#209082=CARTESIAN_POINT('Ctrl Pts',(2.52028415758831,-6.28271462300916,
104.318570490676));
#209083=CARTESIAN_POINT('Ctrl Pts',(2.68460881655648,-6.21169578312293,
104.327018513438));
#209084=CARTESIAN_POINT('Ctrl Pts',(2.84878299852662,-6.14074197730947,
104.335458800094));
#209085=CARTESIAN_POINT('Ctrl Pts',(3.01026364408896,-6.06322319471181,
104.34389908675));
#209086=CARTESIAN_POINT('Ctrl Pts',(3.16850999156815,-5.97936731045458,
104.352339373406));
#209087=CARTESIAN_POINT('Ctrl Pts',(3.3266357892767,-5.89557530639284,104.360773230374));
#209088=CARTESIAN_POINT('Ctrl Pts',(3.48153190691948,-5.80545597994448,
104.369207087342));
#209089=CARTESIAN_POINT('Ctrl Pts',(3.63267947922354,-5.70928443863399,
104.37764094431));
#209090=CARTESIAN_POINT('Ctrl Pts',(3.78373514595703,-5.61317137461322,
104.386069673055));
#209091=CARTESIAN_POINT('Ctrl Pts',(3.93104653099945,-5.51101361138082,
104.3944984018));
#209092=CARTESIAN_POINT('Ctrl Pts',(4.07412086986689,-5.40313132708386,
104.402927130545));
#209093=CARTESIAN_POINT('Ctrl Pts',(4.21713018301642,-5.29529807410197,
104.411352028525));
#209094=CARTESIAN_POINT('Ctrl Pts',(4.35590602398585,-5.18174568838335,
104.419776926505));
#209095=CARTESIAN_POINT('Ctrl Pts',(4.48998571657338,-5.06283687915847,
104.428201824485));
#209096=CARTESIAN_POINT('Ctrl Pts',(4.62403572369899,-4.94395439653726,
104.43662485718));
#209097=CARTESIAN_POINT('Ctrl Pts',(4.75339140443516,-4.81971807401098,
104.445047889874));
#209098=CARTESIAN_POINT('Ctrl Pts',(4.87762380648971,-4.69053035406071,
104.453470922568));
#209099=CARTESIAN_POINT('Ctrl Pts',(5.00184215178932,-4.56135725155395,
104.461893002206));
#209100=CARTESIAN_POINT('Ctrl Pts',(5.12093814295353,-4.42723410881617,
104.470315081843));
#209101=CARTESIAN_POINT('Ctrl Pts',(5.23452007913682,-4.28859983457463,
104.478737161481));
#209102=CARTESIAN_POINT('Ctrl Pts',(5.34810501884234,-4.1499618943353,104.487159463829));
#209103=CARTESIAN_POINT('Ctrl Pts',(5.45617540181385,-4.00681284295275,
104.495581766177));
#209104=CARTESIAN_POINT('Ctrl Pts',(5.55837994643813,-3.8596245116636,104.504004068525));
#209105=CARTESIAN_POINT('Ctrl Pts',(5.6606014615458,-3.71241174058912,104.512427769349));
#209106=CARTESIAN_POINT('Ctrl Pts',(5.75695500678292,-3.5611586266538,104.520851470173));
#209107=CARTESIAN_POINT('Ctrl Pts',(5.84713254406289,-3.40636610072385,
104.529275170996));
#209108=CARTESIAN_POINT('Ctrl Pts',(5.93737110530676,-3.25146882527647,
104.537704572215));
#209109=CARTESIAN_POINT('Ctrl Pts',(6.02142513918779,-3.09302764017662,
104.546133973434));
#209110=CARTESIAN_POINT('Ctrl Pts',(6.09903202398758,-2.93156909698099,
104.554563374653));
#209111=CARTESIAN_POINT('Ctrl Pts',(6.17666659881646,-2.77005294560062,
104.562995783471));
#209112=CARTESIAN_POINT('Ctrl Pts',(6.2478492989051,-2.60551759265549,104.571428192289));
#209113=CARTESIAN_POINT('Ctrl Pts',(6.31236539513704,-2.43851022517365,
104.579860601106));
#209114=CARTESIAN_POINT('Ctrl Pts',(6.37694118353806,-2.27134833761696,
104.588300811834));
#209115=CARTESIAN_POINT('Ctrl Pts',(6.43483792971866,-2.10171017917188,
104.596741022562));
#209116=CARTESIAN_POINT('Ctrl Pts',(6.48589022627108,-1.93015983088483,
104.605181233289));
#209117=CARTESIAN_POINT('Ctrl Pts',(6.51492790138721,-1.83258492013611,
104.609981881126));
#209118=CARTESIAN_POINT('Ctrl Pts',(6.54175222038416,-1.73439164339507,
104.614782528963));
#209119=CARTESIAN_POINT('Ctrl Pts',(6.56634009650628,-1.63568540282473,
104.6195831768));
#209120=CARTESIAN_POINT('Ctrl Pts',(6.6080299499784,-1.46832451790231,104.627722891833));
#209121=CARTESIAN_POINT('Ctrl Pts',(6.6433704814629,-1.29915463673605,104.635862606866));
#209122=CARTESIAN_POINT('Ctrl Pts',(6.67220489363832,-1.12870317502381,
104.644002321899));
#209123=CARTESIAN_POINT('Ctrl Pts',(6.70101408740983,-0.958400789137468,
104.652134917986));
#209124=CARTESIAN_POINT('Ctrl Pts',(6.72332842754207,-0.786819412381466,
104.660267514073));
#209125=CARTESIAN_POINT('Ctrl Pts',(6.73904139668091,-0.614499840375114,
104.66840011016));
#209126=CARTESIAN_POINT('Ctrl Pts',(6.75474362359105,-0.442298075273033,
104.676527146368));
#209127=CARTESIAN_POINT('Ctrl Pts',(6.76385343164389,-0.269359482892504,
104.684654182576));
#209128=CARTESIAN_POINT('Ctrl Pts',(6.76631570154596,-0.0962331908053344,
104.692781218783));
#209129=CARTESIAN_POINT('Ctrl Pts',(6.76877679443847,0.0768103437815226,
104.700904370121));
#209130=CARTESIAN_POINT('Ctrl Pts',(6.76459667171424,0.250041034011858,
104.709027521459));
#209131=CARTESIAN_POINT('Ctrl Pts',(6.75377220999347,0.422906532841329,
104.717150672796));
#209132=CARTESIAN_POINT('Ctrl Pts',(6.74295079002694,0.59572345518014,104.725271541468));
#209133=CARTESIAN_POINT('Ctrl Pts',(6.72548877363209,0.768175025394373,
104.733392410139));
#209134=CARTESIAN_POINT('Ctrl Pts',(6.7014351104815,0.939710838506064,104.741513278811));
#209135=CARTESIAN_POINT('Ctrl Pts',(6.6773801473788,1.11125592207034,104.749634586366));
#209136=CARTESIAN_POINT('Ctrl Pts',(6.6467328727442,1.28188478642956,104.75775589392));
#209137=CARTESIAN_POINT('Ctrl Pts',(6.60959390715445,1.4510538868377,104.765877201475));
#209138=CARTESIAN_POINT('Ctrl Pts',(6.59029520961563,1.53896003203717,104.770097315191));
#209139=CARTESIAN_POINT('Ctrl Pts',(6.56924446865013,1.62647215923695,104.774317428908));
#209140=CARTESIAN_POINT('Ctrl Pts',(6.5464612221734,1.71351523675161,104.778537542625));
#209141=CARTESIAN_POINT('Ctrl Pts',(6.49795668150834,1.89882616235804,104.787521981151));
#209142=CARTESIAN_POINT('Ctrl Pts',(6.44162091720304,2.08191852549232,104.796506419677));
#209143=CARTESIAN_POINT('Ctrl Pts',(6.37768797078266,2.26216381973856,104.805490858203));
#209144=CARTESIAN_POINT('Ctrl Pts',(6.3136446799129,2.44272020660387,104.814490803333));
#209145=CARTESIAN_POINT('Ctrl Pts',(6.24197807890539,2.62041947783379,104.823490748463));
#209146=CARTESIAN_POINT('Ctrl Pts',(6.16297031630131,2.79465308766382,104.832490693594));
#209147=CARTESIAN_POINT('Ctrl Pts',(6.08377636987625,2.9692972834686,104.841511847326));
#209148=CARTESIAN_POINT('Ctrl Pts',(5.99720674718061,3.14045925867974,104.850533001058));
#209149=CARTESIAN_POINT('Ctrl Pts',(5.90359083813182,3.30755260214044,104.859554154791));
#209150=CARTESIAN_POINT('Ctrl Pts',(5.80987967415799,3.47481596439463,104.868584487618));
#209151=CARTESIAN_POINT('Ctrl Pts',(5.70910802255661,3.6380022191138,104.877614820445));
#209152=CARTESIAN_POINT('Ctrl Pts',(5.60164951120217,3.79655261436589,104.886645153272));
#209153=CARTESIAN_POINT('Ctrl Pts',(5.49403865755124,3.95532778410088,104.895688288265));
#209154=CARTESIAN_POINT('Ctrl Pts',(5.37972212307625,4.10945375520907,104.904731423258));
#209155=CARTESIAN_POINT('Ctrl Pts',(5.25911622901807,4.25840175296774,104.91377455825));
#209156=CARTESIAN_POINT('Ctrl Pts',(5.15367889163944,4.38861661861916,104.92168034165));
#209157=CARTESIAN_POINT('Ctrl Pts',(5.04343541851787,4.51487448688405,104.92958612505));
#209158=CARTESIAN_POINT('Ctrl Pts',(4.92868823279422,4.63684389471069,104.93749190845));
#209159=CARTESIAN_POINT('Ctrl Pts',(4.79755503406507,4.77623065608998,104.946526645635));
#209160=CARTESIAN_POINT('Ctrl Pts',(4.66041770868393,4.91014402847871,104.955561382819));
#209161=CARTESIAN_POINT('Ctrl Pts',(4.51775470906506,5.03807318215213,104.964596120004));
#209162=CARTESIAN_POINT('Ctrl Pts',(4.38125891205211,5.16047206510353,104.973240293028));
#209163=CARTESIAN_POINT('Ctrl Pts',(4.23970535783228,5.27739295980276,104.981884466052));
#209164=CARTESIAN_POINT('Ctrl Pts',(4.09355174753297,5.38842491738261,104.990528639076));
#209165=CARTESIAN_POINT('Ctrl Pts',(3.94751050382896,5.49937151078282,104.999166166241));
#209166=CARTESIAN_POINT('Ctrl Pts',(3.79687649770736,5.60443801198851,105.007803693406));
#209167=CARTESIAN_POINT('Ctrl Pts',(3.64214091206989,5.70325333267134,105.016441220571));
#209168=CARTESIAN_POINT('Ctrl Pts',(3.48754311963719,5.80198065756663,105.025071055953));
#209169=CARTESIAN_POINT('Ctrl Pts',(3.32885129101073,5.89446774573588,105.033700891335));
#209170=CARTESIAN_POINT('Ctrl Pts',(3.16658630182934,5.98038629129146,105.042330726717));
#209171=CARTESIAN_POINT('Ctrl Pts',(3.14416066484509,5.99226056018066,105.0435234027));
#209172=CARTESIAN_POINT('Ctrl Pts',(3.12166682451649,6.00400943580988,105.044716078683));
#209173=CARTESIAN_POINT('Ctrl Pts',(3.09910619832126,6.01563211736944,105.045908754666));
#209174=CARTESIAN_POINT('Ctrl Pts',(3.09910619832139,6.01563211736937,103.045799558392));
#209175=CARTESIAN_POINT('Ctrl Pts',(2.94236430513783,6.09638169833182,103.054111211667));
#209176=CARTESIAN_POINT('Ctrl Pts',(2.78233017481925,6.17107055504067,103.062422864941));
#209177=CARTESIAN_POINT('Ctrl Pts',(2.61950763306529,6.2394285603982,103.070734518215));
#209178=CARTESIAN_POINT('Ctrl Pts',(2.45680390152898,6.30773668550323,103.079040106547));
#209179=CARTESIAN_POINT('Ctrl Pts',(2.29131613225174,6.36972302967539,103.087345694879));
#209180=CARTESIAN_POINT('Ctrl Pts',(2.12357116630314,6.42516416145502,103.095651283211));
#209181=CARTESIAN_POINT('Ctrl Pts',(1.9559178560199,6.48057500026106,103.103952333379));
#209182=CARTESIAN_POINT('Ctrl Pts',(1.78601013636463,6.52944764453699,103.112253383547));
#209183=CARTESIAN_POINT('Ctrl Pts',(1.61439338256553,6.57160733811209,103.120554433714));
#209184=CARTESIAN_POINT('Ctrl Pts',(1.44283895574051,6.61375172032585,103.128852469145));
#209185=CARTESIAN_POINT('Ctrl Pts',(1.26957706925807,6.64918792812348,103.137150504576));
#209186=CARTESIAN_POINT('Ctrl Pts',(1.09516698237773,6.67779142237235,103.145448540007));
#209187=CARTESIAN_POINT('Ctrl Pts',(0.917825849735268,6.70687561215953,
103.153886027932));
#209188=CARTESIAN_POINT('Ctrl Pts',(0.739297935222967,6.72889528581189,
103.162323515856));
#209189=CARTESIAN_POINT('Ctrl Pts',(0.560181124280923,6.74377387728854,
103.170761003781));
#209190=CARTESIAN_POINT('Ctrl Pts',(0.384014197523693,6.75840743245924,
103.179059534273));
#209191=CARTESIAN_POINT('Ctrl Pts',(0.207277979361667,6.76613330032755,
103.187358064766));
#209192=CARTESIAN_POINT('Ctrl Pts',(0.0305455202347726,6.76693106002962,
103.195656595258));
#209193=CARTESIAN_POINT('Ctrl Pts',(-0.14622375551021,6.7677289859197,103.203956854486));
#209194=CARTESIAN_POINT('Ctrl Pts',(-0.322988922558483,6.76159592535089,
103.212257113715));
#209195=CARTESIAN_POINT('Ctrl Pts',(-0.499177629272033,6.74856360231082,
103.220557372943));
#209196=CARTESIAN_POINT('Ctrl Pts',(-0.675432321873086,6.73552639842783,
103.22886074077));
#209197=CARTESIAN_POINT('Ctrl Pts',(-0.851109776893836,6.71558480798511,
103.237164108598));
#209198=CARTESIAN_POINT('Ctrl Pts',(-1.02564326441134,6.68882238470777,
103.245467476425));
#209199=CARTESIAN_POINT('Ctrl Pts',(-1.20515202141174,6.66129706904963,
103.254007540906));
#209200=CARTESIAN_POINT('Ctrl Pts',(-1.38345023086992,6.62655634228058,
103.262547605388));
#209201=CARTESIAN_POINT('Ctrl Pts',(-1.55993391594156,6.58474716127318,
103.271087669869));
#209202=CARTESIAN_POINT('Ctrl Pts',(-1.73182960695066,6.54402488115492,
103.279405720825));
#209203=CARTESIAN_POINT('Ctrl Pts',(-1.90200362431914,6.49659723332589,
103.287723771781));
#209204=CARTESIAN_POINT('Ctrl Pts',(-2.0699146776535,6.44265024871245,103.296041822737));
#209205=CARTESIAN_POINT('Ctrl Pts',(-2.24454819370229,6.3865434504035,103.304692893981));
#209206=CARTESIAN_POINT('Ctrl Pts',(-2.41673340417195,6.32338468216138,
103.313343965225));
#209207=CARTESIAN_POINT('Ctrl Pts',(-2.58588599787128,6.25343766307887,
103.321995036469));
#209208=CARTESIAN_POINT('Ctrl Pts',(-2.7550385915706,6.18349064399635,103.330646107713));
#209209=CARTESIAN_POINT('Ctrl Pts',(-2.92115821549834,6.1067556047809,103.339297178958));
#209210=CARTESIAN_POINT('Ctrl Pts',(-3.08369109684616,6.02354864006524,
103.347948250202));
#209211=CARTESIAN_POINT('Ctrl Pts',(-3.23530414982311,5.94593196432015,
103.356018096205));
#209212=CARTESIAN_POINT('Ctrl Pts',(-3.38426480533369,5.86244398788228,
103.364087942207));
#209213=CARTESIAN_POINT('Ctrl Pts',(-3.5300736531061,5.7732892707404,103.37215778821));
#209214=CARTESIAN_POINT('Ctrl Pts',(-3.67569905480191,5.68424672157268,
103.38021748132));
#209215=CARTESIAN_POINT('Ctrl Pts',(-3.81818022451315,5.58955180955035,
103.38827717443));
#209216=CARTESIAN_POINT('Ctrl Pts',(-3.95703853568271,5.48945671511508,
103.39633686754));
#209217=CARTESIAN_POINT('Ctrl Pts',(-4.09575262044103,5.38946558533365,
103.404388189379));
#209218=CARTESIAN_POINT('Ctrl Pts',(-4.23085103481182,5.28408565131226,
103.412439511218));
#209219=CARTESIAN_POINT('Ctrl Pts',(-4.36188064280269,5.17361442880538,
103.420490833056));
#209220=CARTESIAN_POINT('Ctrl Pts',(-4.49280286878587,5.06323374020031,
103.428535556637));
#209221=CARTESIAN_POINT('Ctrl Pts',(-4.61966264130249,4.94777030686426,
103.436580280218));
#209222=CARTESIAN_POINT('Ctrl Pts',(-4.74203676498044,4.82756422221122,
103.444625003799));
#209223=CARTESIAN_POINT('Ctrl Pts',(-4.86433738778352,4.70743033625609,
103.452664895524));
#209224=CARTESIAN_POINT('Ctrl Pts',(-4.98215745955112,4.58255973036248,
103.460704787248));
#209225=CARTESIAN_POINT('Ctrl Pts',(-5.09510787076625,4.45333187459186,
103.468744678972));
#209226=CARTESIAN_POINT('Ctrl Pts',(-5.21049041378296,4.32132138904337,
103.476957691592));
#209227=CARTESIAN_POINT('Ctrl Pts',(-5.3207908982104,4.1847641347449,103.485170704212));
#209228=CARTESIAN_POINT('Ctrl Pts',(-5.42563495129075,4.04410365536447,
103.493383716832));
#209229=CARTESIAN_POINT('Ctrl Pts',(-5.5282332020267,3.90645618077615,103.501420803375));
#209230=CARTESIAN_POINT('Ctrl Pts',(-5.62560618959596,3.76487980538032,
103.509457889917));
#209231=CARTESIAN_POINT('Ctrl Pts',(-5.71744473488568,3.61982246850975,
103.51749497646));
#209232=CARTESIAN_POINT('Ctrl Pts',(-5.80929206955164,3.47475124897689,
103.525532832189));
#209233=CARTESIAN_POINT('Ctrl Pts',(-5.89560370729836,3.32619872024178,
103.533570687918));
#209234=CARTESIAN_POINT('Ctrl Pts',(-5.97611480369843,3.17464027143493,
103.541608543648));
#209235=CARTESIAN_POINT('Ctrl Pts',(-6.05664955732139,3.0230372889903,103.549648761205));
#209236=CARTESIAN_POINT('Ctrl Pts',(-6.13138020182837,2.86842695816172,
103.557688978762));
#209237=CARTESIAN_POINT('Ctrl Pts',(-6.20008876476533,2.71130749068245,
103.565729196319));
#209238=CARTESIAN_POINT('Ctrl Pts',(-6.27139318123286,2.54825194905253,
103.574073178446));
#209239=CARTESIAN_POINT('Ctrl Pts',(-6.33621141358448,2.38249438169519,
103.582417160574));
#209240=CARTESIAN_POINT('Ctrl Pts',(-6.39435583166184,2.21461113925045,
103.590761142702));
#209241=CARTESIAN_POINT('Ctrl Pts',(-6.45048102793904,2.05255809537398,
103.598815357537));
#209242=CARTESIAN_POINT('Ctrl Pts',(-6.50038812801885,1.88852491222502,
103.606869572372));
#209243=CARTESIAN_POINT('Ctrl Pts',(-6.54396024116556,1.72304189213275,
103.614923787207));
#209244=CARTESIAN_POINT('Ctrl Pts',(-6.58756496083387,1.55743503536424,
103.62298402929));
#209245=CARTESIAN_POINT('Ctrl Pts',(-6.62482517347593,1.39037654348746,
103.631044271373));
#209246=CARTESIAN_POINT('Ctrl Pts',(-6.65567557661696,1.2224040325623,103.639104513456));
#209247=CARTESIAN_POINT('Ctrl Pts',(-6.68656911073776,1.05419668454476,
103.647176024311));
#209248=CARTESIAN_POINT('Ctrl Pts',(-6.71103490292835,0.885073134178257,
103.655247535165));
#209249=CARTESIAN_POINT('Ctrl Pts',(-6.72905960490018,0.715573779355196,
103.663319046019));
#209250=CARTESIAN_POINT('Ctrl Pts',(-6.7309487818599,0.697808477253693,
103.66416502463));
#209251=CARTESIAN_POINT('Ctrl Pts',(-6.73276724909369,0.680039044307874,
103.665011003241));
#209252=CARTESIAN_POINT('Ctrl Pts',(-6.73451502427644,0.662266100442202,
103.665856981852));
#209253=CARTESIAN_POINT('Ctrl Pts',(-6.75608578867897,0.442915243049773,
103.676297915838));
#209254=CARTESIAN_POINT('Ctrl Pts',(-6.76693576375581,0.222572616147481,
103.686738849824));
#209255=CARTESIAN_POINT('Ctrl Pts',(-6.76699971567234,0.00196165502752502,
103.69717978381));
#209256=CARTESIAN_POINT('',(-6.767,-8.20588493674615E-10,103.302820216229));
#209257=CARTESIAN_POINT('Ctrl Pts',(3.09910619832148,6.01563211736933,102.651395695404));
#209258=CARTESIAN_POINT('Ctrl Pts',(2.93375330764841,6.10081787314646,102.660145143307));
#209259=CARTESIAN_POINT('Ctrl Pts',(2.76488627843085,6.17918207037032,102.668894591209));
#209260=CARTESIAN_POINT('Ctrl Pts',(2.59307866646717,6.25045854553991,102.677644039111));
#209261=CARTESIAN_POINT('Ctrl Pts',(2.42127244185387,6.32173444515033,102.686393416361));
#209262=CARTESIAN_POINT('Ctrl Pts',(2.2465259467247,6.38592262741836,102.695142793612));
#209263=CARTESIAN_POINT('Ctrl Pts',(2.06943269687121,6.44280508110562,102.703892170862));
#209264=CARTESIAN_POINT('Ctrl Pts',(1.89234081822078,6.49968709436166,102.712641480367));
#209265=CARTESIAN_POINT('Ctrl Pts',(1.7129024940559,6.54926340459544,102.721390789873));
#209266=CARTESIAN_POINT('Ctrl Pts',(1.53172716625061,6.59136563150383,102.730140099378));
#209267=CARTESIAN_POINT('Ctrl Pts',(1.35055318107354,6.63346754640705,102.738889344045));
#209268=CARTESIAN_POINT('Ctrl Pts',(1.16764249714457,6.66809542395769,102.747638588713));
#209269=CARTESIAN_POINT('Ctrl Pts',(0.983616340614903,6.6951316562466,102.75638783338));
#209270=CARTESIAN_POINT('Ctrl Pts',(0.799591486714394,6.72216769715954,
102.765137016116));
#209271=CARTESIAN_POINT('Ctrl Pts',(0.614451459527268,6.74161215869366,
102.773886198851));
#209272=CARTESIAN_POINT('Ctrl Pts',(0.428825047910842,6.75339900185709,
102.782635381587));
#209273=CARTESIAN_POINT('Ctrl Pts',(0.243199888597644,6.76518576550218,
102.791384505298));
#209274=CARTESIAN_POINT('Ctrl Pts',(0.057088637392555,6.76931499599834,
102.800133629008));
#209275=CARTESIAN_POINT('Ctrl Pts',(-0.128876626810473,6.76577266947848,
102.808882752719));
#209276=CARTESIAN_POINT('Ctrl Pts',(-0.314840698187551,6.76223036567996,
102.81763182031));
#209277=CARTESIAN_POINT('Ctrl Pts',(-0.500658497950714,6.75101660879227,
102.826380887902));
#209278=CARTESIAN_POINT('Ctrl Pts',(-0.685698951925747,6.73216948296223,
102.835129955493));
#209279=CARTESIAN_POINT('Ctrl Pts',(-0.870738280459417,6.71332247176299,
102.843878969872));
#209280=CARTESIAN_POINT('Ctrl Pts',(-1.05499998761211,6.68684221356193,
102.85262798425));
#209281=CARTESIAN_POINT('Ctrl Pts',(-1.23785829161383,6.65281863948529,
102.861376998629));
#209282=CARTESIAN_POINT('Ctrl Pts',(-1.43007412917363,6.6170539536887,102.870573732328));
#209283=CARTESIAN_POINT('Ctrl Pts',(-1.62073882535748,6.57295372727801,
102.879770466027));
#209284=CARTESIAN_POINT('Ctrl Pts',(-1.80913696091466,6.52068343478293,
102.888967199726));
#209285=CARTESIAN_POINT('Ctrl Pts',(-1.98838356186064,6.47095219815213,
102.89771719744));
#209286=CARTESIAN_POINT('Ctrl Pts',(-2.16557827572486,6.41382586850907,
102.906467195154));
#209287=CARTESIAN_POINT('Ctrl Pts',(-2.34011918621653,6.34949849943295,
102.915217192867));
#209288=CARTESIAN_POINT('Ctrl Pts',(-2.51465655691045,6.28517243495572,
102.923967013126));
#209289=CARTESIAN_POINT('Ctrl Pts',(-2.68653996295269,6.213645722424,102.932716833384));
#209290=CARTESIAN_POINT('Ctrl Pts',(-2.85518555379923,6.13516132252251,
102.941466653642));
#209291=CARTESIAN_POINT('Ctrl Pts',(-3.02382794858626,6.05667841000538,
102.95021630808));
#209292=CARTESIAN_POINT('Ctrl Pts',(-3.1892323910922,5.97123819492113,102.958965962517));
#209293=CARTESIAN_POINT('Ctrl Pts',(-3.3508370596764,5.87913088810746,102.967715616955));
#209294=CARTESIAN_POINT('Ctrl Pts',(-3.51243888042337,5.78702520443141,
102.976465117204));
#209295=CARTESIAN_POINT('Ctrl Pts',(-3.67024081223624,5.68825280605826,
102.985214617453));
#209296=CARTESIAN_POINT('Ctrl Pts',(-3.82370687544332,5.58314917682552,
102.993964117702));
#209297=CARTESIAN_POINT('Ctrl Pts',(-3.97717043817743,5.47804726008073,
103.002713475392));
#209298=CARTESIAN_POINT('Ctrl Pts',(-4.12629803722387,5.36661448084292,
103.011462833083));
#209299=CARTESIAN_POINT('Ctrl Pts',(-4.27058317206833,5.24922931204638,
103.020212190773));
#209300=CARTESIAN_POINT('Ctrl Pts',(-4.41486614774765,5.13184589986851,
103.028961417533));
#209301=CARTESIAN_POINT('Ctrl Pts',(-4.55430658194349,5.00851045723093,
103.037710644293));
#209302=CARTESIAN_POINT('Ctrl Pts',(-4.68843089001786,4.87964187103176,
103.046459871053));
#209303=CARTESIAN_POINT('Ctrl Pts',(-4.82255336917795,4.75077504208004,
103.055208978509));
#209304=CARTESIAN_POINT('Ctrl Pts',(-4.95135966065109,4.61637541908121,
103.063958085965));
#209305=CARTESIAN_POINT('Ctrl Pts',(-5.07441230869235,4.47689945401855,
103.072707193421));
#209306=CARTESIAN_POINT('Ctrl Pts',(-5.19746344226414,4.3374252055552,103.081456193197));
#209307=CARTESIAN_POINT('Ctrl Pts',(-5.31476088454769,4.19287495491334,
103.090205192974));
#209308=CARTESIAN_POINT('Ctrl Pts',(-5.42590627628861,4.04373961586696,
103.09895419275));
#209309=CARTESIAN_POINT('Ctrl Pts',(-5.53706380672676,3.89458798906723,
103.107704148045));
#209310=CARTESIAN_POINT('Ctrl Pts',(-5.64206777071873,3.7408505015527,103.11645410334));
#209311=CARTESIAN_POINT('Ctrl Pts',(-5.74056148164017,3.58304938223145,
103.125204058634));
#209312=CARTESIAN_POINT('Ctrl Pts',(-5.83905138951896,3.42525435593261,
103.133953676075));
#209313=CARTESIAN_POINT('Ctrl Pts',(-5.93103139557668,3.26339625497156,
103.142703293516));
#209314=CARTESIAN_POINT('Ctrl Pts',(-6.01618907820863,3.09802485064971,
103.151452910958));
#209315=CARTESIAN_POINT('Ctrl Pts',(-6.10134392544994,2.93265895249617,
103.160202237073));
#209316=CARTESIAN_POINT('Ctrl Pts',(-6.17967677261837,2.76378023986023,
103.168951563189));
#209317=CARTESIAN_POINT('Ctrl Pts',(-6.25092157009224,2.59196229227116,
103.177700889305));
#209318=CARTESIAN_POINT('Ctrl Pts',(-6.32216437407745,2.4201491522911,103.186449970608));
#209319=CARTESIAN_POINT('Ctrl Pts',(-6.38631941548907,2.2453972066289,103.19519905191));
#209320=CARTESIAN_POINT('Ctrl Pts',(-6.44316881037518,2.06829994947746,
103.203948133213));
#209321=CARTESIAN_POINT('Ctrl Pts',(-6.50002334524552,1.89118668024516,
103.212698005555));
#209322=CARTESIAN_POINT('Ctrl Pts',(-6.54957082411077,1.71172794807774,
103.221447877897));
#209323=CARTESIAN_POINT('Ctrl Pts',(-6.59164294296065,1.53053334250419,
103.23019775024));
#209324=CARTESIAN_POINT('Ctrl Pts',(-6.63371214082118,1.34935131693678,
103.238947015094));
#209325=CARTESIAN_POINT('Ctrl Pts',(-6.66830695239676,1.16643393829841,
103.247696279949));
#209326=CARTESIAN_POINT('Ctrl Pts',(-6.69530988153977,0.982402458341761,
103.256445544804));
#209327=CARTESIAN_POINT('Ctrl Pts',(-6.72231419690474,0.798361530947849,
103.265195258811));
#209328=CARTESIAN_POINT('Ctrl Pts',(-6.7417258082927,0.613206671363285,
103.273944972818));
#209329=CARTESIAN_POINT('Ctrl Pts',(-6.75347878028174,0.427566795114224,
103.282694686825));
#209330=CARTESIAN_POINT('Ctrl Pts',(-6.76248992368206,0.285234494207036,
103.289403196614));
#209331=CARTESIAN_POINT('Ctrl Pts',(-6.76699999999989,0.142617266094836,
103.296111706402));
#209332=CARTESIAN_POINT('Ctrl Pts',(-6.767,5.08377026670387E-12,103.30282021619));
#209333=CARTESIAN_POINT('Ctrl Pts',(-6.767,-8.20396992685389E-10,103.302820216229));
#209334=CARTESIAN_POINT('Ctrl Pts',(-6.76699999997745,-0.18600725034739,
103.31156972804));
#209335=CARTESIAN_POINT('Ctrl Pts',(-6.75932637290009,-0.372014356569628,
103.320319239851));
#209336=CARTESIAN_POINT('Ctrl Pts',(-6.7440051825742,-0.557389538305465,
103.329068751662));
#209337=CARTESIAN_POINT('Ctrl Pts',(-6.72868405696075,-0.742763937068103,
103.337818226518));
#209338=CARTESIAN_POINT('Ctrl Pts',(-6.7057154563447,-0.927506131055983,
103.346567701374));
#209339=CARTESIAN_POINT('Ctrl Pts',(-6.67517739391316,-1.11098864071181,
103.355317176229));
#209340=CARTESIAN_POINT('Ctrl Pts',(-6.6446394579296,-1.29447039062751,
103.364066614856));
#209341=CARTESIAN_POINT('Ctrl Pts',(-6.60653216990395,-1.47669218394034,
103.372816053483));
#209342=CARTESIAN_POINT('Ctrl Pts',(-6.56098496072521,-1.65703510679093,
103.38156549211));
#209343=CARTESIAN_POINT('Ctrl Pts',(-6.51543793635944,-1.83737729787963,
103.390314895236));
#209344=CARTESIAN_POINT('Ctrl Pts',(-6.46245112142894,-2.01584035589556,
103.399064298361));
#209345=CARTESIAN_POINT('Ctrl Pts',(-6.40220448347582,-2.19181813838697,
103.407813701486));
#209346=CARTESIAN_POINT('Ctrl Pts',(-6.34195808497692,-2.36779522144313,
103.416563069836));
#209347=CARTESIAN_POINT('Ctrl Pts',(-6.27445201402183,-2.5412867776051,
103.425312438186));
#209348=CARTESIAN_POINT('Ctrl Pts',(-6.19991555038909,-2.71170355460246,
103.434061806536));
#209349=CARTESIAN_POINT('Ctrl Pts',(-6.12537937681621,-2.88211966842015,
103.442811140838));
#209350=CARTESIAN_POINT('Ctrl Pts',(-6.04381298015407,-3.04946076445341,
103.45156047514));
#209351=CARTESIAN_POINT('Ctrl Pts',(-5.9554933929672,-3.21315848447038,
103.460309809442));
#209352=CARTESIAN_POINT('Ctrl Pts',(-5.86717414214314,-3.37685558104894,
103.469059110422));
#209353=CARTESIAN_POINT('Ctrl Pts',(-5.77210188833564,-3.53690907716986,
103.477808411402));
#209354=CARTESIAN_POINT('Ctrl Pts',(-5.67059953302075,-3.69277537038267,
103.486557712382));
#209355=CARTESIAN_POINT('Ctrl Pts',(-5.56909755584588,-3.84864108292636,
103.495306980767));
#209356=CARTESIAN_POINT('Ctrl Pts',(-5.46116568148233,-4.00031938363886,
103.504056249153));
#209357=CARTESIAN_POINT('Ctrl Pts',(-5.34717048483224,-4.14729511924808,
103.512805517538));
#209358=CARTESIAN_POINT('Ctrl Pts',(-5.23317570339677,-4.2942703195148,
103.521554754055));
#209359=CARTESIAN_POINT('Ctrl Pts',(-5.11311781949632,-4.43654276251646,
103.530303990572));
#209360=CARTESIAN_POINT('Ctrl Pts',(-4.98740458929211,-4.57362924412419,
103.539053227089));
#209361=CARTESIAN_POINT('Ctrl Pts',(-4.86169180654557,-4.71071523779284,
103.547802432465));
#209362=CARTESIAN_POINT('Ctrl Pts',(-4.73032391145408,-4.84261509580638,
103.55655163784));
#209363=CARTESIAN_POINT('Ctrl Pts',(-4.59374706953327,-4.96888084594052,
103.565300843215));
#209364=CARTESIAN_POINT('Ctrl Pts',(-4.45717070239636,-5.09514615713534,
103.574050018176));
#209365=CARTESIAN_POINT('Ctrl Pts',(-4.31538563507762,-5.21577720511883,
103.582799193136));
#209366=CARTESIAN_POINT('Ctrl Pts',(-4.16887340964834,-5.33036429283469,
103.591548368097));
#209367=CARTESIAN_POINT('Ctrl Pts',(-4.02236168137632,-5.44495099172427,
103.600297513369));
#209368=CARTESIAN_POINT('Ctrl Pts',(-3.87112305280765,-5.55349359485584,
103.609046658641));
#209369=CARTESIAN_POINT('Ctrl Pts',(-3.71567116949112,-5.65562346343995,
103.617795803913));
#209370=CARTESIAN_POINT('Ctrl Pts',(-3.56021980075929,-5.75775299394859,
103.626544920223));
#209371=CARTESIAN_POINT('Ctrl Pts',(-3.40055544467297,-5.8534696750515,
103.635294036533));
#209372=CARTESIAN_POINT('Ctrl Pts',(-3.2372203591472,-5.94244843026197,
103.644043152843));
#209373=CARTESIAN_POINT('Ctrl Pts',(-3.07388580073972,-6.03142689831839,
103.652792240918));
#209374=CARTESIAN_POINT('Ctrl Pts',(-2.90688078822377,-6.11366734692062,
103.661541328993));
#209375=CARTESIAN_POINT('Ctrl Pts',(-2.73677250646261,-6.18889046985567,
103.670290417068));
#209376=CARTESIAN_POINT('Ctrl Pts',(-2.5666647595545,-6.26411335627481,
103.679039477634));
#209377=CARTESIAN_POINT('Ctrl Pts',(-2.39345402498295,-6.33231884529611,
103.6877885382));
#209378=CARTESIAN_POINT('Ctrl Pts',(-2.2177285598797,-6.39327529789653,
103.696537598766));
#209379=CARTESIAN_POINT('Ctrl Pts',(-2.04200363270099,-6.45423156389922,
103.70528663255));
#209380=CARTESIAN_POINT('Ctrl Pts',(-1.86376426110157,-6.50793874398319,
103.714035666333));
#209381=CARTESIAN_POINT('Ctrl Pts',(-1.68361577673416,-6.55421443930025,
103.722784700117));
#209382=CARTESIAN_POINT('Ctrl Pts',(-1.50346782887536,-6.6004899968015,
103.731533707845));
#209383=CARTESIAN_POINT('Ctrl Pts',(-1.32141105714289,-6.63933404253772,
103.740282715573));
#209384=CARTESIAN_POINT('Ctrl Pts',(-1.13806375405982,-6.67061465621387,
103.749031723301));
#209385=CARTESIAN_POINT('Ctrl Pts',(-0.954716981788821,-6.70189517932895,
103.757780705699));
#209386=CARTESIAN_POINT('Ctrl Pts',(-0.770079968085066,-6.72561226601584,
103.766529688097));
#209387=CARTESIAN_POINT('Ctrl Pts',(-0.584779764739224,-6.74168536990207,
103.775278670496));
#209388=CARTESIAN_POINT('Ctrl Pts',(-0.391489829838794,-6.75845151018535,
103.784404889505));
#209389=CARTESIAN_POINT('Ctrl Pts',(-0.197478577433421,-6.7668998303395,
103.793531108515));
#209390=CARTESIAN_POINT('Ctrl Pts',(-0.0034628756550048,-6.76699911397159,
103.802657327524));
#209391=CARTESIAN_POINT('Ctrl Pts',(0.184489835442792,-6.76709529499017,
103.81149835219));
#209392=CARTESIAN_POINT('Ctrl Pts',(0.372446405029021,-6.75935639733849,
103.820339376855));
#209393=CARTESIAN_POINT('Ctrl Pts',(0.559755020257901,-6.74380925866799,
103.82918040152));
#209394=CARTESIAN_POINT('Ctrl Pts',(0.745134706289568,-6.72842222651303,
103.83793038013));
#209395=CARTESIAN_POINT('Ctrl Pts',(0.929879431993717,-6.70538706046913,
103.84668035874));
#209396=CARTESIAN_POINT('Ctrl Pts',(1.1133616370299,-6.67478200881423,103.85543033735));
#209397=CARTESIAN_POINT('Ctrl Pts',(1.29684196376553,-6.64417727046211,
103.864180226386));
#209398=CARTESIAN_POINT('Ctrl Pts',(1.47905951292928,-6.60600284873705,
103.872930115423));
#209399=CARTESIAN_POINT('Ctrl Pts',(1.65939532142,-6.56038841588281,103.881680004459));
#209400=CARTESIAN_POINT('Ctrl Pts',(1.83972934375199,-6.51477443482247,
103.890429806831));
#209401=CARTESIAN_POINT('Ctrl Pts',(2.01818138480058,-6.46172066039093,
103.899179609204));
#209402=CARTESIAN_POINT('Ctrl Pts',(2.19414528427307,-6.4014073039842,103.907929411576));
#209403=CARTESIAN_POINT('Ctrl Pts',(2.3701074993642,-6.34109452491574,103.916679130192));
#209404=CARTESIAN_POINT('Ctrl Pts',(2.5435813493811,-6.27352239587453,103.925428848808));
#209405=CARTESIAN_POINT('Ctrl Pts',(2.71397759506356,-6.19892043935821,
103.934178567425));
#209406=CARTESIAN_POINT('Ctrl Pts',(2.8843722662808,-6.12431917216568,103.942928205193));
#209407=CARTESIAN_POINT('Ctrl Pts',(3.05168912749988,-6.04268832243936,
103.951677842962));
#209408=CARTESIAN_POINT('Ctrl Pts',(3.21535986341885,-5.95430516086597,
103.960427480731));
#209409=CARTESIAN_POINT('Ctrl Pts',(3.3790291413987,-5.8659227865883,103.96917704056));
#209410=CARTESIAN_POINT('Ctrl Pts',(3.5390521068752,-5.77078835701498,103.977926600389));
#209411=CARTESIAN_POINT('Ctrl Pts',(3.69488522896492,-5.66922500389399,
103.986676160218));
#209412=CARTESIAN_POINT('Ctrl Pts',(3.85071701470592,-5.56766252173071,
103.995425645015));
#209413=CARTESIAN_POINT('Ctrl Pts',(4.00235878884838,-5.45967138283602,
104.004175129812));
#209414=CARTESIAN_POINT('Ctrl Pts',(4.14929549672471,-5.34561838152145,
104.012924614609));
#209415=CARTESIAN_POINT('Ctrl Pts',(4.29623099335929,-5.23156632037875,
104.021674027282));
#209416=CARTESIAN_POINT('Ctrl Pts',(4.4384612749449,-5.11145267254199,104.030423439955));
#209417=CARTESIAN_POINT('Ctrl Pts',(4.57550326111464,-4.98568539997555,
104.039172852627));
#209418=CARTESIAN_POINT('Ctrl Pts',(4.71254416313363,-4.85991912236464,
104.047922196082));
#209419=CARTESIAN_POINT('Ctrl Pts',(4.84439664072839,-4.72849950330015,
104.056671539538));
#209420=CARTESIAN_POINT('Ctrl Pts',(4.9706128684726,-4.59187289804222,104.065420882993));
#209421=CARTESIAN_POINT('Ctrl Pts',(5.09682813963641,-4.45524732826391,
104.074170160138));
#209422=CARTESIAN_POINT('Ctrl Pts',(5.21740705197177,-4.31341506176109,
104.082919437283));
#209423=CARTESIAN_POINT('Ctrl Pts',(5.33194007593362,-4.16685781214731,
104.091668714427));
#209424=CARTESIAN_POINT('Ctrl Pts',(5.44647226990471,-4.02030162459543,
104.100417928168));
#209425=CARTESIAN_POINT('Ctrl Pts',(5.55495848672365,-3.86902074824399,
104.10916714191));
#209426=CARTESIAN_POINT('Ctrl Pts',(5.65703027334258,-3.71352898015965,
104.117916355651));
#209427=CARTESIAN_POINT('Ctrl Pts',(5.75910135417682,-3.55803828723734,
104.126665508895));
#209428=CARTESIAN_POINT('Ctrl Pts',(5.85475793631605,-3.39833700039775,
104.135414662138));
#209429=CARTESIAN_POINT('Ctrl Pts',(5.94367514464377,-3.23496750755612,
104.144163815382));
#209430=CARTESIAN_POINT('Ctrl Pts',(6.03259176767751,-3.07159909008767,
104.152912911035));
#209431=CARTESIAN_POINT('Ctrl Pts',(6.11476896869126,-2.90456276661537,
104.161662006688));
#209432=CARTESIAN_POINT('Ctrl Pts',(6.18992765579143,-2.73442582932294,
104.170411102341));
#209433=CARTESIAN_POINT('Ctrl Pts',(6.26508587312365,-2.56428995544558,
104.179160143309));
#209434=CARTESIAN_POINT('Ctrl Pts',(6.3332255485449,-2.39105376862813,104.187909184277));
#209435=CARTESIAN_POINT('Ctrl Pts',(6.3941152675835,-2.21530560980998,104.196658225245));
#209436=CARTESIAN_POINT('Ctrl Pts',(6.45500462626153,-2.03955849111338,
104.205407214434));
#209437=CARTESIAN_POINT('Ctrl Pts',(6.50864402062003,-1.8612997009019,104.214156203623));
#209438=CARTESIAN_POINT('Ctrl Pts',(6.55485128387801,-1.68113463061194,
104.222905192812));
#209439=CARTESIAN_POINT('Ctrl Pts',(6.60199809571025,-1.49730620043037,
104.231832078283));
#209440=CARTESIAN_POINT('Ctrl Pts',(6.64140720722179,-1.31149343173021,
104.240758963754));
#209441=CARTESIAN_POINT('Ctrl Pts',(6.67293928734917,-1.1243532662611,104.249685849224));
#209442=CARTESIAN_POINT('Ctrl Pts',(6.70384625886327,-0.940923066289126,
104.258435763402));
#209443=CARTESIAN_POINT('Ctrl Pts',(6.72718554587889,-0.756217898801698,
104.267185677579));
#209444=CARTESIAN_POINT('Ctrl Pts',(6.74287786821437,-0.570865180532846,
104.275935591757));
#209445=CARTESIAN_POINT('Ctrl Pts',(6.75856988194971,-0.385516107350657,
104.284685333861));
#209446=CARTESIAN_POINT('Ctrl Pts',(6.76661520775538,-0.199519794502239,
104.293435075966));
#209447=CARTESIAN_POINT('Ctrl Pts',(6.76698651789723,-0.013508019731541,
104.30218481807));
#209448=CARTESIAN_POINT('Ctrl Pts',(6.76735782123057,0.172500344237066,
104.310934399735));
#209449=CARTESIAN_POINT('Ctrl Pts',(6.76005538991348,0.358523882934203,
104.3196839814));
#209450=CARTESIAN_POINT('Ctrl Pts',(6.74510402736542,0.543930749286017,
104.328433563065));
#209451=CARTESIAN_POINT('Ctrl Pts',(6.73015291910227,0.729334462335302,
104.337182995922));
#209452=CARTESIAN_POINT('Ctrl Pts',(6.70755316296814,0.914121238352356,
104.345932428778));
#209453=CARTESIAN_POINT('Ctrl Pts',(6.67738151862829,1.09766345237569,104.354681861635));
#209454=CARTESIAN_POINT('Ctrl Pts',(6.64721034733862,1.28120278870779,104.363431157313));
#209455=CARTESIAN_POINT('Ctrl Pts',(6.60946757189487,1.4634973193103,104.37218045299));
#209456=CARTESIAN_POINT('Ctrl Pts',(6.5642813809394,1.6439279034837,104.380929748668));
#209457=CARTESIAN_POINT('Ctrl Pts',(6.51909583840338,1.8243558984878,104.389678918793));
#209458=CARTESIAN_POINT('Ctrl Pts',(6.46646716371454,2.00291972261425,104.398428088919));
#209459=CARTESIAN_POINT('Ctrl Pts',(6.40657409849579,2.17901292343182,104.407177259044));
#209460=CARTESIAN_POINT('Ctrl Pts',(6.34668181316888,2.35510383126856,104.415926315244));
#209461=CARTESIAN_POINT('Ctrl Pts',(6.27952541887005,2.52872390889741,104.424675371443));
#209462=CARTESIAN_POINT('Ctrl Pts',(6.20533299146647,2.69928350956653,104.433424427642));
#209463=CARTESIAN_POINT('Ctrl Pts',(6.12831602961987,2.87633638028405,104.442506563799));
#209464=CARTESIAN_POINT('Ctrl Pts',(6.04371690575289,3.05009086660679,104.451588699955));
#209465=CARTESIAN_POINT('Ctrl Pts',(5.95184520286494,3.21991112938442,104.460670836112));
#209466=CARTESIAN_POINT('Ctrl Pts',(5.86333549477603,3.38351691237901,104.469420616456));
#209467=CARTESIAN_POINT('Ctrl Pts',(5.76807618066197,3.54347103766002,104.478170396799));
#209468=CARTESIAN_POINT('Ctrl Pts',(5.66639083274382,3.69923018080746,104.486920177143));
#209469=CARTESIAN_POINT('Ctrl Pts',(5.56470914046111,3.85498372434145,104.495669642928));
#209470=CARTESIAN_POINT('Ctrl Pts',(5.45660203334561,4.00654234753078,104.504419108713));
#209471=CARTESIAN_POINT('Ctrl Pts',(5.34243669800338,4.15339128036677,104.513168574498));
#209472=CARTESIAN_POINT('Ctrl Pts',(5.22827486010339,4.30023571450219,104.521917772244));
#209473=CARTESIAN_POINT('Ctrl Pts',(5.10805534125529,4.44237052076283,104.53066696999));
#209474=CARTESIAN_POINT('Ctrl Pts',(4.98218644297088,4.57931296675355,104.539416167736));
#209475=CARTESIAN_POINT('Ctrl Pts',(4.85632073175437,4.71625194528822,104.548165143947));
#209476=CARTESIAN_POINT('Ctrl Pts',(4.72480612124931,4.84799861568743,104.556914120159));
#209477=CARTESIAN_POINT('Ctrl Pts',(4.58808925188738,4.97410554941444,104.565663096371));
#209478=CARTESIAN_POINT('Ctrl Pts',(4.45136349426295,5.10022068162884,104.574412641372));
#209479=CARTESIAN_POINT('Ctrl Pts',(4.309435011612,5.22069514912182,104.583162186374));
#209480=CARTESIAN_POINT('Ctrl Pts',(4.16278587381831,5.33511975205231,104.591911731376));
#209481=CARTESIAN_POINT('Ctrl Pts',(4.01614535689419,5.44953762845449,104.600660762029));
#209482=CARTESIAN_POINT('Ctrl Pts',(3.86478496605872,5.55790617568979,104.609409792683));
#209483=CARTESIAN_POINT('Ctrl Pts',(3.70921874694181,5.65985735574099,104.618158823337));
#209484=CARTESIAN_POINT('Ctrl Pts',(3.55365041551934,5.76180992010331,104.626907972786));
#209485=CARTESIAN_POINT('Ctrl Pts',(3.39387638119663,5.857344785846,104.635657122236));
#209486=CARTESIAN_POINT('Ctrl Pts',(3.2304392784885,5.94613749151487,104.644406271686));
#209487=CARTESIAN_POINT('Ctrl Pts',(3.18691767033081,5.96978206963911,104.646736079592));
#209488=CARTESIAN_POINT('Ctrl Pts',(3.14313645900847,5.99294880643102,104.649065887498));
#209489=CARTESIAN_POINT('Ctrl Pts',(3.09910619832133,6.0156321173694,104.651395695404));
#209490=CARTESIAN_POINT('Origin',(0.,0.,4.30282021618968));
#209491=CARTESIAN_POINT('',(3.09910619832138,6.01563211736938,107.045755263024));
#209492=CARTESIAN_POINT('',(3.09910619832136,6.01563211736939,106.651504649108));
#209493=CARTESIAN_POINT('',(3.09910619832133,6.0156321173694,4.30282021618968));
#209494=CARTESIAN_POINT('',(-6.76699890702215,0.00271959186415095,105.69717978381));
#209495=CARTESIAN_POINT('Ctrl Pts',(-6.767,5.0761025263598E-12,105.69717978381));
#209496=CARTESIAN_POINT('Ctrl Pts',(-6.76700000000014,-0.186007249521759,
105.705929295621));
#209497=CARTESIAN_POINT('Ctrl Pts',(-6.75932637294548,-0.372014355744774,
105.714678807432));
#209498=CARTESIAN_POINT('Ctrl Pts',(-6.74400518264223,-0.557389537482324,
105.723428319244));
#209499=CARTESIAN_POINT('Ctrl Pts',(-6.72868405705141,-0.742763936246801,
105.732177794099));
#209500=CARTESIAN_POINT('Ctrl Pts',(-6.70571545645792,-0.927506130237453,
105.740927268955));
#209501=CARTESIAN_POINT('Ctrl Pts',(-6.67517739404878,-1.11098863989697,
105.749676743811));
#209502=CARTESIAN_POINT('Ctrl Pts',(-6.64463945808762,-1.29447038981637,
105.758426182438));
#209503=CARTESIAN_POINT('Ctrl Pts',(-6.60653217008422,-1.47669218313383,
105.767175621065));
#209504=CARTESIAN_POINT('Ctrl Pts',(-6.56098496092751,-1.65703510598994,
105.775925059692));
#209505=CARTESIAN_POINT('Ctrl Pts',(-6.51543793658379,-1.83737729708406,
105.784674462817));
#209506=CARTESIAN_POINT('Ctrl Pts',(-6.46245112167513,-2.0158403551063,
105.793423865942));
#209507=CARTESIAN_POINT('Ctrl Pts',(-6.40220448374356,-2.19181813760493,
105.802173269067));
#209508=CARTESIAN_POINT('Ctrl Pts',(-6.34195808526612,-2.36779522066854,
105.810922637417));
#209509=CARTESIAN_POINT('Ctrl Pts',(-6.27445201433218,-2.54128677683884,
105.819672005767));
#209510=CARTESIAN_POINT('Ctrl Pts',(-6.19991555072021,-2.71170355384539,
105.828421374117));
#209511=CARTESIAN_POINT('Ctrl Pts',(-6.12537937716821,-2.88211966767204,
105.837170708419));
#209512=CARTESIAN_POINT('Ctrl Pts',(-6.04381298052658,-3.04946076371513,
105.845920042721));
#209513=CARTESIAN_POINT('Ctrl Pts',(-5.95549339335978,-3.21315848374275,
105.854669377023));
#209514=CARTESIAN_POINT('Ctrl Pts',(-5.86717414255561,-3.37685558033229,
105.863418678003));
#209515=CARTESIAN_POINT('Ctrl Pts',(-5.77210188876755,-3.53690907646502,
105.872167978983));
#209516=CARTESIAN_POINT('Ctrl Pts',(-5.67059953347156,-3.69277536969041,
105.880917279963));
#209517=CARTESIAN_POINT('Ctrl Pts',(-5.56909755631545,-3.8486410822469,
105.889666548349));
#209518=CARTESIAN_POINT('Ctrl Pts',(-5.46116568197013,-4.00031938297295,
105.898415816734));
#209519=CARTESIAN_POINT('Ctrl Pts',(-5.34717048533766,-4.14729511859644,
105.907165085119));
#209520=CARTESIAN_POINT('Ctrl Pts',(-5.23317570392011,-4.29427031887703,
105.915914321636));
#209521=CARTESIAN_POINT('Ctrl Pts',(-5.11311782003702,-4.43654276189331,
105.924663558153));
#209522=CARTESIAN_POINT('Ctrl Pts',(-4.98740458984954,-4.57362924351634,
105.93341279467));
#209523=CARTESIAN_POINT('Ctrl Pts',(-4.86169180711956,-4.71071523720047,
105.942162000046));
#209524=CARTESIAN_POINT('Ctrl Pts',(-4.73032391204397,-4.84261509523018,
105.950911205421));
#209525=CARTESIAN_POINT('Ctrl Pts',(-4.59374707013837,-4.9688808453811,
105.959660410797));
#209526=CARTESIAN_POINT('Ctrl Pts',(-4.45717070301705,-5.09514615659236,
105.968409585757));
#209527=CARTESIAN_POINT('Ctrl Pts',(-4.31538563571323,-5.21577720459293,
105.977158760717));
#209528=CARTESIAN_POINT('Ctrl Pts',(-4.16887341029814,-5.33036429232648,
105.985907935678));
#209529=CARTESIAN_POINT('Ctrl Pts',(-4.02236168204012,-5.4449509912339,
105.99465708095));
#209530=CARTESIAN_POINT('Ctrl Pts',(-3.87112305348471,-5.55349359438389,
106.003406226222));
#209531=CARTESIAN_POINT('Ctrl Pts',(-3.71567117018065,-5.65562346298694,
106.012155371494));
#209532=CARTESIAN_POINT('Ctrl Pts',(-3.56021980146119,-5.75775299351459,
106.020904487804));
#209533=CARTESIAN_POINT('Ctrl Pts',(-3.40055544538645,-5.85346967463701,
106.029653604114));
#209534=CARTESIAN_POINT('Ctrl Pts',(-3.23722035987143,-5.94244842986743,
106.038402720425));
#209535=CARTESIAN_POINT('Ctrl Pts',(-3.07388580147449,-6.03142689794393,
106.047151808499));
#209536=CARTESIAN_POINT('Ctrl Pts',(-2.90688078896824,-6.11366734656666,
106.055900896574));
#209537=CARTESIAN_POINT('Ctrl Pts',(-2.73677250721591,-6.18889046952256,
106.064649984649));
#209538=CARTESIAN_POINT('Ctrl Pts',(-2.56666476031699,-6.26411335596239,
106.073399045215));
#209539=CARTESIAN_POINT('Ctrl Pts',(-2.39345402575377,-6.33231884500476,
106.082148105781));
#209540=CARTESIAN_POINT('Ctrl Pts',(-2.21772856065797,-6.39327529762656,
106.090897166347));
#209541=CARTESIAN_POINT('Ctrl Pts',(-2.04200363348683,-6.45423156365059,
106.099646200131));
#209542=CARTESIAN_POINT('Ctrl Pts',(-1.8637642618941,-6.50793874375622,
106.108395233915));
#209543=CARTESIAN_POINT('Ctrl Pts',(-1.68361577753247,-6.55421443909518,
106.117144267698));
#209544=CARTESIAN_POINT('Ctrl Pts',(-1.50346782967897,-6.60048999661846,
106.125893275426));
#209545=CARTESIAN_POINT('Ctrl Pts',(-1.32141105795088,-6.63933404237692,
106.134642283154));
#209546=CARTESIAN_POINT('Ctrl Pts',(-1.13806375487127,-6.67061465607543,
106.143391290882));
#209547=CARTESIAN_POINT('Ctrl Pts',(-0.954716982603977,-6.70189517921283,
106.15214027328));
#209548=CARTESIAN_POINT('Ctrl Pts',(-0.770079968903007,-6.72561226592218,
106.160889255679));
#209549=CARTESIAN_POINT('Ctrl Pts',(-0.584779765559023,-6.74168536983096,
106.169638238077));
#209550=CARTESIAN_POINT('Ctrl Pts',(-0.391489830652104,-6.75845151013848,
106.178764457087));
#209551=CARTESIAN_POINT('Ctrl Pts',(-0.197478578239171,-6.76689983031623,
106.187890676097));
#209552=CARTESIAN_POINT('Ctrl Pts',(-0.00346287645220683,-6.76699911397118,
106.197016895107));
#209553=CARTESIAN_POINT('Ctrl Pts',(0.184489834653883,-6.76709529501191,
106.205857919772));
#209554=CARTESIAN_POINT('Ctrl Pts',(0.372446404249327,-6.75935639738168,
106.214698944438));
#209555=CARTESIAN_POINT('Ctrl Pts',(0.559755019488257,-6.74380925873187,
106.223539969104));
#209556=CARTESIAN_POINT('Ctrl Pts',(0.74513470552165,-6.72842222659807,
106.232289947714));
#209557=CARTESIAN_POINT('Ctrl Pts',(0.9298794312284,-6.70538706057526,106.241039926324));
#209558=CARTESIAN_POINT('Ctrl Pts',(1.11336163626804,-6.67478200894131,
106.249789904933));
#209559=CARTESIAN_POINT('Ctrl Pts',(1.29684196300714,-6.64417727061014,
106.25853979397));
#209560=CARTESIAN_POINT('Ctrl Pts',(1.47905951217522,-6.60600284890588,
106.267289683006));
#209561=CARTESIAN_POINT('Ctrl Pts',(1.65939532067112,-6.56038841607224,
106.276039572043));
#209562=CARTESIAN_POINT('Ctrl Pts',(1.83972934300828,-6.51477443503249,
106.284789374415));
#209563=CARTESIAN_POINT('Ctrl Pts',(2.0181813840629,-6.46172066062133,106.293539176787));
#209564=CARTESIAN_POINT('Ctrl Pts',(2.19414528354225,-6.4014073042347,106.302288979159));
#209565=CARTESIAN_POINT('Ctrl Pts',(2.37010749864023,-6.34109452518633,
106.311038697776));
#209566=CARTESIAN_POINT('Ctrl Pts',(2.54358134866482,-6.27352239616495,
106.319788416392));
#209567=CARTESIAN_POINT('Ctrl Pts',(2.71397759435577,-6.1989204396681,106.328538135008));
#209568=CARTESIAN_POINT('Ctrl Pts',(2.88437226558162,-6.12431917249498,
106.337287772777));
#209569=CARTESIAN_POINT('Ctrl Pts',(3.0516891268101,-6.04268832278772,106.346037410546));
#209570=CARTESIAN_POINT('Ctrl Pts',(3.21535986273924,-5.95430516123296,
106.354787048314));
#209571=CARTESIAN_POINT('Ctrl Pts',(3.37902914072916,-5.86592278697398,
106.363536608144));
#209572=CARTESIAN_POINT('Ctrl Pts',(3.5390521062165,-5.77078835741894,106.372286167973));
#209573=CARTESIAN_POINT('Ctrl Pts',(3.69488522831778,-5.66922500431577,
106.381035727802));
#209574=CARTESIAN_POINT('Ctrl Pts',(3.85071701407023,-5.56766252217036,
106.389785212599));
#209575=CARTESIAN_POINT('Ctrl Pts',(4.0023587882249,-5.45967138329307,106.398534697396));
#209576=CARTESIAN_POINT('Ctrl Pts',(4.14929549611414,-5.34561838199538,
106.407284182193));
#209577=CARTESIAN_POINT('Ctrl Pts',(4.29623099276182,-5.2315663208694,106.416033594866));
#209578=CARTESIAN_POINT('Ctrl Pts',(4.43846127436122,-5.11145267304882,
106.424783007538));
#209579=CARTESIAN_POINT('Ctrl Pts',(4.57550326054539,-4.98568540049796,
106.433532420211));
#209580=CARTESIAN_POINT('Ctrl Pts',(4.71254416257872,-4.85991912290272,
106.442281763666));
#209581=CARTESIAN_POINT('Ctrl Pts',(4.84439664018847,-4.72849950385331,
106.451031107121));
#209582=CARTESIAN_POINT('Ctrl Pts',(4.97061286794825,-4.59187289860981,
106.459780450577));
#209583=CARTESIAN_POINT('Ctrl Pts',(5.09682813912764,-4.45524732884594,
106.468529727721));
#209584=CARTESIAN_POINT('Ctrl Pts',(5.21740705147918,-4.31341506235692,
106.477279004866));
#209585=CARTESIAN_POINT('Ctrl Pts',(5.33194007545775,-4.16685781275623,
106.486028282011));
#209586=CARTESIAN_POINT('Ctrl Pts',(5.44647226944556,-4.02030162521746,
106.494777495752));
#209587=CARTESIAN_POINT('Ctrl Pts',(5.55495848628176,-3.86902074887843,
106.503526709493));
#209588=CARTESIAN_POINT('Ctrl Pts',(5.65703027291843,-3.71352898080578,
106.512275923234));
#209589=CARTESIAN_POINT('Ctrl Pts',(5.75910135377042,-3.55803828789515,
106.521025076478));
#209590=CARTESIAN_POINT('Ctrl Pts',(5.85475793592787,-3.39833700106652,
106.529774229722));
#209591=CARTESIAN_POINT('Ctrl Pts',(5.94367514427424,-3.23496750823506,
106.538523382966));
#209592=CARTESIAN_POINT('Ctrl Pts',(6.03259176732663,-3.0715990907768,106.547272478619));
#209593=CARTESIAN_POINT('Ctrl Pts',(6.11476896835944,-2.90456276731392,
106.556021574272));
#209594=CARTESIAN_POINT('Ctrl Pts',(6.18992765547904,-2.7344258300301,106.564770669925));
#209595=CARTESIAN_POINT('Ctrl Pts',(6.26508587283073,-2.56428995616123,
106.573519710893));
#209596=CARTESIAN_POINT('Ctrl Pts',(6.33322554827181,-2.39105376935148,
106.582268751861));
#209597=CARTESIAN_POINT('Ctrl Pts',(6.39411526733052,-2.21530561054019,
106.591017792829));
#209598=CARTESIAN_POINT('Ctrl Pts',(6.4550046260286,-2.03955849185057,106.599766782018));
#209599=CARTESIAN_POINT('Ctrl Pts',(6.50864402040746,-1.86129970164524,
106.608515771207));
#209600=CARTESIAN_POINT('Ctrl Pts',(6.55485128368601,-1.6811346313606,106.617264760396));
#209601=CARTESIAN_POINT('Ctrl Pts',(6.60199809554324,-1.49730620116879,
106.626191645867));
#209602=CARTESIAN_POINT('Ctrl Pts',(6.64140720707869,-1.31149343245718,
106.635118531339));
#209603=CARTESIAN_POINT('Ctrl Pts',(6.67293928722879,-1.12435326697554,
106.64404541681));
#209604=CARTESIAN_POINT('Ctrl Pts',(6.70384625876252,-0.940923067006904,
106.652795330988));
#209605=CARTESIAN_POINT('Ctrl Pts',(6.72718554579792,-0.756217899522007,
106.661545245165));
#209606=CARTESIAN_POINT('Ctrl Pts',(6.74287786815325,-0.570865181254865,
106.670295159343));
#209607=CARTESIAN_POINT('Ctrl Pts',(6.75856988190843,-0.385516108074387,
106.679044901447));
#209608=CARTESIAN_POINT('Ctrl Pts',(6.76661520773401,-0.199519795226859,
106.687794643552));
#209609=CARTESIAN_POINT('Ctrl Pts',(6.76698651789579,-0.0135080204562311,
106.696544385656));
#209610=CARTESIAN_POINT('Ctrl Pts',(6.76735782124904,0.172500343512306,
106.705293967321));
#209611=CARTESIAN_POINT('Ctrl Pts',(6.76005538995187,0.358523882210194,
106.714043548986));
#209612=CARTESIAN_POINT('Ctrl Pts',(6.74510402742368,0.54393074856358,106.722793130651));
#209613=CARTESIAN_POINT('Ctrl Pts',(6.73015291918039,0.729334461614436,
106.731542563508));
#209614=CARTESIAN_POINT('Ctrl Pts',(6.70755316306606,0.91412123763388,106.740291996364));
#209615=CARTESIAN_POINT('Ctrl Pts',(6.67738151874587,1.09766345166042,106.749041429221));
#209616=CARTESIAN_POINT('Ctrl Pts',(6.64721034747585,1.28120278799584,106.757790724899));
#209617=CARTESIAN_POINT('Ctrl Pts',(6.60946757205159,1.46349731860249,106.766540020576));
#209618=CARTESIAN_POINT('Ctrl Pts',(6.56428138111543,1.64392790278083,106.775289316254));
#209619=CARTESIAN_POINT('Ctrl Pts',(6.51909583859873,1.82435589778973,106.784038486379));
#209620=CARTESIAN_POINT('Ctrl Pts',(6.46646716392902,2.00291972192179,106.792787656505));
#209621=CARTESIAN_POINT('Ctrl Pts',(6.40657409872914,2.17901292274575,106.80153682663));
#209622=CARTESIAN_POINT('Ctrl Pts',(6.3466818134211,2.35510383058887,106.810285882829));
#209623=CARTESIAN_POINT('Ctrl Pts',(6.27952541914087,2.52872390822489,106.819034939029));
#209624=CARTESIAN_POINT('Ctrl Pts',(6.20533299175557,2.69928350890193,106.827783995228));
#209625=CARTESIAN_POINT('Ctrl Pts',(6.12831602991588,2.87633637965541,106.836866131386));
#209626=CARTESIAN_POINT('Ctrl Pts',(6.04371690605307,3.0500908660139,106.845948267544));
#209627=CARTESIAN_POINT('Ctrl Pts',(5.95184520316665,3.21991112882672,106.855030403702));
#209628=CARTESIAN_POINT('Ctrl Pts',(5.86333549509308,3.38351691182958,106.863780184046));
#209629=CARTESIAN_POINT('Ctrl Pts',(5.76807618099402,3.54347103711949,106.872529964389));
#209630=CARTESIAN_POINT('Ctrl Pts',(5.66639083309049,3.69923018027644,106.881279744733));
#209631=CARTESIAN_POINT('Ctrl Pts',(5.56470914082232,3.85498372382004,106.890029210518));
#209632=CARTESIAN_POINT('Ctrl Pts',(5.45660203372097,4.00654234701958,106.898778676303));
#209633=CARTESIAN_POINT('Ctrl Pts',(5.34243669839244,4.15339127986634,106.907528142088));
#209634=CARTESIAN_POINT('Ctrl Pts',(5.22827486050622,4.30023571401242,106.916277339834));
#209635=CARTESIAN_POINT('Ctrl Pts',(5.10805534167145,4.4423705202843,106.92502653758));
#209636=CARTESIAN_POINT('Ctrl Pts',(4.98218644339989,4.5793129662868,106.933775735326));
#209637=CARTESIAN_POINT('Ctrl Pts',(4.8563207321964,4.71625194483304,106.942524711537));
#209638=CARTESIAN_POINT('Ctrl Pts',(4.7248061217039,4.84799861524438,106.951273687749));
#209639=CARTESIAN_POINT('Ctrl Pts',(4.58808925235401,4.97410554898402,106.960022663961));
#209640=CARTESIAN_POINT('Ctrl Pts',(4.45136349474143,5.10022068121123,106.968772208962));
#209641=CARTESIAN_POINT('Ctrl Pts',(4.30943501210181,5.22069514871751,106.977521753964));
#209642=CARTESIAN_POINT('Ctrl Pts',(4.16278587431888,5.33511975166174,106.986271298966));
#209643=CARTESIAN_POINT('Ctrl Pts',(4.01614535740551,5.44953762807766,106.995020329619));
#209644=CARTESIAN_POINT('Ctrl Pts',(3.86478496658024,5.55790617532714,107.003769360273));
#209645=CARTESIAN_POINT('Ctrl Pts',(3.70921874747293,5.65985735539292,107.012518390927));
#209646=CARTESIAN_POINT('Ctrl Pts',(3.55365041605993,5.76180991976989,107.021267540377));
#209647=CARTESIAN_POINT('Ctrl Pts',(3.39387638174611,5.85734478552762,107.030016689826));
#209648=CARTESIAN_POINT('Ctrl Pts',(3.23043927904622,5.94613749121187,107.038765839276));
#209649=CARTESIAN_POINT('Ctrl Pts',(3.18691767070485,5.96978206944118,107.041095647192));
#209650=CARTESIAN_POINT('Ctrl Pts',(3.14313645919658,5.99294880633411,107.043425455108));
#209651=CARTESIAN_POINT('Ctrl Pts',(3.09910619832137,6.01563211736938,107.045755263024));
#209652=CARTESIAN_POINT('Ctrl Pts',(3.09910619832126,6.01563211736944,105.045908754666));
#209653=CARTESIAN_POINT('Ctrl Pts',(2.93603787272548,6.09964092122308,105.054529422988));
#209654=CARTESIAN_POINT('Ctrl Pts',(2.76947833120977,6.17705310480651,105.063150091309));
#209655=CARTESIAN_POINT('Ctrl Pts',(2.59997745762146,6.24759203372469,105.071770759631));
#209656=CARTESIAN_POINT('Ctrl Pts',(2.4382529009184,6.31489479605329,105.079995931179));
#209657=CARTESIAN_POINT('Ctrl Pts',(2.2738510884678,6.37594069435382,105.088221102727));
#209658=CARTESIAN_POINT('Ctrl Pts',(2.10726897706669,6.43052925180287,105.096446274275));
#209659=CARTESIAN_POINT('Ctrl Pts',(1.9366406840343,6.48644373324562,105.104871230408));
#209660=CARTESIAN_POINT('Ctrl Pts',(1.76379950164895,6.53555832413088,105.113296186541));
#209661=CARTESIAN_POINT('Ctrl Pts',(1.58931484550919,6.57771748571221,105.121721142675));
#209662=CARTESIAN_POINT('Ctrl Pts',(1.41478968980506,6.61988643283982,105.130148054321));
#209663=CARTESIAN_POINT('Ctrl Pts',(1.23862062209066,6.655096653863,105.138574965967));
#209664=CARTESIAN_POINT('Ctrl Pts',(1.0613883661554,6.68324350418193,105.147001877614));
#209665=CARTESIAN_POINT('Ctrl Pts',(0.884090935017014,6.71140070519395,
105.155431888164));
#209666=CARTESIAN_POINT('Ctrl Pts',(0.705729863433054,6.73248930439252,
105.163861898714));
#209667=CARTESIAN_POINT('Ctrl Pts',(0.526892519575836,6.74645634928553,
105.172291909264));
#209668=CARTESIAN_POINT('Ctrl Pts',(0.347890434496955,6.76043626032824,
105.180729685363));
#209669=CARTESIAN_POINT('Ctrl Pts',(0.168411531428975,6.76728148447363,
105.189167461463));
#209670=CARTESIAN_POINT('Ctrl Pts',(-0.0109541556863898,6.76699113391419,
105.197605237562));
#209671=CARTESIAN_POINT('Ctrl Pts',(-0.190413996565524,6.76670063094211,
105.206047442872));
#209672=CARTESIAN_POINT('Ctrl Pts',(-0.369760171767688,6.75926709135523,
105.214489648182));
#209673=CARTESIAN_POINT('Ctrl Pts',(-0.548405656251683,6.74474167305103,
105.222931853492));
#209674=CARTESIAN_POINT('Ctrl Pts',(-0.727239601892981,6.73020093122968,
105.231382964864));
#209675=CARTESIAN_POINT('Ctrl Pts',(-0.905371050717434,6.70855340028196,
105.239834076236));
#209676=CARTESIAN_POINT('Ctrl Pts',(-1.08222000645191,6.67990185988052,
105.248285187608));
#209677=CARTESIAN_POINT('Ctrl Pts',(-1.13185293981417,6.67186076068622,
105.250657005105));
#209678=CARTESIAN_POINT('Ctrl Pts',(-1.18138492736455,6.66326829616464,
105.253028822602));
#209679=CARTESIAN_POINT('Ctrl Pts',(-1.23080332752517,6.65412745361501,
105.2554006401));
#209680=CARTESIAN_POINT('Ctrl Pts',(-1.40407841213977,6.62207703795834,
105.263716912504));
#209681=CARTESIAN_POINT('Ctrl Pts',(-1.5762688014823,6.58322310852279,105.272033184908));
#209682=CARTESIAN_POINT('Ctrl Pts',(-1.74681042239048,6.53765572267522,
105.280349457312));
#209683=CARTESIAN_POINT('Ctrl Pts',(-1.91720785015746,6.492126864106,105.288658698298));
#209684=CARTESIAN_POINT('Ctrl Pts',(-2.08595895246826,6.43989594763906,
105.296967939284));
#209685=CARTESIAN_POINT('Ctrl Pts',(-2.25250951445243,6.38110412760216,
105.30527718027));
#209686=CARTESIAN_POINT('Ctrl Pts',(-2.41894979418782,6.32235123684922,
105.313580919252));
#209687=CARTESIAN_POINT('Ctrl Pts',(-2.58319211002671,6.25704621452549,
105.321884658235));
#209688=CARTESIAN_POINT('Ctrl Pts',(-2.74469687365095,6.18538018813482,
105.330188397217));
#209689=CARTESIAN_POINT('Ctrl Pts',(-2.9061242942684,6.11374848188333,105.338488159623));
#209690=CARTESIAN_POINT('Ctrl Pts',(-3.06481645794534,6.0357619831874,105.346787922028));
#209691=CARTESIAN_POINT('Ctrl Pts',(-3.22025304185457,5.95166021765578,
105.355087684434));
#209692=CARTESIAN_POINT('Ctrl Pts',(-3.37564366520775,5.86758331991146,
105.363384992708));
#209693=CARTESIAN_POINT('Ctrl Pts',(-3.52778032193459,5.77739492497551,
105.371682300983));
#209694=CARTESIAN_POINT('Ctrl Pts',(-3.6761664216275,5.68138094484945,105.379979609258));
#209695=CARTESIAN_POINT('Ctrl Pts',(-3.82456751358164,5.58535726390455,
105.388277755855));
#209696=CARTESIAN_POINT('Ctrl Pts',(-3.96921699511729,5.48350700435032,
105.396575902452));
#209697=CARTESIAN_POINT('Ctrl Pts',(-4.10964596501876,5.37616025079285,
105.404874049049));
#209698=CARTESIAN_POINT('Ctrl Pts',(-4.2500890559367,5.26880270284391,105.413173030077));
#209699=CARTESIAN_POINT('Ctrl Pts',(-4.386310512387,5.15594777022021,105.421472011105));
#209700=CARTESIAN_POINT('Ctrl Pts',(-4.51787341058359,5.03796673728021,
105.429770992133));
#209701=CARTESIAN_POINT('Ctrl Pts',(-4.64947140252216,4.91995423349254,
105.438072186873));
#209702=CARTESIAN_POINT('Ctrl Pts',(-4.77640810036555,4.79681313647768,
105.446373381613));
#209703=CARTESIAN_POINT('Ctrl Pts',(-4.89828230214976,4.66895271859187,
105.454674576352));
#209704=CARTESIAN_POINT('Ctrl Pts',(-5.02020926976148,4.54103694312705,
105.462979365121));
#209705=CARTESIAN_POINT('Ctrl Pts',(-5.13706913301943,4.40839802634082,
105.471284153889));
#209706=CARTESIAN_POINT('Ctrl Pts',(-5.24849982706175,4.27147966931049,
105.479588942658));
#209707=CARTESIAN_POINT('Ctrl Pts',(-5.36006262119077,4.13439899679795,
105.487903576679));
#209708=CARTESIAN_POINT('Ctrl Pts',(-5.46618316670318,3.99302901800606,
105.4962182107));
#209709=CARTESIAN_POINT('Ctrl Pts',(-5.56654103991165,3.84784483197794,
105.504532844721));
#209710=CARTESIAN_POINT('Ctrl Pts',(-5.66696237029346,3.70256884470132,
105.512852736158));
#209711=CARTESIAN_POINT('Ctrl Pts',(-5.76161357549936,3.55347413394155,
105.521172627596));
#209712=CARTESIAN_POINT('Ctrl Pts',(-5.85021929934244,3.40106206200376,
105.529492519034));
#209713=CARTESIAN_POINT('Ctrl Pts',(-5.93895751747274,3.24842208459938,
105.537824851407));
#209714=CARTESIAN_POINT('Ctrl Pts',(-6.0216320250837,3.09245513978424,105.54615718378));
#209715=CARTESIAN_POINT('Ctrl Pts',(-6.0980142825194,2.9336855336231,105.554489516154));
#209716=CARTESIAN_POINT('Ctrl Pts',(-6.1555213121882,2.81415033319126,105.560762801352));
#209717=CARTESIAN_POINT('Ctrl Pts',(-6.20946265235995,2.69302694323137,
105.567036086551));
#209718=CARTESIAN_POINT('Ctrl Pts',(-6.25975931743687,2.5705451343562,105.573309371749));
#209719=CARTESIAN_POINT('Ctrl Pts',(-6.33159816989002,2.39560406057879,
105.582269520679));
#209720=CARTESIAN_POINT('Ctrl Pts',(-6.3961918499594,2.21742488974813,105.591229669609));
#209721=CARTESIAN_POINT('Ctrl Pts',(-6.45325885736035,2.03659989195232,
105.600189818539));
#209722=CARTESIAN_POINT('Ctrl Pts',(-6.51007255865339,1.85657753088988,
105.609110195619));
#209723=CARTESIAN_POINT('Ctrl Pts',(-6.55942612505177,1.67393299626588,
105.618030572699));
#209724=CARTESIAN_POINT('Ctrl Pts',(-6.60108670157509,1.48927611888747,
105.626950949779));
#209725=CARTESIAN_POINT('Ctrl Pts',(-6.64263461531691,1.30511860947664,
105.635847203465));
#209726=CARTESIAN_POINT('Ctrl Pts',(-6.67653095978652,1.11895984650007,
105.644743457152));
#209727=CARTESIAN_POINT('Ctrl Pts',(-6.70259152190307,0.931426803626106,
105.653639710838));
#209728=CARTESIAN_POINT('Ctrl Pts',(-6.72854166544343,0.74468833807128,
105.662498271106));
#209729=CARTESIAN_POINT('Ctrl Pts',(-6.74672218185817,0.556587447153096,
105.671356831374));
#209730=CARTESIAN_POINT('Ctrl Pts',(-6.75699935893056,0.367761693780166,
105.680215391642));
#209731=CARTESIAN_POINT('Ctrl Pts',(-6.76355972001835,0.247226150208622,
105.685870189032));
#209732=CARTESIAN_POINT('Ctrl Pts',(-6.7669005915834,0.126395601807584,
105.691524986421));
#209733=CARTESIAN_POINT('Ctrl Pts',(-6.76699781404431,0.0054391837232258,
105.69717978381));
#209734=CARTESIAN_POINT('',(-6.76699999713954,0.000196757566297466,105.302810960999));
#209735=CARTESIAN_POINT('Ctrl Pts',(3.09910619832133,6.0156321173694,104.651395695404));
#209736=CARTESIAN_POINT('Ctrl Pts',(2.93375330812867,6.10081787289904,104.660145143281));
#209737=CARTESIAN_POINT('Ctrl Pts',(2.76488627941195,6.17918206991506,104.668894591158));
#209738=CARTESIAN_POINT('Ctrl Pts',(2.5930786679645,6.25045854491872,104.677644039035));
#209739=CARTESIAN_POINT('Ctrl Pts',(2.42127244384742,6.32173444437152,104.686393416261));
#209740=CARTESIAN_POINT('Ctrl Pts',(2.24652594922919,6.38592262652219,104.695142793487));
#209741=CARTESIAN_POINT('Ctrl Pts',(2.0694326998963,6.44280508013396,104.703892170713));
#209742=CARTESIAN_POINT('Ctrl Pts',(1.89234082174572,6.49968709332118,104.712641480195));
#209743=CARTESIAN_POINT('Ctrl Pts',(1.7129024980898,6.5492634035263,104.721390789677));
#209744=CARTESIAN_POINT('Ctrl Pts',(1.5317271707976,6.59136563044718,104.730140099159));
#209745=CARTESIAN_POINT('Ctrl Pts',(1.35055318611214,6.63346754536789,104.738889343804));
#209746=CARTESIAN_POINT('Ctrl Pts',(1.1676425026785,6.6680954229754,104.747638588448));
#209747=CARTESIAN_POINT('Ctrl Pts',(0.983616346643032,6.69513165536098,
104.756387833093));
#209748=CARTESIAN_POINT('Ctrl Pts',(0.79959149321553,6.72216769637369,104.765137015808));
#209749=CARTESIAN_POINT('Ctrl Pts',(0.614451466500017,6.74161215804563,
104.773886198522));
#209750=CARTESIAN_POINT('Ctrl Pts',(0.428825055349143,6.75339900138477,
104.782635381236));
#209751=CARTESIAN_POINT('Ctrl Pts',(0.243199896479616,6.76518576520697,
104.791384504927));
#209752=CARTESIAN_POINT('Ctrl Pts',(0.0570886457120184,6.76931499591632,
104.800133628617));
#209753=CARTESIAN_POINT('Ctrl Pts',(-0.128876618064112,6.76577266964508,
104.808882752307));
#209754=CARTESIAN_POINT('Ctrl Pts',(-0.314840689036212,6.76223036609477,
104.817631819879));
#209755=CARTESIAN_POINT('Ctrl Pts',(-0.500658488404962,6.7510166094889,
104.826380887452));
#209756=CARTESIAN_POINT('Ctrl Pts',(-0.68569894200026,6.73216948397318,
104.835129955024));
#209757=CARTESIAN_POINT('Ctrl Pts',(-0.87073827017588,6.71332247308605,
104.843878969384));
#209758=CARTESIAN_POINT('Ctrl Pts',(-1.05499997698502,6.6868422152278,104.852627983744));
#209759=CARTESIAN_POINT('Ctrl Pts',(-1.23785828066146,6.65281864152314,
104.861376998105));
#209760=CARTESIAN_POINT('Ctrl Pts',(-1.43007008855791,6.61705470583422,
104.870573538998));
#209761=CARTESIAN_POINT('Ctrl Pts',(-1.62073082018146,6.57295557924323,
104.879770079892));
#209762=CARTESIAN_POINT('Ctrl Pts',(-1.80912510111958,6.52068672522297,
104.888966620786));
#209763=CARTESIAN_POINT('Ctrl Pts',(-1.9883717912753,6.47095581494953,104.897716618439));
#209764=CARTESIAN_POINT('Ctrl Pts',(-2.16556660782784,6.41382980803431,
104.906466616092));
#209765=CARTESIAN_POINT('Ctrl Pts',(-2.34010763414595,6.34950275695758,
104.915216613745));
#209766=CARTESIAN_POINT('Ctrl Pts',(-2.51464512074081,6.28517701044495,
104.923966433947));
#209767=CARTESIAN_POINT('Ctrl Pts',(-2.68652865581904,6.21365061114273,
104.932716254148));
#209768=CARTESIAN_POINT('Ctrl Pts',(-2.85517438840589,6.13516651866851,
104.94146607435));
#209769=CARTESIAN_POINT('Ctrl Pts',(-3.02381692500434,6.05668391353847,
104.950215728734));
#209770=CARTESIAN_POINT('Ctrl Pts',(-3.18922152202248,5.97124400003274,
104.958965383119));
#209771=CARTESIAN_POINT('Ctrl Pts',(-3.35082635730161,5.87913698796114,
104.967715037504));
#209772=CARTESIAN_POINT('Ctrl Pts',(-3.51242834481176,5.7870315989814,104.976464537703));
#209773=CARTESIAN_POINT('Ctrl Pts',(-3.67023045556651,5.68825948846204,
104.985214037903));
#209774=CARTESIAN_POINT('Ctrl Pts',(-3.82369670929241,5.58315613925908,
104.993963538103));
#209775=CARTESIAN_POINT('Ctrl Pts',(-3.97716046260951,5.47805450249345,
105.002712895749));
#209776=CARTESIAN_POINT('Ctrl Pts',(-4.12628826381138,5.36662199540506,
105.011462253394));
#209777=CARTESIAN_POINT('Ctrl Pts',(-4.27057361170237,5.24923708999997,
105.020211611039));
#209778=CARTESIAN_POINT('Ctrl Pts',(-4.41485680048839,5.13185394115808,
105.028960837758));
#209779=CARTESIAN_POINT('Ctrl Pts',(-4.5542974586771,5.00851875309314,105.037710064476));
#209780=CARTESIAN_POINT('Ctrl Pts',(-4.68842200087424,4.87965041183468,
105.046459291195));
#209781=CARTESIAN_POINT('Ctrl Pts',(-4.8225447142129,4.75078382776366,105.055208398614));
#209782=CARTESIAN_POINT('Ctrl Pts',(-4.9513512499892,4.61638444000864,105.063957506032));
#209783=CARTESIAN_POINT('Ctrl Pts',(-5.07440415163224,4.47690869975003,
105.07270661345));
#209784=CARTESIAN_POINT('Ctrl Pts',(-5.1974555388563,4.3374346760272,105.081455613193));
#209785=CARTESIAN_POINT('Ctrl Pts',(-5.31475324408513,4.1928846396816,105.090204612936));
#209786=CARTESIAN_POINT('Ctrl Pts',(-5.42589890717437,4.04374950375564,
105.098953612678));
#209787=CARTESIAN_POINT('Ctrl Pts',(-5.53705670790261,3.89459808155823,
105.107703567854));
#209788=CARTESIAN_POINT('Ctrl Pts',(-5.64206095070966,3.74086078755725,
105.116453523029));
#209789=CARTESIAN_POINT('Ctrl Pts',(-5.74055494803381,3.58305984998919,
105.125203478205));
#209790=CARTESIAN_POINT('Ctrl Pts',(-5.83904514247732,3.42526500515924,
105.133953095542));
#209791=CARTESIAN_POINT('Ctrl Pts',(-5.93102544266345,3.26340707389305,
105.142702712879));
#209792=CARTESIAN_POINT('Ctrl Pts',(-6.01618342599591,3.0980358269026,105.151452330216));
#209793=CARTESIAN_POINT('Ctrl Pts',(-6.10133857407737,2.9326700857846,105.160201656243));
#209794=CARTESIAN_POINT('Ctrl Pts',(-6.17967172863313,2.76379151780895,
105.168950982271));
#209795=CARTESIAN_POINT('Ctrl Pts',(-6.25091683900291,2.59197370200198,
105.177700308298));
#209796=CARTESIAN_POINT('Ctrl Pts',(-6.32215995600044,2.42016069349849,
105.186449389527));
#209797=CARTESIAN_POINT('Ctrl Pts',(-6.38631531590723,2.24540886642485,
105.195198470756));
#209798=CARTESIAN_POINT('Ctrl Pts',(-6.44316503369334,2.0683117145613,105.203947551986));
#209799=CARTESIAN_POINT('Ctrl Pts',(-6.50001989046453,1.89119855382987,
105.212697424096));
#209800=CARTESIAN_POINT('Ctrl Pts',(-6.54956769590024,1.71173991694497,
105.221447296207));
#209801=CARTESIAN_POINT('Ctrl Pts',(-6.59164014488978,1.53054539307967,
105.230197168318));
#209802=CARTESIAN_POINT('Ctrl Pts',(-6.63370967316269,1.34936344794161,
105.238946433003));
#209803=CARTESIAN_POINT('Ctrl Pts',(-6.66830481861374,1.16644613613568,
105.247695697688));
#209804=CARTESIAN_POINT('Ctrl Pts',(-6.69530808396591,0.982414709163446,
105.256444962373));
#209805=CARTESIAN_POINT('Ctrl Pts',(-6.72231273474192,0.798373840313651,
105.265194675946));
#209806=CARTESIAN_POINT('Ctrl Pts',(-6.74172468433312,0.61321902549096,
105.273944389519));
#209807=CARTESIAN_POINT('Ctrl Pts',(-6.75347799617534,0.427579180007128,
105.282694103092));
#209808=CARTESIAN_POINT('Ctrl Pts',(-6.76248551786179,0.285308222126213,
105.289399722394));
#209809=CARTESIAN_POINT('Ctrl Pts',(-6.76699585218083,0.142752574305234,
105.296105341697));
#209810=CARTESIAN_POINT('Ctrl Pts',(-6.76699999713954,0.000196757566300471,
105.302810960999));
#209811=CARTESIAN_POINT('Ctrl Pts',(-6.76699999690187,0.00020476833760498,
105.302983892799));
#209812=CARTESIAN_POINT('Ctrl Pts',(-6.76700511243132,-0.168848651656523,
105.310950501476));
#209813=CARTESIAN_POINT('Ctrl Pts',(-6.76067096858633,-0.338125069321827,
105.318917110153));
#209814=CARTESIAN_POINT('Ctrl Pts',(-6.74797342414344,-0.507093351419459,
105.32688371883));
#209815=CARTESIAN_POINT('Ctrl Pts',(-6.73528508990087,-0.675939071888637,
105.334844548905));
#209816=CARTESIAN_POINT('Ctrl Pts',(-6.7162425649944,-0.844476722711796,
105.34280537898));
#209817=CARTESIAN_POINT('Ctrl Pts',(-6.69087376521969,-1.01217451948514,
105.350766209054));
#209818=CARTESIAN_POINT('Ctrl Pts',(-6.6655172193102,-1.17979131336441,
105.358723193817));
#209819=CARTESIAN_POINT('Ctrl Pts',(-6.63384053379525,-1.34656868357456,
105.36668017858));
#209820=CARTESIAN_POINT('Ctrl Pts',(-6.5959235073992,-1.51197952517176,
105.374637163343));
#209821=CARTESIAN_POINT('Ctrl Pts',(-6.55801769950983,-1.67734142668037,
105.382591793874));
#209822=CARTESIAN_POINT('Ctrl Pts',(-6.51387531155373,-1.84133723257834,
105.390546424405));
#209823=CARTESIAN_POINT('Ctrl Pts',(-6.46362727444644,-2.0034498888248,
105.398501054936));
#209824=CARTESIAN_POINT('Ctrl Pts',(-6.41337338753906,-2.16558141798025,
105.406456611532));
#209825=CARTESIAN_POINT('Ctrl Pts',(-6.35701253929677,-2.32582899297134,
105.414412168129));
#209826=CARTESIAN_POINT('Ctrl Pts',(-6.29472559629214,-2.48369053373898,
105.422367724726));
#209827=CARTESIAN_POINT('Ctrl Pts',(-6.25125037920287,-2.59387517957091,
105.427920566677));
#209828=CARTESIAN_POINT('Ctrl Pts',(-6.20488913351062,-2.70289770984355,
105.433473408628));
#209829=CARTESIAN_POINT('Ctrl Pts',(-6.15571725662235,-2.81059318588119,
105.439026250579));
#209830=CARTESIAN_POINT('Ctrl Pts',(-6.07615768892623,-2.98484330726363,
105.448010689104));
#209831=CARTESIAN_POINT('Ctrl Pts',(-5.98926326254738,-3.15556498263556,
105.45699512763));
#209832=CARTESIAN_POINT('Ctrl Pts',(-5.89537231653845,-3.32217914167675,
105.465979566156));
#209833=CARTESIAN_POINT('Ctrl Pts',(-5.80131932036034,-3.48908086681252,
105.474979511286));
#209834=CARTESIAN_POINT('Ctrl Pts',(-5.70024578606546,-3.65186069775247,
105.483979456417));
#209835=CARTESIAN_POINT('Ctrl Pts',(-5.59253402486987,-3.80996747763979,
105.492979401547));
#209836=CARTESIAN_POINT('Ctrl Pts',(-5.48456843814425,-3.96844684021222,
105.502000555279));
#209837=CARTESIAN_POINT('Ctrl Pts',(-5.36993346019752,-4.12223091989116,
105.511021709011));
#209838=CARTESIAN_POINT('Ctrl Pts',(-5.24905414884304,-4.2707984666235,
105.520042862744));
#209839=CARTESIAN_POINT('Ctrl Pts',(-5.12805184183638,-4.41951718200579,
105.529073195571));
#209840=CARTESIAN_POINT('Ctrl Pts',(-5.00079266370581,-4.56300857922963,
105.538103528398));
#209841=CARTESIAN_POINT('Ctrl Pts',(-4.86774051267167,-4.7007862428848,
105.547133861225));
#209842=CARTESIAN_POINT('Ctrl Pts',(-4.73449973562801,-4.8387592318368,
105.556176996218));
#209843=CARTESIAN_POINT('Ctrl Pts',(-4.5954497304539,-4.971002118546,105.56522013121));
#209844=CARTESIAN_POINT('Ctrl Pts',(-4.45109131661908,-5.09706534106815,
105.574263266203));
#209845=CARTESIAN_POINT('Ctrl Pts',(-4.32488880469304,-5.20727364082124,
105.582169049603));
#209846=CARTESIAN_POINT('Ctrl Pts',(-4.19462979517459,-5.31275948396984,
105.590074833003));
#209847=CARTESIAN_POINT('Ctrl Pts',(-4.06066906516676,-5.41324816937093,
105.597980616403));
#209848=CARTESIAN_POINT('Ctrl Pts',(-3.91404043325983,-5.52323949639361,
105.606634004631));
#209849=CARTESIAN_POINT('Ctrl Pts',(-3.76284656150001,-5.6273400054027,
105.61528739286));
#209850=CARTESIAN_POINT('Ctrl Pts',(-3.60757784903758,-5.72517869268143,
105.623940781088));
#209851=CARTESIAN_POINT('Ctrl Pts',(-3.45245253824524,-5.82292701899217,
105.632586177298));
#209852=CARTESIAN_POINT('Ctrl Pts',(-3.2932601492652,-5.91442489684805,
105.641231573509));
#209853=CARTESIAN_POINT('Ctrl Pts',(-3.13052099310498,-5.99934390677256,
105.649876969719));
#209854=CARTESIAN_POINT('Ctrl Pts',(-2.96258449650236,-6.08697494381471,
105.658798470762));
#209855=CARTESIAN_POINT('Ctrl Pts',(-2.79087119428749,-6.16759974134333,
105.667719971804));
#209856=CARTESIAN_POINT('Ctrl Pts',(-2.6159836391453,-6.2409068731815,105.676641472846));
#209857=CARTESIAN_POINT('Ctrl Pts',(-2.44683132678979,-6.31180997919437,
105.685270403188));
#209858=CARTESIAN_POINT('Ctrl Pts',(-2.27470995381919,-6.37586761055618,
105.69389933353));
#209859=CARTESIAN_POINT('Ctrl Pts',(-2.1001885551175,-6.43284517402319,
105.702528263872));
#209860=CARTESIAN_POINT('Ctrl Pts',(-1.91679122756421,-6.49272054144567,
105.711596050265));
#209861=CARTESIAN_POINT('Ctrl Pts',(-1.73074368961585,-6.54477675029657,
105.720663836658));
#209862=CARTESIAN_POINT('Ctrl Pts',(-1.54272919699996,-6.58879925515445,
105.72973162305));
#209863=CARTESIAN_POINT('Ctrl Pts',(-1.35471470438408,-6.63282176001234,
105.738799409443));
#209864=CARTESIAN_POINT('Ctrl Pts',(-1.16473362930391,-6.66881043757078,
105.747867195835));
#209865=CARTESIAN_POINT('Ctrl Pts',(-0.97348730648406,-6.69661193919092,
105.756934982228));
#209866=CARTESIAN_POINT('Ctrl Pts',(-0.795798749362242,-6.72244254673341,
105.765359938361));
#209867=CARTESIAN_POINT('Ctrl Pts',(-0.617095979185703,-6.74119454122236,
105.773784894494));
#209868=CARTESIAN_POINT('Ctrl Pts',(-0.437966647770672,-6.75281231898537,
105.782209850627));
#209869=CARTESIAN_POINT('Ctrl Pts',(-0.258795738717023,-6.7644327933462,
105.790636762274));
#209870=CARTESIAN_POINT('Ctrl Pts',(-0.0791984019269233,-6.76891572785916,
105.79906367392));
#209871=CARTESIAN_POINT('Ctrl Pts',(0.100235296339718,-6.76625759821245,
105.807490585567));
#209872=CARTESIAN_POINT('Ctrl Pts',(0.279734979366334,-6.76359849106793,
105.815920596117));
#209873=CARTESIAN_POINT('Ctrl Pts',(0.459070572473804,-6.75379308858288,
105.824350606667));
#209874=CARTESIAN_POINT('Ctrl Pts',(0.637654326518938,-6.73688993229604,
105.832780617217));
#209875=CARTESIAN_POINT('Ctrl Pts',(0.816402588182952,-6.71997120517517,
105.841218393316));
#209876=CARTESIAN_POINT('Ctrl Pts',(0.994397296711167,-6.69594169257105,
105.849656169416));
#209877=CARTESIAN_POINT('Ctrl Pts',(1.1710570036539,-6.66490168676127,105.858093945515));
#209878=CARTESIAN_POINT('Ctrl Pts',(1.34780944392092,-6.63384538723643,
105.866536150825));
#209879=CARTESIAN_POINT('Ctrl Pts',(1.52322516012246,-6.59577132020763,
105.874978356135));
#209880=CARTESIAN_POINT('Ctrl Pts',(1.69673459188276,-6.55083053701654,
105.883420561445));
#209881=CARTESIAN_POINT('Ctrl Pts',(1.87042706654646,-6.50584234377199,
105.891871672817));
#209882=CARTESIAN_POINT('Ctrl Pts',(2.04220892088487,-6.45397305443475,
105.900322784189));
#209883=CARTESIAN_POINT('Ctrl Pts',(2.21152637024734,-6.39542337251418,
105.908773895561));
#209884=CARTESIAN_POINT('Ctrl Pts',(2.25904557468133,-6.37899131359052,
105.911145713058));
#209885=CARTESIAN_POINT('Ctrl Pts',(2.30637079135772,-6.3620333625382,105.913517530556));
#209886=CARTESIAN_POINT('Ctrl Pts',(2.35349007810657,-6.34455462993692,
105.915889348053));
#209887=CARTESIAN_POINT('Ctrl Pts',(2.51870381168923,-6.2832691803769,105.924205620457));
#209888=CARTESIAN_POINT('Ctrl Pts',(2.68168238585124,-6.2154669504817,105.932521892861));
#209889=CARTESIAN_POINT('Ctrl Pts',(2.84188552188961,-6.14133337968834,
105.940838165265));
#209890=CARTESIAN_POINT('Ctrl Pts',(3.00195320598697,-6.06726248891677,
105.949147406251));
#209891=CARTESIAN_POINT('Ctrl Pts',(3.15924981314508,-5.98687106809083,
105.957456647237));
#209892=CARTESIAN_POINT('Ctrl Pts',(3.3132535380234,-5.90039320662407,105.965765888223));
#209893=CARTESIAN_POINT('Ctrl Pts',(3.46715528860129,-5.81397260688544,
105.974069627206));
#209894=CARTESIAN_POINT('Ctrl Pts',(3.61776819921841,-5.72147376684853,
105.982373366188));
#209895=CARTESIAN_POINT('Ctrl Pts',(3.76459344286126,-5.62317750119681,
105.990677105171));
#209896=CARTESIAN_POINT('Ctrl Pts',(3.91134837337348,-5.52492830863686,
105.998976867576));
#209897=CARTESIAN_POINT('Ctrl Pts',(4.05431896323696,-5.42088741655098,
106.007276629982));
#209898=CARTESIAN_POINT('Ctrl Pts',(4.19303366394567,-5.31138001775606,
106.015576392387));
#209899=CARTESIAN_POINT('Ctrl Pts',(4.33170734853682,-5.20190499886262,
106.023873700662));
#209900=CARTESIAN_POINT('Ctrl Pts',(4.46612737956734,-5.08696691049196,
106.032171008936));
#209901=CARTESIAN_POINT('Ctrl Pts',(4.59585354289005,-4.96693257577602,
106.040468317211));
#209902=CARTESIAN_POINT('Ctrl Pts',(4.72559281315962,-4.8468861133319,106.048766463808));
#209903=CARTESIAN_POINT('Ctrl Pts',(4.85063700760493,-4.72174260644738,
106.057064610405));
#209904=CARTESIAN_POINT('Ctrl Pts',(4.97058076503971,-4.59190764913857,
106.065362757002));
#209905=CARTESIAN_POINT('Ctrl Pts',(5.09053658357387,-4.46205963610801,
106.073661738031));
#209906=CARTESIAN_POINT('Ctrl Pts',(5.20539070617779,-4.32751948769192,
106.081960719059));
#209907=CARTESIAN_POINT('Ctrl Pts',(5.31477633963618,-4.1887279047037,106.090259700087));
#209908=CARTESIAN_POINT('Ctrl Pts',(5.42419115116262,-4.04989929975816,
106.098560894826));
#209909=CARTESIAN_POINT('Ctrl Pts',(5.52813435078339,-3.90681727333276,
106.106862089566));
#209910=CARTESIAN_POINT('Ctrl Pts',(5.62628085151066,-3.75995382683412,
106.115163284305));
#209911=CARTESIAN_POINT('Ctrl Pts',(5.72446984508069,-3.61302679533455,
106.123468073074));
#209912=CARTESIAN_POINT('Ctrl Pts',(5.81685694465353,-3.46231537002372,
106.131772861842));
#209913=CARTESIAN_POINT('Ctrl Pts',(5.90316152390068,-3.30831876075123,
106.140077650611));
#209914=CARTESIAN_POINT('Ctrl Pts',(5.9895684164515,-3.15413958988138,106.148392284632));
#209915=CARTESIAN_POINT('Ctrl Pts',(6.06987821134061,-2.99666775770691,
106.156706918653));
#209916=CARTESIAN_POINT('Ctrl Pts',(6.143856690237,-2.83642626730011,106.165021552674));
#209917=CARTESIAN_POINT('Ctrl Pts',(6.21788194638141,-2.6760834547784,106.173341444112));
#209918=CARTESIAN_POINT('Ctrl Pts',(6.28556776967601,-2.51296781252368,
106.181661335549));
#209919=CARTESIAN_POINT('Ctrl Pts',(6.34672884497938,-2.34762049068981,
106.189981226987));
#209920=CARTESIAN_POINT('Ctrl Pts',(6.40798137592181,-2.18202592099595,
106.19831355936));
#209921=CARTESIAN_POINT('Ctrl Pts',(6.46268955258892,-2.01419333330978,
106.206645891734));
#209922=CARTESIAN_POINT('Ctrl Pts',(6.51071811699813,-1.84467845463441,
106.214978224107));
#209923=CARTESIAN_POINT('Ctrl Pts',(6.54687808622572,-1.71705330339534,
106.221251509305));
#209924=CARTESIAN_POINT('Ctrl Pts',(6.57925285944496,-1.58847485328167,
106.227524794504));
#209925=CARTESIAN_POINT('Ctrl Pts',(6.6078040171022,-1.45918301510402,106.233798079702));
#209926=CARTESIAN_POINT('Ctrl Pts',(6.64453173443157,-1.2928642219191,106.241867925705));
#209927=CARTESIAN_POINT('Ctrl Pts',(6.67504371885449,-1.12485071678804,
106.249937771707));
#209928=CARTESIAN_POINT('Ctrl Pts',(6.69917958941325,-0.955657798999658,
106.25800761771));
#209929=CARTESIAN_POINT('Ctrl Pts',(6.72328509397694,-0.786677747422023,
106.26606731082));
#209930=CARTESIAN_POINT('Ctrl Pts',(6.74103039415247,-0.616521600289532,
106.27412700393));
#209931=CARTESIAN_POINT('Ctrl Pts',(6.7523050586329,-0.445718964326782,
106.28218669704));
#209932=CARTESIAN_POINT('Ctrl Pts',(6.76356801258344,-0.275093734031229,
106.290238018879));
#209933=CARTESIAN_POINT('Ctrl Pts',(6.76837368089856,-0.103823720276054,
106.298289340717));
#209934=CARTESIAN_POINT('Ctrl Pts',(6.76666281810618,0.0675522468859296,
106.306340662556));
#209935=CARTESIAN_POINT('Ctrl Pts',(6.76495335740821,0.23878776720118,106.314385386137));
#209936=CARTESIAN_POINT('Ctrl Pts',(6.75673799853821,0.410128696927685,
106.322430109718));
#209937=CARTESIAN_POINT('Ctrl Pts',(6.7420093902107,0.581032169772714,106.330474833299));
#209938=CARTESIAN_POINT('Ctrl Pts',(6.7272896282436,0.751832993834989,106.338514725024));
#209939=CARTESIAN_POINT('Ctrl Pts',(6.70606443638829,0.922196513281735,
106.346554616748));
#209940=CARTESIAN_POINT('Ctrl Pts',(6.6783785299524,1.09158106005499,106.354594508472));
#209941=CARTESIAN_POINT('Ctrl Pts',(6.65009647010046,1.26461292017956,106.362807521092));
#209942=CARTESIAN_POINT('Ctrl Pts',(6.61507230951299,1.4366227708902,106.371020533712));
#209943=CARTESIAN_POINT('Ctrl Pts',(6.57340954600896,1.60703949560624,106.379233546332));
#209944=CARTESIAN_POINT('Ctrl Pts',(6.53263921587813,1.77380582462841,106.387270632875));
#209945=CARTESIAN_POINT('Ctrl Pts',(6.48551191000055,1.93904621260604,106.395307719417));
#209946=CARTESIAN_POINT('Ctrl Pts',(6.43217603789486,2.10223700317809,106.40334480596));
#209947=CARTESIAN_POINT('Ctrl Pts',(6.37883506129792,2.26544341186847,106.411382661689));
#209948=CARTESIAN_POINT('Ctrl Pts',(6.31928445129713,2.42659947738446,106.419420517418));
#209949=CARTESIAN_POINT('Ctrl Pts',(6.25372201686337,2.5851982391682,106.427458373147));
#209950=CARTESIAN_POINT('Ctrl Pts',(6.18814031769203,2.74384360330209,106.435498590704));
#209951=CARTESIAN_POINT('Ctrl Pts',(6.11654342058265,2.89992982291108,106.443538808261));
#209952=CARTESIAN_POINT('Ctrl Pts',(6.03917658274562,3.05297153645706,106.451579025818));
#209953=CARTESIAN_POINT('Ctrl Pts',(5.95888677620512,3.21179526399669,106.459923007946));
#209954=CARTESIAN_POINT('Ctrl Pts',(5.87238272970772,3.36733954811179,106.468266990074));
#209955=CARTESIAN_POINT('Ctrl Pts',(5.7799892658019,3.51909265112683,106.476610972201));
#209956=CARTESIAN_POINT('Ctrl Pts',(5.69080441422155,3.66557571818717,106.484665187037));
#209957=CARTESIAN_POINT('Ctrl Pts',(5.59613259808764,3.80852623774655,106.492719401872));
#209958=CARTESIAN_POINT('Ctrl Pts',(5.49630819495313,3.94751633639318,106.500773616707));
#209959=CARTESIAN_POINT('Ctrl Pts',(5.39640908975963,4.08661044614554,106.50883385879));
#209960=CARTESIAN_POINT('Ctrl Pts',(5.29134994779295,4.22173794091867,106.516894100873));
#209961=CARTESIAN_POINT('Ctrl Pts',(5.18150364243719,4.35250606012331,106.524954342956));
#209962=CARTESIAN_POINT('Ctrl Pts',(5.07150376441194,4.48345700212827,106.53302585381));
#209963=CARTESIAN_POINT('Ctrl Pts',(4.95670361835191,4.61003613445532,106.541097364664));
#209964=CARTESIAN_POINT('Ctrl Pts',(4.83751131274927,4.73188897788429,106.549168875519));
#209965=CARTESIAN_POINT('Ctrl Pts',(4.82501871465519,4.7446604281208,106.55001485413));
#209966=CARTESIAN_POINT('Ctrl Pts',(4.8124778957345,4.75737999694354,106.55086083274));
#209967=CARTESIAN_POINT('Ctrl Pts',(4.79988934516451,4.77004730313822,106.551706811351));
#209968=CARTESIAN_POINT('Ctrl Pts',(4.67613620380326,4.89457466039519,106.560023297831));
#209969=CARTESIAN_POINT('Ctrl Pts',(4.54735003171967,5.01446784966951,106.568339784311));
#209970=CARTESIAN_POINT('Ctrl Pts',(4.41391181903876,5.12929541494248,106.57665627079));
#209971=CARTESIAN_POINT('Ctrl Pts',(4.2820334896682,5.24278065406286,106.584875538129));
#209972=CARTESIAN_POINT('Ctrl Pts',(4.14561154969721,5.35131778996561,106.593094805467));
#209973=CARTESIAN_POINT('Ctrl Pts',(4.00505336407265,5.45452441106742,106.601314072806));
#209974=CARTESIAN_POINT('Ctrl Pts',(3.86200135286363,5.55956215506716,106.609679168856));
#209975=CARTESIAN_POINT('Ctrl Pts',(3.71466517784795,5.65907816395306,106.618044264906));
#209976=CARTESIAN_POINT('Ctrl Pts',(3.56351232619173,5.75270970074795,106.626409360957));
#209977=CARTESIAN_POINT('Ctrl Pts',(3.41235947453541,5.84634123754292,106.634774457007));
#209978=CARTESIAN_POINT('Ctrl Pts',(3.25739025212274,5.93408805306152,106.643139553057));
#209979=CARTESIAN_POINT('Ctrl Pts',(3.09910619832136,6.01563211736939,106.651504649108));
#209980=CARTESIAN_POINT('Origin',(0.,0.,4.30282021618968));
#209981=CARTESIAN_POINT('',(3.09910619832136,6.01563211736939,109.045804610872));
#209982=CARTESIAN_POINT('',(3.09910619832125,6.01563211736945,108.651395695404));
#209983=CARTESIAN_POINT('',(3.09910619832133,6.0156321173694,4.30282021618968));
#209984=CARTESIAN_POINT('',(-6.76699852330449,-0.00312165100701077,107.69717978381));
#209985=CARTESIAN_POINT('Ctrl Pts',(-6.76699697141835,-0.00640225076298612,
107.69717978381));
#209986=CARTESIAN_POINT('Ctrl Pts',(-6.7667890499928,-0.226169284123469,
107.707514248948));
#209987=CARTESIAN_POINT('Ctrl Pts',(-6.75587179968307,-0.44545334613587,
107.717848714086));
#209988=CARTESIAN_POINT('Ctrl Pts',(-6.7344074901004,-0.663358694282056,
107.728183179225));
#209989=CARTESIAN_POINT('Ctrl Pts',(-6.71267045783008,-0.884032719052677,
107.738648952714));
#209990=CARTESIAN_POINT('Ctrl Pts',(-6.68011670896827,-1.10329295106132,
107.749114726204));
#209991=CARTESIAN_POINT('Ctrl Pts',(-6.6369625513362,-1.3202337263382,107.759580499694));
#209992=CARTESIAN_POINT('Ctrl Pts',(-6.59330374048131,-1.53971144978907,
107.770168662001));
#209993=CARTESIAN_POINT('Ctrl Pts',(-6.53879512245999,-1.75681535057055,
107.780756824308));
#209994=CARTESIAN_POINT('Ctrl Pts',(-6.47370892271277,-1.9706297937434,
107.791344986615));
#209995=CARTESIAN_POINT('Ctrl Pts',(-6.45869878286014,-2.01993955075795,
107.793786822175));
#209996=CARTESIAN_POINT('Ctrl Pts',(-6.44312627285897,-2.06907444182178,
107.796228657736));
#209997=CARTESIAN_POINT('Ctrl Pts',(-6.42699509465897,-2.11802338354174,
107.798670493296));
#209998=CARTESIAN_POINT('Ctrl Pts',(-6.37368432875604,-2.27979120613193,
107.806740339298));
#209999=CARTESIAN_POINT('Ctrl Pts',(-6.31416349739519,-2.43984366545063,
107.814810185301));
#210000=CARTESIAN_POINT('Ctrl Pts',(-6.24855770860955,-2.5976557820805,
107.822880031304));
#210001=CARTESIAN_POINT('Ctrl Pts',(-6.18303446025095,-2.75526935099468,
107.830939724414));
#210002=CARTESIAN_POINT('Ctrl Pts',(-6.11144162849685,-2.91064784540945,
107.838999417524));
#210003=CARTESIAN_POINT('Ctrl Pts',(-6.03395457703162,-3.0632794783237,
107.847059110634));
#210004=CARTESIAN_POINT('Ctrl Pts',(-5.95654800817668,-3.21575257904456,
107.855110432473));
#210005=CARTESIAN_POINT('Ctrl Pts',(-5.87325957007225,-3.36548416601938,
107.863161754311));
#210006=CARTESIAN_POINT('Ctrl Pts',(-5.7843133500058,-3.51198064757547,
107.87121307615));
#210007=CARTESIAN_POINT('Ctrl Pts',(-5.69544002356877,-3.65835707163808,
107.879257799731));
#210008=CARTESIAN_POINT('Ctrl Pts',(-5.60091833632212,-3.80150334983204,
107.887302523312));
#210009=CARTESIAN_POINT('Ctrl Pts',(-5.50101906065008,-3.9409489078602,
107.895347246893));
#210010=CARTESIAN_POINT('Ctrl Pts',(-5.40117978691283,-4.08031071149452,
107.903387138617));
#210011=CARTESIAN_POINT('Ctrl Pts',(-5.29596957123947,-4.21597591722323,
107.911427030342));
#210012=CARTESIAN_POINT('Ctrl Pts',(-5.18570334754686,-4.34750155735928,
107.919466922066));
#210013=CARTESIAN_POINT('Ctrl Pts',(-5.07306278996375,-4.48185930486589,
107.927679934686));
#210014=CARTESIAN_POINT('Ctrl Pts',(-4.95514622170093,-4.61189685134965,
107.935892947306));
#210015=CARTESIAN_POINT('Ctrl Pts',(-4.83233415631449,-4.73717590994005,
107.944105959926));
#210016=CARTESIAN_POINT('Ctrl Pts',(-4.71215277541851,-4.85977144004019,
107.952143046469));
#210017=CARTESIAN_POINT('Ctrl Pts',(-4.58728378140174,-4.97781000624466,
107.960180133011));
#210018=CARTESIAN_POINT('Ctrl Pts',(-4.45812208332028,-5.09091705787985,
107.968217219554));
#210019=CARTESIAN_POINT('Ctrl Pts',(-4.32894802386315,-5.20403493438633,
107.976255075283));
#210020=CARTESIAN_POINT('Ctrl Pts',(-4.19548072331569,-5.31222011030555,
107.984292931012));
#210021=CARTESIAN_POINT('Ctrl Pts',(-4.05814904835102,-5.41513760687277,
107.992330786741));
#210022=CARTESIAN_POINT('Ctrl Pts',(-3.92077702011585,-5.51808534451568,
108.000371004298));
#210023=CARTESIAN_POINT('Ctrl Pts',(-3.77953865610771,-5.61576209794088,
108.008411221855));
#210024=CARTESIAN_POINT('Ctrl Pts',(-3.63489259999168,-5.70787568071746,
108.016451439412));
#210025=CARTESIAN_POINT('Ctrl Pts',(-3.48478172319846,-5.80346937367002,
108.02479542154));
#210026=CARTESIAN_POINT('Ctrl Pts',(-3.33100101066344,-5.89307108589456,
108.033139403668));
#210027=CARTESIAN_POINT('Ctrl Pts',(-3.17409098904519,-5.97640656191177,
108.041483385795));
#210028=CARTESIAN_POINT('Ctrl Pts',(-3.02263009129439,-6.0568479886727,
108.04953760063));
#210029=CARTESIAN_POINT('Ctrl Pts',(-2.86825394831563,-6.13145100665045,
108.057591815465));
#210030=CARTESIAN_POINT('Ctrl Pts',(-2.71146849668429,-6.20001835412514,
108.0656460303));
#210031=CARTESIAN_POINT('Ctrl Pts',(-2.55456571706835,-6.26863701292117,
108.073706272383));
#210032=CARTESIAN_POINT('Ctrl Pts',(-2.39525038420781,-6.33121087223865,
108.081766514466));
#210033=CARTESIAN_POINT('Ctrl Pts',(-2.23404361549099,-6.38759251393543,
108.089826756549));
#210034=CARTESIAN_POINT('Ctrl Pts',(-2.07261146865362,-6.44405298103477,
108.097898267404));
#210035=CARTESIAN_POINT('Ctrl Pts',(-1.90928296371488,-6.49430384919237,
108.105969778258));
#210036=CARTESIAN_POINT('Ctrl Pts',(-1.74458997759913,-6.53824860417992,
108.114041289112));
#210037=CARTESIAN_POINT('Ctrl Pts',(-1.72732843312179,-6.54285447332258,
108.114887267723));
#210038=CARTESIAN_POINT('Ctrl Pts',(-1.71005190425678,-6.54739111532215,
108.115733246334));
#210039=CARTESIAN_POINT('Ctrl Pts',(-1.69276100624007,-6.55185845205413,
108.116579224945));
#210040=CARTESIAN_POINT('Ctrl Pts',(-1.52456394296557,-6.59531443208769,
108.124808474681));
#210041=CARTESIAN_POINT('Ctrl Pts',(-1.35444527003813,-6.63235326078244,
108.133037724417));
#210042=CARTESIAN_POINT('Ctrl Pts',(-1.1829356770626,-6.66280362789813,
108.141266974153));
#210043=CARTESIAN_POINT('Ctrl Pts',(-1.01163020840378,-6.6932177541233,
108.149486429743));
#210044=CARTESIAN_POINT('Ctrl Pts',(-0.838937465623442,-6.71705897043115,
108.157705885333));
#210045=CARTESIAN_POINT('Ctrl Pts',(-0.665402832443382,-6.73420582330065,
108.165925340923));
#210046=CARTESIAN_POINT('Ctrl Pts',(-0.492039883683817,-6.75133571213568,
108.174136664693));
#210047=CARTESIAN_POINT('Ctrl Pts',(-0.317837057694991,-6.76178439201576,
108.182347988462));
#210048=CARTESIAN_POINT('Ctrl Pts',(-0.14334954881376,-6.76548149852284,
108.190559312232));
#210049=CARTESIAN_POINT('Ctrl Pts',(0.0310003616484347,-6.76917568954324,
108.198764160666));
#210050=CARTESIAN_POINT('Ctrl Pts',(0.205634150909775,-6.76612890415982,
108.2069690091));
#210051=CARTESIAN_POINT('Ctrl Pts',(0.37999179587546,-6.75632261182571,
108.215173857534));
#210052=CARTESIAN_POINT('Ctrl Pts',(0.554246938450867,-6.74652208447199,
108.223373882454));
#210053=CARTESIAN_POINT('Ctrl Pts',(0.72822590300902,-6.7299699864952,108.231573907374));
#210054=CARTESIAN_POINT('Ctrl Pts',(0.901368869000644,-6.70669987117334,
108.239773932294));
#210055=CARTESIAN_POINT('Ctrl Pts',(1.07446172349546,-6.68343649075003,
108.247971583941));
#210056=CARTESIAN_POINT('Ctrl Pts',(1.2467187058382,-6.65345900965552,108.256169235588));
#210057=CARTESIAN_POINT('Ctrl Pts',(1.41758506704369,-6.61685284540126,
108.264366887235));
#210058=CARTESIAN_POINT('Ctrl Pts',(1.58842854819504,-6.580251582937,108.272563441166));
#210059=CARTESIAN_POINT('Ctrl Pts',(1.75788142822436,-6.53702347942953,
108.280759995097));
#210060=CARTESIAN_POINT('Ctrl Pts',(1.92539909317718,-6.48730509009654,
108.288956549028));
#210061=CARTESIAN_POINT('Ctrl Pts',(2.09292478555124,-6.43758431826583,
108.297153495736));
#210062=CARTESIAN_POINT('Ctrl Pts',(2.25851473413512,-6.3813727430211,108.305350442445));
#210063=CARTESIAN_POINT('Ctrl Pts',(2.42163938254588,-6.31885683497441,
108.313547389154));
#210064=CARTESIAN_POINT('Ctrl Pts',(2.58480150809921,-6.25632656418351,
108.321746219074));
#210065=CARTESIAN_POINT('Ctrl Pts',(2.74549687047634,-6.18748920418675,
108.329945048993));
#210066=CARTESIAN_POINT('Ctrl Pts',(2.90321574677204,-6.11257943324215,
108.338143878913));
#210067=CARTESIAN_POINT('Ctrl Pts',(3.06108400300623,-6.03759871316806,
108.346350474173));
#210068=CARTESIAN_POINT('Ctrl Pts',(3.21596981635108,-5.95653424559037,
108.354557069433));
#210069=CARTESIAN_POINT('Ctrl Pts',(3.36738710586005,-5.86966720345264,
108.362763664692));
#210070=CARTESIAN_POINT('Ctrl Pts',(3.51887768220526,-5.78275811716848,
108.370974231991));
#210071=CARTESIAN_POINT('Ctrl Pts',(3.66689608377019,-5.69004104721331,
108.37918479929));
#210072=CARTESIAN_POINT('Ctrl Pts',(3.8109851959247,-5.59184055892537,108.387395366589));
#210073=CARTESIAN_POINT('Ctrl Pts',(3.95527302759268,-5.49350463810569,
108.395617257436));
#210074=CARTESIAN_POINT('Ctrl Pts',(4.09562045136291,-5.38967039883068,
108.403839148283));
#210075=CARTESIAN_POINT('Ctrl Pts',(4.23160246303918,-5.28070351324525,
108.412061039129));
#210076=CARTESIAN_POINT('Ctrl Pts',(4.35524220355758,-5.18162689794298,
108.419536678284));
#210077=CARTESIAN_POINT('Ctrl Pts',(4.47527329368927,-5.07830769704904,
108.427012317439));
#210078=CARTESIAN_POINT('Ctrl Pts',(4.5914033168387,-4.97104662843979,108.434487956594));
#210079=CARTESIAN_POINT('Ctrl Pts',(4.73021837977693,-4.84283299697727,
108.443423900045));
#210080=CARTESIAN_POINT('Ctrl Pts',(4.86374843634968,-4.70871996212397,
108.452359843496));
#210081=CARTESIAN_POINT('Ctrl Pts',(4.99151051770733,-4.56914781459488,
108.461295786946));
#210082=CARTESIAN_POINT('Ctrl Pts',(5.11908053876973,-4.42978548102292,
108.470218297304));
#210083=CARTESIAN_POINT('Ctrl Pts',(5.24089971189132,-4.28498059957015,
108.479140807662));
#210084=CARTESIAN_POINT('Ctrl Pts',(5.35652160943637,-4.13521042362311,
108.488063318019));
#210085=CARTESIAN_POINT('Ctrl Pts',(5.47186019745173,-3.985807231085,108.496963965458));
#210086=CARTESIAN_POINT('Ctrl Pts',(5.58103165945079,-3.83146323026634,
108.505864612896));
#210087=CARTESIAN_POINT('Ctrl Pts',(5.68362993773233,-3.67268835199949,
108.514765260334));
#210088=CARTESIAN_POINT('Ctrl Pts',(5.78606966303756,-3.51415884071088,
108.523652152921));
#210089=CARTESIAN_POINT('Ctrl Pts',(5.8819563278233,-3.351212326475,108.532539045507));
#210090=CARTESIAN_POINT('Ctrl Pts',(5.97092549082285,-3.18438970338775,
108.541425938093));
#210091=CARTESIAN_POINT('Ctrl Pts',(6.05966596986221,-3.01799587671501,
108.550289988048));
#210092=CARTESIAN_POINT('Ctrl Pts',(6.14152430585439,-2.84774604890684,
108.559154038003));
#210093=CARTESIAN_POINT('Ctrl Pts',(6.21618091139597,-2.67420714919326,
108.568018087958));
#210094=CARTESIAN_POINT('Ctrl Pts',(6.28755863200182,-2.50829000082916,
108.576492832778));
#210095=CARTESIAN_POINT('Ctrl Pts',(6.35235347621247,-2.33936670065238,
108.584967577599));
#210096=CARTESIAN_POINT('Ctrl Pts',(6.41032417248772,-2.16795595057179,
108.593442322419));
#210097=CARTESIAN_POINT('Ctrl Pts',(6.46647648092975,-2.00192190359221,
108.601651236848));
#210098=CARTESIAN_POINT('Ctrl Pts',(6.51617098957402,-1.83371374559318,
108.609860151277));
#210099=CARTESIAN_POINT('Ctrl Pts',(6.55925379458158,-1.66387459210939,
108.618069065706));
#210100=CARTESIAN_POINT('Ctrl Pts',(6.60234684230714,-1.49399506022973,
108.626279931763));
#210101=CARTESIAN_POINT('Ctrl Pts',(6.63882496717623,-1.32248410549377,
108.63449079782));
#210102=CARTESIAN_POINT('Ctrl Pts',(6.66858508908188,-1.14989647780781,
108.642701663877));
#210103=CARTESIAN_POINT('Ctrl Pts',(6.69835759117187,-0.977237053821706,
108.650915945647));
#210104=CARTESIAN_POINT('Ctrl Pts',(6.72140646224253,-0.80350041519878,
108.659130227416));
#210105=CARTESIAN_POINT('Ctrl Pts',(6.73768031109416,-0.629247984100162,
108.667344509186));
#210106=CARTESIAN_POINT('Ctrl Pts',(6.75397247744739,-0.454799418134226,
108.675568036779));
#210107=CARTESIAN_POINT('Ctrl Pts',(6.76347435717635,-0.279834254788,108.683791564371));
#210108=CARTESIAN_POINT('Ctrl Pts',(6.76618663175958,-0.104916462950289,
108.692015091963));
#210109=CARTESIAN_POINT('Ctrl Pts',(6.76890064480531,0.0701134443878388,
108.700243890517));
#210110=CARTESIAN_POINT('Ctrl Pts',(6.76481638580924,0.24509556462914,108.708472689071));
#210111=CARTESIAN_POINT('Ctrl Pts',(6.75398654891632,0.419469542466905,
108.716701487625));
#210112=CARTESIAN_POINT('Ctrl Pts',(6.74314180561956,0.5940835321312,108.724941612461));
#210113=CARTESIAN_POINT('Ctrl Pts',(6.72553297473834,0.76808735420976,108.733181737297));
#210114=CARTESIAN_POINT('Ctrl Pts',(6.70126427248376,0.940928344951234,
108.741421862134));
#210115=CARTESIAN_POINT('Ctrl Pts',(6.69048997021494,1.01766261195728,108.745080137504));
#210116=CARTESIAN_POINT('Ctrl Pts',(6.67840368088764,1.09416784928394,108.748738412874));
#210117=CARTESIAN_POINT('Ctrl Pts',(6.66501768919725,1.17039660059648,108.752396688244));
#210118=CARTESIAN_POINT('Ctrl Pts',(6.63410429598899,1.34643804882107,108.760845050352));
#210119=CARTESIAN_POINT('Ctrl Pts',(6.59618518998594,1.52140684464478,108.76929341246));
#210120=CARTESIAN_POINT('Ctrl Pts',(6.55135103948677,1.69472374073644,108.777741774569));
#210121=CARTESIAN_POINT('Ctrl Pts',(6.50655830089898,1.86788054939779,108.786182333187));
#210122=CARTESIAN_POINT('Ctrl Pts',(6.45486333288775,2.03938817839978,108.794622891806));
#210123=CARTESIAN_POINT('Ctrl Pts',(6.39640792026916,2.20867714198294,108.803063450425));
#210124=CARTESIAN_POINT('Ctrl Pts',(6.33799750137578,2.37783580213028,108.81149751226));
#210125=CARTESIAN_POINT('Ctrl Pts',(6.27283712005258,2.54477888714468,108.819931574094));
#210126=CARTESIAN_POINT('Ctrl Pts',(6.20111860653571,2.70895127820282,108.828365635929));
#210127=CARTESIAN_POINT('Ctrl Pts',(6.12944426910723,2.87302254482733,108.836794502678));
#210128=CARTESIAN_POINT('Ctrl Pts',(6.05121998684421,3.03432621533776,108.845223369427));
#210129=CARTESIAN_POINT('Ctrl Pts',(5.96668614481783,3.19232602489767,108.853652236176));
#210130=CARTESIAN_POINT('Ctrl Pts',(5.88219147519993,3.35025261841853,108.862077197045));
#210131=CARTESIAN_POINT('Ctrl Pts',(5.79139323334351,3.50487811038034,108.870502157914));
#210132=CARTESIAN_POINT('Ctrl Pts',(5.69457846111091,3.65568942201764,108.878927118783));
#210133=CARTESIAN_POINT('Ctrl Pts',(5.59778920128535,3.80646099220353,108.887349859526));
#210134=CARTESIAN_POINT('Ctrl Pts',(5.49498675170909,3.95342010536718,108.895772600268));
#210135=CARTESIAN_POINT('Ctrl Pts',(5.38650257052733,4.09608093886126,108.904195341011));
#210136=CARTESIAN_POINT('Ctrl Pts',(5.27803183083916,4.23872409627888,108.912617038153));
#210137=CARTESIAN_POINT('Ctrl Pts',(5.16388096519308,4.37706977073814,108.921038735294));
#210138=CARTESIAN_POINT('Ctrl Pts',(5.04442318747724,4.51066333321852,108.929460432436));
#210139=CARTESIAN_POINT('Ctrl Pts',(4.92496353609314,4.64425899108374,108.93788226167));
#210140=CARTESIAN_POINT('Ctrl Pts',(4.80019702962241,4.773102140486,108.946304090904));
#210141=CARTESIAN_POINT('Ctrl Pts',(4.67053562242961,4.89677301900099,108.954725920138));
#210142=CARTESIAN_POINT('Ctrl Pts',(4.54081539464964,5.02050000051414,108.963151569914));
#210143=CARTESIAN_POINT('Ctrl Pts',(4.40619606946129,5.13904979115333,108.971577219691));
#210144=CARTESIAN_POINT('Ctrl Pts',(4.26712540358998,5.25204053583339,108.980002869468));
#210145=CARTESIAN_POINT('Ctrl Pts',(4.12802309634482,5.36505698818064,108.988430436249));
#210146=CARTESIAN_POINT('Ctrl Pts',(3.98446769129501,5.47251166655314,108.996858003031));
#210147=CARTESIAN_POINT('Ctrl Pts',(3.83693863843192,5.57406412637209,109.005285569812));
#210148=CARTESIAN_POINT('Ctrl Pts',(3.68930056888781,5.67569162844139,109.013719364149));
#210149=CARTESIAN_POINT('Ctrl Pts',(3.53768326227873,5.77140801246674,109.022153158486));
#210150=CARTESIAN_POINT('Ctrl Pts',(3.38259450415134,5.86091660241683,109.030586952823));
#210151=CARTESIAN_POINT('Ctrl Pts',(3.28931550483894,5.91475204349728,109.035659505506));
#210152=CARTESIAN_POINT('Ctrl Pts',(3.19478121801629,5.96634269262134,109.040732058189));
#210153=CARTESIAN_POINT('Ctrl Pts',(3.09910619832136,6.01563211736939,109.045804610872));
#210154=CARTESIAN_POINT('Ctrl Pts',(3.09910619832137,6.01563211736938,107.045755263024));
#210155=CARTESIAN_POINT('Ctrl Pts',(2.9337533076483,6.10081787314651,107.054504710927));
#210156=CARTESIAN_POINT('Ctrl Pts',(2.76488627843074,6.17918207037038,107.063254158829));
#210157=CARTESIAN_POINT('Ctrl Pts',(2.59307866646705,6.25045854553996,107.072003606731));
#210158=CARTESIAN_POINT('Ctrl Pts',(2.42127244185375,6.32173444515038,107.080752983982));
#210159=CARTESIAN_POINT('Ctrl Pts',(2.24652594672458,6.38592262741841,107.089502361232));
#210160=CARTESIAN_POINT('Ctrl Pts',(2.06943269687108,6.44280508110566,107.098251738482));
#210161=CARTESIAN_POINT('Ctrl Pts',(1.89234081822065,6.4996870943617,107.107001047987));
#210162=CARTESIAN_POINT('Ctrl Pts',(1.71290249405577,6.54926340459548,107.115750357493));
#210163=CARTESIAN_POINT('Ctrl Pts',(1.53172716625047,6.59136563150386,107.124499666998));
#210164=CARTESIAN_POINT('Ctrl Pts',(1.35055318107328,6.63346754640711,107.133248911665));
#210165=CARTESIAN_POINT('Ctrl Pts',(1.16764249714418,6.66809542395776,107.141998156333));
#210166=CARTESIAN_POINT('Ctrl Pts',(0.983616340614383,6.69513165624668,
107.150747401));
#210167=CARTESIAN_POINT('Ctrl Pts',(0.799591486713997,6.72216769715959,
107.159496583736));
#210168=CARTESIAN_POINT('Ctrl Pts',(0.614451459526995,6.74161215869368,
107.168245766471));
#210169=CARTESIAN_POINT('Ctrl Pts',(0.428825047910695,6.7533990018571,107.176994949207));
#210170=CARTESIAN_POINT('Ctrl Pts',(0.243199888597368,6.7651857655022,107.185744072918));
#210171=CARTESIAN_POINT('Ctrl Pts',(0.0570886373921497,6.76931499599834,
107.194493196628));
#210172=CARTESIAN_POINT('Ctrl Pts',(-0.128876626811008,6.76577266947847,
107.203242320339));
#210173=CARTESIAN_POINT('Ctrl Pts',(-0.314840698187959,6.76223036567994,
107.21199138793));
#210174=CARTESIAN_POINT('Ctrl Pts',(-0.500658497950996,6.75101660879225,
107.220740455522));
#210175=CARTESIAN_POINT('Ctrl Pts',(-0.685698951925902,6.73216948296221,
107.229489523113));
#210176=CARTESIAN_POINT('Ctrl Pts',(-0.870738280459446,6.71332247176298,
107.238238537492));
#210177=CARTESIAN_POINT('Ctrl Pts',(-1.05499998761201,6.68684221356194,
107.24698755187));
#210178=CARTESIAN_POINT('Ctrl Pts',(-1.23785829161361,6.65281863948533,
107.255736566249));
#210179=CARTESIAN_POINT('Ctrl Pts',(-1.43007412917341,6.61705395368875,
107.264933299948));
#210180=CARTESIAN_POINT('Ctrl Pts',(-1.62073882535726,6.57295372727806,
107.274130033647));
#210181=CARTESIAN_POINT('Ctrl Pts',(-1.80913696091445,6.52068343478299,
107.283326767346));
#210182=CARTESIAN_POINT('Ctrl Pts',(-1.98838356186044,6.4709521981522,107.29207676506));
#210183=CARTESIAN_POINT('Ctrl Pts',(-2.16557827572465,6.41382586850914,
107.300826762774));
#210184=CARTESIAN_POINT('Ctrl Pts',(-2.34011918621633,6.34949849943303,
107.309576760487));
#210185=CARTESIAN_POINT('Ctrl Pts',(-2.51465655691025,6.2851724349558,107.318326580746));
#210186=CARTESIAN_POINT('Ctrl Pts',(-2.68653996295249,6.21364572242408,
107.327076401004));
#210187=CARTESIAN_POINT('Ctrl Pts',(-2.85518555379904,6.1351613225226,107.335826221262));
#210188=CARTESIAN_POINT('Ctrl Pts',(-3.02382794858607,6.05667841000547,
107.3445758757));
#210189=CARTESIAN_POINT('Ctrl Pts',(-3.18923239109202,5.97123819492123,
107.353325530137));
#210190=CARTESIAN_POINT('Ctrl Pts',(-3.35083705967622,5.87913088810757,
107.362075184575));
#210191=CARTESIAN_POINT('Ctrl Pts',(-3.5124388804232,5.78702520443151,107.370824684824));
#210192=CARTESIAN_POINT('Ctrl Pts',(-3.67024081223607,5.68825280605837,
107.379574185073));
#210193=CARTESIAN_POINT('Ctrl Pts',(-3.82370687544316,5.58314917682563,
107.388323685322));
#210194=CARTESIAN_POINT('Ctrl Pts',(-3.97717043817738,5.47804726008077,
107.397073043012));
#210195=CARTESIAN_POINT('Ctrl Pts',(-4.12629803722392,5.36661448084289,
107.405822400703));
#210196=CARTESIAN_POINT('Ctrl Pts',(-4.27058317206847,5.24922931204626,
107.414571758393));
#210197=CARTESIAN_POINT('Ctrl Pts',(-4.4148661477477,5.13184589986846,107.423320985153));
#210198=CARTESIAN_POINT('Ctrl Pts',(-4.55430658194344,5.00851045723098,
107.432070211913));
#210199=CARTESIAN_POINT('Ctrl Pts',(-4.68843089001772,4.8796418710319,107.440819438673));
#210200=CARTESIAN_POINT('Ctrl Pts',(-4.82255336917744,4.75077504208053,
107.449568546129));
#210201=CARTESIAN_POINT('Ctrl Pts',(-4.95135966065026,4.61637541908209,
107.458317653585));
#210202=CARTESIAN_POINT('Ctrl Pts',(-5.0744123086912,4.47689945401985,107.467066761041));
#210203=CARTESIAN_POINT('Ctrl Pts',(-5.19746344226278,4.33742520555681,
107.475815760817));
#210204=CARTESIAN_POINT('Ctrl Pts',(-5.31476088454614,4.19287495491529,
107.484564760594));
#210205=CARTESIAN_POINT('Ctrl Pts',(-5.42590627628689,4.04373961586927,
107.49331376037));
#210206=CARTESIAN_POINT('Ctrl Pts',(-5.53706380672511,3.89458798906957,
107.502063715665));
#210207=CARTESIAN_POINT('Ctrl Pts',(-5.64206777071714,3.7408505015551,107.510813670959));
#210208=CARTESIAN_POINT('Ctrl Pts',(-5.74056148163865,3.58304938223389,
107.519563626254));
#210209=CARTESIAN_POINT('Ctrl Pts',(-5.83905138951744,3.42525435593519,
107.528313243695));
#210210=CARTESIAN_POINT('Ctrl Pts',(-5.93103139557517,3.26339625497429,
107.537062861136));
#210211=CARTESIAN_POINT('Ctrl Pts',(-6.01618907820715,3.0980248506526,107.545812478577));
#210212=CARTESIAN_POINT('Ctrl Pts',(-6.10134392544859,2.93265895249898,
107.554561804693));
#210213=CARTESIAN_POINT('Ctrl Pts',(-6.17967677261715,2.76378023986296,
107.563311130809));
#210214=CARTESIAN_POINT('Ctrl Pts',(-6.25092157009115,2.59196229227379,
107.572060456925));
#210215=CARTESIAN_POINT('Ctrl Pts',(-6.32216437407663,2.42014915229329,
107.580809538228));
#210216=CARTESIAN_POINT('Ctrl Pts',(-6.38631941548848,2.24539720663063,
107.58955861953));
#210217=CARTESIAN_POINT('Ctrl Pts',(-6.44316881037478,2.06829994947871,
107.598307700832));
#210218=CARTESIAN_POINT('Ctrl Pts',(-6.5000233452452,1.89118668024629,107.607057573175));
#210219=CARTESIAN_POINT('Ctrl Pts',(-6.54957082411051,1.71172794807877,
107.615807445517));
#210220=CARTESIAN_POINT('Ctrl Pts',(-6.59164294296045,1.53053334250509,
107.62455731786));
#210221=CARTESIAN_POINT('Ctrl Pts',(-6.633712140821,1.34935131693768,107.633306582714));
#210222=CARTESIAN_POINT('Ctrl Pts',(-6.66830695239661,1.16643393829932,
107.642055847569));
#210223=CARTESIAN_POINT('Ctrl Pts',(-6.69530988153964,0.982402458342671,
107.650805112424));
#210224=CARTESIAN_POINT('Ctrl Pts',(-6.72231419690463,0.798361530948761,
107.659554826431));
#210225=CARTESIAN_POINT('Ctrl Pts',(-6.74172580829262,0.6132066713642,107.668304540438));
#210226=CARTESIAN_POINT('Ctrl Pts',(-6.75347878028168,0.427566795115138,
107.677054254445));
#210227=CARTESIAN_POINT('Ctrl Pts',(-6.76248992368204,0.285234494207695,
107.683762764234));
#210228=CARTESIAN_POINT('Ctrl Pts',(-6.76699999999989,0.142617266095235,
107.690471274022));
#210229=CARTESIAN_POINT('Ctrl Pts',(-6.767,5.22501239580748E-12,107.69717978381));
#210230=CARTESIAN_POINT('',(-6.76742387024867,0.00103549087071322,107.30355369317));
#210231=CARTESIAN_POINT('Ctrl Pts',(3.09910619832136,6.01563211736939,106.651504649108));
#210232=CARTESIAN_POINT('Ctrl Pts',(2.9439492773614,6.0955651594966,106.659704480459));
#210233=CARTESIAN_POINT('Ctrl Pts',(2.78560761231443,6.16953806982017,106.66790431181));
#210234=CARTESIAN_POINT('Ctrl Pts',(2.62458091016097,6.23729621278472,106.676104143161));
#210235=CARTESIAN_POINT('Ctrl Pts',(2.46359874742784,6.30503561408488,106.684301706467));
#210236=CARTESIAN_POINT('Ctrl Pts',(2.29993335547208,6.36656352928214,106.692499269774));
#210237=CARTESIAN_POINT('Ctrl Pts',(2.13410633458906,6.42167261332021,106.70069683308));
#210238=CARTESIAN_POINT('Ctrl Pts',(1.96830004468343,6.4767748078588,106.708893371562));
#210239=CARTESIAN_POINT('Ctrl Pts',(1.80033300415287,6.52545965556149,106.717089910045));
#210240=CARTESIAN_POINT('Ctrl Pts',(1.6307439661636,6.56756904164859,106.725286448527));
#210241=CARTESIAN_POINT('Ctrl Pts',(1.461145293775,6.60968081998136,106.733483452657));
#210242=CARTESIAN_POINT('Ctrl Pts',(1.28992478855158,6.64521630602577,106.741680456787));
#210243=CARTESIAN_POINT('Ctrl Pts',(1.11763349252699,6.67406805302298,106.749877460917));
#210244=CARTESIAN_POINT('Ctrl Pts',(0.945301081621044,6.7029266850816,106.758076421147));
#210245=CARTESIAN_POINT('Ctrl Pts',(0.771897724715815,6.72509834213783,
106.766275381376));
#210246=CARTESIAN_POINT('Ctrl Pts',(0.5979817694663,6.74052719031575,106.774474341605));
#210247=CARTESIAN_POINT('Ctrl Pts',(0.423900403987636,6.75597071276153,
106.782681099807));
#210248=CARTESIAN_POINT('Ctrl Pts',(0.249305823948718,6.76465858239079,
106.790887858009));
#210249=CARTESIAN_POINT('Ctrl Pts',(0.0747595227450543,6.76658702846265,
106.799094616211));
#210250=CARTESIAN_POINT('Ctrl Pts',(-0.0998726519923158,6.7685164232941,
106.807305411985));
#210251=CARTESIAN_POINT('Ctrl Pts',(-0.274456142191708,6.76367977437215,
106.815516207759));
#210252=CARTESIAN_POINT('Ctrl Pts',(-0.448432463893874,6.7521253931874,
106.823727003534));
#210253=CARTESIAN_POINT('Ctrl Pts',(-0.622646552553638,6.74055522106033,
106.831949020697));
#210254=CARTESIAN_POINT('Ctrl Pts',(-0.796251457698808,6.72224900732025,
106.84017103786));
#210255=CARTESIAN_POINT('Ctrl Pts',(-0.968695606756374,6.69730675879871,
106.848393055023));
#210256=CARTESIAN_POINT('Ctrl Pts',(-1.11706527516134,6.67584663293977,
106.855467217682));
#210257=CARTESIAN_POINT('Ctrl Pts',(-1.26457568858267,6.64947488513452,
106.862541380342));
#210258=CARTESIAN_POINT('Ctrl Pts',(-1.41088394946056,6.61828493502317,
106.869615543001));
#210259=CARTESIAN_POINT('Ctrl Pts',(-1.59569767350388,6.57888640210221,
106.878551486452));
#210260=CARTESIAN_POINT('Ctrl Pts',(-1.77897792879254,6.53171723688859,
106.887487429903));
#210261=CARTESIAN_POINT('Ctrl Pts',(-1.96008466387585,6.4769095339088,106.896423373353));
#210262=CARTESIAN_POINT('Ctrl Pts',(-2.140919147501,6.42218422144336,106.905345883711));
#210263=CARTESIAN_POINT('Ctrl Pts',(-2.31958638389205,6.35984335785542,
106.914268394069));
#210264=CARTESIAN_POINT('Ctrl Pts',(-2.49545887738146,6.2900694742823,106.923190904426));
#210265=CARTESIAN_POINT('Ctrl Pts',(-2.67090042868285,6.22046655837706,
106.932091551865));
#210266=CARTESIAN_POINT('Ctrl Pts',(-2.84356066487769,6.1434670678563,106.940992199303));
#210267=CARTESIAN_POINT('Ctrl Pts',(-3.01283012577512,6.05930223979807,
106.949892846741));
#210268=CARTESIAN_POINT('Ctrl Pts',(-3.18183800161143,5.97526747809424,
106.958779739327));
#210269=CARTESIAN_POINT('Ctrl Pts',(-3.34746532457885,5.88408958125895,
106.967666631913));
#210270=CARTESIAN_POINT('Ctrl Pts',(-3.50912261682026,5.78604765449789,
106.9765535245));
#210271=CARTESIAN_POINT('Ctrl Pts',(-3.67036438947681,5.68825773208592,
106.985417574454));
#210272=CARTESIAN_POINT('Ctrl Pts',(-3.82765627358926,5.58363911886481,
106.994281624409));
#210273=CARTESIAN_POINT('Ctrl Pts',(-3.98043407301949,5.47251620283992,
107.003145674364));
#210274=CARTESIAN_POINT('Ctrl Pts',(-4.12650193940196,5.36627375589745,
107.011620419185));
#210275=CARTESIAN_POINT('Ctrl Pts',(-4.26844347634824,5.25408617516802,
107.020095164005));
#210276=CARTESIAN_POINT('Ctrl Pts',(-4.4057864497103,5.13627635155558,107.028569908826));
#210277=CARTESIAN_POINT('Ctrl Pts',(-4.53882133626306,5.02216191136675,
107.036778823255));
#210278=CARTESIAN_POINT('Ctrl Pts',(-4.66741275280672,4.90288166908814,
107.044987737684));
#210279=CARTESIAN_POINT('Ctrl Pts',(-4.79115113310689,4.77882410428848,
107.053196652113));
#210280=CARTESIAN_POINT('Ctrl Pts',(-4.91491893157851,4.65473704543287,
107.06140751817));
#210281=CARTESIAN_POINT('Ctrl Pts',(-5.0338311436749,4.5258706533721,107.069618384227));
#210282=CARTESIAN_POINT('Ctrl Pts',(-5.14751596904057,4.39264935414522,
107.077829250284));
#210283=CARTESIAN_POINT('Ctrl Pts',(-5.2612480871909,4.25937263497819,107.086043532053));
#210284=CARTESIAN_POINT('Ctrl Pts',(-5.36974825542041,4.12173767012273,
107.094257813823));
#210285=CARTESIAN_POINT('Ctrl Pts',(-5.47268571603573,3.98020100667021,
107.102472095593));
#210286=CARTESIAN_POINT('Ctrl Pts',(-5.57573904089067,3.83850503252758,
107.110695623185));
#210287=CARTESIAN_POINT('Ctrl Pts',(-5.67321694279769,3.69289887626075,
107.118919150777));
#210288=CARTESIAN_POINT('Ctrl Pts',(-5.76483214252082,3.54386785427432,
107.12714267837));
#210289=CARTESIAN_POINT('Ctrl Pts',(-5.85650606402328,3.39474130919987,
107.135371476923));
#210290=CARTESIAN_POINT('Ctrl Pts',(-5.94230961837022,3.24218583195639,
107.143600275477));
#210291=CARTESIAN_POINT('Ctrl Pts',(-6.02200209756949,3.08671018025156,
107.151829074031));
#210292=CARTESIAN_POINT('Ctrl Pts',(-6.10180426708943,2.93102052875326,
107.160069198867));
#210293=CARTESIAN_POINT('Ctrl Pts',(-6.17547841088812,2.77240299643548,
107.168309323704));
#210294=CARTESIAN_POINT('Ctrl Pts',(-6.24283205184973,2.61138602515939,
107.17654944854));
#210295=CARTESIAN_POINT('Ctrl Pts',(-6.27273428885559,2.53990113483536,
107.18020772391));
#210296=CARTESIAN_POINT('Ctrl Pts',(-6.30139141788821,2.46794351755978,
107.18386599928));
#210297=CARTESIAN_POINT('Ctrl Pts',(-6.32878977979195,2.39556025246726,
107.18752427465));
#210298=CARTESIAN_POINT('Ctrl Pts',(-6.40195836908091,2.20225740415991,
107.197293867774));
#210299=CARTESIAN_POINT('Ctrl Pts',(-6.46627366852963,2.00558245517283,
107.207063460898));
#210300=CARTESIAN_POINT('Ctrl Pts',(-6.52147440592114,1.80628363578802,
107.216833054022));
#210301=CARTESIAN_POINT('Ctrl Pts',(-6.57653288654883,1.60749842557613,
107.226577470115));
#210302=CARTESIAN_POINT('Ctrl Pts',(-6.62252368424138,1.40610290668516,
107.236321886207));
#210303=CARTESIAN_POINT('Ctrl Pts',(-6.65923584019387,1.20285785722065,
107.2460663023));
#210304=CARTESIAN_POINT('Ctrl Pts',(-6.6956926317681,1.00102655054363,107.255742937662));
#210305=CARTESIAN_POINT('Ctrl Pts',(-6.7229993837118,0.797371419371896,
107.265419573023));
#210306=CARTESIAN_POINT('Ctrl Pts',(-6.74099766105347,0.592654649582421,
107.275096208385));
#210307=CARTESIAN_POINT('Ctrl Pts',(-6.75818629335671,0.39714697874161,
107.28433754432));
#210308=CARTESIAN_POINT('Ctrl Pts',(-6.76688532234933,0.200671188027621,
107.293578880255));
#210309=CARTESIAN_POINT('Ctrl Pts',(-6.76699887320081,0.00390513750720152,
107.30282021619));
#210310=CARTESIAN_POINT('Ctrl Pts',(-6.767,4.98895312755119E-12,107.30282021619));
#210311=CARTESIAN_POINT('Ctrl Pts',(-6.76700000000014,-0.186007249522004,
107.311569728001));
#210312=CARTESIAN_POINT('Ctrl Pts',(-6.75932637294547,-0.372014355745178,
107.320319239812));
#210313=CARTESIAN_POINT('Ctrl Pts',(-6.74400518264218,-0.557389537482884,
107.329068751624));
#210314=CARTESIAN_POINT('Ctrl Pts',(-6.72868405705135,-0.74276393624739,
107.337818226479));
#210315=CARTESIAN_POINT('Ctrl Pts',(-6.70571545645783,-0.927506130238072,
107.346567701335));
#210316=CARTESIAN_POINT('Ctrl Pts',(-6.67517739404867,-1.11098863989762,
107.355317176191));
#210317=CARTESIAN_POINT('Ctrl Pts',(-6.64463945808747,-1.29447038981717,
107.364066614818));
#210318=CARTESIAN_POINT('Ctrl Pts',(-6.60653217008401,-1.47669218313478,
107.372816053445));
#210319=CARTESIAN_POINT('Ctrl Pts',(-6.56098496092723,-1.65703510599104,
107.381565492072));
#210320=CARTESIAN_POINT('Ctrl Pts',(-6.51543793658348,-1.83737729708517,
107.390314895197));
#210321=CARTESIAN_POINT('Ctrl Pts',(-6.46245112167477,-2.01584035510744,
107.399064298322));
#210322=CARTESIAN_POINT('Ctrl Pts',(-6.40220448374316,-2.19181813760608,
107.407813701447));
#210323=CARTESIAN_POINT('Ctrl Pts',(-6.34195808526573,-2.36779522066959,
107.416563069797));
#210324=CARTESIAN_POINT('Ctrl Pts',(-6.27445201433179,-2.54128677683979,
107.425312438147));
#210325=CARTESIAN_POINT('Ctrl Pts',(-6.19991555071984,-2.71170355384624,
107.434061806497));
#210326=CARTESIAN_POINT('Ctrl Pts',(-6.12537937716775,-2.88211966767303,
107.442811140799));
#210327=CARTESIAN_POINT('Ctrl Pts',(-6.04381298052602,-3.04946076371624,
107.451560475101));
#210328=CARTESIAN_POINT('Ctrl Pts',(-5.95549339335912,-3.21315848374398,
107.460309809403));
#210329=CARTESIAN_POINT('Ctrl Pts',(-5.86717414255502,-3.3768555803333,
107.469059110383));
#210330=CARTESIAN_POINT('Ctrl Pts',(-5.77210188876704,-3.53690907646582,
107.477808411363));
#210331=CARTESIAN_POINT('Ctrl Pts',(-5.67059953347117,-3.69277536969101,
107.486557712343));
#210332=CARTESIAN_POINT('Ctrl Pts',(-5.56909755631517,-3.8486410822473,
107.495306980729));
#210333=CARTESIAN_POINT('Ctrl Pts',(-5.46116568196996,-4.00031938297317,
107.504056249114));
#210334=CARTESIAN_POINT('Ctrl Pts',(-5.34717048533763,-4.14729511859648,
107.512805517499));
#210335=CARTESIAN_POINT('Ctrl Pts',(-5.23317570392007,-4.29427031887709,
107.521554754016));
#210336=CARTESIAN_POINT('Ctrl Pts',(-5.11311782003695,-4.43654276189339,
107.530303990533));
#210337=CARTESIAN_POINT('Ctrl Pts',(-4.98740458984944,-4.57362924351643,
107.53905322705));
#210338=CARTESIAN_POINT('Ctrl Pts',(-4.86169180711944,-4.71071523720059,
107.547802432426));
#210339=CARTESIAN_POINT('Ctrl Pts',(-4.73032391204383,-4.84261509523031,
107.556551637801));
#210340=CARTESIAN_POINT('Ctrl Pts',(-4.59374707013821,-4.96888084538125,
107.565300843177));
#210341=CARTESIAN_POINT('Ctrl Pts',(-4.45717070301695,-5.09514615659244,
107.574050018137));
#210342=CARTESIAN_POINT('Ctrl Pts',(-4.3153856357132,-5.21577720459295,
107.582799193097));
#210343=CARTESIAN_POINT('Ctrl Pts',(-4.16887341029819,-5.33036429232644,
107.591548368058));
#210344=CARTESIAN_POINT('Ctrl Pts',(-4.02236168204035,-5.44495099123372,
107.60029751333));
#210345=CARTESIAN_POINT('Ctrl Pts',(-3.87112305348513,-5.55349359438359,
107.609046658602));
#210346=CARTESIAN_POINT('Ctrl Pts',(-3.71567117018127,-5.65562346298653,
107.617795803874));
#210347=CARTESIAN_POINT('Ctrl Pts',(-3.56021980146169,-5.75775299351428,
107.626544920184));
#210348=CARTESIAN_POINT('Ctrl Pts',(-3.40055544538682,-5.8534696746368,
107.635294036494));
#210349=CARTESIAN_POINT('Ctrl Pts',(-3.23722035987167,-5.9424484298673,
107.644043152804));
#210350=CARTESIAN_POINT('Ctrl Pts',(-3.07388580147504,-6.03142689794364,
107.652792240879));
#210351=CARTESIAN_POINT('Ctrl Pts',(-2.90688078896912,-6.11366734656623,
107.661541328954));
#210352=CARTESIAN_POINT('Ctrl Pts',(-2.73677250721714,-6.18889046952202,
107.670290417029));
#210353=CARTESIAN_POINT('Ctrl Pts',(-2.56666476031831,-6.26411335596184,
107.679039477595));
#210354=CARTESIAN_POINT('Ctrl Pts',(-2.3934540257552,-6.33231884500422,
107.687788538161));
#210355=CARTESIAN_POINT('Ctrl Pts',(-2.21772856065951,-6.39327529762602,
107.696537598727));
#210356=CARTESIAN_POINT('Ctrl Pts',(-2.04200363348871,-6.45423156364998,
107.705286632511));
#210357=CARTESIAN_POINT('Ctrl Pts',(-1.86376426189634,-6.50793874375556,
107.714035666294));
#210358=CARTESIAN_POINT('Ctrl Pts',(-1.68361577753508,-6.55421443909451,
107.722784700078));
#210359=CARTESIAN_POINT('Ctrl Pts',(-1.50346782968131,-6.60048999661793,
107.731533707806));
#210360=CARTESIAN_POINT('Ctrl Pts',(-1.32141105795296,-6.63933404237652,
107.740282715534));
#210361=CARTESIAN_POINT('Ctrl Pts',(-1.13806375487307,-6.67061465607512,
107.749031723262));
#210362=CARTESIAN_POINT('Ctrl Pts',(-0.954716982606139,-6.70189517921251,
107.75778070566));
#210363=CARTESIAN_POINT('Ctrl Pts',(-0.770079968905529,-6.72561226592189,
107.766529688058));
#210364=CARTESIAN_POINT('Ctrl Pts',(-0.584779765561904,-6.74168536983071,
107.775278670457));
#210365=CARTESIAN_POINT('Ctrl Pts',(-0.391489830654962,-6.75845151013832,
107.784404889467));
#210366=CARTESIAN_POINT('Ctrl Pts',(-0.197478578242002,-6.76689983031615,
107.793531108477));
#210367=CARTESIAN_POINT('Ctrl Pts',(-0.00346287645500613,-6.76699911397118,
107.802657327486));
#210368=CARTESIAN_POINT('Ctrl Pts',(0.184489834651114,-6.76709529501199,
107.811498352152));
#210369=CARTESIAN_POINT('Ctrl Pts',(0.372446404246595,-6.75935639738183,
107.820339376818));
#210370=CARTESIAN_POINT('Ctrl Pts',(0.559755019485561,-6.7438092587321,
107.829180401484));
#210371=CARTESIAN_POINT('Ctrl Pts',(0.745134705518991,-6.72842222659836,
107.837930380094));
#210372=CARTESIAN_POINT('Ctrl Pts',(0.929879431225777,-6.70538706057562,
107.846680358703));
#210373=CARTESIAN_POINT('Ctrl Pts',(1.11336163626546,-6.67478200894174,
107.855430337313));
#210374=CARTESIAN_POINT('Ctrl Pts',(1.29684196300447,-6.64417727061066,
107.86418022635));
#210375=CARTESIAN_POINT('Ctrl Pts',(1.47905951217247,-6.60600284890649,
107.872930115386));
#210376=CARTESIAN_POINT('Ctrl Pts',(1.6593953206683,-6.56038841607295,107.881680004423));
#210377=CARTESIAN_POINT('Ctrl Pts',(1.83972934300564,-6.51477443503324,
107.890429806795));
#210378=CARTESIAN_POINT('Ctrl Pts',(2.01818138406043,-6.46172066062211,
107.899179609167));
#210379=CARTESIAN_POINT('Ctrl Pts',(2.19414528353995,-6.40140730423549,
107.907929411539));
#210380=CARTESIAN_POINT('Ctrl Pts',(2.37010749863798,-6.34109452518717,
107.916679130156));
#210381=CARTESIAN_POINT('Ctrl Pts',(2.54358134866262,-6.27352239616584,
107.925428848772));
#210382=CARTESIAN_POINT('Ctrl Pts',(2.71397759435362,-6.19892043966903,
107.934178567388));
#210383=CARTESIAN_POINT('Ctrl Pts',(2.88437226557929,-6.12431917249607,
107.942928205157));
#210384=CARTESIAN_POINT('Ctrl Pts',(3.0516891268076,-6.04268832278897,107.951677842926));
#210385=CARTESIAN_POINT('Ctrl Pts',(3.21535986273659,-5.9543051612344,107.960427480694));
#210386=CARTESIAN_POINT('Ctrl Pts',(3.37902914072657,-5.86592278697547,
107.969177040523));
#210387=CARTESIAN_POINT('Ctrl Pts',(3.53905210621397,-5.77078835742049,
107.977926600352));
#210388=CARTESIAN_POINT('Ctrl Pts',(3.69488522831533,-5.66922500431736,
107.986676160182));
#210389=CARTESIAN_POINT('Ctrl Pts',(3.85071701406796,-5.56766252217194,
107.995425644979));
#210390=CARTESIAN_POINT('Ctrl Pts',(4.0023587882228,-5.45967138329462,108.004175129776));
#210391=CARTESIAN_POINT('Ctrl Pts',(4.1492954961122,-5.34561838199689,108.012924614573));
#210392=CARTESIAN_POINT('Ctrl Pts',(4.29623099275994,-5.23156632087094,
108.021674027246));
#210393=CARTESIAN_POINT('Ctrl Pts',(4.43846127435942,-5.11145267305039,
108.030423439918));
#210394=CARTESIAN_POINT('Ctrl Pts',(4.57550326054365,-4.98568540049956,
108.039172852591));
#210395=CARTESIAN_POINT('Ctrl Pts',(4.71254416257714,-4.85991912290426,
108.047922196046));
#210396=CARTESIAN_POINT('Ctrl Pts',(4.84439664018704,-4.72849950385478,
108.056671539501));
#210397=CARTESIAN_POINT('Ctrl Pts',(4.97061286794697,-4.5918728986112,108.065420882956));
#210398=CARTESIAN_POINT('Ctrl Pts',(5.09682813912642,-4.45524732884734,
108.074170160101));
#210399=CARTESIAN_POINT('Ctrl Pts',(5.21740705147802,-4.31341506235832,
108.082919437246));
#210400=CARTESIAN_POINT('Ctrl Pts',(5.33194007545664,-4.16685781275765,
108.091668714391));
#210401=CARTESIAN_POINT('Ctrl Pts',(5.44647226944451,-4.02030162521888,
108.100417928132));
#210402=CARTESIAN_POINT('Ctrl Pts',(5.55495848628077,-3.86902074887986,
108.109167141873));
#210403=CARTESIAN_POINT('Ctrl Pts',(5.6570302729175,-3.71352898080721,108.117916355614));
#210404=CARTESIAN_POINT('Ctrl Pts',(5.75910135376961,-3.55803828789647,
108.126665508858));
#210405=CARTESIAN_POINT('Ctrl Pts',(5.85475793592718,-3.39833700106772,
108.135414662102));
#210406=CARTESIAN_POINT('Ctrl Pts',(5.94367514427366,-3.23496750823614,
108.144163815346));
#210407=CARTESIAN_POINT('Ctrl Pts',(6.03259176732602,-3.07159909077798,
108.152912910999));
#210408=CARTESIAN_POINT('Ctrl Pts',(6.11476896835883,-2.9045627673152,108.161662006652));
#210409=CARTESIAN_POINT('Ctrl Pts',(6.18992765547842,-2.7344258300315,108.170411102305));
#210410=CARTESIAN_POINT('Ctrl Pts',(6.26508587283007,-2.56428995616285,
108.179160143273));
#210411=CARTESIAN_POINT('Ctrl Pts',(6.3332255482711,-2.39105376935333,108.187909184241));
#210412=CARTESIAN_POINT('Ctrl Pts',(6.39411526732979,-2.21530561054227,
108.196658225209));
#210413=CARTESIAN_POINT('Ctrl Pts',(6.4550046260279,-2.03955849185277,108.205407214398));
#210414=CARTESIAN_POINT('Ctrl Pts',(6.50864402040679,-1.86129970164755,
108.214156203587));
#210415=CARTESIAN_POINT('Ctrl Pts',(6.55485128368539,-1.68113463136301,
108.222905192776));
#210416=CARTESIAN_POINT('Ctrl Pts',(6.6019980955427,-1.49730620117119,108.231832078247));
#210417=CARTESIAN_POINT('Ctrl Pts',(6.64140720707822,-1.31149343245957,
108.240758963719));
#210418=CARTESIAN_POINT('Ctrl Pts',(6.67293928722839,-1.12435326697791,
108.24968584919));
#210419=CARTESIAN_POINT('Ctrl Pts',(6.70384625876219,-0.940923067009255,
108.258435763368));
#210420=CARTESIAN_POINT('Ctrl Pts',(6.72718554579766,-0.756217899524335,
108.267185677545));
#210421=CARTESIAN_POINT('Ctrl Pts',(6.74287786815305,-0.570865181257168,
108.275935591722));
#210422=CARTESIAN_POINT('Ctrl Pts',(6.7585698819083,-0.385516108076666,
108.284685333827));
#210423=CARTESIAN_POINT('Ctrl Pts',(6.76661520773395,-0.199519795229111,
108.293435075931));
#210424=CARTESIAN_POINT('Ctrl Pts',(6.76698651789578,-0.0135080204584527,
108.302184818036));
#210425=CARTESIAN_POINT('Ctrl Pts',(6.7673578212491,0.172500343510114,108.310934399701));
#210426=CARTESIAN_POINT('Ctrl Pts',(6.76005538995199,0.358523882208035,
108.319683981366));
#210427=CARTESIAN_POINT('Ctrl Pts',(6.74510402742385,0.543930748561455,
108.328433563031));
#210428=CARTESIAN_POINT('Ctrl Pts',(6.73015291918063,0.729334461612219,
108.337182995888));
#210429=CARTESIAN_POINT('Ctrl Pts',(6.70755316306637,0.914121237631574,
108.345932428744));
#210430=CARTESIAN_POINT('Ctrl Pts',(6.67738151874627,1.09766345165802,108.354681861601));
#210431=CARTESIAN_POINT('Ctrl Pts',(6.6472103474763,1.28120278799349,108.363431157278));
#210432=CARTESIAN_POINT('Ctrl Pts',(6.6094675720521,1.46349731860019,108.372180452956));
#210433=CARTESIAN_POINT('Ctrl Pts',(6.56428138111599,1.64392790277856,108.380929748633));
#210434=CARTESIAN_POINT('Ctrl Pts',(6.51909583859935,1.82435589778752,108.389678918759));
#210435=CARTESIAN_POINT('Ctrl Pts',(6.46646716392969,2.00291972191962,108.398428088885));
#210436=CARTESIAN_POINT('Ctrl Pts',(6.40657409872986,2.17901292274362,108.40717725901));
#210437=CARTESIAN_POINT('Ctrl Pts',(6.34668181342182,2.35510383058691,108.415926315209));
#210438=CARTESIAN_POINT('Ctrl Pts',(6.27952541914159,2.5287239082231,108.424675371408));
#210439=CARTESIAN_POINT('Ctrl Pts',(6.20533299175627,2.69928350890031,108.433424427608));
#210440=CARTESIAN_POINT('Ctrl Pts',(6.12831602991661,2.87633637965384,108.442506563766));
#210441=CARTESIAN_POINT('Ctrl Pts',(6.04371690605384,3.05009086601238,108.451588699924));
#210442=CARTESIAN_POINT('Ctrl Pts',(5.95184520316745,3.21991112882525,108.460670836082));
#210443=CARTESIAN_POINT('Ctrl Pts',(5.86333549509391,3.38351691182816,108.469420616426));
#210444=CARTESIAN_POINT('Ctrl Pts',(5.76807618099487,3.54347103711811,108.478170396769));
#210445=CARTESIAN_POINT('Ctrl Pts',(5.66639083309136,3.69923018027511,108.486920177113));
#210446=CARTESIAN_POINT('Ctrl Pts',(5.56470914082328,3.85498372381866,108.495669642898));
#210447=CARTESIAN_POINT('Ctrl Pts',(5.45660203372202,4.00654234701814,108.504419108683));
#210448=CARTESIAN_POINT('Ctrl Pts',(5.34243669839359,4.15339127986486,108.513168574468));
#210449=CARTESIAN_POINT('Ctrl Pts',(5.22827486050731,4.3002357140111,108.521917772214));
#210450=CARTESIAN_POINT('Ctrl Pts',(5.10805534167248,4.44237052028313,108.53066696996));
#210451=CARTESIAN_POINT('Ctrl Pts',(4.98218644340084,4.57931296628577,108.539416167706));
#210452=CARTESIAN_POINT('Ctrl Pts',(4.85632073219736,4.71625194483206,108.548165143917));
#210453=CARTESIAN_POINT('Ctrl Pts',(4.72480612170486,4.84799861524345,108.556914120129));
#210454=CARTESIAN_POINT('Ctrl Pts',(4.58808925235497,4.97410554898313,108.565663096341));
#210455=CARTESIAN_POINT('Ctrl Pts',(4.4513634947424,5.10022068121039,108.574412641342));
#210456=CARTESIAN_POINT('Ctrl Pts',(4.30943501210277,5.22069514871671,108.583162186344));
#210457=CARTESIAN_POINT('Ctrl Pts',(4.16278587431984,5.33511975166099,108.591911731346));
#210458=CARTESIAN_POINT('Ctrl Pts',(4.01614535740647,5.44953762807696,108.600660761999));
#210459=CARTESIAN_POINT('Ctrl Pts',(3.86478496658119,5.55790617532648,108.609409792653));
#210460=CARTESIAN_POINT('Ctrl Pts',(3.70921874747387,5.65985735539231,108.618158823307));
#210461=CARTESIAN_POINT('Ctrl Pts',(3.55365041606098,5.76180991976925,108.626907972756));
#210462=CARTESIAN_POINT('Ctrl Pts',(3.39387638174725,5.85734478552696,108.635657122206));
#210463=CARTESIAN_POINT('Ctrl Pts',(3.23043927904746,5.94613749121119,108.644406271656));
#210464=CARTESIAN_POINT('Ctrl Pts',(3.18691767070565,5.96978206944076,108.646736079572));
#210465=CARTESIAN_POINT('Ctrl Pts',(3.14313645919691,5.99294880633394,108.649065887488));
#210466=CARTESIAN_POINT('Ctrl Pts',(3.09910619832125,6.01563211736945,108.651395695404));
#210467=CARTESIAN_POINT('Origin',(0.,0.,4.30282021618968));
#210468=CARTESIAN_POINT('',(3.09910619832136,6.01563211736939,111.045833125094));
#210469=CARTESIAN_POINT('',(3.10339103771845,6.02380226238954,110.651315755419));
#210470=CARTESIAN_POINT('',(3.09910619832133,6.0156321173694,4.30282021618968));
#210471=CARTESIAN_POINT('',(-6.76699997532778,-0.000577852782592789,109.697179783856));
#210472=CARTESIAN_POINT('Ctrl Pts',(-6.76699997532778,-0.000577852782404293,
109.697179783856));
#210473=CARTESIAN_POINT('Ctrl Pts',(-6.76699458046941,-0.0637548549022476,
109.700160816967));
#210474=CARTESIAN_POINT('Ctrl Pts',(-6.76610444111257,-0.126923442093359,
109.70314185008));
#210475=CARTESIAN_POINT('Ctrl Pts',(-6.76433032192147,-0.190063925913952,
109.706122883192));
#210476=CARTESIAN_POINT('Ctrl Pts',(-6.75938101142591,-0.366208719812691,
109.714439155596));
#210477=CARTESIAN_POINT('Ctrl Pts',(-6.74754229967233,-0.542330844824209,
109.722755428001));
#210478=CARTESIAN_POINT('Ctrl Pts',(-6.72881619087231,-0.717859087464032,
109.731071700405));
#210479=CARTESIAN_POINT('Ctrl Pts',(-6.71010591501938,-0.893238920767603,
109.739380941391));
#210480=CARTESIAN_POINT('Ctrl Pts',(-6.68451988100679,-1.06802552789029,
109.747690182377));
#210481=CARTESIAN_POINT('Ctrl Pts',(-6.65211209900524,-1.2416495569476,
109.755999423363));
#210482=CARTESIAN_POINT('Ctrl Pts',(-6.61972577597116,-1.41515862002568,
109.764303162345));
#210483=CARTESIAN_POINT('Ctrl Pts',(-6.58052676930825,-1.58750629807545,
109.772606901328));
#210484=CARTESIAN_POINT('Ctrl Pts',(-6.53462072003349,-1.75812998532787,
109.78091064031));
#210485=CARTESIAN_POINT('Ctrl Pts',(-6.48873665470299,-1.9286719626164,
109.789210402716));
#210486=CARTESIAN_POINT('Ctrl Pts',(-6.43615203801171,-2.0974912591431,
109.797510165121));
#210487=CARTESIAN_POINT('Ctrl Pts',(-6.37702330088023,-2.26403684157979,
109.805809927527));
#210488=CARTESIAN_POINT('Ctrl Pts',(-6.31791204734133,-2.43053317867066,
109.814107235802));
#210489=CARTESIAN_POINT('Ctrl Pts',(-6.25226064665968,-2.59475681426828,
109.822404544076));
#210490=CARTESIAN_POINT('Ctrl Pts',(-6.18027502077515,-2.75617301118467,
109.830701852351));
#210491=CARTESIAN_POINT('Ctrl Pts',(-6.10828212178721,-2.91760551686656,
109.838999998948));
#210492=CARTESIAN_POINT('Ctrl Pts',(-6.02995385363303,-3.07622969625858,
109.847298145545));
#210493=CARTESIAN_POINT('Ctrl Pts',(-5.94554405206541,-3.23153135911594,
109.855596292142));
#210494=CARTESIAN_POINT('Ctrl Pts',(-5.86112576256122,-3.38684863853249,
109.86389527317));
#210495=CARTESIAN_POINT('Ctrl Pts',(-5.77062488649076,-3.53884242934451,
109.872194254199));
#210496=CARTESIAN_POINT('Ctrl Pts',(-5.67434089733694,-3.68702378359693,
109.880493235227));
#210497=CARTESIAN_POINT('Ctrl Pts',(-5.57803122491292,-3.83524466448086,
109.888794429966));
#210498=CARTESIAN_POINT('Ctrl Pts',(-5.47593555446037,-3.97965079007181,
109.897095624706));
#210499=CARTESIAN_POINT('Ctrl Pts',(-5.368396401207,-4.11978264954691,109.905396819445));
#210500=CARTESIAN_POINT('Ctrl Pts',(-5.26081068853162,-4.25997517956092,
109.913701608214));
#210501=CARTESIAN_POINT('Ctrl Pts',(-5.1477770077279,-4.39588947936302,
109.922006396982));
#210502=CARTESIAN_POINT('Ctrl Pts',(-5.02967792567021,-4.527099398514,109.930311185751));
#210503=CARTESIAN_POINT('Ctrl Pts',(-4.9114388382113,-4.65846486584584,
109.938625819772));
#210504=CARTESIAN_POINT('Ctrl Pts',(-4.78812258470138,-4.78511455081905,
109.946940453793));
#210505=CARTESIAN_POINT('Ctrl Pts',(-4.6601491752623,-4.90665860482489,
109.955255087814));
#210506=CARTESIAN_POINT('Ctrl Pts',(-4.53209484710205,-5.02827951221346,
109.963574979252));
#210507=CARTESIAN_POINT('Ctrl Pts',(-4.39937775159597,-5.14478812126722,
109.971894870689));
#210508=CARTESIAN_POINT('Ctrl Pts',(-4.26245079713221,-5.25583506229286,
109.980214762127));
#210509=CARTESIAN_POINT('Ctrl Pts',(-4.12531909247298,-5.36704805450229,
109.9885470945));
#210510=CARTESIAN_POINT('Ctrl Pts',(-3.98396522669826,-5.47278284874803,
109.996879426874));
#210511=CARTESIAN_POINT('Ctrl Pts',(-3.83887199634723,-5.57273279420977,
110.005211759247));
#210512=CARTESIAN_POINT('Ctrl Pts',(-3.72963352942183,-5.64798357458803,
110.011485044445));
#210513=CARTESIAN_POINT('Ctrl Pts',(-3.6182760621482,-5.71995619617045,
110.017758329644));
#210514=CARTESIAN_POINT('Ctrl Pts',(-3.50501443822741,-5.78853718894656,
110.024031614842));
#210515=CARTESIAN_POINT('Ctrl Pts',(-3.35931663649457,-5.87675859653582,
110.032101460845));
#210516=CARTESIAN_POINT('Ctrl Pts',(-3.21001676095259,-5.95963842679075,
110.040171306848));
#210517=CARTESIAN_POINT('Ctrl Pts',(-3.05755125178259,-6.03685922833411,
110.04824115285));
#210518=CARTESIAN_POINT('Ctrl Pts',(-2.90527756361614,-6.11398287628695,
110.056300845961));
#210519=CARTESIAN_POINT('Ctrl Pts',(-2.74984649503231,-6.18546149549647,
110.064360539071));
#210520=CARTESIAN_POINT('Ctrl Pts',(-2.59172408469217,-6.25102033821892,
110.072420232181));
#210521=CARTESIAN_POINT('Ctrl Pts',(-2.43376590958989,-6.31651108767043,
110.080471554019));
#210522=CARTESIAN_POINT('Ctrl Pts',(-2.27312229729032,-6.37609415478897,
110.088522875858));
#210523=CARTESIAN_POINT('Ctrl Pts',(-2.11028446764011,-6.42954029971326,
110.096574197696));
#210524=CARTESIAN_POINT('Ctrl Pts',(-1.94758008762283,-6.48294264419857,
110.104618921278));
#210525=CARTESIAN_POINT('Ctrl Pts',(-1.7826854219628,-6.53021796077703,
110.112663644859));
#210526=CARTESIAN_POINT('Ctrl Pts',(-1.6161121872759,-6.57118485496629,
110.12070836844));
#210527=CARTESIAN_POINT('Ctrl Pts',(-1.44963900052513,-6.61212714344251,
110.128748260164));
#210528=CARTESIAN_POINT('Ctrl Pts',(-1.28148961312893,-6.64676846336198,
110.136788151888));
#210529=CARTESIAN_POINT('Ctrl Pts',(-1.11219133697324,-6.67497711081931,
110.144828043613));
#210530=CARTESIAN_POINT('Ctrl Pts',(-0.939247605108738,-6.70379316773908,
110.153041056233));
#210531=CARTESIAN_POINT('Ctrl Pts',(-0.76510532443646,-6.72589625912002,
110.161254068853));
#210532=CARTESIAN_POINT('Ctrl Pts',(-0.590338581657058,-6.74120088404189,
110.169467081473));
#210533=CARTESIAN_POINT('Ctrl Pts',(-0.419315413730825,-6.75617767766082,
110.177504168015));
#210534=CARTESIAN_POINT('Ctrl Pts',(-0.247694653530352,-6.76464428539989,
110.185541254558));
#210535=CARTESIAN_POINT('Ctrl Pts',(-0.0760198752609056,-6.76657298627343,
110.1935783411));
#210536=CARTESIAN_POINT('Ctrl Pts',(0.095671333083986,-6.76850187173262,
110.20161619683));
#210537=CARTESIAN_POINT('Ctrl Pts',(0.267416196179675,-6.76389160011226,
110.209654052559));
#210538=CARTESIAN_POINT('Ctrl Pts',(0.438671077303047,-6.75276659495483,
110.217691908288));
#210539=CARTESIAN_POINT('Ctrl Pts',(0.609976279625294,-6.74163832084767,
110.225732125845));
#210540=CARTESIAN_POINT('Ctrl Pts',(0.78079084076752,-6.72399152711062,
110.233772343402));
#210541=CARTESIAN_POINT('Ctrl Pts',(0.950576331654277,-6.69990250956674,
110.241812560959));
#210542=CARTESIAN_POINT('Ctrl Pts',(1.12677642717072,-6.67490339350587,
110.250156543087));
#210543=CARTESIAN_POINT('Ctrl Pts',(1.30186773512499,-6.64296582534395,
110.258500525214));
#210544=CARTESIAN_POINT('Ctrl Pts',(1.47526128317876,-6.60423297184115,
110.266844507342));
#210545=CARTESIAN_POINT('Ctrl Pts',(1.64263327243482,-6.56684522118322,
110.274898722177));
#210546=CARTESIAN_POINT('Ctrl Pts',(1.80842310476819,-6.52312640021052,
110.282952937012));
#210547=CARTESIAN_POINT('Ctrl Pts',(1.97211815467876,-6.47325567114311,
110.291007151847));
#210548=CARTESIAN_POINT('Ctrl Pts',(2.13593570326556,-6.42334762208162,
110.29906739393));
#210549=CARTESIAN_POINT('Ctrl Pts',(2.29765499757764,-6.36727861993701,
110.307127636013));
#210550=CARTESIAN_POINT('Ctrl Pts',(2.45678429351917,-6.30527556377337,
110.315187878096));
#210551=CARTESIAN_POINT('Ctrl Pts',(2.61613606313192,-6.24318582308409,
110.323259388951));
#210552=CARTESIAN_POINT('Ctrl Pts',(2.77289027039732,-6.17514562334383,
110.331330899805));
#210553=CARTESIAN_POINT('Ctrl Pts',(2.92658010087692,-6.10142753076288,
110.339402410659));
#210554=CARTESIAN_POINT('Ctrl Pts',(2.94268839976087,-6.09370110498218,
110.34024838927));
#210555=CARTESIAN_POINT('Ctrl Pts',(2.95876306269006,-6.08591234500733,
110.341094367881));
#210556=CARTESIAN_POINT('Ctrl Pts',(2.97480357148381,-6.07806159158388,
110.341940346492));
#210557=CARTESIAN_POINT('Ctrl Pts',(3.13083748424129,-6.00169345448138,
110.350169596228));
#210558=CARTESIAN_POINT('Ctrl Pts',(3.2841580440009,-5.91920076592815,110.358398845964));
#210559=CARTESIAN_POINT('Ctrl Pts',(3.43425069767606,-5.83079849982072,
110.3666280957));
#210560=CARTESIAN_POINT('Ctrl Pts',(3.58416471667626,-5.74250144679124,
110.37484755129));
#210561=CARTESIAN_POINT('Ctrl Pts',(3.73085817330173,-5.64830900130154,
110.38306700688));
#210562=CARTESIAN_POINT('Ctrl Pts',(3.8738377741439,-5.54848356757194,110.39128646247));
#210563=CARTESIAN_POINT('Ctrl Pts',(4.01667591982277,-5.44875689494495,
110.399497786239));
#210564=CARTESIAN_POINT('Ctrl Pts',(4.15580723487193,-5.3434085363126,110.407709110009));
#210565=CARTESIAN_POINT('Ctrl Pts',(4.29076419683617,-5.2327460866307,110.415920433779));
#210566=CARTESIAN_POINT('Ctrl Pts',(4.42561473361974,-5.12217090381542,
110.424125282213));
#210567=CARTESIAN_POINT('Ctrl Pts',(4.55629719779224,-5.00629020304635,
110.432330130647));
#210568=CARTESIAN_POINT('Ctrl Pts',(4.68237410674298,-4.88545409603886,
110.440534979081));
#210569=CARTESIAN_POINT('Ctrl Pts',(4.8083768968647,-4.76468902686717,110.448735004001));
#210570=CARTESIAN_POINT('Ctrl Pts',(4.92977926722306,-4.63897460236606,
110.456935028921));
#210571=CARTESIAN_POINT('Ctrl Pts',(5.04617775972311,-4.50870036898394,
110.465135053841));
#210572=CARTESIAN_POINT('Ctrl Pts',(5.1625425638624,-4.37846383991634,110.473332705488));
#210573=CARTESIAN_POINT('Ctrl Pts',(5.27390613322989,-4.24367039513359,
110.481530357135));
#210574=CARTESIAN_POINT('Ctrl Pts',(5.37990259028466,-4.10474568262742,
110.489728008782));
#210575=CARTESIAN_POINT('Ctrl Pts',(5.48588485376347,-3.96583957299265,
110.497924562713));
#210576=CARTESIAN_POINT('Ctrl Pts',(5.58650121808187,-3.8228035820166,110.506121116644));
#210577=CARTESIAN_POINT('Ctrl Pts',(5.68142676034186,-3.67609561448984,
110.514317670575));
#210578=CARTESIAN_POINT('Ctrl Pts',(5.77635685141951,-3.52938061673941,
110.522514617283));
#210579=CARTESIAN_POINT('Ctrl Pts',(5.86559538219838,-3.37899359307046,
110.530711563992));
#210580=CARTESIAN_POINT('Ctrl Pts',(5.94886132904145,-3.22542057534132,
110.538908510701));
#210581=CARTESIAN_POINT('Ctrl Pts',(6.03214640585528,-3.07181227491323,
110.547107340621));
#210582=CARTESIAN_POINT('Ctrl Pts',(6.10945599481781,-2.91501683787723,
110.55530617054));
#210583=CARTESIAN_POINT('Ctrl Pts',(6.18055548909299,-2.75554402001539,
110.56350500046));
#210584=CARTESIAN_POINT('Ctrl Pts',(6.25172232367859,-2.59592016100806,
110.57171159572));
#210585=CARTESIAN_POINT('Ctrl Pts',(6.31666716609735,-2.43361418292214,
110.57991819098));
#210586=CARTESIAN_POINT('Ctrl Pts',(6.37520360554201,-2.26915578748664,
110.58812478624));
#210587=CARTESIAN_POINT('Ctrl Pts',(6.43376837695898,-2.10461779324486,
110.596335353539));
#210588=CARTESIAN_POINT('Ctrl Pts',(6.48591845429311,-1.93792564676811,
110.604545920838));
#210589=CARTESIAN_POINT('Ctrl Pts',(6.53151765006207,-1.7696231765344,110.612756488136));
#210590=CARTESIAN_POINT('Ctrl Pts',(6.57717973364994,-1.60108859310017,
110.620978378983));
#210591=CARTESIAN_POINT('Ctrl Pts',(6.61627279960274,-1.43093959721949,
110.62920026983));
#210592=CARTESIAN_POINT('Ctrl Pts',(6.64871178590921,-1.25973036317775,
110.637422160677));
#210593=CARTESIAN_POINT('Ctrl Pts',(6.67820648009823,-1.10406076386633,
110.644897799832));
#210594=CARTESIAN_POINT('Ctrl Pts',(6.70220079846837,-0.947514947705724,
110.652373438986));
#210595=CARTESIAN_POINT('Ctrl Pts',(6.72066816122545,-0.790511522174436,
110.659849078141));
#210596=CARTESIAN_POINT('Ctrl Pts',(6.74274297059785,-0.602838775664545,
110.668785021592));
#210597=CARTESIAN_POINT('Ctrl Pts',(6.75696648332447,-0.414121331288979,
110.677720965043));
#210598=CARTESIAN_POINT('Ctrl Pts',(6.76325812868762,-0.225007743735387,
110.686656908494));
#210599=CARTESIAN_POINT('Ctrl Pts',(6.76954031603903,-0.036178444063279,
110.695579418851));
#210600=CARTESIAN_POINT('Ctrl Pts',(6.76791441933773,0.153045553073953,
110.704501929209));
#210601=CARTESIAN_POINT('Ctrl Pts',(6.75835166428807,0.342011376732841,
110.713424439567));
#210602=CARTESIAN_POINT('Ctrl Pts',(6.74881234095588,0.530514175482277,
110.722325087005));
#210603=CARTESIAN_POINT('Ctrl Pts',(6.73137498658916,0.718759805913537,
110.731225734443));
#210604=CARTESIAN_POINT('Ctrl Pts',(6.70606274514698,0.906096826035595,
110.740126381882));
#210605=CARTESIAN_POINT('Ctrl Pts',(6.68078962064989,1.09314433991435,110.749013274468));
#210606=CARTESIAN_POINT('Ctrl Pts',(6.64766591877159,1.27928578978323,110.757900167054));
#210607=CARTESIAN_POINT('Ctrl Pts',(6.60676653390246,1.46387327542604,110.76678705964));
#210608=CARTESIAN_POINT('Ctrl Pts',(6.56597227571975,1.64798630232613,110.775651109595));
#210609=CARTESIAN_POINT('Ctrl Pts',(6.51744227172776,1.83055308395059,110.78451515955));
#210610=CARTESIAN_POINT('Ctrl Pts',(6.46130242130803,2.01093511093694,110.793379209505));
#210611=CARTESIAN_POINT('Ctrl Pts',(6.4076282081688,2.1833948394643,110.801853954325));
#210612=CARTESIAN_POINT('Ctrl Pts',(6.34699825849784,2.35385733499185,110.810328699146));
#210613=CARTESIAN_POINT('Ctrl Pts',(6.27956660306105,2.52177165455564,110.818803443966));
#210614=CARTESIAN_POINT('Ctrl Pts',(6.21425010079115,2.68441894482156,110.827012358395));
#210615=CARTESIAN_POINT('Ctrl Pts',(6.14261396346791,2.84451826535749,110.835221272824));
#210616=CARTESIAN_POINT('Ctrl Pts',(6.06489446879602,3.0015569430493,110.843430187253));
#210617=CARTESIAN_POINT('Ctrl Pts',(5.98715649670913,3.1586329558889,110.85164105331));
#210618=CARTESIAN_POINT('Ctrl Pts',(5.90333244380904,3.31264655705338,110.859851919367));
#210619=CARTESIAN_POINT('Ctrl Pts',(5.81370476294961,3.46310928635772,110.868062785424));
#210620=CARTESIAN_POINT('Ctrl Pts',(5.72403979705445,3.61363460802397,110.876277067193));
#210621=CARTESIAN_POINT('Ctrl Pts',(5.62856657547765,3.76060580934986,110.884491348963));
#210622=CARTESIAN_POINT('Ctrl Pts',(5.52761115655308,3.90356297527655,110.892705630733));
#210623=CARTESIAN_POINT('Ctrl Pts',(5.42654210433466,4.04668105077916,110.900929158325));
#210624=CARTESIAN_POINT('Ctrl Pts',(5.31997873544013,4.18577577574331,110.909152685918));
#210625=CARTESIAN_POINT('Ctrl Pts',(5.20828832234937,4.32041916384039,110.91737621351));
#210626=CARTESIAN_POINT('Ctrl Pts',(5.09652632004847,4.45514885311172,110.925605012064));
#210627=CARTESIAN_POINT('Ctrl Pts',(4.97963095984321,4.58542125363471,110.933833810618));
#210628=CARTESIAN_POINT('Ctrl Pts',(4.85800667665738,4.710844948579,110.942062609171));
#210629=CARTESIAN_POINT('Ctrl Pts',(4.73621498737851,4.83644127920258,110.950302734008));
#210630=CARTESIAN_POINT('Ctrl Pts',(4.60968163088599,4.95717532873931,110.958542858844));
#210631=CARTESIAN_POINT('Ctrl Pts',(4.47884517990586,5.0726950287233,110.966782983681));
#210632=CARTESIAN_POINT('Ctrl Pts',(4.42075919508984,5.12398100819579,110.970441259051));
#210633=CARTESIAN_POINT('Ctrl Pts',(4.36182547515876,5.17423980228559,110.974099534421));
#210634=CARTESIAN_POINT('Ctrl Pts',(4.3020842137546,5.22344334876559,110.977757809791));
#210635=CARTESIAN_POINT('Ctrl Pts',(4.16411366449314,5.33707737948233,110.986206480781));
#210636=CARTESIAN_POINT('Ctrl Pts',(4.02151831318311,5.44534026955538,110.994655151772));
#210637=CARTESIAN_POINT('Ctrl Pts',(3.87474377772024,5.54785090436092,111.003103822762));
#210638=CARTESIAN_POINT('Ctrl Pts',(3.72812333430209,5.6502539178187,111.011543623869));
#210639=CARTESIAN_POINT('Ctrl Pts',(3.57733272790036,5.74691652811108,111.019983424977));
#210640=CARTESIAN_POINT('Ctrl Pts',(3.42284988151364,5.83749841016013,111.028423226084));
#210641=CARTESIAN_POINT('Ctrl Pts',(3.31662578451512,5.89978350426696,111.034226525754));
#210642=CARTESIAN_POINT('Ctrl Pts',(3.20865666708964,5.9591944014046,111.040029825424));
#210643=CARTESIAN_POINT('Ctrl Pts',(3.09910619832136,6.01563211736939,111.045833125094));
#210644=CARTESIAN_POINT('Ctrl Pts',(3.09910619832136,6.01563211736939,109.045804610872));
#210645=CARTESIAN_POINT('Ctrl Pts',(2.94506703026755,6.09498932060019,109.053971547213));
#210646=CARTESIAN_POINT('Ctrl Pts',(2.78807013938386,6.16837911515625,109.062138483553));
#210647=CARTESIAN_POINT('Ctrl Pts',(2.62860754293066,6.23560032276348,109.070305419894));
#210648=CARTESIAN_POINT('Ctrl Pts',(2.46967645305377,6.3025974746065,109.078445134926));
#210649=CARTESIAN_POINT('Ctrl Pts',(2.30797898013572,6.36360017218061,109.086584849959));
#210650=CARTESIAN_POINT('Ctrl Pts',(2.14401205532608,6.4183721695315,109.094724564992));
#210651=CARTESIAN_POINT('Ctrl Pts',(1.98018853500527,6.47309626362207,109.102857161079));
#210652=CARTESIAN_POINT('Ctrl Pts',(1.8140998585861,6.52160038912026,109.110989757166));
#210653=CARTESIAN_POINT('Ctrl Pts',(1.64626392994504,6.56369591563792,109.119122353253));
#210654=CARTESIAN_POINT('Ctrl Pts',(1.47854274294873,6.60576266339535,109.127249389461));
#210655=CARTESIAN_POINT('Ctrl Pts',(1.30907703569928,6.64142944631574,109.135376425669));
#210656=CARTESIAN_POINT('Ctrl Pts',(1.13840086960319,6.67055713266041,109.143503461877));
#210657=CARTESIAN_POINT('Ctrl Pts',(0.967806289803363,6.69967089544386,
109.151626613215));
#210658=CARTESIAN_POINT('Ctrl Pts',(0.796002763603998,6.72225172468213,
109.159749764552));
#210659=CARTESIAN_POINT('Ctrl Pts',(0.623535550787872,6.73821136629771,
109.16787291589));
#210660=CARTESIAN_POINT('Ctrl Pts',(0.451116802540562,6.75416652313537,
109.175993784561));
#210661=CARTESIAN_POINT('Ctrl Pts',(0.278035103555909,6.76350416537771,
109.184114653233));
#210662=CARTESIAN_POINT('Ctrl Pts',(0.104841824076422,6.76618778869788,
109.192235521905));
#210663=CARTESIAN_POINT('Ctrl Pts',(-0.0683608154309681,6.76887155705133,
109.200356829459));
#210664=CARTESIAN_POINT('Ctrl Pts',(-0.24167468136091,6.76490057840372,
109.208478137014));
#210665=CARTESIAN_POINT('Ctrl Pts',(-0.414547214367548,6.75429045918667,
109.216599444568));
#210666=CARTESIAN_POINT('Ctrl Pts',(-0.504377791882841,6.74877707241437,
109.220819558285));
#210667=CARTESIAN_POINT('Ctrl Pts',(-0.594089216401721,6.74147184052699,
109.225039672002));
#210668=CARTESIAN_POINT('Ctrl Pts',(-0.683604340951769,6.73238249842,109.229259785719));
#210669=CARTESIAN_POINT('Ctrl Pts',(-0.874178147161722,6.71303168446559,
109.238244224245));
#210670=CARTESIAN_POINT('Ctrl Pts',(-1.06376744316211,6.68560121564277,
109.24722866277));
#210671=CARTESIAN_POINT('Ctrl Pts',(-1.25171515143828,6.65022542322137,
109.256213101296));
#210672=CARTESIAN_POINT('Ctrl Pts',(-1.43998724624216,6.61478857429349,
109.265213046427));
#210673=CARTESIAN_POINT('Ctrl Pts',(-1.62661185548438,6.5713790370777,109.274212991557));
#210674=CARTESIAN_POINT('Ctrl Pts',(-1.81094420582182,6.52018175232872,
109.283212936688));
#210675=CARTESIAN_POINT('Ctrl Pts',(-1.99571094007356,6.46886381986429,
109.29223409042));
#210676=CARTESIAN_POINT('Ctrl Pts',(-2.17817437618374,6.40972148465066,
109.301255244152));
#210677=CARTESIAN_POINT('Ctrl Pts',(-2.3577043264137,6.34298977684894,109.310276397884));
#210678=CARTESIAN_POINT('Ctrl Pts',(-2.53741694978348,6.27619016900839,
109.319306730711));
#210679=CARTESIAN_POINT('Ctrl Pts',(-2.71418990258968,6.2017858502352,109.328337063538));
#210680=CARTESIAN_POINT('Ctrl Pts',(-2.8874135043512,6.12005982445354,109.337367396366));
#210681=CARTESIAN_POINT('Ctrl Pts',(-3.0608826825763,6.03821793692909,109.346410531358));
#210682=CARTESIAN_POINT('Ctrl Pts',(-3.23079223220093,5.94903368960606,
109.355453666351));
#210683=CARTESIAN_POINT('Ctrl Pts',(-3.39655550842975,5.85283689147028,
109.364496801343));
#210684=CARTESIAN_POINT('Ctrl Pts',(-3.54147080147756,5.76873872745437,
109.372402584743));
#210685=CARTESIAN_POINT('Ctrl Pts',(-3.68321749238951,5.67928176416991,
109.380308368143));
#210686=CARTESIAN_POINT('Ctrl Pts',(-3.8214214506314,5.58471369871852,109.388214151543));
#210687=CARTESIAN_POINT('Ctrl Pts',(-3.97269456865795,5.48120287089162,
109.396867539771));
#210688=CARTESIAN_POINT('Ctrl Pts',(-4.11985614833642,5.37147606331934,
109.405520928));
#210689=CARTESIAN_POINT('Ctrl Pts',(-4.26239728548914,5.25587845946373,
109.414174316228));
#210690=CARTESIAN_POINT('Ctrl Pts',(-4.40480677579062,5.14038761819514,
109.422819712438));
#210691=CARTESIAN_POINT('Ctrl Pts',(-4.54260409948993,5.01903698596568,
109.431465108649));
#210692=CARTESIAN_POINT('Ctrl Pts',(-4.67531106722114,4.89221375501107,
109.440110504859));
#210693=CARTESIAN_POINT('Ctrl Pts',(-4.81225624846365,4.7613402172778,109.449032005901));
#210694=CARTESIAN_POINT('Ctrl Pts',(-4.94378028079967,4.62463891862904,
109.457953506944));
#210695=CARTESIAN_POINT('Ctrl Pts',(-5.06939464124876,4.48258039205973,
109.466875007986));
#210696=CARTESIAN_POINT('Ctrl Pts',(-5.19088961850813,4.34518051681192,
109.475503938328));
#210697=CARTESIAN_POINT('Ctrl Pts',(-5.30685614307209,4.2027694485995,109.48413286867));
#210698=CARTESIAN_POINT('Ctrl Pts',(-5.41688922042392,4.0558106678758,109.492761799012));
#210699=CARTESIAN_POINT('Ctrl Pts',(-5.53251843540277,3.90137775680674,
109.501829585405));
#210700=CARTESIAN_POINT('Ctrl Pts',(-5.64159469459853,3.74192273199829,
109.510897371797));
#210701=CARTESIAN_POINT('Ctrl Pts',(-5.74369528692449,3.57802367948584,
109.51996515819));
#210702=CARTESIAN_POINT('Ctrl Pts',(-5.84579587925052,3.41412462697329,
109.529032944582));
#210703=CARTESIAN_POINT('Ctrl Pts',(-5.94092056834331,3.2457818596018,109.538100730975));
#210704=CARTESIAN_POINT('Ctrl Pts',(-6.02869878558639,3.07361024735884,
109.547168517368));
#210705=CARTESIAN_POINT('Ctrl Pts',(-6.10946478949627,2.91519266331201,
109.555511918433));
#210706=CARTESIAN_POINT('Ctrl Pts',(-6.18398210624984,2.75359092372838,
109.563855319498));
#210707=CARTESIAN_POINT('Ctrl Pts',(-6.25201121645123,2.58933287728094,
109.572198720563));
#210708=CARTESIAN_POINT('Ctrl Pts',(-6.32005143258252,2.42504801527847,
109.58054348371));
#210709=CARTESIAN_POINT('Ctrl Pts',(-6.38160120048745,2.25810629807558,
109.588888246857));
#210710=CARTESIAN_POINT('Ctrl Pts',(-6.43646945579045,2.08905479695401,
109.597233010004));
#210711=CARTESIAN_POINT('Ctrl Pts',(-6.49138068718608,1.91987088460614,
109.605584309268));
#210712=CARTESIAN_POINT('Ctrl Pts',(-6.53959984126778,1.74857421142531,
109.613935608532));
#210713=CARTESIAN_POINT('Ctrl Pts',(-6.58098568620455,1.57572726002021,
109.622286907796));
#210714=CARTESIAN_POINT('Ctrl Pts',(-6.62238729118817,1.4028144871717,109.630641387298));
#210715=CARTESIAN_POINT('Ctrl Pts',(-6.65695032667952,1.22835059338328,
109.638995866801));
#210716=CARTESIAN_POINT('Ctrl Pts',(-6.68458481328139,1.05290781839997,
109.647350346303));
#210717=CARTESIAN_POINT('Ctrl Pts',(-6.71225178347566,0.87725881517463,
109.655714646271));
#210718=CARTESIAN_POINT('Ctrl Pts',(-6.73297388082621,0.700628970344419,
109.664078946238));
#210719=CARTESIAN_POINT('Ctrl Pts',(-6.74671295041825,0.523596566698737,
109.672443246205));
#210720=CARTESIAN_POINT('Ctrl Pts',(-6.76025690161313,0.349078327393853,
109.68068875874));
#210721=CARTESIAN_POINT('Ctrl Pts',(-6.76701489743579,0.174169205078094,
109.688934271275));
#210722=CARTESIAN_POINT('Ctrl Pts',(-6.76699997532786,-0.000577851814927111,
109.69717978381));
#210723=CARTESIAN_POINT('',(-6.76441351452996,-0.00287859500701793,109.30282021619));
#210724=CARTESIAN_POINT('Ctrl Pts',(3.09910619832125,6.01563211736945,108.651395695404));
#210725=CARTESIAN_POINT('Ctrl Pts',(2.93375330764814,6.10081787314659,108.660145143307));
#210726=CARTESIAN_POINT('Ctrl Pts',(2.76488627843055,6.17918207037046,108.668894591209));
#210727=CARTESIAN_POINT('Ctrl Pts',(2.59307866646684,6.25045854554005,108.677644039111));
#210728=CARTESIAN_POINT('Ctrl Pts',(2.42127244185362,6.32173444515042,108.686393416362));
#210729=CARTESIAN_POINT('Ctrl Pts',(2.24652594672454,6.38592262741842,108.695142793612));
#210730=CARTESIAN_POINT('Ctrl Pts',(2.06943269687114,6.44280508110564,108.703892170862));
#210731=CARTESIAN_POINT('Ctrl Pts',(1.89234081822056,6.49968709436173,108.712641480367));
#210732=CARTESIAN_POINT('Ctrl Pts',(1.71290249405552,6.54926340459555,108.721390789873));
#210733=CARTESIAN_POINT('Ctrl Pts',(1.53172716625007,6.59136563150396,108.730140099378));
#210734=CARTESIAN_POINT('Ctrl Pts',(1.35055318107284,6.6334675464072,108.738889344045));
#210735=CARTESIAN_POINT('Ctrl Pts',(1.16764249714371,6.66809542395784,108.747638588713));
#210736=CARTESIAN_POINT('Ctrl Pts',(0.983616340613883,6.69513165624675,
108.75638783338));
#210737=CARTESIAN_POINT('Ctrl Pts',(0.799591486713338,6.72216769715967,
108.765137016116));
#210738=CARTESIAN_POINT('Ctrl Pts',(0.614451459526177,6.74161215869376,
108.773886198851));
#210739=CARTESIAN_POINT('Ctrl Pts',(0.428825047909717,6.75339900185716,
108.782635381587));
#210740=CARTESIAN_POINT('Ctrl Pts',(0.243199888596486,6.76518576550223,
108.791384505298));
#210741=CARTESIAN_POINT('Ctrl Pts',(0.0570886373913634,6.76931499599835,
108.800133629008));
#210742=CARTESIAN_POINT('Ctrl Pts',(-0.128876626811696,6.76577266947846,
108.808882752719));
#210743=CARTESIAN_POINT('Ctrl Pts',(-0.314840698188805,6.7622303656799,
108.81763182031));
#210744=CARTESIAN_POINT('Ctrl Pts',(-0.500658497951997,6.75101660879218,
108.826380887902));
#210745=CARTESIAN_POINT('Ctrl Pts',(-0.685698951927058,6.7321694829621,
108.835129955493));
#210746=CARTESIAN_POINT('Ctrl Pts',(-0.870738280460756,6.71332247176282,
108.843878969872));
#210747=CARTESIAN_POINT('Ctrl Pts',(-1.05499998761347,6.68684221356171,
108.85262798425));
#210748=CARTESIAN_POINT('Ctrl Pts',(-1.23785829161522,6.65281863948503,
108.861376998629));
#210749=CARTESIAN_POINT('Ctrl Pts',(-1.43007412917492,6.61705395368842,
108.870573732328));
#210750=CARTESIAN_POINT('Ctrl Pts',(-1.62073882535866,6.57295372727771,
108.879770466027));
#210751=CARTESIAN_POINT('Ctrl Pts',(-1.80913696091575,6.52068343478263,
108.888967199726));
#210752=CARTESIAN_POINT('Ctrl Pts',(-1.98838356186176,6.47095219815179,
108.89771719744));
#210753=CARTESIAN_POINT('Ctrl Pts',(-2.16557827572599,6.41382586850869,
108.906467195154));
#210754=CARTESIAN_POINT('Ctrl Pts',(-2.34011918621768,6.34949849943253,
108.915217192867));
#210755=CARTESIAN_POINT('Ctrl Pts',(-2.51465655691162,6.28517243495525,
108.923967013126));
#210756=CARTESIAN_POINT('Ctrl Pts',(-2.68653996295387,6.21364572242349,
108.932716833384));
#210757=CARTESIAN_POINT('Ctrl Pts',(-2.85518555380043,6.13516132252196,
108.941466653642));
#210758=CARTESIAN_POINT('Ctrl Pts',(-3.02382794858735,6.05667841000483,
108.95021630808));
#210759=CARTESIAN_POINT('Ctrl Pts',(-3.1892323910932,5.9712381949206,108.958965962517));
#210760=CARTESIAN_POINT('Ctrl Pts',(-3.35083705967729,5.87913088810695,
108.967715616955));
#210761=CARTESIAN_POINT('Ctrl Pts',(-3.51243888042428,5.78702520443086,
108.976465117204));
#210762=CARTESIAN_POINT('Ctrl Pts',(-3.67024081223716,5.68825280605766,
108.985214617453));
#210763=CARTESIAN_POINT('Ctrl Pts',(-3.82370687544425,5.58314917682488,
108.993964117702));
#210764=CARTESIAN_POINT('Ctrl Pts',(-3.97717043817848,5.47804726007998,
109.002713475392));
#210765=CARTESIAN_POINT('Ctrl Pts',(-4.12629803722502,5.36661448084204,
109.011462833083));
#210766=CARTESIAN_POINT('Ctrl Pts',(-4.27058317206957,5.24922931204536,
109.020212190773));
#210767=CARTESIAN_POINT('Ctrl Pts',(-4.4148661477487,5.1318458998676,109.028961417533));
#210768=CARTESIAN_POINT('Ctrl Pts',(-4.55430658194434,5.00851045723015,
109.037710644293));
#210769=CARTESIAN_POINT('Ctrl Pts',(-4.68843089001853,4.87964187103112,
109.046459871053));
#210770=CARTESIAN_POINT('Ctrl Pts',(-4.82255336917844,4.75077504207952,
109.055208978509));
#210771=CARTESIAN_POINT('Ctrl Pts',(-4.95135966065142,4.61637541908085,
109.063958085965));
#210772=CARTESIAN_POINT('Ctrl Pts',(-5.07441230869252,4.47689945401836,
109.072707193421));
#210773=CARTESIAN_POINT('Ctrl Pts',(-5.19746344226424,4.33742520555507,
109.081456193197));
#210774=CARTESIAN_POINT('Ctrl Pts',(-5.31476088454774,4.19287495491329,
109.090205192974));
#210775=CARTESIAN_POINT('Ctrl Pts',(-5.42590627628859,4.04373961586698,
109.09895419275));
#210776=CARTESIAN_POINT('Ctrl Pts',(-5.53706380672676,3.89458798906722,
109.107704148045));
#210777=CARTESIAN_POINT('Ctrl Pts',(-5.64206777071875,3.74085050155267,
109.11645410334));
#210778=CARTESIAN_POINT('Ctrl Pts',(-5.74056148164021,3.58304938223139,
109.125204058634));
#210779=CARTESIAN_POINT('Ctrl Pts',(-5.83905138951902,3.42525435593252,
109.133953676075));
#210780=CARTESIAN_POINT('Ctrl Pts',(-5.93103139557674,3.26339625497144,
109.142703293517));
#210781=CARTESIAN_POINT('Ctrl Pts',(-6.01618907820871,3.09802485064956,
109.151452910958));
#210782=CARTESIAN_POINT('Ctrl Pts',(-6.10134392545009,2.93265895249588,
109.160202237074));
#210783=CARTESIAN_POINT('Ctrl Pts',(-6.17967677261857,2.76378023985979,
109.168951563189));
#210784=CARTESIAN_POINT('Ctrl Pts',(-6.25092157009249,2.59196229227056,
109.177700889305));
#210785=CARTESIAN_POINT('Ctrl Pts',(-6.3221643740777,2.42014915229047,109.186449970608));
#210786=CARTESIAN_POINT('Ctrl Pts',(-6.38631941548931,2.24539720662823,
109.19519905191));
#210787=CARTESIAN_POINT('Ctrl Pts',(-6.44316881037541,2.06829994947675,
109.203948133213));
#210788=CARTESIAN_POINT('Ctrl Pts',(-6.50002334524578,1.89118668024429,
109.212698005555));
#210789=CARTESIAN_POINT('Ctrl Pts',(-6.54957082411104,1.71172794807672,
109.221447877897));
#210790=CARTESIAN_POINT('Ctrl Pts',(-6.59164294296093,1.530533342503,109.23019775024));
#210791=CARTESIAN_POINT('Ctrl Pts',(-6.63371214082146,1.34935131693542,
109.238947015095));
#210792=CARTESIAN_POINT('Ctrl Pts',(-6.66830695239703,1.16643393829689,
109.247696279949));
#210793=CARTESIAN_POINT('Ctrl Pts',(-6.69530988154002,0.982402458340078,
109.256445544804));
#210794=CARTESIAN_POINT('Ctrl Pts',(-6.72231419690494,0.798361530946127,
109.265195258811));
#210795=CARTESIAN_POINT('Ctrl Pts',(-6.74172580829287,0.613206671361529,
109.273944972818));
#210796=CARTESIAN_POINT('Ctrl Pts',(-6.75347878028186,0.427566795112433,
109.282694686825));
#210797=CARTESIAN_POINT('Ctrl Pts',(-6.7624899236821,0.285234494205859,
109.289403196614));
#210798=CARTESIAN_POINT('Ctrl Pts',(-6.76699999999989,0.142617266094271,
109.296111706402));
#210799=CARTESIAN_POINT('Ctrl Pts',(-6.767,5.13485784531581E-12,109.30282021619));
#210800=CARTESIAN_POINT('Ctrl Pts',(-6.76410475442949,-0.00322222550308449,
109.30282021619));
#210801=CARTESIAN_POINT('Ctrl Pts',(-6.76710928112432,-0.786032822436749,
109.339508609526));
#210802=CARTESIAN_POINT('Ctrl Pts',(-6.2656633635301,-3.8265755522471,109.482166580078));
#210803=CARTESIAN_POINT('Ctrl Pts',(-2.76332679390342,-6.93290299659207,
109.677809339238));
#210804=CARTESIAN_POINT('Ctrl Pts',(1.90804949459011,-6.7813526609264,109.889748493671));
#210805=CARTESIAN_POINT('Ctrl Pts',(4.92590585172162,-5.05725987228767,
110.048702859496));
#210806=CARTESIAN_POINT('Ctrl Pts',(6.73094077380569,-2.07889163802113,
110.207657225321));
#210807=CARTESIAN_POINT('Ctrl Pts',(6.98677885739346,2.33141846444617,110.408528190629));
#210808=CARTESIAN_POINT('Ctrl Pts',(4.880745451628,5.09104750816176,110.556414367328));
#210809=CARTESIAN_POINT('Ctrl Pts',(3.10339103771845,6.02380226238954,110.651315755419));
#210810=CARTESIAN_POINT('Origin',(0.,0.,4.30282021618968));
#210811=CARTESIAN_POINT('',(3.09910619832131,6.01563211736942,113.045755263024));
#210812=CARTESIAN_POINT('',(3.09910619832117,6.01563211736949,112.651476300929));
#210813=CARTESIAN_POINT('',(3.09910619832133,6.0156321173694,4.30282021618968));
#210814=CARTESIAN_POINT('',(-6.767,5.13019531370174E-12,111.69717978381));
#210815=CARTESIAN_POINT('Ctrl Pts',(-6.767,5.13019525665479E-12,111.69717978381));
#210816=CARTESIAN_POINT('Ctrl Pts',(-6.76700000000014,-0.186007249521703,
111.705929295621));
#210817=CARTESIAN_POINT('Ctrl Pts',(-6.75932637294549,-0.372014355744713,
111.714678807432));
#210818=CARTESIAN_POINT('Ctrl Pts',(-6.74400518264224,-0.557389537482261,
111.723428319244));
#210819=CARTESIAN_POINT('Ctrl Pts',(-6.72868405705143,-0.742763936246609,
111.732177794099));
#210820=CARTESIAN_POINT('Ctrl Pts',(-6.70571545645796,-0.927506130237137,
111.740927268955));
#210821=CARTESIAN_POINT('Ctrl Pts',(-6.67517739404886,-1.11098863989653,
111.749676743811));
#210822=CARTESIAN_POINT('Ctrl Pts',(-6.64463945808768,-1.29447038981606,
111.758426182438));
#210823=CARTESIAN_POINT('Ctrl Pts',(-6.60653217008427,-1.47669218313364,
111.767175621065));
#210824=CARTESIAN_POINT('Ctrl Pts',(-6.56098496092752,-1.65703510598988,
111.775925059692));
#210825=CARTESIAN_POINT('Ctrl Pts',(-6.51543793658381,-1.83737729708399,
111.784674462817));
#210826=CARTESIAN_POINT('Ctrl Pts',(-6.46245112167515,-2.01584035510623,
111.793423865942));
#210827=CARTESIAN_POINT('Ctrl Pts',(-6.40220448374358,-2.19181813760486,
111.802173269067));
#210828=CARTESIAN_POINT('Ctrl Pts',(-6.34195808526619,-2.36779522066834,
111.810922637417));
#210829=CARTESIAN_POINT('Ctrl Pts',(-6.2744520143323,-2.54128677683853,
111.819672005767));
#210830=CARTESIAN_POINT('Ctrl Pts',(-6.1999155507204,-2.71170355384496,
111.828421374117));
#210831=CARTESIAN_POINT('Ctrl Pts',(-6.1253793771684,-2.88211966767162,
111.837170708419));
#210832=CARTESIAN_POINT('Ctrl Pts',(-6.04381298052679,-3.04946076371471,
111.845920042721));
#210833=CARTESIAN_POINT('Ctrl Pts',(-5.95549339336001,-3.21315848374233,
111.854669377023));
#210834=CARTESIAN_POINT('Ctrl Pts',(-5.86717414255591,-3.37685558033177,
111.863418678003));
#210835=CARTESIAN_POINT('Ctrl Pts',(-5.77210188876792,-3.53690907646439,
111.872167978983));
#210836=CARTESIAN_POINT('Ctrl Pts',(-5.67059953347203,-3.69277536968969,
111.880917279963));
#210837=CARTESIAN_POINT('Ctrl Pts',(-5.56909755631601,-3.84864108224608,
111.889666548349));
#210838=CARTESIAN_POINT('Ctrl Pts',(-5.46116568197078,-4.00031938297205,
111.898415816734));
#210839=CARTESIAN_POINT('Ctrl Pts',(-5.34717048533842,-4.14729511859546,
111.907165085119));
#210840=CARTESIAN_POINT('Ctrl Pts',(-5.23317570392075,-4.29427031887627,
111.915914321636));
#210841=CARTESIAN_POINT('Ctrl Pts',(-5.1131178200375,-4.43654276189275,
111.924663558153));
#210842=CARTESIAN_POINT('Ctrl Pts',(-4.98740458984986,-4.57362924351598,
111.93341279467));
#210843=CARTESIAN_POINT('Ctrl Pts',(-4.86169180711989,-4.71071523720012,
111.942162000046));
#210844=CARTESIAN_POINT('Ctrl Pts',(-4.73032391204432,-4.84261509522984,
111.950911205421));
#210845=CARTESIAN_POINT('Ctrl Pts',(-4.59374707013873,-4.96888084538077,
111.959660410797));
#210846=CARTESIAN_POINT('Ctrl Pts',(-4.45717070301713,-5.0951461565923,
111.968409585757));
#210847=CARTESIAN_POINT('Ctrl Pts',(-4.31538563571302,-5.21577720459312,
111.977158760717));
#210848=CARTESIAN_POINT('Ctrl Pts',(-4.16887341029762,-5.33036429232688,
111.985907935678));
#210849=CARTESIAN_POINT('Ctrl Pts',(-4.02236168203969,-5.44495099123422,
111.99465708095));
#210850=CARTESIAN_POINT('Ctrl Pts',(-3.87112305348437,-5.55349359438412,
112.003406226222));
#210851=CARTESIAN_POINT('Ctrl Pts',(-3.71567117018042,-5.65562346298709,
112.012155371494));
#210852=CARTESIAN_POINT('Ctrl Pts',(-3.56021980146096,-5.75775299351473,
112.020904487804));
#210853=CARTESIAN_POINT('Ctrl Pts',(-3.40055544538622,-5.85346967463715,
112.029653604114));
#210854=CARTESIAN_POINT('Ctrl Pts',(-3.2372203598712,-5.94244842986756,
112.038402720425));
#210855=CARTESIAN_POINT('Ctrl Pts',(-3.0738858014747,-6.0314268979438,112.047151808499));
#210856=CARTESIAN_POINT('Ctrl Pts',(-2.90688078896892,-6.11366734656631,
112.055900896574));
#210857=CARTESIAN_POINT('Ctrl Pts',(-2.73677250721709,-6.18889046952204,
112.064649984649));
#210858=CARTESIAN_POINT('Ctrl Pts',(-2.56666476031853,-6.26411335596174,
112.073399045215));
#210859=CARTESIAN_POINT('Ctrl Pts',(-2.39345402575568,-6.33231884500403,
112.082148105781));
#210860=CARTESIAN_POINT('Ctrl Pts',(-2.21772856066027,-6.39327529762576,
112.090897166347));
#210861=CARTESIAN_POINT('Ctrl Pts',(-2.04200363348964,-6.45423156364968,
112.099646200131));
#210862=CARTESIAN_POINT('Ctrl Pts',(-1.86376426189743,-6.50793874375525,
112.108395233914));
#210863=CARTESIAN_POINT('Ctrl Pts',(-1.68361577753633,-6.55421443909419,
112.117144267698));
#210864=CARTESIAN_POINT('Ctrl Pts',(-1.5034678296826,-6.60048999661764,
112.125893275426));
#210865=CARTESIAN_POINT('Ctrl Pts',(-1.32141105795429,-6.63933404237625,
112.134642283154));
#210866=CARTESIAN_POINT('Ctrl Pts',(-1.13806375487444,-6.67061465607489,
112.143391290882));
#210867=CARTESIAN_POINT('Ctrl Pts',(-0.954716982607419,-6.70189517921233,
112.15214027328));
#210868=CARTESIAN_POINT('Ctrl Pts',(-0.770079968906719,-6.72561226592175,
112.160889255678));
#210869=CARTESIAN_POINT('Ctrl Pts',(-0.584779765563001,-6.74168536983061,
112.169638238077));
#210870=CARTESIAN_POINT('Ctrl Pts',(-0.391489830656095,-6.75845151013825,
112.178764457087));
#210871=CARTESIAN_POINT('Ctrl Pts',(-0.197478578243166,-6.76689983031611,
112.187890676097));
#210872=CARTESIAN_POINT('Ctrl Pts',(-0.00346287645620368,-6.76699911397117,
112.197016895106));
#210873=CARTESIAN_POINT('Ctrl Pts',(0.184489834650012,-6.76709529501202,
112.205857919772));
#210874=CARTESIAN_POINT('Ctrl Pts',(0.37244640424559,-6.75935639738189,
112.214698944438));
#210875=CARTESIAN_POINT('Ctrl Pts',(0.559755019484654,-6.74380925873217,
112.223539969104));
#210876=CARTESIAN_POINT('Ctrl Pts',(0.745134705518054,-6.72842222659847,
112.232289947714));
#210877=CARTESIAN_POINT('Ctrl Pts',(0.929879431224811,-6.70538706057576,
112.241039926323));
#210878=CARTESIAN_POINT('Ctrl Pts',(1.11336163626447,-6.6747820089419,112.249789904933));
#210879=CARTESIAN_POINT('Ctrl Pts',(1.29684196300358,-6.64417727061084,
112.25853979397));
#210880=CARTESIAN_POINT('Ctrl Pts',(1.47905951217168,-6.60600284890667,
112.267289683006));
#210881=CARTESIAN_POINT('Ctrl Pts',(1.6593953206676,-6.56038841607313,112.276039572043));
#210882=CARTESIAN_POINT('Ctrl Pts',(1.83972934300479,-6.51477443503348,
112.284789374415));
#210883=CARTESIAN_POINT('Ctrl Pts',(2.01818138405944,-6.46172066062241,
112.293539176787));
#210884=CARTESIAN_POINT('Ctrl Pts',(2.19414528353881,-6.40140730423588,
112.302288979159));
#210885=CARTESIAN_POINT('Ctrl Pts',(2.37010749863671,-6.34109452518765,
112.311038697776));
#210886=CARTESIAN_POINT('Ctrl Pts',(2.54358134866121,-6.27352239616641,
112.319788416392));
#210887=CARTESIAN_POINT('Ctrl Pts',(2.71397759435208,-6.19892043966971,
112.328538135008));
#210888=CARTESIAN_POINT('Ctrl Pts',(2.88437226557786,-6.12431917249674,
112.337287772777));
#210889=CARTESIAN_POINT('Ctrl Pts',(3.05168912680628,-6.04268832278964,
112.346037410546));
#210890=CARTESIAN_POINT('Ctrl Pts',(3.21535986273536,-5.95430516123506,
112.354787048314));
#210891=CARTESIAN_POINT('Ctrl Pts',(3.37902914072545,-5.86592278697612,
112.363536608143));
#210892=CARTESIAN_POINT('Ctrl Pts',(3.53905210621295,-5.77078835742112,
112.372286167972));
#210893=CARTESIAN_POINT('Ctrl Pts',(3.6948852283144,-5.66922500431797,112.381035727801));
#210894=CARTESIAN_POINT('Ctrl Pts',(3.85071701406703,-5.56766252217258,
112.389785212599));
#210895=CARTESIAN_POINT('Ctrl Pts',(4.00235878822186,-5.45967138329531,
112.398534697396));
#210896=CARTESIAN_POINT('Ctrl Pts',(4.14929549611125,-5.34561838199762,
112.407284182193));
#210897=CARTESIAN_POINT('Ctrl Pts',(4.29623099275899,-5.23156632087172,
112.416033594865));
#210898=CARTESIAN_POINT('Ctrl Pts',(4.43846127435846,-5.11145267305122,
112.424783007538));
#210899=CARTESIAN_POINT('Ctrl Pts',(4.5755032605427,-4.98568540050043,112.433532420211));
#210900=CARTESIAN_POINT('Ctrl Pts',(4.71254416257609,-4.85991912290527,
112.442281763666));
#210901=CARTESIAN_POINT('Ctrl Pts',(4.84439664018591,-4.72849950385593,
112.451031107121));
#210902=CARTESIAN_POINT('Ctrl Pts',(4.97061286794577,-4.5918728986125,112.459780450576));
#210903=CARTESIAN_POINT('Ctrl Pts',(5.09682813912523,-4.45524732884869,
112.468529727721));
#210904=CARTESIAN_POINT('Ctrl Pts',(5.21740705147685,-4.31341506235974,
112.477279004866));
#210905=CARTESIAN_POINT('Ctrl Pts',(5.33194007545549,-4.16685781275912,
112.486028282011));
#210906=CARTESIAN_POINT('Ctrl Pts',(5.44647226944338,-4.02030162522041,
112.494777495752));
#210907=CARTESIAN_POINT('Ctrl Pts',(5.55495848627966,-3.86902074888145,
112.503526709493));
#210908=CARTESIAN_POINT('Ctrl Pts',(5.65703027291642,-3.71352898080885,
112.512275923234));
#210909=CARTESIAN_POINT('Ctrl Pts',(5.75910135376856,-3.55803828789817,
112.521025076478));
#210910=CARTESIAN_POINT('Ctrl Pts',(5.85475793592616,-3.39833700106948,
112.529774229722));
#210911=CARTESIAN_POINT('Ctrl Pts',(5.94367514427267,-3.23496750823795,
112.538523382966));
#210912=CARTESIAN_POINT('Ctrl Pts',(6.03259176732513,-3.07159909077973,
112.547272478619));
#210913=CARTESIAN_POINT('Ctrl Pts',(6.11476896835803,-2.90456276731689,
112.556021574272));
#210914=CARTESIAN_POINT('Ctrl Pts',(6.1899276554777,-2.73442583003312,112.564770669925));
#210915=CARTESIAN_POINT('Ctrl Pts',(6.26508587282948,-2.56428995616429,
112.573519710893));
#210916=CARTESIAN_POINT('Ctrl Pts',(6.33322554827064,-2.39105376935457,
112.582268751861));
#210917=CARTESIAN_POINT('Ctrl Pts',(6.39411526732943,-2.21530561054331,
112.591017792829));
#210918=CARTESIAN_POINT('Ctrl Pts',(6.45500462602756,-2.03955849185385,
112.599766782018));
#210919=CARTESIAN_POINT('Ctrl Pts',(6.50864402040647,-1.86129970164867,
112.608515771207));
#210920=CARTESIAN_POINT('Ctrl Pts',(6.55485128368509,-1.68113463136417,
112.617264760396));
#210921=CARTESIAN_POINT('Ctrl Pts',(6.60199809554242,-1.49730620117239,
112.626191645867));
#210922=CARTESIAN_POINT('Ctrl Pts',(6.64140720707798,-1.3114934324608,112.635118531339));
#210923=CARTESIAN_POINT('Ctrl Pts',(6.67293928722817,-1.12435326697919,
112.64404541681));
#210924=CARTESIAN_POINT('Ctrl Pts',(6.70384625876201,-0.940923067010568,
112.652795330988));
#210925=CARTESIAN_POINT('Ctrl Pts',(6.72718554579751,-0.756217899525683,
112.661545245165));
#210926=CARTESIAN_POINT('Ctrl Pts',(6.74287786815293,-0.570865181258552,
112.670295159342));
#210927=CARTESIAN_POINT('Ctrl Pts',(6.75856988190823,-0.385516108077956,
112.679044901447));
#210928=CARTESIAN_POINT('Ctrl Pts',(6.76661520773391,-0.199519795230309,
112.687794643551));
#210929=CARTESIAN_POINT('Ctrl Pts',(6.76698651789578,-0.0135080204595548,
112.696544385656));
#210930=CARTESIAN_POINT('Ctrl Pts',(6.76735782124913,0.17250034350898,112.705293967321));
#210931=CARTESIAN_POINT('Ctrl Pts',(6.76005538995205,0.358523882206871,
112.714043548986));
#210932=CARTESIAN_POINT('Ctrl Pts',(6.74510402742394,0.543930748560262,
112.722793130651));
#210933=CARTESIAN_POINT('Ctrl Pts',(6.73015291918076,0.729334461610996,
112.731542563507));
#210934=CARTESIAN_POINT('Ctrl Pts',(6.70755316306654,0.914121237630324,
112.740291996364));
#210935=CARTESIAN_POINT('Ctrl Pts',(6.67738151874648,1.09766345165675,112.749041429221));
#210936=CARTESIAN_POINT('Ctrl Pts',(6.64721034747655,1.28120278799219,112.757790724898));
#210937=CARTESIAN_POINT('Ctrl Pts',(6.6094675720524,1.46349731859886,112.766540020576));
#210938=CARTESIAN_POINT('Ctrl Pts',(6.56428138111633,1.64392790277722,112.775289316253));
#210939=CARTESIAN_POINT('Ctrl Pts',(6.51909583859973,1.82435589778615,112.784038486379));
#210940=CARTESIAN_POINT('Ctrl Pts',(6.46646716393012,2.00291972191823,112.792787656505));
#210941=CARTESIAN_POINT('Ctrl Pts',(6.40657409873034,2.17901292274222,112.80153682663));
#210942=CARTESIAN_POINT('Ctrl Pts',(6.34668181342244,2.35510383058525,112.810285882829));
#210943=CARTESIAN_POINT('Ctrl Pts',(6.27952541914236,2.52872390822118,112.819034939028));
#210944=CARTESIAN_POINT('Ctrl Pts',(6.20533299175721,2.69928350889815,112.827783995228));
#210945=CARTESIAN_POINT('Ctrl Pts',(6.12831602991758,2.8763363796518,112.836866131386));
#210946=CARTESIAN_POINT('Ctrl Pts',(6.04371690605481,3.05009086601045,112.845948267544));
#210947=CARTESIAN_POINT('Ctrl Pts',(5.95184520316843,3.21991112882343,112.855030403702));
#210948=CARTESIAN_POINT('Ctrl Pts',(5.86333549509495,3.38351691182634,112.863780184046));
#210949=CARTESIAN_POINT('Ctrl Pts',(5.76807618099598,3.5434710371163,112.872529964389));
#210950=CARTESIAN_POINT('Ctrl Pts',(5.66639083309254,3.6992301802733,112.881279744733));
#210951=CARTESIAN_POINT('Ctrl Pts',(5.56470914082445,3.85498372381696,112.890029210518));
#210952=CARTESIAN_POINT('Ctrl Pts',(5.45660203372318,4.00654234701656,112.898778676303));
#210953=CARTESIAN_POINT('Ctrl Pts',(5.34243669839474,4.15339127986338,112.907528142088));
#210954=CARTESIAN_POINT('Ctrl Pts',(5.22827486050852,4.30023571400963,112.916277339834));
#210955=CARTESIAN_POINT('Ctrl Pts',(5.10805534167375,4.44237052028167,112.92502653758));
#210956=CARTESIAN_POINT('Ctrl Pts',(4.98218644340217,4.57931296628432,112.933775735326));
#210957=CARTESIAN_POINT('Ctrl Pts',(4.85632073219849,4.71625194483091,112.942524711537));
#210958=CARTESIAN_POINT('Ctrl Pts',(4.72480612170577,4.84799861524257,112.951273687749));
#210959=CARTESIAN_POINT('Ctrl Pts',(4.58808925235564,4.97410554898252,112.960022663961));
#210960=CARTESIAN_POINT('Ctrl Pts',(4.45136349474301,5.10022068120986,112.968772208962));
#210961=CARTESIAN_POINT('Ctrl Pts',(4.30943501210333,5.22069514871626,112.977521753964));
#210962=CARTESIAN_POINT('Ctrl Pts',(4.16278587432033,5.33511975166061,112.986271298966));
#210963=CARTESIAN_POINT('Ctrl Pts',(4.016145357407,5.44953762807657,112.995020329619));
#210964=CARTESIAN_POINT('Ctrl Pts',(3.86478496658175,5.55790617532609,113.003769360273));
#210965=CARTESIAN_POINT('Ctrl Pts',(3.70921874747447,5.65985735539191,113.012518390927));
#210966=CARTESIAN_POINT('Ctrl Pts',(3.55365041606161,5.76180991976885,113.021267540376));
#210967=CARTESIAN_POINT('Ctrl Pts',(3.39387638174793,5.85734478552657,113.030016689826));
#210968=CARTESIAN_POINT('Ctrl Pts',(3.23043927904818,5.9461374912108,113.038765839276));
#210969=CARTESIAN_POINT('Ctrl Pts',(3.18691767070615,5.9697820694405,113.041095647192));
#210970=CARTESIAN_POINT('Ctrl Pts',(3.1431364591972,5.9929488063338,113.043425455108));
#210971=CARTESIAN_POINT('Ctrl Pts',(3.09910619832131,6.01563211736942,113.045755263024));
#210972=CARTESIAN_POINT('Ctrl Pts',(3.09910619832136,6.01563211736939,111.045833125094));
#210973=CARTESIAN_POINT('Ctrl Pts',(2.93996722179409,6.09761661690788,111.054263314215));
#210974=CARTESIAN_POINT('Ctrl Pts',(2.77749027747824,6.17332502379726,111.062693503336));
#210975=CARTESIAN_POINT('Ctrl Pts',(2.61219945089555,6.24249173237266,111.071123692456));
#210976=CARTESIAN_POINT('Ctrl Pts',(2.44699166283165,6.31162369309696,111.079549646433));
#210977=CARTESIAN_POINT('Ctrl Pts',(2.27897311824067,6.37422037982185,111.08797560041));
#210978=CARTESIAN_POINT('Ctrl Pts',(2.10868962993586,6.43006353348091,111.096401554387));
#210979=CARTESIAN_POINT('Ctrl Pts',(1.93845430658069,6.48589089181705,111.10482512507));
#210980=CARTESIAN_POINT('Ctrl Pts',(1.76595563272836,6.53496841996684,111.113248695752));
#210981=CARTESIAN_POINT('Ctrl Pts',(1.59175688308495,6.57712695826618,111.121672266435));
#210982=CARTESIAN_POINT('Ctrl Pts',(1.41758542984143,6.61927889045427,111.13009451717));
#210983=CARTESIAN_POINT('Ctrl Pts',(1.24171475585187,6.65451391558974,111.138516767906));
#210984=CARTESIAN_POINT('Ctrl Pts',(1.06472103315279,6.68271338017441,111.146939018641));
#210985=CARTESIAN_POINT('Ctrl Pts',(0.887730337138724,6.71091236253352,
111.155361125352));
#210986=CARTESIAN_POINT('Ctrl Pts',(0.709616960052614,6.73207597198672,
111.163783232063));
#210987=CARTESIAN_POINT('Ctrl Pts',(0.530965317924063,6.74613703026864,
111.172205338773));
#210988=CARTESIAN_POINT('Ctrl Pts',(0.352291791994926,6.76019981094948,
111.180628477143));
#210989=CARTESIAN_POINT('Ctrl Pts',(0.173080202039716,6.76715828029015,
111.189051615514));
#210990=CARTESIAN_POINT('Ctrl Pts',(-0.0060815151668908,6.7669972672651,
111.197474753884));
#210991=CARTESIAN_POINT('Ctrl Pts',(-0.185361193648259,6.76683614822799,
111.205903438105));
#210992=CARTESIAN_POINT('Ctrl Pts',(-0.364590599861592,6.75954617843287,
111.214332122326));
#210993=CARTESIAN_POINT('Ctrl Pts',(-0.543182331353419,6.74516433861366,
111.222760806547));
#210994=CARTESIAN_POINT('Ctrl Pts',(-0.721830655650253,6.73077794142413,
111.231192161681));
#210995=CARTESIAN_POINT('Ctrl Pts',(-0.899840570268462,6.70929522590876,
111.239623516814));
#210996=CARTESIAN_POINT('Ctrl Pts',(-1.07663080166935,6.68080497521794,
111.248054871948));
#210997=CARTESIAN_POINT('Ctrl Pts',(-1.25359503468112,6.65228668367059,
111.256494525444));
#210998=CARTESIAN_POINT('Ctrl Pts',(-1.42933685649182,6.61674713144458,
111.264934178939));
#210999=CARTESIAN_POINT('Ctrl Pts',(-1.60328490953062,6.57432631521066,
111.273373832435));
#211000=CARTESIAN_POINT('Ctrl Pts',(-1.75644180277676,6.53697585161046,
111.280804735437));
#211001=CARTESIAN_POINT('Ctrl Pts',(-1.90820813575328,6.4942915777034,111.288235638438));
#211002=CARTESIAN_POINT('Ctrl Pts',(-2.05820434700911,6.44640084589477,
111.29566654144));
#211003=CARTESIAN_POINT('Ctrl Pts',(-2.22250825668757,6.39394195771593,
111.303806256473));
#211004=CARTESIAN_POINT('Ctrl Pts',(-2.38501544551448,6.33513026296877,
111.311945971506));
#211005=CARTESIAN_POINT('Ctrl Pts',(-2.54519477728016,6.27010945245024,
111.320085686539));
#211006=CARTESIAN_POINT('Ctrl Pts',(-2.70523401716352,6.20514550874239,
111.328218282626));
#211007=CARTESIAN_POINT('Ctrl Pts',(-2.86294911549623,6.13398339534557,
111.336350878713));
#211008=CARTESIAN_POINT('Ctrl Pts',(-3.01782396863838,6.05681661389147,
111.3444834748));
#211009=CARTESIAN_POINT('Ctrl Pts',(-3.1725929410222,5.97970258778901,111.352610511008));
#211010=CARTESIAN_POINT('Ctrl Pts',(-3.3245252076969,5.8965922293451,111.360737547216));
#211011=CARTESIAN_POINT('Ctrl Pts',(-3.47312458013503,5.80772715017345,
111.368864583424));
#211012=CARTESIAN_POINT('Ctrl Pts',(-3.62165291938359,5.71890455011804,
111.376987734761));
#211013=CARTESIAN_POINT('Ctrl Pts',(-3.7668512233192,5.62433289475613,111.385110886099));
#211014=CARTESIAN_POINT('Ctrl Pts',(-3.90824788262623,5.52429972828662,
111.393234037436));
#211015=CARTESIAN_POINT('Ctrl Pts',(-4.04960480842116,5.42429467188032,
111.401354906108));
#211016=CARTESIAN_POINT('Ctrl Pts',(-4.18716191917053,5.31883137320026,
111.40947577478));
#211017=CARTESIAN_POINT('Ctrl Pts',(-4.32047661703014,5.20824066280504,
111.417596643451));
#211018=CARTESIAN_POINT('Ctrl Pts',(-4.45379851972622,5.09764397566459,
111.425717951006));
#211019=CARTESIAN_POINT('Ctrl Pts',(-4.58287726707774,4.98191955396713,
111.43383925856));
#211020=CARTESIAN_POINT('Ctrl Pts',(-4.70730324607933,4.86143858846855,
111.441960566115));
#211021=CARTESIAN_POINT('Ctrl Pts',(-4.77195931004163,4.79883249065824,
111.446180679832));
#211022=CARTESIAN_POINT('Ctrl Pts',(-4.83535960185525,4.73494267065707,
111.450400793548));
#211023=CARTESIAN_POINT('Ctrl Pts',(-4.89745054546376,4.66982517389428,
111.454620907265));
#211024=CARTESIAN_POINT('Ctrl Pts',(-5.02963946341902,4.53119285593014,
111.463605345791));
#211025=CARTESIAN_POINT('Ctrl Pts',(-5.15582619695452,4.38706291435779,
111.472589784317));
#211026=CARTESIAN_POINT('Ctrl Pts',(-5.27559894187177,4.23796470071679,
111.481574222843));
#211027=CARTESIAN_POINT('Ctrl Pts',(-5.3955784073981,4.08860915245797,111.490574167973));
#211028=CARTESIAN_POINT('Ctrl Pts',(-5.50912160836431,3.9342683794576,111.499574113104));
#211029=CARTESIAN_POINT('Ctrl Pts',(-5.61585899953535,3.77550217816622,
111.508574058234));
#211030=CARTESIAN_POINT('Ctrl Pts',(-5.72284792010836,3.61636184024636,
111.517595211966));
#211031=CARTESIAN_POINT('Ctrl Pts',(-5.82299880745891,3.45277540714538,
111.526616365699));
#211032=CARTESIAN_POINT('Ctrl Pts',(-5.91598577023615,3.28533124149808,
111.535637519431));
#211033=CARTESIAN_POINT('Ctrl Pts',(-6.00906734798116,3.11771670009207,
111.544667852258));
#211034=CARTESIAN_POINT('Ctrl Pts',(-6.09497032815903,2.94623679604312,
111.553698185085));
#211035=CARTESIAN_POINT('Ctrl Pts',(-6.17341559597288,2.77150300007033,
111.562728517913));
#211036=CARTESIAN_POINT('Ctrl Pts',(-6.25197207444889,2.5965214866546,111.571771652905));
#211037=CARTESIAN_POINT('Ctrl Pts',(-6.32304960230133,2.41827707563771,
111.580814787898));
#211038=CARTESIAN_POINT('Ctrl Pts',(-6.38641700203635,2.2374018137342,111.589857922891));
#211039=CARTESIAN_POINT('Ctrl Pts',(-6.44181470839864,2.07927516361074,
111.59776370629));
#211040=CARTESIAN_POINT('Ctrl Pts',(-6.49132044455546,1.91913817615428,
111.60566948969));
#211041=CARTESIAN_POINT('Ctrl Pts',(-6.53481107523639,1.75742232003802,
111.61357527309));
#211042=CARTESIAN_POINT('Ctrl Pts',(-6.58497038076436,1.57090961813762,
111.622693296875));
#211043=CARTESIAN_POINT('Ctrl Pts',(-6.62716167707037,1.38216962683381,
111.631811320661));
#211044=CARTESIAN_POINT('Ctrl Pts',(-6.66121233591839,1.19186375723432,
111.640929344446));
#211045=CARTESIAN_POINT('Ctrl Pts',(-6.69622292896478,0.99619290738016,
111.650304417674));
#211046=CARTESIAN_POINT('Ctrl Pts',(-6.7226270800968,0.798866808204857,
111.659679490901));
#211047=CARTESIAN_POINT('Ctrl Pts',(-6.74029265815554,0.600619582110436,
111.669054564128));
#211048=CARTESIAN_POINT('Ctrl Pts',(-6.75795823621427,0.402372356016142,
111.678429637355));
#211049=CARTESIAN_POINT('Ctrl Pts',(-6.76688515647705,0.203204251837742,
111.687804710583));
#211050=CARTESIAN_POINT('Ctrl Pts',(-6.76699889844774,0.00386114065237677,
111.69717978381));
#211051=CARTESIAN_POINT('',(-6.77219403443551,-0.00312713327445556,111.302818667387));
#211052=CARTESIAN_POINT('Ctrl Pts',(3.10339103771845,6.02380226238954,110.651315755419));
#211053=CARTESIAN_POINT('Ctrl Pts',(2.89610118462354,6.13258787907032,110.662383944544));
#211054=CARTESIAN_POINT('Ctrl Pts',(0.642912696893712,7.1623602499167,110.779421710886));
#211055=CARTESIAN_POINT('Ctrl Pts',(-4.56900862909321,6.49795736804409,
110.996589297456));
#211056=CARTESIAN_POINT('Ctrl Pts',(-6.75983703898571,2.11762530079817,
111.202688694898));
#211057=CARTESIAN_POINT('Ctrl Pts',(-6.77270472585136,-0.00312414668946661,
111.302818515126));
#211058=CARTESIAN_POINT('Ctrl Pts',(-6.76699926334503,-0.00315751292227859,
111.30282021619));
#211059=CARTESIAN_POINT('Ctrl Pts',(-6.7669416052657,-0.126726977238388,
111.308659406158));
#211060=CARTESIAN_POINT('Ctrl Pts',(-6.76349934956323,-0.250225686892749,
111.314498596126));
#211061=CARTESIAN_POINT('Ctrl Pts',(-6.75668362546576,-0.373517583739894,
111.320337786094));
#211062=CARTESIAN_POINT('Ctrl Pts',(-6.74625325319796,-0.562196051842372,
111.329273729545));
#211063=CARTESIAN_POINT('Ctrl Pts',(-6.72790872944149,-0.750557567481397,
111.338209672996));
#211064=CARTESIAN_POINT('Ctrl Pts',(-6.70168187751392,-0.937949365691698,
111.347145616446));
#211065=CARTESIAN_POINT('Ctrl Pts',(-6.67549445150109,-1.12505946432645,
111.356068126804));
#211066=CARTESIAN_POINT('Ctrl Pts',(-6.64144837630606,-1.311202499104,111.364990637162));
#211067=CARTESIAN_POINT('Ctrl Pts',(-6.59962724468697,-1.49573033371176,
111.373913147519));
#211068=CARTESIAN_POINT('Ctrl Pts',(-6.55790858781864,-1.67980601786048,
111.382813794957));
#211069=CARTESIAN_POINT('Ctrl Pts',(-6.50845295450852,-1.86227414942701,
111.391714442396));
#211070=CARTESIAN_POINT('Ctrl Pts',(-6.45139484191311,-2.04249690176923,
111.400615089834));
#211071=CARTESIAN_POINT('Ctrl Pts',(-6.3944249055886,-2.22244114209082,
111.40950198242));
#211072=CARTESIAN_POINT('Ctrl Pts',(-6.32987600308755,-2.40014667990826,
111.418388875006));
#211073=CARTESIAN_POINT('Ctrl Pts',(-6.25793300836317,-2.57498805100892,
111.427275767593));
#211074=CARTESIAN_POINT('Ctrl Pts',(-6.18617493399066,-2.74938001451971,
111.436139817548));
#211075=CARTESIAN_POINT('Ctrl Pts',(-6.10706078966566,-2.92092226356557,
111.445003867503));
#211076=CARTESIAN_POINT('Ctrl Pts',(-6.02082408885677,-3.08900733101137,
111.453867917457));
#211077=CARTESIAN_POINT('Ctrl Pts',(-5.93837486561982,-3.24971017699978,
111.462342662278));
#211078=CARTESIAN_POINT('Ctrl Pts',(-5.8494153568189,-3.40725273941956,
111.470817407098));
#211079=CARTESIAN_POINT('Ctrl Pts',(-5.75419177662111,-3.56111864417153,
111.479292151919));
#211080=CARTESIAN_POINT('Ctrl Pts',(-5.66195510896502,-3.71015818134007,
111.487501066348));
#211081=CARTESIAN_POINT('Ctrl Pts',(-5.56392926635857,-3.85560391963464,
111.495709980777));
#211082=CARTESIAN_POINT('Ctrl Pts',(-5.46043493019616,-3.9969912900948,
111.503918895206));
#211083=CARTESIAN_POINT('Ctrl Pts',(-5.3569159887812,-4.13841227468388,
111.512129761263));
#211084=CARTESIAN_POINT('Ctrl Pts',(-5.24792617395999,-4.27577268183795,
111.52034062732));
#211085=CARTESIAN_POINT('Ctrl Pts',(-5.13382750693869,-4.40863971412949,
111.528551493377));
#211086=CARTESIAN_POINT('Ctrl Pts',(-5.0196813749727,-4.54156201898908,
111.536765775147));
#211087=CARTESIAN_POINT('Ctrl Pts',(-4.90042238859834,-4.669986955145,111.544980056916));
#211088=CARTESIAN_POINT('Ctrl Pts',(-4.77645063442172,-4.79351732415064,
111.553194338686));
#211089=CARTESIAN_POINT('Ctrl Pts',(-4.65233934024955,-4.91718673633799,
111.561417866279));
#211090=CARTESIAN_POINT('Ctrl Pts',(-4.5235049355893,-5.03595032620794,
111.569641393871));
#211091=CARTESIAN_POINT('Ctrl Pts',(-4.39038263637481,-5.14944941777455,
111.577864921463));
#211092=CARTESIAN_POINT('Ctrl Pts',(-4.25717501094456,-5.26302125784408,
111.586093720017));
#211093=CARTESIAN_POINT('Ctrl Pts',(-4.11967429125731,-5.37132165332404,
111.594322518571));
#211094=CARTESIAN_POINT('Ctrl Pts',(-3.97834603516961,-5.47403432802995,
111.602551317124));
#211095=CARTESIAN_POINT('Ctrl Pts',(-3.83682325204705,-5.57688837851312,
111.610791441961));
#211096=CARTESIAN_POINT('Ctrl Pts',(-3.69146270466835,-5.67413914863146,
111.619031566797));
#211097=CARTESIAN_POINT('Ctrl Pts',(-3.5427568364995,-5.7655149811128,111.627271691634));
#211098=CARTESIAN_POINT('Ctrl Pts',(-3.47673756789631,-5.80608207979363,
111.630929967004));
#211099=CARTESIAN_POINT('Ctrl Pts',(-3.41005923886211,-5.84549185225258,
111.634588242374));
#211100=CARTESIAN_POINT('Ctrl Pts',(-3.34276625935395,-5.88372354341405,
111.638246517744));
#211101=CARTESIAN_POINT('Ctrl Pts',(-3.18736718051395,-5.97201164764738,
111.646694540506));
#211102=CARTESIAN_POINT('Ctrl Pts',(-3.02833327895385,-6.05421611942821,
111.655142563269));
#211103=CARTESIAN_POINT('Ctrl Pts',(-2.86616880205378,-6.13003796057852,
111.663590586031));
#211104=CARTESIAN_POINT('Ctrl Pts',(-2.70415282400838,-6.2057903694044,
111.672030872687));
#211105=CARTESIAN_POINT('Ctrl Pts',(-2.53901228559528,-6.27517165736614,
111.680471159343));
#211106=CARTESIAN_POINT('Ctrl Pts',(-2.37127647446706,-6.33792843771836,
111.688911445999));
#211107=CARTESIAN_POINT('Ctrl Pts',(-2.20366844204516,-6.40063741086619,
111.697345302967));
#211108=CARTESIAN_POINT('Ctrl Pts',(-2.03346938941416,-6.45673182006865,
111.705779159935));
#211109=CARTESIAN_POINT('Ctrl Pts',(-1.86122941383928,-6.50600599977125,
111.714213016902));
#211110=CARTESIAN_POINT('Ctrl Pts',(-1.6890941691114,-6.55525021821452,
111.722641745647));
#211111=CARTESIAN_POINT('Ctrl Pts',(-1.51492079549191,-6.59768238376883,
111.731070474393));
#211112=CARTESIAN_POINT('Ctrl Pts',(-1.33927579284736,-6.63314626332731,
111.739499203138));
#211113=CARTESIAN_POINT('Ctrl Pts',(-1.16371061892958,-6.6685940249416,
111.747924101118));
#211114=CARTESIAN_POINT('Ctrl Pts',(-0.986675476022788,-6.69707974970367,
111.756348999098));
#211115=CARTESIAN_POINT('Ctrl Pts',(-0.808748720862408,-6.71849793529055,
111.764773897078));
#211116=CARTESIAN_POINT('Ctrl Pts',(-0.630861358975024,-6.73991137885631,
111.773196929773));
#211117=CARTESIAN_POINT('Ctrl Pts',(-0.45208310891277,-6.75426036064216,
111.781619962467));
#211118=CARTESIAN_POINT('Ctrl Pts',(-0.272999678763831,-6.76149097281028,
111.790042995161));
#211119=CARTESIAN_POINT('Ctrl Pts',(-0.0939365117016369,-6.76872076684283,
111.798465074798));
#211120=CARTESIAN_POINT('Ctrl Pts',(0.0854314334736309,-6.76883378348118,
111.806887154436));
#211121=CARTESIAN_POINT('Ctrl Pts',(0.264515882139856,-6.76182818090609,
111.815309234074));
#211122=CARTESIAN_POINT('Ctrl Pts',(0.443605066455603,-6.75482239307718,
111.823731536422));
#211123=CARTESIAN_POINT('Ctrl Pts',(0.622410406113715,-6.74069762414627,
111.83215383877));
#211124=CARTESIAN_POINT('Ctrl Pts',(0.800345813124003,-6.71950411707701,
111.840576141118));
#211125=CARTESIAN_POINT('Ctrl Pts',(0.978310765296193,-6.69830709094649,
111.848999841942));
#211126=CARTESIAN_POINT('Ctrl Pts',(1.1554051658182,-6.67003902665602,111.857423542766));
#211127=CARTESIAN_POINT('Ctrl Pts',(1.33104984743644,-6.634801828513,111.865847243589));
#211128=CARTESIAN_POINT('Ctrl Pts',(1.50681338941625,-6.5995407850359,111.874276644808));
#211129=CARTESIAN_POINT('Ctrl Pts',(1.68112492485148,-6.55730124950671,
111.882706046027));
#211130=CARTESIAN_POINT('Ctrl Pts',(1.85341625176118,-6.50823610494484,
111.891135447246));
#211131=CARTESIAN_POINT('Ctrl Pts',(2.02576905197698,-6.45915345400754,
111.899567856064));
#211132=CARTESIAN_POINT('Ctrl Pts',(2.1960998874038,-6.40324043528048,111.908000264882));
#211133=CARTESIAN_POINT('Ctrl Pts',(2.36385689412829,-6.34069945542936,
111.916432673699));
#211134=CARTESIAN_POINT('Ctrl Pts',(2.53176911451663,-6.27810061084393,
111.924872884427));
#211135=CARTESIAN_POINT('Ctrl Pts',(2.69710243777705,-6.20886167498664,
111.933313095154));
#211136=CARTESIAN_POINT('Ctrl Pts',(2.8593250855342,-6.13323316491676,111.941753305882));
#211137=CARTESIAN_POINT('Ctrl Pts',(2.95159455939098,-6.09021695892334,
111.946553953719));
#211138=CARTESIAN_POINT('Ctrl Pts',(3.04285810585875,-6.04513449256421,
111.951354601556));
#211139=CARTESIAN_POINT('Ctrl Pts',(3.13302154779196,-5.99803842777547,
111.956155249393));
#211140=CARTESIAN_POINT('Ctrl Pts',(3.28589773213795,-5.91818492475652,
111.964294964426));
#211141=CARTESIAN_POINT('Ctrl Pts',(3.43591455379587,-5.83238075773,111.972434679459));
#211142=CARTESIAN_POINT('Ctrl Pts',(3.58257337921973,-5.74085855796031,
111.980574394492));
#211143=CARTESIAN_POINT('Ctrl Pts',(3.72910393771476,-5.64941640295745,
111.988706990579));
#211144=CARTESIAN_POINT('Ctrl Pts',(3.872282037274,-5.55226636213545,111.996839586666));
#211145=CARTESIAN_POINT('Ctrl Pts',(4.01163239484831,-5.44968756247582,
112.004972182753));
#211146=CARTESIAN_POINT('Ctrl Pts',(4.15088748504222,-5.34717889118685,
112.013099218961));
#211147=CARTESIAN_POINT('Ctrl Pts',(4.2863197495549,-5.23924906645606,112.021226255169));
#211148=CARTESIAN_POINT('Ctrl Pts',(4.41748177444461,-5.12622119815851,
112.029353291377));
#211149=CARTESIAN_POINT('Ctrl Pts',(4.54858110151278,-5.01324735922749,
112.037476442714));
#211150=CARTESIAN_POINT('Ctrl Pts',(4.67541397693466,-4.89518056806295,
112.045599594052));
#211151=CARTESIAN_POINT('Ctrl Pts',(4.79756507756997,-4.77238497257724,
112.053722745389));
#211152=CARTESIAN_POINT('Ctrl Pts',(4.91968185283819,-4.64962388356646,
112.061843614061));
#211153=CARTESIAN_POINT('Ctrl Pts',(5.03711921628153,-4.52213689696127,
112.069964482733));
#211154=CARTESIAN_POINT('Ctrl Pts',(5.14949784846359,-4.39032583172011,
112.078085351404));
#211155=CARTESIAN_POINT('Ctrl Pts',(5.26188255401701,-4.25850764290454,
112.086206658959));
#211156=CARTESIAN_POINT('Ctrl Pts',(5.36920774149492,-4.12236518469301,
112.094327966513));
#211157=CARTESIAN_POINT('Ctrl Pts',(5.47113350797286,-3.98233438298902,
112.102449274068));
#211158=CARTESIAN_POINT('Ctrl Pts',(5.52409767935999,-3.90956951069805,
112.106669387785));
#211159=CARTESIAN_POINT('Ctrl Pts',(5.57560456872712,-3.83575524073842,
112.110889501501));
#211160=CARTESIAN_POINT('Ctrl Pts',(5.62561100293929,-3.76095597469692,
112.115109615218));
#211161=CARTESIAN_POINT('Ctrl Pts',(5.73207252607099,-3.60171159110169,
112.124094053744));
#211162=CARTESIAN_POINT('Ctrl Pts',(5.83167813022279,-3.43808012896981,
112.13307849227));
#211163=CARTESIAN_POINT('Ctrl Pts',(5.9241128718985,-3.2706537085125,112.142062930796));
#211164=CARTESIAN_POINT('Ctrl Pts',(6.01670715042143,-3.10293832004621,
112.151062875926));
#211165=CARTESIAN_POINT('Ctrl Pts',(6.10210571370995,-2.93141509105327,
112.160062821056));
#211166=CARTESIAN_POINT('Ctrl Pts',(6.18004047149519,-2.75669889010054,
112.169062766187));
#211167=CARTESIAN_POINT('Ctrl Pts',(6.25815888453759,-2.58157096593562,
112.178083919919));
#211168=CARTESIAN_POINT('Ctrl Pts',(6.32877820230573,-2.40323523398682,
112.187105073651));
#211169=CARTESIAN_POINT('Ctrl Pts',(6.39167823989611,-2.22232722109923,
112.196126227384));
#211170=CARTESIAN_POINT('Ctrl Pts',(6.45464227877061,-2.04123513288232,
112.205156560211));
#211171=CARTESIAN_POINT('Ctrl Pts',(6.50987127351077,-1.85756576244736,
112.214186893038));
#211172=CARTESIAN_POINT('Ctrl Pts',(6.55719508516186,-1.67196938223437,
112.223217225865));
#211173=CARTESIAN_POINT('Ctrl Pts',(6.60458598706047,-1.48610988485787,
112.232260360858));
#211174=CARTESIAN_POINT('Ctrl Pts',(6.64404923801519,-1.29831814689144,
112.241303495851));
#211175=CARTESIAN_POINT('Ctrl Pts',(6.67546545442912,-1.10925649275693,
112.250346630843));
#211176=CARTESIAN_POINT('Ctrl Pts',(6.70293046544743,-0.943973049788264,
112.258252414243));
#211177=CARTESIAN_POINT('Ctrl Pts',(6.7242460679943,-0.777719274635746,
112.266158197643));
#211178=CARTESIAN_POINT('Ctrl Pts',(6.73936492970172,-0.610941359138955,
112.274063981043));
#211179=CARTESIAN_POINT('Ctrl Pts',(6.75591349589758,-0.428392207753313,
112.282717369271));
#211180=CARTESIAN_POINT('Ctrl Pts',(6.76505125333847,-0.245053711462206,
112.2913707575));
#211181=CARTESIAN_POINT('Ctrl Pts',(6.76672018542856,-0.0615380541914957,
112.300024145728));
#211182=CARTESIAN_POINT('Ctrl Pts',(6.76838757614148,0.121808113351996,
112.308669541938));
#211183=CARTESIAN_POINT('Ctrl Pts',(6.76259989693947,0.305330812575991,
112.317314938149));
#211184=CARTESIAN_POINT('Ctrl Pts',(6.74935107993639,0.488414782496964,
112.325960334359));
#211185=CARTESIAN_POINT('Ctrl Pts',(6.73567914034827,0.677345837679467,
112.334881835401));
#211186=CARTESIAN_POINT('Ctrl Pts',(6.71406156928113,0.865809353393924,
112.343803336444));
#211187=CARTESIAN_POINT('Ctrl Pts',(6.68454996728575,1.05312902099413,112.352724837486));
#211188=CARTESIAN_POINT('Ctrl Pts',(6.65600616544271,1.23430574851037,112.361353767828));
#211189=CARTESIAN_POINT('Ctrl Pts',(6.62007790720542,1.41441212660026,112.36998269817));
#211190=CARTESIAN_POINT('Ctrl Pts',(6.57686455678845,1.59284073330005,112.378611628512));
#211191=CARTESIAN_POINT('Ctrl Pts',(6.53145343219199,1.78034398431475,112.387679414905));
#211192=CARTESIAN_POINT('Ctrl Pts',(6.47799690861243,1.96599401890645,112.396747201297));
#211193=CARTESIAN_POINT('Ctrl Pts',(6.41667141943653,2.1490967625927,112.40581498769));
#211194=CARTESIAN_POINT('Ctrl Pts',(6.35534593026067,2.33219950627884,112.414882774083));
#211195=CARTESIAN_POINT('Ctrl Pts',(6.28615156612699,2.51275457758295,112.423950560475));
#211196=CARTESIAN_POINT('Ctrl Pts',(6.2093263287872,2.69008467201873,112.433018346868));
#211197=CARTESIAN_POINT('Ctrl Pts',(6.13794735860817,2.85484354502542,112.441443303001));
#211198=CARTESIAN_POINT('Ctrl Pts',(6.06001263660661,3.01674628271946,112.449868259134));
#211199=CARTESIAN_POINT('Ctrl Pts',(5.9757836028002,3.17526366346234,112.458293215267));
#211200=CARTESIAN_POINT('Ctrl Pts',(5.89153501862637,3.33381783761118,112.466720126914));
#211201=CARTESIAN_POINT('Ctrl Pts',(5.80098936528815,3.48898479525786,112.47514703856));
#211202=CARTESIAN_POINT('Ctrl Pts',(5.70445366342969,3.64026062278289,112.483573950207));
#211203=CARTESIAN_POINT('Ctrl Pts',(5.60788246163335,3.79159208032226,112.492003960757));
#211204=CARTESIAN_POINT('Ctrl Pts',(5.50531699749254,3.93902927521756,112.500433971307));
#211205=CARTESIAN_POINT('Ctrl Pts',(5.39710737483285,4.08209762065104,112.508863981857));
#211206=CARTESIAN_POINT('Ctrl Pts',(5.2887980717319,4.22529775765215,112.517301757956));
#211207=CARTESIAN_POINT('Ctrl Pts',(5.17483442258572,4.36412073994748,112.525739534055));
#211208=CARTESIAN_POINT('Ctrl Pts',(5.05560725332516,4.49812453141596,112.534177310155));
#211209=CARTESIAN_POINT('Ctrl Pts',(4.9363174985895,4.63219866499695,112.542619515465));
#211210=CARTESIAN_POINT('Ctrl Pts',(4.81175893933917,4.76144832026906,112.551061720775));
#211211=CARTESIAN_POINT('Ctrl Pts',(4.68235934424135,4.8854682448457,112.559503926085));
#211212=CARTESIAN_POINT('Ctrl Pts',(4.55282323969055,5.00961900361892,112.567955037457));
#211213=CARTESIAN_POINT('Ctrl Pts',(4.41843614209166,5.12852878730048,112.576406148829));
#211214=CARTESIAN_POINT('Ctrl Pts',(4.27965977847555,5.24183185351253,112.584857260201));
#211215=CARTESIAN_POINT('Ctrl Pts',(4.24071197706516,5.2736305345489,112.587229077698));
#211216=CARTESIAN_POINT('Ctrl Pts',(4.20141863738297,5.30498785735915,112.589600895195));
#211217=CARTESIAN_POINT('Ctrl Pts',(4.16179038218708,5.33589634595118,112.591972712692));
#211218=CARTESIAN_POINT('Ctrl Pts',(4.02282528575888,5.44428368413728,112.600290006642));
#211219=CARTESIAN_POINT('Ctrl Pts',(3.87948861439683,5.54734401221526,112.608607300593));
#211220=CARTESIAN_POINT('Ctrl Pts',(3.73222217648751,5.64471492861552,112.616924594543));
#211221=CARTESIAN_POINT('Ctrl Pts',(3.58509593048532,5.74199315169974,112.625233970754));
#211222=CARTESIAN_POINT('Ctrl Pts',(3.43404766322085,5.8335925672391,112.633543346964));
#211223=CARTESIAN_POINT('Ctrl Pts',(3.2795507336467,5.9191921733829,112.641852723175));
#211224=CARTESIAN_POINT('Ctrl Pts',(3.21990673724492,5.95223815439306,112.645060582426));
#211225=CARTESIAN_POINT('Ctrl Pts',(3.15974908850186,5.98439038696173,112.648268441677));
#211226=CARTESIAN_POINT('Ctrl Pts',(3.09910619832117,6.01563211736949,112.651476300929));
#211227=CARTESIAN_POINT('Origin',(0.,0.,4.30282021618968));
#211228=CARTESIAN_POINT('',(3.09910619832124,6.01563211736945,115.045544419485));
#211229=CARTESIAN_POINT('',(3.09910619832145,6.01563211736935,114.651477942722));
#211230=CARTESIAN_POINT('',(3.09910619832133,6.0156321173694,4.30282021618968));
#211231=CARTESIAN_POINT('',(-6.76699958356027,-0.0015344574147271,113.69717978381));
#211232=CARTESIAN_POINT('Ctrl Pts',(-6.76699900317075,-0.00367302138866391,
113.69717978381));
#211233=CARTESIAN_POINT('Ctrl Pts',(-6.76689437423714,-0.196436366462953,
113.706228878238));
#211234=CARTESIAN_POINT('Ctrl Pts',(-6.75854901500553,-0.389028701790154,
113.715277972666));
#211235=CARTESIAN_POINT('Ctrl Pts',(-6.74203162654055,-0.58077409267894,
113.724327067093));
#211236=CARTESIAN_POINT('Ctrl Pts',(-6.72548378829893,-0.772872965859097,
113.733392843511));
#211237=CARTESIAN_POINT('Ctrl Pts',(-6.70073382333768,-0.964121546945956,
113.742458619928));
#211238=CARTESIAN_POINT('Ctrl Pts',(-6.66790201356897,-1.15385082980553,
113.751524396346));
#211239=CARTESIAN_POINT('Ctrl Pts',(-6.63499621702891,-1.34400766926847,
113.76061060257));
#211240=CARTESIAN_POINT('Ctrl Pts',(-6.59397217635658,-1.53263813607671,
113.769696808794));
#211241=CARTESIAN_POINT('Ctrl Pts',(-6.54500142042759,-1.71908272244265,
113.778783015018));
#211242=CARTESIAN_POINT('Ctrl Pts',(-6.49598097478889,-1.90571649064166,
113.787878440846));
#211243=CARTESIAN_POINT('Ctrl Pts',(-6.43899776506071,-2.09015972871107,
113.796973866673));
#211244=CARTESIAN_POINT('Ctrl Pts',(-6.37427315611694,-2.27176819486651,
113.806069292501));
#211245=CARTESIAN_POINT('Ctrl Pts',(-6.30947624815692,-2.45357952224675,
113.815174878148));
#211246=CARTESIAN_POINT('Ctrl Pts',(-6.23692073063983,-2.63254953413714,
113.824280463795));
#211247=CARTESIAN_POINT('Ctrl Pts',(-6.15687675812367,-2.80805227609397,
113.833386049442));
#211248=CARTESIAN_POINT('Ctrl Pts',(-6.14061305305923,-2.84371173605658,
113.835236164507));
#211249=CARTESIAN_POINT('Ctrl Pts',(-6.12404035022347,-2.879228126544,113.837086279572));
#211250=CARTESIAN_POINT('Ctrl Pts',(-6.1071611522584,-2.91459631172927,
113.838936394636));
#211251=CARTESIAN_POINT('Ctrl Pts',(-6.02821349340788,-3.08002096187836,
113.847589782865));
#211252=CARTESIAN_POINT('Ctrl Pts',(-5.9424902228326,-3.2423417052089,113.856243171093));
#211253=CARTESIAN_POINT('Ctrl Pts',(-5.85025392639332,-3.40100249878172,
113.864896559321));
#211254=CARTESIAN_POINT('Ctrl Pts',(-5.75810281671668,-3.55951675785693,
113.873541955532));
#211255=CARTESIAN_POINT('Ctrl Pts',(-5.6594508309726,-3.71437754718037,
113.882187351742));
#211256=CARTESIAN_POINT('Ctrl Pts',(-5.55460679741111,-3.86505269383929,
113.890832747952));
#211257=CARTESIAN_POINT('Ctrl Pts',(-5.44641439859597,-4.02053989711718,
113.899754248995));
#211258=CARTESIAN_POINT('Ctrl Pts',(-5.33162803129022,-4.17156938435437,
113.908675750037));
#211259=CARTESIAN_POINT('Ctrl Pts',(-5.21063727443873,-4.31758592204368,
113.91759725108));
#211260=CARTESIAN_POINT('Ctrl Pts',(-5.09361427484186,-4.45881400983989,
113.926226181421));
#211261=CARTESIAN_POINT('Ctrl Pts',(-4.97078756366853,-4.59535245201296,
113.934855111763));
#211262=CARTESIAN_POINT('Ctrl Pts',(-4.84255263117004,-4.72672963203398,
113.943484042105));
#211263=CARTESIAN_POINT('Ctrl Pts',(-4.70779583862508,-4.86478848267864,
113.952551828498));
#211264=CARTESIAN_POINT('Ctrl Pts',(-4.56706657312259,-4.99714712081148,
113.961619614891));
#211265=CARTESIAN_POINT('Ctrl Pts',(-4.42087082812759,-5.12329875383141,
113.970687401283));
#211266=CARTESIAN_POINT('Ctrl Pts',(-4.27467508313269,-5.24945038685125,
113.979755187676));
#211267=CARTESIAN_POINT('Ctrl Pts',(-4.12301313130337,-5.36939473298295,
113.988822974069));
#211268=CARTESIAN_POINT('Ctrl Pts',(-3.96643535015231,-5.48267084668249,
113.997890760461));
#211269=CARTESIAN_POINT('Ctrl Pts',(-3.82095762488303,-5.58791663077274,
114.006315716594));
#211270=CARTESIAN_POINT('Ctrl Pts',(-3.67130032260777,-5.68736012850898,
114.014740672728));
#211271=CARTESIAN_POINT('Ctrl Pts',(-3.51795839032686,-5.78067969739968,
114.023165628861));
#211272=CARTESIAN_POINT('Ctrl Pts',(-3.36458086591139,-5.87402092665819,
114.031592540507));
#211273=CARTESIAN_POINT('Ctrl Pts',(-3.20751728954559,-5.9612352205724,
114.040019452154));
#211274=CARTESIAN_POINT('Ctrl Pts',(-3.04728888604715,-6.04204596514902,
114.0484463638));
#211275=CARTESIAN_POINT('Ctrl Pts',(-2.88700156032323,-6.12288642698431,
114.05687637435));
#211276=CARTESIAN_POINT('Ctrl Pts',(-2.72354738283741,-6.19731849490898,
114.0653063849));
#211277=CARTESIAN_POINT('Ctrl Pts',(-2.55746965732247,-6.26511276449793,
114.07373639545));
#211278=CARTESIAN_POINT('Ctrl Pts',(-2.39123894448031,-6.33296948475011,
114.08217417155));
#211279=CARTESIAN_POINT('Ctrl Pts',(-2.2223801623688,-6.39417606482082,
114.090611947649));
#211280=CARTESIAN_POINT('Ctrl Pts',(-2.05145501773262,-6.4485518769891,
114.099049723749));
#211281=CARTESIAN_POINT('Ctrl Pts',(-1.88044014999527,-6.50295623245045,
114.107491929058));
#211282=CARTESIAN_POINT('Ctrl Pts',(-1.70735707444414,-6.55052257589034,
114.115934134368));
#211283=CARTESIAN_POINT('Ctrl Pts',(-1.53278049021885,-6.59112076727505,
114.124376339678));
#211284=CARTESIAN_POINT('Ctrl Pts',(-1.35801973730266,-6.6317617875179,
114.13282745105));
#211285=CARTESIAN_POINT('Ctrl Pts',(-1.18176265275826,-6.66541990398635,
114.141278562422));
#211286=CARTESIAN_POINT('Ctrl Pts',(-1.00459297023075,-6.69201628540778,
114.149729673794));
#211287=CARTESIAN_POINT('Ctrl Pts',(-0.954870024398131,-6.69948060105082,
114.152101491292));
#211288=CARTESIAN_POINT('Ctrl Pts',(-0.905075224424326,-6.70638901133912,
114.154473308789));
#211289=CARTESIAN_POINT('Ctrl Pts',(-0.855221520991905,-6.71274050966014,
114.156845126286));
#211290=CARTESIAN_POINT('Ctrl Pts',(-0.680420138253832,-6.7350106844422,
114.16516139869));
#211291=CARTESIAN_POINT('Ctrl Pts',(-0.504578855812174,-6.75047035467769,
114.173477671094));
#211292=CARTESIAN_POINT('Ctrl Pts',(-0.32826236490003,-6.75903342348521,
114.181793943498));
#211293=CARTESIAN_POINT('Ctrl Pts',(-0.152094949788854,-6.76758925220797,
114.190103184484));
#211294=CARTESIAN_POINT('Ctrl Pts',(0.0245465275011359,-6.76926008037718,
114.19841242547));
#211295=CARTESIAN_POINT('Ctrl Pts',(0.201091196118341,-6.7640114821638,
114.206721666456));
#211296=CARTESIAN_POINT('Ctrl Pts',(0.377518964841279,-6.75876635933476,
114.215025405439));
#211297=CARTESIAN_POINT('Ctrl Pts',(0.553849705999729,-6.74661095003823,
114.223329144421));
#211298=CARTESIAN_POINT('Ctrl Pts',(0.72951125306365,-6.72756288202894,
114.231632883403));
#211299=CARTESIAN_POINT('Ctrl Pts',(0.905088677582643,-6.70852393594748,
114.239932645809));
#211300=CARTESIAN_POINT('Ctrl Pts',(1.07999720147008,-6.68259894677218,
114.248232408214));
#211301=CARTESIAN_POINT('Ctrl Pts',(1.25366826079113,-6.64985750914145,
114.25653217062));
#211302=CARTESIAN_POINT('Ctrl Pts',(1.42728796785662,-6.61712575272462,
114.264829478895));
#211303=CARTESIAN_POINT('Ctrl Pts',(1.5996705981879,-6.57758162976744,114.273126787169));
#211304=CARTESIAN_POINT('Ctrl Pts',(1.77025605793167,-6.53134614680284,
114.281424095444));
#211305=CARTESIAN_POINT('Ctrl Pts',(1.94085875286182,-6.48510599241331,
114.289722242041));
#211306=CARTESIAN_POINT('Ctrl Pts',(2.10966357660211,-6.43217321087091,
114.298020388638));
#211307=CARTESIAN_POINT('Ctrl Pts',(2.27612334854146,-6.37271931770296,
114.306318535235));
#211308=CARTESIAN_POINT('Ctrl Pts',(2.44259985905783,-6.31325944607211,
114.314617516263));
#211309=CARTESIAN_POINT('Ctrl Pts',(2.60673051971744,-6.24727727237146,
114.322916497291));
#211310=CARTESIAN_POINT('Ctrl Pts',(2.76798605330123,-6.17499329624979,
114.33121547832));
#211311=CARTESIAN_POINT('Ctrl Pts',(2.92928460098828,-6.10269003874073,
114.339516673059));
#211312=CARTESIAN_POINT('Ctrl Pts',(3.0877061754348,-6.0240817708348,114.347817867799));
#211313=CARTESIAN_POINT('Ctrl Pts',(3.24274394777183,-5.93943605817835,
114.356119062538));
#211314=CARTESIAN_POINT('Ctrl Pts',(3.39784884421087,-5.85475369788845,
114.364423851307));
#211315=CARTESIAN_POINT('Ctrl Pts',(3.5495667134581,-5.76402884992579,114.372728640075));
#211316=CARTESIAN_POINT('Ctrl Pts',(3.69741751237913,-5.66757379653341,
114.381033428844));
#211317=CARTESIAN_POINT('Ctrl Pts',(3.84544358709434,-5.57100439654156,
114.389348062865));
#211318=CARTESIAN_POINT('Ctrl Pts',(3.98959314018117,-5.46869140895762,
114.397662696886));
#211319=CARTESIAN_POINT('Ctrl Pts',(4.12941622270605,-5.36098970896719,
114.405977330907));
#211320=CARTESIAN_POINT('Ctrl Pts',(4.26932771660553,-5.25321990823708,
114.414297222344));
#211321=CARTESIAN_POINT('Ctrl Pts',(4.40490701755354,-5.14005482273073,
114.422617113782));
#211322=CARTESIAN_POINT('Ctrl Pts',(4.53573909875177,-5.02188807402699,
114.43093700522));
#211323=CARTESIAN_POINT('Ctrl Pts',(4.66676681633366,-4.90354462771839,
114.439269337593));
#211324=CARTESIAN_POINT('Ctrl Pts',(4.79303287882259,-4.78018481437875,
114.447601669967));
#211325=CARTESIAN_POINT('Ctrl Pts',(4.91415985886355,-4.6522383732494,114.45593400234));
#211326=CARTESIAN_POINT('Ctrl Pts',(5.00535450365117,-4.55590946084123,
114.462207287538));
#211327=CARTESIAN_POINT('Ctrl Pts',(5.09363692900752,-4.45698142058885,
114.468480572737));
#211328=CARTESIAN_POINT('Ctrl Pts',(5.17886189454271,-4.35564903054108,
114.474753857935));
#211329=CARTESIAN_POINT('Ctrl Pts',(5.28849382194581,-4.2252967897448,114.482823703938));
#211330=CARTESIAN_POINT('Ctrl Pts',(5.393403467879,-4.09056191938812,114.490893549941));
#211331=CARTESIAN_POINT('Ctrl Pts',(5.49320988142311,-3.95182669137141,
114.498963395943));
#211332=CARTESIAN_POINT('Ctrl Pts',(5.59289072580415,-3.81326600991792,
114.507023089053));
#211333=CARTESIAN_POINT('Ctrl Pts',(5.68748089774783,-3.67071528400997,
114.515082782164));
#211334=CARTESIAN_POINT('Ctrl Pts',(5.77663707538635,-3.52459261465377,
114.523142475274));
#211335=CARTESIAN_POINT('Ctrl Pts',(5.86570065017356,-3.3786217168986,114.531193797112));
#211336=CARTESIAN_POINT('Ctrl Pts',(5.94934126973096,-3.22908657447404,
114.539245118951));
#211337=CARTESIAN_POINT('Ctrl Pts',(6.0272566930702,-3.07643718542091,114.547296440789));
#211338=CARTESIAN_POINT('Ctrl Pts',(6.10510826279098,-2.9239128963214,114.55534116437));
#211339=CARTESIAN_POINT('Ctrl Pts',(6.17724380601086,-2.76827977091082,
114.563385887951));
#211340=CARTESIAN_POINT('Ctrl Pts',(6.24340519446697,-2.6100154362959,114.571430611533));
#211341=CARTESIAN_POINT('Ctrl Pts',(6.309526844784,-2.45184615908966,114.579470503257));
#211342=CARTESIAN_POINT('Ctrl Pts',(6.36968133983959,-2.29104916206528,
114.587510394981));
#211343=CARTESIAN_POINT('Ctrl Pts',(6.42365724300405,-2.12812514303122,
114.595550286706));
#211344=CARTESIAN_POINT('Ctrl Pts',(6.47879539524045,-1.96169292350735,
114.603763299326));
#211345=CARTESIAN_POINT('Ctrl Pts',(6.52748567183706,-1.79304139659062,
114.611976311946));
#211346=CARTESIAN_POINT('Ctrl Pts',(6.56955507424686,-1.62272459968948,
114.620189324566));
#211347=CARTESIAN_POINT('Ctrl Pts',(6.61072333291237,-1.45605605798767,
114.628226411108));
#211348=CARTESIAN_POINT('Ctrl Pts',(6.64555140720951,-1.28779324564021,
114.636263497651));
#211349=CARTESIAN_POINT('Ctrl Pts',(6.67392809233436,-1.11846896172861,
114.644300584193));
#211350=CARTESIAN_POINT('Ctrl Pts',(6.70230749324007,-0.949128472694808,
114.652338439923));
#211351=CARTESIAN_POINT('Ctrl Pts',(6.72423421368997,-0.778726678295768,
114.660376295652));
#211352=CARTESIAN_POINT('Ctrl Pts',(6.73964856015882,-0.607804479704708,
114.668414151381));
#211353=CARTESIAN_POINT('Ctrl Pts',(6.75506743594906,-0.436832057669557,
114.676454368938));
#211354=CARTESIAN_POINT('Ctrl Pts',(6.76397009529906,-0.265339298977427,
114.684494586495));
#211355=CARTESIAN_POINT('Ctrl Pts',(6.76634889959327,-0.0938699577763024,
114.692534804052));
#211356=CARTESIAN_POINT('Ctrl Pts',(6.76881757663786,0.0840776049989044,
114.70087878618));
#211357=CARTESIAN_POINT('Ctrl Pts',(6.76425981300117,0.261999501268101,
114.709222768307));
#211358=CARTESIAN_POINT('Ctrl Pts',(6.75272624786064,0.439291727049298,
114.717566750435));
#211359=CARTESIAN_POINT('Ctrl Pts',(6.74159321688892,0.610427001929132,
114.72562096527));
#211360=CARTESIAN_POINT('Ctrl Pts',(6.72396087294501,0.780975248063278,
114.733675180105));
#211361=CARTESIAN_POINT('Ctrl Pts',(6.6999271923359,0.950402345008659,114.74172939494));
#211362=CARTESIAN_POINT('Ctrl Pts',(6.67587552649109,1.11995623011949,114.749789637023));
#211363=CARTESIAN_POINT('Ctrl Pts',(6.6454130518287,1.28838693038434,114.757849879106));
#211364=CARTESIAN_POINT('Ctrl Pts',(6.60868813036923,1.45517359635093,114.765910121189));
#211365=CARTESIAN_POINT('Ctrl Pts',(6.57191186495037,1.62219344151743,114.773981632044));
#211366=CARTESIAN_POINT('Ctrl Pts',(6.52885577758208,1.78756430840956,114.782053142898));
#211367=CARTESIAN_POINT('Ctrl Pts',(6.47971719526489,1.95078293753779,114.790124653752));
#211368=CARTESIAN_POINT('Ctrl Pts',(6.47456695879007,1.96788995400967,114.790970632363));
#211369=CARTESIAN_POINT('Ctrl Pts',(6.46934994716255,1.98497334828446,114.791816610974));
#211370=CARTESIAN_POINT('Ctrl Pts',(6.46406641715298,2.00203255583794,114.792662589585));
#211371=CARTESIAN_POINT('Ctrl Pts',(6.41266291324009,2.16800171672818,114.800893121967));
#211372=CARTESIAN_POINT('Ctrl Pts',(6.35478770461155,2.33223379567073,114.809123654349));
#211373=CARTESIAN_POINT('Ctrl Pts',(6.29057391996948,2.49418699327053,114.81735418673));
#211374=CARTESIAN_POINT('Ctrl Pts',(6.22643842146596,2.65594274587407,114.825574684871));
#211375=CARTESIAN_POINT('Ctrl Pts',(6.15597986670637,2.81542481943731,114.833795183012));
#211376=CARTESIAN_POINT('Ctrl Pts',(6.07938154006315,2.97210516138635,114.842015681153));
#211377=CARTESIAN_POINT('Ctrl Pts',(6.00036179113173,3.13373847409526,114.85049604525));
#211378=CARTESIAN_POINT('Ctrl Pts',(5.914807788731,3.2923896370957,114.858976409347));
#211379=CARTESIAN_POINT('Ctrl Pts',(5.82297578598399,3.44749793268163,114.867456773444));
#211380=CARTESIAN_POINT('Ctrl Pts',(5.7341351925341,3.59755360626655,114.875660891361));
#211381=CARTESIAN_POINT('Ctrl Pts',(5.63941936316632,3.74429324906899,114.883865009278));
#211382=CARTESIAN_POINT('Ctrl Pts',(5.53910821141044,3.88723156273014,114.892069127194));
#211383=CARTESIAN_POINT('Ctrl Pts',(5.43885052391342,4.03009369252869,114.900268872446));
#211384=CARTESIAN_POINT('Ctrl Pts',(5.33300365820056,4.16915823509333,114.908468617697));
#211385=CARTESIAN_POINT('Ctrl Pts',(5.22189168595363,4.30396749757341,114.916668362949));
#211386=CARTESIAN_POINT('Ctrl Pts',(5.1108187307566,4.4387294216829,114.924865228854));
#211387=CARTESIAN_POINT('Ctrl Pts',(4.99448457957083,4.56923876574986,114.933062094759));
#211388=CARTESIAN_POINT('Ctrl Pts',(4.87325458860311,4.69506961765838,114.941258960664));
#211389=CARTESIAN_POINT('Ctrl Pts',(4.75204512506641,4.82087916308891,114.949454438623));
#211390=CARTESIAN_POINT('Ctrl Pts',(4.62594172279734,4.94201153723402,114.957649916583));
#211391=CARTESIAN_POINT('Ctrl Pts',(4.49534774608675,5.05807647646344,114.965845394543));
#211392=CARTESIAN_POINT('Ctrl Pts',(4.36472312348555,5.17416865212076,114.974042795698));
#211393=CARTESIAN_POINT('Ctrl Pts',(4.22960608763914,5.28519077688526,114.982240196853));
#211394=CARTESIAN_POINT('Ctrl Pts',(4.0904346602753,5.39079152722664,114.990437598008));
#211395=CARTESIAN_POINT('Ctrl Pts',(3.95124280374421,5.49640777884892,114.998636202471));
#211396=CARTESIAN_POINT('Ctrl Pts',(3.80799565962158,5.59660085905567,115.006834806933));
#211397=CARTESIAN_POINT('Ctrl Pts',(3.66116159176703,5.69106183404906,115.015033411396));
#211398=CARTESIAN_POINT('Ctrl Pts',(3.51424171971715,5.78557800841184,115.023236806809));
#211399=CARTESIAN_POINT('Ctrl Pts',(3.36373104430196,5.87435520186402,115.031440202222));
#211400=CARTESIAN_POINT('Ctrl Pts',(3.21012436996803,5.95712938665406,115.039643597635));
#211401=CARTESIAN_POINT('Ctrl Pts',(3.17329386362767,5.97697627905601,115.041610538251));
#211402=CARTESIAN_POINT('Ctrl Pts',(3.13628547049504,5.99647826776648,115.043577478868));
#211403=CARTESIAN_POINT('Ctrl Pts',(3.09910619832125,6.01563211736945,115.045544419485));
#211404=CARTESIAN_POINT('Ctrl Pts',(3.09910619832131,6.01563211736942,113.045755263024));
#211405=CARTESIAN_POINT('Ctrl Pts',(2.93375330764823,6.10081787314654,113.054504710927));
#211406=CARTESIAN_POINT('Ctrl Pts',(2.76488627843068,6.1791820703704,113.063254158829));
#211407=CARTESIAN_POINT('Ctrl Pts',(2.59307866646699,6.25045854553998,113.072003606731));
#211408=CARTESIAN_POINT('Ctrl Pts',(2.4212724418538,6.32173444515035,113.080752983982));
#211409=CARTESIAN_POINT('Ctrl Pts',(2.24652594672476,6.38592262741834,113.089502361232));
#211410=CARTESIAN_POINT('Ctrl Pts',(2.06943269687139,6.44280508110556,113.098251738482));
#211411=CARTESIAN_POINT('Ctrl Pts',(1.89234081822096,6.49968709436161,113.107001047987));
#211412=CARTESIAN_POINT('Ctrl Pts',(1.71290249405608,6.5492634045954,113.115750357493));
#211413=CARTESIAN_POINT('Ctrl Pts',(1.53172716625079,6.59136563150379,113.124499666998));
#211414=CARTESIAN_POINT('Ctrl Pts',(1.35055318107347,6.63346754640707,113.133248911665));
#211415=CARTESIAN_POINT('Ctrl Pts',(1.16764249714425,6.66809542395775,113.141998156333));
#211416=CARTESIAN_POINT('Ctrl Pts',(0.983616340614331,6.69513165624669,
113.150747401));
#211417=CARTESIAN_POINT('Ctrl Pts',(0.799591486713946,6.72216769715959,
113.159496583736));
#211418=CARTESIAN_POINT('Ctrl Pts',(0.614451459526949,6.74161215869368,
113.168245766471));
#211419=CARTESIAN_POINT('Ctrl Pts',(0.42882504791065,6.7533990018571,113.176994949207));
#211420=CARTESIAN_POINT('Ctrl Pts',(0.24319988859758,6.76518576550218,113.185744072918));
#211421=CARTESIAN_POINT('Ctrl Pts',(0.0570886373926176,6.76931499599833,
113.194493196628));
#211422=CARTESIAN_POINT('Ctrl Pts',(-0.128876626810283,6.76577266947849,
113.203242320339));
#211423=CARTESIAN_POINT('Ctrl Pts',(-0.314840698187232,6.76223036567997,
113.21199138793));
#211424=CARTESIAN_POINT('Ctrl Pts',(-0.500658497950266,6.7510166087923,
113.220740455522));
#211425=CARTESIAN_POINT('Ctrl Pts',(-0.685698951925173,6.73216948296229,
113.229489523113));
#211426=CARTESIAN_POINT('Ctrl Pts',(-0.870738280458717,6.71332247176308,
113.238238537492));
#211427=CARTESIAN_POINT('Ctrl Pts',(-1.05499998761128,6.68684221356206,
113.24698755187));
#211428=CARTESIAN_POINT('Ctrl Pts',(-1.23785829161289,6.65281863948547,
113.255736566249));
#211429=CARTESIAN_POINT('Ctrl Pts',(-1.43007412917269,6.6170539536889,113.264933299948));
#211430=CARTESIAN_POINT('Ctrl Pts',(-1.62073882535654,6.57295372727824,
113.274130033647));
#211431=CARTESIAN_POINT('Ctrl Pts',(-1.80913696091373,6.52068343478318,
113.283326767346));
#211432=CARTESIAN_POINT('Ctrl Pts',(-1.98838356185972,6.47095219815241,
113.29207676506));
#211433=CARTESIAN_POINT('Ctrl Pts',(-2.16557827572394,6.41382586850938,
113.300826762774));
#211434=CARTESIAN_POINT('Ctrl Pts',(-2.34011918621563,6.34949849943328,
113.309576760487));
#211435=CARTESIAN_POINT('Ctrl Pts',(-2.51465655690956,6.28517243495607,
113.318326580746));
#211436=CARTESIAN_POINT('Ctrl Pts',(-2.68653996295181,6.21364572242438,
113.327076401004));
#211437=CARTESIAN_POINT('Ctrl Pts',(-2.85518555379836,6.13516132252292,
113.335826221262));
#211438=CARTESIAN_POINT('Ctrl Pts',(-3.02382794858528,6.05667841000586,
113.3445758757));
#211439=CARTESIAN_POINT('Ctrl Pts',(-3.18923239109113,5.97123819492171,
113.353325530137));
#211440=CARTESIAN_POINT('Ctrl Pts',(-3.35083705967523,5.87913088810813,
113.362075184575));
#211441=CARTESIAN_POINT('Ctrl Pts',(-3.51243888042233,5.78702520443204,
113.370824684824));
#211442=CARTESIAN_POINT('Ctrl Pts',(-3.67024081223533,5.68825280605885,
113.379574185073));
#211443=CARTESIAN_POINT('Ctrl Pts',(-3.82370687544253,5.58314917682606,
113.388323685322));
#211444=CARTESIAN_POINT('Ctrl Pts',(-3.97717043817676,5.47804726008122,
113.397073043012));
#211445=CARTESIAN_POINT('Ctrl Pts',(-4.12629803722331,5.36661448084336,
113.405822400703));
#211446=CARTESIAN_POINT('Ctrl Pts',(-4.27058317206788,5.24922931204674,
113.414571758393));
#211447=CARTESIAN_POINT('Ctrl Pts',(-4.41486614774711,5.13184589986897,
113.423320985153));
#211448=CARTESIAN_POINT('Ctrl Pts',(-4.55430658194287,5.00851045723149,
113.432070211913));
#211449=CARTESIAN_POINT('Ctrl Pts',(-4.68843089001716,4.87964187103243,
113.440819438673));
#211450=CARTESIAN_POINT('Ctrl Pts',(-4.82255336917709,4.7507750420809,113.449568546129));
#211451=CARTESIAN_POINT('Ctrl Pts',(-4.95135966065008,4.61637541908229,
113.458317653585));
#211452=CARTESIAN_POINT('Ctrl Pts',(-5.0744123086912,4.47689945401986,113.467066761041));
#211453=CARTESIAN_POINT('Ctrl Pts',(-5.19746344226277,4.33742520555682,
113.475815760817));
#211454=CARTESIAN_POINT('Ctrl Pts',(-5.31476088454614,4.1928749549153,113.484564760594));
#211455=CARTESIAN_POINT('Ctrl Pts',(-5.42590627628689,4.04373961586928,
113.49331376037));
#211456=CARTESIAN_POINT('Ctrl Pts',(-5.5370638067251,3.89458798906959,113.502063715665));
#211457=CARTESIAN_POINT('Ctrl Pts',(-5.64206777071714,3.74085050155511,
113.510813670959));
#211458=CARTESIAN_POINT('Ctrl Pts',(-5.74056148163865,3.5830493822339,113.519563626254));
#211459=CARTESIAN_POINT('Ctrl Pts',(-5.83905138951744,3.42525435593521,
113.528313243695));
#211460=CARTESIAN_POINT('Ctrl Pts',(-5.93103139557516,3.26339625497431,
113.537062861136));
#211461=CARTESIAN_POINT('Ctrl Pts',(-6.01618907820714,3.09802485065262,
113.545812478577));
#211462=CARTESIAN_POINT('Ctrl Pts',(-6.10134392544864,2.93265895249889,
113.554561804693));
#211463=CARTESIAN_POINT('Ctrl Pts',(-6.17967677261725,2.76378023986275,
113.563311130809));
#211464=CARTESIAN_POINT('Ctrl Pts',(-6.25092157009129,2.59196229227346,
113.572060456925));
#211465=CARTESIAN_POINT('Ctrl Pts',(-6.32216437407666,2.4201491522932,113.580809538228));
#211466=CARTESIAN_POINT('Ctrl Pts',(-6.38631941548842,2.24539720663077,
113.58955861953));
#211467=CARTESIAN_POINT('Ctrl Pts',(-6.44316881037466,2.06829994947911,
113.598307700832));
#211468=CARTESIAN_POINT('Ctrl Pts',(-6.50002334524508,1.8911866802467,113.607057573175));
#211469=CARTESIAN_POINT('Ctrl Pts',(-6.5495708241104,1.71172794807917,113.615807445517));
#211470=CARTESIAN_POINT('Ctrl Pts',(-6.59164294296035,1.5305333425055,113.62455731786));
#211471=CARTESIAN_POINT('Ctrl Pts',(-6.63371214082094,1.34935131693797,
113.633306582714));
#211472=CARTESIAN_POINT('Ctrl Pts',(-6.66830695239658,1.16643393829949,
113.642055847569));
#211473=CARTESIAN_POINT('Ctrl Pts',(-6.69530988153963,0.982402458342716,
113.650805112424));
#211474=CARTESIAN_POINT('Ctrl Pts',(-6.7223141969046,0.798361530948934,
113.659554826431));
#211475=CARTESIAN_POINT('Ctrl Pts',(-6.74172580829259,0.613206671364498,
113.668304540438));
#211476=CARTESIAN_POINT('Ctrl Pts',(-6.75347878028166,0.427566795115567,
113.677054254445));
#211477=CARTESIAN_POINT('Ctrl Pts',(-6.76248992368202,0.285234494208126,
113.683762764234));
#211478=CARTESIAN_POINT('Ctrl Pts',(-6.76699999999988,0.14261726609567,
113.690471274022));
#211479=CARTESIAN_POINT('Ctrl Pts',(-6.767,5.6607593898505E-12,113.69717978381));
#211480=CARTESIAN_POINT('',(-6.76699758240985,0.00572011007101653,113.302820216219));
#211481=CARTESIAN_POINT('Ctrl Pts',(3.09910619832117,6.01563211736949,112.651476300929));
#211482=CARTESIAN_POINT('Ctrl Pts',(2.94216084648394,6.09648651524266,112.65977832277));
#211483=CARTESIAN_POINT('Ctrl Pts',(2.78196365508099,6.17123922757144,112.668080344612));
#211484=CARTESIAN_POINT('Ctrl Pts',(2.61902520880535,6.23963107528339,112.676382366453));
#211485=CARTESIAN_POINT('Ctrl Pts',(2.45615325715405,6.30799501251548,112.684681000268));
#211486=CARTESIAN_POINT('Ctrl Pts',(2.29054260050473,6.37000312427212,112.692979634083));
#211487=CARTESIAN_POINT('Ctrl Pts',(2.12272554717872,6.42544358401463,112.701278267898));
#211488=CARTESIAN_POINT('Ctrl Pts',(1.94695780854505,6.48351065195929,112.709970066916));
#211489=CARTESIAN_POINT('Ctrl Pts',(1.76876988491877,6.53437243729533,112.718661865935));
#211490=CARTESIAN_POINT('Ctrl Pts',(1.58879394997375,6.57784332319696,112.727353664953));
#211491=CARTESIAN_POINT('Ctrl Pts',(1.4169651523386,6.61934637225124,112.735652004257));
#211492=CARTESIAN_POINT('Ctrl Pts',(1.24350702150804,6.65411283860715,112.74395034356));
#211493=CARTESIAN_POINT('Ctrl Pts',(1.06898240011114,6.68203304603117,112.752248682864));
#211494=CARTESIAN_POINT('Ctrl Pts',(0.894427644215701,6.70995807433057,
112.76054845501));
#211495=CARTESIAN_POINT('Ctrl Pts',(0.718806374435361,6.73103443232346,
112.768848227156));
#211496=CARTESIAN_POINT('Ctrl Pts',(0.542688928166128,6.74520405378858,
112.777147999302));
#211497=CARTESIAN_POINT('Ctrl Pts',(0.366511802430087,6.75937847679649,
112.785450583923));
#211498=CARTESIAN_POINT('Ctrl Pts',(0.189838511953434,6.7666414708263,112.793753168544));
#211499=CARTESIAN_POINT('Ctrl Pts',(0.0132419777114451,6.76698704373123,
112.802055753166));
#211500=CARTESIAN_POINT('Ctrl Pts',(-0.163443752358986,6.76733279117901,
112.810362531278));
#211501=CARTESIAN_POINT('Ctrl Pts',(-0.340052301292425,6.76075415346924,
112.81866930939));
#211502=CARTESIAN_POINT('Ctrl Pts',(-0.516013097001385,6.74729719841383,
112.826976087502));
#211503=CARTESIAN_POINT('Ctrl Pts',(-0.692185344402196,6.73382407216583,
112.83529284785));
#211504=CARTESIAN_POINT('Ctrl Pts',(-0.867707936634538,6.71345614436573,
112.843609608199));
#211505=CARTESIAN_POINT('Ctrl Pts',(-1.04201666411697,6.68629121948054,
112.851926368547));
#211506=CARTESIAN_POINT('Ctrl Pts',(-1.21644694796818,6.6591073507956,112.860248928692));
#211507=CARTESIAN_POINT('Ctrl Pts',(-1.38966133851836,6.62511709999945,
112.868571488838));
#211508=CARTESIAN_POINT('Ctrl Pts',(-1.56110797599251,6.58446891459688,
112.876894048983));
#211509=CARTESIAN_POINT('Ctrl Pts',(-1.73279006376821,6.54376490641673,
112.885228038628));
#211510=CARTESIAN_POINT('Ctrl Pts',(-1.9026992149796,6.49638479275102,112.893562028273));
#211511=CARTESIAN_POINT('Ctrl Pts',(-2.0702998180236,6.44252649691807,112.901896017918));
#211512=CARTESIAN_POINT('Ctrl Pts',(-2.12383009348857,6.42532459334703,
112.904557826726));
#211513=CARTESIAN_POINT('Ctrl Pts',(-2.17712503241312,6.40746220700864,
112.907219635534));
#211514=CARTESIAN_POINT('Ctrl Pts',(-2.23016766295307,6.38894679858257,
112.909881444342));
#211515=CARTESIAN_POINT('Ctrl Pts',(-2.39097780782322,6.33281335495399,
112.917951290345));
#211516=CARTESIAN_POINT('Ctrl Pts',(-2.54996417962467,6.27050081463263,
112.926021136347));
#211517=CARTESIAN_POINT('Ctrl Pts',(-2.70660406864465,6.20214345332291,
112.93409098235));
#211518=CARTESIAN_POINT('Ctrl Pts',(-2.86304688476049,6.13387209426841,
112.94215067546));
#211519=CARTESIAN_POINT('Ctrl Pts',(-3.01714875451401,6.05957119371045,
112.95021036857));
#211520=CARTESIAN_POINT('Ctrl Pts',(-3.16840103803268,5.9794250444498,112.95827006168));
#211521=CARTESIAN_POINT('Ctrl Pts',(-3.31949622203139,5.89936213969483,
112.966321383519));
#211522=CARTESIAN_POINT('Ctrl Pts',(-3.46774738285662,5.81346624122508,
112.974372705358));
#211523=CARTESIAN_POINT('Ctrl Pts',(-3.61266492581227,5.72197003957604,
112.982424027196));
#211524=CARTESIAN_POINT('Ctrl Pts',(-3.75746370525339,5.63054882132965,
112.990468750777));
#211525=CARTESIAN_POINT('Ctrl Pts',(-3.89893399048018,5.5335366328246,112.998513474358));
#211526=CARTESIAN_POINT('Ctrl Pts',(-4.03661001760902,5.43121243975399,
113.006558197939));
#211527=CARTESIAN_POINT('Ctrl Pts',(-4.17420335316732,5.32894970508254,
113.014598089664));
#211528=CARTESIAN_POINT('Ctrl Pts',(-4.30800666856627,5.22138153917995,
113.022637981388));
#211529=CARTESIAN_POINT('Ctrl Pts',(-4.43758257510572,5.10883057941034,
113.030677873112));
#211530=CARTESIAN_POINT('Ctrl Pts',(-4.56994860590984,4.99385608912296,
113.038890885732));
#211531=CARTESIAN_POINT('Ctrl Pts',(-4.69790277016815,4.87368199700927,
113.047103898352));
#211532=CARTESIAN_POINT('Ctrl Pts',(-4.8210135068851,4.74869642811914,113.055316910972));
#211533=CARTESIAN_POINT('Ctrl Pts',(-4.94148716144998,4.62638810105029,
113.063353997515));
#211534=CARTESIAN_POINT('Ctrl Pts',(-5.05732251945938,4.49947262282481,
113.071391084057));
#211535=CARTESIAN_POINT('Ctrl Pts',(-5.16815199826767,4.36835139644259,
113.0794281706));
#211536=CARTESIAN_POINT('Ctrl Pts',(-5.27899208397301,4.23721762114862,
113.087466026329));
#211537=CARTESIAN_POINT('Ctrl Pts',(-5.38482509524323,4.10187758150911,
113.095503882058));
#211538=CARTESIAN_POINT('Ctrl Pts',(-5.48532360952023,3.96276594045623,
113.103541737787));
#211539=CARTESIAN_POINT('Ctrl Pts',(-5.58585165408385,3.82361342311118,
113.111581955344));
#211540=CARTESIAN_POINT('Ctrl Pts',(-5.68104186297204,3.68068740113054,
113.119622172901));
#211541=CARTESIAN_POINT('Ctrl Pts',(-5.77061012048762,3.53445156103828,
113.127662390458));
#211542=CARTESIAN_POINT('Ctrl Pts',(-5.86356232415993,3.38269083721172,
113.136006372586));
#211543=CARTESIAN_POINT('Ctrl Pts',(-5.95045924468415,3.22736569570295,
113.144350354714));
#211544=CARTESIAN_POINT('Ctrl Pts',(-6.03103612747287,3.06902137971,113.152694336841));
#211545=CARTESIAN_POINT('Ctrl Pts',(-6.10881476059825,2.9161759973266,113.160748551677));
#211546=CARTESIAN_POINT('Ctrl Pts',(-6.18070486389119,2.76051798480914,
113.168802766512));
#211547=CARTESIAN_POINT('Ctrl Pts',(-6.24651805942797,2.60255665322394,
113.176856981347));
#211548=CARTESIAN_POINT('Ctrl Pts',(-6.31238050525878,2.44447711370245,
113.18491722343));
#211549=CARTESIAN_POINT('Ctrl Pts',(-6.37215685897739,2.28409117076968,
113.192977465513));
#211550=CARTESIAN_POINT('Ctrl Pts',(-6.42570884426063,2.12192244174727,
113.201037707596));
#211551=CARTESIAN_POINT('Ctrl Pts',(-6.47933569889267,1.95952698971783,
113.20910921845));
#211552=CARTESIAN_POINT('Ctrl Pts',(-6.52672072029348,1.79534413427019,
113.217180729304));
#211553=CARTESIAN_POINT('Ctrl Pts',(-6.56777671654455,1.62990735982612,
113.225252240159));
#211554=CARTESIAN_POINT('Ctrl Pts',(-6.5720798136106,1.61256785856608,113.22609821877));
#211555=CARTESIAN_POINT('Ctrl Pts',(-6.57631343191616,1.59521458664683,
113.22694419738));
#211556=CARTESIAN_POINT('Ctrl Pts',(-6.58047750411495,1.57784816057727,
113.227790175991));
#211557=CARTESIAN_POINT('Ctrl Pts',(-6.64202959311043,1.32114276452838,
113.240295182691));
#211558=CARTESIAN_POINT('Ctrl Pts',(-6.68855950918872,1.06082125580226,
113.252800189391));
#211559=CARTESIAN_POINT('Ctrl Pts',(-6.71974545345721,0.798317005168496,
113.26530519609));
#211560=CARTESIAN_POINT('Ctrl Pts',(-6.74888740619546,0.553017828087361,
113.27699059869));
#211561=CARTESIAN_POINT('Ctrl Pts',(-6.76463117401001,0.305811782513401,
113.28867600129));
#211562=CARTESIAN_POINT('Ctrl Pts',(-6.76675232742443,0.0578959350566465,
113.30036140389));
#211563=CARTESIAN_POINT('Ctrl Pts',(-6.76690110330271,0.040507330491761,
113.30118100799));
#211564=CARTESIAN_POINT('Ctrl Pts',(-6.76698287838215,0.0231152489778019,
113.30200061209));
#211565=CARTESIAN_POINT('Ctrl Pts',(-6.76699758240933,0.00572011068525729,
113.30282021619));
#211566=CARTESIAN_POINT('Ctrl Pts',(-6.76699758240985,0.00572011007081819,
113.302820216219));
#211567=CARTESIAN_POINT('Ctrl Pts',(-6.76714174656369,-0.164828789928473,
113.310855942944));
#211568=CARTESIAN_POINT('Ctrl Pts',(-6.76083424723953,-0.335598683486344,
113.318891669669));
#211569=CARTESIAN_POINT('Ctrl Pts',(-6.7480517151586,-0.506050441700267,
113.326927396394));
#211570=CARTESIAN_POINT('Ctrl Pts',(-6.73527935231447,-0.676366595772572,
113.334956730238));
#211571=CARTESIAN_POINT('Ctrl Pts',(-6.7160422371159,-0.846364745793231,
113.342986064082));
#211572=CARTESIAN_POINT('Ctrl Pts',(-6.69036905850181,-1.01550522452696,
113.351015397926));
#211573=CARTESIAN_POINT('Ctrl Pts',(-6.66443215942169,-1.18638315098963,
113.35912721083));
#211574=CARTESIAN_POINT('Ctrl Pts',(-6.63192622110713,-1.35638529931067,
113.367239023735));
#211575=CARTESIAN_POINT('Ctrl Pts',(-6.59293474517086,-1.52495916204957,
113.37535083664));
#211576=CARTESIAN_POINT('Ctrl Pts',(-6.55437159343104,-1.69168122865691,
113.383373540691));
#211577=CARTESIAN_POINT('Ctrl Pts',(-6.50946476917128,-1.85700585832273,
113.391396244741));
#211578=CARTESIAN_POINT('Ctrl Pts',(-6.45834656910374,-2.02040802645059,
113.399418948792));
#211579=CARTESIAN_POINT('Ctrl Pts',(-6.40723257841055,-2.18379673907934,
113.407440992206));
#211580=CARTESIAN_POINT('Ctrl Pts',(-6.34990834169189,-2.34526294668844,
113.415463035619));
#211581=CARTESIAN_POINT('Ctrl Pts',(-6.28655606611847,-2.50429667322965,
113.423485079033));
#211582=CARTESIAN_POINT('Ctrl Pts',(-6.22319633607003,-2.66334911279943,
113.431508066377));
#211583=CARTESIAN_POINT('Ctrl Pts',(-6.15380729516008,-2.81996815297206,
113.439531053721));
#211584=CARTESIAN_POINT('Ctrl Pts',(-6.07861927087379,-2.97366386125968,
113.447554041065));
#211585=CARTESIAN_POINT('Ctrl Pts',(-6.0019716094381,-3.13034328893145,
113.455732779946));
#211586=CARTESIAN_POINT('Ctrl Pts',(-5.91929767150677,-3.28398434690864,
113.463911518828));
#211587=CARTESIAN_POINT('Ctrl Pts',(-5.83089016333719,-3.43409506320043,
113.472090257709));
#211588=CARTESIAN_POINT('Ctrl Pts',(-5.74405442827701,-3.5815370017811,
113.48012358901));
#211589=CARTESIAN_POINT('Ctrl Pts',(-5.65168754281564,-3.72557279410439,
113.488156920311));
#211590=CARTESIAN_POINT('Ctrl Pts',(-5.55410990549534,-3.8657666972644,
113.496190251612));
#211591=CARTESIAN_POINT('Ctrl Pts',(-5.45388295727248,-4.00976697703195,
113.504441694283));
#211592=CARTESIAN_POINT('Ctrl Pts',(-5.348158559119,-4.14971344832943,113.512693136955));
#211593=CARTESIAN_POINT('Ctrl Pts',(-5.23732671965755,-4.28517185554572,
113.520944579626));
#211594=CARTESIAN_POINT('Ctrl Pts',(-5.12649488019601,-4.42063026276211,
113.529196022298));
#211595=CARTESIAN_POINT('Ctrl Pts',(-5.01055592820781,-4.55160033312452,
113.537447464969));
#211596=CARTESIAN_POINT('Ctrl Pts',(-4.88993859368385,-4.67769062144999,
113.545698907641));
#211597=CARTESIAN_POINT('Ctrl Pts',(-4.75931541378705,-4.81424076559122,
113.554634851091));
#211598=CARTESIAN_POINT('Ctrl Pts',(-4.62288621833232,-4.94540347657821,
113.563570794542));
#211599=CARTESIAN_POINT('Ctrl Pts',(-4.48109968228315,-5.07070356434311,
113.572506737993));
#211600=CARTESIAN_POINT('Ctrl Pts',(-4.33952628900438,-5.19581529284215,
113.581429248351));
#211601=CARTESIAN_POINT('Ctrl Pts',(-4.19261181767249,-5.31508181264485,
113.590351758708));
#211602=CARTESIAN_POINT('Ctrl Pts',(-4.04084126081295,-5.4280651161267,
113.599274269066));
#211603=CARTESIAN_POINT('Ctrl Pts',(-3.88944258891635,-5.54077157545316,
113.608174916504));
#211604=CARTESIAN_POINT('Ctrl Pts',(-3.73321178635691,-5.64722539189653,
113.617075563942));
#211605=CARTESIAN_POINT('Ctrl Pts',(-3.57266581165222,-5.74702949342105,
113.625976211381));
#211606=CARTESIAN_POINT('Ctrl Pts',(-3.41236794093672,-5.84667936002457,
113.634863103967));
#211607=CARTESIAN_POINT('Ctrl Pts',(-3.2477684183083,-5.93969987462143,
113.643749996553));
#211608=CARTESIAN_POINT('Ctrl Pts',(-3.07941443254387,-6.02573611707653,
113.652636889139));
#211609=CARTESIAN_POINT('Ctrl Pts',(-2.91149317936791,-6.11155121427196,
113.661500939094));
#211610=CARTESIAN_POINT('Ctrl Pts',(-2.73983694893589,-6.19041774452342,
113.670364989049));
#211611=CARTESIAN_POINT('Ctrl Pts',(-2.56501817625615,-6.26202609029023,
113.679229039004));
#211612=CARTESIAN_POINT('Ctrl Pts',(-2.39787736637741,-6.33048942933603,
113.687703783824));
#211613=CARTESIAN_POINT('Ctrl Pts',(-2.227846061442,-6.3923182941236,113.696178528645));
#211614=CARTESIAN_POINT('Ctrl Pts',(-2.05544710604081,-6.44728052703374,
113.704653273465));
#211615=CARTESIAN_POINT('Ctrl Pts',(-1.88845585113592,-6.50051873967071,
113.712862187894));
#211616=CARTESIAN_POINT('Ctrl Pts',(-1.71940382579393,-6.54726209571515,
113.721071102323));
#211617=CARTESIAN_POINT('Ctrl Pts',(-1.54883675561019,-6.58736621909477,
113.729280016752));
#211618=CARTESIAN_POINT('Ctrl Pts',(-1.37822913397182,-6.62747987702604,
113.737490882809));
#211619=CARTESIAN_POINT('Ctrl Pts',(-1.20610609652001,-6.6609510760869,
113.745701748866));
#211620=CARTESIAN_POINT('Ctrl Pts',(-1.03302411205503,-6.68768645974921,
113.753912614923));
#211621=CARTESIAN_POINT('Ctrl Pts',(-0.859870125636911,-6.71443296530759,
113.762126896693));
#211622=CARTESIAN_POINT('Ctrl Pts',(-0.685756749089357,-6.73443801879406,
113.770341178463));
#211623=CARTESIAN_POINT('Ctrl Pts',(-0.511246217920508,-6.7476600614333,
113.778555460233));
#211624=CARTESIAN_POINT('Ctrl Pts',(-0.336539261373363,-6.76089698652525,
113.786778987825));
#211625=CARTESIAN_POINT('Ctrl Pts',(-0.161434612541626,-6.76733562461684,
113.795002515417));
#211626=CARTESIAN_POINT('Ctrl Pts',(0.0135038579698645,-6.76698652620352,
113.80322604301));
#211627=CARTESIAN_POINT('Ctrl Pts',(0.188554457236126,-6.76663720403169,
113.811454841563));
#211628=CARTESIAN_POINT('Ctrl Pts',(0.363438310991927,-6.75949148705857,
113.819683640117));
#211629=CARTESIAN_POINT('Ctrl Pts',(0.537596071852023,-6.74561186724594,
113.827912438671));
#211630=CARTESIAN_POINT('Ctrl Pts',(0.711993546933154,-6.73171314324734,
113.836152563507));
#211631=CARTESIAN_POINT('Ctrl Pts',(0.885662580337927,-6.71106204499546,
113.844392688344));
#211632=CARTESIAN_POINT('Ctrl Pts',(1.05805241666431,-6.6837724440312,113.85263281318));
#211633=CARTESIAN_POINT('Ctrl Pts',(1.13458638972954,-6.67165698740298,
113.85629108855));
#211634=CARTESIAN_POINT('Ctrl Pts',(1.21086840919001,-6.65823375249968,
113.85994936392));
#211635=CARTESIAN_POINT('Ctrl Pts',(1.28685124095268,-6.64351585259331,
113.86360763929));
#211636=CARTESIAN_POINT('Ctrl Pts',(1.46231771828376,-6.60952793729226,
113.872055662053));
#211637=CARTESIAN_POINT('Ctrl Pts',(1.63658920769549,-6.56855471427455,
113.880503684816));
#211638=CARTESIAN_POINT('Ctrl Pts',(1.80908820664905,-6.52069696125831,
113.888951707578));
#211639=CARTESIAN_POINT('Ctrl Pts',(1.98142924311719,-6.47288303301589,
113.897391994234));
#211640=CARTESIAN_POINT('Ctrl Pts',(2.15200070466085,-6.41819722998244,
113.90583228089));
#211641=CARTESIAN_POINT('Ctrl Pts',(2.32023572801532,-6.35679126340021,
113.914272567546));
#211642=CARTESIAN_POINT('Ctrl Pts',(2.48834259237072,-6.2954320749921,113.922706424513));
#211643=CARTESIAN_POINT('Ctrl Pts',(2.65411625450859,-6.22736304237392,
113.931140281481));
#211644=CARTESIAN_POINT('Ctrl Pts',(2.81700507633562,-6.15278566178762,
113.939574138449));
#211645=CARTESIAN_POINT('Ctrl Pts',(2.97979485330259,-6.07825362812041,
113.948002867194));
#211646=CARTESIAN_POINT('Ctrl Pts',(3.13970298473907,-5.99722127500127,
113.956431595939));
#211647=CARTESIAN_POINT('Ctrl Pts',(3.29619751843952,-5.90993831773507,
113.964860324684));
#211648=CARTESIAN_POINT('Ctrl Pts',(3.45262092709158,-5.8226950296152,113.973285222665));
#211649=CARTESIAN_POINT('Ctrl Pts',(3.6056335408127,-5.72920696416549,113.981710120645));
#211650=CARTESIAN_POINT('Ctrl Pts',(3.75472739085711,-5.62977008592246,
113.990135018625));
#211651=CARTESIAN_POINT('Ctrl Pts',(3.90378823128062,-5.53035522316601,
113.998558051319));
#211652=CARTESIAN_POINT('Ctrl Pts',(4.04893175922937,-5.42499435629292,
114.006981084014));
#211653=CARTESIAN_POINT('Ctrl Pts',(4.1896779737907,-5.31402742521461,114.015404116708));
#211654=CARTESIAN_POINT('Ctrl Pts',(4.3304082630777,-5.20307304991853,114.023826196345));
#211655=CARTESIAN_POINT('Ctrl Pts',(4.46674196904989,-5.08651408138716,
114.032248275983));
#211656=CARTESIAN_POINT('Ctrl Pts',(4.59823100014777,-4.96473168149902,
114.040670355621));
#211657=CARTESIAN_POINT('Ctrl Pts',(4.7297235082977,-4.84294606123773,114.049092657969));
#211658=CARTESIAN_POINT('Ctrl Pts',(4.85637084175589,-4.7159369611089,114.057514960317));
#211659=CARTESIAN_POINT('Ctrl Pts',(4.97776044134983,-4.58412368817997,
114.065937262665));
#211660=CARTESIAN_POINT('Ctrl Pts',(5.09917019699575,-4.45228852840745,
114.074360963489));
#211661=CARTESIAN_POINT('Ctrl Pts',(5.21532025281299,-4.31564785112412,
114.082784664313));
#211662=CARTESIAN_POINT('Ctrl Pts',(5.32583690300029,-4.17465570827587,
114.091208365136));
#211663=CARTESIAN_POINT('Ctrl Pts',(5.43642834081537,-4.03356815475528,
114.099637766355));
#211664=CARTESIAN_POINT('Ctrl Pts',(5.54137854941775,-3.88812351421506,
114.108067167574));
#211665=CARTESIAN_POINT('Ctrl Pts',(5.64035530496227,-3.73880743470214,
114.116496568793));
#211666=CARTESIAN_POINT('Ctrl Pts',(5.73936737527575,-3.58943807941935,
114.124928977611));
#211667=CARTESIAN_POINT('Ctrl Pts',(5.83240156368424,-3.43619481220138,
114.133361386429));
#211668=CARTESIAN_POINT('Ctrl Pts',(5.9191702635985,-3.27959027784436,114.141793795246));
#211669=CARTESIAN_POINT('Ctrl Pts',(6.00601924443839,-3.12284084841588,
114.150234005974));
#211670=CARTESIAN_POINT('Ctrl Pts',(6.08659099809977,-2.9627242330044,114.158674216701));
#211671=CARTESIAN_POINT('Ctrl Pts',(6.1606444630324,-2.79977656253284,114.167114427429));
#211672=CARTESIAN_POINT('Ctrl Pts',(6.2027648102288,-2.70709470812738,114.171915075266));
#211673=CARTESIAN_POINT('Ctrl Pts',(6.2427772754782,-2.61349734538853,114.176715723103));
#211674=CARTESIAN_POINT('Ctrl Pts',(6.2806445619527,-2.51908572430833,114.18151637094));
#211675=CARTESIAN_POINT('Ctrl Pts',(6.34485025489866,-2.35900656052433,
114.189656085973));
#211676=CARTESIAN_POINT('Ctrl Pts',(6.40301400142117,-2.19626633670184,
114.197795801006));
#211677=CARTESIAN_POINT('Ctrl Pts',(6.45490828774196,-2.03136604206138,
114.205935516039));
#211678=CARTESIAN_POINT('Ctrl Pts',(6.50675718763125,-1.86660996822941,
114.214068112126));
#211679=CARTESIAN_POINT('Ctrl Pts',(6.55234743248018,-1.69969793091769,
114.222200708213));
#211680=CARTESIAN_POINT('Ctrl Pts',(6.59149948379578,-1.53115105561796,
114.2303333043));
#211681=CARTESIAN_POINT('Ctrl Pts',(6.63062476866846,-1.36271940800526,
114.238460340507));
#211682=CARTESIAN_POINT('Ctrl Pts',(6.66332054063709,-1.19265550286258,
114.246587376715));
#211683=CARTESIAN_POINT('Ctrl Pts',(6.68945703502577,-1.0214957545405,114.254714412923));
#211684=CARTESIAN_POINT('Ctrl Pts',(6.71558103569723,-0.850417823674971,
114.262837564261));
#211685=CARTESIAN_POINT('Ctrl Pts',(6.73515194734242,-0.678245453996151,
114.270960715598));
#211686=CARTESIAN_POINT('Ctrl Pts',(6.74809107112088,-0.505525366187226,
114.279083866936));
#211687=CARTESIAN_POINT('Ctrl Pts',(6.76102655890939,-0.332853814006485,
114.287204735608));
#211688=CARTESIAN_POINT('Ctrl Pts',(6.76733394417353,-0.159635215186562,
114.295325604279));
#211689=CARTESIAN_POINT('Ctrl Pts',(6.76698637682862,0.0135785056552626,
114.303446472951));
#211690=CARTESIAN_POINT('Ctrl Pts',(6.76663879069985,0.18680158762972,114.311567780505));
#211691=CARTESIAN_POINT('Ctrl Pts',(6.75963553019068,0.360019424867068,
114.31968908806));
#211692=CARTESIAN_POINT('Ctrl Pts',(6.74600186880402,0.532679815736148,
114.327810395614));
#211693=CARTESIAN_POINT('Ctrl Pts',(6.73891734441633,0.622400156824949,
114.332030509331));
#211694=CARTESIAN_POINT('Ctrl Pts',(6.73004333439897,0.711970006935379,
114.336250623048));
#211695=CARTESIAN_POINT('Ctrl Pts',(6.7193889224893,0.801312366264337,114.340470736765));
#211696=CARTESIAN_POINT('Ctrl Pts',(6.69670614300686,0.99151836282981,114.349455175291));
#211697=CARTESIAN_POINT('Ctrl Pts',(6.66596217420908,1.1805986107691,114.358439613817));
#211698=CARTESIAN_POINT('Ctrl Pts',(6.62730282526317,1.36789848390105,114.367424052342));
#211699=CARTESIAN_POINT('Ctrl Pts',(6.58857675258871,1.55552162543339,114.376423997473));
#211700=CARTESIAN_POINT('Ctrl Pts',(6.5419080424759,1.74135801635826,114.385423942603));
#211701=CARTESIAN_POINT('Ctrl Pts',(6.4874928905115,1.92476621841792,114.394423887734));
#211702=CARTESIAN_POINT('Ctrl Pts',(6.43294950784435,2.10860662661483,114.403445041466));
#211703=CARTESIAN_POINT('Ctrl Pts',(6.37062322690239,2.29000716695555,114.412466195198));
#211704=CARTESIAN_POINT('Ctrl Pts',(6.30076006976931,2.46834186108826,114.42148734893));
#211705=CARTESIAN_POINT('Ctrl Pts',(6.23082582632298,2.64685801217841,114.430517681757));
#211706=CARTESIAN_POINT('Ctrl Pts',(6.15333947891796,2.82230186491228,114.439548014585));
#211707=CARTESIAN_POINT('Ctrl Pts',(6.06859465719012,2.99406878456785,114.448578347412));
#211708=CARTESIAN_POINT('Ctrl Pts',(5.98372969401841,3.16607921557095,114.457621482404));
#211709=CARTESIAN_POINT('Ctrl Pts',(5.8915857867474,3.33440207610212,114.466664617397));
#211710=CARTESIAN_POINT('Ctrl Pts',(5.79250295979664,3.49845658265858,114.47570775239));
#211711=CARTESIAN_POINT('Ctrl Pts',(5.70588174169629,3.64187801733197,114.48361353579));
#211712=CARTESIAN_POINT('Ctrl Pts',(5.61395799356018,3.7820375592553,114.491519319189));
#211713=CARTESIAN_POINT('Ctrl Pts',(5.51698592162353,3.91856546973607,114.499425102589));
#211714=CARTESIAN_POINT('Ctrl Pts',(5.41084110074195,4.06800778146459,114.508078707139));
#211715=CARTESIAN_POINT('Ctrl Pts',(5.29855289410897,4.21323019737577,114.516732311688));
#211716=CARTESIAN_POINT('Ctrl Pts',(5.18047536494763,4.35372989437457,114.525385916238));
#211717=CARTESIAN_POINT('Ctrl Pts',(5.0625069617822,4.49409974304853,114.534031523218));
#211718=CARTESIAN_POINT('Ctrl Pts',(4.93876010259894,4.62975534632004,114.542677130199));
#211719=CARTESIAN_POINT('Ctrl Pts',(4.8096303188304,4.76022533040059,114.551322737179));
#211720=CARTESIAN_POINT('Ctrl Pts',(4.68064926194655,4.89054504400355,114.559958386471));
#211721=CARTESIAN_POINT('Ctrl Pts',(4.54629786719942,5.01569084297337,114.568594035762));
#211722=CARTESIAN_POINT('Ctrl Pts',(4.40700993565848,5.13522661885603,114.577229685054));
#211723=CARTESIAN_POINT('Ctrl Pts',(4.26782239730844,5.25467623811453,114.585859110114));
#211724=CARTESIAN_POINT('Ctrl Pts',(4.12370564771509,5.3685237005485,114.594488535174));
#211725=CARTESIAN_POINT('Ctrl Pts',(3.97512911074323,5.47637083778315,114.603117960233));
#211726=CARTESIAN_POINT('Ctrl Pts',(3.82668177955634,5.58412418851351,114.611739880934));
#211727=CARTESIAN_POINT('Ctrl Pts',(3.67378264598822,5.6858874490197,114.620361801635));
#211728=CARTESIAN_POINT('Ctrl Pts',(3.51693309246344,5.78130354013138,114.628983722336));
#211729=CARTESIAN_POINT('Ctrl Pts',(3.38052851214159,5.8642823664752,114.636481795798));
#211730=CARTESIAN_POINT('Ctrl Pts',(3.24113685638985,5.94246140410373,114.64397986926));
#211731=CARTESIAN_POINT('Ctrl Pts',(3.09910619832145,6.01563211736934,114.651477942722));
#211732=CARTESIAN_POINT('Origin',(0.,0.,4.30282021618968));
#211733=CARTESIAN_POINT('',(3.09910619832145,6.01563211736934,117.045755263024));
#211734=CARTESIAN_POINT('',(3.09910619832134,6.0156321173694,116.651219418659));
#211735=CARTESIAN_POINT('',(3.09910619832133,6.0156321173694,4.30282021618968));
#211736=CARTESIAN_POINT('',(-6.76699999999965,-2.16894222160891E-6,115.697132037191));
#211737=CARTESIAN_POINT('Ctrl Pts',(-6.767,5.80635438534225E-12,115.69717978381));
#211738=CARTESIAN_POINT('Ctrl Pts',(-6.76700000000016,-0.18600724952103,
115.705929295621));
#211739=CARTESIAN_POINT('Ctrl Pts',(-6.75932637294552,-0.372014355744046,
115.714678807432));
#211740=CARTESIAN_POINT('Ctrl Pts',(-6.74400518264229,-0.557389537481599,
115.723428319244));
#211741=CARTESIAN_POINT('Ctrl Pts',(-6.72868405705149,-0.74276393624608,
115.732177794099));
#211742=CARTESIAN_POINT('Ctrl Pts',(-6.70571545645802,-0.927506130236736,
115.740927268955));
#211743=CARTESIAN_POINT('Ctrl Pts',(-6.6751773940489,-1.11098863989626,
115.749676743811));
#211744=CARTESIAN_POINT('Ctrl Pts',(-6.64463945808771,-1.29447038981592,
115.758426182438));
#211745=CARTESIAN_POINT('Ctrl Pts',(-6.60653217008427,-1.47669218313363,
115.767175621065));
#211746=CARTESIAN_POINT('Ctrl Pts',(-6.56098496092749,-1.65703510599,115.775925059692));
#211747=CARTESIAN_POINT('Ctrl Pts',(-6.51543793658372,-1.83737729708436,
115.784674462817));
#211748=CARTESIAN_POINT('Ctrl Pts',(-6.46245112167496,-2.01584035510685,
115.793423865942));
#211749=CARTESIAN_POINT('Ctrl Pts',(-6.40220448374329,-2.19181813760571,
115.802173269067));
#211750=CARTESIAN_POINT('Ctrl Pts',(-6.34195808526583,-2.36779522066931,
115.810922637417));
#211751=CARTESIAN_POINT('Ctrl Pts',(-6.27445201433187,-2.54128677683961,
115.819672005767));
#211752=CARTESIAN_POINT('Ctrl Pts',(-6.19991555071988,-2.71170355384615,
115.828421374117));
#211753=CARTESIAN_POINT('Ctrl Pts',(-6.1253793771679,-2.88211966767268,
115.837170708419));
#211754=CARTESIAN_POINT('Ctrl Pts',(-6.04381298052631,-3.04946076371564,
115.845920042721));
#211755=CARTESIAN_POINT('Ctrl Pts',(-5.95549339335957,-3.21315848374314,
115.854669377023));
#211756=CARTESIAN_POINT('Ctrl Pts',(-5.86717414255538,-3.37685558033268,
115.863418678003));
#211757=CARTESIAN_POINT('Ctrl Pts',(-5.77210188876731,-3.53690907646541,
115.872167978983));
#211758=CARTESIAN_POINT('Ctrl Pts',(-5.67059953347131,-3.69277536969079,
115.880917279963));
#211759=CARTESIAN_POINT('Ctrl Pts',(-5.56909755631526,-3.84864108224717,
115.889666548349));
#211760=CARTESIAN_POINT('Ctrl Pts',(-5.46116568197,-4.00031938297312,115.898415816734));
#211761=CARTESIAN_POINT('Ctrl Pts',(-5.34717048533761,-4.14729511859651,
115.907165085119));
#211762=CARTESIAN_POINT('Ctrl Pts',(-5.23317570391998,-4.29427031887719,
115.915914321636));
#211763=CARTESIAN_POINT('Ctrl Pts',(-5.1131178200368,-4.43654276189357,
115.924663558153));
#211764=CARTESIAN_POINT('Ctrl Pts',(-4.98740458984922,-4.57362924351668,
115.93341279467));
#211765=CARTESIAN_POINT('Ctrl Pts',(-4.86169180711923,-4.71071523720081,
115.942162000046));
#211766=CARTESIAN_POINT('Ctrl Pts',(-4.73032391204363,-4.84261509523051,
115.950911205421));
#211767=CARTESIAN_POINT('Ctrl Pts',(-4.59374707013802,-4.96888084538142,
115.959660410797));
#211768=CARTESIAN_POINT('Ctrl Pts',(-4.4571707030164,-5.09514615659294,
115.968409585757));
#211769=CARTESIAN_POINT('Ctrl Pts',(-4.31538563571227,-5.21577720459374,
115.977158760718));
#211770=CARTESIAN_POINT('Ctrl Pts',(-4.16887341029686,-5.33036429232748,
115.985907935678));
#211771=CARTESIAN_POINT('Ctrl Pts',(-4.022361682039,-5.44495099123472,115.99465708095));
#211772=CARTESIAN_POINT('Ctrl Pts',(-3.87112305348378,-5.55349359438453,
116.003406226222));
#211773=CARTESIAN_POINT('Ctrl Pts',(-3.71567117017992,-5.65562346298742,
116.012155371494));
#211774=CARTESIAN_POINT('Ctrl Pts',(-3.56021980146045,-5.75775299351505,
116.020904487804));
#211775=CARTESIAN_POINT('Ctrl Pts',(-3.40055544538569,-5.85346967463745,
116.029653604114));
#211776=CARTESIAN_POINT('Ctrl Pts',(-3.23722035987067,-5.94244842986785,
116.038402720425));
#211777=CARTESIAN_POINT('Ctrl Pts',(-3.07388580147382,-6.03142689794427,
116.047151808499));
#211778=CARTESIAN_POINT('Ctrl Pts',(-2.90688078896767,-6.11366734656692,
116.055900896574));
#211779=CARTESIAN_POINT('Ctrl Pts',(-2.73677250721546,-6.18889046952276,
116.064649984649));
#211780=CARTESIAN_POINT('Ctrl Pts',(-2.56666476031641,-6.26411335596263,
116.073399045215));
#211781=CARTESIAN_POINT('Ctrl Pts',(-2.39345402575306,-6.33231884500503,
116.082148105781));
#211782=CARTESIAN_POINT('Ctrl Pts',(-2.21772856065713,-6.39327529762685,
116.090897166347));
#211783=CARTESIAN_POINT('Ctrl Pts',(-2.04200363348598,-6.45423156365086,
116.099646200131));
#211784=CARTESIAN_POINT('Ctrl Pts',(-1.86376426189325,-6.50793874375646,
116.108395233915));
#211785=CARTESIAN_POINT('Ctrl Pts',(-1.68361577753161,-6.5542144390954,
116.117144267698));
#211786=CARTESIAN_POINT('Ctrl Pts',(-1.5034678296781,-6.60048999661866,
116.125893275426));
#211787=CARTESIAN_POINT('Ctrl Pts',(-1.32141105795,-6.6393340423771,116.134642283154));
#211788=CARTESIAN_POINT('Ctrl Pts',(-1.13806375487039,-6.67061465607558,
116.143391290882));
#211789=CARTESIAN_POINT('Ctrl Pts',(-0.95471698260385,-6.70189517921283,
116.15214027328));
#211790=CARTESIAN_POINT('Ctrl Pts',(-0.770079968903642,-6.72561226592209,
116.160889255679));
#211791=CARTESIAN_POINT('Ctrl Pts',(-0.584779765560425,-6.74168536983083,
116.169638238077));
#211792=CARTESIAN_POINT('Ctrl Pts',(-0.391489830653509,-6.7584515101384,
116.178764457087));
#211793=CARTESIAN_POINT('Ctrl Pts',(-0.197478578240578,-6.76689983031619,
116.187890676097));
#211794=CARTESIAN_POINT('Ctrl Pts',(-0.00346287645361174,-6.76699911397118,
116.197016895107));
#211795=CARTESIAN_POINT('Ctrl Pts',(0.184489834652479,-6.76709529501195,
116.205857919772));
#211796=CARTESIAN_POINT('Ctrl Pts',(0.372446404247931,-6.75935639738176,
116.214698944438));
#211797=CARTESIAN_POINT('Ctrl Pts',(0.559755019486866,-6.74380925873199,
116.223539969104));
#211798=CARTESIAN_POINT('Ctrl Pts',(0.745134705520392,-6.72842222659821,
116.232289947714));
#211799=CARTESIAN_POINT('Ctrl Pts',(0.929879431227269,-6.70538706057542,
116.241039926323));
#211800=CARTESIAN_POINT('Ctrl Pts',(1.11336163626704,-6.67478200894147,
116.249789904933));
#211801=CARTESIAN_POINT('Ctrl Pts',(1.29684196300602,-6.64417727061036,
116.25853979397));
#211802=CARTESIAN_POINT('Ctrl Pts',(1.47905951217398,-6.60600284890615,
116.267289683006));
#211803=CARTESIAN_POINT('Ctrl Pts',(1.65939532066977,-6.56038841607258,
116.276039572043));
#211804=CARTESIAN_POINT('Ctrl Pts',(1.83972934300695,-6.51477443503287,
116.284789374415));
#211805=CARTESIAN_POINT('Ctrl Pts',(2.01818138406158,-6.46172066062174,
116.293539176787));
#211806=CARTESIAN_POINT('Ctrl Pts',(2.19414528354094,-6.40140730423515,
116.302288979159));
#211807=CARTESIAN_POINT('Ctrl Pts',(2.37010749863894,-6.34109452518682,
116.311038697776));
#211808=CARTESIAN_POINT('Ctrl Pts',(2.54358134866354,-6.27352239616547,
116.319788416392));
#211809=CARTESIAN_POINT('Ctrl Pts',(2.71397759435451,-6.19892043966865,
116.328538135008));
#211810=CARTESIAN_POINT('Ctrl Pts',(2.88437226558026,-6.12431917249561,
116.337287772777));
#211811=CARTESIAN_POINT('Ctrl Pts',(3.05168912680864,-6.04268832278845,
116.346037410546));
#211812=CARTESIAN_POINT('Ctrl Pts',(3.2153598627377,-5.9543051612338,116.354787048314));
#211813=CARTESIAN_POINT('Ctrl Pts',(3.37902914072775,-5.8659227869748,116.363536608143));
#211814=CARTESIAN_POINT('Ctrl Pts',(3.53905210621522,-5.77078835741973,
116.372286167973));
#211815=CARTESIAN_POINT('Ctrl Pts',(3.69488522831663,-5.66922500431651,
116.381035727802));
#211816=CARTESIAN_POINT('Ctrl Pts',(3.85071701406922,-5.56766252217106,
116.389785212599));
#211817=CARTESIAN_POINT('Ctrl Pts',(4.00235878822401,-5.45967138329373,
116.398534697396));
#211818=CARTESIAN_POINT('Ctrl Pts',(4.14929549611337,-5.34561838199598,
116.407284182193));
#211819=CARTESIAN_POINT('Ctrl Pts',(4.29623099276106,-5.23156632087002,
116.416033594866));
#211820=CARTESIAN_POINT('Ctrl Pts',(4.43846127436049,-5.11145267304946,
116.424783007538));
#211821=CARTESIAN_POINT('Ctrl Pts',(4.57550326054468,-4.98568540049862,
116.433532420211));
#211822=CARTESIAN_POINT('Ctrl Pts',(4.71254416257812,-4.85991912290331,
116.442281763666));
#211823=CARTESIAN_POINT('Ctrl Pts',(4.84439664018797,-4.72849950385382,
116.451031107121));
#211824=CARTESIAN_POINT('Ctrl Pts',(4.97061286794785,-4.59187289861024,
116.459780450576));
#211825=CARTESIAN_POINT('Ctrl Pts',(5.09682813912717,-4.45524732884647,
116.468529727721));
#211826=CARTESIAN_POINT('Ctrl Pts',(5.21740705147865,-4.31341506235756,
116.477279004866));
#211827=CARTESIAN_POINT('Ctrl Pts',(5.33194007545716,-4.16685781275699,
116.486028282011));
#211828=CARTESIAN_POINT('Ctrl Pts',(5.44647226944499,-4.02030162521823,
116.494777495752));
#211829=CARTESIAN_POINT('Ctrl Pts',(5.55495848628121,-3.86902074887922,
116.503526709493));
#211830=CARTESIAN_POINT('Ctrl Pts',(5.65703027291791,-3.71352898080658,
116.512275923234));
#211831=CARTESIAN_POINT('Ctrl Pts',(5.75910135376999,-3.55803828789586,
116.521025076478));
#211832=CARTESIAN_POINT('Ctrl Pts',(5.85475793592752,-3.39833700106712,
116.529774229722));
#211833=CARTESIAN_POINT('Ctrl Pts',(5.94367514427397,-3.23496750823556,
116.538523382966));
#211834=CARTESIAN_POINT('Ctrl Pts',(6.03259176732643,-3.07159909077719,
116.547272478619));
#211835=CARTESIAN_POINT('Ctrl Pts',(6.11476896835931,-2.9045627673142,116.556021574272));
#211836=CARTESIAN_POINT('Ctrl Pts',(6.18992765547897,-2.73442583003026,
116.564770669925));
#211837=CARTESIAN_POINT('Ctrl Pts',(6.26508587283062,-2.56428995616152,
116.573519710893));
#211838=CARTESIAN_POINT('Ctrl Pts',(6.33322554827165,-2.39105376935188,
116.582268751861));
#211839=CARTESIAN_POINT('Ctrl Pts',(6.39411526733033,-2.21530561054071,
116.591017792829));
#211840=CARTESIAN_POINT('Ctrl Pts',(6.45500462602851,-2.03955849185086,
116.599766782018));
#211841=CARTESIAN_POINT('Ctrl Pts',(6.50864402040745,-1.86129970164529,
116.608515771207));
#211842=CARTESIAN_POINT('Ctrl Pts',(6.55485128368606,-1.68113463136039,
116.617264760396));
#211843=CARTESIAN_POINT('Ctrl Pts',(6.60199809554329,-1.49730620116858,
116.626191645867));
#211844=CARTESIAN_POINT('Ctrl Pts',(6.64140720707874,-1.31149343245696,
116.635118531339));
#211845=CARTESIAN_POINT('Ctrl Pts',(6.67293928722883,-1.12435326697532,
116.64404541681));
#211846=CARTESIAN_POINT('Ctrl Pts',(6.70384625876255,-0.940923067006682,
116.652795330988));
#211847=CARTESIAN_POINT('Ctrl Pts',(6.72718554579795,-0.756217899521783,
116.661545245165));
#211848=CARTESIAN_POINT('Ctrl Pts',(6.74287786815327,-0.570865181254639,
116.670295159343));
#211849=CARTESIAN_POINT('Ctrl Pts',(6.75856988190844,-0.385516108074159,
116.679044901447));
#211850=CARTESIAN_POINT('Ctrl Pts',(6.76661520773402,-0.199519795226629,
116.687794643552));
#211851=CARTESIAN_POINT('Ctrl Pts',(6.76698651789579,-0.0135080204559997,
116.696544385656));
#211852=CARTESIAN_POINT('Ctrl Pts',(6.76735782124904,0.172500343512539,
116.705293967321));
#211853=CARTESIAN_POINT('Ctrl Pts',(6.76005538995186,0.35852388221043,116.714043548986));
#211854=CARTESIAN_POINT('Ctrl Pts',(6.74510402742366,0.543930748563817,
116.722793130651));
#211855=CARTESIAN_POINT('Ctrl Pts',(6.73015291918037,0.729334461614674,
116.731542563508));
#211856=CARTESIAN_POINT('Ctrl Pts',(6.70755316306602,0.914121237634118,
116.740291996364));
#211857=CARTESIAN_POINT('Ctrl Pts',(6.67738151874583,1.09766345166066,116.749041429221));
#211858=CARTESIAN_POINT('Ctrl Pts',(6.6472103474758,1.28120278799608,116.757790724899));
#211859=CARTESIAN_POINT('Ctrl Pts',(6.60946757205154,1.46349731860273,116.766540020576));
#211860=CARTESIAN_POINT('Ctrl Pts',(6.56428138111537,1.64392790278107,116.775289316254));
#211861=CARTESIAN_POINT('Ctrl Pts',(6.51909583859866,1.82435589778997,116.784038486379));
#211862=CARTESIAN_POINT('Ctrl Pts',(6.46646716392894,2.00291972192203,116.792787656505));
#211863=CARTESIAN_POINT('Ctrl Pts',(6.40657409872906,2.17901292274598,116.80153682663));
#211864=CARTESIAN_POINT('Ctrl Pts',(6.34668181342101,2.35510383058911,116.810285882829));
#211865=CARTESIAN_POINT('Ctrl Pts',(6.27952541914077,2.52872390822512,116.819034939029));
#211866=CARTESIAN_POINT('Ctrl Pts',(6.20533299175547,2.69928350890216,116.827783995228));
#211867=CARTESIAN_POINT('Ctrl Pts',(6.12831602991577,2.87633637965564,116.836866131386));
#211868=CARTESIAN_POINT('Ctrl Pts',(6.04371690605295,3.05009086601413,116.845948267544));
#211869=CARTESIAN_POINT('Ctrl Pts',(5.95184520316652,3.21991112882695,116.855030403702));
#211870=CARTESIAN_POINT('Ctrl Pts',(5.86333549509295,3.38351691182981,116.863780184046));
#211871=CARTESIAN_POINT('Ctrl Pts',(5.76807618099388,3.54347103711972,116.872529964389));
#211872=CARTESIAN_POINT('Ctrl Pts',(5.66639083309035,3.69923018027666,116.881279744733));
#211873=CARTESIAN_POINT('Ctrl Pts',(5.56470914082217,3.85498372382026,116.890029210518));
#211874=CARTESIAN_POINT('Ctrl Pts',(5.45660203372081,4.0065423470198,116.898778676303));
#211875=CARTESIAN_POINT('Ctrl Pts',(5.34243669839227,4.15339127986656,116.907528142088));
#211876=CARTESIAN_POINT('Ctrl Pts',(5.22827486050597,4.30023571401274,116.916277339834));
#211877=CARTESIAN_POINT('Ctrl Pts',(5.1080553416711,4.44237052028471,116.92502653758));
#211878=CARTESIAN_POINT('Ctrl Pts',(4.98218644339944,4.57931296628729,116.933775735326));
#211879=CARTESIAN_POINT('Ctrl Pts',(4.85632073219594,4.71625194483352,116.942524711537));
#211880=CARTESIAN_POINT('Ctrl Pts',(4.72480612170342,4.84799861524485,116.951273687749));
#211881=CARTESIAN_POINT('Ctrl Pts',(4.58808925235352,4.97410554898447,116.960022663961));
#211882=CARTESIAN_POINT('Ctrl Pts',(4.45136349474093,5.10022068121167,116.968772208962));
#211883=CARTESIAN_POINT('Ctrl Pts',(4.30943501210129,5.22069514871793,116.977521753964));
#211884=CARTESIAN_POINT('Ctrl Pts',(4.16278587431835,5.33511975166215,116.986271298966));
#211885=CARTESIAN_POINT('Ctrl Pts',(4.01614535740487,5.44953762807814,116.99502032962));
#211886=CARTESIAN_POINT('Ctrl Pts',(3.86478496657947,5.55790617532767,117.003769360273));
#211887=CARTESIAN_POINT('Ctrl Pts',(3.70921874747204,5.65985735539351,117.012518390927));
#211888=CARTESIAN_POINT('Ctrl Pts',(3.55365041605914,5.76180991977038,117.021267540377));
#211889=CARTESIAN_POINT('Ctrl Pts',(3.3938763817454,5.85734478552803,117.030016689826));
#211890=CARTESIAN_POINT('Ctrl Pts',(3.23043927904562,5.9461374912122,117.038765839276));
#211891=CARTESIAN_POINT('Ctrl Pts',(3.18691767070448,5.96978206944138,117.041095647192));
#211892=CARTESIAN_POINT('Ctrl Pts',(3.14313645919642,5.99294880633419,117.043425455108));
#211893=CARTESIAN_POINT('Ctrl Pts',(3.09910619832145,6.01563211736934,117.045755263024));
#211894=CARTESIAN_POINT('Ctrl Pts',(3.09910619832125,6.01563211736945,115.045544419485));
#211895=CARTESIAN_POINT('Ctrl Pts',(2.9438845807917,6.09559848958332,115.053756299016));
#211896=CARTESIAN_POINT('Ctrl Pts',(2.78568313497432,6.1694928599194,115.061968178546));
#211897=CARTESIAN_POINT('Ctrl Pts',(2.62502327036983,6.23711005434543,115.070180058077));
#211898=CARTESIAN_POINT('Ctrl Pts',(2.4641528064675,6.30481588406133,115.078402702064));
#211899=CARTESIAN_POINT('Ctrl Pts',(2.30081782092016,6.36622797282393,115.08662534605));
#211900=CARTESIAN_POINT('Ctrl Pts',(2.13555632712065,6.42119055734176,115.094847990037));
#211901=CARTESIAN_POINT('Ctrl Pts',(2.03021870881675,6.45622368947572,115.100089100436));
#211902=CARTESIAN_POINT('Ctrl Pts',(1.92409866911816,6.48863754529247,115.105330210835));
#211903=CARTESIAN_POINT('Ctrl Pts',(1.81733761904495,6.5184026400955,115.110571321234));
#211904=CARTESIAN_POINT('Ctrl Pts',(1.63531307967276,6.56915127611188,115.119507264685));
#211905=CARTESIAN_POINT('Ctrl Pts',(1.4510457212125,6.61230359623252,115.128443208136));
#211906=CARTESIAN_POINT('Ctrl Pts',(1.26516391868083,6.64767999070865,115.137379151587));
#211907=CARTESIAN_POINT('Ctrl Pts',(1.0795615458007,6.68300320508084,115.146301661944));
#211908=CARTESIAN_POINT('Ctrl Pts',(0.8923498244926,6.71057376976984,115.155224172302));
#211909=CARTESIAN_POINT('Ctrl Pts',(0.704169381055813,6.73026258646596,
115.164146682659));
#211910=CARTESIAN_POINT('Ctrl Pts',(0.516450038102957,6.7499031594512,115.173047330098));
#211911=CARTESIAN_POINT('Ctrl Pts',(0.327766966782434,6.76170050240035,
115.181947977536));
#211912=CARTESIAN_POINT('Ctrl Pts',(0.138767386962045,6.76557703468934,
115.190848624974));
#211913=CARTESIAN_POINT('Ctrl Pts',(-0.0499401173342233,6.76944757627611,
115.19973551756));
#211914=CARTESIAN_POINT('Ctrl Pts',(-0.238962897593013,6.76542171879273,
115.208622410147));
#211915=CARTESIAN_POINT('Ctrl Pts',(-0.427649253809822,6.75347355926681,
115.217509302733));
#211916=CARTESIAN_POINT('Ctrl Pts',(-0.615850615656471,6.741556110971,115.226373352688));
#211917=CARTESIAN_POINT('Ctrl Pts',(-0.803717022064636,6.72175701040347,
115.235237402643));
#211918=CARTESIAN_POINT('Ctrl Pts',(-0.990598186963022,6.69410219760541,
115.244101452598));
#211919=CARTESIAN_POINT('Ctrl Pts',(-1.16927161415724,6.66766197189443,
115.252576197418));
#211920=CARTESIAN_POINT('Ctrl Pts',(-1.34704421969019,6.63404123570768,
115.261050942239));
#211921=CARTESIAN_POINT('Ctrl Pts',(-1.52334789899765,6.59330722616651,
115.269525687059));
#211922=CARTESIAN_POINT('Ctrl Pts',(-1.69412139691798,6.55385093506134,
115.277734601488));
#211923=CARTESIAN_POINT('Ctrl Pts',(-1.86335184044806,6.50775770790848,
115.285943515917));
#211924=CARTESIAN_POINT('Ctrl Pts',(-2.03049625529198,6.45518194609922,
115.294152430346));
#211925=CARTESIAN_POINT('Ctrl Pts',(-2.19768040787136,6.40259368466969,
115.302363296403));
#211926=CARTESIAN_POINT('Ctrl Pts',(-2.36277720402664,6.34351992494846,
115.31057416246));
#211927=CARTESIAN_POINT('Ctrl Pts',(-2.52526047293741,6.27816442472001,
115.318785028517));
#211928=CARTESIAN_POINT('Ctrl Pts',(-2.68781133474426,6.2127817366613,115.326999310287));
#211929=CARTESIAN_POINT('Ctrl Pts',(-2.84774617323817,6.14111223482421,
115.335213592057));
#211930=CARTESIAN_POINT('Ctrl Pts',(-3.00456029768648,6.06340716244309,
115.343427873826));
#211931=CARTESIAN_POINT('Ctrl Pts',(-3.16155092881134,5.98561462686868,
115.351651401419));
#211932=CARTESIAN_POINT('Ctrl Pts',(-3.3154135108691,5.9017731100307,115.359874929011));
#211933=CARTESIAN_POINT('Ctrl Pts',(-3.46566854508051,5.81217949960594,
115.368098456604));
#211934=CARTESIAN_POINT('Ctrl Pts',(-3.61601988692384,5.72252846316214,
115.376327255157));
#211935=CARTESIAN_POINT('Ctrl Pts',(-3.76275877374925,5.62711817719222,
115.384556053711));
#211936=CARTESIAN_POINT('Ctrl Pts',(-3.90543610874289,5.52628788614267,
115.392784852265));
#211937=CARTESIAN_POINT('Ctrl Pts',(-4.04830982767065,5.42531881026625,
115.401024977101));
#211938=CARTESIAN_POINT('Ctrl Pts',(-4.18711054668306,5.31891504424023,
115.409265101938));
#211939=CARTESIAN_POINT('Ctrl Pts',(-4.32142278294332,5.2074556292933,115.417505226774));
#211940=CARTESIAN_POINT('Ctrl Pts',(-4.38105187298164,5.157972248817,115.421163502144));
#211941=CARTESIAN_POINT('Ctrl Pts',(-4.43979677683306,5.10749288670311,
115.424821777514));
#211942=CARTESIAN_POINT('Ctrl Pts',(-4.49762357029527,5.05605292890852,
115.428480052884));
#211943=CARTESIAN_POINT('Ctrl Pts',(-4.62926406240587,4.93895182485625,
115.436807977383));
#211944=CARTESIAN_POINT('Ctrl Pts',(-4.75646792189858,4.81658222905124,
115.445135901882));
#211945=CARTESIAN_POINT('Ctrl Pts',(-4.87879671095418,4.6893103600831,115.453463826381));
#211946=CARTESIAN_POINT('Ctrl Pts',(-5.00100731009477,4.56216145686564,
115.461783704723));
#211947=CARTESIAN_POINT('Ctrl Pts',(-5.11835198390155,4.43011996680556,
115.470103583065));
#211948=CARTESIAN_POINT('Ctrl Pts',(-5.23042689719935,4.29359097645008,
115.478423461407));
#211949=CARTESIAN_POINT('Ctrl Pts',(-5.34241403046563,4.15716891920502,
115.4867368234));
#211950=CARTESIAN_POINT('Ctrl Pts',(-5.44913940828953,4.0162666332726,115.495050185394));
#211951=CARTESIAN_POINT('Ctrl Pts',(-5.5502373195323,3.87132466952476,115.503363547387));
#211952=CARTESIAN_POINT('Ctrl Pts',(-5.65127056400372,3.72647541717632,
115.51167159178));
#211953=CARTESIAN_POINT('Ctrl Pts',(-5.74668331921865,3.57759192253999,
115.519979636173));
#211954=CARTESIAN_POINT('Ctrl Pts',(-5.83615121480684,3.4251464199226,115.528287680566));
#211955=CARTESIAN_POINT('Ctrl Pts',(-5.92558733207976,3.27275506478697,
115.536592774005));
#211956=CARTESIAN_POINT('Ctrl Pts',(-6.00908262087056,3.11680452169815,
115.544897867444));
#211957=CARTESIAN_POINT('Ctrl Pts',(-6.08635676429967,2.95779484374147,
115.553202960883));
#211958=CARTESIAN_POINT('Ctrl Pts',(-6.1636162693674,2.79881528764738,115.561506481054));
#211959=CARTESIAN_POINT('Ctrl Pts',(-6.23465682574867,2.63677806402313,
115.569810001224));
#211960=CARTESIAN_POINT('Ctrl Pts',(-6.29924461315929,2.47220676796736,
115.578113521395));
#211961=CARTESIAN_POINT('Ctrl Pts',(-6.36383087010756,2.30763937156792,
115.586416844807));
#211962=CARTESIAN_POINT('Ctrl Pts',(-6.42196453669024,2.14053834627063,
115.594720168219));
#211963=CARTESIAN_POINT('Ctrl Pts',(-6.47346030690991,1.97144633578038,
115.60302349163));
#211964=CARTESIAN_POINT('Ctrl Pts',(-6.52498103083715,1.80227238705392,
115.611330838648));
#211965=CARTESIAN_POINT('Ctrl Pts',(-6.56985732780373,1.63110585761185,
115.619638185666));
#211966=CARTESIAN_POINT('Ctrl Pts',(-6.60795384897111,1.45850434688001,
115.627945532684));
#211967=CARTESIAN_POINT('Ctrl Pts',(-6.64605950621598,1.28586144389693,
115.63625487192));
#211968=CARTESIAN_POINT('Ctrl Pts',(-6.67738207840241,1.111783214658,115.644564211156));
#211969=CARTESIAN_POINT('Ctrl Pts',(-6.70183750366304,0.936836738442482,
115.652873550392));
#211970=CARTESIAN_POINT('Ctrl Pts',(-6.72631443957702,0.761736381729536,
115.661190198407));
#211971=CARTESIAN_POINT('Ctrl Pts',(-6.7439121175271,0.58576659754841,115.669506846423));
#211972=CARTESIAN_POINT('Ctrl Pts',(-6.75459834917407,0.409499867319873,
115.677823494438));
#211973=CARTESIAN_POINT('Ctrl Pts',(-6.76286833007035,0.273088591596379,
115.684259675356));
#211974=CARTESIAN_POINT('Ctrl Pts',(-6.76700004375086,0.136499598629859,
115.690695856274));
#211975=CARTESIAN_POINT('Ctrl Pts',(-6.76699999999965,-2.1689422216089E-6,
115.697132037191));
#211976=CARTESIAN_POINT('',(-6.76699990640493,-0.00112548466659665,115.302820216217));
#211977=CARTESIAN_POINT('Ctrl Pts',(3.09910619832145,6.01563211736934,114.651477942722));
#211978=CARTESIAN_POINT('Ctrl Pts',(3.05552930528257,6.0380818644093,114.653778451286));
#211979=CARTESIAN_POINT('Ctrl Pts',(3.01170410465358,6.0600603354701,114.65607895985));
#211980=CARTESIAN_POINT('Ctrl Pts',(2.96764094135406,6.08156199040996,114.658379468414));
#211981=CARTESIAN_POINT('Ctrl Pts',(2.80627217981612,6.16030566582604,114.666804424547));
#211982=CARTESIAN_POINT('Ctrl Pts',(2.64178059318266,6.23261635171114,114.675229380681));
#211983=CARTESIAN_POINT('Ctrl Pts',(2.47470894753367,6.29826203210035,114.683654336814));
#211984=CARTESIAN_POINT('Ctrl Pts',(2.30759852295219,6.36392294948203,114.69208124846));
#211985=CARTESIAN_POINT('Ctrl Pts',(2.13790715396069,6.42291565558589,114.700508160106));
#211986=CARTESIAN_POINT('Ctrl Pts',(1.9661957747478,6.4750570017077,114.708935071753));
#211987=CARTESIAN_POINT('Ctrl Pts',(1.79442125057133,6.52721752223378,114.717365082303));
#211988=CARTESIAN_POINT('Ctrl Pts',(1.62062555217479,6.57252156280522,114.725795092853));
#211989=CARTESIAN_POINT('Ctrl Pts',(1.4453832711689,6.61083627080758,114.734225103403));
#211990=CARTESIAN_POINT('Ctrl Pts',(1.26997956063984,6.6491862735174,114.742662879503));
#211991=CARTESIAN_POINT('Ctrl Pts',(1.0931269293425,6.6805340093711,114.751100655602));
#211992=CARTESIAN_POINT('Ctrl Pts',(0.915409736141963,6.70479783550381,
114.759538431702));
#211993=CARTESIAN_POINT('Ctrl Pts',(0.737599254515185,6.72907439835665,
114.767980637011));
#211994=CARTESIAN_POINT('Ctrl Pts',(0.55892363509588,6.74625959825403,114.776422842321));
#211995=CARTESIAN_POINT('Ctrl Pts',(0.379971380147108,6.75632376002432,
114.784865047631));
#211996=CARTESIAN_POINT('Ctrl Pts',(0.200830340415839,6.76639853893151,
114.793316159003));
#211997=CARTESIAN_POINT('Ctrl Pts',(0.0214124133284428,6.76933726242584,
114.801767270375));
#211998=CARTESIAN_POINT('Ctrl Pts',(-0.15769379551268,6.76516235332581,
114.810218381747));
#211999=CARTESIAN_POINT('Ctrl Pts',(-0.207960230455875,6.76399065862004,
114.812590199244));
#212000=CARTESIAN_POINT('Ctrl Pts',(-0.25820214019769,6.76225897079329,
114.814962016742));
#212001=CARTESIAN_POINT('Ctrl Pts',(-0.308406593246736,6.75996851865761,
114.817333834239));
#212002=CARTESIAN_POINT('Ctrl Pts',(-0.484437804735678,6.75193753654718,
114.825650106643));
#212003=CARTESIAN_POINT('Ctrl Pts',(-0.660325790370236,6.73701860481971,
114.833966379047));
#212004=CARTESIAN_POINT('Ctrl Pts',(-0.83549945920629,6.71522372327728,
114.842282651451));
#212005=CARTESIAN_POINT('Ctrl Pts',(-1.01052501849841,6.69344726933295,
114.850591892437));
#212006=CARTESIAN_POINT('Ctrl Pts',(-1.18483712075597,6.66480649119529,
114.858901133423));
#212007=CARTESIAN_POINT('Ctrl Pts',(-1.35786744642325,6.62936535408511,
114.867210374409));
#212008=CARTESIAN_POINT('Ctrl Pts',(-1.53078319923608,6.59394768449271,
114.875514113392));
#212009=CARTESIAN_POINT('Ctrl Pts',(-1.70241852693393,6.55173869802239,
114.883817852374));
#212010=CARTESIAN_POINT('Ctrl Pts',(-1.87221275855266,6.50285386478219,
114.892121591356));
#212011=CARTESIAN_POINT('Ctrl Pts',(-2.04192567742581,6.45399244199575,
114.900421353762));
#212012=CARTESIAN_POINT('Ctrl Pts',(-2.20979892364782,6.39846163977165,
114.908721116168));
#212013=CARTESIAN_POINT('Ctrl Pts',(-2.37528428571661,6.3364275078334,114.917020878573));
#212014=CARTESIAN_POINT('Ctrl Pts',(-2.54072071593177,6.27441171857528,
114.925318186848));
#212015=CARTESIAN_POINT('Ctrl Pts',(-2.70377034396579,6.20589655457228,
114.933615495122));
#212016=CARTESIAN_POINT('Ctrl Pts',(-2.86390211802493,6.13109726381602,
114.941912803397));
#212017=CARTESIAN_POINT('Ctrl Pts',(-3.02405007107716,6.05629041567639,
114.950210949994));
#212018=CARTESIAN_POINT('Ctrl Pts',(-3.1812792626631,5.97519831252793,114.958509096591));
#212019=CARTESIAN_POINT('Ctrl Pts',(-3.33508002324927,5.88808374927902,
114.966807243189));
#212020=CARTESIAN_POINT('Ctrl Pts',(-3.48889624946947,5.80096042611274,
114.975106224217));
#212021=CARTESIAN_POINT('Ctrl Pts',(-3.63928305433931,5.70781360686508,
114.983405205245));
#212022=CARTESIAN_POINT('Ctrl Pts',(-3.785756805383,5.60895127546106,114.991704186273));
#212023=CARTESIAN_POINT('Ctrl Pts',(-3.93226962756321,5.5100625730273,115.000005381013));
#212024=CARTESIAN_POINT('Ctrl Pts',(-4.0748670270541,5.40545551451027,115.008306575752));
#212025=CARTESIAN_POINT('Ctrl Pts',(-4.21309555720953,5.29548060385659,
115.016607770492));
#212026=CARTESIAN_POINT('Ctrl Pts',(-4.35138393385082,5.18545807921231,
115.02491255926));
#212027=CARTESIAN_POINT('Ctrl Pts',(-4.48529939917705,5.07006328716004,
115.033217348029));
#212028=CARTESIAN_POINT('Ctrl Pts',(-4.61442256269739,4.9496861933732,115.041522136797));
#212029=CARTESIAN_POINT('Ctrl Pts',(-4.74369880056909,4.82916639362216,
115.049836770818));
#212030=CARTESIAN_POINT('Ctrl Pts',(-4.8681711307963,4.70365272866408,115.058151404839));
#212031=CARTESIAN_POINT('Ctrl Pts',(-4.98745711439453,4.57357196642574,
115.06646603886));
#212032=CARTESIAN_POINT('Ctrl Pts',(-5.10681852357731,4.44340895296866,
115.074785930298));
#212033=CARTESIAN_POINT('Ctrl Pts',(-5.22098682158818,4.3086733483489,115.083105821735));
#212034=CARTESIAN_POINT('Ctrl Pts',(-5.32962061785988,4.16982410536498,
115.091425713173));
#212035=CARTESIAN_POINT('Ctrl Pts',(-5.43841685688205,4.03076723774025,
115.099758045547));
#212036=CARTESIAN_POINT('Ctrl Pts',(-5.54166185148013,3.88758472074133,
115.10809037792));
#212037=CARTESIAN_POINT('Ctrl Pts',(-5.63905744644338,3.74076464318613,
115.116422710293));
#212038=CARTESIAN_POINT('Ctrl Pts',(-5.71238509552381,3.63022605949566,
115.122695995492));
#212039=CARTESIAN_POINT('Ctrl Pts',(-5.78239800653076,3.51762616576756,
115.12896928069));
#212040=CARTESIAN_POINT('Ctrl Pts',(-5.84898648646649,3.40318175846257,
115.135242565889));
#212041=CARTESIAN_POINT('Ctrl Pts',(-5.93760450071311,3.25087559188858,
115.143591248388));
#212042=CARTESIAN_POINT('Ctrl Pts',(-6.02041506441768,3.09485622417132,
115.151939930887));
#212043=CARTESIAN_POINT('Ctrl Pts',(-6.09709480253619,2.9355960159542,115.160288613387));
#212044=CARTESIAN_POINT('Ctrl Pts',(-6.17365467097237,2.77658477142731,
115.168624244799));
#212045=CARTESIAN_POINT('Ctrl Pts',(-6.24410265488161,2.61434308122859,
115.176959876212));
#212046=CARTESIAN_POINT('Ctrl Pts',(-6.30815875215348,2.44937178836318,
115.185295507624));
#212047=CARTESIAN_POINT('Ctrl Pts',(-6.37212489898538,2.28463215557399,
115.19361943377));
#212048=CARTESIAN_POINT('Ctrl Pts',(-6.4297169150105,2.11717087142884,115.201943359916));
#212049=CARTESIAN_POINT('Ctrl Pts',(-6.48070071169988,1.94751310274738,
115.210267286061));
#212050=CARTESIAN_POINT('Ctrl Pts',(-6.53160010017454,1.77813621760732,
115.218577431206));
#212051=CARTESIAN_POINT('Ctrl Pts',(-6.57591298334361,1.60657042382224,
115.226887576351));
#212052=CARTESIAN_POINT('Ctrl Pts',(-6.61345353604174,1.43336015244495,
115.235197721496));
#212053=CARTESIAN_POINT('Ctrl Pts',(-6.65095821626886,1.26031539489182,
115.243499925749));
#212054=CARTESIAN_POINT('Ctrl Pts',(-6.68170338189337,1.08562962205983,
115.251802130003));
#212055=CARTESIAN_POINT('Ctrl Pts',(-6.70555282026724,0.909862832852349,
115.260104334257));
#212056=CARTESIAN_POINT('Ctrl Pts',(-6.72937745224773,0.734278863049114,
115.268397903182));
#212057=CARTESIAN_POINT('Ctrl Pts',(-6.74632060922838,0.557616456564615,
115.276691472106));
#212058=CARTESIAN_POINT('Ctrl Pts',(-6.75629704702972,0.380446070156476,
115.284985041031));
#212059=CARTESIAN_POINT('Ctrl Pts',(-6.76344843212745,0.253445462690426,
115.290930099418));
#212060=CARTESIAN_POINT('Ctrl Pts',(-6.76702108047258,0.126184102351834,
115.296875157804));
#212061=CARTESIAN_POINT('Ctrl Pts',(-6.76699990640502,-0.00112548408345884,
115.30282021619));
#212062=CARTESIAN_POINT('Ctrl Pts',(-6.76699990640493,-0.00112548466660582,
115.302820216217));
#212063=CARTESIAN_POINT('Ctrl Pts',(-6.76696947764202,-0.184079052889598,
115.311363717736));
#212064=CARTESIAN_POINT('Ctrl Pts',(-6.75951525884011,-0.366837573503022,
115.319907219255));
#212065=CARTESIAN_POINT('Ctrl Pts',(-6.74471008487077,-0.548794015130008,
115.328450720773));
#212066=CARTESIAN_POINT('Ctrl Pts',(-6.72988099850545,-0.731044341482288,
115.337008021224));
#212067=CARTESIAN_POINT('Ctrl Pts',(-6.70767727598725,-0.912489697216475,
115.345565321675));
#212068=CARTESIAN_POINT('Ctrl Pts',(-6.67822298376905,-1.0925322782686,
115.354122622126));
#212069=CARTESIAN_POINT('Ctrl Pts',(-6.64868572237082,-1.27308201750368,
115.362704027458));
#212070=CARTESIAN_POINT('Ctrl Pts',(-6.61185708748473,-1.45222077415082,
115.371285432789));
#212071=CARTESIAN_POINT('Ctrl Pts',(-6.56791194030996,-1.62936237354798,
115.379866838121));
#212072=CARTESIAN_POINT('Ctrl Pts',(-6.52390165183023,-1.8067665556349,
115.388460963946));
#212073=CARTESIAN_POINT('Ctrl Pts',(-6.47275387666453,-1.98216737667207,
115.397055089771));
#212074=CARTESIAN_POINT('Ctrl Pts',(-6.41469224619908,-2.15499707344428,
115.405649215595));
#212075=CARTESIAN_POINT('Ctrl Pts',(-6.35647289287564,-2.32829625744071,
115.414266687132));
#212076=CARTESIAN_POINT('Ctrl Pts',(-6.29130222624172,-2.49901005935072,
115.422884158668));
#212077=CARTESIAN_POINT('Ctrl Pts',(-6.21945171751244,-2.6665913323064,
115.431501630205));
#212078=CARTESIAN_POINT('Ctrl Pts',(-6.15928172429549,-2.80692943478278,
115.438718185983));
#212079=CARTESIAN_POINT('Ctrl Pts',(-6.09442806186373,-2.94507108580868,
115.44593474176));
#212080=CARTESIAN_POINT('Ctrl Pts',(-6.02507358098221,-3.080710525796,115.453151297538));
#212081=CARTESIAN_POINT('Ctrl Pts',(-5.94598663686851,-3.23538414851715,
115.461380547274));
#212082=CARTESIAN_POINT('Ctrl Pts',(-5.86082356120344,-3.38723765770617,
115.46960979701));
#212083=CARTESIAN_POINT('Ctrl Pts',(-5.76980829933938,-3.53576034098388,
115.477839046746));
#212084=CARTESIAN_POINT('Ctrl Pts',(-5.6789013604433,-3.68410625810681,
115.486058502336));
#212085=CARTESIAN_POINT('Ctrl Pts',(-5.58215628975952,-3.82912894013437,
115.494277957926));
#212086=CARTESIAN_POINT('Ctrl Pts',(-5.47984408366963,-3.97033976111252,
115.502497413516));
#212087=CARTESIAN_POINT('Ctrl Pts',(-5.37763309894116,-4.11141087684832,
115.510708737286));
#212088=CARTESIAN_POINT('Ctrl Pts',(-5.26986615637442,-4.24867735339501,
115.518920061055));
#212089=CARTESIAN_POINT('Ctrl Pts',(-5.1568589851902,-4.38167712261676,
115.527131384825));
#212090=CARTESIAN_POINT('Ctrl Pts',(-5.04394092988708,-4.51457201007308,
115.535336233259));
#212091=CARTESIAN_POINT('Ctrl Pts',(-4.92579110784487,-4.64320661974069,
115.543541081693));
#212092=CARTESIAN_POINT('Ctrl Pts',(-4.80276723285398,-4.76714966274651,
115.551745930127));
#212093=CARTESIAN_POINT('Ctrl Pts',(-4.67981568185696,-4.8910198413926,
115.559945955047));
#212094=CARTESIAN_POINT('Ctrl Pts',(-4.55199603802627,-5.01020369393627,
115.568145979967));
#212095=CARTESIAN_POINT('Ctrl Pts',(-4.41970484843799,-5.12430464089458,
115.576346004887));
#212096=CARTESIAN_POINT('Ctrl Pts',(-4.28745194691695,-5.23837256445396,
115.584543656534));
#212097=CARTESIAN_POINT('Ctrl Pts',(-4.1507303461087,-5.34736027573843,
115.592741308181));
#212098=CARTESIAN_POINT('Ctrl Pts',(-4.00997203146715,-5.45090940182014,
115.600938959828));
#212099=CARTESIAN_POINT('Ctrl Pts',(-3.86923256522737,-5.55444466203868,
115.609135513759));
#212100=CARTESIAN_POINT('Ctrl Pts',(-3.72445775009467,-5.65254257428186,
115.61733206769));
#212101=CARTESIAN_POINT('Ctrl Pts',(-3.57611110670047,-5.74488627846832,
115.625528621621));
#212102=CARTESIAN_POINT('Ctrl Pts',(-3.42775735455738,-5.83723440775123,
115.63372556833));
#212103=CARTESIAN_POINT('Ctrl Pts',(-3.27583173771128,-5.9238275899862,
115.641922515038));
#212104=CARTESIAN_POINT('Ctrl Pts',(-3.12082513134332,-6.00439334983776,
115.650119461747));
#212105=CARTESIAN_POINT('Ctrl Pts',(-2.96578291291584,-6.08497761930452,
115.658318291667));
#212106=CARTESIAN_POINT('Ctrl Pts',(-2.80765861341052,-6.15953154292312,
115.666517121587));
#212107=CARTESIAN_POINT('Ctrl Pts',(-2.64696601603294,-6.22782947020603,
115.674715951506));
#212108=CARTESIAN_POINT('Ctrl Pts',(-2.48612122222321,-6.29619208435707,
115.682922546766));
#212109=CARTESIAN_POINT('Ctrl Pts',(-2.32270360121288,-6.35828672359817,
115.691129142026));
#212110=CARTESIAN_POINT('Ctrl Pts',(-2.15724603569831,-6.41393627513277,
115.699335737286));
#212111=CARTESIAN_POINT('Ctrl Pts',(-1.99170838777328,-6.4696127613694,
115.707546304585));
#212112=CARTESIAN_POINT('Ctrl Pts',(-1.82412917081494,-6.51883783939465,
115.715756871884));
#212113=CARTESIAN_POINT('Ctrl Pts',(-1.65505451322706,-6.56148485925608,
115.723967439183));
#212114=CARTESIAN_POINT('Ctrl Pts',(-1.48574667748174,-6.60419069546322,
115.732189330029));
#212115=CARTESIAN_POINT('Ctrl Pts',(-1.31493963041393,-6.64030026866411,
115.740411220876));
#212116=CARTESIAN_POINT('Ctrl Pts',(-1.14318894998513,-6.66973822759424,
115.748633111723));
#212117=CARTESIAN_POINT('Ctrl Pts',(-0.987027048126935,-6.69650427965223,
115.756108750878));
#212118=CARTESIAN_POINT('Ctrl Pts',(-0.830085316907989,-6.7177554648684,
115.763584390033));
#212119=CARTESIAN_POINT('Ctrl Pts',(-0.672782764837577,-6.73347253290139,
115.771060029188));
#212120=CARTESIAN_POINT('Ctrl Pts',(-0.484752459891771,-6.75225980021652,
115.779995972638));
#212121=CARTESIAN_POINT('Ctrl Pts',(-0.295815010088564,-6.76317869153292,
115.788931916089));
#212122=CARTESIAN_POINT('Ctrl Pts',(-0.106620280744591,-6.76615999779298,
115.79786785954));
#212123=CARTESIAN_POINT('Ctrl Pts',(0.0822900387402636,-6.769136822359,
115.806790369898));
#212124=CARTESIAN_POINT('Ctrl Pts',(0.2714566084682,-6.76419986683672,115.815712880255));
#212125=CARTESIAN_POINT('Ctrl Pts',(0.460226153934383,-6.75133178619113,
115.824635390613));
#212126=CARTESIAN_POINT('Ctrl Pts',(0.648533155433595,-6.73849523633646,
115.833536038051));
#212127=CARTESIAN_POINT('Ctrl Pts',(0.836444817132283,-6.7177663651371,
115.84243668549));
#212128=CARTESIAN_POINT('Ctrl Pts',(1.02331020179792,-6.6891797128569,115.851337332928));
#212129=CARTESIAN_POINT('Ctrl Pts',(1.20988680907452,-6.66063723771962,
115.860224225514));
#212130=CARTESIAN_POINT('Ctrl Pts',(1.39542011063273,-6.62426124291457,
115.8691111181));
#212131=CARTESIAN_POINT('Ctrl Pts',(1.5792636160744,-6.58013794923356,115.877998010687));
#212132=CARTESIAN_POINT('Ctrl Pts',(1.76263457508044,-6.53612806888802,
115.886862060642));
#212133=CARTESIAN_POINT('Ctrl Pts',(1.94432415461541,-6.48441068565554,
115.895726110596));
#212134=CARTESIAN_POINT('Ctrl Pts',(2.12369614625398,-6.42512285317456,
115.904590160551));
#212135=CARTESIAN_POINT('Ctrl Pts',(2.29519019974067,-6.368438915946,115.913064905372));
#212136=CARTESIAN_POINT('Ctrl Pts',(2.46456560479013,-6.30483525768566,
115.921539650192));
#212137=CARTESIAN_POINT('Ctrl Pts',(2.63127419824938,-6.23447552674859,
115.930014395013));
#212138=CARTESIAN_POINT('Ctrl Pts',(2.79275358285557,-6.16632279498463,
115.938223309442));
#212139=CARTESIAN_POINT('Ctrl Pts',(2.95157479802554,-6.09189598382998,
115.946432223871));
#212140=CARTESIAN_POINT('Ctrl Pts',(3.10722938386873,-6.01144030628458,
115.9546411383));
#212141=CARTESIAN_POINT('Ctrl Pts',(3.26292097579913,-5.93096550081047,
115.962852004357));
#212142=CARTESIAN_POINT('Ctrl Pts',(3.41544412218355,-5.84445913685158,
115.971062870414));
#212143=CARTESIAN_POINT('Ctrl Pts',(3.56431538039064,-5.7522121717745,115.97927373647));
#212144=CARTESIAN_POINT('Ctrl Pts',(3.71324856890886,-5.65992683204192,
115.98748801824));
#212145=CARTESIAN_POINT('Ctrl Pts',(3.85852654028454,-5.56189632102397,
115.99570230001));
#212146=CARTESIAN_POINT('Ctrl Pts',(3.99969515571156,-5.45845469536731,
116.00391658178));
#212147=CARTESIAN_POINT('Ctrl Pts',(4.14102266755972,-5.35489663799485,
116.012140109372));
#212148=CARTESIAN_POINT('Ctrl Pts',(4.27823129766527,-5.24591551152056,
116.020363636965));
#212149=CARTESIAN_POINT('Ctrl Pts',(4.4108995522863,-5.13188602169227,116.028587164557));
#212150=CARTESIAN_POINT('Ctrl Pts',(4.54365284209776,-5.01778344339674,
116.036815963111));
#212151=CARTESIAN_POINT('Ctrl Pts',(4.67185969496866,-4.89862629316028,
116.045044761664));
#212152=CARTESIAN_POINT('Ctrl Pts',(4.79513583137633,-4.77482579353958,
116.053273560218));
#212153=CARTESIAN_POINT('Ctrl Pts',(4.91858164752081,-4.65085489243805,
116.061513685054));
#212154=CARTESIAN_POINT('Ctrl Pts',(5.03708295075616,-4.52222813723402,
116.069753809891));
#212155=CARTESIAN_POINT('Ctrl Pts',(5.15029540129018,-4.38939019448594,
116.077993934727));
#212156=CARTESIAN_POINT('Ctrl Pts',(5.20055705722302,-4.33041562992402,
116.081652210097));
#212157=CARTESIAN_POINT('Ctrl Pts',(5.24977685020032,-4.27061143519299,
116.085310485467));
#212158=CARTESIAN_POINT('Ctrl Pts',(5.29792742565693,-4.21001828885246,
116.088968760837));
#212159=CARTESIAN_POINT('Ctrl Pts',(5.40912112113917,-4.07009107513575,
116.0974167836));
#212160=CARTESIAN_POINT('Ctrl Pts',(5.51486440411148,-3.92563445489108,
116.105864806362));
#212161=CARTESIAN_POINT('Ctrl Pts',(5.61478410077162,-3.77710054164861,
116.114312829125));
#212162=CARTESIAN_POINT('Ctrl Pts',(5.71461229798134,-3.6287026453466,116.12275311578));
#212163=CARTESIAN_POINT('Ctrl Pts',(5.80862735353041,-3.47623517380994,
116.131193402436));
#212164=CARTESIAN_POINT('Ctrl Pts',(5.89649729853568,-3.3201820143422,116.139633689092));
#212165=CARTESIAN_POINT('Ctrl Pts',(5.98430030549211,-3.16424773390653,
116.14806754606));
#212166=CARTESIAN_POINT('Ctrl Pts',(6.06596737094342,-3.00473350043247,
116.156501403028));
#212167=CARTESIAN_POINT('Ctrl Pts',(6.14121046779082,-2.84215112024263,
116.164935259996));
#212168=CARTESIAN_POINT('Ctrl Pts',(6.21640781292909,-2.67966759858042,
116.173363988741));
#212169=CARTESIAN_POINT('Ctrl Pts',(6.28518883746487,-2.51411995161613,
116.181792717486));
#212170=CARTESIAN_POINT('Ctrl Pts',(6.34731182640543,-2.34604381424853,
116.190221446231));
#212171=CARTESIAN_POINT('Ctrl Pts',(6.40940658112922,-2.17804406564098,
116.198646344211));
#212172=CARTESIAN_POINT('Ctrl Pts',(6.46484921870031,-2.0075184303876,116.207071242191));
#212173=CARTESIAN_POINT('Ctrl Pts',(6.51344631996132,-1.83502208078876,
116.215496140172));
#212174=CARTESIAN_POINT('Ctrl Pts',(6.56203266174497,-1.66256392216267,
116.223919172866));
#212175=CARTESIAN_POINT('Ctrl Pts',(6.60377639616261,-1.48813623912324,
116.23234220556));
#212176=CARTESIAN_POINT('Ctrl Pts',(6.6385339479833,-1.31230942291568,116.240765238254));
#212177=CARTESIAN_POINT('Ctrl Pts',(6.67328756702648,-1.13650250131269,
116.249187317892));
#212178=CARTESIAN_POINT('Ctrl Pts',(6.70105651467291,-0.959297089217605,
116.257609397529));
#212179=CARTESIAN_POINT('Ctrl Pts',(6.72174826329795,-0.781274141931635,
116.266031477167));
#212180=CARTESIAN_POINT('Ctrl Pts',(6.74244055908869,-0.60324648706626,
116.274453779515));
#212181=CARTESIAN_POINT('Ctrl Pts',(6.75605524461533,-0.424401585194312,
116.282876081863));
#212182=CARTESIAN_POINT('Ctrl Pts',(6.76255159130435,-0.245326262244779,
116.291298384212));
#212183=CARTESIAN_POINT('Ctrl Pts',(6.76904901667478,-0.0662212048566616,
116.299722085035));
#212184=CARTESIAN_POINT('Ctrl Pts',(6.76842573524668,0.113114016656728,
116.308145785859));
#212185=CARTESIAN_POINT('Ctrl Pts',(6.76069312908836,0.292091448518292,
116.316569486682));
#212186=CARTESIAN_POINT('Ctrl Pts',(6.75295529020476,0.471189996044104,
116.324998887901));
#212187=CARTESIAN_POINT('Ctrl Pts',(6.73809852757025,0.64992993660467,116.33342828912));
#212188=CARTESIAN_POINT('Ctrl Pts',(6.71618628306615,0.827726289998191,
116.341857690339));
#212189=CARTESIAN_POINT('Ctrl Pts',(6.69426622030366,1.0055860808835,116.350290099157));
#212190=CARTESIAN_POINT('Ctrl Pts',(6.66528570302216,1.18250128310897,116.358722507975));
#212191=CARTESIAN_POINT('Ctrl Pts',(6.62935962369917,1.35789542294949,116.367154916792));
#212192=CARTESIAN_POINT('Ctrl Pts',(6.59340030452226,1.53345184255162,116.37559512752));
#212193=CARTESIAN_POINT('Ctrl Pts',(6.55048265670781,1.70748406234172,116.384035338248));
#212194=CARTESIAN_POINT('Ctrl Pts',(6.500772204812,1.87942803563843,116.392475548975));
#212195=CARTESIAN_POINT('Ctrl Pts',(6.47249774803957,1.97722683357428,116.397276196812));
#212196=CARTESIAN_POINT('Ctrl Pts',(6.4420266348651,2.07435033715814,116.402076844649));
#212197=CARTESIAN_POINT('Ctrl Pts',(6.40939637597011,2.1706973754306,116.406877492486));
#212198=CARTESIAN_POINT('Ctrl Pts',(6.35407029960003,2.33405812640248,116.415017207519));
#212199=CARTESIAN_POINT('Ctrl Pts',(6.29242383099363,2.49551126129875,116.423156922552));
#212200=CARTESIAN_POINT('Ctrl Pts',(6.22460993351384,2.65452823974445,116.431296637585));
#212201=CARTESIAN_POINT('Ctrl Pts',(6.15685534566194,2.81340614289484,116.439429233672));
#212202=CARTESIAN_POINT('Ctrl Pts',(6.0829442083237,2.96985179608627,116.447561829759));
#212203=CARTESIAN_POINT('Ctrl Pts',(6.00307902500841,3.12335256087175,116.455694425846));
#212204=CARTESIAN_POINT('Ctrl Pts',(5.92326844181703,3.27674838429942,116.463821462054));
#212205=CARTESIAN_POINT('Ctrl Pts',(5.83751208514919,3.42720300413067,116.471948498261));
#212206=CARTESIAN_POINT('Ctrl Pts',(5.74606021262659,3.57422453587764,116.480075534469));
#212207=CARTESIAN_POINT('Ctrl Pts',(5.6546520557542,3.72117578867155,116.488198685807));
#212208=CARTESIAN_POINT('Ctrl Pts',(5.55755399755129,3.86469691100852,116.496321837145));
#212209=CARTESIAN_POINT('Ctrl Pts',(5.45506179106966,4.00432139764178,116.504444988482));
#212210=CARTESIAN_POINT('Ctrl Pts',(5.35259838565977,4.14390664875663,116.512565857154));
#212211=CARTESIAN_POINT('Ctrl Pts',(5.24474406828782,4.27959715067328,116.520686725825));
#212212=CARTESIAN_POINT('Ctrl Pts',(5.13183736405347,4.4109561626596,116.528807594497));
#212213=CARTESIAN_POINT('Ctrl Pts',(5.01892455790864,4.54232227378975,116.536928902052));
#212214=CARTESIAN_POINT('Ctrl Pts',(4.90095905510152,4.66935614699891,116.545050209606));
#212215=CARTESIAN_POINT('Ctrl Pts',(4.77831915753368,4.79165472762246,116.553171517161));
#212216=CARTESIAN_POINT('Ctrl Pts',(4.71459120357028,4.8552053214368,116.557391630878));
#212217=CARTESIAN_POINT('Ctrl Pts',(4.64960169925592,4.91747787101678,116.561611744594));
#212218=CARTESIAN_POINT('Ctrl Pts',(4.58340761898701,4.97841978927167,116.565831858311));
#212219=CARTESIAN_POINT('Ctrl Pts',(4.44246601318343,5.10817839887396,116.574817399035));
#212220=CARTESIAN_POINT('Ctrl Pts',(4.29613133671346,5.23183804094533,116.583802939758));
#212221=CARTESIAN_POINT('Ctrl Pts',(4.14494026557815,5.34899609223908,116.592788480482));
#212222=CARTESIAN_POINT('Ctrl Pts',(3.99352790923918,5.46632561756927,116.601787172559));
#212223=CARTESIAN_POINT('Ctrl Pts',(3.83724514719207,5.57713439577659,116.610785864636));
#212224=CARTESIAN_POINT('Ctrl Pts',(3.67665792189673,5.68106288693886,116.619784556714));
#212225=CARTESIAN_POINT('Ctrl Pts',(3.51577657434522,5.78518172750311,116.628799730274));
#212226=CARTESIAN_POINT('Ctrl Pts',(3.35057519985205,5.88239495346927,116.637814903834));
#212227=CARTESIAN_POINT('Ctrl Pts',(3.18164658582711,5.97238762999311,116.646830077394));
#212228=CARTESIAN_POINT('Ctrl Pts',(3.15423038832485,5.98699295312072,116.648293191149));
#212229=CARTESIAN_POINT('Ctrl Pts',(3.12671606358679,6.00140819161904,116.649756304904));
#212230=CARTESIAN_POINT('Ctrl Pts',(3.09910619832135,6.0156321173694,116.651219418659));
#212231=CARTESIAN_POINT('Origin',(0.,0.,4.30282021618968));
#212232=CARTESIAN_POINT('',(3.09910619832142,6.01563211736936,119.045959136766));
#212233=CARTESIAN_POINT('',(3.09910619832126,6.01563211736944,118.651553971577));
#212234=CARTESIAN_POINT('',(3.09910619832133,6.0156321173694,4.30282021618968));
#212235=CARTESIAN_POINT('',(-6.76699999999861,4.3460530827503E-6,117.697273959568));
#212236=CARTESIAN_POINT('Ctrl Pts',(-6.76699999999861,4.34605308275028E-6,
117.697273959568));
#212237=CARTESIAN_POINT('Ctrl Pts',(-6.76700011305956,-0.176036644547901,
117.705588278987));
#212238=CARTESIAN_POINT('Ctrl Pts',(-6.760126440919,-0.352257286263359,
117.713902598407));
#212239=CARTESIAN_POINT('Ctrl Pts',(-6.74636291712061,-0.528087483756204,
117.722216917826));
#212240=CARTESIAN_POINT('Ctrl Pts',(-6.73261188350642,-0.703758118074181,
117.73052369213));
#212241=CARTESIAN_POINT('Ctrl Pts',(-6.71198348273243,-0.879038668276297,
117.738830466434));
#212242=CARTESIAN_POINT('Ctrl Pts',(-6.68451369221068,-1.05335924482007,
117.747137240738));
#212243=CARTESIAN_POINT('Ctrl Pts',(-6.6570637548589,-1.22755383510886,
117.755438011508));
#212244=CARTESIAN_POINT('Ctrl Pts',(-6.62278233466031,-1.40078949100303,
117.763738782278));
#212245=CARTESIAN_POINT('Ctrl Pts',(-6.58175723051189,-1.57250143357788,
117.772039553049));
#212246=CARTESIAN_POINT('Ctrl Pts',(-6.54063083866197,-1.74463731920768,
117.780360817758));
#212247=CARTESIAN_POINT('Ctrl Pts',(-6.49272745480837,-1.91524160647387,
117.788682082468));
#212248=CARTESIAN_POINT('Ctrl Pts',(-6.43818734215969,-2.08375448343962,
117.797003347178));
#212249=CARTESIAN_POINT('Ctrl Pts',(-6.38382669575631,-2.25171286259,117.80529723046));
#212250=CARTESIAN_POINT('Ctrl Pts',(-6.32287304359227,-2.41759324207099,
117.813591113742));
#212251=CARTESIAN_POINT('Ctrl Pts',(-6.2555154742714,-2.5808555076081,117.821884997024));
#212252=CARTESIAN_POINT('Ctrl Pts',(-6.18816636687098,-2.74409726301817,
117.830177838372));
#212253=CARTESIAN_POINT('Ctrl Pts',(-6.11441507831726,-2.90472123763043,
117.83847067972));
#212254=CARTESIAN_POINT('Ctrl Pts',(-6.03449910347032,-3.06220665047544,
117.846763521067));
#212255=CARTESIAN_POINT('Ctrl Pts',(-5.95457978942486,-3.21969864367007,
117.855056708922));
#212256=CARTESIAN_POINT('Ctrl Pts',(-5.86849543416824,-3.37405150315763,
117.863349896777));
#212257=CARTESIAN_POINT('Ctrl Pts',(-5.77652989209185,-3.5247682768899,
117.871643084631));
#212258=CARTESIAN_POINT('Ctrl Pts',(-5.68402045079509,-3.67637641421203,
117.879985319752));
#212259=CARTESIAN_POINT('Ctrl Pts',(-5.5855602058369,-3.8243050052865,117.888327554873));
#212260=CARTESIAN_POINT('Ctrl Pts',(-5.48148265944007,-3.96807722382741,
117.896669789994));
#212261=CARTESIAN_POINT('Ctrl Pts',(-5.37792086648259,-4.11113698306501,
117.904970685396));
#212262=CARTESIAN_POINT('Ctrl Pts',(-5.26879756661816,-4.25008121831449,
117.913271580798));
#212263=CARTESIAN_POINT('Ctrl Pts',(-5.15448211887255,-4.38447295421276,
117.921572476201));
#212264=CARTESIAN_POINT('Ctrl Pts',(-5.0393127087195,-4.51986862695938,
117.929935381181));
#212265=CARTESIAN_POINT('Ctrl Pts',(-4.91887349889496,-4.6506432355397,
117.93829828616));
#212266=CARTESIAN_POINT('Ctrl Pts',(-4.79358027298436,-4.77638745983355,
117.94666119114));
#212267=CARTESIAN_POINT('Ctrl Pts',(-4.66828704707384,-4.90213168412732,
117.95502409612));
#212268=CARTESIAN_POINT('Ctrl Pts',(-4.5381400908651,-5.02284530400535,
117.9633870011));
#212269=CARTESIAN_POINT('Ctrl Pts',(-4.40358931946243,-5.13816018682917,
117.97174990608));
#212270=CARTESIAN_POINT('Ctrl Pts',(-4.27262945093562,-5.25039753587118,
117.979889621113));
#212271=CARTESIAN_POINT('Ctrl Pts',(-4.1372082456562,-5.35776838396358,
117.988029336146));
#212272=CARTESIAN_POINT('Ctrl Pts',(-3.99772702156077,-5.4598963049753,
117.996169051179));
#212273=CARTESIAN_POINT('Ctrl Pts',(-3.85836778690731,-5.56193490551987,
118.004301647266));
#212274=CARTESIAN_POINT('Ctrl Pts',(-3.71495589486778,-5.65873949139583,
118.012434243353));
#212275=CARTESIAN_POINT('Ctrl Pts',(-3.56792714719738,-5.74997259752531,
118.020566839439));
#212276=CARTESIAN_POINT('Ctrl Pts',(-3.42099891626635,-5.84114333180918,
118.028693875647));
#212277=CARTESIAN_POINT('Ctrl Pts',(-3.2704590625712,-5.92674997750293,
118.036820911855));
#212278=CARTESIAN_POINT('Ctrl Pts',(-3.11677385922776,-6.00649729130335,
118.044947948063));
#212279=CARTESIAN_POINT('Ctrl Pts',(-2.96316212019301,-6.08620648444446,
118.053071099401));
#212280=CARTESIAN_POINT('Ctrl Pts',(-2.80640834990148,-6.16006175482521,
118.061194250739));
#212281=CARTESIAN_POINT('Ctrl Pts',(-2.6470049896705,-6.22781290539942,
118.069317402076));
#212282=CARTESIAN_POINT('Ctrl Pts',(-2.48764642296852,-6.29554501739674,
118.077438270748));
#212283=CARTESIAN_POINT('Ctrl Pts',(-2.32564008637862,-6.35717628373792,
118.085559139419));
#212284=CARTESIAN_POINT('Ctrl Pts',(-2.16150000916222,-6.41250393453226,
118.093680008091));
#212285=CARTESIAN_POINT('Ctrl Pts',(-1.99735106118775,-6.46783457544463,
118.101801315646));
#212286=CARTESIAN_POINT('Ctrl Pts',(-1.83106848797845,-6.51686079946705,
118.1099226232));
#212287=CARTESIAN_POINT('Ctrl Pts',(-1.66318332939714,-6.559429107233,118.118043930755));
#212288=CARTESIAN_POINT('Ctrl Pts',(-1.57594436500362,-6.58154907970029,
118.122264044471));
#212289=CARTESIAN_POINT('Ctrl Pts',(-1.488272916242,-6.6019261053456,118.126484158188));
#212290=CARTESIAN_POINT('Ctrl Pts',(-1.40024481847838,-6.62054404473865,
118.130704271905));
#212291=CARTESIAN_POINT('Ctrl Pts',(-1.21283682760999,-6.66018082781594,
118.139688710431));
#212292=CARTESIAN_POINT('Ctrl Pts',(-1.02390467830441,-6.69182217318139,
118.148673148957));
#212293=CARTESIAN_POINT('Ctrl Pts',(-0.834115133867594,-6.71539581435473,
118.157657587482));
#212294=CARTESIAN_POINT('Ctrl Pts',(-0.643998024004414,-6.73901014222578,
118.166657532613));
#212295=CARTESIAN_POINT('Ctrl Pts',(-0.45302079843496,-6.75452890537391,
118.175657477743));
#212296=CARTESIAN_POINT('Ctrl Pts',(-0.261853921974926,-6.76193178932961,
118.184657422874));
#212297=CARTESIAN_POINT('Ctrl Pts',(-0.070236555863476,-6.76935211837138,
118.193678576606));
#212298=CARTESIAN_POINT('Ctrl Pts',(0.121571115597132,-6.7686182923628,
118.202699730338));
#212299=CARTESIAN_POINT('Ctrl Pts',(0.312897257496911,-6.7597621486448,
118.211720884071));
#212300=CARTESIAN_POINT('Ctrl Pts',(0.504418075254281,-6.75089699373075,
118.220751216898));
#212301=CARTESIAN_POINT('Ctrl Pts',(0.69545614641719,-6.73389302765554,
118.229781549725));
#212302=CARTESIAN_POINT('Ctrl Pts',(0.885344550686241,-6.70883402884363,
118.238811882552));
#212303=CARTESIAN_POINT('Ctrl Pts',(1.07550215685612,-6.68373950427047,
118.247855017545));
#212304=CARTESIAN_POINT('Ctrl Pts',(1.26450660014674,-6.65056714468046,
118.256898152538));
#212305=CARTESIAN_POINT('Ctrl Pts',(1.4516986391693,-6.60945232685992,118.26594128753));
#212306=CARTESIAN_POINT('Ctrl Pts',(1.61534760779666,-6.57350850378515,
118.27384707093));
#212307=CARTESIAN_POINT('Ctrl Pts',(1.77761145950585,-6.53149523096438,
118.28175285433));
#212308=CARTESIAN_POINT('Ctrl Pts',(1.93805838123315,-6.48353443045782,
118.28965863773));
#212309=CARTESIAN_POINT('Ctrl Pts',(2.11367785289102,-6.43103825069584,
118.298312025958));
#212310=CARTESIAN_POINT('Ctrl Pts',(2.28727529007613,-6.37136888974459,
118.306965414187));
#212311=CARTESIAN_POINT('Ctrl Pts',(2.45826081080456,-6.30470005520187,
118.315618802415));
#212312=CARTESIAN_POINT('Ctrl Pts',(2.62908841427546,-6.23809279405712,
118.324264198625));
#212313=CARTESIAN_POINT('Ctrl Pts',(2.79730863038597,-6.16449906298657,
118.332909594836));
#212314=CARTESIAN_POINT('Ctrl Pts',(2.96234803145788,-6.08414193954395,
118.341554991046));
#212315=CARTESIAN_POINT('Ctrl Pts',(3.13265823504674,-6.00121848027034,
118.350476492089));
#212316=CARTESIAN_POINT('Ctrl Pts',(3.29958077737196,-5.911092562811,118.359397993131));
#212317=CARTESIAN_POINT('Ctrl Pts',(3.4625069947561,-5.81406349391414,118.368319494173));
#212318=CARTESIAN_POINT('Ctrl Pts',(3.62009022811629,-5.72021638537515,
118.376948424515));
#212319=CARTESIAN_POINT('Ctrl Pts',(3.77393479224612,-5.6199118627624,118.385577354857));
#212320=CARTESIAN_POINT('Ctrl Pts',(3.92351372896765,-5.51346796658894,
118.394206285199));
#212321=CARTESIAN_POINT('Ctrl Pts',(4.08070005372313,-5.4016104738237,118.403274071592));
#212322=CARTESIAN_POINT('Ctrl Pts',(4.23317524980973,-5.28297300151781,
118.412341857984));
#212323=CARTESIAN_POINT('Ctrl Pts',(4.38036056483422,-5.15797734795775,
118.421409644377));
#212324=CARTESIAN_POINT('Ctrl Pts',(4.52754587985881,-5.0329816943976,118.43047743077));
#212325=CARTESIAN_POINT('Ctrl Pts',(4.66944099337389,-4.90162808553282,
118.439545217162));
#212326=CARTESIAN_POINT('Ctrl Pts',(4.80550560803706,-4.764389242193,118.448613003555));
#212327=CARTESIAN_POINT('Ctrl Pts',(4.93192437885736,-4.63687948569408,
118.457037959688));
#212328=CARTESIAN_POINT('Ctrl Pts',(5.05325471587774,-4.50434546483646,
118.465462915821));
#212329=CARTESIAN_POINT('Ctrl Pts',(5.16910250584504,-4.36722661240135,
118.473887871954));
#212330=CARTESIAN_POINT('Ctrl Pts',(5.28497718519686,-4.23007593336385,
118.482314783601));
#212331=CARTESIAN_POINT('Ctrl Pts',(5.39536656620621,-4.08833855422847,
118.490741695247));
#212332=CARTESIAN_POINT('Ctrl Pts',(5.49991697375534,-3.94248681441016,
118.499168606893));
#212333=CARTESIAN_POINT('Ctrl Pts',(5.60450582856158,-3.79658143922616,
118.507598617443));
#212334=CARTESIAN_POINT('Ctrl Pts',(5.70325123545573,-3.64655895594379,
118.516028627993));
#212335=CARTESIAN_POINT('Ctrl Pts',(5.79584275988278,-3.49292079823096,
118.524458638544));
#212336=CARTESIAN_POINT('Ctrl Pts',(5.88851957768537,-3.33914111226093,
118.532896414643));
#212337=CARTESIAN_POINT('Ctrl Pts',(5.975031015918,-3.18173938166461,118.541334190742));
#212338=CARTESIAN_POINT('Ctrl Pts',(6.05511199578107,-3.02124274406216,
118.549771966842));
#212339=CARTESIAN_POINT('Ctrl Pts',(6.13523501225579,-2.8606618575552,118.558214172152));
#212340=CARTESIAN_POINT('Ctrl Pts',(6.20892069740678,-2.69698312382876,
118.566656377462));
#212341=CARTESIAN_POINT('Ctrl Pts',(6.27595185299024,-2.53075430236687,
118.575098582771));
#212342=CARTESIAN_POINT('Ctrl Pts',(6.34305372275449,-2.36435011864497,
118.583549694143));
#212343=CARTESIAN_POINT('Ctrl Pts',(6.40348692293132,-2.19539078338207,
118.592000805515));
#212344=CARTESIAN_POINT('Ctrl Pts',(6.457083557366,-2.02444089397384,118.600451916887));
#212345=CARTESIAN_POINT('Ctrl Pts',(6.47212553584083,-1.97646354271147,
118.602823734385));
#212346=CARTESIAN_POINT('Ctrl Pts',(6.48662933657987,-1.92832947991222,
118.605195551882));
#212347=CARTESIAN_POINT('Ctrl Pts',(6.50059196810422,-1.88005134616555,
118.607567369379));
#212348=CARTESIAN_POINT('Ctrl Pts',(6.54954895883781,-1.71077436264357,
118.615883641783));
#212349=CARTESIAN_POINT('Ctrl Pts',(6.59193723883534,-1.53941978367531,
118.624199914187));
#212350=CARTESIAN_POINT('Ctrl Pts',(6.62758466943129,-1.36653227167141,
118.632516186591));
#212351=CARTESIAN_POINT('Ctrl Pts',(6.66320196008258,-1.19379093626301,
118.640825427577));
#212352=CARTESIAN_POINT('Ctrl Pts',(6.69208968671876,-1.01951958917555,
118.649134668563));
#212353=CARTESIAN_POINT('Ctrl Pts',(6.71412581092551,-0.844276965849392,
118.657443909549));
#212354=CARTESIAN_POINT('Ctrl Pts',(6.73614734380756,-0.669150380261748,
118.665747648532));
#212355=CARTESIAN_POINT('Ctrl Pts',(6.75132627111712,-0.493054144020304,
118.674051387514));
#212356=CARTESIAN_POINT('Ctrl Pts',(6.75959178571707,-0.316556299047095,
118.682355126497));
#212357=CARTESIAN_POINT('Ctrl Pts',(6.7678533420454,-0.140142977112431,
118.690654888902));
#212358=CARTESIAN_POINT('Ctrl Pts',(6.76920806741503,0.0366712234252294,
118.698954651308));
#212359=CARTESIAN_POINT('Ctrl Pts',(6.7636370555824,0.21331380722471,118.707254413713));
#212360=CARTESIAN_POINT('Ctrl Pts',(6.75806769102494,0.389904160127534,
118.715551721988));
#212361=CARTESIAN_POINT('Ctrl Pts',(6.74557668216467,0.566322650083412,
118.723849030263));
#212362=CARTESIAN_POINT('Ctrl Pts',(6.72619722583197,0.741997223182337,
118.732146338537));
#212363=CARTESIAN_POINT('Ctrl Pts',(6.70681581148639,0.917689545647974,
118.740444485135));
#212364=CARTESIAN_POINT('Ctrl Pts',(6.68054458964911,1.09263745441796,118.748742631732));
#212365=CARTESIAN_POINT('Ctrl Pts',(6.64746865322672,1.26627386625808,118.757040778329));
#212366=CARTESIAN_POINT('Ctrl Pts',(6.61438939081074,1.43992773833226,118.765339759357));
#212367=CARTESIAN_POINT('Ctrl Pts',(6.57450411454754,1.61226950852305,118.773638740385));
#212368=CARTESIAN_POINT('Ctrl Pts',(6.52794907622942,1.7827422298682,118.781937721413));
#212369=CARTESIAN_POINT('Ctrl Pts',(6.48138161958898,1.95326042395439,118.790238916153));
#212370=CARTESIAN_POINT('Ctrl Pts',(6.42814094661717,2.1219082397564,118.798540110892));
#212371=CARTESIAN_POINT('Ctrl Pts',(6.36841327360824,2.2881436529489,118.806841305632));
#212372=CARTESIAN_POINT('Ctrl Pts',(6.30865974131138,2.45445103829766,118.8151460944));
#212373=CARTESIAN_POINT('Ctrl Pts',(6.24241372907965,2.61834361210753,118.823450883169));
#212374=CARTESIAN_POINT('Ctrl Pts',(6.16990976519984,2.77929892046388,118.831755671937));
#212375=CARTESIAN_POINT('Ctrl Pts',(6.09731984852195,2.94044503989287,118.840070305958));
#212376=CARTESIAN_POINT('Ctrl Pts',(6.01845730074957,3.09864661903254,118.848384939979));
#212377=CARTESIAN_POINT('Ctrl Pts',(5.93360337404752,3.25340437073105,118.856699574));
#212378=CARTESIAN_POINT('Ctrl Pts',(5.84869579345521,3.40825997712822,118.865019465438));
#212379=CARTESIAN_POINT('Ctrl Pts',(5.75778945781166,3.55966711554366,118.873339356876));
#212380=CARTESIAN_POINT('Ctrl Pts',(5.66120928704602,3.70715502889533,118.881659248314));
#212381=CARTESIAN_POINT('Ctrl Pts',(5.56448469760912,3.85486348450018,118.889991580687));
#212382=CARTESIAN_POINT('Ctrl Pts',(5.46206951923441,3.99864071956232,118.89832391306));
#212383=CARTESIAN_POINT('Ctrl Pts',(5.35433015514444,4.13804755769081,118.906656245434));
#212384=CARTESIAN_POINT('Ctrl Pts',(5.27321484099762,4.24300482715794,118.912929530632));
#212385=CARTESIAN_POINT('Ctrl Pts',(5.18908243876761,4.34548547249859,118.91920281583));
#212386=CARTESIAN_POINT('Ctrl Pts',(5.10210300205094,4.44531595687672,118.925476101029));
#212387=CARTESIAN_POINT('Ctrl Pts',(4.9901919625416,4.573761641319,118.933547547502));
#212388=CARTESIAN_POINT('Ctrl Pts',(4.8732205556082,4.69821570632098,118.941618993974));
#212389=CARTESIAN_POINT('Ctrl Pts',(4.75150793565389,4.81824255693071,118.949690440447));
#212390=CARTESIAN_POINT('Ctrl Pts',(4.6299902243914,4.93807719841335,118.957748961431));
#212391=CARTESIAN_POINT('Ctrl Pts',(4.50374668384009,5.05349848643888,118.965807482416));
#212392=CARTESIAN_POINT('Ctrl Pts',(4.37313732504745,5.16410291689436,118.9738660034));
#212393=CARTESIAN_POINT('Ctrl Pts',(4.24264786178556,5.274605815752,118.9819171269));
#212394=CARTESIAN_POINT('Ctrl Pts',(4.10780083282578,5.38030041198575,118.9899682504));
#212395=CARTESIAN_POINT('Ctrl Pts',(3.96899422323161,5.48081872131839,118.9980193739));
#212396=CARTESIAN_POINT('Ctrl Pts',(3.83030672184986,5.5812507771493,119.006063588832));
#212397=CARTESIAN_POINT('Ctrl Pts',(3.68766670429912,5.67651517070081,119.014107803764));
#212398=CARTESIAN_POINT('Ctrl Pts',(3.54150620200399,5.76628327618122,119.022152018696));
#212399=CARTESIAN_POINT('Ctrl Pts',(3.39731726769152,5.85484049417939,119.030087724719));
#212400=CARTESIAN_POINT('Ctrl Pts',(3.24970253348462,5.93804857724542,119.038023430743));
#212401=CARTESIAN_POINT('Ctrl Pts',(3.09910619832142,6.01563211736936,119.045959136766));
#212402=CARTESIAN_POINT('Ctrl Pts',(3.09910619832145,6.01563211736934,117.045755263024));
#212403=CARTESIAN_POINT('Ctrl Pts',(2.93375330764837,6.10081787314648,117.054504710927));
#212404=CARTESIAN_POINT('Ctrl Pts',(2.76488627843081,6.17918207037034,117.063254158829));
#212405=CARTESIAN_POINT('Ctrl Pts',(2.59307866646713,6.25045854553993,117.072003606731));
#212406=CARTESIAN_POINT('Ctrl Pts',(2.42127244185382,6.32173444515035,117.080752983982));
#212407=CARTESIAN_POINT('Ctrl Pts',(2.24652594672465,6.38592262741838,117.089502361232));
#212408=CARTESIAN_POINT('Ctrl Pts',(2.06943269687116,6.44280508110563,117.098251738482));
#212409=CARTESIAN_POINT('Ctrl Pts',(1.89234081822072,6.49968709436168,117.107001047987));
#212410=CARTESIAN_POINT('Ctrl Pts',(1.71290249405584,6.54926340459546,117.115750357493));
#212411=CARTESIAN_POINT('Ctrl Pts',(1.53172716625054,6.59136563150385,117.124499666998));
#212412=CARTESIAN_POINT('Ctrl Pts',(1.35055318107334,6.6334675464071,117.133248911665));
#212413=CARTESIAN_POINT('Ctrl Pts',(1.16764249714424,6.66809542395775,117.141998156333));
#212414=CARTESIAN_POINT('Ctrl Pts',(0.983616340614447,6.69513165624667,
117.150747401));
#212415=CARTESIAN_POINT('Ctrl Pts',(0.799591486713932,6.7221676971596,117.159496583736));
#212416=CARTESIAN_POINT('Ctrl Pts',(0.614451459526802,6.7416121586937,117.168245766471));
#212417=CARTESIAN_POINT('Ctrl Pts',(0.428825047910371,6.75339900185712,
117.176994949207));
#212418=CARTESIAN_POINT('Ctrl Pts',(0.243199888597042,6.76518576550221,
117.185744072918));
#212419=CARTESIAN_POINT('Ctrl Pts',(0.0570886373918207,6.76931499599835,
117.194493196628));
#212420=CARTESIAN_POINT('Ctrl Pts',(-0.128876626811339,6.76577266947846,
117.203242320339));
#212421=CARTESIAN_POINT('Ctrl Pts',(-0.314840698188291,6.76223036567992,
117.21199138793));
#212422=CARTESIAN_POINT('Ctrl Pts',(-0.500658497951327,6.75101660879222,
117.220740455522));
#212423=CARTESIAN_POINT('Ctrl Pts',(-0.685698951926234,6.73216948296218,
117.229489523113));
#212424=CARTESIAN_POINT('Ctrl Pts',(-0.870738280459779,6.71332247176294,
117.238238537492));
#212425=CARTESIAN_POINT('Ctrl Pts',(-1.05499998761234,6.68684221356189,
117.24698755187));
#212426=CARTESIAN_POINT('Ctrl Pts',(-1.23785829161395,6.65281863948527,
117.255736566249));
#212427=CARTESIAN_POINT('Ctrl Pts',(-1.43007412917375,6.61705395368867,
117.264933299948));
#212428=CARTESIAN_POINT('Ctrl Pts',(-1.6207388253576,6.57295372727798,117.274130033647));
#212429=CARTESIAN_POINT('Ctrl Pts',(-1.80913696091478,6.52068343478289,
117.283326767346));
#212430=CARTESIAN_POINT('Ctrl Pts',(-1.98838356186077,6.47095219815209,
117.29207676506));
#212431=CARTESIAN_POINT('Ctrl Pts',(-2.16557827572498,6.41382586850902,
117.300826762774));
#212432=CARTESIAN_POINT('Ctrl Pts',(-2.34011918621666,6.3494984994329,117.309576760487));
#212433=CARTESIAN_POINT('Ctrl Pts',(-2.5146565569107,6.28517243495562,117.318326580746));
#212434=CARTESIAN_POINT('Ctrl Pts',(-2.68653996295305,6.21364572242384,
117.327076401004));
#212435=CARTESIAN_POINT('Ctrl Pts',(-2.85518555379971,6.13516132252229,
117.335826221262));
#212436=CARTESIAN_POINT('Ctrl Pts',(-3.02382794858662,6.0566784100052,117.3445758757));
#212437=CARTESIAN_POINT('Ctrl Pts',(-3.18923239109245,5.971238194921,117.353325530137));
#212438=CARTESIAN_POINT('Ctrl Pts',(-3.35083705967653,5.87913088810739,
117.362075184575));
#212439=CARTESIAN_POINT('Ctrl Pts',(-3.51243888042351,5.78702520443133,
117.370824684824));
#212440=CARTESIAN_POINT('Ctrl Pts',(-3.67024081223638,5.68825280605817,
117.379574185073));
#212441=CARTESIAN_POINT('Ctrl Pts',(-3.82370687544346,5.58314917682543,
117.388323685322));
#212442=CARTESIAN_POINT('Ctrl Pts',(-3.97717043817757,5.47804726008063,
117.397073043012));
#212443=CARTESIAN_POINT('Ctrl Pts',(-4.126298037224,5.36661448084282,117.405822400703));
#212444=CARTESIAN_POINT('Ctrl Pts',(-4.27058317206846,5.24922931204626,
117.414571758393));
#212445=CARTESIAN_POINT('Ctrl Pts',(-4.41486614774769,5.13184589986847,
117.423320985153));
#212446=CARTESIAN_POINT('Ctrl Pts',(-4.55430658194343,5.00851045723098,
117.432070211913));
#212447=CARTESIAN_POINT('Ctrl Pts',(-4.68843089001771,4.8796418710319,117.440819438673));
#212448=CARTESIAN_POINT('Ctrl Pts',(-4.82255336917744,4.75077504208053,
117.449568546129));
#212449=CARTESIAN_POINT('Ctrl Pts',(-4.95135966065025,4.61637541908209,
117.458317653585));
#212450=CARTESIAN_POINT('Ctrl Pts',(-5.0744123086912,4.47689945401985,117.467066761041));
#212451=CARTESIAN_POINT('Ctrl Pts',(-5.19746344226295,4.33742520555662,
117.475815760817));
#212452=CARTESIAN_POINT('Ctrl Pts',(-5.31476088454647,4.19287495491489,
117.484564760594));
#212453=CARTESIAN_POINT('Ctrl Pts',(-5.42590627628735,4.04373961586865,
117.49331376037));
#212454=CARTESIAN_POINT('Ctrl Pts',(-5.53706380672555,3.89458798906894,
117.502063715665));
#212455=CARTESIAN_POINT('Ctrl Pts',(-5.64206777071757,3.74085050155445,
117.510813670959));
#212456=CARTESIAN_POINT('Ctrl Pts',(-5.74056148163907,3.58304938223323,
117.519563626254));
#212457=CARTESIAN_POINT('Ctrl Pts',(-5.83905138951784,3.42525435593452,
117.528313243695));
#212458=CARTESIAN_POINT('Ctrl Pts',(-5.93103139557555,3.26339625497361,
117.537062861136));
#212459=CARTESIAN_POINT('Ctrl Pts',(-6.01618907820751,3.0980248506519,117.545812478578));
#212460=CARTESIAN_POINT('Ctrl Pts',(-6.10134392544887,2.93265895249839,
117.554561804693));
#212461=CARTESIAN_POINT('Ctrl Pts',(-6.17967677261736,2.76378023986248,
117.563311130809));
#212462=CARTESIAN_POINT('Ctrl Pts',(-6.2509215700913,2.59196229227342,117.572060456925));
#212463=CARTESIAN_POINT('Ctrl Pts',(-6.32216437407667,2.42014915229315,
117.580809538228));
#212464=CARTESIAN_POINT('Ctrl Pts',(-6.38631941548843,2.24539720663073,
117.58955861953));
#212465=CARTESIAN_POINT('Ctrl Pts',(-6.44316881037467,2.06829994947905,
117.598307700832));
#212466=CARTESIAN_POINT('Ctrl Pts',(-6.5000233452451,1.89118668024664,117.607057573175));
#212467=CARTESIAN_POINT('Ctrl Pts',(-6.54957082411042,1.71172794807911,
117.615807445517));
#212468=CARTESIAN_POINT('Ctrl Pts',(-6.59164294296036,1.53053334250543,
117.62455731786));
#212469=CARTESIAN_POINT('Ctrl Pts',(-6.63371214082099,1.34935131693778,
117.633306582714));
#212470=CARTESIAN_POINT('Ctrl Pts',(-6.66830695239664,1.16643393829917,
117.642055847569));
#212471=CARTESIAN_POINT('Ctrl Pts',(-6.6953098815397,0.982402458342261,
117.650805112424));
#212472=CARTESIAN_POINT('Ctrl Pts',(-6.72231419690466,0.798361530948474,
117.659554826431));
#212473=CARTESIAN_POINT('Ctrl Pts',(-6.74172580829263,0.613206671364035,
117.668304540438));
#212474=CARTESIAN_POINT('Ctrl Pts',(-6.75347878028169,0.427566795115099,
117.677054254445));
#212475=CARTESIAN_POINT('Ctrl Pts',(-6.76248992368203,0.285234494207782,
117.683762764234));
#212476=CARTESIAN_POINT('Ctrl Pts',(-6.76699999999988,0.142617266095451,
117.690471274022));
#212477=CARTESIAN_POINT('Ctrl Pts',(-6.767,5.56759968767579E-12,117.69717978381));
#212478=CARTESIAN_POINT('',(-6.7669984993276,-0.00450667260642098,117.302820216158));
#212479=CARTESIAN_POINT('Ctrl Pts',(3.09910619832135,6.0156321173694,116.651219418659));
#212480=CARTESIAN_POINT('Ctrl Pts',(2.92867251040946,6.10343537533217,116.660251113336));
#212481=CARTESIAN_POINT('Ctrl Pts',(2.75459674554507,6.1839446942324,116.669282808013));
#212482=CARTESIAN_POINT('Ctrl Pts',(2.57749842811073,6.25689946004303,116.67831450269));
#212483=CARTESIAN_POINT('Ctrl Pts',(2.40016442018673,6.32995131737167,116.687358217157));
#212484=CARTESIAN_POINT('Ctrl Pts',(2.21980003807894,6.3954284291477,116.696401931623));
#212485=CARTESIAN_POINT('Ctrl Pts',(2.0370438345111,6.45311873564096,116.70544564609));
#212486=CARTESIAN_POINT('Ctrl Pts',(1.90676511509041,6.49424357357369,116.711892505438));
#212487=CARTESIAN_POINT('Ctrl Pts',(1.77527131444625,6.53141248191877,116.718339364787));
#212488=CARTESIAN_POINT('Ctrl Pts',(1.64279789201603,6.56456427236322,116.724786224136));
#212489=CARTESIAN_POINT('Ctrl Pts',(1.46498356534959,6.60906273241299,116.733439612364));
#212490=CARTESIAN_POINT('Ctrl Pts',(1.28524663887641,6.64636072291105,116.742093000592));
#212491=CARTESIAN_POINT('Ctrl Pts',(1.10418302950636,6.67630652661711,116.750746388821));
#212492=CARTESIAN_POINT('Ctrl Pts',(0.92328664522348,6.70622467324921,116.759391785031));
#212493=CARTESIAN_POINT('Ctrl Pts',(0.741066320808893,6.72880412698695,
116.768037181241));
#212494=CARTESIAN_POINT('Ctrl Pts',(0.558129023558517,6.7439440235712,116.776682577452));
#212495=CARTESIAN_POINT('Ctrl Pts',(0.369349325277105,6.75956743745204,
116.785604078494));
#212496=CARTESIAN_POINT('Ctrl Pts',(0.179806414240386,6.7672681523581,116.794525579537));
#212497=CARTESIAN_POINT('Ctrl Pts',(-0.00982353260787742,6.76699286967314,
116.803447080579));
#212498=CARTESIAN_POINT('Ctrl Pts',(-0.193234776334296,6.76672661457755,
116.812076010921));
#212499=CARTESIAN_POINT('Ctrl Pts',(-0.376727102741681,6.75899917527757,
116.820704941263));
#212500=CARTESIAN_POINT('Ctrl Pts',(-0.559685032912536,6.74381506744763,
116.829333871605));
#212501=CARTESIAN_POINT('Ctrl Pts',(-0.7519479628348,6.72785871585952,116.838401657998));
#212502=CARTESIAN_POINT('Ctrl Pts',(-0.943620383670555,6.70366742924272,
116.84746944439));
#212503=CARTESIAN_POINT('Ctrl Pts',(-1.13398931675573,6.67130850954173,
116.856537230783));
#212504=CARTESIAN_POINT('Ctrl Pts',(-1.32435824984104,6.63894958984072,
116.865605017176));
#212505=CARTESIAN_POINT('Ctrl Pts',(-1.51342330428553,6.59842306778905,
116.874672803568));
#212506=CARTESIAN_POINT('Ctrl Pts',(-1.7004785774534,6.54985966320059,116.883740589961));
#212507=CARTESIAN_POINT('Ctrl Pts',(-1.87427319531016,6.50473899806595,
116.892165546094));
#212508=CARTESIAN_POINT('Ctrl Pts',(-2.04625668617868,6.45270058691727,
116.900590502227));
#212509=CARTESIAN_POINT('Ctrl Pts',(-2.21586584529398,6.39392114086963,
116.90901545836));
#212510=CARTESIAN_POINT('Ctrl Pts',(-2.38551437232335,6.33512805154828,
116.917442370007));
#212511=CARTESIAN_POINT('Ctrl Pts',(-2.5527871554529,6.26959091621465,116.925869281653));
#212512=CARTESIAN_POINT('Ctrl Pts',(-2.71713896705784,6.19753538381959,
116.9342961933));
#212513=CARTESIAN_POINT('Ctrl Pts',(-2.88155121722582,6.12545335379853,
116.94272620385));
#212514=CARTESIAN_POINT('Ctrl Pts',(-3.04304005055162,6.04684828027295,
116.9511562144));
#212515=CARTESIAN_POINT('Ctrl Pts',(-3.2010825723603,5.96199290212016,116.95958622495));
#212516=CARTESIAN_POINT('Ctrl Pts',(-3.35927067963495,5.87705935696759,
116.968024001049));
#212517=CARTESIAN_POINT('Ctrl Pts',(-3.51400584031833,5.78586416088612,
116.976461777149));
#212518=CARTESIAN_POINT('Ctrl Pts',(-3.66479104208636,5.68872530694211,
116.984899553248));
#212519=CARTESIAN_POINT('Ctrl Pts',(-3.81565539497006,5.59153546226045,
116.993341758558));
#212520=CARTESIAN_POINT('Ctrl Pts',(-3.96256537950829,5.48839592322071,
117.001783963868));
#212521=CARTESIAN_POINT('Ctrl Pts',(-4.10505463089388,5.3796668556126,117.010226169178));
#212522=CARTESIAN_POINT('Ctrl Pts',(-4.24769420059981,5.27082308482052,
117.01867728055));
#212523=CARTESIAN_POINT('Ctrl Pts',(-4.38590346256215,5.15637821353292,
117.027128391922));
#212524=CARTESIAN_POINT('Ctrl Pts',(-4.51924985333012,5.0367320519535,117.035579503294));
#212525=CARTESIAN_POINT('Ctrl Pts',(-4.55667372445094,5.00315317137592,
117.037951320791));
#212526=CARTESIAN_POINT('Ctrl Pts',(-4.59371479524521,4.96916483055476,
117.040323138288));
#212527=CARTESIAN_POINT('Ctrl Pts',(-4.63036404117311,4.93477637246218,
117.042694955786));
#212528=CARTESIAN_POINT('Ctrl Pts',(-4.75612322711841,4.81677491332864,
117.050833672698));
#212529=CARTESIAN_POINT('Ctrl Pts',(-4.87752809522168,4.69381341047697,
117.05897238961));
#212530=CARTESIAN_POINT('Ctrl Pts',(-4.9941613067096,4.56625030441441,117.067111106523));
#212531=CARTESIAN_POINT('Ctrl Pts',(-5.11068809710025,4.43880359234927,
117.075242397324));
#212532=CARTESIAN_POINT('Ctrl Pts',(-5.22245165363688,4.30676390536643,
117.083373688126));
#212533=CARTESIAN_POINT('Ctrl Pts',(-5.32906974451272,4.17052810302474,
117.091504978927));
#212534=CARTESIAN_POINT('Ctrl Pts',(-5.43561306016616,4.03438784790524,
117.099630566952));
#212535=CARTESIAN_POINT('Ctrl Pts',(-5.53701787134075,3.89405762520549,
117.107756154978));
#212536=CARTESIAN_POINT('Ctrl Pts',(-5.63294069499284,3.7499690834317,117.115881743003));
#212537=CARTESIAN_POINT('Ctrl Pts',(-5.72882107426334,3.6059442986327,117.12400373558));
#212538=CARTESIAN_POINT('Ctrl Pts',(-5.81922409260315,3.45816481004148,
117.132125728157));
#212539=CARTESIAN_POINT('Ctrl Pts',(-5.9038482315136,3.30709314341972,117.140247720735));
#212540=CARTESIAN_POINT('Ctrl Pts',(-5.98845380005447,3.15605462876521,
117.148367930979));
#212541=CARTESIAN_POINT('Ctrl Pts',(-6.06728283432045,3.00172569360243,
117.156488141223));
#212542=CARTESIAN_POINT('Ctrl Pts',(-6.14007862740587,2.84459548077994,
117.164608351467));
#212543=CARTESIAN_POINT('Ctrl Pts',(-6.2128723581993,2.6874697194287,117.172728331666));
#212544=CARTESIAN_POINT('Ctrl Pts',(-6.27963303420768,2.52754317104278,
117.180848311866));
#212545=CARTESIAN_POINT('Ctrl Pts',(-6.34015118731402,2.36532702221082,
117.188968292066));
#212546=CARTESIAN_POINT('Ctrl Pts',(-6.40067919224474,2.20308446601299,
117.197089594128));
#212547=CARTESIAN_POINT('Ctrl Pts',(-6.45496252354291,2.03855191085368,
117.205210896189));
#212548=CARTESIAN_POINT('Ctrl Pts',(-6.50284089981284,1.87225778986797,
117.21333219825));
#212549=CARTESIAN_POINT('Ctrl Pts',(-6.55075870739758,1.70582671361466,
117.221460188793));
#212550=CARTESIAN_POINT('Ctrl Pts',(-6.59226092228593,1.53763152631706,
117.229588179336));
#212551=CARTESIAN_POINT('Ctrl Pts',(-6.62723775543208,1.36821370150117,
117.237716169878));
#212552=CARTESIAN_POINT('Ctrl Pts',(-6.66223011155152,1.19872068782076,
117.245847767682));
#212553=CARTESIAN_POINT('Ctrl Pts',(-6.6906912538452,1.02800431633688,117.253979365486));
#212554=CARTESIAN_POINT('Ctrl Pts',(-6.71256307327743,0.856613090766393,
117.26211096329));
#212555=CARTESIAN_POINT('Ctrl Pts',(-6.73446153202622,0.685013115067537,
117.270252465172));
#212556=CARTESIAN_POINT('Ctrl Pts',(-6.74975460336435,0.512737007993231,
117.278393967054));
#212557=CARTESIAN_POINT('Ctrl Pts',(-6.75843623491466,0.340336096517249,
117.286535468936));
#212558=CARTESIAN_POINT('Ctrl Pts',(-6.7642246089892,0.225389849301825,
117.29196371801));
#212559=CARTESIAN_POINT('Ctrl Pts',(-6.76707501674682,0.110388130318301,
117.297391967084));
#212560=CARTESIAN_POINT('Ctrl Pts',(-6.7669984993276,-0.00450667260661398,
117.302820216158));
#212561=CARTESIAN_POINT('Ctrl Pts',(-6.76699849932715,-0.00450667328524485,
117.30282021619));
#212562=CARTESIAN_POINT('Ctrl Pts',(-6.76678083879045,-0.331335008064387,
117.31826134634));
#212563=CARTESIAN_POINT('Ctrl Pts',(-6.74288468106681,-0.657266287959785,
117.33370247649));
#212564=CARTESIAN_POINT('Ctrl Pts',(-6.69570264497888,-0.979721945259407,
117.34914360664));
#212565=CARTESIAN_POINT('Ctrl Pts',(-6.68403014129684,-1.05949520557632,
117.352963633572));
#212566=CARTESIAN_POINT('Ctrl Pts',(-6.67093255580375,-1.13905600377084,
117.356783660503));
#212567=CARTESIAN_POINT('Ctrl Pts',(-6.65641602025991,-1.21836561229676,
117.360603687435));
#212568=CARTESIAN_POINT('Ctrl Pts',(-6.62574969030051,-1.38590797229451,
117.368673533438));
#212569=CARTESIAN_POINT('Ctrl Pts',(-6.58869694798007,-1.5526011436797,
117.37674337944));
#212570=CARTESIAN_POINT('Ctrl Pts',(-6.54530986498409,-1.71790796358302,
117.384813225443));
#212571=CARTESIAN_POINT('Ctrl Pts',(-6.50197736845718,-1.88300680648052,
117.392872918553));
#212572=CARTESIAN_POINT('Ctrl Pts',(-6.45232648168555,-2.04672241211413,
117.400932611663));
#212573=CARTESIAN_POINT('Ctrl Pts',(-6.39646086475483,-2.20852380690358,
117.408992304773));
#212574=CARTESIAN_POINT('Ctrl Pts',(-6.34065327314052,-2.37015714524538,
117.417043626612));
#212575=CARTESIAN_POINT('Ctrl Pts',(-6.27864391757971,-2.52987987964089,
117.425094948451));
#212576=CARTESIAN_POINT('Ctrl Pts',(-6.21058721372502,-2.68717239132798,
117.433146270289));
#212577=CARTESIAN_POINT('Ctrl Pts',(-6.14258628402404,-2.84433599790761,
117.44119099387));
#212578=CARTESIAN_POINT('Ctrl Pts',(-6.06854801736682,-2.99907300508787,
117.449235717451));
#212579=CARTESIAN_POINT('Ctrl Pts',(-5.98867622569187,-3.15088020461473,
117.457280441032));
#212580=CARTESIAN_POINT('Ctrl Pts',(-5.90885240695776,-3.30259622504508,
117.465320332757));
#212581=CARTESIAN_POINT('Ctrl Pts',(-5.82320221138867,-3.45138561151586,
117.473360224481));
#212582=CARTESIAN_POINT('Ctrl Pts',(-5.73197697556836,-3.59676645774426,
117.481400116206));
#212583=CARTESIAN_POINT('Ctrl Pts',(-5.63878741049257,-3.74527775188946,
117.489613128826));
#212584=CARTESIAN_POINT('Ctrl Pts',(-5.53978014798251,-3.8902316843531,
117.497826141446));
#212585=CARTESIAN_POINT('Ctrl Pts',(-5.43527212771515,-4.03114200911886,
117.506039154066));
#212586=CARTESIAN_POINT('Ctrl Pts',(-5.33300271183239,-4.16903397730253,
117.514076240608));
#212587=CARTESIAN_POINT('Ctrl Pts',(-5.22546604999359,-4.30305350997931,
117.522113327151));
#212588=CARTESIAN_POINT('Ctrl Pts',(-5.11300206604545,-4.4327755269825,
117.530150413693));
#212589=CARTESIAN_POINT('Ctrl Pts',(-5.00052731877043,-4.56250995898668,
117.538188269423));
#212590=CARTESIAN_POINT('Ctrl Pts',(-4.88312455507379,-4.68794577397006,
117.546226125152));
#212591=CARTESIAN_POINT('Ctrl Pts',(-4.76117275337515,-4.80869244311987,
117.554263980881));
#212592=CARTESIAN_POINT('Ctrl Pts',(-4.63918511759793,-4.92947459223446,
117.562304198438));
#212593=CARTESIAN_POINT('Ctrl Pts',(-4.51264604855618,-5.04556459022498,
117.570344415995));
#212594=CARTESIAN_POINT('Ctrl Pts',(-4.3819698787759,-5.15661022198699,
117.578384633552));
#212595=CARTESIAN_POINT('Ctrl Pts',(-4.24635667957483,-5.27185122886583,
117.58672861568));
#212596=CARTESIAN_POINT('Ctrl Pts',(-4.10628800815647,-5.38165897753822,
117.595072597807));
#212597=CARTESIAN_POINT('Ctrl Pts',(-3.96226176371165,-5.48568780699637,
117.603416579935));
#212598=CARTESIAN_POINT('Ctrl Pts',(-3.82323721920956,-5.58610395466622,
117.61147079477));
#212599=CARTESIAN_POINT('Ctrl Pts',(-3.68052571141551,-5.68113568281839,
117.619525009605));
#212600=CARTESIAN_POINT('Ctrl Pts',(-3.53460141385745,-5.77051833418428,
117.62757922444));
#212601=CARTESIAN_POINT('Ctrl Pts',(-3.38856791609294,-5.85996787368426,
117.635639466523));
#212602=CARTESIAN_POINT('Ctrl Pts',(-3.23931716494388,-5.94375973746419,
117.643699708606));
#212603=CARTESIAN_POINT('Ctrl Pts',(-3.08734519441779,-6.02167656475382,
117.651759950689));
#212604=CARTESIAN_POINT('Ctrl Pts',(-2.93516075665225,-6.09970232511277,
117.659831461544));
#212605=CARTESIAN_POINT('Ctrl Pts',(-2.78024784445155,-6.17183650501122,
117.667902972398));
#212606=CARTESIAN_POINT('Ctrl Pts',(-2.62312011777808,-6.23791069571438,
117.675974483252));
#212607=CARTESIAN_POINT('Ctrl Pts',(-2.60665149147746,-6.24483596077004,
117.676820461863));
#212608=CARTESIAN_POINT('Ctrl Pts',(-2.59015854606553,-6.25169470131863,
117.677666440474));
#212609=CARTESIAN_POINT('Ctrl Pts',(-2.57364188029386,-6.25848675575794,
117.678512419085));
#212610=CARTESIAN_POINT('Ctrl Pts',(-2.41297615459709,-6.32455640749932,
117.686741668821));
#212611=CARTESIAN_POINT('Ctrl Pts',(-2.24952853096778,-6.3845323363346,
117.694970918557));
#212612=CARTESIAN_POINT('Ctrl Pts',(-2.08380125520086,-6.43817220403612,
117.703200168293));
#212613=CARTESIAN_POINT('Ctrl Pts',(-1.91827122185263,-6.49174823156894,
117.711419623883));
#212614=CARTESIAN_POINT('Ctrl Pts',(-1.750467276677,-6.53900310420169,117.719639079473));
#212615=CARTESIAN_POINT('Ctrl Pts',(-1.58091304563219,-6.57974185984146,
117.727858535063));
#212616=CARTESIAN_POINT('Ctrl Pts',(-1.41152656104436,-6.62044031107905,
117.736069858833));
#212617=CARTESIAN_POINT('Ctrl Pts',(-1.24039358538537,-6.65463540043232,
117.744281182602));
#212618=CARTESIAN_POINT('Ctrl Pts',(-1.06805445592739,-6.68218143117752,
117.752492506372));
#212619=CARTESIAN_POINT('Ctrl Pts',(-0.895851230706605,-6.70970573950653,
117.760697354806));
#212620=CARTESIAN_POINT('Ctrl Pts',(-0.722444098717129,-6.73059137639154,
117.76890220324));
#212621=CARTESIAN_POINT('Ctrl Pts',(-0.548385275521854,-6.74474333014911,
117.777107051674));
#212622=CARTESIAN_POINT('Ctrl Pts',(-0.374428779043003,-6.75888696417354,
117.785307076594));
#212623=CARTESIAN_POINT('Ctrl Pts',(-0.19982171108126,-6.76630477208352,
117.793507101514));
#212624=CARTESIAN_POINT('Ctrl Pts',(-0.0251232157561799,-6.76695336351819,
117.801707126434));
#212625=CARTESIAN_POINT('Ctrl Pts',(0.149524717866146,-6.76760176723579,
117.809904778081));
#212626=CARTESIAN_POINT('Ctrl Pts',(0.324263667964969,-6.76148485159074,
117.818102429728));
#212627=CARTESIAN_POINT('Ctrl Pts',(0.49853241511165,-6.74861129648782,
117.826300081375));
#212628=CARTESIAN_POINT('Ctrl Pts',(0.672777826603831,-6.73573946523291,
117.834496635306));
#212629=CARTESIAN_POINT('Ctrl Pts',(0.846552802823156,-6.71611282203787,
117.842693189237));
#212630=CARTESIAN_POINT('Ctrl Pts',(1.01929916428635,-6.68979209046777,
117.850889743168));
#212631=CARTESIAN_POINT('Ctrl Pts',(1.19205380372901,-6.66347009761221,
117.859086689877));
#212632=CARTESIAN_POINT('Ctrl Pts',(1.36377937552539,-6.63045343129485,
117.867283636585));
#212633=CARTESIAN_POINT('Ctrl Pts',(1.53392578365535,-6.59085432172775,
117.875480583294));
#212634=CARTESIAN_POINT('Ctrl Pts',(1.70411128214523,-6.55124611444614,
117.883679413214));
#212635=CARTESIAN_POINT('Ctrl Pts',(1.87271654503031,-6.50505253320008,
117.891878243133));
#212636=CARTESIAN_POINT('Ctrl Pts',(2.03920452446303,-6.45243627689647,
117.900077073053));
#212637=CARTESIAN_POINT('Ctrl Pts',(2.20585018929581,-6.39977018627176,
117.908283668313));
#212638=CARTESIAN_POINT('Ctrl Pts',(2.37037422167481,-6.34066937537288,
117.916490263573));
#212639=CARTESIAN_POINT('Ctrl Pts',(2.53225662902831,-6.27534583626609,
117.924696858833));
#212640=CARTESIAN_POINT('Ctrl Pts',(2.69421738839498,-6.2099906801919,117.932907426132));
#212641=CARTESIAN_POINT('Ctrl Pts',(2.85353364655053,-6.13840693797222,
117.941117993431));
#212642=CARTESIAN_POINT('Ctrl Pts',(3.00970816508193,-6.06085355053553,
117.949328560729));
#212643=CARTESIAN_POINT('Ctrl Pts',(3.16609807063245,-5.98319320587497,
117.957550451576));
#212644=CARTESIAN_POINT('Ctrl Pts',(3.31933726223946,-5.89954693422829,
117.965772342423));
#212645=CARTESIAN_POINT('Ctrl Pts',(3.46895468302242,-5.8102187916753,117.97399423327));
#212646=CARTESIAN_POINT('Ctrl Pts',(3.6049922283895,-5.72899842855505,117.981469872424));
#212647=CARTESIAN_POINT('Ctrl Pts',(3.73803581094111,-5.64308146275042,
117.988945511579));
#212648=CARTESIAN_POINT('Ctrl Pts',(3.86775460434079,-5.5527257559329,117.996421150734));
#212649=CARTESIAN_POINT('Ctrl Pts',(4.02281289143836,-5.44471980890373,
118.005357094185));
#212650=CARTESIAN_POINT('Ctrl Pts',(4.17344342205021,-5.33014657741647,
118.014293037636));
#212651=CARTESIAN_POINT('Ctrl Pts',(4.31910750648569,-5.20937609963218,
118.023228981086));
#212652=CARTESIAN_POINT('Ctrl Pts',(4.46455261916716,-5.08878717190847,
118.032151491444));
#212653=CARTESIAN_POINT('Ctrl Pts',(4.60504598436316,-4.96201975113923,
118.041074001802));
#212654=CARTESIAN_POINT('Ctrl Pts',(4.74008005023805,-4.82948549198931,
118.049996512159));
#212655=CARTESIAN_POINT('Ctrl Pts',(4.87478324074672,-4.69727598290337,
118.058897159598));
#212656=CARTESIAN_POINT('Ctrl Pts',(5.00405364606396,-4.55932801802952,
118.067797807036));
#212657=CARTESIAN_POINT('Ctrl Pts',(5.12741923145142,-4.41609114771674,
118.076698454474));
#212658=CARTESIAN_POINT('Ctrl Pts',(5.25059417055246,-4.27307563230872,
118.085585347061));
#212659=CARTESIAN_POINT('Ctrl Pts',(5.36788232438541,-4.12478770982086,
118.094472239647));
#212660=CARTESIAN_POINT('Ctrl Pts',(5.4788486447128,-3.9717132988584,118.103359132233));
#212661=CARTESIAN_POINT('Ctrl Pts',(5.58952974017444,-3.81903234627313,
118.112223182188));
#212662=CARTESIAN_POINT('Ctrl Pts',(5.69392127573436,-3.6615896635484,118.121087232143));
#212663=CARTESIAN_POINT('Ctrl Pts',(5.79162907117197,-3.49990309893799,
118.129951282098));
#212664=CARTESIAN_POINT('Ctrl Pts',(5.88504558365832,-3.34531773638677,
118.138426026918));
#212665=CARTESIAN_POINT('Ctrl Pts',(5.97235265936608,-3.18685345741418,
118.146900771739));
#212666=CARTESIAN_POINT('Ctrl Pts',(6.05324029812882,-3.02499105669906,
118.155375516559));
#212667=CARTESIAN_POINT('Ctrl Pts',(6.13159070502032,-2.86820585255108,
118.163584430988));
#212668=CARTESIAN_POINT('Ctrl Pts',(6.20384168534277,-2.70838306178184,
118.171793345417));
#212669=CARTESIAN_POINT('Ctrl Pts',(6.26976644258405,-2.54603962173548,
118.180002259846));
#212670=CARTESIAN_POINT('Ctrl Pts',(6.33570687310144,-2.38365758536103,
118.188213125903));
#212671=CARTESIAN_POINT('Ctrl Pts',(6.39531795011633,-2.218754035716,118.19642399196));
#212672=CARTESIAN_POINT('Ctrl Pts',(6.44842162997804,-2.05186439172557,
118.204634858017));
#212673=CARTESIAN_POINT('Ctrl Pts',(6.50154740092355,-1.88490532179105,
118.212849139787));
#212674=CARTESIAN_POINT('Ctrl Pts',(6.54816027377841,-1.71595885055863,
118.221063421556));
#212675=CARTESIAN_POINT('Ctrl Pts',(6.5881324939963,-1.54557408154707,118.229277703326));
#212676=CARTESIAN_POINT('Ctrl Pts',(6.62814970610357,-1.37499753102733,
118.237501230919));
#212677=CARTESIAN_POINT('Ctrl Pts',(6.66151125501597,-1.20297979601922,
118.245724758511));
#212678=CARTESIAN_POINT('Ctrl Pts',(6.68814062014948,-1.03007963046874,
118.253948286103));
#212679=CARTESIAN_POINT('Ctrl Pts',(6.71478705367018,-0.857068642637813,
118.262177084657));
#212680=CARTESIAN_POINT('Ctrl Pts',(6.73469266120561,-0.683174449622825,
118.270405883211));
#212681=CARTESIAN_POINT('Ctrl Pts',(6.74783293990576,-0.508959345255335,
118.278634681765));
#212682=CARTESIAN_POINT('Ctrl Pts',(6.76099130514803,-0.334504447737934,
118.286874806601));
#212683=CARTESIAN_POINT('Ctrl Pts',(6.76736572887999,-0.159728111396207,
118.295114931437));
#212684=CARTESIAN_POINT('Ctrl Pts',(6.7669837981931,0.0148079367960404,
118.303355056274));
#212685=CARTESIAN_POINT('Ctrl Pts',(6.76681423672981,0.0922947393577986,
118.307013331644));
#212686=CARTESIAN_POINT('Ctrl Pts',(6.76531368755961,0.169734251754895,
118.310671607014));
#212687=CARTESIAN_POINT('Ctrl Pts',(6.76248782396277,0.247077782803955,
118.314329882384));
#212688=CARTESIAN_POINT('Ctrl Pts',(6.75596208230168,0.425686510891996,
118.322777905146));
#212689=CARTESIAN_POINT('Ctrl Pts',(6.74235031320975,0.604191627816968,
118.331225927909));
#212690=CARTESIAN_POINT('Ctrl Pts',(6.72166304232655,0.782006998319967,
118.339673950672));
#212691=CARTESIAN_POINT('Ctrl Pts',(6.70099471539513,0.959659537977716,
118.348114237327));
#212692=CARTESIAN_POINT('Ctrl Pts',(6.67326384008797,1.13662326053509,118.356554523983));
#212693=CARTESIAN_POINT('Ctrl Pts',(6.63853290694353,1.31231468917632,118.364994810639));
#212694=CARTESIAN_POINT('Ctrl Pts',(6.6038284313199,1.48787227863704,118.373428667607));
#212695=CARTESIAN_POINT('Ctrl Pts',(6.56213459275031,1.66215918028363,118.381862524575));
#212696=CARTESIAN_POINT('Ctrl Pts',(6.51356541899638,1.83459928389132,118.390296381543));
#212697=CARTESIAN_POINT('Ctrl Pts',(6.46502577782156,2.00693453496379,118.398725110288));
#212698=CARTESIAN_POINT('Ctrl Pts',(6.40961922657633,2.17742490662948,118.407153839033));
#212699=CARTESIAN_POINT('Ctrl Pts',(6.34751047084745,2.34550630408062,118.415582567778));
#212700=CARTESIAN_POINT('Ctrl Pts',(6.28542994286655,2.51351131038094,118.424007465758));
#212701=CARTESIAN_POINT('Ctrl Pts',(6.21665339970778,2.67910921329788,118.432432363738));
#212702=CARTESIAN_POINT('Ctrl Pts',(6.14139494116504,2.84175248335115,118.440857261719));
#212703=CARTESIAN_POINT('Ctrl Pts',(6.06615314496755,3.00435974391965,118.449280294413));
#212704=CARTESIAN_POINT('Ctrl Pts',(5.98443243223829,3.16401337239285,118.457703327107));
#212705=CARTESIAN_POINT('Ctrl Pts',(5.89649466467768,3.32018669195388,118.466126359801));
#212706=CARTESIAN_POINT('Ctrl Pts',(5.80856684717554,3.47634234068128,118.474548439439));
#212707=CARTESIAN_POINT('Ctrl Pts',(5.71442354079235,3.62901817502473,118.482970519076));
#212708=CARTESIAN_POINT('Ctrl Pts',(5.61437225641073,3.77771268976951,118.491392598714));
#212709=CARTESIAN_POINT('Ctrl Pts',(5.5143183263064,3.92641113654229,118.499814901062));
#212710=CARTESIAN_POINT('Ctrl Pts',(5.40835629320467,4.07112777735644,118.50823720341));
#212711=CARTESIAN_POINT('Ctrl Pts',(5.29683683583468,4.21139033272206,118.516659505759));
#212712=CARTESIAN_POINT('Ctrl Pts',(5.18529886129325,4.35167617788703,118.525083206582));
#212713=CARTESIAN_POINT('Ctrl Pts',(5.06820183071655,4.48750620249545,118.533506907406));
#212714=CARTESIAN_POINT('Ctrl Pts',(4.94593674310747,4.61844115835413,118.54193060823));
#212715=CARTESIAN_POINT('Ctrl Pts',(4.82358891759602,4.74946471909428,118.550360009448));
#212716=CARTESIAN_POINT('Ctrl Pts',(4.69606627448414,4.87558634785518,118.558789410668));
#212717=CARTESIAN_POINT('Ctrl Pts',(4.56379742723748,4.9964029104087,118.567218811887));
#212718=CARTESIAN_POINT('Ctrl Pts',(4.43148138664995,5.11726258014383,118.575651220704));
#212719=CARTESIAN_POINT('Ctrl Pts',(4.29441601564268,5.23281318910369,118.584083629522));
#212720=CARTESIAN_POINT('Ctrl Pts',(4.15306348123833,5.34269152401714,118.592516038339));
#212721=CARTESIAN_POINT('Ctrl Pts',(4.01158016335622,5.45267152156317,118.600956249067));
#212722=CARTESIAN_POINT('Ctrl Pts',(3.86580202399501,5.5569685594087,118.609396459795));
#212723=CARTESIAN_POINT('Ctrl Pts',(3.71622161234702,5.65526179128119,118.617836670522));
#212724=CARTESIAN_POINT('Ctrl Pts',(3.63114282666162,5.71116930428152,118.622637318359));
#212725=CARTESIAN_POINT('Ctrl Pts',(3.54483446078583,5.76513530901095,118.627437966196));
#212726=CARTESIAN_POINT('Ctrl Pts',(3.45739080292736,5.81710734264319,118.632238614033));
#212727=CARTESIAN_POINT('Ctrl Pts',(3.34011458148202,5.8868103248204,118.638677066548));
#212728=CARTESIAN_POINT('Ctrl Pts',(3.22061103733692,5.9530358029053,118.645115519062));
#212729=CARTESIAN_POINT('Ctrl Pts',(3.09910619832126,6.01563211736944,118.651553971577));
#212730=CARTESIAN_POINT('Origin',(0.,0.,4.30282021618968));
#212731=CARTESIAN_POINT('',(3.09910619832141,6.01563211736936,121.045612484544));
#212732=CARTESIAN_POINT('',(3.09910619832143,6.01563211736935,120.651489390257));
#212733=CARTESIAN_POINT('',(3.09910619832133,6.0156321173694,4.30282021618968));
#212734=CARTESIAN_POINT('',(-6.76699914956147,0.00339261468657372,119.697179783785));
#212735=CARTESIAN_POINT('Ctrl Pts',(-6.76699914956174,0.00339261414470956,
119.69717978381));
#212736=CARTESIAN_POINT('Ctrl Pts',(-6.76708137641015,-0.160619262692798,
119.704869165924));
#212737=CARTESIAN_POINT('Ctrl Pts',(-6.76119737850267,-0.324736712568498,
119.712558548038));
#212738=CARTESIAN_POINT('Ctrl Pts',(-6.74934578577639,-0.488487936414527,
119.720247930153));
#212739=CARTESIAN_POINT('Ctrl Pts',(-6.73669344140177,-0.663302994923102,
119.728456844582));
#212740=CARTESIAN_POINT('Ctrl Pts',(-6.71724560558489,-0.837616821938097,
119.736665759011));
#212741=CARTESIAN_POINT('Ctrl Pts',(-6.69107111035296,-1.01086912911614,
119.74487467344));
#212742=CARTESIAN_POINT('Ctrl Pts',(-6.66489039226773,-1.18416262615027,
119.753085539497));
#212743=CARTESIAN_POINT('Ctrl Pts',(-6.63197988184707,-1.35639374846011,
119.761296405554));
#212744=CARTESIAN_POINT('Ctrl Pts',(-6.59245976822417,-1.52701119981019,
119.769507271611));
#212745=CARTESIAN_POINT('Ctrl Pts',(-6.55292321426923,-1.69769962786792,
119.77772155338));
#212746=CARTESIAN_POINT('Ctrl Pts',(-6.50677165963721,-1.86677270101151,
119.78593583515));
#212747=CARTESIAN_POINT('Ctrl Pts',(-6.4541755230999,-2.0336930242832,119.79415011692));
#212748=CARTESIAN_POINT('Ctrl Pts',(-6.4015201854586,-2.20080122955663,
119.802373644512));
#212749=CARTESIAN_POINT('Ctrl Pts',(-6.3424058845656,-2.36575150549719,
119.810597172105));
#212750=CARTESIAN_POINT('Ctrl Pts',(-6.27705202218472,-2.52802430976974,
119.818820699697));
#212751=CARTESIAN_POINT('Ctrl Pts',(-6.2116562705203,-2.69040112459744,
119.827049498251));
#212752=CARTESIAN_POINT('Ctrl Pts',(-6.14001313035681,-2.85009672266746,
119.835278296805));
#212753=CARTESIAN_POINT('Ctrl Pts',(-6.06238854144283,-3.00661506890768,
119.843507095358));
#212754=CARTESIAN_POINT('Ctrl Pts',(-5.98465710849403,-3.16334885012628,
119.851747220195));
#212755=CARTESIAN_POINT('Ctrl Pts',(-5.90092795213283,-3.3168963326771,
119.859987345031));
#212756=CARTESIAN_POINT('Ctrl Pts',(-5.81151151599038,-3.4667885570815,
119.868227469867));
#212757=CARTESIAN_POINT('Ctrl Pts',(-5.77181430842122,-3.53333451889667,
119.871885745237));
#212758=CARTESIAN_POINT('Ctrl Pts',(-5.73099669508534,-3.5991604421339,
119.875544020608));
#212759=CARTESIAN_POINT('Ctrl Pts',(-5.68908840787528,-3.66422735203196,
119.879202295978));
#212760=CARTESIAN_POINT('Ctrl Pts',(-5.59230997310274,-3.81448578812258,
119.88765031874));
#212761=CARTESIAN_POINT('Ctrl Pts',(-5.48949100218155,-3.9610382232606,
119.896098341503));
#212762=CARTESIAN_POINT('Ctrl Pts',(-5.38093972590706,-4.10338600014126,
119.904546364265));
#212763=CARTESIAN_POINT('Ctrl Pts',(-5.27248785327816,-4.24560342491138,
119.912986650921));
#212764=CARTESIAN_POINT('Ctrl Pts',(-5.15831433985564,-4.38362360234712,
119.921426937577));
#212765=CARTESIAN_POINT('Ctrl Pts',(-5.03877074518791,-4.51697668550973,
119.929867224233));
#212766=CARTESIAN_POINT('Ctrl Pts',(-4.91931821709575,-4.65022818222885,
119.9383010812));
#212767=CARTESIAN_POINT('Ctrl Pts',(-4.79450398471884,-4.77881942476241,
119.946734938168));
#212768=CARTESIAN_POINT('Ctrl Pts',(-4.66472016542312,-4.90231320687437,
119.955168795136));
#212769=CARTESIAN_POINT('Ctrl Pts',(-4.53501526142728,-5.02573189835563,
119.963597523881));
#212770=CARTESIAN_POINT('Ctrl Pts',(-4.40034703612036,-5.14405907969709,
119.972026252626));
#212771=CARTESIAN_POINT('Ctrl Pts',(-4.26114505278284,-5.256893744327,119.980454981371));
#212772=CARTESIAN_POINT('Ctrl Pts',(-4.12200633521901,-5.3696771268402,
119.988879879351));
#212773=CARTESIAN_POINT('Ctrl Pts',(-3.97833822701335,-5.47697276060053,
119.997304777332));
#212774=CARTESIAN_POINT('Ctrl Pts',(-3.83060431115137,-5.57841909606911,
120.005729675312));
#212775=CARTESIAN_POINT('Ctrl Pts',(-3.68290310381919,-5.67984297115365,
120.014152708006));
#212776=CARTESIAN_POINT('Ctrl Pts',(-3.53113815678626,-5.77541993922471,
120.0225757407));
#212777=CARTESIAN_POINT('Ctrl Pts',(-3.3758034807196,-5.86483076137423,
120.030998773394));
#212778=CARTESIAN_POINT('Ctrl Pts',(-3.22048638059502,-5.95423146679083,
120.039420853032));
#212779=CARTESIAN_POINT('Ctrl Pts',(-3.06160064560909,-6.03746725084514,
120.04784293267));
#212780=CARTESIAN_POINT('Ctrl Pts',(-2.89966669282957,-6.11426382081235,
120.056265012307));
#212781=CARTESIAN_POINT('Ctrl Pts',(-2.73772845792289,-6.19106242156231,
120.064687314655));
#212782=CARTESIAN_POINT('Ctrl Pts',(-2.57274214598494,-6.26142132619124,
120.073109617004));
#212783=CARTESIAN_POINT('Ctrl Pts',(-2.40525037739631,-6.32511340783981,
120.081531919352));
#212784=CARTESIAN_POINT('Ctrl Pts',(-2.23773079775204,-6.38881606519631,
120.089955620175));
#212785=CARTESIAN_POINT('Ctrl Pts',(-2.06770524391366,-6.44584957461821,
120.098379320999));
#212786=CARTESIAN_POINT('Ctrl Pts',(-1.89573414841888,-6.49603579412233,
120.106803021823));
#212787=CARTESIAN_POINT('Ctrl Pts',(-1.72364667851209,-6.54625597509986,
120.115232423042));
#212788=CARTESIAN_POINT('Ctrl Pts',(-1.54961135657742,-6.58961951354594,
120.123661824261));
#212789=CARTESIAN_POINT('Ctrl Pts',(-1.37420252704782,-6.6259985220837,
120.13209122548));
#212790=CARTESIAN_POINT('Ctrl Pts',(-1.1987311118915,-6.66239051060118,
120.140523634297));
#212791=CARTESIAN_POINT('Ctrl Pts',(-1.02188553972036,-6.6917929384565,
120.148956043115));
#212792=CARTESIAN_POINT('Ctrl Pts',(-0.844248631611878,-6.71412937379237,
120.157388451933));
#212793=CARTESIAN_POINT('Ctrl Pts',(-0.666447368667443,-6.73648647544811,
120.16582866266));
#212794=CARTESIAN_POINT('Ctrl Pts',(-0.487853638694062,-6.75176448687257,
120.174268873388));
#212795=CARTESIAN_POINT('Ctrl Pts',(-0.309054763744897,-6.75993891636652,
120.182709084115));
#212796=CARTESIAN_POINT('Ctrl Pts',(-0.207357014719193,-6.76458839237324,
120.187509731952));
#212797=CARTESIAN_POINT('Ctrl Pts',(-0.105592923447541,-6.76694071350546,
120.19231037979));
#212798=CARTESIAN_POINT('Ctrl Pts',(-0.00387034878925978,-6.76699889318746,
120.197111027627));
#212799=CARTESIAN_POINT('Ctrl Pts',(0.168604866686761,-6.76709753946359,
120.20525074266));
#212800=CARTESIAN_POINT('Ctrl Pts',(0.341304484230173,-6.76059800410953,
120.213390457692));
#212801=CARTESIAN_POINT('Ctrl Pts',(0.513678841380611,-6.74747530917438,
120.221530172725));
#212802=CARTESIAN_POINT('Ctrl Pts',(0.685902440952836,-6.73436409126946,
120.229662768812));
#212803=CARTESIAN_POINT('Ctrl Pts',(0.857800983717736,-6.71464127147748,
120.237795364899));
#212804=CARTESIAN_POINT('Ctrl Pts',(1.02882394771252,-6.68833389452211,
120.245927960986));
#212805=CARTESIAN_POINT('Ctrl Pts',(1.19972999123408,-6.66204450270096,
120.254054997194));
#212806=CARTESIAN_POINT('Ctrl Pts',(1.3697612872857,-6.62917957153362,120.262182033402));
#212807=CARTESIAN_POINT('Ctrl Pts',(1.53837162302158,-6.58981803614348,
120.27030906961));
#212808=CARTESIAN_POINT('Ctrl Pts',(1.70690135996525,-6.55047531627968,
120.278432220948));
#212809=CARTESIAN_POINT('Ctrl Pts',(1.87401113332999,-6.50464225932621,
120.286555372285));
#212810=CARTESIAN_POINT('Ctrl Pts',(2.03916414515222,-6.45244903808822,
120.294678523623));
#212811=CARTESIAN_POINT('Ctrl Pts',(2.20427074775036,-6.40027048353341,
120.302799392295));
#212812=CARTESIAN_POINT('Ctrl Pts',(2.36742133538362,-6.3417354355619,120.310920260966));
#212813=CARTESIAN_POINT('Ctrl Pts',(2.52809355277149,-6.27702413476603,
120.319041129638));
#212814=CARTESIAN_POINT('Ctrl Pts',(2.68877445350089,-6.21230933672381,
120.327162437193));
#212815=CARTESIAN_POINT('Ctrl Pts',(2.84697637520379,-6.14141775214237,
120.335283744747));
#212816=CARTESIAN_POINT('Ctrl Pts',(3.00219608130839,-6.06457811305754,
120.343405052302));
#212817=CARTESIAN_POINT('Ctrl Pts',(3.08285363631955,-6.0246495655035,120.347625166018));
#212818=CARTESIAN_POINT('Ctrl Pts',(3.16270627987442,-5.98311570679573,
120.351845279735));
#212819=CARTESIAN_POINT('Ctrl Pts',(3.24168590658268,-5.94001359283489,
120.356065393452));
#212820=CARTESIAN_POINT('Ctrl Pts',(3.40983009619075,-5.84825106717607,
120.365049831978));
#212821=CARTESIAN_POINT('Ctrl Pts',(3.57393262566276,-5.74942348196402,
120.374034270503));
#212822=CARTESIAN_POINT('Ctrl Pts',(3.73343998016136,-5.64390954166815,
120.383018709029));
#212823=CARTESIAN_POINT('Ctrl Pts',(3.89322263483352,-5.538213490609,120.39201865416));
#212824=CARTESIAN_POINT('Ctrl Pts',(4.04839406327755,-5.42580815047542,
120.40101859929));
#212825=CARTESIAN_POINT('Ctrl Pts',(4.19843172366319,-5.30711409918221,
120.410018544421));
#212826=CARTESIAN_POINT('Ctrl Pts',(4.34882295164683,-5.18814034231037,
120.419039698153));
#212827=CARTESIAN_POINT('Ctrl Pts',(4.49405601755882,-5.0628483717073,120.428060851885));
#212828=CARTESIAN_POINT('Ctrl Pts',(4.63364125361111,-4.93169927437118,
120.437082005617));
#212829=CARTESIAN_POINT('Ctrl Pts',(4.77336851874162,-4.80041673179451,
120.446112338444));
#212830=CARTESIAN_POINT('Ctrl Pts',(4.9074363036084,-4.66326532437559,120.455142671272));
#212831=CARTESIAN_POINT('Ctrl Pts',(5.03539245172121,-4.52074240110505,
120.464173004099));
#212832=CARTESIAN_POINT('Ctrl Pts',(5.16353000131758,-4.37801742525553,
120.473216139091));
#212833=CARTESIAN_POINT('Ctrl Pts',(5.28553842981156,-4.22990588485169,
120.482259274084));
#212834=CARTESIAN_POINT('Ctrl Pts',(5.40100496908738,-4.0769393328689,120.491302409077));
#212835=CARTESIAN_POINT('Ctrl Pts',(5.50194932634741,-3.94321132500592,
120.499208192477));
#212836=CARTESIAN_POINT('Ctrl Pts',(5.59789442793137,-3.80577330207824,
120.507113975876));
#212837=CARTESIAN_POINT('Ctrl Pts',(5.68859152615184,-3.66499869694295,
120.515019759276));
#212838=CARTESIAN_POINT('Ctrl Pts',(5.78786533146371,-3.51091184061282,
120.523673147504));
#212839=CARTESIAN_POINT('Ctrl Pts',(5.88093826684653,-3.35269069306102,
120.532326535733));
#212840=CARTESIAN_POINT('Ctrl Pts',(5.9674751812739,-3.19085082084388,120.540979923961));
#212841=CARTESIAN_POINT('Ctrl Pts',(6.05393217272209,-3.02916041922923,
120.549625320171));
#212842=CARTESIAN_POINT('Ctrl Pts',(6.13386504024526,-2.86385822610878,
120.558270716382));
#212843=CARTESIAN_POINT('Ctrl Pts',(6.20698323842898,-2.69548661244342,
120.566916112592));
#212844=CARTESIAN_POINT('Ctrl Pts',(6.2824365855564,-2.52173777661496,120.575837613634));
#212845=CARTESIAN_POINT('Ctrl Pts',(6.35063259972096,-2.34472048992701,
120.584759114677));
#212846=CARTESIAN_POINT('Ctrl Pts',(6.41130354045417,-2.16505794660555,
120.593680615719));
#212847=CARTESIAN_POINT('Ctrl Pts',(6.46998484518969,-1.99128723649631,
120.602309546061));
#212848=CARTESIAN_POINT('Ctrl Pts',(6.52162667706992,-1.81504232630351,
120.610938476403));
#212849=CARTESIAN_POINT('Ctrl Pts',(6.56603554749569,-1.63690750777894,
120.619567406745));
#212850=CARTESIAN_POINT('Ctrl Pts',(6.61270299467635,-1.44971298662063,
120.628635193138));
#212851=CARTESIAN_POINT('Ctrl Pts',(6.65138245437574,-1.26043162289371,
120.63770297953));
#212852=CARTESIAN_POINT('Ctrl Pts',(6.68190856630119,-1.06976021219282,
120.646770765923));
#212853=CARTESIAN_POINT('Ctrl Pts',(6.71243467822665,-0.879088801491813,
120.655838552316));
#212854=CARTESIAN_POINT('Ctrl Pts',(6.73480734588162,-0.687027723853866,
120.664906338708));
#212855=CARTESIAN_POINT('Ctrl Pts',(6.74892353752581,-0.494287451418825,
120.673974125101));
#212856=CARTESIAN_POINT('Ctrl Pts',(6.76203900917683,-0.315210853222223,
120.682399081234));
#212857=CARTESIAN_POINT('Ctrl Pts',(6.76802162613719,-0.135626539707275,
120.690824037367));
#212858=CARTESIAN_POINT('Ctrl Pts',(6.76685776057962,0.0438753698941443,
120.699248993501));
#212859=CARTESIAN_POINT('Ctrl Pts',(6.76569362487769,0.223418943612258,
120.707675905147));
#212860=CARTESIAN_POINT('Ctrl Pts',(6.75737970147142,0.402879743681405,
120.716102816793));
#212861=CARTESIAN_POINT('Ctrl Pts',(6.74195448164165,0.581668950066981,
120.72452972844));
#212862=CARTESIAN_POINT('Ctrl Pts',(6.72652358935783,0.760523904206612,
120.73295973899));
#212863=CARTESIAN_POINT('Ctrl Pts',(6.70397621487706,0.938706442005982,
120.74138974954));
#212864=CARTESIAN_POINT('Ctrl Pts',(6.67440261827401,1.11563376122145,120.74981976009));
#212865=CARTESIAN_POINT('Ctrl Pts',(6.64480177909213,1.29272406218394,120.758257536189));
#212866=CARTESIAN_POINT('Ctrl Pts',(6.60816184119489,1.46855650711627,120.766695312289));
#212867=CARTESIAN_POINT('Ctrl Pts',(6.56462423554889,1.64255826260264,120.775133088388));
#212868=CARTESIAN_POINT('Ctrl Pts',(6.52106377586943,1.81665135618357,120.783575293698));
#212869=CARTESIAN_POINT('Ctrl Pts',(6.47059851522227,1.9889115243536,120.792017499008));
#212870=CARTESIAN_POINT('Ctrl Pts',(6.41341966854322,2.15878140513183,120.800459704318));
#212871=CARTESIAN_POINT('Ctrl Pts',(6.35618050132671,2.32883048928864,120.80891081569));
#212872=CARTESIAN_POINT('Ctrl Pts',(6.29221371330304,2.49648393746741,120.817361927062));
#212873=CARTESIAN_POINT('Ctrl Pts',(6.22175892252848,2.66120365810985,120.825813038434));
#212874=CARTESIAN_POINT('Ctrl Pts',(6.20198567636399,2.70743250285698,120.828184855931));
#212875=CARTESIAN_POINT('Ctrl Pts',(6.18170168230166,2.75343041392113,120.830556673428));
#212876=CARTESIAN_POINT('Ctrl Pts',(6.1609128881143,2.79918584325284,120.832928490926));
#212877=CARTESIAN_POINT('Ctrl Pts',(6.08800916389898,2.95964446203028,120.841246160876));
#212878=CARTESIAN_POINT('Ctrl Pts',(6.00876218134742,3.11740875883951,120.849563830826));
#212879=CARTESIAN_POINT('Ctrl Pts',(5.92339548843894,3.27195276364761,120.857881500775));
#212880=CARTESIAN_POINT('Ctrl Pts',(5.83812063497889,3.42633050646668,120.866190222385));
#212881=CARTESIAN_POINT('Ctrl Pts',(5.74673936565344,3.57749456176352,120.874498943995));
#212882=CARTESIAN_POINT('Ctrl Pts',(5.64952227878135,3.72494121048282,120.882807665604));
#212883=CARTESIAN_POINT('Ctrl Pts',(5.55236581984638,3.8722959063733,120.891111205608));
#212884=CARTESIAN_POINT('Ctrl Pts',(5.44938098450012,4.01593752467037,120.899414745611));
#212885=CARTESIAN_POINT('Ctrl Pts',(5.34088336776008,4.15538853201283,120.907718285615));
#212886=CARTESIAN_POINT('Ctrl Pts',(5.23243537626774,4.2947757564724,120.916018027699));
#212887=CARTESIAN_POINT('Ctrl Pts',(5.11847984071684,4.42997591510587,120.924317769783));
#212888=CARTESIAN_POINT('Ctrl Pts',(4.99937469894725,4.56054181205766,120.932617511866));
#212889=CARTESIAN_POINT('Ctrl Pts',(4.88030423815276,4.69106969089743,120.940914837236));
#212890=CARTESIAN_POINT('Ctrl Pts',(4.75608739403087,4.81696574089087,120.949212162605));
#212891=CARTESIAN_POINT('Ctrl Pts',(4.62712140323199,4.93781697916725,120.957509487974));
#212892=CARTESIAN_POINT('Ctrl Pts',(4.49814918357328,5.05867405437335,120.965807214091));
#212893=CARTESIAN_POINT('Ctrl Pts',(4.3644276084,5.17448558849553,120.974104940208));
#212894=CARTESIAN_POINT('Ctrl Pts',(4.22639003624488,5.28487618223265,120.982402666325));
#212895=CARTESIAN_POINT('Ctrl Pts',(4.08835066300326,5.39526821632406,120.99070050071));
#212896=CARTESIAN_POINT('Ctrl Pts',(3.94599545500002,5.50023895518012,120.998998335094));
#212897=CARTESIAN_POINT('Ctrl Pts',(3.79978991268035,5.59945404655602,121.007296169478));
#212898=CARTESIAN_POINT('Ctrl Pts',(3.65351899532164,5.69871350143806,121.015597714196));
#212899=CARTESIAN_POINT('Ctrl Pts',(3.50339459407795,5.79221197473081,121.023899258913));
#212900=CARTESIAN_POINT('Ctrl Pts',(3.34991071589721,5.87965876522754,121.03220080363));
#212901=CARTESIAN_POINT('Ctrl Pts',(3.26725634776005,5.92675074192114,121.036671363935));
#212902=CARTESIAN_POINT('Ctrl Pts',(3.18362816542099,5.97208847191001,121.041141924239));
#212903=CARTESIAN_POINT('Ctrl Pts',(3.09910619832141,6.01563211736936,121.045612484544));
#212904=CARTESIAN_POINT('Ctrl Pts',(3.09910619832142,6.01563211736936,119.045959136766));
#212905=CARTESIAN_POINT('Ctrl Pts',(2.94299959721802,6.0960544114258,119.054185207429));
#212906=CARTESIAN_POINT('Ctrl Pts',(2.78368938707234,6.17043254245761,119.062411278092));
#212907=CARTESIAN_POINT('Ctrl Pts',(2.62169848255776,6.23850832062877,119.070637348755));
#212908=CARTESIAN_POINT('Ctrl Pts',(2.46342911699797,6.30502014271794,119.078674435706));
#212909=CARTESIAN_POINT('Ctrl Pts',(2.30260124994709,6.36551589321831,119.086711522657));
#212910=CARTESIAN_POINT('Ctrl Pts',(2.13972395147972,6.41980298852418,119.094748609608));
#212911=CARTESIAN_POINT('Ctrl Pts',(1.97683143186611,6.47409515704667,119.102786447638));
#212912=CARTESIAN_POINT('Ctrl Pts',(1.8118894539032,6.52217739679846,119.110824285668));
#212913=CARTESIAN_POINT('Ctrl Pts',(1.64542309271336,6.56390675177258,119.118862123698));
#212914=CARTESIAN_POINT('Ctrl Pts',(1.47890819253908,6.60564827437322,119.126902305436));
#212915=CARTESIAN_POINT('Ctrl Pts',(1.31086838661548,6.64103313425422,119.134942487173));
#212916=CARTESIAN_POINT('Ctrl Pts',(1.14183965418601,6.66996935556142,119.142982668911));
#212917=CARTESIAN_POINT('Ctrl Pts',(0.965943438688855,6.70008122912024,
119.151349515892));
#212918=CARTESIAN_POINT('Ctrl Pts',(0.788976697826705,6.7232093964497,119.159716362872));
#212919=CARTESIAN_POINT('Ctrl Pts',(0.611548981277227,6.73930981952149,
119.168083209853));
#212920=CARTESIAN_POINT('Ctrl Pts',(0.440751913338224,6.75480855391721,
119.176137379517));
#212921=CARTESIAN_POINT('Ctrl Pts',(0.269528071443023,6.76379536032711,
119.184191549181));
#212922=CARTESIAN_POINT('Ctrl Pts',(0.0984203184121964,6.76628424180685,
119.192245718845));
#212923=CARTESIAN_POINT('Ctrl Pts',(-0.0728152208507917,6.76877498202636,
119.200305903502));
#212924=CARTESIAN_POINT('Ctrl Pts',(-0.243934127675586,6.76475814353421,
119.208366088159));
#212925=CARTESIAN_POINT('Ctrl Pts',(-0.414398837444021,6.7542995642424,
119.216426272817));
#212926=CARTESIAN_POINT('Ctrl Pts',(-0.585102261964316,6.74382633900326,
119.224497744766));
#212927=CARTESIAN_POINT('Ctrl Pts',(-0.755149293307429,6.72689341119881,
119.232569216715));
#212928=CARTESIAN_POINT('Ctrl Pts',(-0.924012146161016,6.70361772133129,
119.240640688665));
#212929=CARTESIAN_POINT('Ctrl Pts',(-0.943148845126037,6.7009799601975,
119.241555403336));
#212930=CARTESIAN_POINT('Ctrl Pts',(-0.962270351802463,6.69826079176369,
119.242470118007));
#212931=CARTESIAN_POINT('Ctrl Pts',(-0.981375910956522,6.69546042639297,
119.243384832678));
#212932=CARTESIAN_POINT('Ctrl Pts',(-1.15325947486922,6.67026688056177,
119.251614082414));
#212933=CARTESIAN_POINT('Ctrl Pts',(-1.32442484658178,6.63841325853528,
119.25984333215));
#212934=CARTESIAN_POINT('Ctrl Pts',(-1.49431643839945,6.59994752872545,
119.268072581886));
#212935=CARTESIAN_POINT('Ctrl Pts',(-1.66400583158525,6.56152757939162,
119.276292037476));
#212936=CARTESIAN_POINT('Ctrl Pts',(-1.83242411721639,6.51651127046675,
119.284511493066));
#212937=CARTESIAN_POINT('Ctrl Pts',(-1.99902150443574,6.46499822310907,
119.292730948656));
#212938=CARTESIAN_POINT('Ctrl Pts',(-2.16545407051533,6.41353613957094,
119.300942272426));
#212939=CARTESIAN_POINT('Ctrl Pts',(-2.33006898551629,6.35559022295231,
119.309153596195));
#212940=CARTESIAN_POINT('Ctrl Pts',(-2.49232723457679,6.29131098864035,
119.317364919965));
#212941=CARTESIAN_POINT('Ctrl Pts',(-2.65445752904232,6.22708244403717,
119.325569768399));
#212942=CARTESIAN_POINT('Ctrl Pts',(-2.81423452719401,6.15653066082484,
119.333774616833));
#212943=CARTESIAN_POINT('Ctrl Pts',(-2.97113487082171,6.07985580251598,
119.341979465267));
#212944=CARTESIAN_POINT('Ctrl Pts',(-3.12794297496018,6.00322602027009,
119.350179490187));
#212945=CARTESIAN_POINT('Ctrl Pts',(-3.2818774721375,5.9204804908737,119.358379515107));
#212946=CARTESIAN_POINT('Ctrl Pts',(-3.43243539507857,5.8318673046128,119.366579540027));
#212947=CARTESIAN_POINT('Ctrl Pts',(-3.5829497431455,5.74327976501576,119.374777191674));
#212948=CARTESIAN_POINT('Ctrl Pts',(-3.73008915283969,5.64882812949028,
119.382974843321));
#212949=CARTESIAN_POINT('Ctrl Pts',(-3.87337545038235,5.54880632392007,
119.391172494968));
#212950=CARTESIAN_POINT('Ctrl Pts',(-4.01664256101049,5.4487979118834,119.399369048899));
#212951=CARTESIAN_POINT('Ctrl Pts',(-4.15605729252507,5.34322101990534,
119.40756560283));
#212952=CARTESIAN_POINT('Ctrl Pts',(-4.29117064977704,5.23241277562198,
119.415762156761));
#212953=CARTESIAN_POINT('Ctrl Pts',(-4.42629048164051,5.12159922142443,
119.423959103469));
#212954=CARTESIAN_POINT('Ctrl Pts',(-4.55710825114736,5.00555404296093,
119.432156050178));
#212955=CARTESIAN_POINT('Ctrl Pts',(-4.6832082046975,4.88465453348075,119.440352996887));
#212956=CARTESIAN_POINT('Ctrl Pts',(-4.80933712913686,4.76372724788965,
119.448551826807));
#212957=CARTESIAN_POINT('Ctrl Pts',(-4.93074581991987,4.6379436582462,119.456750656726));
#212958=CARTESIAN_POINT('Ctrl Pts',(-5.04705550445287,4.50771779673173,
119.464949486646));
#212959=CARTESIAN_POINT('Ctrl Pts',(-5.16347534912545,4.37736859467913,
119.473156081906));
#212960=CARTESIAN_POINT('Ctrl Pts',(-5.27478629954112,4.24256898267375,
119.481362677166));
#212961=CARTESIAN_POINT('Ctrl Pts',(-5.38064940987826,4.10376667562579,
119.489569272426));
#212962=CARTESIAN_POINT('Ctrl Pts',(-5.48656375856759,3.96489718746562,
119.497779839725));
#212963=CARTESIAN_POINT('Ctrl Pts',(-5.58702480383399,3.82202143498506,
119.505990407024));
#212964=CARTESIAN_POINT('Ctrl Pts',(-5.68173713062174,3.6756158910466,119.514200974323));
#212965=CARTESIAN_POINT('Ctrl Pts',(-5.77658007926708,3.52900843290373,
119.522422865169));
#212966=CARTESIAN_POINT('Ctrl Pts',(-5.86565828156683,3.37886176301135,
119.530644756016));
#212967=CARTESIAN_POINT('Ctrl Pts',(-5.94872186452454,3.22567778591224,
119.538866646863));
#212968=CARTESIAN_POINT('Ctrl Pts',(-6.02424626453097,3.08639739914034,
119.546342286018));
#212969=CARTESIAN_POINT('Ctrl Pts',(-6.0947988183756,2.94460650726778,119.553817925173));
#212970=CARTESIAN_POINT('Ctrl Pts',(-6.16022666132065,2.8006957137744,119.561293564328));
#212971=CARTESIAN_POINT('Ctrl Pts',(-6.24075632375582,2.62356794829797,
119.570494703637));
#212972=CARTESIAN_POINT('Ctrl Pts',(-6.3136817809473,2.44287871718486,119.579695842946));
#212973=CARTESIAN_POINT('Ctrl Pts',(-6.37871688280959,2.25926092538245,
119.588896982256));
#212974=CARTESIAN_POINT('Ctrl Pts',(-6.44355477530049,2.07619992749991,
119.598070220465));
#212975=CARTESIAN_POINT('Ctrl Pts',(-6.50055000002209,1.89022828930608,
119.607243458674));
#212976=CARTESIAN_POINT('Ctrl Pts',(-6.54946562842066,1.70199558816595,
119.616416696883));
#212977=CARTESIAN_POINT('Ctrl Pts',(-6.59827946816817,1.51415458091512,
119.625570846478));
#212978=CARTESIAN_POINT('Ctrl Pts',(-6.63904720679574,1.3240620983253,119.634724996073));
#212979=CARTESIAN_POINT('Ctrl Pts',(-6.67158131231452,1.13238323600081,
119.643879145668));
#212980=CARTESIAN_POINT('Ctrl Pts',(-6.70398688902506,0.941461617662176,
119.652997131));
#212981=CARTESIAN_POINT('Ctrl Pts',(-6.72822368441412,0.748966325945265,
119.662115116333));
#212982=CARTESIAN_POINT('Ctrl Pts',(-6.74415522421459,0.555571158087826,
119.671233101665));
#212983=CARTESIAN_POINT('Ctrl Pts',(-6.75926713705514,0.372125555399899,
119.679881995705));
#212984=CARTESIAN_POINT('Ctrl Pts',(-6.76690666210251,0.187870551008656,
119.688530889745));
#212985=CARTESIAN_POINT('Ctrl Pts',(-6.76699914956147,0.00339261468657305,
119.697179783785));
#212986=CARTESIAN_POINT('',(-6.76699963580264,0.00222014570200688,119.302820216224));
#212987=CARTESIAN_POINT('Ctrl Pts',(3.09910619832126,6.01563211736944,118.651553971577));
#212988=CARTESIAN_POINT('Ctrl Pts',(2.94560425794161,6.09471255407224,118.65968792708));
#212989=CARTESIAN_POINT('Ctrl Pts',(2.78890749860663,6.167999247523,118.667821882584));
#212990=CARTESIAN_POINT('Ctrl Pts',(2.62949778773241,6.23522496661591,118.675955838087));
#212991=CARTESIAN_POINT('Ctrl Pts',(2.47020342135523,6.30240204302128,118.684083908083));
#212992=CARTESIAN_POINT('Ctrl Pts',(2.30820034737353,6.36352673437524,118.69221197808));
#212993=CARTESIAN_POINT('Ctrl Pts',(2.14399417848796,6.41837814113579,118.700340048076));
#212994=CARTESIAN_POINT('Ctrl Pts',(1.97987418690326,6.47320076124225,118.708463852367));
#212995=CARTESIAN_POINT('Ctrl Pts',(1.81355374925965,6.52175653697069,118.716587656658));
#212996=CARTESIAN_POINT('Ctrl Pts',(1.64555753385012,6.56387304895434,118.724711460949));
#212997=CARTESIAN_POINT('Ctrl Pts',(1.47761453133848,6.60597622050859,118.73283269202));
#212998=CARTESIAN_POINT('Ctrl Pts',(1.30799716315632,6.64164410195529,118.740953923091));
#212999=CARTESIAN_POINT('Ctrl Pts',(1.13724428424649,6.67075441295426,118.749075154162));
#213000=CARTESIAN_POINT('Ctrl Pts',(0.966483224829056,6.69986611858342,
118.757196774309));
#213001=CARTESIAN_POINT('Ctrl Pts',(0.79458690590592,6.72241955796674,118.765318394456));
#213002=CARTESIAN_POINT('Ctrl Pts',(0.62210361561856,6.73834372019077,118.773440014603));
#213003=CARTESIAN_POINT('Ctrl Pts',(0.496427137110643,6.74994654054612,
118.779357669688));
#213004=CARTESIAN_POINT('Ctrl Pts',(0.37043925022077,6.75803093605965,118.785275324773));
#213005=CARTESIAN_POINT('Ctrl Pts',(0.244353506160759,6.76258681009175,
118.791192979858));
#213006=CARTESIAN_POINT('Ctrl Pts',(0.0529247053570507,6.76950373403966,
118.800177418384));
#213007=CARTESIAN_POINT('Ctrl Pts',(-0.138634788944055,6.76828229191352,
118.80916185691));
#213008=CARTESIAN_POINT('Ctrl Pts',(-0.329655696648002,6.75896561033325,
118.818146295435));
#213009=CARTESIAN_POINT('Ctrl Pts',(-0.521006295037945,6.74963284871662,
118.827146240566));
#213010=CARTESIAN_POINT('Ctrl Pts',(-0.71181621016391,6.73217693322853,
118.836146185696));
#213011=CARTESIAN_POINT('Ctrl Pts',(-0.901421422903568,6.70669280781001,
118.845146130827));
#213012=CARTESIAN_POINT('Ctrl Pts',(-1.09147344519387,6.68114862839581,
118.854167284559));
#213013=CARTESIAN_POINT('Ctrl Pts',(-1.28031484710437,6.64753841780098,
118.863188438291));
#213014=CARTESIAN_POINT('Ctrl Pts',(-1.46728920163244,6.60600873438515,
118.872209592024));
#213015=CARTESIAN_POINT('Ctrl Pts',(-1.65445380404015,6.56443679418906,
118.881239924851));
#213016=CARTESIAN_POINT('Ctrl Pts',(-1.8397473320953,6.51492934064104,118.890270257678));
#213017=CARTESIAN_POINT('Ctrl Pts',(-2.02252710641955,6.45768326134057,
118.899300590505));
#213018=CARTESIAN_POINT('Ctrl Pts',(-2.20556600484802,6.40035602514473,
118.908343725498));
#213019=CARTESIAN_POINT('Ctrl Pts',(-2.38608379566362,6.33526829801148,
118.91738686049));
#213020=CARTESIAN_POINT('Ctrl Pts',(-2.56345421171337,6.2626664851682,118.926429995483));
#213021=CARTESIAN_POINT('Ctrl Pts',(-2.71851681909309,6.19919577426443,
118.934335778883));
#213022=CARTESIAN_POINT('Ctrl Pts',(-2.87117415656889,6.12998298657736,
118.942241562283));
#213023=CARTESIAN_POINT('Ctrl Pts',(-3.02102171042347,6.05522227710511,
118.950147345683));
#213024=CARTESIAN_POINT('Ctrl Pts',(-3.18503949246517,5.97339187389812,
118.958800733911));
#213025=CARTESIAN_POINT('Ctrl Pts',(-3.34583527378926,5.88484121302058,
118.967454122139));
#213026=CARTESIAN_POINT('Ctrl Pts',(-3.5028576916983,5.78984257054629,118.976107510368));
#213027=CARTESIAN_POINT('Ctrl Pts',(-3.65973508826632,5.69493166605687,
118.984752906578));
#213028=CARTESIAN_POINT('Ctrl Pts',(-3.81284581304721,5.59358481451052,
118.993398302788));
#213029=CARTESIAN_POINT('Ctrl Pts',(-3.96166317892922,5.48612010957803,
119.002043698999));
#213030=CARTESIAN_POINT('Ctrl Pts',(-4.11523327016959,5.37522334397685,
119.010965200041));
#213031=CARTESIAN_POINT('Ctrl Pts',(-4.264230937423,5.25781162698386,119.019886701083));
#213032=CARTESIAN_POINT('Ctrl Pts',(-4.40810784960378,5.1342841941464,119.028808202126));
#213033=CARTESIAN_POINT('Ctrl Pts',(-4.54726647853002,5.01480770602967,
119.037437132468));
#213034=CARTESIAN_POINT('Ctrl Pts',(-4.68163461842893,4.88961046105629,
119.04606606281));
#213035=CARTESIAN_POINT('Ctrl Pts',(-4.81074764583352,4.7590961419273,119.054694993152));
#213036=CARTESIAN_POINT('Ctrl Pts',(-4.94642719203587,4.62194403614605,
119.063762779544));
#213037=CARTESIAN_POINT('Ctrl Pts',(-5.07630288384259,4.47892012229055,
119.072830565937));
#213038=CARTESIAN_POINT('Ctrl Pts',(-5.19987686084161,4.33053918491497,
119.081898352329));
#213039=CARTESIAN_POINT('Ctrl Pts',(-5.32345083784064,4.18215824753938,
119.090966138722));
#213040=CARTESIAN_POINT('Ctrl Pts',(-5.44072282307123,4.02842056419096,
119.100033925115));
#213041=CARTESIAN_POINT('Ctrl Pts',(-5.55124157285252,3.86988449437885,
119.109101711507));
#213042=CARTESIAN_POINT('Ctrl Pts',(-5.6539254670784,3.7225873067452,119.11752666764));
#213043=CARTESIAN_POINT('Ctrl Pts',(-5.75073482331306,3.57121271868087,
119.125951623774));
#213044=CARTESIAN_POINT('Ctrl Pts',(-5.84135670959601,3.41626122994974,
119.134376579907));
#213045=CARTESIAN_POINT('Ctrl Pts',(-5.93199963008893,3.2612737754902,119.142803491553));
#213046=CARTESIAN_POINT('Ctrl Pts',(-6.01645204970856,3.10270805124885,
119.1512304032));
#213047=CARTESIAN_POINT('Ctrl Pts',(-6.09444651794385,2.94109004281102,
119.159657314846));
#213048=CARTESIAN_POINT('Ctrl Pts',(-6.17246966778262,2.77941260113724,
119.168087325396));
#213049=CARTESIAN_POINT('Ctrl Pts',(-6.24402998697614,2.61468093572495,
119.176517335946));
#213050=CARTESIAN_POINT('Ctrl Pts',(-6.30890761372049,2.44744228155429,
119.184947346496));
#213051=CARTESIAN_POINT('Ctrl Pts',(-6.37384500437809,2.28004957063213,
119.193385122596));
#213052=CARTESIAN_POINT('Ctrl Pts',(-6.4320872835115,2.11014556637865,119.201822898695));
#213053=CARTESIAN_POINT('Ctrl Pts',(-6.48346368059371,1.93829505040443,
119.210260674795));
#213054=CARTESIAN_POINT('Ctrl Pts',(-6.5348670464971,1.76635432557756,119.218702880105));
#213055=CARTESIAN_POINT('Ctrl Pts',(-6.57939725504807,1.59246537079121,
119.227145085415));
#213056=CARTESIAN_POINT('Ctrl Pts',(-6.61693424303508,1.41720507455688,
119.235587290724));
#213057=CARTESIAN_POINT('Ctrl Pts',(-6.65451083047907,1.24175988835311,
119.244038402097));
#213058=CARTESIAN_POINT('Ctrl Pts',(-6.68507939849873,1.0649407963259,119.252489513469));
#213059=CARTESIAN_POINT('Ctrl Pts',(-6.70857134288537,0.887332822235909,
119.260940624841));
#213060=CARTESIAN_POINT('Ctrl Pts',(-6.71516439346638,0.837486869193784,
119.263312442338));
#213061=CARTESIAN_POINT('Ctrl Pts',(-6.72120036641145,0.787578801027417,
119.265684259835));
#213062=CARTESIAN_POINT('Ctrl Pts',(-6.72667848189145,0.737621584051423,
119.268056077332));
#213063=CARTESIAN_POINT('Ctrl Pts',(-6.75344304358904,0.493544397129153,
119.279644123618));
#213064=CARTESIAN_POINT('Ctrl Pts',(-6.76691898797299,0.248034488533764,
119.291232169904));
#213065=CARTESIAN_POINT('Ctrl Pts',(-6.7669996358024,0.00222014642263019,
119.30282021619));
#213066=CARTESIAN_POINT('Ctrl Pts',(-6.76699963580264,0.00222014570181755,
119.302820216224));
#213067=CARTESIAN_POINT('Ctrl Pts',(-6.76705696129302,-0.172507833740427,
119.311057147787));
#213068=CARTESIAN_POINT('Ctrl Pts',(-6.76034264214386,-0.347406008666543,
119.31929407935));
#213069=CARTESIAN_POINT('Ctrl Pts',(-6.74684347290728,-0.521912015658256,
119.327531010913));
#213070=CARTESIAN_POINT('Ctrl Pts',(-6.73335440568663,-0.696287432209061,
119.335761778422));
#213071=CARTESIAN_POINT('Ctrl Pts',(-6.71309062957964,-0.870270911770145,
119.34399254593));
#213072=CARTESIAN_POINT('Ctrl Pts',(-6.68609099639552,-1.0433006220255,
119.352223313439));
#213073=CARTESIAN_POINT('Ctrl Pts',(-6.65910624848612,-1.21623493858593,
119.360449543211));
#213074=CARTESIAN_POINT('Ctrl Pts',(-6.62539309662568,-1.38821618236226,
119.368675772982));
#213075=CARTESIAN_POINT('Ctrl Pts',(-6.58504218384844,-1.55868804991138,
119.376902002754));
#213076=CARTESIAN_POINT('Ctrl Pts',(-6.54470556828706,-1.72909951552858,
119.385125317791));
#213077=CARTESIAN_POINT('Ctrl Pts',(-6.497735960321,-1.89800232445434,119.393348632829));
#213078=CARTESIAN_POINT('Ctrl Pts',(-6.44427504019162,-2.06485064989295,
119.401571947866));
#213079=CARTESIAN_POINT('Ctrl Pts',(-6.39081239929268,-2.23170434575012,
119.409795527591));
#213080=CARTESIAN_POINT('Ctrl Pts',(-6.330858129143,-2.39650308418088,119.418019107316));
#213081=CARTESIAN_POINT('Ctrl Pts',(-6.26460382614251,-2.55871606503744,
119.426242687041));
#213082=CARTESIAN_POINT('Ctrl Pts',(-6.19834462893252,-2.72094102857702,
119.434466874242));
#213083=CARTESIAN_POINT('Ctrl Pts',(-6.12578460586727,-2.8805795238249,
119.442691061443));
#213084=CARTESIAN_POINT('Ctrl Pts',(-6.0471635143063,-3.03712074689873,
119.450915248645));
#213085=CARTESIAN_POINT('Ctrl Pts',(-5.96852257831873,-3.19370148189932,
119.459141511679));
#213086=CARTESIAN_POINT('Ctrl Pts',(-5.88381768582728,-3.34718306880869,
119.467367774714));
#213087=CARTESIAN_POINT('Ctrl Pts',(-5.79333459240561,-3.49707925281034,
119.475594037748));
#213088=CARTESIAN_POINT('Ctrl Pts',(-5.70281250573809,-3.64704003383819,
119.48382384585));
#213089=CARTESIAN_POINT('Ctrl Pts',(-5.60650744128516,-3.79341202898163,
119.492053653953));
#213090=CARTESIAN_POINT('Ctrl Pts',(-5.50474854942942,-3.93573784792061,
119.500283462055));
#213091=CARTESIAN_POINT('Ctrl Pts',(-5.40287236336662,-4.07822772126085,
119.508522756393));
#213092=CARTESIAN_POINT('Ctrl Pts',(-5.29553000096965,-4.21666181303084,
119.516762050731));
#213093=CARTESIAN_POINT('Ctrl Pts',(-5.18309160179715,-4.35061495048457,
119.525001345068));
#213094=CARTESIAN_POINT('Ctrl Pts',(-5.07057965381129,-4.48465571008855,
119.533246028938));
#213095=CARTESIAN_POINT('Ctrl Pts',(-4.95296526303893,-4.61420940946759,
119.541490712807));
#213096=CARTESIAN_POINT('Ctrl Pts',(-4.83065545569473,-4.73888772481125,
119.549735396677));
#213097=CARTESIAN_POINT('Ctrl Pts',(-4.7081736682752,-4.86374135059429,
119.557991673414));
#213098=CARTESIAN_POINT('Ctrl Pts',(-4.58098353516427,-4.98370565562182,
119.56624795015));
#213099=CARTESIAN_POINT('Ctrl Pts',(-4.44952594158702,-5.09843190551214,
119.574504226887));
#213100=CARTESIAN_POINT('Ctrl Pts',(-4.3887002776264,-5.15151594678656,
119.578324420919));
#213101=CARTESIAN_POINT('Ctrl Pts',(-4.32696140432062,-5.20347915514866,
119.58214461495));
#213102=CARTESIAN_POINT('Ctrl Pts',(-4.2643550524789,-5.25429015057198,
119.585964808981));
#213103=CARTESIAN_POINT('Ctrl Pts',(-4.13210427829957,-5.36162420348957,
119.594034654984));
#213104=CARTESIAN_POINT('Ctrl Pts',(-3.99555418278254,-5.46416000462343,
119.602104500987));
#213105=CARTESIAN_POINT('Ctrl Pts',(-3.85509364570755,-5.56152335091972,
119.610174346989));
#213106=CARTESIAN_POINT('Ctrl Pts',(-3.71480982585413,-5.6587642017422,
119.618234040099));
#213107=CARTESIAN_POINT('Ctrl Pts',(-3.57062565627738,-5.75084533623054,
119.62629373321));
#213108=CARTESIAN_POINT('Ctrl Pts',(-3.42296518189044,-5.83743080160834,
119.63435342632));
#213109=CARTESIAN_POINT('Ctrl Pts',(-3.27545807635908,-5.92392633422796,
119.642404748158));
#213110=CARTESIAN_POINT('Ctrl Pts',(-3.12448217044023,-6.00493736984605,
119.650456069997));
#213111=CARTESIAN_POINT('Ctrl Pts',(-2.97049268230625,-6.08016958845434,
119.658507391835));
#213112=CARTESIAN_POINT('Ctrl Pts',(-2.81662939237062,-6.15534015239671,
119.666552115416));
#213113=CARTESIAN_POINT('Ctrl Pts',(-2.65975776924429,-6.22474116231977,
119.674596838998));
#213114=CARTESIAN_POINT('Ctrl Pts',(-2.50035988398835,-6.28812288767815,
119.682641562579));
#213115=CARTESIAN_POINT('Ctrl Pts',(-2.34105773697832,-6.35146654443104,
119.690681454303));
#213116=CARTESIAN_POINT('Ctrl Pts',(-2.17923269420338,-6.4087979761119,
119.698721346027));
#213117=CARTESIAN_POINT('Ctrl Pts',(-2.01538907681763,-6.45991454038242,
119.706761237752));
#213118=CARTESIAN_POINT('Ctrl Pts',(-1.84801745747078,-6.51213178432462,
119.714974250372));
#213119=CARTESIAN_POINT('Ctrl Pts',(-1.67853970456727,-6.5578633034028,
119.723187262992));
#213120=CARTESIAN_POINT('Ctrl Pts',(-1.50751279804986,-6.59694582088681,
119.731400275612));
#213121=CARTESIAN_POINT('Ctrl Pts',(-1.34014935756891,-6.63519117491895,
119.739437362154));
#213122=CARTESIAN_POINT('Ctrl Pts',(-1.1713028400355,-6.6670694166407,119.747474448697));
#213123=CARTESIAN_POINT('Ctrl Pts',(-1.0015079089637,-6.69247868194462,
119.755511535239));
#213124=CARTESIAN_POINT('Ctrl Pts',(-0.831696727726329,-6.71789037903355,
119.763549390969));
#213125=CARTESIAN_POINT('Ctrl Pts',(-0.660937321720731,-6.73683181152722,
119.771587246698));
#213126=CARTESIAN_POINT('Ctrl Pts',(-0.48977155389521,-6.74925276049098,
119.779625102427));
#213127=CARTESIAN_POINT('Ctrl Pts',(-0.318555491056461,-6.761677359202,
119.787665319984));
#213128=CARTESIAN_POINT('Ctrl Pts',(-0.146933201163257,-6.76757763369418,
119.795705537541));
#213129=CARTESIAN_POINT('Ctrl Pts',(0.0245515112282709,-6.76695546189691,
119.803745755098));
#213130=CARTESIAN_POINT('Ctrl Pts',(0.202515025927437,-6.76630978405051,
119.812089737226));
#213131=CARTESIAN_POINT('Ctrl Pts',(0.380329919503763,-6.75863919060469,
119.820433719353));
#213132=CARTESIAN_POINT('Ctrl Pts',(0.557393166619768,-6.74400488269438,
119.828777701481));
#213133=CARTESIAN_POINT('Ctrl Pts',(0.728307414736377,-6.72987879061182,
119.836831916316));
#213134=CARTESIAN_POINT('Ctrl Pts',(0.898520989872278,-6.70926465342827,
119.844886131151));
#213135=CARTESIAN_POINT('Ctrl Pts',(1.0675015678996,-6.68226977923908,119.852940345986));
#213136=CARTESIAN_POINT('Ctrl Pts',(1.2366085999468,-6.65525470385046,119.861000588069));
#213137=CARTESIAN_POINT('Ctrl Pts',(1.40448043378287,-6.62184945637709,
119.869060830152));
#213138=CARTESIAN_POINT('Ctrl Pts',(1.57059889595873,-6.58221149067798,
119.877121072235));
#213139=CARTESIAN_POINT('Ctrl Pts',(1.73694960313938,-6.54251810838391,
119.88519258309));
#213140=CARTESIAN_POINT('Ctrl Pts',(1.90154169138591,-6.49657472188905,
119.893264093944));
#213141=CARTESIAN_POINT('Ctrl Pts',(2.06387543137661,-6.44458743472071,
119.901335604798));
#213142=CARTESIAN_POINT('Ctrl Pts',(2.08088970222854,-6.43913862423442,
119.902181583409));
#213143=CARTESIAN_POINT('Ctrl Pts',(2.09787918597496,-6.43362346219491,
119.90302756202));
#213144=CARTESIAN_POINT('Ctrl Pts',(2.11484332267144,-6.42804221521234,
119.903873540631));
#213145=CARTESIAN_POINT('Ctrl Pts',(2.27986181797582,-6.37375068270096,
119.912102790367));
#213146=CARTESIAN_POINT('Ctrl Pts',(2.44303082318764,-6.31302084285292,
119.920332040103));
#213147=CARTESIAN_POINT('Ctrl Pts',(2.60381120285945,-6.24599521452455,
119.928561289839));
#213148=CARTESIAN_POINT('Ctrl Pts',(2.76440022772322,-6.17904935759783,
119.936780745429));
#213149=CARTESIAN_POINT('Ctrl Pts',(2.92260595999053,-6.10582276897258,
119.945000201019));
#213150=CARTESIAN_POINT('Ctrl Pts',(3.07790383156231,-6.02650786141145,
119.953219656609));
#213151=CARTESIAN_POINT('Ctrl Pts',(3.23304806103674,-5.94727142310831,
119.961430980379));
#213152=CARTESIAN_POINT('Ctrl Pts',(3.38528984180507,-5.86195882332208,
119.969642304148));
#213153=CARTESIAN_POINT('Ctrl Pts',(3.53412394848384,-5.77081076771306,
119.977853627918));
#213154=CARTESIAN_POINT('Ctrl Pts',(3.68284068665845,-5.67973459019155,
119.986058476352));
#213155=CARTESIAN_POINT('Ctrl Pts',(3.82815479862485,-5.58283230891746,
119.994263324786));
#213156=CARTESIAN_POINT('Ctrl Pts',(3.96958499643833,-5.48039085796367,
120.00246817322));
#213157=CARTESIAN_POINT('Ctrl Pts',(4.11093204944244,-5.3780096308874,120.01066819814));
#213158=CARTESIAN_POINT('Ctrl Pts',(4.24839944717174,-5.27009593102541,
120.01886822306));
#213159=CARTESIAN_POINT('Ctrl Pts',(4.38153420815219,-5.15698041326435,
120.02706824798));
#213160=CARTESIAN_POINT('Ctrl Pts',(4.51463043691663,-5.04389763369678,
120.035265899627));
#213161=CARTESIAN_POINT('Ctrl Pts',(4.6433962511269,-4.92561626394849,120.043463551274));
#213162=CARTESIAN_POINT('Ctrl Pts',(4.76741095459218,-4.80250786465097,
120.051661202921));
#213163=CARTESIAN_POINT('Ctrl Pts',(4.89140905172758,-4.67941595032366,
120.059857756852));
#213164=CARTESIAN_POINT('Ctrl Pts',(5.01065705008485,-4.55149854583567,
120.068054310783));
#213165=CARTESIAN_POINT('Ctrl Pts',(5.12477040735327,-4.41916477084938,
120.076250864714));
#213166=CARTESIAN_POINT('Ctrl Pts',(5.23888923291697,-4.28682465444807,
120.084447811423));
#213167=CARTESIAN_POINT('Ctrl Pts',(5.34787269285735,-4.15006801759549,
120.092644758131));
#213168=CARTESIAN_POINT('Ctrl Pts',(5.45137588092092,-4.00933785118112,
120.10084170484));
#213169=CARTESIAN_POINT('Ctrl Pts',(5.55490284836831,-3.86857535265501,
120.10904053476));
#213170=CARTESIAN_POINT('Ctrl Pts',(5.65294682374694,-3.72383779528758,
120.11723936468));
#213171=CARTESIAN_POINT('Ctrl Pts',(5.74520563340386,-3.57559802409394,
120.125438194599));
#213172=CARTESIAN_POINT('Ctrl Pts',(5.83755182394802,-3.42721785088582,
120.133644789859));
#213173=CARTESIAN_POINT('Ctrl Pts',(5.92410171184173,-3.27532914167813,
120.141851385119));
#213174=CARTESIAN_POINT('Ctrl Pts',(6.00459813564056,-3.12043109673358,
120.150057980379));
#213175=CARTESIAN_POINT('Ctrl Pts',(6.0851335201702,-2.96545808024686,120.158268547678));
#213176=CARTESIAN_POINT('Ctrl Pts',(6.1596094461796,-2.80747314834473,120.166479114977));
#213177=CARTESIAN_POINT('Ctrl Pts',(6.22781656917511,-2.64699636960612,
120.174689682276));
#213178=CARTESIAN_POINT('Ctrl Pts',(6.29611775955756,-2.48629827041624,
120.182911573123));
#213179=CARTESIAN_POINT('Ctrl Pts',(6.35813274121453,-2.32310179173224,
120.191133463969));
#213180=CARTESIAN_POINT('Ctrl Pts',(6.41370139779053,-2.15794424858009,
120.199355354816));
#213181=CARTESIAN_POINT('Ctrl Pts',(6.46422642088154,-2.00777706449482,
120.206830993971));
#213182=CARTESIAN_POINT('Ctrl Pts',(6.50942277505385,-1.85598902333105,
120.214306633126));
#213183=CARTESIAN_POINT('Ctrl Pts',(6.54920683200432,-1.70299115430115,
120.221782272281));
#213184=CARTESIAN_POINT('Ctrl Pts',(6.59676237552186,-1.52010641663347,
120.230718215731));
#213185=CARTESIAN_POINT('Ctrl Pts',(6.6366835183352,-1.33511213433792,120.239654159182));
#213186=CARTESIAN_POINT('Ctrl Pts',(6.66880167438889,-1.14863972927456,
120.248590102633));
#213187=CARTESIAN_POINT('Ctrl Pts',(6.70087154833531,-0.962447641694246,
120.25751261299));
#213188=CARTESIAN_POINT('Ctrl Pts',(6.72516179708992,-0.774782118893723,
120.266435123348));
#213189=CARTESIAN_POINT('Ctrl Pts',(6.74155455269187,-0.586285948219416,
120.275357633706));
#213190=CARTESIAN_POINT('Ctrl Pts',(6.7579071409554,-0.398251651659642,
120.284258281144));
#213191=CARTESIAN_POINT('Ctrl Pts',(6.76640083551289,-0.209391026181027,
120.293158928582));
#213192=CARTESIAN_POINT('Ctrl Pts',(6.76696939358396,-0.0203525501598814,
120.302059576021));
#213193=CARTESIAN_POINT('Ctrl Pts',(6.76753707301869,0.168393790227225,
120.310946468607));
#213194=CARTESIAN_POINT('Ctrl Pts',(6.76020404538767,0.357317175996606,
120.319833361193));
#213195=CARTESIAN_POINT('Ctrl Pts',(6.74495581604873,0.545765553649547,
120.328720253779));
#213196=CARTESIAN_POINT('Ctrl Pts',(6.72974678035114,0.733729548626838,
120.337584303734));
#213197=CARTESIAN_POINT('Ctrl Pts',(6.70666316079215,0.921220715213209,
120.346448353689));
#213198=CARTESIAN_POINT('Ctrl Pts',(6.67574227306163,1.10758932084862,120.355312403644));
#213199=CARTESIAN_POINT('Ctrl Pts',(6.64617941697724,1.28577270015728,120.363787148465));
#213200=CARTESIAN_POINT('Ctrl Pts',(6.60945291378741,1.46292974106706,120.372261893285));
#213201=CARTESIAN_POINT('Ctrl Pts',(6.56563993181082,1.63849360261527,120.380736638106));
#213202=CARTESIAN_POINT('Ctrl Pts',(6.52320124751472,1.80855048890599,120.388945552535));
#213203=CARTESIAN_POINT('Ctrl Pts',(6.47415364599792,1.97694841464193,120.397154466964));
#213204=CARTESIAN_POINT('Ctrl Pts',(6.41866100673713,2.14314719060364,120.405363381393));
#213205=CARTESIAN_POINT('Ctrl Pts',(6.36315517438321,2.30938547948022,120.41357424745));
#213206=CARTESIAN_POINT('Ctrl Pts',(6.30120136433841,2.47342323918611,120.421785113507));
#213207=CARTESIAN_POINT('Ctrl Pts',(6.23301251086401,2.63473794511195,120.429995979563));
#213208=CARTESIAN_POINT('Ctrl Pts',(6.16479529088696,2.79611975781258,120.438210261333));
#213209=CARTESIAN_POINT('Ctrl Pts',(6.09033799866573,2.95477593226773,120.446424543103));
#213210=CARTESIAN_POINT('Ctrl Pts',(6.00990067075137,3.11020625163384,120.454638824873));
#213211=CARTESIAN_POINT('Ctrl Pts',(5.92937280427444,3.26581152009463,120.462862352465));
#213212=CARTESIAN_POINT('Ctrl Pts',(5.84285162179691,3.41818336488845,120.471085880058));
#213213=CARTESIAN_POINT('Ctrl Pts',(5.75064235647865,3.5668475560183,120.47930940765));
#213214=CARTESIAN_POINT('Ctrl Pts',(5.65837398860826,3.71560703511164,120.487538206204));
#213215=CARTESIAN_POINT('Ctrl Pts',(5.56041046892615,3.86065382889616,120.495767004757));
#213216=CARTESIAN_POINT('Ctrl Pts',(5.45709884885961,4.00154484590329,120.503995803311));
#213217=CARTESIAN_POINT('Ctrl Pts',(5.35364502861537,4.14262978812077,120.512235928147));
#213218=CARTESIAN_POINT('Ctrl Pts',(5.24482862550006,4.27954725025028,120.520476052984));
#213219=CARTESIAN_POINT('Ctrl Pts',(5.13103589340455,4.41188844607319,120.52871617782));
#213220=CARTESIAN_POINT('Ctrl Pts',(5.08051661640693,4.47064247549893,120.53237445319));
#213221=CARTESIAN_POINT('Ctrl Pts',(5.02901698301694,4.52849502504167,120.53603272856));
#213222=CARTESIAN_POINT('Ctrl Pts',(4.97657296742637,4.58541279492709,120.53969100393));
#213223=CARTESIAN_POINT('Ctrl Pts',(4.85544412036637,4.71687457880862,120.548140446117));
#213224=CARTESIAN_POINT('Ctrl Pts',(4.72899783207813,4.84364795984233,120.556589888304));
#213225=CARTESIAN_POINT('Ctrl Pts',(4.59762346793425,4.96529429612186,120.565039330491));
#213226=CARTESIAN_POINT('Ctrl Pts',(4.46639956677605,5.08680131092057,120.573479095537));
#213227=CARTESIAN_POINT('Ctrl Pts',(4.33025909046391,5.20319276688578,120.581918860583));
#213228=CARTESIAN_POINT('Ctrl Pts',(4.18962887805883,5.31406613283421,120.590358625629));
#213229=CARTESIAN_POINT('Ctrl Pts',(4.04909396097928,5.42486436760478,120.598792671632));
#213230=CARTESIAN_POINT('Ctrl Pts',(3.90407563137865,5.53015175787443,120.607226717635));
#213231=CARTESIAN_POINT('Ctrl Pts',(3.75503519795098,5.62956478443487,120.615660763638));
#213232=CARTESIAN_POINT('Ctrl Pts',(3.60609226047604,5.72891277919478,120.624089292445));
#213233=CARTESIAN_POINT('Ctrl Pts',(3.45313274279014,5.82239388875738,120.632517821252));
#213234=CARTESIAN_POINT('Ctrl Pts',(3.29664857169228,5.90968672560223,120.640946350059));
#213235=CARTESIAN_POINT('Ctrl Pts',(3.23140116635628,5.94608421595916,120.644460696791));
#213236=CARTESIAN_POINT('Ctrl Pts',(3.16554133918318,5.98140636140324,120.647975043524));
#213237=CARTESIAN_POINT('Ctrl Pts',(3.09910619832143,6.01563211736935,120.651489390257));
#213238=CARTESIAN_POINT('Origin',(0.,0.,4.30282021618968));
#213239=CARTESIAN_POINT('',(3.09910619832136,6.01563211736939,123.045720569644));
#213240=CARTESIAN_POINT('',(3.09910619832147,6.01563211736933,122.651395695404));
#213241=CARTESIAN_POINT('',(3.09910619832133,6.0156321173694,4.30282021618968));
#213242=CARTESIAN_POINT('',(-6.76699803762956,-0.00515351508554775,121.69717978385));
#213243=CARTESIAN_POINT('Ctrl Pts',(-6.76699803762956,-0.0051535150855464,
121.69717978385));
#213244=CARTESIAN_POINT('Ctrl Pts',(-6.76684306719459,-0.208642708749951,
121.706729803712));
#213245=CARTESIAN_POINT('Ctrl Pts',(-6.75750558641317,-0.411774755921207,
121.716279823574));
#213246=CARTESIAN_POINT('Ctrl Pts',(-6.73910552699447,-0.613796135563451,
121.725829843436));
#213247=CARTESIAN_POINT('Ctrl Pts',(-6.72060756771969,-0.816892395647138,
121.735430675392));
#213248=CARTESIAN_POINT('Ctrl Pts',(-6.69295042803033,-1.01886605019071,
121.745031507349));
#213249=CARTESIAN_POINT('Ctrl Pts',(-6.65630536300722,-1.21897002194531,
121.754632339306));
#213250=CARTESIAN_POINT('Ctrl Pts',(-6.61944545005337,-1.42024719189828,
121.764289460394));
#213251=CARTESIAN_POINT('Ctrl Pts',(-6.57349197828484,-1.61963260654731,
121.773946581483));
#213252=CARTESIAN_POINT('Ctrl Pts',(-6.51866788492275,-1.81638597387141,
121.783603702571));
#213253=CARTESIAN_POINT('Ctrl Pts',(-6.51289434254675,-1.83710613236748,
121.784620697005));
#213254=CARTESIAN_POINT('Ctrl Pts',(-6.50702246635849,-1.85779711962993,
121.78563769144));
#213255=CARTESIAN_POINT('Ctrl Pts',(-6.50105254746679,-1.87845808446065,
121.786654685875));
#213256=CARTESIAN_POINT('Ctrl Pts',(-6.44859713984116,-2.05999812743206,
121.795590629325));
#213257=CARTESIAN_POINT('Ctrl Pts',(-6.38849998283156,-2.23945540325317,
121.804526572776));
#213258=CARTESIAN_POINT('Ctrl Pts',(-6.32093840089574,-2.41620088818825,
121.813462516227));
#213259=CARTESIAN_POINT('Ctrl Pts',(-6.25347838193716,-2.59268067778064,
121.822385026584));
#213260=CARTESIAN_POINT('Ctrl Pts',(-6.17857641980313,-2.76645656995512,
121.831307536942));
#213261=CARTESIAN_POINT('Ctrl Pts',(-6.09645925375148,-2.93691565547054,
121.8402300473));
#213262=CARTESIAN_POINT('Ctrl Pts',(-6.01454330024006,-3.10695706332791,
121.849130694738));
#213263=CARTESIAN_POINT('Ctrl Pts',(-5.92544753979026,-3.27369765278781,
121.858031342176));
#213264=CARTESIAN_POINT('Ctrl Pts',(-5.82944601008305,-3.43654597168827,
121.866931989614));
#213265=CARTESIAN_POINT('Ctrl Pts',(-5.73359283889089,-3.59914262861163,
121.875818882201));
#213266=CARTESIAN_POINT('Ctrl Pts',(-5.63085531678332,-3.75785879205058,
121.884705774787));
#213267=CARTESIAN_POINT('Ctrl Pts',(-5.52155380558094,-3.91212634919614,
121.893592667373));
#213268=CARTESIAN_POINT('Ctrl Pts',(-5.412533240064,-4.0659973811326,121.902456717328));
#213269=CARTESIAN_POINT('Ctrl Pts',(-5.29698250099016,-4.21544241363451,
121.911320767283));
#213270=CARTESIAN_POINT('Ctrl Pts',(-5.1752653182894,-4.35992177513667,
121.920184817238));
#213271=CARTESIAN_POINT('Ctrl Pts',(-5.05889390015725,-4.49805566729363,
121.928659562058));
#213272=CARTESIAN_POINT('Ctrl Pts',(-4.93688618450119,-4.63165046696655,
121.937134306879));
#213273=CARTESIAN_POINT('Ctrl Pts',(-4.80959786120011,-4.76025812467552,
121.945609051699));
#213274=CARTESIAN_POINT('Ctrl Pts',(-4.6863022368542,-4.88483169938894,
121.953817966128));
#213275=CARTESIAN_POINT('Ctrl Pts',(-4.55817024650373,-5.0046053261003,
121.962026880557));
#213276=CARTESIAN_POINT('Ctrl Pts',(-4.42561854096926,-5.11919813348039,
121.970235794986));
#213277=CARTESIAN_POINT('Ctrl Pts',(-4.29303532194022,-5.23381818471826,
121.978446661043));
#213278=CARTESIAN_POINT('Ctrl Pts',(-4.15603056368776,-5.34325472982332,
121.9866575271));
#213279=CARTESIAN_POINT('Ctrl Pts',(-4.01505408375687,-5.44716712654452,
121.994868393157));
#213280=CARTESIAN_POINT('Ctrl Pts',(-3.87401895773528,-5.55112275073066,
122.003082674927));
#213281=CARTESIAN_POINT('Ctrl Pts',(-3.72900910483554,-5.64954943725195,
122.011296956696));
#213282=CARTESIAN_POINT('Ctrl Pts',(-3.58050346034168,-5.74214976907441,
122.019511238466));
#213283=CARTESIAN_POINT('Ctrl Pts',(-3.43183066102137,-5.83485432988054,
122.027734766059));
#213284=CARTESIAN_POINT('Ctrl Pts',(-3.27965451330539,-5.92171924897578,
122.035958293651));
#213285=CARTESIAN_POINT('Ctrl Pts',(-3.12447955357813,-6.00249252554905,
122.044181821243));
#213286=CARTESIAN_POINT('Ctrl Pts',(-2.96920513273786,-6.08331757465059,
122.052410619797));
#213287=CARTESIAN_POINT('Ctrl Pts',(-2.81092838942147,-6.15804304621675,
122.060639418351));
#213288=CARTESIAN_POINT('Ctrl Pts',(-2.65017392644733,-6.22646506129913,
122.068868216904));
#213289=CARTESIAN_POINT('Ctrl Pts',(-2.48919819781889,-6.29498125380996,
122.077108341741));
#213290=CARTESIAN_POINT('Ctrl Pts',(-2.32573826943377,-6.35717653365713,
122.085348466577));
#213291=CARTESIAN_POINT('Ctrl Pts',(-2.1603349447785,-6.41289653170616,
122.093588591414));
#213292=CARTESIAN_POINT('Ctrl Pts',(-2.08690269457443,-6.43763391136062,
122.097246866784));
#213293=CARTESIAN_POINT('Ctrl Pts',(-2.01308755571051,-6.46109568883975,
122.100905142154));
#213294=CARTESIAN_POINT('Ctrl Pts',(-1.93893746026329,-6.48327159119435,
122.104563417524));
#213295=CARTESIAN_POINT('Ctrl Pts',(-1.76770330459528,-6.53448220519242,
122.113011440286));
#213296=CARTESIAN_POINT('Ctrl Pts',(-1.59429039342887,-6.57894926341465,
122.121459463049));
#213297=CARTESIAN_POINT('Ctrl Pts',(-1.41925716203101,-6.61649439718826,
122.129907485811));
#213298=CARTESIAN_POINT('Ctrl Pts',(-1.24438421379054,-6.6540051497616,
122.138347772467));
#213299=CARTESIAN_POINT('Ctrl Pts',(-1.067894227451,-6.68460654300549,122.146788059123));
#213300=CARTESIAN_POINT('Ctrl Pts',(-0.890359818097933,-6.70817027171468,
122.155228345779));
#213301=CARTESIAN_POINT('Ctrl Pts',(-0.712960651881478,-6.7317160499173,
122.163662202747));
#213302=CARTESIAN_POINT('Ctrl Pts',(-0.534518978186544,-6.74823480740924,
122.172096059714));
#213303=CARTESIAN_POINT('Ctrl Pts',(-0.355616996016955,-6.75764941027158,
122.180529916682));
#213304=CARTESIAN_POINT('Ctrl Pts',(-0.176823795539978,-6.76705828856664,
122.188958645427));
#213305=CARTESIAN_POINT('Ctrl Pts',(0.00242882315528636,-6.76937160706409,
122.197387374172));
#213306=CARTESIAN_POINT('Ctrl Pts',(0.181553755591427,-6.76456408306039,
122.205816102917));
#213307=CARTESIAN_POINT('Ctrl Pts',(0.360597277710887,-6.75975874402361,
122.214241000898));
#213308=CARTESIAN_POINT('Ctrl Pts',(0.539512896455443,-6.74783902471258,
122.222665898878));
#213309=CARTESIAN_POINT('Ctrl Pts',(0.717713322958444,-6.72883174006067,
122.231090796858));
#213310=CARTESIAN_POINT('Ctrl Pts',(0.895874295597169,-6.70982866365251,
122.239513829552));
#213311=CARTESIAN_POINT('Ctrl Pts',(1.07332006010618,-6.68374118329547,
122.247936862247));
#213312=CARTESIAN_POINT('Ctrl Pts',(1.24946772770158,-6.65064804341895,
122.256359894941));
#213313=CARTESIAN_POINT('Ctrl Pts',(1.42559546438857,-6.6175586479936,122.264781974578));
#213314=CARTESIAN_POINT('Ctrl Pts',(1.60042506929696,-6.57746523485965,
122.273204054216));
#213315=CARTESIAN_POINT('Ctrl Pts',(1.77338282249357,-6.53049786500882,
122.281626133854));
#213316=CARTESIAN_POINT('Ctrl Pts',(1.94634514932715,-6.48352925316857,
122.290048436202));
#213317=CARTESIAN_POINT('Ctrl Pts',(2.11743520404457,-6.42968640996452,
122.29847073855));
#213318=CARTESIAN_POINT('Ctrl Pts',(2.28609307199985,-6.36914966586234,
122.306893040898));
#213319=CARTESIAN_POINT('Ctrl Pts',(2.45477894463458,-6.3086028699782,122.315316741722));
#213320=CARTESIAN_POINT('Ctrl Pts',(2.62103151172699,-6.2413600704372,122.323740442546));
#213321=CARTESIAN_POINT('Ctrl Pts',(2.7843091826631,-6.1676503934106,122.332164143369));
#213322=CARTESIAN_POINT('Ctrl Pts',(2.94769734509162,-6.0938908363718,122.340593544588));
#213323=CARTESIAN_POINT('Ctrl Pts',(3.1081062843796,-6.01365579450131,122.349022945807));
#213324=CARTESIAN_POINT('Ctrl Pts',(3.26501652257053,-5.92722161786966,
122.357452347026));
#213325=CARTESIAN_POINT('Ctrl Pts',(3.42198274611659,-5.8407566016438,122.365884755844));
#213326=CARTESIAN_POINT('Ctrl Pts',(3.57544749035845,-5.74808820662621,
122.374317164661));
#213327=CARTESIAN_POINT('Ctrl Pts',(3.72491829995301,-5.64953738448337,
122.382749573479));
#213328=CARTESIAN_POINT('Ctrl Pts',(3.87452740428954,-5.55089538025249,
122.391189784207));
#213329=CARTESIAN_POINT('Ctrl Pts',(4.02013491565663,-5.44636026341438,
122.399629994934));
#213330=CARTESIAN_POINT('Ctrl Pts',(4.16127873668112,-5.33629536997771,
122.408070205662));
#213331=CARTESIAN_POINT('Ctrl Pts',(4.24155893358552,-5.27369233675089,
122.412870853499));
#213332=CARTESIAN_POINT('Ctrl Pts',(4.32039566512156,-5.20930108386711,
122.417671501336));
#213333=CARTESIAN_POINT('Ctrl Pts',(4.39770895395286,-5.14319404225845,
122.422472149173));
#213334=CARTESIAN_POINT('Ctrl Pts',(4.52879712386033,-5.03110657018901,
122.430611864206));
#213335=CARTESIAN_POINT('Ctrl Pts',(4.6557648994597,-4.91386073521467,122.438751579239));
#213336=CARTESIAN_POINT('Ctrl Pts',(4.77817847597647,-4.79179501353253,
122.446891294272));
#213337=CARTESIAN_POINT('Ctrl Pts',(4.90048499031364,-4.66983604979823,
122.455023890359));
#213338=CARTESIAN_POINT('Ctrl Pts',(5.01824497631346,-4.54306584698048,
122.463156486446));
#213339=CARTESIAN_POINT('Ctrl Pts',(5.13105780714589,-4.41186296021616,
122.471289082533));
#213340=CARTESIAN_POINT('Ctrl Pts',(5.24379351307515,-4.28074977078379,
122.479416118741));
#213341=CARTESIAN_POINT('Ctrl Pts',(5.35158855972921,-4.14521020735507,
122.487543154949));
#213342=CARTESIAN_POINT('Ctrl Pts',(5.45407933864111,-4.0056594423151,122.495670191157));
#213343=CARTESIAN_POINT('Ctrl Pts',(5.55652112510568,-3.8661753850666,122.503793342494));
#213344=CARTESIAN_POINT('Ctrl Pts',(5.65366347659911,-3.72268423896338,
122.511916493832));
#213345=CARTESIAN_POINT('Ctrl Pts',(5.7451832572382,-3.57563397745768,122.520039645169));
#213346=CARTESIAN_POINT('Ctrl Pts',(5.8366773201387,-3.42862503816844,122.528160513841));
#213347=CARTESIAN_POINT('Ctrl Pts',(5.92255176653967,-3.27805928661287,
122.536281382513));
#213348=CARTESIAN_POINT('Ctrl Pts',(6.00252699181003,-3.12441333894733,
122.544402251184));
#213349=CARTESIAN_POINT('Ctrl Pts',(6.08250653924776,-2.97075908766654,
122.552523558739));
#213350=CARTESIAN_POINT('Ctrl Pts',(6.15658605600262,-2.81402463072592,
122.560644866293));
#213351=CARTESIAN_POINT('Ctrl Pts',(6.22453199581333,-2.65471098861932,
122.568766173848));
#213352=CARTESIAN_POINT('Ctrl Pts',(6.25983906806303,-2.57192608214969,
122.572986287565));
#213353=CARTESIAN_POINT('Ctrl Pts',(6.29349072389814,-2.48844511329279,
122.577206401281));
#213354=CARTESIAN_POINT('Ctrl Pts',(6.32545932362092,-2.40434052189309,
122.581426514998));
#213355=CARTESIAN_POINT('Ctrl Pts',(6.39351908178095,-2.22528550539411,
122.590410953524));
#213356=CARTESIAN_POINT('Ctrl Pts',(6.45391403626528,-2.04349171768177,
122.59939539205));
#213357=CARTESIAN_POINT('Ctrl Pts',(6.50646997460851,-1.85960680508486,
122.608379830575));
#213358=CARTESIAN_POINT('Ctrl Pts',(6.5591166213646,-1.67540451810375,122.617379775706));
#213359=CARTESIAN_POINT('Ctrl Pts',(6.60389714413356,-1.4891041223001,122.626379720836));
#213360=CARTESIAN_POINT('Ctrl Pts',(6.6406880904066,-1.30136493188191,122.635379665967));
#213361=CARTESIAN_POINT('Ctrl Pts',(6.67756573548888,-1.11318332924256,
122.644400819699));
#213362=CARTESIAN_POINT('Ctrl Pts',(6.70641608688096,-0.923556383487338,
122.653421973431));
#213363=CARTESIAN_POINT('Ctrl Pts',(6.72716700892878,-0.733152803977599,
122.662443127164));
#213364=CARTESIAN_POINT('Ctrl Pts',(6.74793904520336,-0.542555487324775,
122.671473459991));
#213365=CARTESIAN_POINT('Ctrl Pts',(6.76059516827323,-0.351180196221352,
122.680503792818));
#213366=CARTESIAN_POINT('Ctrl Pts',(6.7651153201899,-0.159698793144974,
122.689534125645));
#213367=CARTESIAN_POINT('Ctrl Pts',(6.76964188025714,0.0320540702023941,
122.698577260638));
#213368=CARTESIAN_POINT('Ctrl Pts',(6.76600940053277,0.223913107298821,
122.707620395631));
#213369=CARTESIAN_POINT('Ctrl Pts',(6.75424998838656,0.415206086636707,
122.716663530623));
#213370=CARTESIAN_POINT('Ctrl Pts',(6.74396955296085,0.582440221899917,
122.724569314023));
#213371=CARTESIAN_POINT('Ctrl Pts',(6.72747867853568,0.749241671908771,
122.732475097423));
#213372=CARTESIAN_POINT('Ctrl Pts',(6.70483124652019,0.915164988232458,
122.740380880823));
#213373=CARTESIAN_POINT('Ctrl Pts',(6.68004217607765,1.09677872587814,122.749034269051));
#213374=CARTESIAN_POINT('Ctrl Pts',(6.64785392676412,1.27750066544207,122.75768765728));
#213375=CARTESIAN_POINT('Ctrl Pts',(6.60834717308811,1.45672119499182,122.766341045508));
#213376=CARTESIAN_POINT('Ctrl Pts',(6.56887690670154,1.63577620166947,122.774986441718));
#213377=CARTESIAN_POINT('Ctrl Pts',(6.52210168245897,1.81333226819031,122.783631837929));
#213378=CARTESIAN_POINT('Ctrl Pts',(6.46815349153584,1.98878842764451,122.792277234139));
#213379=CARTESIAN_POINT('Ctrl Pts',(6.41248237712525,2.16984806578764,122.801198735182));
#213380=CARTESIAN_POINT('Ctrl Pts',(6.34917258687866,2.34867112524306,122.810120236224));
#213381=CARTESIAN_POINT('Ctrl Pts',(6.27842599637712,2.52461007048931,122.819041737266));
#213382=CARTESIAN_POINT('Ctrl Pts',(6.20999946159672,2.69477929378009,122.827670667608));
#213383=CARTESIAN_POINT('Ctrl Pts',(6.13461626194751,2.86225024761858,122.83629959795));
#213384=CARTESIAN_POINT('Ctrl Pts',(6.05250938115007,3.02645323623056,122.844928528292));
#213385=CARTESIAN_POINT('Ctrl Pts',(5.96622665236134,3.19900737292537,122.853996314685));
#213386=CARTESIAN_POINT('Ctrl Pts',(5.8725186044353,3.36795214795712,122.863064101078));
#213387=CARTESIAN_POINT('Ctrl Pts',(5.77171275169471,3.53265069203349,122.87213188747));
#213388=CARTESIAN_POINT('Ctrl Pts',(5.67090689895412,3.69734923610987,122.881199673863));
#213389=CARTESIAN_POINT('Ctrl Pts',(5.56300341523561,3.85780119777594,122.890267460255));
#213390=CARTESIAN_POINT('Ctrl Pts',(5.44838605790935,4.01339985099653,122.899335246648));
#213391=CARTESIAN_POINT('Ctrl Pts',(5.34189812586908,4.15796241286531,122.907759885321));
#213392=CARTESIAN_POINT('Ctrl Pts',(5.22966184849886,4.29827242193654,122.916184523994));
#213393=CARTESIAN_POINT('Ctrl Pts',(5.11205059082547,4.43387277183739,122.924609162667));
#213394=CARTESIAN_POINT('Ctrl Pts',(4.99441265715437,4.56950387793195,122.933035712175));
#213395=CARTESIAN_POINT('Ctrl Pts',(4.87139752987366,4.7004229447189,122.941462261682));
#213396=CARTESIAN_POINT('Ctrl Pts',(4.74341731004143,4.82620774757981,122.949888811189));
#213397=CARTESIAN_POINT('Ctrl Pts',(4.61533543104192,4.95209246571146,122.9583220542));
#213398=CARTESIAN_POINT('Ctrl Pts',(4.48228081448538,5.07283453686664,122.966755297211));
#213399=CARTESIAN_POINT('Ctrl Pts',(4.3447015490879,5.18804948408872,122.975188540221));
#213400=CARTESIAN_POINT('Ctrl Pts',(4.20706729330589,5.30331048268513,122.983625153996));
#213401=CARTESIAN_POINT('Ctrl Pts',(4.06490504063142,5.41303974396053,122.992061767771));
#213402=CARTESIAN_POINT('Ctrl Pts',(3.91869455972253,5.51689423023508,123.000498381546));
#213403=CARTESIAN_POINT('Ctrl Pts',(3.7723277024002,5.62085979193994,123.008944018528));
#213404=CARTESIAN_POINT('Ctrl Pts',(3.62190423832323,5.71893783470141,123.01738965551));
#213405=CARTESIAN_POINT('Ctrl Pts',(3.46793251418037,5.81082894921978,123.025835292491));
#213406=CARTESIAN_POINT('Ctrl Pts',(3.34709022149075,5.88294824916281,123.032463718209));
#213407=CARTESIAN_POINT('Ctrl Pts',(3.22406290923529,5.95125748312322,123.039092143926));
#213408=CARTESIAN_POINT('Ctrl Pts',(3.09910619832137,6.01563211736939,123.045720569644));
#213409=CARTESIAN_POINT('Ctrl Pts',(3.09910619832141,6.01563211736936,121.045612484544));
#213410=CARTESIAN_POINT('Ctrl Pts',(2.94204558016879,6.09654589762258,121.053919780138));
#213411=CARTESIAN_POINT('Ctrl Pts',(2.7818976882948,6.171261813576,121.062227075732));
#213412=CARTESIAN_POINT('Ctrl Pts',(2.61919150026186,6.2395612734355,121.070534371327));
#213413=CARTESIAN_POINT('Ctrl Pts',(2.4562892289586,6.3079430435108,121.078851678351));
#213414=CARTESIAN_POINT('Ctrl Pts',(2.29082282420696,6.36989277750003,121.087168985376));
#213415=CARTESIAN_POINT('Ctrl Pts',(2.12333909727934,6.42524085758386,121.095486292401));
#213416=CARTESIAN_POINT('Ctrl Pts',(1.95573595193907,6.48062840168004,121.103809529791));
#213417=CARTESIAN_POINT('Ctrl Pts',(1.78611294965967,6.52940480989312,121.11213276718));
#213418=CARTESIAN_POINT('Ctrl Pts',(1.61502892522468,6.57145117692338,121.12045600457));
#213419=CARTESIAN_POINT('Ctrl Pts',(1.44371479025191,6.61355409693783,121.128790436836));
#213420=CARTESIAN_POINT('Ctrl Pts',(1.27093604800497,6.64890882715584,121.137124869103));
#213421=CARTESIAN_POINT('Ctrl Pts',(1.09725947931928,6.67744791331569,121.14545930137));
#213422=CARTESIAN_POINT('Ctrl Pts',(1.05990364943842,6.68358634209517,121.147251941772));
#213423=CARTESIAN_POINT('Ctrl Pts',(1.02250629318168,6.68940964984961,121.149044582174));
#213424=CARTESIAN_POINT('Ctrl Pts',(0.985073060578742,6.69491748009802,
121.150837222576));
#213425=CARTESIAN_POINT('Ctrl Pts',(0.81656161670387,6.71971182360619,121.158907068579));
#213426=CARTESIAN_POINT('Ctrl Pts',(0.646802256991129,6.73818555874121,
121.166976914581));
#213427=CARTESIAN_POINT('Ctrl Pts',(0.476320390783657,6.75021539547619,
121.175046760584));
#213428=CARTESIAN_POINT('Ctrl Pts',(0.306053012448628,6.76223009714639,
121.183106453694));
#213429=CARTESIAN_POINT('Ctrl Pts',(0.135065303714053,6.76781700567055,
121.191166146804));
#213430=CARTESIAN_POINT('Ctrl Pts',(-0.0361066108435397,6.76690367248222,
121.199225839914));
#213431=CARTESIAN_POINT('Ctrl Pts',(-0.207100736180612,6.76599128793548,
121.207277161753));
#213432=CARTESIAN_POINT('Ctrl Pts',(-0.378278316683939,6.75859209926884,
121.215328483592));
#213433=CARTESIAN_POINT('Ctrl Pts',(-0.549097671755492,6.74468537048784,
121.22337980543));
#213434=CARTESIAN_POINT('Ctrl Pts',(-0.719777036137056,6.73079003861533,
121.231424529011));
#213435=CARTESIAN_POINT('Ctrl Pts',(-0.890098389427189,6.7103978113129,
121.239469252592));
#213436=CARTESIAN_POINT('Ctrl Pts',(-1.0595197193612,6.68354000244517,121.247513976173));
#213437=CARTESIAN_POINT('Ctrl Pts',(-1.22883929072215,6.65669832503094,
121.255553867898));
#213438=CARTESIAN_POINT('Ctrl Pts',(-1.39725954727955,6.6233988549412,121.263593759622));
#213439=CARTESIAN_POINT('Ctrl Pts',(-1.56424337856943,6.58372475522798,
121.271633651346));
#213440=CARTESIAN_POINT('Ctrl Pts',(-1.73482282923047,6.5431963634533,121.279846663966));
#213441=CARTESIAN_POINT('Ctrl Pts',(-1.90390289527555,6.49601573360834,
121.288059676586));
#213442=CARTESIAN_POINT('Ctrl Pts',(-2.0709212771454,6.44232675854512,121.296272689206));
#213443=CARTESIAN_POINT('Ctrl Pts',(-2.23436205721034,6.3897878232077,121.304309775749));
#213444=CARTESIAN_POINT('Ctrl Pts',(-2.39582821654682,6.33101667239781,
121.312346862291));
#213445=CARTESIAN_POINT('Ctrl Pts',(-2.55480799265003,6.26619861803722,
121.320383948834));
#213446=CARTESIAN_POINT('Ctrl Pts',(-2.71380298385776,6.20137436028714,
121.328421804563));
#213447=CARTESIAN_POINT('Ctrl Pts',(-2.87031077198364,6.13050218760935,
121.336459660292));
#213448=CARTESIAN_POINT('Ctrl Pts',(-3.02383976469844,6.0538154974717,121.344497516021));
#213449=CARTESIAN_POINT('Ctrl Pts',(-3.1774138700719,5.97710627386715,121.352537733578));
#213450=CARTESIAN_POINT('Ctrl Pts',(-3.32800710375322,5.89457929890251,
121.360577951135));
#213451=CARTESIAN_POINT('Ctrl Pts',(-3.47515279545853,5.80651376027103,
121.368618168692));
#213452=CARTESIAN_POINT('Ctrl Pts',(-3.62785774567492,5.71512104916513,
121.37696215082));
#213453=CARTESIAN_POINT('Ctrl Pts',(-3.7768491831015,5.61776332756665,121.385306132948));
#213454=CARTESIAN_POINT('Ctrl Pts',(-3.92163979247268,5.51480102434302,
121.393650115075));
#213455=CARTESIAN_POINT('Ctrl Pts',(-4.061402157267,5.41541436490633,121.40170432991));
#213456=CARTESIAN_POINT('Ctrl Pts',(-4.1972503219034,5.31080614354025,121.409758544745));
#213457=CARTESIAN_POINT('Ctrl Pts',(-4.32878130281717,5.20134034960033,
121.41781275958));
#213458=CARTESIAN_POINT('Ctrl Pts',(-4.46041071291908,5.09179263861584,
121.425873001663));
#213459=CARTESIAN_POINT('Ctrl Pts',(-4.58771623060037,4.97738036514048,
121.433933243746));
#213460=CARTESIAN_POINT('Ctrl Pts',(-4.7103326365377,4.8585034170172,121.441993485829));
#213461=CARTESIAN_POINT('Ctrl Pts',(-4.83312046862225,4.73946027076525,
121.450064996684));
#213462=CARTESIAN_POINT('Ctrl Pts',(-4.95120585348521,4.61594026364948,
121.458136507538));
#213463=CARTESIAN_POINT('Ctrl Pts',(-5.06426426442198,4.48837570398229,
121.466208018392));
#213464=CARTESIAN_POINT('Ctrl Pts',(-5.07611396631286,4.47500560624809,
121.467053997003));
#213465=CARTESIAN_POINT('Ctrl Pts',(-5.08790848559677,4.46159110345672,
121.467899975614));
#213466=CARTESIAN_POINT('Ctrl Pts',(-5.09964747685105,4.44813271068285,
121.468745954225));
#213467=CARTESIAN_POINT('Ctrl Pts',(-5.21424242035397,4.31675312906851,
121.477004318936));
#213468=CARTESIAN_POINT('Ctrl Pts',(-5.32392444122093,4.1807505237948,121.485262683647));
#213469=CARTESIAN_POINT('Ctrl Pts',(-5.42830024888106,4.04052538761951,
121.493521048358));
#213470=CARTESIAN_POINT('Ctrl Pts',(-5.53555032069353,3.89643878113611,
121.502006829002));
#213471=CARTESIAN_POINT('Ctrl Pts',(-5.63719743999163,3.74789396437864,
121.510492609646));
#213472=CARTESIAN_POINT('Ctrl Pts',(-5.73285536328357,3.59536623776644,
121.51897839029));
#213473=CARTESIAN_POINT('Ctrl Pts',(-5.82570433800763,3.44731741394123,
121.527214990097));
#213474=CARTESIAN_POINT('Ctrl Pts',(-5.91291065018202,3.29551660341996,
121.535451589903));
#213475=CARTESIAN_POINT('Ctrl Pts',(-5.99416188644328,3.14043186187996,
121.54368818971));
#213476=CARTESIAN_POINT('Ctrl Pts',(-6.07534980920209,2.98546796721707,
121.551918371301));
#213477=CARTESIAN_POINT('Ctrl Pts',(-6.15059173290633,2.82722555084991,
121.560148552892));
#213478=CARTESIAN_POINT('Ctrl Pts',(-6.21961939842397,2.66620020605135,
121.568378734483));
#213479=CARTESIAN_POINT('Ctrl Pts',(-6.28860554740525,2.50527170958934,
121.576603966049));
#213480=CARTESIAN_POINT('Ctrl Pts',(-6.35138474309997,2.34156394440105,
121.584829197616));
#213481=CARTESIAN_POINT('Ctrl Pts',(-6.40773536301101,2.17559566960826,
121.593054429182));
#213482=CARTESIAN_POINT('Ctrl Pts',(-6.46406210785872,2.00969771352849,
121.601276175819));
#213483=CARTESIAN_POINT('Ctrl Pts',(-6.51396558948852,1.84154149221128,
121.609497922457));
#213484=CARTESIAN_POINT('Ctrl Pts',(-6.55727285957674,1.67166433384763,
121.617719669094));
#213485=CARTESIAN_POINT('Ctrl Pts',(-6.60057367130336,1.5018125090623,121.625940189632));
#213486=CARTESIAN_POINT('Ctrl Pts',(-6.63728013996174,1.33024060200164,
121.63416071017));
#213487=CARTESIAN_POINT('Ctrl Pts',(-6.66726953062416,1.15749989460504,
121.642381230707));
#213488=CARTESIAN_POINT('Ctrl Pts',(-6.69725658057649,0.984772669840407,
121.650601109623));
#213489=CARTESIAN_POINT('Ctrl Pts',(-6.72052754009912,0.810877177457831,
121.658820988539));
#213490=CARTESIAN_POINT('Ctrl Pts',(-6.73701103441075,0.636373571283254,
121.667040867455));
#213491=CARTESIAN_POINT('Ctrl Pts',(-6.75349872518262,0.461825539003984,
121.675262839033));
#213492=CARTESIAN_POINT('Ctrl Pts',(-6.76319546963717,0.286669438060289,
121.683484810612));
#213493=CARTESIAN_POINT('Ctrl Pts',(-6.76608184523593,0.111469563418846,
121.691706782191));
#213494=CARTESIAN_POINT('Ctrl Pts',(-6.76672228928576,0.0725953028088449,
121.693531116064));
#213495=CARTESIAN_POINT('Ctrl Pts',(-6.76702764152326,0.0337188896224528,
121.695355449937));
#213496=CARTESIAN_POINT('Ctrl Pts',(-6.76699803763021,-0.00515351422502416,
121.69717978381));
#213497=CARTESIAN_POINT('',(-6.76699969784176,0.00142993171423264,121.30282021619));
#213498=CARTESIAN_POINT('Ctrl Pts',(3.09910619832143,6.01563211736935,120.651489390257));
#213499=CARTESIAN_POINT('Ctrl Pts',(2.93676012016632,6.0992688370469,120.660077321312));
#213500=CARTESIAN_POINT('Ctrl Pts',(2.77097677061675,6.17635490515243,120.668665252367));
#213501=CARTESIAN_POINT('Ctrl Pts',(2.6023165691788,6.24661808291315,120.677253183423));
#213502=CARTESIAN_POINT('Ctrl Pts',(2.43690585560943,6.31552753678527,120.685675655303));
#213503=CARTESIAN_POINT('Ctrl Pts',(2.2687284581089,6.37787448913762,120.694098127183));
#213504=CARTESIAN_POINT('Ctrl Pts',(2.09833435009174,6.43345023725412,120.702520599063));
#213505=CARTESIAN_POINT('Ctrl Pts',(1.92794913531729,6.48902308475027,120.710942631356));
#213506=CARTESIAN_POINT('Ctrl Pts',(1.75534775773976,6.53782532931774,120.719364663649));
#213507=CARTESIAN_POINT('Ctrl Pts',(1.58109654221623,6.5796977684535,120.727786695941));
#213508=CARTESIAN_POINT('Ctrl Pts',(1.40683009712605,6.62157386724293,120.73620946432));
#213509=CARTESIAN_POINT('Ctrl Pts',(1.23091385096143,6.65651887566472,120.744632232699));
#213510=CARTESIAN_POINT('Ctrl Pts',(1.05392590273805,6.68442437248996,120.753055001078));
#213511=CARTESIAN_POINT('Ctrl Pts',(0.87085903342554,6.71328832617544,120.761767062287));
#213512=CARTESIAN_POINT('Ctrl Pts',(0.686645910593815,6.73462053310505,
120.770479123495));
#213513=CARTESIAN_POINT('Ctrl Pts',(0.501933752710862,6.74835917152382,
120.779191184704));
#213514=CARTESIAN_POINT('Ctrl Pts',(0.323187364936479,6.76165408409719,
120.787621866739));
#213515=CARTESIAN_POINT('Ctrl Pts',(0.14397401722713,6.76783830706771,120.796052548774));
#213516=CARTESIAN_POINT('Ctrl Pts',(-0.0351181501188691,6.76690887448119,
120.804483230808));
#213517=CARTESIAN_POINT('Ctrl Pts',(-0.22317628353502,6.7659329113224,120.813335981604));
#213518=CARTESIAN_POINT('Ctrl Pts',(-0.411100371938996,6.75711274275371,
120.822188732399));
#213519=CARTESIAN_POINT('Ctrl Pts',(-0.598213628239119,6.74050661708666,
120.831041483194));
#213520=CARTESIAN_POINT('Ctrl Pts',(-0.785326884539114,6.72390049141962,
120.839894233989));
#213521=CARTESIAN_POINT('Ctrl Pts',(-0.971628892828559,6.69950849344904,
120.848746984785));
#213522=CARTESIAN_POINT('Ctrl Pts',(-1.15645336321467,6.66745113358242,
120.85759973558));
#213523=CARTESIAN_POINT('Ctrl Pts',(-1.32639133558461,6.63797580099314,
120.865739450613));
#213524=CARTESIAN_POINT('Ctrl Pts',(-1.49541906581941,6.60196152228329,
120.873879165646));
#213525=CARTESIAN_POINT('Ctrl Pts',(-1.66299074861171,6.55947793425909,
120.882018880678));
#213526=CARTESIAN_POINT('Ctrl Pts',(-1.83041587421548,6.51703150212612,
120.890151476765));
#213527=CARTESIAN_POINT('Ctrl Pts',(-1.99638713462422,6.46812711231021,
120.898284072852));
#213528=CARTESIAN_POINT('Ctrl Pts',(-2.16036679753926,6.41288580126685,
120.906416668939));
#213529=CARTESIAN_POINT('Ctrl Pts',(-2.32423435516029,6.35768225614706,
120.914543705147));
#213530=CARTESIAN_POINT('Ctrl Pts',(-2.48611268046784,6.29615053153927,
120.922670741355));
#213531=CARTESIAN_POINT('Ctrl Pts',(-2.64547718357034,6.22846204702323,
120.930797777563));
#213532=CARTESIAN_POINT('Ctrl Pts',(-2.80476550755562,6.16080591882805,
120.9389209289));
#213533=CARTESIAN_POINT('Ctrl Pts',(-2.96154206587183,6.08699903414881,
120.947044080238));
#213534=CARTESIAN_POINT('Ctrl Pts',(-3.11530032927466,6.00726167720545,
120.955167231575));
#213535=CARTESIAN_POINT('Ctrl Pts',(-3.26901538546231,5.92754672705222,
120.963288100247));
#213536=CARTESIAN_POINT('Ctrl Pts',(-3.41971351166351,5.84190479313356,
120.971408968919));
#213537=CARTESIAN_POINT('Ctrl Pts',(-3.56691099203656,5.75060300967549,
120.97952983759));
#213538=CARTESIAN_POINT('Ctrl Pts',(-3.71411642752588,5.65929629191894,
120.987651145145));
#213539=CARTESIAN_POINT('Ctrl Pts',(-3.85782052591071,5.56232930319305,
120.995772452699));
#213540=CARTESIAN_POINT('Ctrl Pts',(-3.99756672125206,5.46001367298087,
121.003893760254));
#213541=CARTESIAN_POINT('Ctrl Pts',(-4.07018370218445,5.40684691484442,
121.008113873971));
#213542=CARTESIAN_POINT('Ctrl Pts',(-4.14173244557785,5.35223662807531,
121.012333987688));
#213543=CARTESIAN_POINT('Ctrl Pts',(-4.21215220819042,5.29623099713717,
121.016554101404));
#213544=CARTESIAN_POINT('Ctrl Pts',(-4.36207281949341,5.17699744514624,
121.02553853993));
#213545=CARTESIAN_POINT('Ctrl Pts',(-4.50680025120209,5.05149644001659,
121.034522978456));
#213546=CARTESIAN_POINT('Ctrl Pts',(-4.64585411787622,4.92019598343527,
121.043507416982));
#213547=CARTESIAN_POINT('Ctrl Pts',(-4.78514798322573,4.78866891010168,
121.052507362112));
#213548=CARTESIAN_POINT('Ctrl Pts',(-4.91874853773518,4.65132254309186,
121.061507307243));
#213549=CARTESIAN_POINT('Ctrl Pts',(-5.0462130898982,4.50866082682432,121.070507252373));
#213550=CARTESIAN_POINT('Ctrl Pts',(-5.17397801554991,4.3656629245608,121.079528406106));
#213551=CARTESIAN_POINT('Ctrl Pts',(-5.29557784759204,4.21732478995254,
121.088549559838));
#213552=CARTESIAN_POINT('Ctrl Pts',(-5.41060922740221,4.0641846400416,121.09757071357));
#213553=CARTESIAN_POINT('Ctrl Pts',(-5.52575765254882,3.91088866882001,
121.106601046397));
#213554=CARTESIAN_POINT('Ctrl Pts',(-5.63432413497768,3.75278111558691,
121.115631379225));
#213555=CARTESIAN_POINT('Ctrl Pts',(-5.73594848932957,3.5904294907097,121.124661712052));
#213556=CARTESIAN_POINT('Ctrl Pts',(-5.83771691498145,3.42784770240559,
121.133704847044));
#213557=CARTESIAN_POINT('Ctrl Pts',(-5.93252340688742,3.26101001446649,
121.142747982037));
#213558=CARTESIAN_POINT('Ctrl Pts',(-6.02005244936564,3.09051088121152,
121.15179111703));
#213559=CARTESIAN_POINT('Ctrl Pts',(-6.09657299800208,2.94145535804667,
121.15969690043));
#213560=CARTESIAN_POINT('Ctrl Pts',(-6.16753220670303,2.78960193080615,
121.16760268383));
#213561=CARTESIAN_POINT('Ctrl Pts',(-6.23274904006365,2.63536115240125,
121.175508467229));
#213562=CARTESIAN_POINT('Ctrl Pts',(-6.30502491071771,2.46442542959591,
121.184269968654));
#213563=CARTESIAN_POINT('Ctrl Pts',(-6.37030605864747,2.29041717942685,
121.19303147008));
#213564=CARTESIAN_POINT('Ctrl Pts',(-6.42834697419434,2.11391678629187,
121.201792971505));
#213565=CARTESIAN_POINT('Ctrl Pts',(-6.48630562091307,1.93766656978438,
121.210542054131));
#213566=CARTESIAN_POINT('Ctrl Pts',(-6.537044430923,1.75893153360658,121.219291136757));
#213567=CARTESIAN_POINT('Ctrl Pts',(-6.58036679249632,1.57830981629455,
121.228040219383));
#213568=CARTESIAN_POINT('Ctrl Pts',(-6.62365002613026,1.39785123310881,
121.236781400003));
#213569=CARTESIAN_POINT('Ctrl Pts',(-6.65953010532025,1.2155096460269,121.245522580623));
#213570=CARTESIAN_POINT('Ctrl Pts',(-6.68786034475579,1.03189777063573,
121.254263761243));
#213571=CARTESIAN_POINT('Ctrl Pts',(-6.71615447184363,0.848519943950757,
121.262993799544));
#213572=CARTESIAN_POINT('Ctrl Pts',(-6.73691792362148,0.663875343858194,
121.271723837846));
#213573=CARTESIAN_POINT('Ctrl Pts',(-6.75005511578671,0.47858639119979,
121.280453876147));
#213574=CARTESIAN_POINT('Ctrl Pts',(-6.76127426882419,0.320349753577202,
121.287909322828));
#213575=CARTESIAN_POINT('Ctrl Pts',(-6.76693229069058,0.161643476358914,
121.295364769509));
#213576=CARTESIAN_POINT('Ctrl Pts',(-6.76699939568353,0.00285986342245457,
121.30282021619));
#213577=CARTESIAN_POINT('Ctrl Pts',(-6.767,6.39536411522111E-12,121.30282021619));
#213578=CARTESIAN_POINT('Ctrl Pts',(-6.76700000000018,-0.18600724952047,
121.311569728001));
#213579=CARTESIAN_POINT('Ctrl Pts',(-6.75932637294556,-0.372014355743516,
121.320319239812));
#213580=CARTESIAN_POINT('Ctrl Pts',(-6.74400518264233,-0.557389537481099,
121.329068751624));
#213581=CARTESIAN_POINT('Ctrl Pts',(-6.72868405705155,-0.742763936245481,
121.337818226479));
#213582=CARTESIAN_POINT('Ctrl Pts',(-6.70571545645811,-0.927506130236042,
121.346567701335));
#213583=CARTESIAN_POINT('Ctrl Pts',(-6.67517739404903,-1.11098863989547,
121.355317176191));
#213584=CARTESIAN_POINT('Ctrl Pts',(-6.64463945808788,-1.29447038981503,
121.364066614818));
#213585=CARTESIAN_POINT('Ctrl Pts',(-6.60653217008449,-1.47669218313265,
121.372816053445));
#213586=CARTESIAN_POINT('Ctrl Pts',(-6.56098496092776,-1.65703510598893,
121.381565492072));
#213587=CARTESIAN_POINT('Ctrl Pts',(-6.51543793658404,-1.8373772970832,
121.390314895197));
#213588=CARTESIAN_POINT('Ctrl Pts',(-6.46245112167535,-2.01584035510561,
121.399064298322));
#213589=CARTESIAN_POINT('Ctrl Pts',(-6.40220448374374,-2.19181813760439,
121.407813701447));
#213590=CARTESIAN_POINT('Ctrl Pts',(-6.34195808526631,-2.36779522066803,
121.416563069797));
#213591=CARTESIAN_POINT('Ctrl Pts',(-6.27445201433237,-2.54128677683837,
121.425312438147));
#213592=CARTESIAN_POINT('Ctrl Pts',(-6.1999155507204,-2.71170355384495,
121.434061806497));
#213593=CARTESIAN_POINT('Ctrl Pts',(-6.1253793771684,-2.88211966767164,
121.442811140799));
#213594=CARTESIAN_POINT('Ctrl Pts',(-6.04381298052677,-3.04946076371475,
121.451560475101));
#213595=CARTESIAN_POINT('Ctrl Pts',(-5.95549339335997,-3.2131584837424,
121.460309809403));
#213596=CARTESIAN_POINT('Ctrl Pts',(-5.86717414255579,-3.37685558033198,
121.469059110383));
#213597=CARTESIAN_POINT('Ctrl Pts',(-5.77210188876772,-3.53690907646473,
121.477808411363));
#213598=CARTESIAN_POINT('Ctrl Pts',(-5.67059953347172,-3.69277536969016,
121.486557712343));
#213599=CARTESIAN_POINT('Ctrl Pts',(-5.56909755631575,-3.84864108224646,
121.495306980729));
#213600=CARTESIAN_POINT('Ctrl Pts',(-5.46116568197057,-4.00031938297234,
121.504056249114));
#213601=CARTESIAN_POINT('Ctrl Pts',(-5.34717048533825,-4.14729511859567,
121.512805517499));
#213602=CARTESIAN_POINT('Ctrl Pts',(-5.23317570392064,-4.2942703188764,
121.521554754016));
#213603=CARTESIAN_POINT('Ctrl Pts',(-5.11311782003745,-4.43654276189281,
121.530303990533));
#213604=CARTESIAN_POINT('Ctrl Pts',(-4.98740458984987,-4.57362924351597,
121.53905322705));
#213605=CARTESIAN_POINT('Ctrl Pts',(-4.86169180711989,-4.71071523720013,
121.547802432426));
#213606=CARTESIAN_POINT('Ctrl Pts',(-4.73032391204428,-4.84261509522987,
121.556551637801));
#213607=CARTESIAN_POINT('Ctrl Pts',(-4.59374707013867,-4.96888084538082,
121.565300843177));
#213608=CARTESIAN_POINT('Ctrl Pts',(-4.45717070301724,-5.0951461565922,
121.574050018137));
#213609=CARTESIAN_POINT('Ctrl Pts',(-4.3153856357133,-5.21577720459288,
121.582799193098));
#213610=CARTESIAN_POINT('Ctrl Pts',(-4.16887341029809,-5.33036429232652,
121.591548368058));
#213611=CARTESIAN_POINT('Ctrl Pts',(-4.02236168204004,-5.44495099123396,
121.60029751333));
#213612=CARTESIAN_POINT('Ctrl Pts',(-3.8711230534846,-5.55349359438396,
121.609046658602));
#213613=CARTESIAN_POINT('Ctrl Pts',(-3.71567117018052,-5.65562346298703,
121.617795803874));
#213614=CARTESIAN_POINT('Ctrl Pts',(-3.56021980146092,-5.75775299351476,
121.626544920184));
#213615=CARTESIAN_POINT('Ctrl Pts',(-3.40055544538604,-5.85346967463726,
121.635294036494));
#213616=CARTESIAN_POINT('Ctrl Pts',(-3.23722035987088,-5.94244842986773,
121.644043152805));
#213617=CARTESIAN_POINT('Ctrl Pts',(-3.07388580147412,-6.03142689794411,
121.652792240879));
#213618=CARTESIAN_POINT('Ctrl Pts',(-2.90688078896807,-6.11366734656673,
121.661541328954));
#213619=CARTESIAN_POINT('Ctrl Pts',(-2.73677250721596,-6.18889046952254,
121.670290417029));
#213620=CARTESIAN_POINT('Ctrl Pts',(-2.56666476031712,-6.26411335596233,
121.679039477595));
#213621=CARTESIAN_POINT('Ctrl Pts',(-2.393454025754,-6.33231884500468,121.687788538161));
#213622=CARTESIAN_POINT('Ctrl Pts',(-2.21772856065829,-6.39327529762645,
121.696537598727));
#213623=CARTESIAN_POINT('Ctrl Pts',(-2.04200363348737,-6.45423156365041,
121.705286632511));
#213624=CARTESIAN_POINT('Ctrl Pts',(-1.86376426189486,-6.50793874375599,
121.714035666295));
#213625=CARTESIAN_POINT('Ctrl Pts',(-1.68361577753346,-6.55421443909493,
121.722784700078));
#213626=CARTESIAN_POINT('Ctrl Pts',(-1.50346782967993,-6.60048999661824,
121.731533707806));
#213627=CARTESIAN_POINT('Ctrl Pts',(-1.32141105795182,-6.63933404237674,
121.740282715534));
#213628=CARTESIAN_POINT('Ctrl Pts',(-1.13806375487219,-6.67061465607527,
121.749031723262));
#213629=CARTESIAN_POINT('Ctrl Pts',(-0.954716982604867,-6.7018951792127,
121.75778070566));
#213630=CARTESIAN_POINT('Ctrl Pts',(-0.770079968903871,-6.72561226592209,
121.766529688059));
#213631=CARTESIAN_POINT('Ctrl Pts',(-0.584779765559858,-6.74168536983088,
121.775278670457));
#213632=CARTESIAN_POINT('Ctrl Pts',(-0.39148983065291,-6.75845151013844,
121.784404889467));
#213633=CARTESIAN_POINT('Ctrl Pts',(-0.197478578239945,-6.76689983031621,
121.793531108477));
#213634=CARTESIAN_POINT('Ctrl Pts',(-0.0034628764529491,-6.76699911397118,
121.802657327487));
#213635=CARTESIAN_POINT('Ctrl Pts',(0.184489834653171,-6.76709529501193,
121.811498352152));
#213636=CARTESIAN_POINT('Ctrl Pts',(0.372446404248647,-6.75935639738172,
121.820339376818));
#213637=CARTESIAN_POINT('Ctrl Pts',(0.559755019487608,-6.74380925873193,
121.829180401484));
#213638=CARTESIAN_POINT('Ctrl Pts',(0.745134705521033,-6.72842222659814,
121.837930380094));
#213639=CARTESIAN_POINT('Ctrl Pts',(0.929879431227813,-6.70538706057534,
121.846680358704));
#213640=CARTESIAN_POINT('Ctrl Pts',(1.11336163626749,-6.6747820089414,121.855430337313));
#213641=CARTESIAN_POINT('Ctrl Pts',(1.29684196300662,-6.64417727061024,
121.86418022635));
#213642=CARTESIAN_POINT('Ctrl Pts',(1.47905951217473,-6.60600284890599,
121.872930115386));
#213643=CARTESIAN_POINT('Ctrl Pts',(1.65939532067066,-6.56038841607235,
121.881680004423));
#213644=CARTESIAN_POINT('Ctrl Pts',(1.83972934300786,-6.51477443503261,
121.890429806795));
#213645=CARTESIAN_POINT('Ctrl Pts',(2.01818138406251,-6.46172066062145,
121.899179609167));
#213646=CARTESIAN_POINT('Ctrl Pts',(2.19414528354189,-6.40140730423482,
121.907929411539));
#213647=CARTESIAN_POINT('Ctrl Pts',(2.37010749863978,-6.3410945251865,121.916679130156));
#213648=CARTESIAN_POINT('Ctrl Pts',(2.54358134866429,-6.27352239616516,
121.925428848772));
#213649=CARTESIAN_POINT('Ctrl Pts',(2.71397759435515,-6.19892043966837,
121.934178567388));
#213650=CARTESIAN_POINT('Ctrl Pts',(2.88437226558081,-6.12431917249535,
121.942928205157));
#213651=CARTESIAN_POINT('Ctrl Pts',(3.05168912680909,-6.04268832278822,
121.951677842926));
#213652=CARTESIAN_POINT('Ctrl Pts',(3.21535986273805,-5.9543051612336,121.960427480694));
#213653=CARTESIAN_POINT('Ctrl Pts',(3.37902914072801,-5.86592278697464,
121.969177040524));
#213654=CARTESIAN_POINT('Ctrl Pts',(3.5390521062154,-5.77078835741962,121.977926600353));
#213655=CARTESIAN_POINT('Ctrl Pts',(3.69488522831672,-5.66922500431645,
121.986676160182));
#213656=CARTESIAN_POINT('Ctrl Pts',(3.85071701406922,-5.56766252217106,
121.995425644979));
#213657=CARTESIAN_POINT('Ctrl Pts',(4.00235878822393,-5.45967138329378,
122.004175129776));
#213658=CARTESIAN_POINT('Ctrl Pts',(4.14929549611321,-5.3456183819961,122.012924614573));
#213659=CARTESIAN_POINT('Ctrl Pts',(4.29623099276083,-5.23156632087021,
122.021674027246));
#213660=CARTESIAN_POINT('Ctrl Pts',(4.43846127436019,-5.11145267304972,
122.030423439918));
#213661=CARTESIAN_POINT('Ctrl Pts',(4.57550326054431,-4.98568540049895,
122.039172852591));
#213662=CARTESIAN_POINT('Ctrl Pts',(4.7125441625776,-4.8599191229038,122.047922196046));
#213663=CARTESIAN_POINT('Ctrl Pts',(4.84439664018731,-4.7284995038545,122.056671539501));
#213664=CARTESIAN_POINT('Ctrl Pts',(4.97061286794706,-4.5918728986111,122.065420882957));
#213665=CARTESIAN_POINT('Ctrl Pts',(5.09682813912642,-4.45524732884733,
122.074170160101));
#213666=CARTESIAN_POINT('Ctrl Pts',(5.21740705147794,-4.31341506235842,
122.082919437246));
#213667=CARTESIAN_POINT('Ctrl Pts',(5.33194007545648,-4.16685781275785,
122.091668714391));
#213668=CARTESIAN_POINT('Ctrl Pts',(5.44647226944436,-4.02030162521908,
122.100417928132));
#213669=CARTESIAN_POINT('Ctrl Pts',(5.55495848628062,-3.86902074888007,
122.109167141873));
#213670=CARTESIAN_POINT('Ctrl Pts',(5.65703027291736,-3.71352898080742,
122.117916355614));
#213671=CARTESIAN_POINT('Ctrl Pts',(5.7591013537694,-3.5580382878968,122.126665508858));
#213672=CARTESIAN_POINT('Ctrl Pts',(5.85475793592692,-3.39833700106816,
122.135414662102));
#213673=CARTESIAN_POINT('Ctrl Pts',(5.94367514427335,-3.2349675082367,122.144163815346));
#213674=CARTESIAN_POINT('Ctrl Pts',(6.0325917673258,-3.07159909077844,122.152912910999));
#213675=CARTESIAN_POINT('Ctrl Pts',(6.11476896835867,-2.90456276731555,
122.161662006652));
#213676=CARTESIAN_POINT('Ctrl Pts',(6.18992765547832,-2.73442583003173,
122.170411102305));
#213677=CARTESIAN_POINT('Ctrl Pts',(6.26508587283002,-2.56428995616297,
122.179160143273));
#213678=CARTESIAN_POINT('Ctrl Pts',(6.33322554827111,-2.39105376935333,
122.187909184241));
#213679=CARTESIAN_POINT('Ctrl Pts',(6.39411526732984,-2.21530561054214,
122.196658225209));
#213680=CARTESIAN_POINT('Ctrl Pts',(6.45500462602798,-2.03955849185252,
122.205407214398));
#213681=CARTESIAN_POINT('Ctrl Pts',(6.5086440204069,-1.86129970164718,122.214156203587));
#213682=CARTESIAN_POINT('Ctrl Pts',(6.55485128368551,-1.68113463136251,
122.222905192776));
#213683=CARTESIAN_POINT('Ctrl Pts',(6.60199809554281,-1.49730620117069,
122.231832078247));
#213684=CARTESIAN_POINT('Ctrl Pts',(6.64140720707832,-1.31149343245906,
122.240758963719));
#213685=CARTESIAN_POINT('Ctrl Pts',(6.67293928722847,-1.1243532669774,122.24968584919));
#213686=CARTESIAN_POINT('Ctrl Pts',(6.70384625876226,-0.940923067008742,
122.258435763368));
#213687=CARTESIAN_POINT('Ctrl Pts',(6.72718554579772,-0.756217899523822,
122.267185677545));
#213688=CARTESIAN_POINT('Ctrl Pts',(6.7428778681531,-0.570865181256655,
122.275935591723));
#213689=CARTESIAN_POINT('Ctrl Pts',(6.75856988190833,-0.385516108076151,
122.284685333827));
#213690=CARTESIAN_POINT('Ctrl Pts',(6.76661520773396,-0.199519795228596,
122.293435075932));
#213691=CARTESIAN_POINT('Ctrl Pts',(6.76698651789579,-0.0135080204579373,
122.302184818036));
#213692=CARTESIAN_POINT('Ctrl Pts',(6.76735782124909,0.17250034351063,122.310934399701));
#213693=CARTESIAN_POINT('Ctrl Pts',(6.76005538995196,0.358523882208551,
122.319683981366));
#213694=CARTESIAN_POINT('Ctrl Pts',(6.7451040274238,0.54393074856197,122.328433563031));
#213695=CARTESIAN_POINT('Ctrl Pts',(6.73015291918057,0.729334461612732,
122.337182995888));
#213696=CARTESIAN_POINT('Ctrl Pts',(6.7075531630663,0.914121237632085,122.345932428744));
#213697=CARTESIAN_POINT('Ctrl Pts',(6.67738151874618,1.09766345165853,122.354681861601));
#213698=CARTESIAN_POINT('Ctrl Pts',(6.64721034747622,1.28120278799387,122.363431157279));
#213699=CARTESIAN_POINT('Ctrl Pts',(6.60946757205205,1.46349731860044,122.372180452956));
#213700=CARTESIAN_POINT('Ctrl Pts',(6.56428138111596,1.64392790277869,122.380929748634));
#213701=CARTESIAN_POINT('Ctrl Pts',(6.51909583859932,1.82435589778764,122.389678918759));
#213702=CARTESIAN_POINT('Ctrl Pts',(6.46646716392965,2.00291972191975,122.398428088885));
#213703=CARTESIAN_POINT('Ctrl Pts',(6.40657409872982,2.17901292274375,122.40717725901));
#213704=CARTESIAN_POINT('Ctrl Pts',(6.34668181342186,2.35510383058679,122.415926315209));
#213705=CARTESIAN_POINT('Ctrl Pts',(6.27952541914173,2.52872390822274,122.424675371409));
#213706=CARTESIAN_POINT('Ctrl Pts',(6.20533299175653,2.69928350889972,122.433424427608));
#213707=CARTESIAN_POINT('Ctrl Pts',(6.12831602991689,2.87633637965326,122.442506563766));
#213708=CARTESIAN_POINT('Ctrl Pts',(6.04371690605412,3.05009086601181,122.451588699924));
#213709=CARTESIAN_POINT('Ctrl Pts',(5.95184520316775,3.21991112882469,122.460670836082));
#213710=CARTESIAN_POINT('Ctrl Pts',(5.86333549509423,3.38351691182761,122.469420616426));
#213711=CARTESIAN_POINT('Ctrl Pts',(5.7680761809952,3.54347103711757,122.478170396769));
#213712=CARTESIAN_POINT('Ctrl Pts',(5.66639083309171,3.69923018027458,122.486920177113));
#213713=CARTESIAN_POINT('Ctrl Pts',(5.56470914082364,3.85498372381813,122.495669642898));
#213714=CARTESIAN_POINT('Ctrl Pts',(5.4566020337224,4.00654234701763,122.504419108683));
#213715=CARTESIAN_POINT('Ctrl Pts',(5.34243669839398,4.15339127986435,122.513168574468));
#213716=CARTESIAN_POINT('Ctrl Pts',(5.2282748605078,4.30023571401051,122.521917772214));
#213717=CARTESIAN_POINT('Ctrl Pts',(5.10805534167306,4.44237052028245,122.53066696996));
#213718=CARTESIAN_POINT('Ctrl Pts',(4.98218644340153,4.57931296628501,122.539416167706));
#213719=CARTESIAN_POINT('Ctrl Pts',(4.85632073219798,4.71625194483142,122.548165143917));
#213720=CARTESIAN_POINT('Ctrl Pts',(4.72480612170541,4.84799861524291,122.556914120129));
#213721=CARTESIAN_POINT('Ctrl Pts',(4.58808925235544,4.9741055489827,122.565663096341));
#213722=CARTESIAN_POINT('Ctrl Pts',(4.45136349474297,5.10022068120989,122.574412641342));
#213723=CARTESIAN_POINT('Ctrl Pts',(4.30943501210346,5.22069514871614,122.583162186344));
#213724=CARTESIAN_POINT('Ctrl Pts',(4.16278587432065,5.33511975166036,122.591911731346));
#213725=CARTESIAN_POINT('Ctrl Pts',(4.0161453574073,5.44953762807635,122.600660761999));
#213726=CARTESIAN_POINT('Ctrl Pts',(3.86478496658203,5.5579061753259,122.609409792653));
#213727=CARTESIAN_POINT('Ctrl Pts',(3.70921874747473,5.65985735539175,122.618158823307));
#213728=CARTESIAN_POINT('Ctrl Pts',(3.55365041606185,5.76180991976871,122.626907972757));
#213729=CARTESIAN_POINT('Ctrl Pts',(3.39387638174814,5.85734478552645,122.635657122206));
#213730=CARTESIAN_POINT('Ctrl Pts',(3.23043927904836,5.9461374912107,122.644406271656));
#213731=CARTESIAN_POINT('Ctrl Pts',(3.18691767070633,5.9697820694404,122.646736079572));
#213732=CARTESIAN_POINT('Ctrl Pts',(3.14313645919737,5.9929488063337,122.649065887488));
#213733=CARTESIAN_POINT('Ctrl Pts',(3.09910619832147,6.01563211736933,122.651395695404));
#213734=CARTESIAN_POINT('Origin',(0.,0.,4.30282021618968));
#213735=CARTESIAN_POINT('',(3.09910619832122,6.01563211736946,125.045920265688));
#213736=CARTESIAN_POINT('',(3.09910619832142,6.01563211736936,124.651395695404));
#213737=CARTESIAN_POINT('',(3.09910619832133,6.0156321173694,4.30282021618968));
#213738=CARTESIAN_POINT('',(-6.7669996714996,-0.00210853606402713,123.69717978384));
#213739=CARTESIAN_POINT('Ctrl Pts',(-6.7669996714996,-0.00210853606383412,
123.69717978384));
#213740=CARTESIAN_POINT('Ctrl Pts',(-6.76694565606682,-0.175462182760706,
123.705392103411));
#213741=CARTESIAN_POINT('Ctrl Pts',(-6.76022593160184,-0.349074621583547,
123.713604422982));
#213742=CARTESIAN_POINT('Ctrl Pts',(-6.74680638395335,-0.522391249396756,
123.721816742553));
#213743=CARTESIAN_POINT('Ctrl Pts',(-6.73340288079994,-0.695500658766133,
123.730019243423));
#213744=CARTESIAN_POINT('Ctrl Pts',(-6.7133155311019,-0.868314605660701,
123.738221744294));
#213745=CARTESIAN_POINT('Ctrl Pts',(-6.68656216370095,-1.04027661271554,
123.746424245164));
#213746=CARTESIAN_POINT('Ctrl Pts',(-6.65983534449266,-1.2120679765603,
123.75461860644));
#213747=CARTESIAN_POINT('Ctrl Pts',(-6.6264557350455,-1.38300873047955,
123.762812967715));
#213748=CARTESIAN_POINT('Ctrl Pts',(-6.58649308931571,-1.5525455820672,
123.771007328991));
#213749=CARTESIAN_POINT('Ctrl Pts',(-6.54656197943612,-1.72194864649799,
123.779195223824));
#213750=CARTESIAN_POINT('Ctrl Pts',(-6.50005826186666,-1.88994966590426,
123.787383118657));
#213751=CARTESIAN_POINT('Ctrl Pts',(-6.44710309644667,-2.05600356609314,
123.79557101349));
#213752=CARTESIAN_POINT('Ctrl Pts',(-6.39417896219739,-2.22196016044074,
123.803754110303));
#213753=CARTESIAN_POINT('Ctrl Pts',(-6.3348110199199,-2.38597156598849,
123.811937207115));
#213754=CARTESIAN_POINT('Ctrl Pts',(-6.269170819976,-2.54750588418583,123.820120303928));
#213755=CARTESIAN_POINT('Ctrl Pts',(-6.2035492622953,-2.70899432553823,
123.828301076686));
#213756=CARTESIAN_POINT('Ctrl Pts',(-6.13165912670626,-2.86800674577733,
123.836481849443));
#213757=CARTESIAN_POINT('Ctrl Pts',(-6.05372092055435,-3.02402910304161,
123.844662622201));
#213758=CARTESIAN_POINT('Ctrl Pts',(-5.97579265206773,-3.1800315663663,
123.852842351853));
#213759=CARTESIAN_POINT('Ctrl Pts',(-5.89181800912137,-3.33304440324049,
123.861022081505));
#213760=CARTESIAN_POINT('Ctrl Pts',(-5.80206447742371,-3.48257617286656,
123.869201811157));
#213761=CARTESIAN_POINT('Ctrl Pts',(-5.71230587318667,-3.63211639347809,
123.877382003097));
#213762=CARTESIAN_POINT('Ctrl Pts',(-5.61676791513734,-3.7781748458478,
123.885562195037));
#213763=CARTESIAN_POINT('Ctrl Pts',(-5.51576264018297,-3.92028717024172,
123.893742386977));
#213764=CARTESIAN_POINT('Ctrl Pts',(-5.41473306938529,-4.06243367838265,
123.901924546583));
#213765=CARTESIAN_POINT('Ctrl Pts',(-5.30823377140609,-4.20063187445824,
123.91010670619));
#213766=CARTESIAN_POINT('Ctrl Pts',(-5.19661846995674,-4.33444869362927,
123.918288865796));
#213767=CARTESIAN_POINT('Ctrl Pts',(-5.08489707745208,-4.46839270653969,
123.926478802597));
#213768=CARTESIAN_POINT('Ctrl Pts',(-4.96805019817738,-4.59794674588749,
123.934668739398));
#213769=CARTESIAN_POINT('Ctrl Pts',(-4.84647059857533,-4.72271232843426,
123.942858676199));
#213770=CARTESIAN_POINT('Ctrl Pts',(-4.72483049168749,-4.84754000385503,
123.951052688938));
#213771=CARTESIAN_POINT('Ctrl Pts',(-4.59845323018682,-4.96757422375864,
123.959246701677));
#213772=CARTESIAN_POINT('Ctrl Pts',(-4.46776627529135,-5.08245546063803,
123.967440714415));
#213773=CARTESIAN_POINT('Ctrl Pts',(-4.33690206909243,-5.19749251145458,
123.97564584073));
#213774=CARTESIAN_POINT('Ctrl Pts',(-4.20171676916172,-5.30736238659324,
123.983850967045));
#213775=CARTESIAN_POINT('Ctrl Pts',(-4.06266945072584,-5.41174703160994,
123.99205609336));
#213776=CARTESIAN_POINT('Ctrl Pts',(-3.94992104562226,-5.49638873757973,
123.99870933138));
#213777=CARTESIAN_POINT('Ctrl Pts',(-3.83463399959578,-5.57742468112581,
124.005362569401));
#213778=CARTESIAN_POINT('Ctrl Pts',(-3.71706534913166,-5.65470725946841,
124.012015807422));
#213779=CARTESIAN_POINT('Ctrl Pts',(-3.55915925756001,-5.75850525191355,
124.020951750872));
#213780=CARTESIAN_POINT('Ctrl Pts',(-3.39680241327116,-5.85575152298949,
124.029887694323));
#213781=CARTESIAN_POINT('Ctrl Pts',(-3.23053858472132,-5.94608353898823,
124.038823637774));
#213782=CARTESIAN_POINT('Ctrl Pts',(-3.06452469480442,-6.03627976200791,
124.047746148131));
#213783=CARTESIAN_POINT('Ctrl Pts',(-2.89461576610477,-6.11958234648515,
124.056668658489));
#213784=CARTESIAN_POINT('Ctrl Pts',(-2.72138262653257,-6.19567313534266,
124.065591168846));
#213785=CARTESIAN_POINT('Ctrl Pts',(-2.54857396191163,-6.27157747815426,
124.074491816285));
#213786=CARTESIAN_POINT('Ctrl Pts',(-2.3724575790633,-6.34030519014817,
124.083392463723));
#213787=CARTESIAN_POINT('Ctrl Pts',(-2.19362628326869,-6.40158517317022,
124.092293111161));
#213788=CARTESIAN_POINT('Ctrl Pts',(-2.01507134917033,-6.4627704555417,
124.101180003748));
#213789=CARTESIAN_POINT('Ctrl Pts',(-1.83381011421601,-6.51653088418503,
124.110066896334));
#213790=CARTESIAN_POINT('Ctrl Pts',(-1.65045539686298,-6.56264321618705,
124.11895378892));
#213791=CARTESIAN_POINT('Ctrl Pts',(-1.46757196957798,-6.60863702228256,
124.127817838875));
#213792=CARTESIAN_POINT('Ctrl Pts',(-1.28260604702592,-6.64702189605218,
124.13668188883));
#213793=CARTESIAN_POINT('Ctrl Pts',(-1.09618489742445,-6.67762440323343,
124.145545938785));
#213794=CARTESIAN_POINT('Ctrl Pts',(-0.917951281858252,-6.70688286190061,
124.154020683605));
#213795=CARTESIAN_POINT('Ctrl Pts',(-0.738387766226628,-6.72902777179274,
124.162495428426));
#213796=CARTESIAN_POINT('Ctrl Pts',(-0.558055928185681,-6.74395007254775,
124.170970173246));
#213797=CARTESIAN_POINT('Ctrl Pts',(-0.383380624247193,-6.75840430008827,
124.179179087675));
#213798=CARTESIAN_POINT('Ctrl Pts',(-0.208152740196801,-6.76606701879992,
124.187388002104));
#213799=CARTESIAN_POINT('Ctrl Pts',(-0.0329364771647726,-6.76691984498649,
124.195596916533));
#213800=CARTESIAN_POINT('Ctrl Pts',(0.142321442643743,-6.76777287392816,
124.20380778259));
#213801=CARTESIAN_POINT('Ctrl Pts',(0.31756737984478,-6.76181278307413,
124.212018648647));
#213802=CARTESIAN_POINT('Ctrl Pts',(0.492238098970516,-6.74907331816168,
124.220229514704));
#213803=CARTESIAN_POINT('Ctrl Pts',(0.666981480960584,-6.73632855364312,
124.228443796474));
#213804=CARTESIAN_POINT('Ctrl Pts',(0.841148813312677,-6.71679882248702,
124.236658078243));
#213805=CARTESIAN_POINT('Ctrl Pts',(1.01418285052883,-6.69056964284008,
124.244872360013));
#213806=CARTESIAN_POINT('Ctrl Pts',(1.1874116512138,-6.66431094018083,124.253095887606));
#213807=CARTESIAN_POINT('Ctrl Pts',(1.35950425674739,-6.6313377810379,124.261319415198));
#213808=CARTESIAN_POINT('Ctrl Pts',(1.52991350791545,-6.59178683349954,
124.269542942791));
#213809=CARTESIAN_POINT('Ctrl Pts',(1.70043198478499,-6.55221053534225,
124.277771741344));
#213810=CARTESIAN_POINT('Ctrl Pts',(1.86926461385819,-6.50604813791689,
124.286000539898));
#213811=CARTESIAN_POINT('Ctrl Pts',(2.03588028622283,-6.45348591539249,
124.294229338452));
#213812=CARTESIAN_POINT('Ctrl Pts',(2.20272529172712,-6.40085134517506,
124.302469463288));
#213813=CARTESIAN_POINT('Ctrl Pts',(2.36734691131735,-6.34179947487035,
124.310709588125));
#213814=CARTESIAN_POINT('Ctrl Pts',(2.52923392568352,-6.27656472516388,
124.318949712961));
#213815=CARTESIAN_POINT('Ctrl Pts',(2.60110507922975,-6.24760318843371,
124.322607988331));
#213816=CARTESIAN_POINT('Ctrl Pts',(2.67243756405475,-6.21742362024085,
124.326266263701));
#213817=CARTESIAN_POINT('Ctrl Pts',(2.74318828705647,-6.18604938727102,
124.329924539071));
#213818=CARTESIAN_POINT('Ctrl Pts',(2.90657230218699,-6.11359715022285,
124.338372561833));
#213819=CARTESIAN_POINT('Ctrl Pts',(3.06722604579447,-6.03460517790217,
124.346820584596));
#213820=CARTESIAN_POINT('Ctrl Pts',(3.22460929711039,-5.94930112542551,
124.355268607358));
#213821=CARTESIAN_POINT('Ctrl Pts',(3.38184842788281,-5.86407518841731,
124.363708894014));
#213822=CARTESIAN_POINT('Ctrl Pts',(3.53582274425704,-5.77254885098513,
124.37214918067));
#213823=CARTESIAN_POINT('Ctrl Pts',(3.68601381028946,-5.67499702117591,
124.380589467326));
#213824=CARTESIAN_POINT('Ctrl Pts',(3.83609046294761,-5.57751950493479,
124.389023324294));
#213825=CARTESIAN_POINT('Ctrl Pts',(3.98238933188045,-5.47402582778856,
124.397457181262));
#213826=CARTESIAN_POINT('Ctrl Pts',(4.12441797775684,-5.36483600352855,
124.405891038229));
#213827=CARTESIAN_POINT('Ctrl Pts',(4.26636026284292,-5.25571257235044,
124.414319766974));
#213828=CARTESIAN_POINT('Ctrl Pts',(4.40403723788053,-5.14090010222615,
124.422748495719));
#213829=CARTESIAN_POINT('Ctrl Pts',(4.53698645638378,-5.02076118677141,
124.431177224464));
#213830=CARTESIAN_POINT('Ctrl Pts',(4.66987525092612,-4.90067687313539,
124.439602122445));
#213831=CARTESIAN_POINT('Ctrl Pts',(4.79804032645077,-4.77527116451287,
124.448027020425));
#213832=CARTESIAN_POINT('Ctrl Pts',(4.9210529760274,-4.64494635137285,124.456451918405));
#213833=CARTESIAN_POINT('Ctrl Pts',(5.04403839040315,-4.51465039235862,
124.4648749511));
#213834=CARTESIAN_POINT('Ctrl Pts',(5.16187342264695,-4.37943774076962,
124.473297983794));
#213835=CARTESIAN_POINT('Ctrl Pts',(5.27416647872013,-4.23974727486733,
124.481721016488));
#213836=CARTESIAN_POINT('Ctrl Pts',(5.38644682896153,-4.10007261478262,
124.490143096125));
#213837=CARTESIAN_POINT('Ctrl Pts',(5.49318624423301,-3.95592141028999,
124.498565175763));
#213838=CARTESIAN_POINT('Ctrl Pts',(5.59403346747403,-3.80776556063796,
124.506987255401));
#213839=CARTESIAN_POINT('Ctrl Pts',(5.69488335748529,-3.65960579320218,
124.515409557749));
#213840=CARTESIAN_POINT('Ctrl Pts',(5.78984055749235,-3.50744144535963,
124.523831860097));
#213841=CARTESIAN_POINT('Ctrl Pts',(5.87859698863607,-3.35177362678314,
124.532254162445));
#213842=CARTESIAN_POINT('Ctrl Pts',(5.96736815728036,-3.19607996045076,
124.540677863269));
#213843=CARTESIAN_POINT('Ctrl Pts',(6.04993633971336,-3.03688195353878,
124.549101564093));
#213844=CARTESIAN_POINT('Ctrl Pts',(6.12603910961953,-2.87470586798232,
124.557525264916));
#213845=CARTESIAN_POINT('Ctrl Pts',(6.20219337896567,-2.71242003638648,
124.565954666135));
#213846=CARTESIAN_POINT('Ctrl Pts',(6.27187335126468,-2.54715240129741,
124.574384067354));
#213847=CARTESIAN_POINT('Ctrl Pts',(6.33486410868279,-2.37945071907839,
124.582813468573));
#213848=CARTESIAN_POINT('Ctrl Pts',(6.39787734111564,-2.21168920113211,
124.591245877391));
#213849=CARTESIAN_POINT('Ctrl Pts',(6.45419648821382,-2.04149221869552,
124.599678286209));
#213850=CARTESIAN_POINT('Ctrl Pts',(6.5036561652542,-1.86942383748336,124.608110695026));
#213851=CARTESIAN_POINT('Ctrl Pts',(6.55316160382688,-1.69719625359834,
124.616550905754));
#213852=CARTESIAN_POINT('Ctrl Pts',(6.59579480567521,-1.5230941337976,124.624991116481));
#213853=CARTESIAN_POINT('Ctrl Pts',(6.63144101104968,-1.34769399975232,
124.633431327209));
#213854=CARTESIAN_POINT('Ctrl Pts',(6.65171596439557,-1.24792939655625,
124.638231975046));
#213855=CARTESIAN_POINT('Ctrl Pts',(6.66973146463446,-1.14774503930318,
124.643032622883));
#213856=CARTESIAN_POINT('Ctrl Pts',(6.68547385807063,-1.04724796158993,
124.64783327072));
#213857=CARTESIAN_POINT('Ctrl Pts',(6.71216579650349,-0.876850631483663,
124.655972985753));
#213858=CARTESIAN_POINT('Ctrl Pts',(6.73237306386141,-0.705214189533114,
124.664112700786));
#213859=CARTESIAN_POINT('Ctrl Pts',(6.74598622680419,-0.532877873220674,
124.672252415819));
#213860=CARTESIAN_POINT('Ctrl Pts',(6.75958748375635,-0.360692281216413,
124.680385011906));
#213861=CARTESIAN_POINT('Ctrl Pts',(6.76660608715752,-0.187808395814929,
124.688517607993));
#213862=CARTESIAN_POINT('Ctrl Pts',(6.7669838716605,-0.0147743252546067,
124.69665020408));
#213863=CARTESIAN_POINT('Ctrl Pts',(6.76736139788972,0.15814144993203,124.704777240288));
#213864=CARTESIAN_POINT('Ctrl Pts',(6.76110714337227,0.331206841151615,
124.712904276496));
#213865=CARTESIAN_POINT('Ctrl Pts',(6.74821487702592,0.503869996612238,
124.721031312704));
#213866=CARTESIAN_POINT('Ctrl Pts',(6.73532877341621,0.676450615959723,
124.729154464041));
#213867=CARTESIAN_POINT('Ctrl Pts',(6.71581100385033,0.848629018016744,
124.737277615379));
#213868=CARTESIAN_POINT('Ctrl Pts',(6.68970741387236,1.01985475278647,124.745400766717));
#213869=CARTESIAN_POINT('Ctrl Pts',(6.66361115919718,1.1910323718522,124.753521635388));
#213870=CARTESIAN_POINT('Ctrl Pts',(6.63093282619393,1.36125749525762,124.76164250406));
#213871=CARTESIAN_POINT('Ctrl Pts',(6.59176995638125,1.52998622286268,124.769763372732));
#213872=CARTESIAN_POINT('Ctrl Pts',(6.55260497005717,1.69872406921404,124.777884680286));
#213873=CARTESIAN_POINT('Ctrl Pts',(6.50695482572185,1.86596500055958,124.786005987841));
#213874=CARTESIAN_POINT('Ctrl Pts',(6.45496792438712,2.03117652978107,124.794127295395));
#213875=CARTESIAN_POINT('Ctrl Pts',(6.42795372329491,2.11702618341604,124.798347409112));
#213876=CARTESIAN_POINT('Ctrl Pts',(6.39922929765506,2.20232807948675,124.802567522828));
#213877=CARTESIAN_POINT('Ctrl Pts',(6.36882075883247,2.28700921333182,124.806787636545));
#213878=CARTESIAN_POINT('Ctrl Pts',(6.30408230246524,2.46729166361793,124.815772075071));
#213879=CARTESIAN_POINT('Ctrl Pts',(6.23174008365757,2.64467017177402,124.824756513597));
#213880=CARTESIAN_POINT('Ctrl Pts',(6.15208292973967,2.81853944900649,124.833740952122));
#213881=CARTESIAN_POINT('Ctrl Pts',(6.07228829232828,2.99270881423443,124.842740897253));
#213882=CARTESIAN_POINT('Ctrl Pts',(5.98515358509819,3.16335662550598,124.851740842383));
#213883=CARTESIAN_POINT('Ctrl Pts',(5.89101378387091,3.32990174002822,124.860740787514));
#213884=CARTESIAN_POINT('Ctrl Pts',(5.79665213978569,3.49683932238764,124.869761941246));
#213885=CARTESIAN_POINT('Ctrl Pts',(5.6952524905742,3.65965465480885,124.878783094978));
#213886=CARTESIAN_POINT('Ctrl Pts',(5.58719490563032,3.81779282917482,124.88780424871));
#213887=CARTESIAN_POINT('Ctrl Pts',(5.47902737124187,3.97609191037989,124.896834581538));
#213888=CARTESIAN_POINT('Ctrl Pts',(5.36418850698005,4.12970413239017,124.905864914365));
#213889=CARTESIAN_POINT('Ctrl Pts',(5.24309999454458,4.27810605843365,124.914895247192));
#213890=CARTESIAN_POINT('Ctrl Pts',(5.12183981676803,4.42671837162896,124.923938382185));
#213891=CARTESIAN_POINT('Ctrl Pts',(4.99431242612214,4.5701054340135,124.932981517177));
#213892=CARTESIAN_POINT('Ctrl Pts',(4.86097937264908,4.70777745211902,124.94202465217));
#213893=CARTESIAN_POINT('Ctrl Pts',(4.74441556577524,4.82813451372058,124.94993043557));
#213894=CARTESIAN_POINT('Ctrl Pts',(4.62341526258758,4.94412416538557,124.95783621897));
#213895=CARTESIAN_POINT('Ctrl Pts',(4.49830907481142,5.05544305352847,124.96574200237));
#213896=CARTESIAN_POINT('Ctrl Pts',(4.3613729953246,5.17728812279391,124.974395347207));
#213897=CARTESIAN_POINT('Ctrl Pts',(4.2193959874644,5.29364401377653,124.983048692044));
#213898=CARTESIAN_POINT('Ctrl Pts',(4.07283576707601,5.40410009293188,124.991702036881));
#213899=CARTESIAN_POINT('Ctrl Pts',(3.91978829019922,5.51944533583362,125.000738408349));
#213900=CARTESIAN_POINT('Ctrl Pts',(3.76174285278105,5.62835634690295,125.009774779816));
#213901=CARTESIAN_POINT('Ctrl Pts',(3.59926106435887,5.73041087450021,125.018811151284));
#213902=CARTESIAN_POINT('Ctrl Pts',(3.43677927593659,5.83246540209754,125.027847522752));
#213903=CARTESIAN_POINT('Ctrl Pts',(3.26986143267321,5.92766320656322,125.03688389422));
#213904=CARTESIAN_POINT('Ctrl Pts',(3.09910619832122,6.01563211736946,125.045920265688));
#213905=CARTESIAN_POINT('Ctrl Pts',(3.09910619832137,6.01563211736939,123.045720569644));
#213906=CARTESIAN_POINT('Ctrl Pts',(3.02012383166216,6.05632189648086,123.049910250587));
#213907=CARTESIAN_POINT('Ctrl Pts',(2.9403707940658,6.09544007382996,123.05409993153));
#213908=CARTESIAN_POINT('Ctrl Pts',(2.85991315049611,6.13295897358032,123.058289612473));
#213909=CARTESIAN_POINT('Ctrl Pts',(2.70020941886589,6.20743180215135,123.066605884877));
#213910=CARTESIAN_POINT('Ctrl Pts',(2.53744008902743,6.275734827549,123.074922157281));
#213911=CARTESIAN_POINT('Ctrl Pts',(2.37211676705733,6.33761398662348,123.083238429685));
#213912=CARTESIAN_POINT('Ctrl Pts',(2.20693322615066,6.39944082679608,123.091547670671));
#213913=CARTESIAN_POINT('Ctrl Pts',(2.03920031965934,6.45485450061438,123.099856911657));
#213914=CARTESIAN_POINT('Ctrl Pts',(1.86945128349512,6.50364827605541,123.108166152643));
#213915=CARTESIAN_POINT('Ctrl Pts',(1.69981464746498,6.55240974246525,123.116469891626));
#213916=CARTESIAN_POINT('Ctrl Pts',(1.52816487515849,6.59455994910529,123.124773630608));
#213917=CARTESIAN_POINT('Ctrl Pts',(1.35505229717509,6.62994134754754,123.13307736959));
#213918=CARTESIAN_POINT('Ctrl Pts',(1.18202262106089,6.6653058021946,123.141377131996));
#213919=CARTESIAN_POINT('Ctrl Pts',(1.00753187552673,6.69390783910127,123.149676894402));
#213920=CARTESIAN_POINT('Ctrl Pts',(0.832142794086401,6.71564050335112,
123.157976656807));
#213921=CARTESIAN_POINT('Ctrl Pts',(0.656805572898131,6.73736674153706,
123.166273965082));
#213922=CARTESIAN_POINT('Ctrl Pts',(0.480570890164451,6.7522276130539,123.174571273356));
#213923=CARTESIAN_POINT('Ctrl Pts',(0.30400907717678,6.76016771101088,123.182868581631));
#213924=CARTESIAN_POINT('Ctrl Pts',(0.127429425179038,6.76810861119959,
123.191166728228));
#213925=CARTESIAN_POINT('Ctrl Pts',(-0.0494770758812695,6.76912731746488,
123.199464874825));
#213926=CARTESIAN_POINT('Ctrl Pts',(-0.226137003931016,6.76322046479731,
123.207763021422));
#213927=CARTESIAN_POINT('Ctrl Pts',(-0.402814696247761,6.75731301815855,
123.216062002451));
#213928=CARTESIAN_POINT('Ctrl Pts',(-0.579245418172349,6.74447863558347,
123.224360983479));
#213929=CARTESIAN_POINT('Ctrl Pts',(-0.754857874338941,6.72476606206852,
123.232659964507));
#213930=CARTESIAN_POINT('Ctrl Pts',(-0.930517174245742,6.70504823032364,
123.240961159246));
#213931=CARTESIAN_POINT('Ctrl Pts',(-1.1053574274804,6.67844858968281,123.249262353986));
#213932=CARTESIAN_POINT('Ctrl Pts',(-1.27881437867367,6.64506755307254,
123.257563548725));
#213933=CARTESIAN_POINT('Ctrl Pts',(-1.45234642861127,6.61167206403522,
123.265868337494));
#213934=CARTESIAN_POINT('Ctrl Pts',(-1.62449364134901,6.5714893932261,123.274173126262));
#213935=CARTESIAN_POINT('Ctrl Pts',(-1.79470364850953,6.52467070540932,
123.282477915031));
#213936=CARTESIAN_POINT('Ctrl Pts',(-1.96511543810503,6.47779651445858,
123.290792549052));
#213937=CARTESIAN_POINT('Ctrl Pts',(-2.13358509775705,6.42427068088018,
123.299107183073));
#213938=CARTESIAN_POINT('Ctrl Pts',(-2.29957594429869,6.36429410668637,
123.307421817094));
#213939=CARTESIAN_POINT('Ctrl Pts',(-2.46567174832421,6.30427960877296,
123.315741708532));
#213940=CARTESIAN_POINT('Ctrl Pts',(-2.62928529154253,6.23780636679659,
123.324061599969));
#213941=CARTESIAN_POINT('Ctrl Pts',(-2.78990134639432,6.16512282743719,
123.332381491407));
#213942=CARTESIAN_POINT('Ctrl Pts',(-2.95075757432773,6.09233060261888,
123.34071382378));
#213943=CARTESIAN_POINT('Ctrl Pts',(-3.10860704519385,6.01330967734598,
123.349046156154));
#213944=CARTESIAN_POINT('Ctrl Pts',(-3.26295933800925,5.92835435500428,
123.357378488527));
#213945=CARTESIAN_POINT('Ctrl Pts',(-3.37916881099805,5.86439279630733,
123.363651773725));
#213946=CARTESIAN_POINT('Ctrl Pts',(-3.49339649231599,5.79706835352984,
123.369925058924));
#213947=CARTESIAN_POINT('Ctrl Pts',(-3.60544469942284,5.72652228838793,
123.376198344122));
#213948=CARTESIAN_POINT('Ctrl Pts',(-3.74958158267289,5.63577304556057,
123.384268190125));
#213949=CARTESIAN_POINT('Ctrl Pts',(-3.89055611171987,5.53941070198235,
123.392338036128));
#213950=CARTESIAN_POINT('Ctrl Pts',(-4.02788897276636,5.43768327719326,
123.40040788213));
#213951=CARTESIAN_POINT('Ctrl Pts',(-4.16504905160565,5.33608383844372,
123.408467575241));
#213952=CARTESIAN_POINT('Ctrl Pts',(-4.29857628274578,5.22913296827748,
123.416527268351));
#213953=CARTESIAN_POINT('Ctrl Pts',(-4.42801627508799,5.11712427712635,
123.424586961461));
#213954=CARTESIAN_POINT('Ctrl Pts',(-4.5573218234387,5.00523192479176,123.432638283299));
#213955=CARTESIAN_POINT('Ctrl Pts',(-4.68254830134607,4.88829244775038,
123.440689605138));
#213956=CARTESIAN_POINT('Ctrl Pts',(-4.80327072619441,4.76664235399341,
123.448740926976));
#213957=CARTESIAN_POINT('Ctrl Pts',(-4.92389421602702,4.64509195549981,
123.456785650557));
#213958=CARTESIAN_POINT('Ctrl Pts',(-5.0400207379763,4.51883888733626,123.464830374139));
#213959=CARTESIAN_POINT('Ctrl Pts',(-5.15125890602972,4.38825941382794,
123.47287509772));
#213960=CARTESIAN_POINT('Ctrl Pts',(-5.26243026173404,4.25775836952715,
123.480914989444));
#213961=CARTESIAN_POINT('Ctrl Pts',(-5.36871886700291,4.12293637607806,
123.488954881168));
#213962=CARTESIAN_POINT('Ctrl Pts',(-5.46977077762932,3.98420589831805,
123.496994772893));
#213963=CARTESIAN_POINT('Ctrl Pts',(-5.57299861274131,3.84248817329489,
123.505207785513));
#213964=CARTESIAN_POINT('Ctrl Pts',(-5.6707613933312,3.69669201663191,123.513420798133));
#213965=CARTESIAN_POINT('Ctrl Pts',(-5.76272553304017,3.5472924084218,123.521633810753));
#213966=CARTESIAN_POINT('Ctrl Pts',(-5.85271976339828,3.4010930007046,123.529670897295));
#213967=CARTESIAN_POINT('Ctrl Pts',(-5.93716106226926,3.25144329030274,
123.537707983838));
#213968=CARTESIAN_POINT('Ctrl Pts',(-6.01578116995975,3.09881685731147,
123.54574507038));
#213969=CARTESIAN_POINT('Ctrl Pts',(-6.09440880196054,2.94617581726006,
123.55378292611));
#213970=CARTESIAN_POINT('Ctrl Pts',(-6.16721396225864,2.79055781946378,
123.561820781839));
#213971=CARTESIAN_POINT('Ctrl Pts',(-6.23397498433766,2.63245985622807,
123.569858637568));
#213972=CARTESIAN_POINT('Ctrl Pts',(-6.30075562334466,2.47431543779646,
123.577898855125));
#213973=CARTESIAN_POINT('Ctrl Pts',(-6.36148844380825,2.31368994745968,
123.585939072682));
#213974=CARTESIAN_POINT('Ctrl Pts',(-6.41600048956491,2.15109895586021,
123.593979290239));
#213975=CARTESIAN_POINT('Ctrl Pts',(-6.47257203533698,1.9823651724235,123.602323272366));
#213976=CARTESIAN_POINT('Ctrl Pts',(-6.52244343393842,1.81151489298898,
123.610667254494));
#213977=CARTESIAN_POINT('Ctrl Pts',(-6.56547887783275,1.63913883021911,
123.619011236622));
#213978=CARTESIAN_POINT('Ctrl Pts',(-6.60701979982183,1.47274899132513,
123.627065451457));
#213979=CARTESIAN_POINT('Ctrl Pts',(-6.6421915909967,1.30493794008595,123.635119666292));
#213980=CARTESIAN_POINT('Ctrl Pts',(-6.67092482339485,1.136244252181,123.643173881127));
#213981=CARTESIAN_POINT('Ctrl Pts',(-6.69967955786621,0.967424324945361,
123.65123412321));
#213982=CARTESIAN_POINT('Ctrl Pts',(-6.72198609155787,0.797720813758334,
123.659294365293));
#213983=CARTESIAN_POINT('Ctrl Pts',(-6.73782702997512,0.627675006780346,
123.667354607376));
#213984=CARTESIAN_POINT('Ctrl Pts',(-6.75369011511081,0.457391464100649,
123.675426118231));
#213985=CARTESIAN_POINT('Ctrl Pts',(-6.76306954960573,0.286765040342059,
123.683497629085));
#213986=CARTESIAN_POINT('Ctrl Pts',(-6.76599993523862,0.11633518965076,
123.691569139939));
#213987=CARTESIAN_POINT('Ctrl Pts',(-6.7663070702486,0.0984723618691296,
123.69241511855));
#213988=CARTESIAN_POINT('Ctrl Pts',(-6.766543407694,0.080611686774495,123.693261097161));
#213989=CARTESIAN_POINT('Ctrl Pts',(-6.7667090201264,0.0627537802848805,
123.694107075772));
#213990=CARTESIAN_POINT('Ctrl Pts',(-6.76690952899891,0.0411330079578402,
123.695131311784));
#213991=CARTESIAN_POINT('Ctrl Pts',(-6.76700640827308,0.0195120367193917,
123.696155547797));
#213992=CARTESIAN_POINT('Ctrl Pts',(-6.76699967149979,-0.00210853544012529,
123.69717978381));
#213993=CARTESIAN_POINT('',(-6.767,-9.58377703494387E-10,123.302820216235));
#213994=CARTESIAN_POINT('Ctrl Pts',(3.09910619832147,6.01563211736933,122.651395695404));
#213995=CARTESIAN_POINT('Ctrl Pts',(2.93375330764849,6.10081787314642,122.660145143307));
#213996=CARTESIAN_POINT('Ctrl Pts',(2.76488627843102,6.17918207037025,122.668894591209));
#213997=CARTESIAN_POINT('Ctrl Pts',(2.59307866646743,6.2504585455398,122.677644039111));
#213998=CARTESIAN_POINT('Ctrl Pts',(2.42127244185422,6.3217344451502,122.686393416362));
#213999=CARTESIAN_POINT('Ctrl Pts',(2.24652594672514,6.3859226274182,122.695142793612));
#214000=CARTESIAN_POINT('Ctrl Pts',(2.06943269687175,6.44280508110544,122.703892170862));
#214001=CARTESIAN_POINT('Ctrl Pts',(1.89234081822129,6.49968709436151,122.712641480368));
#214002=CARTESIAN_POINT('Ctrl Pts',(1.71290249405639,6.54926340459532,122.721390789873));
#214003=CARTESIAN_POINT('Ctrl Pts',(1.53172716625107,6.59136563150372,122.730140099378));
#214004=CARTESIAN_POINT('Ctrl Pts',(1.35055318107384,6.633467546407,122.738889344046));
#214005=CARTESIAN_POINT('Ctrl Pts',(1.16764249714472,6.66809542395767,122.747638588713));
#214006=CARTESIAN_POINT('Ctrl Pts',(0.983616340614894,6.6951316562466,122.75638783338));
#214007=CARTESIAN_POINT('Ctrl Pts',(0.799591486714353,6.72216769715955,
122.765137016116));
#214008=CARTESIAN_POINT('Ctrl Pts',(0.614451459527195,6.74161215869367,
122.773886198851));
#214009=CARTESIAN_POINT('Ctrl Pts',(0.428825047910737,6.75339900185709,
122.782635381587));
#214010=CARTESIAN_POINT('Ctrl Pts',(0.243199888597508,6.76518576550219,
122.791384505298));
#214011=CARTESIAN_POINT('Ctrl Pts',(0.057088637392387,6.76931499599834,
122.800133629008));
#214012=CARTESIAN_POINT('Ctrl Pts',(-0.128876626810673,6.76577266947848,
122.808882752719));
#214013=CARTESIAN_POINT('Ctrl Pts',(-0.314840698187782,6.76223036567995,
122.81763182031));
#214014=CARTESIAN_POINT('Ctrl Pts',(-0.500658497950976,6.75101660879225,
122.826380887902));
#214015=CARTESIAN_POINT('Ctrl Pts',(-0.68569895192604,6.7321694829622,122.835129955493));
#214016=CARTESIAN_POINT('Ctrl Pts',(-0.870738280459613,6.71332247176296,
122.843878969872));
#214017=CARTESIAN_POINT('Ctrl Pts',(-1.05499998761221,6.68684221356191,
122.85262798425));
#214018=CARTESIAN_POINT('Ctrl Pts',(-1.23785829161384,6.65281863948529,
122.861376998629));
#214019=CARTESIAN_POINT('Ctrl Pts',(-1.43007412917354,6.61705395368871,
122.870573732328));
#214020=CARTESIAN_POINT('Ctrl Pts',(-1.6207388253573,6.57295372727805,122.879770466027));
#214021=CARTESIAN_POINT('Ctrl Pts',(-1.80913696091439,6.520683434783,122.888967199726));
#214022=CARTESIAN_POINT('Ctrl Pts',(-1.98838356186041,6.4709521981522,122.89771719744));
#214023=CARTESIAN_POINT('Ctrl Pts',(-2.16557827572465,6.41382586850914,
122.906467195154));
#214024=CARTESIAN_POINT('Ctrl Pts',(-2.34011918621636,6.34949849943302,
122.915217192867));
#214025=CARTESIAN_POINT('Ctrl Pts',(-2.51465655691031,6.28517243495577,
122.923967013126));
#214026=CARTESIAN_POINT('Ctrl Pts',(-2.68653996295258,6.21364572242405,
122.932716833384));
#214027=CARTESIAN_POINT('Ctrl Pts',(-2.85518555379916,6.13516132252255,
122.941466653642));
#214028=CARTESIAN_POINT('Ctrl Pts',(-3.02382794858621,6.0566784100054,122.95021630808));
#214029=CARTESIAN_POINT('Ctrl Pts',(-3.18923239109218,5.97123819492115,
122.958965962517));
#214030=CARTESIAN_POINT('Ctrl Pts',(-3.3508370596764,5.87913088810746,122.967715616955));
#214031=CARTESIAN_POINT('Ctrl Pts',(-3.51243888042341,5.78702520443139,
122.976465117204));
#214032=CARTESIAN_POINT('Ctrl Pts',(-3.67024081223631,5.68825280605822,
122.985214617453));
#214033=CARTESIAN_POINT('Ctrl Pts',(-3.82370687544341,5.58314917682546,
122.993964117702));
#214034=CARTESIAN_POINT('Ctrl Pts',(-3.97717043817766,5.47804726008058,
123.002713475392));
#214035=CARTESIAN_POINT('Ctrl Pts',(-4.12629803722421,5.36661448084267,
123.011462833083));
#214036=CARTESIAN_POINT('Ctrl Pts',(-4.27058317206878,5.24922931204601,
123.020212190773));
#214037=CARTESIAN_POINT('Ctrl Pts',(-4.41486614774812,5.13184589986811,
123.028961417533));
#214038=CARTESIAN_POINT('Ctrl Pts',(-4.55430658194397,5.0085104572305,123.037710644293));
#214039=CARTESIAN_POINT('Ctrl Pts',(-4.68843089001835,4.87964187103129,
123.046459871053));
#214040=CARTESIAN_POINT('Ctrl Pts',(-4.82255336917826,4.75077504207971,
123.055208978509));
#214041=CARTESIAN_POINT('Ctrl Pts',(-4.95135966065125,4.61637541908104,
123.063958085965));
#214042=CARTESIAN_POINT('Ctrl Pts',(-5.07441230869235,4.47689945401855,
123.072707193421));
#214043=CARTESIAN_POINT('Ctrl Pts',(-5.19746344226408,4.33742520555527,
123.081456193197));
#214044=CARTESIAN_POINT('Ctrl Pts',(-5.31476088454758,4.19287495491348,
123.090205192974));
#214045=CARTESIAN_POINT('Ctrl Pts',(-5.42590627628844,4.04373961586719,
123.09895419275));
#214046=CARTESIAN_POINT('Ctrl Pts',(-5.53706380672662,3.89458798906743,
123.107704148045));
#214047=CARTESIAN_POINT('Ctrl Pts',(-5.64206777071861,3.74085050155288,
123.11645410334));
#214048=CARTESIAN_POINT('Ctrl Pts',(-5.74056148164008,3.58304938223161,
123.125204058634));
#214049=CARTESIAN_POINT('Ctrl Pts',(-5.83905138951875,3.42525435593296,
123.133953676075));
#214050=CARTESIAN_POINT('Ctrl Pts',(-5.93103139557637,3.26339625497211,
123.142703293517));
#214051=CARTESIAN_POINT('Ctrl Pts',(-6.01618907820824,3.09802485065047,
123.151452910958));
#214052=CARTESIAN_POINT('Ctrl Pts',(-6.10134392544964,2.9326589524968,123.160202237074));
#214053=CARTESIAN_POINT('Ctrl Pts',(-6.17967677261815,2.76378023986072,
123.168951563189));
#214054=CARTESIAN_POINT('Ctrl Pts',(-6.2509215700921,2.5919622922715,123.177700889305));
#214055=CARTESIAN_POINT('Ctrl Pts',(-6.32216437407743,2.42014915229118,
123.186449970608));
#214056=CARTESIAN_POINT('Ctrl Pts',(-6.38631941548914,2.24539720662871,
123.19519905191));
#214057=CARTESIAN_POINT('Ctrl Pts',(-6.44316881037533,2.06829994947699,
123.203948133213));
#214058=CARTESIAN_POINT('Ctrl Pts',(-6.50002334524571,1.89118668024453,
123.212698005555));
#214059=CARTESIAN_POINT('Ctrl Pts',(-6.54957082411098,1.71172794807696,
123.221447877897));
#214060=CARTESIAN_POINT('Ctrl Pts',(-6.59164294296087,1.53053334250324,
123.23019775024));
#214061=CARTESIAN_POINT('Ctrl Pts',(-6.63371214082135,1.34935131693592,
123.238947015095));
#214062=CARTESIAN_POINT('Ctrl Pts',(-6.66830695239689,1.16643393829764,
123.247696279949));
#214063=CARTESIAN_POINT('Ctrl Pts',(-6.69530988153987,0.982402458341086,
123.256445544804));
#214064=CARTESIAN_POINT('Ctrl Pts',(-6.72231419690482,0.79836153094714,
123.265195258811));
#214065=CARTESIAN_POINT('Ctrl Pts',(-6.74172580829277,0.613206671362544,
123.273944972818));
#214066=CARTESIAN_POINT('Ctrl Pts',(-6.75347878028179,0.42756679511345,
123.282694686825));
#214067=CARTESIAN_POINT('Ctrl Pts',(-6.76248992368205,0.285234494207005,
123.289403196614));
#214068=CARTESIAN_POINT('Ctrl Pts',(-6.76699999999986,0.142617266095549,
123.296111706402));
#214069=CARTESIAN_POINT('Ctrl Pts',(-6.767,6.54126883298573E-12,123.30282021619));
#214070=CARTESIAN_POINT('Ctrl Pts',(-6.767,-9.58186202505161E-10,123.302820216235));
#214071=CARTESIAN_POINT('Ctrl Pts',(-6.76699999997366,-0.186007250485151,
123.311569728047));
#214072=CARTESIAN_POINT('Ctrl Pts',(-6.75932637289252,-0.372014356707202,
123.320319239858));
#214073=CARTESIAN_POINT('Ctrl Pts',(-6.74400518256286,-0.557389538442699,
123.329068751669));
#214074=CARTESIAN_POINT('Ctrl Pts',(-6.72868405694564,-0.742763937204996,
123.337818226525));
#214075=CARTESIAN_POINT('Ctrl Pts',(-6.70571545632584,-0.92750613119238,
123.34656770138));
#214076=CARTESIAN_POINT('Ctrl Pts',(-6.67517739389057,-1.11098864084755,
123.355317176236));
#214077=CARTESIAN_POINT('Ctrl Pts',(-6.64463945790326,-1.29447039076273,
123.364066614863));
#214078=CARTESIAN_POINT('Ctrl Pts',(-6.60653216987388,-1.47669218407489,
123.37281605349));
#214079=CARTESIAN_POINT('Ctrl Pts',(-6.56098496069144,-1.65703510692464,
123.381565492117));
#214080=CARTESIAN_POINT('Ctrl Pts',(-6.515437936322,-1.83737729801239,123.390314895242));
#214081=CARTESIAN_POINT('Ctrl Pts',(-6.46245112138787,-2.01584035602721,
123.399064298367));
#214082=CARTESIAN_POINT('Ctrl Pts',(-6.40220448343118,-2.19181813851737,
123.407813701493));
#214083=CARTESIAN_POINT('Ctrl Pts',(-6.34195808492866,-2.3677952215724,
123.416563069843));
#214084=CARTESIAN_POINT('Ctrl Pts',(-6.27445201396999,-2.54128677773308,
123.425312438193));
#214085=CARTESIAN_POINT('Ctrl Pts',(-6.19991555033374,-2.71170355472901,
123.434061806543));
#214086=CARTESIAN_POINT('Ctrl Pts',(-6.12537937675744,-2.88211966854504,
123.442811140845));
#214087=CARTESIAN_POINT('Ctrl Pts',(-6.04381298009196,-3.0494607645765,
123.451560475146));
#214088=CARTESIAN_POINT('Ctrl Pts',(-5.95549339290184,-3.21315848459153,
123.460309809448));
#214089=CARTESIAN_POINT('Ctrl Pts',(-5.86717414207446,-3.37685558116826,
123.469059110428));
#214090=CARTESIAN_POINT('Ctrl Pts',(-5.77210188826372,-3.53690907728723,
123.477808411409));
#214091=CARTESIAN_POINT('Ctrl Pts',(-5.67059953294568,-3.69277537049796,
123.486557712389));
#214092=CARTESIAN_POINT('Ctrl Pts',(-5.56909755576737,-3.84864108303999,
123.495306980774));
#214093=CARTESIAN_POINT('Ctrl Pts',(-5.46116568140044,-4.00031938375068,
123.504056249159));
#214094=CARTESIAN_POINT('Ctrl Pts',(-5.34717048474704,-4.14729511935794,
123.512805517545));
#214095=CARTESIAN_POINT('Ctrl Pts',(-5.23317570330848,-4.29427031962239,
123.521554754062));
#214096=CARTESIAN_POINT('Ctrl Pts',(-5.11311781940504,-4.43654276262166,
123.530303990579));
#214097=CARTESIAN_POINT('Ctrl Pts',(-4.98740458919794,-4.57362924422688,
123.539053227096));
#214098=CARTESIAN_POINT('Ctrl Pts',(-4.86169180644861,-4.71071523789291,
123.547802432471));
#214099=CARTESIAN_POINT('Ctrl Pts',(-4.73032391135441,-4.84261509590373,
123.556551637847));
#214100=CARTESIAN_POINT('Ctrl Pts',(-4.59374706943103,-4.96888084603504,
123.565300843222));
#214101=CARTESIAN_POINT('Ctrl Pts',(-4.45717070229154,-5.09514615722703,
123.574050018182));
#214102=CARTESIAN_POINT('Ctrl Pts',(-4.31538563497034,-5.21577720520759,
123.582799193143));
#214103=CARTESIAN_POINT('Ctrl Pts',(-4.16887340953873,-5.33036429292041,
123.591548368103));
#214104=CARTESIAN_POINT('Ctrl Pts',(-4.02236168126448,-5.44495099180689,
123.600297513375));
#214105=CARTESIAN_POINT('Ctrl Pts',(-3.87112305269371,-5.55349359493526,
123.609046658647));
#214106=CARTESIAN_POINT('Ctrl Pts',(-3.71567116937521,-5.6556234635161,
123.617795803919));
#214107=CARTESIAN_POINT('Ctrl Pts',(-3.5602198006411,-5.75775299402168,
123.62654492023));
#214108=CARTESIAN_POINT('Ctrl Pts',(-3.40055544455261,-5.85346967512143,
123.63529403654));
#214109=CARTESIAN_POINT('Ctrl Pts',(-3.23722035902481,-5.94244843032864,
123.64404315285));
#214110=CARTESIAN_POINT('Ctrl Pts',(-3.07388580061552,-6.03142689838168,
123.652792240925));
#214111=CARTESIAN_POINT('Ctrl Pts',(-2.90688078809791,-6.11366734698046,
123.661541329));
#214112=CARTESIAN_POINT('Ctrl Pts',(-2.73677250633523,-6.188890469912,123.670290417074));
#214113=CARTESIAN_POINT('Ctrl Pts',(-2.56666475942524,-6.26411335632778,
123.679039477641));
#214114=CARTESIAN_POINT('Ctrl Pts',(-2.39345402485196,-6.33231884534564,
123.687788538207));
#214115=CARTESIAN_POINT('Ctrl Pts',(-2.21772855974711,-6.39327529794252,
123.696537598773));
#214116=CARTESIAN_POINT('Ctrl Pts',(-2.04200363256776,-6.45423156394135,
123.705286632556));
#214117=CARTESIAN_POINT('Ctrl Pts',(-1.86376426096788,-6.50793874402146,
123.71403566634));
#214118=CARTESIAN_POINT('Ctrl Pts',(-1.68361577660017,-6.55421443933467,
123.722784700124));
#214119=CARTESIAN_POINT('Ctrl Pts',(-1.50346782874008,-6.60048999683232,
123.731533707851));
#214120=CARTESIAN_POINT('Ctrl Pts',(-1.32141105700646,-6.63933404256489,
123.740282715579));
#214121=CARTESIAN_POINT('Ctrl Pts',(-1.1380637539224,-6.67061465623731,
123.749031723307));
#214122=CARTESIAN_POINT('Ctrl Pts',(-0.95471698165129,-6.70189517934853,
123.757780705705));
#214123=CARTESIAN_POINT('Ctrl Pts',(-0.770079967947586,-6.72561226603156,
123.766529688104));
#214124=CARTESIAN_POINT('Ctrl Pts',(-0.584779764601956,-6.74168536991397,
123.775278670502));
#214125=CARTESIAN_POINT('Ctrl Pts',(-0.39148982970262,-6.7584515101932,
123.784404889512));
#214126=CARTESIAN_POINT('Ctrl Pts',(-0.197478577298523,-6.76689983034339,
123.793531108521));
#214127=CARTESIAN_POINT('Ctrl Pts',(-0.00346287552154453,-6.76699911397165,
123.80265732753));
#214128=CARTESIAN_POINT('Ctrl Pts',(0.184489835574943,-6.76709529498653,
123.811498352196));
#214129=CARTESIAN_POINT('Ctrl Pts',(0.372446405159711,-6.75935639733125,
123.820339376861));
#214130=CARTESIAN_POINT('Ctrl Pts',(0.559755020386987,-6.74380925865727,
123.829180401527));
#214131=CARTESIAN_POINT('Ctrl Pts',(0.745134706418459,-6.72842222649875,
123.837930380136));
#214132=CARTESIAN_POINT('Ctrl Pts',(0.929879432122264,-6.7053870604513,
123.846680358746));
#214133=CARTESIAN_POINT('Ctrl Pts',(1.11336163715795,-6.67478200879287,
123.855430337356));
#214134=CARTESIAN_POINT('Ctrl Pts',(1.29684196389297,-6.64417727043724,
123.864180226392));
#214135=CARTESIAN_POINT('Ctrl Pts',(1.47905951305596,-6.60600284870869,
123.872930115429));
#214136=CARTESIAN_POINT('Ctrl Pts',(1.65939532154578,-6.560388415851,123.881680004465));
#214137=CARTESIAN_POINT('Ctrl Pts',(1.83972934387687,-6.51477443478721,
123.890429806838));
#214138=CARTESIAN_POINT('Ctrl Pts',(2.01818138492442,-6.46172066035225,
123.89917960921));
#214139=CARTESIAN_POINT('Ctrl Pts',(2.19414528439572,-6.40140730394216,
123.907929411582));
#214140=CARTESIAN_POINT('Ctrl Pts',(2.37010749948567,-6.34109452487033,
123.916679130198));
#214141=CARTESIAN_POINT('Ctrl Pts',(2.54358134950125,-6.27352239582582,
123.925428848814));
#214142=CARTESIAN_POINT('Ctrl Pts',(2.71397759518225,-6.19892043930625,
123.934178567431));
#214143=CARTESIAN_POINT('Ctrl Pts',(2.88437226639804,-6.12431917211046,
123.942928205199));
#214144=CARTESIAN_POINT('Ctrl Pts',(3.05168912761553,-6.04268832238096,
123.951677842968));
#214145=CARTESIAN_POINT('Ctrl Pts',(3.21535986353278,-5.95430516080445,
123.960427480737));
#214146=CARTESIAN_POINT('Ctrl Pts',(3.37902914151091,-5.86592278652365,
123.969177040566));
#214147=CARTESIAN_POINT('Ctrl Pts',(3.53905210698558,-5.77078835694729,
123.977926600395));
#214148=CARTESIAN_POINT('Ctrl Pts',(3.69488522907333,-5.66922500382334,
123.986676160224));
#214149=CARTESIAN_POINT('Ctrl Pts',(3.85071701481236,-5.56766252165709,
123.995425645021));
#214150=CARTESIAN_POINT('Ctrl Pts',(4.00235878895273,-5.45967138275952,
124.004175129818));
#214151=CARTESIAN_POINT('Ctrl Pts',(4.14929549682686,-5.34561838144216,
124.012924614616));
#214152=CARTESIAN_POINT('Ctrl Pts',(4.29623099345934,-5.23156632029659,
124.021674027288));
#214153=CARTESIAN_POINT('Ctrl Pts',(4.43846127504273,-5.11145267245704,
124.030423439961));
#214154=CARTESIAN_POINT('Ctrl Pts',(4.57550326121013,-4.98568539988791,
124.039172852633));
#214155=CARTESIAN_POINT('Ctrl Pts',(4.71254416322669,-4.85991912227439,
124.047922196089));
#214156=CARTESIAN_POINT('Ctrl Pts',(4.84439664081892,-4.7284995032074,124.056671539544));
#214157=CARTESIAN_POINT('Ctrl Pts',(4.97061286856049,-4.59187289794708,
124.065420882999));
#214158=CARTESIAN_POINT('Ctrl Pts',(5.09682813972158,-4.45524732816647,
124.074170160144));
#214159=CARTESIAN_POINT('Ctrl Pts',(5.21740705205413,-4.31341506166147,
124.082919437289));
#214160=CARTESIAN_POINT('Ctrl Pts',(5.33194007601308,-4.16685781204562,
124.091668714433));
#214161=CARTESIAN_POINT('Ctrl Pts',(5.44647226998129,-4.02030162449168,
124.100417928175));
#214162=CARTESIAN_POINT('Ctrl Pts',(5.55495848679725,-3.86902074813831,
124.109167141916));
#214163=CARTESIAN_POINT('Ctrl Pts',(5.65703027341314,-3.71352898005216,
124.117916355657));
#214164=CARTESIAN_POINT('Ctrl Pts',(5.75910135424448,-3.55803828712783,
124.126665508901));
#214165=CARTESIAN_POINT('Ctrl Pts',(5.85475793638072,-3.39833700028633,
124.135414662145));
#214166=CARTESIAN_POINT('Ctrl Pts',(5.94367514470539,-3.23496750744291,
124.144163815388));
#214167=CARTESIAN_POINT('Ctrl Pts',(6.032591767736,-3.0715990899728,124.152912911041));
#214168=CARTESIAN_POINT('Ctrl Pts',(6.11476896874655,-2.90456276649896,
124.161662006694));
#214169=CARTESIAN_POINT('Ctrl Pts',(6.18992765584347,-2.73442582920513,
124.170411102347));
#214170=CARTESIAN_POINT('Ctrl Pts',(6.2650858731725,-2.56428995532624,124.179160143315));
#214171=CARTESIAN_POINT('Ctrl Pts',(6.33322554859048,-2.3910537685074,124.187909184283));
#214172=CARTESIAN_POINT('Ctrl Pts',(6.39411526762577,-2.215305609688,124.196658225251));
#214173=CARTESIAN_POINT('Ctrl Pts',(6.45500462630047,-2.03955849099014,
124.20540721444));
#214174=CARTESIAN_POINT('Ctrl Pts',(6.5086440206556,-1.86129970077754,124.214156203629));
#214175=CARTESIAN_POINT('Ctrl Pts',(6.55485128391016,-1.6811346304866,124.222905192818));
#214176=CARTESIAN_POINT('Ctrl Pts',(6.6019980957382,-1.49730620030677,124.231832078289));
#214177=CARTESIAN_POINT('Ctrl Pts',(6.64140720724573,-1.31149343160855,
124.24075896376));
#214178=CARTESIAN_POINT('Ctrl Pts',(6.67293928736931,-1.12435326614156,
124.24968584923));
#214179=CARTESIAN_POINT('Ctrl Pts',(6.70384625888012,-0.940923066169056,
124.258435763408));
#214180=CARTESIAN_POINT('Ctrl Pts',(6.72718554589243,-0.75621789868124,
124.267185677585));
#214181=CARTESIAN_POINT('Ctrl Pts',(6.74287786822459,-0.570865180412135,
124.275935591762));
#214182=CARTESIAN_POINT('Ctrl Pts',(6.75856988195661,-0.385516107229694,
124.284685333867));
#214183=CARTESIAN_POINT('Ctrl Pts',(6.76661520775895,-0.199519794381159,
124.293435075971));
#214184=CARTESIAN_POINT('Ctrl Pts',(6.76698651789748,-0.0135080196104832,
124.302184818076));
#214185=CARTESIAN_POINT('Ctrl Pts',(6.76735782122748,0.172500344358102,
124.310934399741));
#214186=CARTESIAN_POINT('Ctrl Pts',(6.76005538990706,0.35852388305508,124.319683981406));
#214187=CARTESIAN_POINT('Ctrl Pts',(6.74510402735569,0.543930749406598,
124.328433563071));
#214188=CARTESIAN_POINT('Ctrl Pts',(6.73015291908924,0.729334462455587,
124.337182995927));
#214189=CARTESIAN_POINT('Ctrl Pts',(6.70755316295181,0.914121238472207,
124.345932428784));
#214190=CARTESIAN_POINT('Ctrl Pts',(6.67738151860868,1.09766345249497,124.354681861641));
#214191=CARTESIAN_POINT('Ctrl Pts',(6.64721034731574,1.28120278882651,124.363431157318));
#214192=CARTESIAN_POINT('Ctrl Pts',(6.60946757186873,1.46349731942832,124.372180452996));
#214193=CARTESIAN_POINT('Ctrl Pts',(6.56428138091005,1.64392790360088,124.380929748673));
#214194=CARTESIAN_POINT('Ctrl Pts',(6.51909583837082,1.82435589860415,124.389678918799));
#214195=CARTESIAN_POINT('Ctrl Pts',(6.4664671636788,2.00291972272963,124.398428088925));
#214196=CARTESIAN_POINT('Ctrl Pts',(6.40657409845692,2.1790129235461,124.40717725905));
#214197=CARTESIAN_POINT('Ctrl Pts',(6.34668181312688,2.35510383138174,124.415926315249));
#214198=CARTESIAN_POINT('Ctrl Pts',(6.27952541882496,2.52872390900938,124.424675371448));
#214199=CARTESIAN_POINT('Ctrl Pts',(6.20533299141835,2.69928350967715,124.433424427648));
#214200=CARTESIAN_POINT('Ctrl Pts',(6.12831602957061,2.87633638038868,124.442506563804));
#214201=CARTESIAN_POINT('Ctrl Pts',(6.04371690570292,3.05009086670547,124.451588699961));
#214202=CARTESIAN_POINT('Ctrl Pts',(5.95184520281472,3.21991112947724,124.460670836117));
#214203=CARTESIAN_POINT('Ctrl Pts',(5.86333549472327,3.38351691247043,124.469420616461));
#214204=CARTESIAN_POINT('Ctrl Pts',(5.76807618060673,3.54347103774993,124.478170396804));
#214205=CARTESIAN_POINT('Ctrl Pts',(5.66639083268618,3.69923018089576,124.486920177148));
#214206=CARTESIAN_POINT('Ctrl Pts',(5.56470914040105,3.85498372442815,124.495669642933));
#214207=CARTESIAN_POINT('Ctrl Pts',(5.45660203328321,4.00654234761577,124.504419108718));
#214208=CARTESIAN_POINT('Ctrl Pts',(5.34243669793871,4.15339128044996,124.513168574503));
#214209=CARTESIAN_POINT('Ctrl Pts',(5.22827486003637,4.30023571458367,124.521917772249));
#214210=CARTESIAN_POINT('Ctrl Pts',(5.10805534118599,4.44237052084252,124.530666969995));
#214211=CARTESIAN_POINT('Ctrl Pts',(4.98218644289937,4.57931296683135,124.539416167741));
#214212=CARTESIAN_POINT('Ctrl Pts',(4.85632073168066,4.71625194536412,124.548165143952));
#214213=CARTESIAN_POINT('Ctrl Pts',(4.72480612117347,4.84799861576135,124.556914120164));
#214214=CARTESIAN_POINT('Ctrl Pts',(4.58808925180949,4.97410554948628,124.565663096376));
#214215=CARTESIAN_POINT('Ctrl Pts',(4.45136349418311,5.10022068169853,124.574412641377));
#214216=CARTESIAN_POINT('Ctrl Pts',(4.30943501153029,5.22069514918927,124.583162186379));
#214217=CARTESIAN_POINT('Ctrl Pts',(4.16278587373484,5.33511975211744,124.591911731381));
#214218=CARTESIAN_POINT('Ctrl Pts',(4.01614535680894,5.44953762851731,124.600660762034));
#214219=CARTESIAN_POINT('Ctrl Pts',(3.8647849659718,5.55790617575023,124.609409792688));
#214220=CARTESIAN_POINT('Ctrl Pts',(3.70921874685333,5.65985735579898,124.618158823342));
#214221=CARTESIAN_POINT('Ctrl Pts',(3.55365041542928,5.76180992015885,124.626907972791));
#214222=CARTESIAN_POINT('Ctrl Pts',(3.39387638110511,5.85734478589903,124.635657122241));
#214223=CARTESIAN_POINT('Ctrl Pts',(3.23043927839561,5.94613749156533,124.644406271691));
#214224=CARTESIAN_POINT('Ctrl Pts',(3.18691767026854,5.96978206967205,124.646736079595));
#214225=CARTESIAN_POINT('Ctrl Pts',(3.1431364589772,5.99294880644713,124.6490658875));
#214226=CARTESIAN_POINT('Ctrl Pts',(3.09910619832142,6.01563211736936,124.651395695404));
#214227=CARTESIAN_POINT('Origin',(0.,0.,4.30282021618968));
#214228=CARTESIAN_POINT('',(3.09910619832142,6.01563211736936,127.045755263024));
#214229=CARTESIAN_POINT('',(3.0991061983215,6.01563211736932,126.651395695404));
#214230=CARTESIAN_POINT('',(3.09910619832133,6.0156321173694,4.30282021618968));
#214231=CARTESIAN_POINT('',(-6.7669980962981,0.00306854827779037,125.69717978381));
#214232=CARTESIAN_POINT('Ctrl Pts',(-6.767,6.53660624432471E-12,125.69717978381));
#214233=CARTESIAN_POINT('Ctrl Pts',(-6.76700000000018,-0.186007249520428,
125.705929295621));
#214234=CARTESIAN_POINT('Ctrl Pts',(-6.75932637294555,-0.372014355743573,
125.714678807432));
#214235=CARTESIAN_POINT('Ctrl Pts',(-6.74400518264232,-0.557389537481255,
125.723428319244));
#214236=CARTESIAN_POINT('Ctrl Pts',(-6.72868405705154,-0.742763936245608,
125.732177794099));
#214237=CARTESIAN_POINT('Ctrl Pts',(-6.7057154564581,-0.927506130236139,
125.740927268955));
#214238=CARTESIAN_POINT('Ctrl Pts',(-6.67517739404902,-1.11098863989554,
125.749676743811));
#214239=CARTESIAN_POINT('Ctrl Pts',(-6.6446394580879,-1.29447038981495,
125.758426182438));
#214240=CARTESIAN_POINT('Ctrl Pts',(-6.60653217008454,-1.47669218313241,
125.767175621065));
#214241=CARTESIAN_POINT('Ctrl Pts',(-6.56098496092786,-1.65703510598854,
125.775925059692));
#214242=CARTESIAN_POINT('Ctrl Pts',(-6.51543793658422,-1.83737729708254,
125.784674462817));
#214243=CARTESIAN_POINT('Ctrl Pts',(-6.46245112167563,-2.01584035510468,
125.793423865942));
#214244=CARTESIAN_POINT('Ctrl Pts',(-6.40220448374415,-2.1918181376032,
125.802173269067));
#214245=CARTESIAN_POINT('Ctrl Pts',(-6.34195808526676,-2.36779522066683,
125.810922637417));
#214246=CARTESIAN_POINT('Ctrl Pts',(-6.27445201433286,-2.54128677683716,
125.819672005767));
#214247=CARTESIAN_POINT('Ctrl Pts',(-6.19991555072094,-2.71170355384373,
125.828421374117));
#214248=CARTESIAN_POINT('Ctrl Pts',(-6.12537937716893,-2.88211966767052,
125.837170708419));
#214249=CARTESIAN_POINT('Ctrl Pts',(-6.04381298052728,-3.04946076371373,
125.845920042721));
#214250=CARTESIAN_POINT('Ctrl Pts',(-5.95549339336046,-3.21315848374148,
125.854669377023));
#214251=CARTESIAN_POINT('Ctrl Pts',(-5.86717414255645,-3.37685558033082,
125.863418678003));
#214252=CARTESIAN_POINT('Ctrl Pts',(-5.77210188876855,-3.53690907646335,
125.872167978983));
#214253=CARTESIAN_POINT('Ctrl Pts',(-5.67059953347276,-3.69277536968857,
125.880917279963));
#214254=CARTESIAN_POINT('Ctrl Pts',(-5.56909755631677,-3.84864108224499,
125.889666548349));
#214255=CARTESIAN_POINT('Ctrl Pts',(-5.46116568197157,-4.00031938297098,
125.898415816734));
#214256=CARTESIAN_POINT('Ctrl Pts',(-5.34717048533923,-4.14729511859441,
125.907165085119));
#214257=CARTESIAN_POINT('Ctrl Pts',(-5.23317570392174,-4.29427031887504,
125.915914321636));
#214258=CARTESIAN_POINT('Ctrl Pts',(-5.1131178200387,-4.43654276189137,
125.924663558153));
#214259=CARTESIAN_POINT('Ctrl Pts',(-4.98740458985127,-4.57362924351444,
125.93341279467));
#214260=CARTESIAN_POINT('Ctrl Pts',(-4.86169180712117,-4.71071523719882,
125.942162000046));
#214261=CARTESIAN_POINT('Ctrl Pts',(-4.73032391204544,-4.84261509522875,
125.950911205421));
#214262=CARTESIAN_POINT('Ctrl Pts',(-4.59374707013969,-4.96888084537988,
125.959660410797));
#214263=CARTESIAN_POINT('Ctrl Pts',(-4.4571707030184,-5.09514615659118,
125.968409585757));
#214264=CARTESIAN_POINT('Ctrl Pts',(-4.31538563571461,-5.21577720459179,
125.977158760717));
#214265=CARTESIAN_POINT('Ctrl Pts',(-4.16887341029955,-5.33036429232537,
125.985907935678));
#214266=CARTESIAN_POINT('Ctrl Pts',(-4.02236168204176,-5.44495099123268,
125.99465708095));
#214267=CARTESIAN_POINT('Ctrl Pts',(-3.87112305348659,-5.55349359438257,
126.003406226222));
#214268=CARTESIAN_POINT('Ctrl Pts',(-3.71567117018278,-5.65562346298554,
126.012155371494));
#214269=CARTESIAN_POINT('Ctrl Pts',(-3.56021980146347,-5.75775299351318,
126.020904487804));
#214270=CARTESIAN_POINT('Ctrl Pts',(-3.40055544538887,-5.8534696746356,
126.029653604114));
#214271=CARTESIAN_POINT('Ctrl Pts',(-3.23722035987401,-5.94244842986603,
126.038402720424));
#214272=CARTESIAN_POINT('Ctrl Pts',(-3.07388580147733,-6.03142689794247,
126.047151808499));
#214273=CARTESIAN_POINT('Ctrl Pts',(-2.90688078897135,-6.11366734656517,
126.055900896574));
#214274=CARTESIAN_POINT('Ctrl Pts',(-2.7367725072193,-6.18889046952106,
126.064649984649));
#214275=CARTESIAN_POINT('Ctrl Pts',(-2.56666476032041,-6.26411335596098,
126.073399045215));
#214276=CARTESIAN_POINT('Ctrl Pts',(-2.39345402575723,-6.33231884500346,
126.082148105781));
#214277=CARTESIAN_POINT('Ctrl Pts',(-2.21772856066146,-6.39327529762535,
126.090897166347));
#214278=CARTESIAN_POINT('Ctrl Pts',(-2.04200363349071,-6.45423156364935,
126.099646200131));
#214279=CARTESIAN_POINT('Ctrl Pts',(-1.86376426189839,-6.50793874375498,
126.108395233914));
#214280=CARTESIAN_POINT('Ctrl Pts',(-1.68361577753716,-6.55421443909398,
126.117144267698));
#214281=CARTESIAN_POINT('Ctrl Pts',(-1.50346782968394,-6.60048999661732,
126.125893275426));
#214282=CARTESIAN_POINT('Ctrl Pts',(-1.32141105795613,-6.63933404237587,
126.134642283154));
#214283=CARTESIAN_POINT('Ctrl Pts',(-1.1380637548768,-6.67061465607449,
126.143391290882));
#214284=CARTESIAN_POINT('Ctrl Pts',(-0.954716982609653,-6.70189517921202,
126.15214027328));
#214285=CARTESIAN_POINT('Ctrl Pts',(-0.770079968908832,-6.72561226592151,
126.160889255678));
#214286=CARTESIAN_POINT('Ctrl Pts',(-0.584779765564988,-6.74168536983044,
126.169638238077));
#214287=CARTESIAN_POINT('Ctrl Pts',(-0.391489830657955,-6.75845151013815,
126.178764457087));
#214288=CARTESIAN_POINT('Ctrl Pts',(-0.197478578244895,-6.76689983031606,
126.187890676097));
#214289=CARTESIAN_POINT('Ctrl Pts',(-0.00346287645780092,-6.76699911397117,
126.197016895106));
#214290=CARTESIAN_POINT('Ctrl Pts',(0.184489834648418,-6.76709529501206,
126.205857919772));
#214291=CARTESIAN_POINT('Ctrl Pts',(0.372446404243999,-6.75935639738198,
126.214698944438));
#214292=CARTESIAN_POINT('Ctrl Pts',(0.55975501948307,-6.7438092587323,126.223539969104));
#214293=CARTESIAN_POINT('Ctrl Pts',(0.745134705516604,-6.72842222659863,
126.232289947714));
#214294=CARTESIAN_POINT('Ctrl Pts',(0.929879431223498,-6.70538706057594,
126.241039926323));
#214295=CARTESIAN_POINT('Ctrl Pts',(1.11336163626329,-6.6747820089421,126.249789904933));
#214296=CARTESIAN_POINT('Ctrl Pts',(1.29684196300241,-6.64417727061106,
126.25853979397));
#214297=CARTESIAN_POINT('Ctrl Pts',(1.47905951217052,-6.60600284890693,
126.267289683006));
#214298=CARTESIAN_POINT('Ctrl Pts',(1.65939532066645,-6.56038841607342,
126.276039572043));
#214299=CARTESIAN_POINT('Ctrl Pts',(1.83972934300365,-6.5147744350338,126.284789374415));
#214300=CARTESIAN_POINT('Ctrl Pts',(2.01818138405831,-6.46172066062276,
126.293539176787));
#214301=CARTESIAN_POINT('Ctrl Pts',(2.1941452835377,-6.40140730423626,126.302288979159));
#214302=CARTESIAN_POINT('Ctrl Pts',(2.37010749863573,-6.34109452518802,
126.311038697775));
#214303=CARTESIAN_POINT('Ctrl Pts',(2.54358134866037,-6.27352239616675,
126.319788416392));
#214304=CARTESIAN_POINT('Ctrl Pts',(2.71397759435137,-6.19892043967002,
126.328538135008));
#214305=CARTESIAN_POINT('Ctrl Pts',(2.88437226557716,-6.12431917249707,
126.337287772777));
#214306=CARTESIAN_POINT('Ctrl Pts',(3.05168912680559,-6.04268832278999,
126.346037410546));
#214307=CARTESIAN_POINT('Ctrl Pts',(3.21535986273469,-5.95430516123542,
126.354787048314));
#214308=CARTESIAN_POINT('Ctrl Pts',(3.37902914072467,-5.86592278697657,
126.363536608143));
#214309=CARTESIAN_POINT('Ctrl Pts',(3.53905210621208,-5.77078835742165,
126.372286167972));
#214310=CARTESIAN_POINT('Ctrl Pts',(3.69488522831344,-5.66922500431859,
126.381035727801));
#214311=CARTESIAN_POINT('Ctrl Pts',(3.85071701406598,-5.5676625221733,126.389785212599));
#214312=CARTESIAN_POINT('Ctrl Pts',(4.00235878822073,-5.45967138329613,
126.398534697396));
#214313=CARTESIAN_POINT('Ctrl Pts',(4.14929549611005,-5.34561838199855,
126.407284182193));
#214314=CARTESIAN_POINT('Ctrl Pts',(4.29623099275782,-5.23156632087268,
126.416033594865));
#214315=CARTESIAN_POINT('Ctrl Pts',(4.43846127435732,-5.11145267305221,
126.424783007538));
#214316=CARTESIAN_POINT('Ctrl Pts',(4.57550326054159,-4.98568540050145,
126.433532420211));
#214317=CARTESIAN_POINT('Ctrl Pts',(4.71254416257501,-4.85991912290631,
126.442281763666));
#214318=CARTESIAN_POINT('Ctrl Pts',(4.84439664018486,-4.728499503857,126.451031107121));
#214319=CARTESIAN_POINT('Ctrl Pts',(4.97061286794475,-4.5918728986136,126.459780450576));
#214320=CARTESIAN_POINT('Ctrl Pts',(5.09682813912425,-4.45524732884982,
126.468529727721));
#214321=CARTESIAN_POINT('Ctrl Pts',(5.2174070514759,-4.31341506236089,126.477279004866));
#214322=CARTESIAN_POINT('Ctrl Pts',(5.33194007545457,-4.16685781276029,
126.486028282011));
#214323=CARTESIAN_POINT('Ctrl Pts',(5.44647226944242,-4.02030162522171,
126.494777495752));
#214324=CARTESIAN_POINT('Ctrl Pts',(5.55495848627867,-3.86902074888287,
126.503526709493));
#214325=CARTESIAN_POINT('Ctrl Pts',(5.6570302729154,-3.71352898081041,126.512275923234));
#214326=CARTESIAN_POINT('Ctrl Pts',(5.75910135376751,-3.55803828789986,
126.521025076478));
#214327=CARTESIAN_POINT('Ctrl Pts',(5.85475793592509,-3.3983370010713,126.529774229722));
#214328=CARTESIAN_POINT('Ctrl Pts',(5.9436751442716,-3.23496750823992,126.538523382966));
#214329=CARTESIAN_POINT('Ctrl Pts',(6.03259176732412,-3.07159909078173,
126.547272478619));
#214330=CARTESIAN_POINT('Ctrl Pts',(6.11476896835707,-2.90456276731891,
126.556021574272));
#214331=CARTESIAN_POINT('Ctrl Pts',(6.18992765547681,-2.73442583003515,
126.564770669925));
#214332=CARTESIAN_POINT('Ctrl Pts',(6.26508587282854,-2.56428995616658,
126.573519710893));
#214333=CARTESIAN_POINT('Ctrl Pts',(6.33322554826967,-2.39105376935712,
126.582268751861));
#214334=CARTESIAN_POINT('Ctrl Pts',(6.39411526732846,-2.21530561054613,
126.591017792829));
#214335=CARTESIAN_POINT('Ctrl Pts',(6.45500462602674,-2.03955849185645,
126.599766782018));
#214336=CARTESIAN_POINT('Ctrl Pts',(6.5086440204058,-1.86129970165104,126.608515771207));
#214337=CARTESIAN_POINT('Ctrl Pts',(6.55485128368454,-1.68113463136631,
126.617264760396));
#214338=CARTESIAN_POINT('Ctrl Pts',(6.60199809554197,-1.49730620117442,
126.626191645867));
#214339=CARTESIAN_POINT('Ctrl Pts',(6.6414072070776,-1.31149343246271,126.635118531339));
#214340=CARTESIAN_POINT('Ctrl Pts',(6.67293928722787,-1.12435326698098,
126.64404541681));
#214341=CARTESIAN_POINT('Ctrl Pts',(6.70384625876176,-0.94092306701236,
126.652795330987));
#214342=CARTESIAN_POINT('Ctrl Pts',(6.72718554579731,-0.75621789952748,
126.661545245165));
#214343=CARTESIAN_POINT('Ctrl Pts',(6.74287786815278,-0.570865181260349,
126.670295159342));
#214344=CARTESIAN_POINT('Ctrl Pts',(6.75856988190812,-0.385516108079882,
126.679044901447));
#214345=CARTESIAN_POINT('Ctrl Pts',(6.76661520773385,-0.19951979523236,
126.687794643551));
#214346=CARTESIAN_POINT('Ctrl Pts',(6.76698651789578,-0.0135080204617305,
126.696544385656));
#214347=CARTESIAN_POINT('Ctrl Pts',(6.76735782124918,0.172500343506936,
126.705293967321));
#214348=CARTESIAN_POINT('Ctrl Pts',(6.76005538995215,0.358523882204961,
126.714043548986));
#214349=CARTESIAN_POINT('Ctrl Pts',(6.74510402742409,0.543930748558488,
126.722793130651));
#214350=CARTESIAN_POINT('Ctrl Pts',(6.73015291918094,0.729334461609357,
126.731542563507));
#214351=CARTESIAN_POINT('Ctrl Pts',(6.70755316306675,0.91412123762882,126.740291996364));
#214352=CARTESIAN_POINT('Ctrl Pts',(6.6773815187467,1.09766345165538,126.749041429221));
#214353=CARTESIAN_POINT('Ctrl Pts',(6.64721034747681,1.28120278799083,126.757790724898));
#214354=CARTESIAN_POINT('Ctrl Pts',(6.6094675720527,1.46349731859751,126.766540020576));
#214355=CARTESIAN_POINT('Ctrl Pts',(6.56428138111666,1.64392790277588,126.775289316253));
#214356=CARTESIAN_POINT('Ctrl Pts',(6.5190958386001,1.82435589778482,126.784038486379));
#214357=CARTESIAN_POINT('Ctrl Pts',(6.46646716393053,2.00291972191692,126.792787656505));
#214358=CARTESIAN_POINT('Ctrl Pts',(6.40657409873078,2.17901292274092,126.80153682663));
#214359=CARTESIAN_POINT('Ctrl Pts',(6.34668181342287,2.35510383058409,126.810285882829));
#214360=CARTESIAN_POINT('Ctrl Pts',(6.27952541914277,2.52872390822016,126.819034939028));
#214361=CARTESIAN_POINT('Ctrl Pts',(6.2053329917576,2.69928350889726,126.827783995228));
#214362=CARTESIAN_POINT('Ctrl Pts',(6.12831602991799,2.87633637965092,126.836866131386));
#214363=CARTESIAN_POINT('Ctrl Pts',(6.04371690605525,3.05009086600959,126.845948267544));
#214364=CARTESIAN_POINT('Ctrl Pts',(5.95184520316888,3.21991112882259,126.855030403702));
#214365=CARTESIAN_POINT('Ctrl Pts',(5.86333549509543,3.38351691182551,126.863780184046));
#214366=CARTESIAN_POINT('Ctrl Pts',(5.76807618099648,3.54347103711549,126.872529964389));
#214367=CARTESIAN_POINT('Ctrl Pts',(5.66639083309306,3.69923018027251,126.881279744733));
#214368=CARTESIAN_POINT('Ctrl Pts',(5.56470914082492,3.85498372381629,126.890029210518));
#214369=CARTESIAN_POINT('Ctrl Pts',(5.45660203372359,4.006542347016,126.898778676303));
#214370=CARTESIAN_POINT('Ctrl Pts',(5.34243669839508,4.15339127986294,126.907528142088));
#214371=CARTESIAN_POINT('Ctrl Pts',(5.22827486050887,4.3002357140092,126.916277339834));
#214372=CARTESIAN_POINT('Ctrl Pts',(5.10805534167411,4.44237052028125,126.92502653758));
#214373=CARTESIAN_POINT('Ctrl Pts',(4.98218644340254,4.57931296628392,126.933775735326));
#214374=CARTESIAN_POINT('Ctrl Pts',(4.85632073219887,4.71625194483052,126.942524711537));
#214375=CARTESIAN_POINT('Ctrl Pts',(4.72480612170616,4.84799861524219,126.951273687749));
#214376=CARTESIAN_POINT('Ctrl Pts',(4.58808925235604,4.97410554898215,126.960022663961));
#214377=CARTESIAN_POINT('Ctrl Pts',(4.45136349474351,5.10022068120942,126.968772208962));
#214378=CARTESIAN_POINT('Ctrl Pts',(4.30943501210393,5.22069514871576,126.977521753964));
#214379=CARTESIAN_POINT('Ctrl Pts',(4.16278587432105,5.33511975166005,126.986271298966));
#214380=CARTESIAN_POINT('Ctrl Pts',(4.01614535740752,5.44953762807619,126.995020329619));
#214381=CARTESIAN_POINT('Ctrl Pts',(3.86478496658208,5.55790617532587,127.003769360273));
#214382=CARTESIAN_POINT('Ctrl Pts',(3.70921874747458,5.65985735539184,127.012518390927));
#214383=CARTESIAN_POINT('Ctrl Pts',(3.55365041606172,5.76180991976879,127.021267540377));
#214384=CARTESIAN_POINT('Ctrl Pts',(3.39387638174803,5.8573447855265,127.030016689826));
#214385=CARTESIAN_POINT('Ctrl Pts',(3.23043927904829,5.94613749121074,127.038765839276));
#214386=CARTESIAN_POINT('Ctrl Pts',(3.18691767070625,5.96978206944044,127.041095647192));
#214387=CARTESIAN_POINT('Ctrl Pts',(3.1431364591973,5.99294880633374,127.043425455108));
#214388=CARTESIAN_POINT('Ctrl Pts',(3.09910619832142,6.01563211736936,127.045755263024));
#214389=CARTESIAN_POINT('Ctrl Pts',(3.09910619832122,6.01563211736946,125.045920265688));
#214390=CARTESIAN_POINT('Ctrl Pts',(2.93605669788026,6.09963122296482,125.054548849515));
#214391=CARTESIAN_POINT('Ctrl Pts',(2.76950882349665,6.17703933309001,125.063177433343));
#214392=CARTESIAN_POINT('Ctrl Pts',(2.60001145328852,6.24757788609062,125.071806017171));
#214393=CARTESIAN_POINT('Ctrl Pts',(2.42685102922923,6.31964086698003,125.080621075675));
#214394=CARTESIAN_POINT('Ctrl Pts',(2.25061244904093,6.38453382912852,125.089436134179));
#214395=CARTESIAN_POINT('Ctrl Pts',(2.07190576960204,6.4420102050439,125.098251192682));
#214396=CARTESIAN_POINT('Ctrl Pts',(1.89319909016315,6.49948658095929,125.107066251186));
#214397=CARTESIAN_POINT('Ctrl Pts',(1.71202462495059,6.54954623780946,125.11588130969));
#214398=CARTESIAN_POINT('Ctrl Pts',(1.52901294840764,6.59199578303884,125.124696368194));
#214399=CARTESIAN_POINT('Ctrl Pts',(1.35410028661987,6.63256676237746,125.133121324327));
#214400=CARTESIAN_POINT('Ctrl Pts',(1.17758614510552,6.66616847679302,125.14154628046));
#214401=CARTESIAN_POINT('Ctrl Pts',(1.00005148439541,6.69269646917881,125.149971236594));
#214402=CARTESIAN_POINT('Ctrl Pts',(0.822475616185957,6.71923061896634,
125.15839814824));
#214403=CARTESIAN_POINT('Ctrl Pts',(0.643879084457784,6.73868772405462,
125.166825059886));
#214404=CARTESIAN_POINT('Ctrl Pts',(0.464849602483791,6.75101502346652,
125.175251971533));
#214405=CARTESIAN_POINT('Ctrl Pts',(0.285754284396154,6.76334685610656,
125.183681982083));
#214406=CARTESIAN_POINT('Ctrl Pts',(0.106226029271025,6.76854363246676,
125.192111992633));
#214407=CARTESIAN_POINT('Ctrl Pts',(-0.0731454130554328,6.76660466914899,
125.200542003183));
#214408=CARTESIAN_POINT('Ctrl Pts',(-0.252682088603254,6.76466391969877,
125.208979779282));
#214409=CARTESIAN_POINT('Ctrl Pts',(-0.432061330928625,6.75557430129622,
125.217417555382));
#214410=CARTESIAN_POINT('Ctrl Pts',(-0.610695349609868,6.739387226593,125.225855331481));
#214411=CARTESIAN_POINT('Ctrl Pts',(-0.789423137983143,6.72319165486878,
125.234297536791));
#214412=CARTESIAN_POINT('Ctrl Pts',(-0.967404593380288,6.69989123416269,
125.242739742101));
#214413=CARTESIAN_POINT('Ctrl Pts',(-1.14405953544785,6.66958895130359,
125.251181947411));
#214414=CARTESIAN_POINT('Ctrl Pts',(-1.32090083875935,6.63925470120336,
125.259633058783));
#214415=CARTESIAN_POINT('Ctrl Pts',(-1.49641250818432,6.60190389730576,
125.268084170155));
#214416=CARTESIAN_POINT('Ctrl Pts',(-1.67002593990945,6.55769032205925,
125.276535281527));
#214417=CARTESIAN_POINT('Ctrl Pts',(-1.7187508184487,6.5452817136799,125.278907099024));
#214418=CARTESIAN_POINT('Ctrl Pts',(-1.76732627885295,6.53233285720752,
125.281278916522));
#214419=CARTESIAN_POINT('Ctrl Pts',(-1.81573999407381,6.51884784865553,
125.283650734019));
#214420=CARTESIAN_POINT('Ctrl Pts',(-1.98549236513071,6.47156554104953,
125.291967006423));
#214421=CARTESIAN_POINT('Ctrl Pts',(-2.15356128852685,6.41760263709694,
125.300283278827));
#214422=CARTESIAN_POINT('Ctrl Pts',(-2.31939289326421,6.35709883568562,
125.308599551231));
#214423=CARTESIAN_POINT('Ctrl Pts',(-2.48508428718448,6.29664619030965,
125.316908792217));
#214424=CARTESIAN_POINT('Ctrl Pts',(-2.64854180610319,6.22966378459738,
125.325218033203));
#214425=CARTESIAN_POINT('Ctrl Pts',(-2.80922592743371,6.15634133951605,
125.333527274189));
#214426=CARTESIAN_POINT('Ctrl Pts',(-2.96980365100676,6.0830674452415,125.341831013172));
#214427=CARTESIAN_POINT('Ctrl Pts',(-3.1276113207775,6.00346202071407,125.350134752154));
#214428=CARTESIAN_POINT('Ctrl Pts',(-3.2821284124593,5.91776326698926,125.358438491137));
#214429=CARTESIAN_POINT('Ctrl Pts',(-3.43657150746257,5.83210555353424,
125.366738253542));
#214430=CARTESIAN_POINT('Ctrl Pts',(-3.58772686117721,5.74036049461802,
125.375038015948));
#214431=CARTESIAN_POINT('Ctrl Pts',(-3.7350974286931,5.64281279134531,125.383337778353));
#214432=CARTESIAN_POINT('Ctrl Pts',(-3.88242442066472,5.54529393164925,
125.391635086628));
#214433=CARTESIAN_POINT('Ctrl Pts',(-4.0259685673482,5.44197603942589,125.399932394903));
#214434=CARTESIAN_POINT('Ctrl Pts',(-4.16526057425219,5.33318791611362,
125.408229703177));
#214435=CARTESIAN_POINT('Ctrl Pts',(-4.30456665459266,5.22438880133976,
125.416527849774));
#214436=CARTESIAN_POINT('Ctrl Pts',(-4.4396194578643,5.11011855933301,125.424825996372));
#214437=CARTESIAN_POINT('Ctrl Pts',(-4.56998118497756,4.99074753608627,
125.433124142969));
#214438=CARTESIAN_POINT('Ctrl Pts',(-4.70035602078258,4.87136450933218,
125.441423123997));
#214439=CARTESIAN_POINT('Ctrl Pts',(-4.82603858307134,4.74687991369302,
125.449722105025));
#214440=CARTESIAN_POINT('Ctrl Pts',(-4.94662657602122,4.61770229848142,
125.458021086053));
#214441=CARTESIAN_POINT('Ctrl Pts',(-5.06724673521217,4.48849022579018,
125.466322280793));
#214442=CARTESIAN_POINT('Ctrl Pts',(-5.18276937903411,4.3545828929151,125.474623475532));
#214443=CARTESIAN_POINT('Ctrl Pts',(-5.29283115991687,4.21642352149462,
125.482924670272));
#214444=CARTESIAN_POINT('Ctrl Pts',(-5.40294059240145,4.07820433353017,
125.49122945904));
#214445=CARTESIAN_POINT('Ctrl Pts',(-5.50758423316813,3.93572971005687,
125.499534247809));
#214446=CARTESIAN_POINT('Ctrl Pts',(-5.60644076926536,3.78947369706128,
125.507839036577));
#214447=CARTESIAN_POINT('Ctrl Pts',(-5.7054144988983,3.6430442988758,125.516153670598));
#214448=CARTESIAN_POINT('Ctrl Pts',(-5.79858722147323,3.49282484324007,
125.524468304619));
#214449=CARTESIAN_POINT('Ctrl Pts',(-5.88568188424686,3.33931695971622,
125.53278293864));
#214450=CARTESIAN_POINT('Ctrl Pts',(-5.97283161774779,3.18571201179689,
125.541102830078));
#214451=CARTESIAN_POINT('Ctrl Pts',(-6.0538954676157,3.02881479809379,125.549422721516));
#214452=CARTESIAN_POINT('Ctrl Pts',(-6.12864359904791,2.86914911356121,
125.557742612954));
#214453=CARTESIAN_POINT('Ctrl Pts',(-6.20350350317373,2.70924467705857,
125.566074945327));
#214454=CARTESIAN_POINT('Ctrl Pts',(-6.27202868001501,2.54656381702103,
125.5744072777));
#214455=CARTESIAN_POINT('Ctrl Pts',(-6.33403796063636,2.38164903233401,
125.582739610073));
#214456=CARTESIAN_POINT('Ctrl Pts',(-6.38072379659001,2.25748722127797,
125.589012895272));
#214457=CARTESIAN_POINT('Ctrl Pts',(-6.42371720929835,2.1320595120651,125.59528618047));
#214458=CARTESIAN_POINT('Ctrl Pts',(-6.46295988947719,2.00560177179044,
125.601559465669));
#214459=CARTESIAN_POINT('Ctrl Pts',(-6.52335173577858,1.81099181193342,
125.611213629803));
#214460=CARTESIAN_POINT('Ctrl Pts',(-6.57501402000094,1.61344508945547,
125.620867793937));
#214461=CARTESIAN_POINT('Ctrl Pts',(-6.61768735554798,1.41368421658462,
125.630521958071));
#214462=CARTESIAN_POINT('Ctrl Pts',(-6.66011135209951,1.21509054038926,
125.640119713219));
#214463=CARTESIAN_POINT('Ctrl Pts',(-6.69365104287442,1.01430857789511,
125.649717468367));
#214464=CARTESIAN_POINT('Ctrl Pts',(-6.71809703750268,0.812072161016336,
125.659315223515));
#214465=CARTESIAN_POINT('Ctrl Pts',(-6.74230300623966,0.611821426330077,
125.668818741968));
#214466=CARTESIAN_POINT('Ctrl Pts',(-6.75759289335629,0.410144744707065,
125.678322260422));
#214467=CARTESIAN_POINT('Ctrl Pts',(-6.76380941444879,0.20777681539077,
125.687825778875));
#214468=CARTESIAN_POINT('Ctrl Pts',(-6.76584898780119,0.141382085947639,
125.69094378052));
#214469=CARTESIAN_POINT('Ctrl Pts',(-6.76691225805108,0.0749131229981565,
125.694061782165));
#214470=CARTESIAN_POINT('Ctrl Pts',(-6.76699479095664,0.00839637813163948,
125.69717978381));
#214471=CARTESIAN_POINT('',(-6.767,8.80633884406398E-10,125.302820216149));
#214472=CARTESIAN_POINT('Ctrl Pts',(3.09910619832142,6.01563211736936,124.651395695404));
#214473=CARTESIAN_POINT('Ctrl Pts',(2.93375330764834,6.10081787314649,124.660145143307));
#214474=CARTESIAN_POINT('Ctrl Pts',(2.76488627843078,6.17918207037036,124.668894591209));
#214475=CARTESIAN_POINT('Ctrl Pts',(2.5930786664671,6.25045854553994,124.677644039111));
#214476=CARTESIAN_POINT('Ctrl Pts',(2.42127244185391,6.32173444515031,124.686393416362));
#214477=CARTESIAN_POINT('Ctrl Pts',(2.24652594672486,6.38592262741831,124.695142793612));
#214478=CARTESIAN_POINT('Ctrl Pts',(2.06943269687149,6.44280508110553,124.703892170862));
#214479=CARTESIAN_POINT('Ctrl Pts',(1.89234081822105,6.49968709436158,124.712641480368));
#214480=CARTESIAN_POINT('Ctrl Pts',(1.71290249405618,6.54926340459537,124.721390789873));
#214481=CARTESIAN_POINT('Ctrl Pts',(1.53172716625088,6.59136563150377,124.730140099378));
#214482=CARTESIAN_POINT('Ctrl Pts',(1.35055318107369,6.63346754640703,124.738889344045));
#214483=CARTESIAN_POINT('Ctrl Pts',(1.16764249714459,6.66809542395769,124.747638588713));
#214484=CARTESIAN_POINT('Ctrl Pts',(0.983616340614793,6.69513165624662,
124.75638783338));
#214485=CARTESIAN_POINT('Ctrl Pts',(0.79959148671428,6.72216769715956,124.765137016116));
#214486=CARTESIAN_POINT('Ctrl Pts',(0.61445145952715,6.74161215869367,124.773886198851));
#214487=CARTESIAN_POINT('Ctrl Pts',(0.428825047910721,6.75339900185709,
124.782635381587));
#214488=CARTESIAN_POINT('Ctrl Pts',(0.243199888597392,6.7651857655022,124.791384505298));
#214489=CARTESIAN_POINT('Ctrl Pts',(0.0570886373921694,6.76931499599834,
124.800133629008));
#214490=CARTESIAN_POINT('Ctrl Pts',(-0.12887662681099,6.76577266947847,
124.808882752719));
#214491=CARTESIAN_POINT('Ctrl Pts',(-0.314840698187942,6.76223036567994,
124.81763182031));
#214492=CARTESIAN_POINT('Ctrl Pts',(-0.500658497950979,6.75101660879225,
124.826380887902));
#214493=CARTESIAN_POINT('Ctrl Pts',(-0.685698951925887,6.73216948296222,
124.835129955493));
#214494=CARTESIAN_POINT('Ctrl Pts',(-0.87073828045956,6.71332247176297,
124.843878969872));
#214495=CARTESIAN_POINT('Ctrl Pts',(-1.05499998761225,6.68684221356191,
124.85262798425));
#214496=CARTESIAN_POINT('Ctrl Pts',(-1.23785829161398,6.65281863948526,
124.861376998629));
#214497=CARTESIAN_POINT('Ctrl Pts',(-1.43007412915576,6.61705395369202,
124.870573732327));
#214498=CARTESIAN_POINT('Ctrl Pts',(-1.62073882532187,6.57295372728624,
124.879770466026));
#214499=CARTESIAN_POINT('Ctrl Pts',(-1.80913696086181,6.52068343479759,
124.888967199724));
#214500=CARTESIAN_POINT('Ctrl Pts',(-1.9883835618082,6.47095219816825,124.897717197438));
#214501=CARTESIAN_POINT('Ctrl Pts',(-2.16557827567288,6.41382586852662,
124.906467195151));
#214502=CARTESIAN_POINT('Ctrl Pts',(-2.34011918616508,6.34949849945192,
124.915217192865));
#214503=CARTESIAN_POINT('Ctrl Pts',(-2.51465655685964,6.28517243497605,
124.923967013123));
#214504=CARTESIAN_POINT('Ctrl Pts',(-2.68653996290258,6.21364572244567,
124.932716833381));
#214505=CARTESIAN_POINT('Ctrl Pts',(-2.85518555374987,6.13516132254548,
124.94146665364));
#214506=CARTESIAN_POINT('Ctrl Pts',(-3.02382794853742,6.05667841002976,
124.950216308077));
#214507=CARTESIAN_POINT('Ctrl Pts',(-3.18923239104394,5.97123819494691,
124.958965962515));
#214508=CARTESIAN_POINT('Ctrl Pts',(-3.35083705962877,5.87913088813461,
124.967715616952));
#214509=CARTESIAN_POINT('Ctrl Pts',(-3.51243888037639,5.78702520445992,
124.976465117201));
#214510=CARTESIAN_POINT('Ctrl Pts',(-3.67024081218995,5.68825280608812,
124.98521461745));
#214511=CARTESIAN_POINT('Ctrl Pts',(-3.82370687539778,5.58314917685671,
124.993964117699));
#214512=CARTESIAN_POINT('Ctrl Pts',(-3.97717043813265,5.47804726011324,
125.00271347539));
#214513=CARTESIAN_POINT('Ctrl Pts',(-4.1262980371799,5.36661448087672,125.01146283308));
#214514=CARTESIAN_POINT('Ctrl Pts',(-4.27058317202522,5.24922931208144,
125.020212190771));
#214515=CARTESIAN_POINT('Ctrl Pts',(-4.41486614770552,5.13184589990476,
125.028961417531));
#214516=CARTESIAN_POINT('Ctrl Pts',(-4.55430658190237,5.00851045726832,
125.037710644291));
#214517=CARTESIAN_POINT('Ctrl Pts',(-4.6884308899778,4.87964187107025,125.046459871051));
#214518=CARTESIAN_POINT('Ctrl Pts',(-4.82255336913904,4.75077504211953,
125.055208978507));
#214519=CARTESIAN_POINT('Ctrl Pts',(-4.95135966061338,4.61637541912167,
125.063958085963));
#214520=CARTESIAN_POINT('Ctrl Pts',(-5.07441230865585,4.47689945405992,
125.072707193419));
#214521=CARTESIAN_POINT('Ctrl Pts',(-5.19746344222887,4.33742520559747,
125.081456193195));
#214522=CARTESIAN_POINT('Ctrl Pts',(-5.31476088451368,4.19287495495646,
125.090205192971));
#214523=CARTESIAN_POINT('Ctrl Pts',(-5.42590627625588,4.04373961591088,
125.098954192748));
#214524=CARTESIAN_POINT('Ctrl Pts',(-5.53706380669524,3.89458798911204,
125.107704148042));
#214525=CARTESIAN_POINT('Ctrl Pts',(-5.64206777068846,3.74085050159836,
125.116454103337));
#214526=CARTESIAN_POINT('Ctrl Pts',(-5.74056148161118,3.5830493822779,125.125204058632));
#214527=CARTESIAN_POINT('Ctrl Pts',(-5.83905138949125,3.42525435597985,
125.133953676073));
#214528=CARTESIAN_POINT('Ctrl Pts',(-5.93103139555028,3.26339625501955,
125.142703293514));
#214529=CARTESIAN_POINT('Ctrl Pts',(-6.01618907818357,3.09802485069838,
125.151452910955));
#214530=CARTESIAN_POINT('Ctrl Pts',(-6.10134392542622,2.93265895254553,
125.160202237071));
#214531=CARTESIAN_POINT('Ctrl Pts',(-6.17967677259601,2.76378023991022,
125.168951563187));
#214532=CARTESIAN_POINT('Ctrl Pts',(-6.25092157007128,2.59196229232171,
125.177700889303));
#214533=CARTESIAN_POINT('Ctrl Pts',(-6.32216437405813,2.42014915234164,
125.186449970605));
#214534=CARTESIAN_POINT('Ctrl Pts',(-6.38631941547135,2.24539720667934,
125.195199051908));
#214535=CARTESIAN_POINT('Ctrl Pts',(-6.44316881035905,2.06829994952773,
125.20394813321));
#214536=CARTESIAN_POINT('Ctrl Pts',(-6.50002334523081,1.89118668029575,
125.212698005552));
#214537=CARTESIAN_POINT('Ctrl Pts',(-6.54957082409748,1.7117279481286,125.221447877895));
#214538=CARTESIAN_POINT('Ctrl Pts',(-6.5916429429488,1.53053334255523,125.230197750237));
#214539=CARTESIAN_POINT('Ctrl Pts',(-6.63371214081076,1.34935131698802,
125.238947015092));
#214540=CARTESIAN_POINT('Ctrl Pts',(-6.66830695238778,1.1664339383498,125.247696279947));
#214541=CARTESIAN_POINT('Ctrl Pts',(-6.69530988153222,0.982402458393223,
125.256445544802));
#214542=CARTESIAN_POINT('Ctrl Pts',(-6.7223141968986,0.798361530999515,
125.265195258809));
#214543=CARTESIAN_POINT('Ctrl Pts',(-6.74172580828799,0.613206671415098,
125.273944972816));
#214544=CARTESIAN_POINT('Ctrl Pts',(-6.75347878027846,0.427566795166124,
125.282694686823));
#214545=CARTESIAN_POINT('Ctrl Pts',(-6.76248992366252,0.285234494532973,
125.289403196598));
#214546=CARTESIAN_POINT('Ctrl Pts',(-6.76699999998144,0.142617266695871,
125.296111706374));
#214547=CARTESIAN_POINT('Ctrl Pts',(-6.767,8.80634713124887E-10,125.302820216149));
#214548=CARTESIAN_POINT('Ctrl Pts',(-6.767,6.68686382847748E-12,125.30282021619));
#214549=CARTESIAN_POINT('Ctrl Pts',(-6.76700000000019,-0.186007249520308,
125.311569728001));
#214550=CARTESIAN_POINT('Ctrl Pts',(-6.75932637294556,-0.372014355743486,
125.320319239812));
#214551=CARTESIAN_POINT('Ctrl Pts',(-6.74400518264232,-0.557389537481198,
125.329068751624));
#214552=CARTESIAN_POINT('Ctrl Pts',(-6.72868405705154,-0.742763936245582,
125.337818226479));
#214553=CARTESIAN_POINT('Ctrl Pts',(-6.7057154564581,-0.927506130236142,
125.346567701335));
#214554=CARTESIAN_POINT('Ctrl Pts',(-6.67517739404902,-1.11098863989558,
125.355317176191));
#214555=CARTESIAN_POINT('Ctrl Pts',(-6.64463945808789,-1.29447038981501,
125.364066614818));
#214556=CARTESIAN_POINT('Ctrl Pts',(-6.60653217008452,-1.47669218313251,
125.372816053445));
#214557=CARTESIAN_POINT('Ctrl Pts',(-6.56098496092783,-1.65703510598866,
125.381565492072));
#214558=CARTESIAN_POINT('Ctrl Pts',(-6.51543793658414,-1.83737729708282,
125.390314895197));
#214559=CARTESIAN_POINT('Ctrl Pts',(-6.4624511216755,-2.0158403551051,125.399064298322));
#214560=CARTESIAN_POINT('Ctrl Pts',(-6.40220448374395,-2.19181813760377,
125.407813701447));
#214561=CARTESIAN_POINT('Ctrl Pts',(-6.34195808526654,-2.36779522066742,
125.416563069797));
#214562=CARTESIAN_POINT('Ctrl Pts',(-6.27445201433262,-2.54128677683776,
125.425312438147));
#214563=CARTESIAN_POINT('Ctrl Pts',(-6.19991555072066,-2.71170355384435,
125.434061806497));
#214564=CARTESIAN_POINT('Ctrl Pts',(-6.12537937716873,-2.88211966767093,
125.442811140799));
#214565=CARTESIAN_POINT('Ctrl Pts',(-6.04381298052717,-3.04946076371394,
125.451560475101));
#214566=CARTESIAN_POINT('Ctrl Pts',(-5.95549339336046,-3.21315848374149,
125.460309809403));
#214567=CARTESIAN_POINT('Ctrl Pts',(-5.8671741425563,-3.37685558033108,
125.469059110383));
#214568=CARTESIAN_POINT('Ctrl Pts',(-5.77210188876825,-3.53690907646386,
125.477808411363));
#214569=CARTESIAN_POINT('Ctrl Pts',(-5.67059953347228,-3.6927753696893,
125.486557712343));
#214570=CARTESIAN_POINT('Ctrl Pts',(-5.56909755631612,-3.84864108224595,
125.495306980729));
#214571=CARTESIAN_POINT('Ctrl Pts',(-5.46116568197072,-4.00031938297215,
125.504056249114));
#214572=CARTESIAN_POINT('Ctrl Pts',(-5.34717048533817,-4.14729511859578,
125.512805517499));
#214573=CARTESIAN_POINT('Ctrl Pts',(-5.23317570392063,-4.2942703188764,
125.521554754016));
#214574=CARTESIAN_POINT('Ctrl Pts',(-5.11311782003753,-4.43654276189272,
125.530303990533));
#214575=CARTESIAN_POINT('Ctrl Pts',(-4.98740458985004,-4.57362924351579,
125.53905322705));
#214576=CARTESIAN_POINT('Ctrl Pts',(-4.86169180712014,-4.71071523719986,
125.547802432426));
#214577=CARTESIAN_POINT('Ctrl Pts',(-4.73032391204464,-4.84261509522952,
125.556551637801));
#214578=CARTESIAN_POINT('Ctrl Pts',(-4.59374707013913,-4.96888084538039,
125.565300843177));
#214579=CARTESIAN_POINT('Ctrl Pts',(-4.45717070301761,-5.09514615659187,
125.574050018137));
#214580=CARTESIAN_POINT('Ctrl Pts',(-4.31538563571359,-5.21577720459265,
125.582799193098));
#214581=CARTESIAN_POINT('Ctrl Pts',(-4.16887341029828,-5.33036429232637,
125.591548368058));
#214582=CARTESIAN_POINT('Ctrl Pts',(-4.02236168204043,-5.44495099123366,
125.60029751333));
#214583=CARTESIAN_POINT('Ctrl Pts',(-3.87112305348521,-5.55349359438353,
125.609046658602));
#214584=CARTESIAN_POINT('Ctrl Pts',(-3.71567117018136,-5.65562346298648,
125.617795803874));
#214585=CARTESIAN_POINT('Ctrl Pts',(-3.56021980146199,-5.75775299351409,
125.626544920184));
#214586=CARTESIAN_POINT('Ctrl Pts',(-3.40055544538734,-5.85346967463649,
125.635294036494));
#214587=CARTESIAN_POINT('Ctrl Pts',(-3.23722035987243,-5.94244842986689,
125.644043152805));
#214588=CARTESIAN_POINT('Ctrl Pts',(-3.07388580147592,-6.03142689794318,
125.652792240879));
#214589=CARTESIAN_POINT('Ctrl Pts',(-2.90688078897012,-6.11366734656575,
125.661541328954));
#214590=CARTESIAN_POINT('Ctrl Pts',(-2.73677250721827,-6.18889046952152,
125.670290417029));
#214591=CARTESIAN_POINT('Ctrl Pts',(-2.56666476031899,-6.26411335596158,
125.679039477595));
#214592=CARTESIAN_POINT('Ctrl Pts',(-2.3934540257554,-6.33231884500416,
125.687788538161));
#214593=CARTESIAN_POINT('Ctrl Pts',(-2.21772856065922,-6.39327529762612,
125.696537598727));
#214594=CARTESIAN_POINT('Ctrl Pts',(-2.04200363348842,-6.45423156365007,
125.705286632511));
#214595=CARTESIAN_POINT('Ctrl Pts',(-1.86376426189605,-6.50793874375565,
125.714035666295));
#214596=CARTESIAN_POINT('Ctrl Pts',(-1.68361577753478,-6.55421443909459,
125.722784700078));
#214597=CARTESIAN_POINT('Ctrl Pts',(-1.50346782968151,-6.60048999661787,
125.731533707806));
#214598=CARTESIAN_POINT('Ctrl Pts',(-1.32141105795366,-6.63933404237636,
125.740282715534));
#214599=CARTESIAN_POINT('Ctrl Pts',(-1.13806375487428,-6.67061465607492,
125.749031723262));
#214600=CARTESIAN_POINT('Ctrl Pts',(-0.954716982607099,-6.70189517921238,
125.75778070566));
#214601=CARTESIAN_POINT('Ctrl Pts',(-0.77007996890624,-6.72561226592181,
125.766529688059));
#214602=CARTESIAN_POINT('Ctrl Pts',(-0.584779765562359,-6.74168536983067,
125.775278670457));
#214603=CARTESIAN_POINT('Ctrl Pts',(-0.391489830655416,-6.75845151013829,
125.784404889467));
#214604=CARTESIAN_POINT('Ctrl Pts',(-0.197478578242453,-6.76689983031613,
125.793531108477));
#214605=CARTESIAN_POINT('Ctrl Pts',(-0.0034628764554554,-6.76699911397117,
125.802657327487));
#214606=CARTESIAN_POINT('Ctrl Pts',(0.184489834650666,-6.767095295012,125.811498352152));
#214607=CARTESIAN_POINT('Ctrl Pts',(0.372446404246149,-6.75935639738186,
125.820339376818));
#214608=CARTESIAN_POINT('Ctrl Pts',(0.559755019485118,-6.74380925873213,
125.829180401484));
#214609=CARTESIAN_POINT('Ctrl Pts',(0.74513470551855,-6.72842222659841,
125.837930380094));
#214610=CARTESIAN_POINT('Ctrl Pts',(0.929879431225341,-6.70538706057568,
125.846680358703));
#214611=CARTESIAN_POINT('Ctrl Pts',(1.11336163626503,-6.67478200894181,
125.855430337313));
#214612=CARTESIAN_POINT('Ctrl Pts',(1.29684196300417,-6.64417727061072,
125.86418022635));
#214613=CARTESIAN_POINT('Ctrl Pts',(1.4790595121723,-6.60600284890654,125.872930115386));
#214614=CARTESIAN_POINT('Ctrl Pts',(1.65939532066825,-6.56038841607296,
125.881680004423));
#214615=CARTESIAN_POINT('Ctrl Pts',(1.83972934300547,-6.51477443503329,
125.890429806795));
#214616=CARTESIAN_POINT('Ctrl Pts',(2.01818138406014,-6.46172066062219,
125.899179609167));
#214617=CARTESIAN_POINT('Ctrl Pts',(2.19414528353954,-6.40140730423563,
125.907929411539));
#214618=CARTESIAN_POINT('Ctrl Pts',(2.37010749863758,-6.34109452518732,
125.916679130156));
#214619=CARTESIAN_POINT('Ctrl Pts',(2.54358134866223,-6.273522396166,125.925428848772));
#214620=CARTESIAN_POINT('Ctrl Pts',(2.71397759435323,-6.1989204396692,125.934178567388));
#214621=CARTESIAN_POINT('Ctrl Pts',(2.88437226557891,-6.12431917249625,
125.942928205157));
#214622=CARTESIAN_POINT('Ctrl Pts',(3.05168912680723,-6.04268832278916,
125.951677842926));
#214623=CARTESIAN_POINT('Ctrl Pts',(3.21535986273622,-5.9543051612346,125.960427480694));
#214624=CARTESIAN_POINT('Ctrl Pts',(3.3790291407262,-5.86592278697568,125.969177040523));
#214625=CARTESIAN_POINT('Ctrl Pts',(3.53905210621362,-5.77078835742071,
125.977926600353));
#214626=CARTESIAN_POINT('Ctrl Pts',(3.69488522831498,-5.66922500431759,
125.986676160182));
#214627=CARTESIAN_POINT('Ctrl Pts',(3.85071701406762,-5.56766252217217,
125.995425644979));
#214628=CARTESIAN_POINT('Ctrl Pts',(4.00235878822247,-5.45967138329486,
126.004175129776));
#214629=CARTESIAN_POINT('Ctrl Pts',(4.14929549611188,-5.34561838199714,
126.012924614573));
#214630=CARTESIAN_POINT('Ctrl Pts',(4.29623099275953,-5.23156632087128,
126.021674027246));
#214631=CARTESIAN_POINT('Ctrl Pts',(4.43846127435892,-5.11145267305082,
126.030423439918));
#214632=CARTESIAN_POINT('Ctrl Pts',(4.57550326054307,-4.98568540050009,
126.039172852591));
#214633=CARTESIAN_POINT('Ctrl Pts',(4.71254416257657,-4.8599191229048,126.047922196046));
#214634=CARTESIAN_POINT('Ctrl Pts',(4.84439664018649,-4.72849950385534,
126.056671539501));
#214635=CARTESIAN_POINT('Ctrl Pts',(4.97061286794644,-4.59187289861178,
126.065420882956));
#214636=CARTESIAN_POINT('Ctrl Pts',(5.09682813912582,-4.45524732884802,
126.074170160101));
#214637=CARTESIAN_POINT('Ctrl Pts',(5.21740705147736,-4.31341506235912,
126.082919437246));
#214638=CARTESIAN_POINT('Ctrl Pts',(5.33194007545593,-4.16685781275856,
126.091668714391));
#214639=CARTESIAN_POINT('Ctrl Pts',(5.4464722694439,-4.02030162521971,126.100417928132));
#214640=CARTESIAN_POINT('Ctrl Pts',(5.55495848628026,-3.8690207488806,126.109167141873));
#214641=CARTESIAN_POINT('Ctrl Pts',(5.65703027291707,-3.71352898080785,
126.117916355614));
#214642=CARTESIAN_POINT('Ctrl Pts',(5.7591013537692,-3.55803828789713,126.126665508858));
#214643=CARTESIAN_POINT('Ctrl Pts',(5.85475793592679,-3.39833700106839,
126.135414662102));
#214644=CARTESIAN_POINT('Ctrl Pts',(5.94367514427329,-3.23496750823682,
126.144163815346));
#214645=CARTESIAN_POINT('Ctrl Pts',(6.03259176732568,-3.07159909077866,
126.152912910999));
#214646=CARTESIAN_POINT('Ctrl Pts',(6.1147689683585,-2.9045627673159,126.161662006652));
#214647=CARTESIAN_POINT('Ctrl Pts',(6.18992765547811,-2.73442583003219,
126.170411102305));
#214648=CARTESIAN_POINT('Ctrl Pts',(6.26508587282978,-2.56428995616356,
126.179160143273));
#214649=CARTESIAN_POINT('Ctrl Pts',(6.33322554827083,-2.39105376935404,
126.187909184241));
#214650=CARTESIAN_POINT('Ctrl Pts',(6.39411526732955,-2.21530561054298,
126.196658225209));
#214651=CARTESIAN_POINT('Ctrl Pts',(6.45500462602776,-2.03955849185324,
126.205407214398));
#214652=CARTESIAN_POINT('Ctrl Pts',(6.50864402040673,-1.86129970164778,
126.214156203587));
#214653=CARTESIAN_POINT('Ctrl Pts',(6.55485128368539,-1.681134631363,126.222905192776));
#214654=CARTESIAN_POINT('Ctrl Pts',(6.6019980955427,-1.49730620117118,126.231832078247));
#214655=CARTESIAN_POINT('Ctrl Pts',(6.64140720707823,-1.31149343245955,
126.240758963719));
#214656=CARTESIAN_POINT('Ctrl Pts',(6.67293928722839,-1.12435326697789,
126.24968584919));
#214657=CARTESIAN_POINT('Ctrl Pts',(6.70384625876218,-0.940923067009357,
126.258435763368));
#214658=CARTESIAN_POINT('Ctrl Pts',(6.72718554579763,-0.756217899524563,
126.267185677545));
#214659=CARTESIAN_POINT('Ctrl Pts',(6.74287786815302,-0.570865181257524,
126.275935591723));
#214660=CARTESIAN_POINT('Ctrl Pts',(6.75856988190828,-0.38551610807702,
126.284685333827));
#214661=CARTESIAN_POINT('Ctrl Pts',(6.76661520773394,-0.199519795229466,
126.293435075931));
#214662=CARTESIAN_POINT('Ctrl Pts',(6.76698651789578,-0.0135080204588065,
126.302184818036));
#214663=CARTESIAN_POINT('Ctrl Pts',(6.76735782124911,0.172500343509762,
126.310934399701));
#214664=CARTESIAN_POINT('Ctrl Pts',(6.76005538995201,0.358523882207686,
126.319683981366));
#214665=CARTESIAN_POINT('Ctrl Pts',(6.74510402742387,0.543930748561109,
126.328433563031));
#214666=CARTESIAN_POINT('Ctrl Pts',(6.73015291918067,0.729334461611875,
126.337182995888));
#214667=CARTESIAN_POINT('Ctrl Pts',(6.70755316306642,0.914121237631232,
126.345932428744));
#214668=CARTESIAN_POINT('Ctrl Pts',(6.67738151874632,1.09766345165769,126.354681861601));
#214669=CARTESIAN_POINT('Ctrl Pts',(6.64721034747636,1.28120278799316,126.363431157278));
#214670=CARTESIAN_POINT('Ctrl Pts',(6.60946757205218,1.46349731859985,126.372180452956));
#214671=CARTESIAN_POINT('Ctrl Pts',(6.56428138111607,1.64392790277824,126.380929748634));
#214672=CARTESIAN_POINT('Ctrl Pts',(6.51909583859944,1.82435589778719,126.389678918759));
#214673=CARTESIAN_POINT('Ctrl Pts',(6.46646716392979,2.0029197219193,126.398428088885));
#214674=CARTESIAN_POINT('Ctrl Pts',(6.40657409872997,2.17901292274331,126.40717725901));
#214675=CARTESIAN_POINT('Ctrl Pts',(6.34668181342194,2.3551038305866,126.415926315209));
#214676=CARTESIAN_POINT('Ctrl Pts',(6.27952541914172,2.5287239082228,126.424675371409));
#214677=CARTESIAN_POINT('Ctrl Pts',(6.2053329917564,2.69928350890001,126.433424427608));
#214678=CARTESIAN_POINT('Ctrl Pts',(6.12831602991675,2.87633637965354,126.442506563766));
#214679=CARTESIAN_POINT('Ctrl Pts',(6.04371690605398,3.05009086601209,126.451588699924));
#214680=CARTESIAN_POINT('Ctrl Pts',(5.9518452031676,3.21991112882497,126.460670836082));
#214681=CARTESIAN_POINT('Ctrl Pts',(5.86333549509407,3.38351691182788,126.469420616426));
#214682=CARTESIAN_POINT('Ctrl Pts',(5.76807618099504,3.54347103711784,126.478170396769));
#214683=CARTESIAN_POINT('Ctrl Pts',(5.66639083309153,3.69923018027485,126.486920177113));
#214684=CARTESIAN_POINT('Ctrl Pts',(5.56470914082346,3.8549837238184,126.495669642898));
#214685=CARTESIAN_POINT('Ctrl Pts',(5.4566020337222,4.00654234701789,126.504419108683));
#214686=CARTESIAN_POINT('Ctrl Pts',(5.34243669839378,4.15339127986461,126.513168574468));
#214687=CARTESIAN_POINT('Ctrl Pts',(5.22827486050759,4.30023571401076,126.521917772214));
#214688=CARTESIAN_POINT('Ctrl Pts',(5.10805534167284,4.4423705202827,126.53066696996));
#214689=CARTESIAN_POINT('Ctrl Pts',(4.9821864434013,4.57931296628526,126.539416167706));
#214690=CARTESIAN_POINT('Ctrl Pts',(4.85632073219784,4.71625194483157,126.548165143917));
#214691=CARTESIAN_POINT('Ctrl Pts',(4.72480612170535,4.84799861524297,126.556914120129));
#214692=CARTESIAN_POINT('Ctrl Pts',(4.58808925235548,4.97410554898267,126.565663096341));
#214693=CARTESIAN_POINT('Ctrl Pts',(4.45136349474291,5.10022068120994,126.574412641342));
#214694=CARTESIAN_POINT('Ctrl Pts',(4.3094350121033,5.22069514871628,126.583162186344));
#214695=CARTESIAN_POINT('Ctrl Pts',(4.16278587432038,5.33511975166057,126.591911731346));
#214696=CARTESIAN_POINT('Ctrl Pts',(4.01614535740682,5.44953762807671,126.600660761999));
#214697=CARTESIAN_POINT('Ctrl Pts',(3.86478496658133,5.55790617532639,126.609409792653));
#214698=CARTESIAN_POINT('Ctrl Pts',(3.70921874747379,5.65985735539236,126.618158823307));
#214699=CARTESIAN_POINT('Ctrl Pts',(3.5536504160609,5.7618099197693,126.626907972757));
#214700=CARTESIAN_POINT('Ctrl Pts',(3.39387638174717,5.85734478552701,126.635657122206));
#214701=CARTESIAN_POINT('Ctrl Pts',(3.23043927904738,5.94613749121124,126.644406271656));
#214702=CARTESIAN_POINT('Ctrl Pts',(3.18691767070567,5.96978206944075,126.646736079572));
#214703=CARTESIAN_POINT('Ctrl Pts',(3.14313645919705,5.99294880633387,126.649065887488));
#214704=CARTESIAN_POINT('Ctrl Pts',(3.0991061983215,6.01563211736932,126.651395695404));
#214705=CARTESIAN_POINT('Origin',(0.,0.,4.30282021618968));
#214706=CARTESIAN_POINT('',(3.09910619832118,6.01563211736948,129.045766611327));
#214707=CARTESIAN_POINT('',(3.09910619832144,6.01563211736935,128.651395695404));
#214708=CARTESIAN_POINT('',(3.09910619832133,6.0156321173694,4.30282021618968));
#214709=CARTESIAN_POINT('',(-6.76699890687685,-0.00271977263060589,127.69717978381));
#214710=CARTESIAN_POINT('Ctrl Pts',(-6.7669978137537,-0.00543954526750962,
127.69717978381));
#214711=CARTESIAN_POINT('Ctrl Pts',(-6.76683644173397,-0.206192374952252,
127.706596882396));
#214712=CARTESIAN_POINT('Ctrl Pts',(-6.7577377857915,-0.406590498140303,
127.716013980982));
#214713=CARTESIAN_POINT('Ctrl Pts',(-6.73981970767303,-0.60590371187369,
127.725431079567));
#214714=CARTESIAN_POINT('Ctrl Pts',(-6.72175068807275,-0.806895935578124,
127.734927507577));
#214715=CARTESIAN_POINT('Ctrl Pts',(-6.69471310070588,-1.00678476574515,
127.744423935587));
#214716=CARTESIAN_POINT('Ctrl Pts',(-6.65887750139783,-1.20483999824782,
127.753920363597));
#214717=CARTESIAN_POINT('Ctrl Pts',(-6.62290041652562,-1.40367718938511,
127.763454285258));
#214718=CARTESIAN_POINT('Ctrl Pts',(-6.57805580290485,-1.60066616659163,
127.772988206919));
#214719=CARTESIAN_POINT('Ctrl Pts',(-6.52456483723941,-1.79508848936734,
127.782522128581));
#214720=CARTESIAN_POINT('Ctrl Pts',(-6.47083000609436,-1.99039718412006,
127.792099515421));
#214721=CARTESIAN_POINT('Ctrl Pts',(-6.40836987881955,-2.18311565971218,
127.801676902261));
#214722=CARTESIAN_POINT('Ctrl Pts',(-6.33745636754904,-2.3725378372983,
127.811254289101));
#214723=CARTESIAN_POINT('Ctrl Pts',(-6.29879055934802,-2.47582085708316,
127.816476388472));
#214724=CARTESIAN_POINT('Ctrl Pts',(-6.25761237472158,-2.57812428063289,
127.821698487844));
#214725=CARTESIAN_POINT('Ctrl Pts',(-6.21397171263012,-2.67933658852946,
127.826920587215));
#214726=CARTESIAN_POINT('Ctrl Pts',(-6.14653266226067,-2.83574260079252,
127.834990433218));
#214727=CARTESIAN_POINT('Ctrl Pts',(-6.07306002673467,-2.9898895791241,
127.84306027922));
#214728=CARTESIAN_POINT('Ctrl Pts',(-5.99372495262846,-3.14126569908357,
127.851130125223));
#214729=CARTESIAN_POINT('Ctrl Pts',(-5.91448969213646,-3.29245136862991,
127.859189818333));
#214730=CARTESIAN_POINT('Ctrl Pts',(-5.82940683964584,-3.44087278991846,
127.867249511443));
#214731=CARTESIAN_POINT('Ctrl Pts',(-5.73869643029757,-3.58603573335374,
127.875309204553));
#214732=CARTESIAN_POINT('Ctrl Pts',(-5.64808023811702,-3.73104790201592,
127.883360526392));
#214733=CARTESIAN_POINT('Ctrl Pts',(-5.55184831694054,-3.87280801420068,
127.891411848231));
#214734=CARTESIAN_POINT('Ctrl Pts',(-5.45026762102806,-4.01084428258854,
127.899463170069));
#214735=CARTESIAN_POINT('Ctrl Pts',(-5.34877017301097,-4.14876742683674,
127.90750789365));
#214736=CARTESIAN_POINT('Ctrl Pts',(-5.24193289474739,-4.28297250235147,
127.915552617231));
#214737=CARTESIAN_POINT('Ctrl Pts',(-5.13006720173639,-4.41301478647745,
127.923597340812));
#214738=CARTESIAN_POINT('Ctrl Pts',(-5.01826869798149,-4.5429789640446,
127.931637232537));
#214739=CARTESIAN_POINT('Ctrl Pts',(-4.90144803443804,-4.66878504536288,
127.939677124261));
#214740=CARTESIAN_POINT('Ctrl Pts',(-4.77995816745076,-4.7900197199407,
127.947717015986));
#214741=CARTESIAN_POINT('Ctrl Pts',(-4.65585229078337,-4.91386490920691,
127.955930028606));
#214742=CARTESIAN_POINT('Ctrl Pts',(-4.52687408429014,-5.0329392675561,
127.964143041226));
#214743=CARTESIAN_POINT('Ctrl Pts',(-4.39344141097314,-5.14683995946507,
127.972356053845));
#214744=CARTESIAN_POINT('Ctrl Pts',(-4.2628669198969,-5.25830085213497,
127.980393140388));
#214745=CARTESIAN_POINT('Ctrl Pts',(-4.1280271659833,-5.36480723477413,
127.988430226931));
#214746=CARTESIAN_POINT('Ctrl Pts',(-3.98934870189478,-5.46602103313648,
127.996467313473));
#214747=CARTESIAN_POINT('Ctrl Pts',(-3.85065696563169,-5.56724451813051,
128.004505169202));
#214748=CARTESIAN_POINT('Ctrl Pts',(-3.70812608940294,-5.66317418989895,
128.012543024932));
#214749=CARTESIAN_POINT('Ctrl Pts',(-3.56221294243062,-5.75351440015403,
128.020580880661));
#214750=CARTESIAN_POINT('Ctrl Pts',(-3.41625692062508,-5.8438811557995,
128.028621098218));
#214751=CARTESIAN_POINT('Ctrl Pts',(-3.26691696736246,-5.92865498423049,
128.036661315775));
#214752=CARTESIAN_POINT('Ctrl Pts',(-3.1146758188146,-6.00758550032304,
128.044701533332));
#214753=CARTESIAN_POINT('Ctrl Pts',(-2.95668290213072,-6.08949806188589,
128.053045515459));
#214754=CARTESIAN_POINT('Ctrl Pts',(-2.79556568532968,-6.16511695391536,
128.061389497587));
#214755=CARTESIAN_POINT('Ctrl Pts',(-2.6318868760193,-6.23421690927075,
128.069733479715));
#214756=CARTESIAN_POINT('Ctrl Pts',(-2.47389225499252,-6.30091718223426,
128.07778769455));
#214757=CARTESIAN_POINT('Ctrl Pts',(-2.3135113428348,-6.36154363543611,
128.085841909385));
#214758=CARTESIAN_POINT('Ctrl Pts',(-2.15126556895633,-6.41594462661758,
128.09389612422));
#214759=CARTESIAN_POINT('Ctrl Pts',(-1.98889838094546,-6.47038632794507,
128.101956366303));
#214760=CARTESIAN_POINT('Ctrl Pts',(-1.82466390852764,-6.51859318662524,
128.110016608386));
#214761=CARTESIAN_POINT('Ctrl Pts',(-1.65909428435162,-6.56046455334009,
128.118076850469));
#214762=CARTESIAN_POINT('Ctrl Pts',(-1.49329318248335,-6.60239445909788,
128.126148361323));
#214763=CARTESIAN_POINT('Ctrl Pts',(-1.32615356655731,-6.63797112369992,
128.134219872178));
#214764=CARTESIAN_POINT('Ctrl Pts',(-1.15821377460314,-6.66714555505724,
128.142291383032));
#214765=CARTESIAN_POINT('Ctrl Pts',(-1.14061193097295,-6.67020334006922,
128.143137361643));
#214766=CARTESIAN_POINT('Ctrl Pts',(-1.12300129779593,-6.67319084227332,
128.143983340254));
#214767=CARTESIAN_POINT('Ctrl Pts',(-1.10538249481115,-6.67610803838322,
128.144829318865));
#214768=CARTESIAN_POINT('Ctrl Pts',(-0.933995738766564,-6.70448503870811,
128.153058568601));
#214769=CARTESIAN_POINT('Ctrl Pts',(-0.761263712658549,-6.72629982420718,
128.161287818337));
#214770=CARTESIAN_POINT('Ctrl Pts',(-0.587730201326801,-6.74142879591918,
128.169517068073));
#214771=CARTESIAN_POINT('Ctrl Pts',(-0.414403223103981,-6.75653976169367,
128.177736523663));
#214772=CARTESIAN_POINT('Ctrl Pts',(-0.240277012831369,-6.76498072728823,
128.185955979253));
#214773=CARTESIAN_POINT('Ctrl Pts',(-0.065905572641955,-6.76667905663441,
128.194175434843));
#214774=CARTESIAN_POINT('Ctrl Pts',(0.108293355242183,-6.7683757057587,
128.202386758613));
#214775=CARTESIAN_POINT('Ctrl Pts',(0.282736673728126,-6.76334299978061,
128.210598082382));
#214776=CARTESIAN_POINT('Ctrl Pts',(0.456865136902315,-6.75156006021447,
128.218809406152));
#214777=CARTESIAN_POINT('Ctrl Pts',(0.630856284795527,-6.73978641251037,
128.227014254586));
#214778=CARTESIAN_POINT('Ctrl Pts',(0.804532715698328,-6.72127315775058,
128.23521910302));
#214779=CARTESIAN_POINT('Ctrl Pts',(0.977334968178098,-6.69605147530814,
128.243423951454));
#214780=CARTESIAN_POINT('Ctrl Pts',(1.15003563266157,-6.67084462033552,
128.251623976374));
#214781=CARTESIAN_POINT('Ctrl Pts',(1.32186278856019,-6.63893724576152,
128.259824001294));
#214782=CARTESIAN_POINT('Ctrl Pts',(1.49226179257834,-6.60041239184423,
128.268024026214));
#214783=CARTESIAN_POINT('Ctrl Pts',(1.66261147926394,-6.56189868789253,
128.276221677861));
#214784=CARTESIAN_POINT('Ctrl Pts',(1.83153348713577,-6.51677139465191,
128.284419329508));
#214785=CARTESIAN_POINT('Ctrl Pts',(1.99848282142742,-6.46516476297855,
128.292616981155));
#214786=CARTESIAN_POINT('Ctrl Pts',(2.16540980017873,-6.41356504174986,
128.300813535086));
#214787=CARTESIAN_POINT('Ctrl Pts',(2.33036428856015,-6.35548781518088,
128.309010089017));
#214788=CARTESIAN_POINT('Ctrl Pts',(2.49281591947777,-6.29111737226371,
128.317206642948));
#214789=CARTESIAN_POINT('Ctrl Pts',(2.65527533505303,-6.22674384472461,
128.325403589657));
#214790=CARTESIAN_POINT('Ctrl Pts',(2.81523132065585,-6.15607663214782,
128.333600536365));
#214791=CARTESIAN_POINT('Ctrl Pts',(2.97217293169374,-6.07934840785648,
128.341797483074));
#214792=CARTESIAN_POINT('Ctrl Pts',(3.12915059934962,-6.00260255560621,
128.349996312994));
#214793=CARTESIAN_POINT('Ctrl Pts',(3.28311219088485,-5.91979307575749,
128.358195142914));
#214794=CARTESIAN_POINT('Ctrl Pts',(3.43357078995366,-5.83119890163052,
128.366393972833));
#214795=CARTESIAN_POINT('Ctrl Pts',(3.58417189255028,-5.74252081749486,
128.374600568093));
#214796=CARTESIAN_POINT('Ctrl Pts',(3.73126306451462,-5.64804727511739,
128.382807163353));
#214797=CARTESIAN_POINT('Ctrl Pts',(3.87438505941322,-5.54810142403648,
128.391013758613));
#214798=CARTESIAN_POINT('Ctrl Pts',(4.01757632617791,-5.44810719859063,
128.399224325912));
#214799=CARTESIAN_POINT('Ctrl Pts',(4.15679429987137,-5.34263560021629,
128.407434893211));
#214800=CARTESIAN_POINT('Ctrl Pts',(4.29161243240706,-5.23205043267065,
128.41564546051));
#214801=CARTESIAN_POINT('Ctrl Pts',(4.4266164984481,-5.12131275234759,128.423867351356));
#214802=CARTESIAN_POINT('Ctrl Pts',(4.55720832794847,-5.00544764684747,
128.432089242203));
#214803=CARTESIAN_POINT('Ctrl Pts',(4.68299700033132,-4.88485701887864,
128.44031113305));
#214804=CARTESIAN_POINT('Ctrl Pts',(4.79736858979085,-4.77521167853558,
128.447786772205));
#214805=CARTESIAN_POINT('Ctrl Pts',(4.90776969492203,-4.66166029872621,
128.455262411359));
#214806=CARTESIAN_POINT('Ctrl Pts',(5.01393570377541,-4.54452833178606,
128.462738050514));
#214807=CARTESIAN_POINT('Ctrl Pts',(5.14084036461515,-4.40451560362031,
128.471673993965));
#214808=CARTESIAN_POINT('Ctrl Pts',(5.26195793272095,-4.25909512080603,
128.480609937416));
#214809=CARTESIAN_POINT('Ctrl Pts',(5.37684636472458,-4.10874824857256,
128.489545880867));
#214810=CARTESIAN_POINT('Ctrl Pts',(5.49156208894257,-3.95862738756519,
128.498468391224));
#214811=CARTESIAN_POINT('Ctrl Pts',(5.60006720512561,-3.80359511868335,
128.507390901582));
#214812=CARTESIAN_POINT('Ctrl Pts',(5.70195934344626,-3.64416638556556,
128.516313411939));
#214813=CARTESIAN_POINT('Ctrl Pts',(5.80360181440798,-3.48512830231919,
128.525214059378));
#214814=CARTESIAN_POINT('Ctrl Pts',(5.89866350871404,-3.32171547240884,
128.534114706816));
#214815=CARTESIAN_POINT('Ctrl Pts',(5.98678516391366,-3.15447181016779,
128.543015354254));
#214816=CARTESIAN_POINT('Ctrl Pts',(6.07477063797122,-2.98748660236538,
128.551902246841));
#214817=CARTESIAN_POINT('Ctrl Pts',(6.15583734667113,-2.81668259853102,
128.560789139427));
#214818=CARTESIAN_POINT('Ctrl Pts',(6.22967022459886,-2.64263086577494,
128.569676032013));
#214819=CARTESIAN_POINT('Ctrl Pts',(6.30331332446926,-2.46902651094377,
128.578540081968));
#214820=CARTESIAN_POINT('Ctrl Pts',(6.36975959536808,-2.29219132178817,
128.587404131923));
#214821=CARTESIAN_POINT('Ctrl Pts',(6.42874095680524,-2.112718322516,128.596268181878));
#214822=CARTESIAN_POINT('Ctrl Pts',(6.48513188306158,-1.94112769760743,
128.604742926698));
#214823=CARTESIAN_POINT('Ctrl Pts',(6.53469939456372,-1.76712621777812,
128.613217671519));
#214824=CARTESIAN_POINT('Ctrl Pts',(6.57724914388337,-1.59125192828965,
128.621692416339));
#214825=CARTESIAN_POINT('Ctrl Pts',(6.6184642197997,-1.42089435136144,128.629901330768));
#214826=CARTESIAN_POINT('Ctrl Pts',(6.6530542122505,-1.24894359960696,128.638110245197));
#214827=CARTESIAN_POINT('Ctrl Pts',(6.68091396152673,-1.07595429209483,
128.646319159626));
#214828=CARTESIAN_POINT('Ctrl Pts',(6.70878033431683,-0.902923857253567,
128.654530025683));
#214829=CARTESIAN_POINT('Ctrl Pts',(6.72991321950296,-0.728854726296877,
128.66274089174));
#214830=CARTESIAN_POINT('Ctrl Pts',(6.74425911227886,-0.554308602173563,
128.670951757797));
#214831=CARTESIAN_POINT('Ctrl Pts',(6.75861097293342,-0.379689867017456,
128.679166039566));
#214832=CARTESIAN_POINT('Ctrl Pts',(6.76617018726055,-0.204594097975946,
128.687380321336));
#214833=CARTESIAN_POINT('Ctrl Pts',(6.7669353273155,-0.0295850626069757,
128.695594603106));
#214834=CARTESIAN_POINT('Ctrl Pts',(6.76770132859599,0.145620959247148,
128.703818130698));
#214835=CARTESIAN_POINT('Ctrl Pts',(6.76165797993374,0.320739696222828,
128.712041658291));
#214836=CARTESIAN_POINT('Ctrl Pts',(6.74885594684485,0.495209459458303,
128.720265185883));
#214837=CARTESIAN_POINT('Ctrl Pts',(6.73604570815073,0.669791051025288,
128.728493984437));
#214838=CARTESIAN_POINT('Ctrl Pts',(6.7164681890796,0.843722486719249,128.736722782991));
#214839=CARTESIAN_POINT('Ctrl Pts',(6.69022554282093,1.01645028712002,128.744951581544));
#214840=CARTESIAN_POINT('Ctrl Pts',(6.66394677565971,1.18941583351581,128.753191706381));
#214841=CARTESIAN_POINT('Ctrl Pts',(6.63098462397198,1.36117408682237,128.761431831217));
#214842=CARTESIAN_POINT('Ctrl Pts',(6.59149187850487,1.53118379550084,128.769671956054));
#214843=CARTESIAN_POINT('Ctrl Pts',(6.57395872932242,1.60666109011455,128.773330231424));
#214844=CARTESIAN_POINT('Ctrl Pts',(6.5551390564748,1.68179397001506,128.776988506794));
#214845=CARTESIAN_POINT('Ctrl Pts',(6.53504930254469,1.75653625448213,128.780646782164));
#214846=CARTESIAN_POINT('Ctrl Pts',(6.48865205642261,1.92915340948616,128.789095561742));
#214847=CARTESIAN_POINT('Ctrl Pts',(6.43537106265126,2.10008102358008,128.797544341319));
#214848=CARTESIAN_POINT('Ctrl Pts',(6.37534799585066,2.26875008138908,128.805993120897));
#214849=CARTESIAN_POINT('Ctrl Pts',(6.31538092067281,2.43726179878286,128.814434019157));
#214850=CARTESIAN_POINT('Ctrl Pts',(6.248684420805,2.60351884688755,128.822874917417));
#214851=CARTESIAN_POINT('Ctrl Pts',(6.1754502253491,2.76696648231159,128.831315815676));
#214852=CARTESIAN_POINT('Ctrl Pts',(6.10227306902599,2.93028681502789,128.839750139664));
#214853=CARTESIAN_POINT('Ctrl Pts',(6.02256850454503,3.09080179402754,128.848184463652));
#214854=CARTESIAN_POINT('Ctrl Pts',(5.93657683693599,3.24797544004802,128.85661878764));
#214855=CARTESIAN_POINT('Ctrl Pts',(5.85064623586848,3.40503747001023,128.865047122036));
#214856=CARTESIAN_POINT('Ctrl Pts',(5.75843759684971,3.55876260801143,128.873475456432));
#214857=CARTESIAN_POINT('Ctrl Pts',(5.66023783981895,3.70863810538069,128.881903790828));
#214858=CARTESIAN_POINT('Ctrl Pts',(5.56207889758102,3.85845130995453,128.890328622152));
#214859=CARTESIAN_POINT('Ctrl Pts',(5.45793398356232,4.0044177849552,128.898753453477));
#214860=CARTESIAN_POINT('Ctrl Pts',(5.34813447293877,4.14605193640455,128.907178284802));
#214861=CARTESIAN_POINT('Ctrl Pts',(5.23836526155172,4.28764700383043,128.91560079129));
#214862=CARTESIAN_POINT('Ctrl Pts',(5.12294476882755,4.42491186805172,128.924023297778));
#214863=CARTESIAN_POINT('Ctrl Pts',(5.00224617872701,4.55739203573832,128.932445804266));
#214864=CARTESIAN_POINT('Ctrl Pts',(4.88156404397508,4.68985414184407,128.940867162478));
#214865=CARTESIAN_POINT('Ctrl Pts',(4.75560547173743,4.81753260630425,128.94928852069));
#214866=CARTESIAN_POINT('Ctrl Pts',(4.62478245260127,4.94000771923601,128.957709878902));
#214867=CARTESIAN_POINT('Ctrl Pts',(4.49393193512466,5.06250857582034,128.966133007242));
#214868=CARTESIAN_POINT('Ctrl Pts',(4.35821516904719,5.17980366523237,128.974556135581));
#214869=CARTESIAN_POINT('Ctrl Pts',(4.21807990138325,5.29151121566861,128.98297926392));
#214870=CARTESIAN_POINT('Ctrl Pts',(4.07793088291443,5.40322972743354,128.991403218781));
#214871=CARTESIAN_POINT('Ctrl Pts',(3.9333627619541,5.5093594026608,128.999827173641));
#214872=CARTESIAN_POINT('Ctrl Pts',(3.7848550896124,5.60955978224987,129.008251128502));
#214873=CARTESIAN_POINT('Ctrl Pts',(3.63627224497738,5.70981088172569,129.016679347438));
#214874=CARTESIAN_POINT('Ctrl Pts',(3.48374614353515,5.8041265058107,129.025107566375));
#214875=CARTESIAN_POINT('Ctrl Pts',(3.32778464020283,5.8922099749101,129.033535785312));
#214876=CARTESIAN_POINT('Ctrl Pts',(3.25234212869507,5.934818169812,129.037612727317));
#214877=CARTESIAN_POINT('Ctrl Pts',(3.17609615240169,5.97596878037611,129.041689669322));
#214878=CARTESIAN_POINT('Ctrl Pts',(3.09910619832118,6.01563211736948,129.045766611327));
#214879=CARTESIAN_POINT('Ctrl Pts',(3.09910619832142,6.01563211736936,127.045755263024));
#214880=CARTESIAN_POINT('Ctrl Pts',(2.93375330764834,6.10081787314649,127.054504710927));
#214881=CARTESIAN_POINT('Ctrl Pts',(2.76488627843078,6.17918207037036,127.063254158829));
#214882=CARTESIAN_POINT('Ctrl Pts',(2.59307866646709,6.25045854553994,127.072003606731));
#214883=CARTESIAN_POINT('Ctrl Pts',(2.4212724418539,6.32173444515032,127.080752983982));
#214884=CARTESIAN_POINT('Ctrl Pts',(2.24652594672485,6.38592262741831,127.089502361232));
#214885=CARTESIAN_POINT('Ctrl Pts',(2.06943269687149,6.44280508110553,127.098251738482));
#214886=CARTESIAN_POINT('Ctrl Pts',(1.89234081822105,6.49968709436158,127.107001047988));
#214887=CARTESIAN_POINT('Ctrl Pts',(1.71290249405617,6.54926340459537,127.115750357493));
#214888=CARTESIAN_POINT('Ctrl Pts',(1.53172716625088,6.59136563150377,127.124499666998));
#214889=CARTESIAN_POINT('Ctrl Pts',(1.35055318107381,6.633467546407,127.133248911665));
#214890=CARTESIAN_POINT('Ctrl Pts',(1.16764249714483,6.66809542395764,127.141998156333));
#214891=CARTESIAN_POINT('Ctrl Pts',(0.983616340615169,6.69513165624656,
127.150747401));
#214892=CARTESIAN_POINT('Ctrl Pts',(0.799591486714658,6.72216769715951,
127.159496583736));
#214893=CARTESIAN_POINT('Ctrl Pts',(0.614451459527529,6.74161215869364,
127.168245766471));
#214894=CARTESIAN_POINT('Ctrl Pts',(0.4288250479111,6.75339900185707,127.176994949207));
#214895=CARTESIAN_POINT('Ctrl Pts',(0.243199888597772,6.76518576550218,
127.185744072918));
#214896=CARTESIAN_POINT('Ctrl Pts',(0.0570886373925512,6.76931499599834,
127.194493196628));
#214897=CARTESIAN_POINT('Ctrl Pts',(-0.128876626810609,6.76577266947848,
127.203242320339));
#214898=CARTESIAN_POINT('Ctrl Pts',(-0.314840698187433,6.76223036567996,
127.21199138793));
#214899=CARTESIAN_POINT('Ctrl Pts',(-0.500658497950342,6.75101660879229,
127.220740455522));
#214900=CARTESIAN_POINT('Ctrl Pts',(-0.685698951925125,6.73216948296229,
127.229489523113));
#214901=CARTESIAN_POINT('Ctrl Pts',(-0.870738280458545,6.7133224717631,
127.238238537492));
#214902=CARTESIAN_POINT('Ctrl Pts',(-1.05499998761099,6.6868422135621,127.24698755187));
#214903=CARTESIAN_POINT('Ctrl Pts',(-1.23785829161247,6.65281863948554,
127.255736566249));
#214904=CARTESIAN_POINT('Ctrl Pts',(-1.43007412917228,6.61705395368899,
127.264933299948));
#214905=CARTESIAN_POINT('Ctrl Pts',(-1.62073882535614,6.57295372727834,
127.274130033647));
#214906=CARTESIAN_POINT('Ctrl Pts',(-1.80913696091334,6.52068343478329,
127.283326767346));
#214907=CARTESIAN_POINT('Ctrl Pts',(-1.98838356185933,6.47095219815253,
127.29207676506));
#214908=CARTESIAN_POINT('Ctrl Pts',(-2.16557827572356,6.41382586850951,
127.300826762774));
#214909=CARTESIAN_POINT('Ctrl Pts',(-2.34011918621525,6.34949849943342,
127.309576760487));
#214910=CARTESIAN_POINT('Ctrl Pts',(-2.51465655690918,6.28517243495622,
127.318326580746));
#214911=CARTESIAN_POINT('Ctrl Pts',(-2.68653996295144,6.21364572242454,
127.327076401004));
#214912=CARTESIAN_POINT('Ctrl Pts',(-2.85518555379801,6.13516132252308,
127.335826221262));
#214913=CARTESIAN_POINT('Ctrl Pts',(-3.02382794858505,6.05667841000599,
127.3445758757));
#214914=CARTESIAN_POINT('Ctrl Pts',(-3.18923239109101,5.97123819492177,
127.353325530137));
#214915=CARTESIAN_POINT('Ctrl Pts',(-3.35083705967523,5.87913088810813,
127.362075184575));
#214916=CARTESIAN_POINT('Ctrl Pts',(-3.51243888042223,5.7870252044321,127.370824684824));
#214917=CARTESIAN_POINT('Ctrl Pts',(-3.67024081223512,5.68825280605898,
127.379574185073));
#214918=CARTESIAN_POINT('Ctrl Pts',(-3.82370687544222,5.58314917682628,
127.388323685322));
#214919=CARTESIAN_POINT('Ctrl Pts',(-3.97717043817636,5.47804726008151,
127.397073043012));
#214920=CARTESIAN_POINT('Ctrl Pts',(-4.12629803722282,5.36661448084373,
127.405822400703));
#214921=CARTESIAN_POINT('Ctrl Pts',(-4.2705831720673,5.24922931204721,127.414571758393));
#214922=CARTESIAN_POINT('Ctrl Pts',(-4.41486614774675,5.13184589986929,
127.423320985153));
#214923=CARTESIAN_POINT('Ctrl Pts',(-4.55430658194271,5.00851045723165,
127.432070211913));
#214924=CARTESIAN_POINT('Ctrl Pts',(-4.68843089001719,4.87964187103241,
127.440819438673));
#214925=CARTESIAN_POINT('Ctrl Pts',(-4.82255336917711,4.75077504208087,
127.449568546129));
#214926=CARTESIAN_POINT('Ctrl Pts',(-4.95135966065011,4.61637541908226,
127.458317653585));
#214927=CARTESIAN_POINT('Ctrl Pts',(-5.07441230869123,4.47689945401982,
127.467066761041));
#214928=CARTESIAN_POINT('Ctrl Pts',(-5.19746344226297,4.33742520555659,
127.475815760817));
#214929=CARTESIAN_POINT('Ctrl Pts',(-5.31476088454649,4.19287495491486,
127.484564760594));
#214930=CARTESIAN_POINT('Ctrl Pts',(-5.42590627628738,4.04373961586862,
127.49331376037));
#214931=CARTESIAN_POINT('Ctrl Pts',(-5.53706380672565,3.89458798906881,
127.502063715665));
#214932=CARTESIAN_POINT('Ctrl Pts',(-5.64206777071774,3.74085050155421,
127.51081367096));
#214933=CARTESIAN_POINT('Ctrl Pts',(-5.74056148163929,3.58304938223287,
127.519563626254));
#214934=CARTESIAN_POINT('Ctrl Pts',(-5.83905138951799,3.42525435593426,
127.528313243695));
#214935=CARTESIAN_POINT('Ctrl Pts',(-5.93103139557562,3.26339625497346,
127.537062861136));
#214936=CARTESIAN_POINT('Ctrl Pts',(-6.01618907820752,3.09802485065187,
127.545812478578));
#214937=CARTESIAN_POINT('Ctrl Pts',(-6.10134392544901,2.93265895249813,
127.554561804693));
#214938=CARTESIAN_POINT('Ctrl Pts',(-6.1796767726176,2.76378023986197,127.563311130809));
#214939=CARTESIAN_POINT('Ctrl Pts',(-6.25092157009161,2.59196229227267,
127.572060456925));
#214940=CARTESIAN_POINT('Ctrl Pts',(-6.32216437407696,2.4201491522924,127.580809538228));
#214941=CARTESIAN_POINT('Ctrl Pts',(-6.3863194154887,2.24539720662996,127.58955861953));
#214942=CARTESIAN_POINT('Ctrl Pts',(-6.44316881037492,2.06829994947828,
127.598307700833));
#214943=CARTESIAN_POINT('Ctrl Pts',(-6.50002334524528,1.89118668024599,
127.607057573175));
#214944=CARTESIAN_POINT('Ctrl Pts',(-6.54957082411055,1.71172794807858,
127.615807445517));
#214945=CARTESIAN_POINT('Ctrl Pts',(-6.59164294296046,1.53053334250502,
127.62455731786));
#214946=CARTESIAN_POINT('Ctrl Pts',(-6.63371214082104,1.34935131693749,
127.633306582715));
#214947=CARTESIAN_POINT('Ctrl Pts',(-6.66830695239666,1.166433938299,127.642055847569));
#214948=CARTESIAN_POINT('Ctrl Pts',(-6.6953098815397,0.982402458342219,
127.650805112424));
#214949=CARTESIAN_POINT('Ctrl Pts',(-6.72231419690468,0.798361530948305,
127.659554826431));
#214950=CARTESIAN_POINT('Ctrl Pts',(-6.74172580829266,0.61320667136374,
127.668304540438));
#214951=CARTESIAN_POINT('Ctrl Pts',(-6.75347878028171,0.427566795114677,
127.677054254445));
#214952=CARTESIAN_POINT('Ctrl Pts',(-6.76248992368202,0.285234494207743,
127.683762764234));
#214953=CARTESIAN_POINT('Ctrl Pts',(-6.76699999999987,0.142617266095797,
127.690471274022));
#214954=CARTESIAN_POINT('Ctrl Pts',(-6.767,6.29785154665824E-12,127.69717978381));
#214955=CARTESIAN_POINT('',(-6.767,6.9710326081884E-10,127.302820216158));
#214956=CARTESIAN_POINT('Ctrl Pts',(3.0991061983215,6.01563211736932,126.651395695404));
#214957=CARTESIAN_POINT('Ctrl Pts',(2.9337533076484,6.10081787314647,126.660145143307));
#214958=CARTESIAN_POINT('Ctrl Pts',(2.76488627843081,6.17918207037034,126.668894591209));
#214959=CARTESIAN_POINT('Ctrl Pts',(2.5930786664671,6.25045854553994,126.677644039111));
#214960=CARTESIAN_POINT('Ctrl Pts',(2.42127244185376,6.32173444515037,126.686393416362));
#214961=CARTESIAN_POINT('Ctrl Pts',(2.24652594672456,6.38592262741841,126.695142793612));
#214962=CARTESIAN_POINT('Ctrl Pts',(2.06943269687104,6.44280508110567,126.703892170862));
#214963=CARTESIAN_POINT('Ctrl Pts',(1.89234081822057,6.49968709436172,126.712641480368));
#214964=CARTESIAN_POINT('Ctrl Pts',(1.71290249405566,6.54926340459551,126.721390789873));
#214965=CARTESIAN_POINT('Ctrl Pts',(1.53172716625033,6.59136563150389,126.730140099378));
#214966=CARTESIAN_POINT('Ctrl Pts',(1.3505531810731,6.63346754640715,126.738889344046));
#214967=CARTESIAN_POINT('Ctrl Pts',(1.16764249714397,6.6680954239578,126.747638588713));
#214968=CARTESIAN_POINT('Ctrl Pts',(0.983616340614145,6.69513165624671,
126.75638783338));
#214969=CARTESIAN_POINT('Ctrl Pts',(0.799591486713599,6.72216769715964,
126.765137016116));
#214970=CARTESIAN_POINT('Ctrl Pts',(0.614451459526438,6.74161215869374,
126.773886198851));
#214971=CARTESIAN_POINT('Ctrl Pts',(0.428825047909977,6.75339900185714,
126.782635381587));
#214972=CARTESIAN_POINT('Ctrl Pts',(0.243199888596744,6.76518576550222,
126.791384505298));
#214973=CARTESIAN_POINT('Ctrl Pts',(0.0570886373916206,6.76931499599834,
126.800133629008));
#214974=CARTESIAN_POINT('Ctrl Pts',(-0.128876626811441,6.76577266947846,
126.808882752719));
#214975=CARTESIAN_POINT('Ctrl Pts',(-0.314840698188423,6.76223036567992,
126.81763182031));
#214976=CARTESIAN_POINT('Ctrl Pts',(-0.500658497951488,6.75101660879221,
126.826380887902));
#214977=CARTESIAN_POINT('Ctrl Pts',(-0.685698951926425,6.73216948296216,
126.835129955493));
#214978=CARTESIAN_POINT('Ctrl Pts',(-0.870738280459872,6.71332247176292,
126.843878969872));
#214979=CARTESIAN_POINT('Ctrl Pts',(-1.05499998761234,6.68684221356189,
126.85262798425));
#214980=CARTESIAN_POINT('Ctrl Pts',(-1.23785829161385,6.65281863948529,
126.861376998629));
#214981=CARTESIAN_POINT('Ctrl Pts',(-1.43007412915944,6.61705395369134,
126.870573732327));
#214982=CARTESIAN_POINT('Ctrl Pts',(-1.6207388253293,6.57295372728452,126.879770466026));
#214983=CARTESIAN_POINT('Ctrl Pts',(-1.80913696087289,6.52068343479452,
126.888967199724));
#214984=CARTESIAN_POINT('Ctrl Pts',(-1.98838356181923,6.47095219816486,
126.897717197438));
#214985=CARTESIAN_POINT('Ctrl Pts',(-2.16557827568384,6.41382586852292,
126.906467195152));
#214986=CARTESIAN_POINT('Ctrl Pts',(-2.34011918617595,6.34949849944791,
126.915217192865));
#214987=CARTESIAN_POINT('Ctrl Pts',(-2.51465655687044,6.28517243497173,
126.923967013124));
#214988=CARTESIAN_POINT('Ctrl Pts',(-2.68653996291328,6.21364572244104,
126.932716833382));
#214989=CARTESIAN_POINT('Ctrl Pts',(-2.85518555376046,6.13516132254055,
126.94146665364));
#214990=CARTESIAN_POINT('Ctrl Pts',(-3.0238279485479,6.05667841002453,126.950216308078));
#214991=CARTESIAN_POINT('Ctrl Pts',(-3.1892323910543,5.97123819494137,126.958965962515));
#214992=CARTESIAN_POINT('Ctrl Pts',(-3.350837059639,5.87913088812878,126.967715616953));
#214993=CARTESIAN_POINT('Ctrl Pts',(-3.51243888038659,5.78702520445373,
126.976465117202));
#214994=CARTESIAN_POINT('Ctrl Pts',(-3.67024081220012,5.68825280608157,
126.985214617451));
#214995=CARTESIAN_POINT('Ctrl Pts',(-3.82370687540789,5.58314917684979,
126.9939641177));
#214996=CARTESIAN_POINT('Ctrl Pts',(-3.9771704381427,5.47804726010595,127.00271347539));
#214997=CARTESIAN_POINT('Ctrl Pts',(-4.12629803718987,5.36661448086907,
127.011462833081));
#214998=CARTESIAN_POINT('Ctrl Pts',(-4.27058317203509,5.24922931207341,
127.020212190771));
#214999=CARTESIAN_POINT('Ctrl Pts',(-4.41486614771509,5.13184589989652,
127.028961417531));
#215000=CARTESIAN_POINT('Ctrl Pts',(-4.55430658191164,5.00851045725989,
127.037710644291));
#215001=CARTESIAN_POINT('Ctrl Pts',(-4.68843088998676,4.87964187106164,
127.046459871051));
#215002=CARTESIAN_POINT('Ctrl Pts',(-4.8225533691476,4.75077504211083,127.055208978507));
#215003=CARTESIAN_POINT('Ctrl Pts',(-4.95135966062154,4.6163754191129,127.063958085963));
#215004=CARTESIAN_POINT('Ctrl Pts',(-5.07441230866363,4.47689945405111,
127.072707193419));
#215005=CARTESIAN_POINT('Ctrl Pts',(-5.19746344223616,4.33742520558871,
127.081456193195));
#215006=CARTESIAN_POINT('Ctrl Pts',(-5.31476088452052,4.19287495494778,
127.090205192972));
#215007=CARTESIAN_POINT('Ctrl Pts',(-5.42590627626227,4.04373961590231,
127.098954192748));
#215008=CARTESIAN_POINT('Ctrl Pts',(-5.53706380670133,3.89458798910337,
127.107704148043));
#215009=CARTESIAN_POINT('Ctrl Pts',(-5.64206777069426,3.74085050158961,
127.116454103338));
#215010=CARTESIAN_POINT('Ctrl Pts',(-5.74056148161669,3.58304938226908,
127.125204058632));
#215011=CARTESIAN_POINT('Ctrl Pts',(-5.83905138949646,3.42525435597096,
127.133953676073));
#215012=CARTESIAN_POINT('Ctrl Pts',(-5.93103139555519,3.26339625501061,
127.142703293514));
#215013=CARTESIAN_POINT('Ctrl Pts',(-6.0161890781882,3.0980248506894,127.151452910956));
#215014=CARTESIAN_POINT('Ctrl Pts',(-6.10134392543061,2.9326589525364,127.160202237071));
#215015=CARTESIAN_POINT('Ctrl Pts',(-6.17967677260016,2.76378023990094,
127.168951563187));
#215016=CARTESIAN_POINT('Ctrl Pts',(-6.25092157007518,2.5919622923123,127.177700889303));
#215017=CARTESIAN_POINT('Ctrl Pts',(-6.32216437406154,2.42014915233269,
127.186449970606));
#215018=CARTESIAN_POINT('Ctrl Pts',(-6.38631941547431,2.24539720667087,
127.195199051908));
#215019=CARTESIAN_POINT('Ctrl Pts',(-6.4431688103616,2.06829994951977,127.20394813321));
#215020=CARTESIAN_POINT('Ctrl Pts',(-6.50002334523311,1.89118668028781,
127.212698005553));
#215021=CARTESIAN_POINT('Ctrl Pts',(-6.54957082409955,1.71172794812069,
127.221447877895));
#215022=CARTESIAN_POINT('Ctrl Pts',(-6.59164294295062,1.53053334254738,
127.230197750238));
#215023=CARTESIAN_POINT('Ctrl Pts',(-6.63371214081235,1.34935131698021,
127.238947015092));
#215024=CARTESIAN_POINT('Ctrl Pts',(-6.66830695238913,1.16643393834204,
127.247696279947));
#215025=CARTESIAN_POINT('Ctrl Pts',(-6.69530988153335,0.982402458385534,
127.256445544802));
#215026=CARTESIAN_POINT('Ctrl Pts',(-6.7223141968995,0.798361530991892,
127.265195258809));
#215027=CARTESIAN_POINT('Ctrl Pts',(-6.74172580828867,0.613206671407551,
127.273944972816));
#215028=CARTESIAN_POINT('Ctrl Pts',(-6.75347878027893,0.427566795158662,
127.282694686823));
#215029=CARTESIAN_POINT('Ctrl Pts',(-6.76248992366655,0.285234494466871,
127.289403196601));
#215030=CARTESIAN_POINT('Ctrl Pts',(-6.76699999998531,0.142617266570896,
127.296111706379));
#215031=CARTESIAN_POINT('Ctrl Pts',(-6.767,6.96911759829614E-10,127.302820216158));
#215032=CARTESIAN_POINT('Ctrl Pts',(-6.767,6.44645169383305E-12,127.30282021619));
#215033=CARTESIAN_POINT('Ctrl Pts',(-6.76700000000018,-0.186007249520387,
127.311569728001));
#215034=CARTESIAN_POINT('Ctrl Pts',(-6.75932637294556,-0.372014355743401,
127.320319239812));
#215035=CARTESIAN_POINT('Ctrl Pts',(-6.74400518264234,-0.557389537480952,
127.329068751624));
#215036=CARTESIAN_POINT('Ctrl Pts',(-6.72868405705156,-0.742763936245431,
127.337818226479));
#215037=CARTESIAN_POINT('Ctrl Pts',(-6.70571545645811,-0.92750613023609,
127.346567701335));
#215038=CARTESIAN_POINT('Ctrl Pts',(-6.67517739404901,-1.11098863989562,
127.355317176191));
#215039=CARTESIAN_POINT('Ctrl Pts',(-6.64463945808784,-1.29447038981527,
127.364066614818));
#215040=CARTESIAN_POINT('Ctrl Pts',(-6.60653217008442,-1.47669218313298,
127.372816053445));
#215041=CARTESIAN_POINT('Ctrl Pts',(-6.56098496092766,-1.65703510598935,
127.381565492072));
#215042=CARTESIAN_POINT('Ctrl Pts',(-6.51543793658396,-1.83737729708346,
127.390314895197));
#215043=CARTESIAN_POINT('Ctrl Pts',(-6.46245112167531,-2.01584035510571,
127.399064298322));
#215044=CARTESIAN_POINT('Ctrl Pts',(-6.40220448374376,-2.19181813760434,
127.407813701447));
#215045=CARTESIAN_POINT('Ctrl Pts',(-6.34195808526638,-2.36779522066783,
127.416563069797));
#215046=CARTESIAN_POINT('Ctrl Pts',(-6.27445201433251,-2.54128677683803,
127.425312438147));
#215047=CARTESIAN_POINT('Ctrl Pts',(-6.19991555072061,-2.71170355384447,
127.434061806497));
#215048=CARTESIAN_POINT('Ctrl Pts',(-6.12537937716864,-2.88211966767113,
127.442811140799));
#215049=CARTESIAN_POINT('Ctrl Pts',(-6.04381298052703,-3.04946076371422,
127.451560475101));
#215050=CARTESIAN_POINT('Ctrl Pts',(-5.95549339336027,-3.21315848374185,
127.460309809403));
#215051=CARTESIAN_POINT('Ctrl Pts',(-5.86717414255612,-3.37685558033141,
127.469059110383));
#215052=CARTESIAN_POINT('Ctrl Pts',(-5.77210188876808,-3.53690907646415,
127.477808411363));
#215053=CARTESIAN_POINT('Ctrl Pts',(-5.67059953347211,-3.69277536968956,
127.486557712343));
#215054=CARTESIAN_POINT('Ctrl Pts',(-5.56909755631596,-3.84864108224617,
127.495306980729));
#215055=CARTESIAN_POINT('Ctrl Pts',(-5.46116568197058,-4.00031938297234,
127.504056249114));
#215056=CARTESIAN_POINT('Ctrl Pts',(-5.34717048533805,-4.14729511859594,
127.512805517499));
#215057=CARTESIAN_POINT('Ctrl Pts',(-5.23317570392044,-4.29427031887663,
127.521554754016));
#215058=CARTESIAN_POINT('Ctrl Pts',(-5.11311782003727,-4.43654276189302,
127.530303990533));
#215059=CARTESIAN_POINT('Ctrl Pts',(-4.98740458984971,-4.57362924351615,
127.53905322705));
#215060=CARTESIAN_POINT('Ctrl Pts',(-4.86169180711974,-4.71071523720028,
127.547802432426));
#215061=CARTESIAN_POINT('Ctrl Pts',(-4.73032391204415,-4.84261509522999,
127.556551637801));
#215062=CARTESIAN_POINT('Ctrl Pts',(-4.59374707013856,-4.96888084538092,
127.565300843177));
#215063=CARTESIAN_POINT('Ctrl Pts',(-4.45717070301705,-5.09514615659236,
127.574050018137));
#215064=CARTESIAN_POINT('Ctrl Pts',(-4.31538563571304,-5.2157772045931,
127.582799193098));
#215065=CARTESIAN_POINT('Ctrl Pts',(-4.16887341029775,-5.33036429232679,
127.591548368058));
#215066=CARTESIAN_POINT('Ctrl Pts',(-4.02236168203971,-5.4449509912342,
127.60029751333));
#215067=CARTESIAN_POINT('Ctrl Pts',(-3.8711230534843,-5.55349359438418,
127.609046658602));
#215068=CARTESIAN_POINT('Ctrl Pts',(-3.71567117018023,-5.65562346298721,
127.617795803874));
#215069=CARTESIAN_POINT('Ctrl Pts',(-3.56021980146088,-5.75775299351478,
127.626544920184));
#215070=CARTESIAN_POINT('Ctrl Pts',(-3.40055544538624,-5.85346967463713,
127.635294036494));
#215071=CARTESIAN_POINT('Ctrl Pts',(-3.23722035987134,-5.94244842986748,
127.644043152805));
#215072=CARTESIAN_POINT('Ctrl Pts',(-3.07388580147439,-6.03142689794398,
127.652792240879));
#215073=CARTESIAN_POINT('Ctrl Pts',(-2.90688078896814,-6.1136673465667,
127.661541328954));
#215074=CARTESIAN_POINT('Ctrl Pts',(-2.73677250721582,-6.1888904695226,
127.670290417029));
#215075=CARTESIAN_POINT('Ctrl Pts',(-2.56666476031689,-6.26411335596242,
127.679039477595));
#215076=CARTESIAN_POINT('Ctrl Pts',(-2.39345402575367,-6.3323188450048,
127.687788538161));
#215077=CARTESIAN_POINT('Ctrl Pts',(-2.21772856065787,-6.39327529762659,
127.696537598727));
#215078=CARTESIAN_POINT('Ctrl Pts',(-2.04200363348673,-6.45423156365062,
127.705286632511));
#215079=CARTESIAN_POINT('Ctrl Pts',(-1.86376426189401,-6.50793874375624,
127.714035666295));
#215080=CARTESIAN_POINT('Ctrl Pts',(-1.68361577753238,-6.5542144390952,
127.722784700078));
#215081=CARTESIAN_POINT('Ctrl Pts',(-1.50346782967888,-6.60048999661848,
127.731533707806));
#215082=CARTESIAN_POINT('Ctrl Pts',(-1.32141105795079,-6.63933404237694,
127.740282715534));
#215083=CARTESIAN_POINT('Ctrl Pts',(-1.13806375487118,-6.67061465607545,
127.749031723262));
#215084=CARTESIAN_POINT('Ctrl Pts',(-0.954716982604014,-6.70189517921282,
127.75778070566));
#215085=CARTESIAN_POINT('Ctrl Pts',(-0.770079968903175,-6.72561226592216,
127.766529688059));
#215086=CARTESIAN_POINT('Ctrl Pts',(-0.58477976555932,-6.74168536983093,
127.775278670457));
#215087=CARTESIAN_POINT('Ctrl Pts',(-0.391489830652405,-6.75845151013846,
127.784404889467));
#215088=CARTESIAN_POINT('Ctrl Pts',(-0.197478578239474,-6.76689983031622,
127.793531108477));
#215089=CARTESIAN_POINT('Ctrl Pts',(-0.00346287645251185,-6.76699911397118,
127.802657327487));
#215090=CARTESIAN_POINT('Ctrl Pts',(0.184489834653576,-6.76709529501192,
127.811498352152));
#215091=CARTESIAN_POINT('Ctrl Pts',(0.372446404249023,-6.7593563973817,
127.820339376818));
#215092=CARTESIAN_POINT('Ctrl Pts',(0.559755019487951,-6.7438092587319,
127.829180401484));
#215093=CARTESIAN_POINT('Ctrl Pts',(0.745134705521472,-6.72842222659809,
127.837930380094));
#215094=CARTESIAN_POINT('Ctrl Pts',(0.929879431228346,-6.70538706057527,
127.846680358704));
#215095=CARTESIAN_POINT('Ctrl Pts',(1.11336163626811,-6.6747820089413,127.855430337313));
#215096=CARTESIAN_POINT('Ctrl Pts',(1.29684196300721,-6.64417727061013,
127.86418022635));
#215097=CARTESIAN_POINT('Ctrl Pts',(1.47905951217528,-6.60600284890587,
127.872930115386));
#215098=CARTESIAN_POINT('Ctrl Pts',(1.65939532067118,-6.56038841607222,
127.881680004423));
#215099=CARTESIAN_POINT('Ctrl Pts',(1.83972934300847,-6.51477443503244,
127.890429806795));
#215100=CARTESIAN_POINT('Ctrl Pts',(2.01818138406321,-6.46172066062124,
127.899179609167));
#215101=CARTESIAN_POINT('Ctrl Pts',(2.19414528354267,-6.40140730423455,
127.907929411539));
#215102=CARTESIAN_POINT('Ctrl Pts',(2.37010749864065,-6.34109452518618,
127.916679130156));
#215103=CARTESIAN_POINT('Ctrl Pts',(2.54358134866523,-6.27352239616478,
127.925428848772));
#215104=CARTESIAN_POINT('Ctrl Pts',(2.71397759435617,-6.19892043966792,
127.934178567388));
#215105=CARTESIAN_POINT('Ctrl Pts',(2.8843722655819,-6.12431917249484,127.942928205157));
#215106=CARTESIAN_POINT('Ctrl Pts',(3.05168912681027,-6.04268832278763,
127.951677842926));
#215107=CARTESIAN_POINT('Ctrl Pts',(3.21535986273929,-5.95430516123294,
127.960427480695));
#215108=CARTESIAN_POINT('Ctrl Pts',(3.37902914072932,-5.86592278697389,
127.969177040524));
#215109=CARTESIAN_POINT('Ctrl Pts',(3.53905210621676,-5.77078835741878,
127.977926600353));
#215110=CARTESIAN_POINT('Ctrl Pts',(3.69488522831815,-5.66922500431553,
127.986676160182));
#215111=CARTESIAN_POINT('Ctrl Pts',(3.8507170140707,-5.56766252217004,127.995425644979));
#215112=CARTESIAN_POINT('Ctrl Pts',(4.00235878822546,-5.45967138329266,
128.004175129776));
#215113=CARTESIAN_POINT('Ctrl Pts',(4.14929549611478,-5.34561838199488,
128.012924614573));
#215114=CARTESIAN_POINT('Ctrl Pts',(4.29623099276244,-5.23156632086889,
128.021674027246));
#215115=CARTESIAN_POINT('Ctrl Pts',(4.43846127436184,-5.11145267304829,
128.030423439918));
#215116=CARTESIAN_POINT('Ctrl Pts',(4.57550326054599,-4.98568540049741,
128.039172852591));
#215117=CARTESIAN_POINT('Ctrl Pts',(4.7125441625794,-4.85991912290207,128.047922196046));
#215118=CARTESIAN_POINT('Ctrl Pts',(4.84439664018921,-4.72849950385255,
128.056671539501));
#215119=CARTESIAN_POINT('Ctrl Pts',(4.97061286794906,-4.59187289860894,
128.065420882957));
#215120=CARTESIAN_POINT('Ctrl Pts',(5.09682813912843,-4.45524732884504,
128.074170160101));
#215121=CARTESIAN_POINT('Ctrl Pts',(5.21740705147994,-4.313415062356,128.082919437246));
#215122=CARTESIAN_POINT('Ctrl Pts',(5.33194007545848,-4.1668578127553,128.091668714391));
#215123=CARTESIAN_POINT('Ctrl Pts',(5.44647226944626,-4.0203016252165,128.100417928132));
#215124=CARTESIAN_POINT('Ctrl Pts',(5.55495848628244,-3.86902074887746,
128.109167141873));
#215125=CARTESIAN_POINT('Ctrl Pts',(5.65703027291908,-3.71352898080479,
128.117916355615));
#215126=CARTESIAN_POINT('Ctrl Pts',(5.75910135377118,-3.55803828789393,
128.126665508858));
#215127=CARTESIAN_POINT('Ctrl Pts',(5.85475793592873,-3.39833700106505,
128.135414662102));
#215128=CARTESIAN_POINT('Ctrl Pts',(5.94367514427518,-3.23496750823335,
128.144163815346));
#215129=CARTESIAN_POINT('Ctrl Pts',(6.03259176732757,-3.07159909077495,
128.152912910999));
#215130=CARTESIAN_POINT('Ctrl Pts',(6.11476896836039,-2.90456276731193,
128.161662006652));
#215131=CARTESIAN_POINT('Ctrl Pts',(6.18992765547998,-2.73442583002797,
128.170411102305));
#215132=CARTESIAN_POINT('Ctrl Pts',(6.26508587283162,-2.56428995615908,
128.179160143273));
#215133=CARTESIAN_POINT('Ctrl Pts',(6.33322554827263,-2.3910537693493,128.187909184241));
#215134=CARTESIAN_POINT('Ctrl Pts',(6.39411526733128,-2.21530561053799,
128.196658225209));
#215135=CARTESIAN_POINT('Ctrl Pts',(6.45500462602938,-2.03955849184812,
128.205407214398));
#215136=CARTESIAN_POINT('Ctrl Pts',(6.50864402040824,-1.86129970164252,
128.214156203587));
#215137=CARTESIAN_POINT('Ctrl Pts',(6.55485128368677,-1.68113463135761,
128.222905192776));
#215138=CARTESIAN_POINT('Ctrl Pts',(6.60199809554389,-1.4973062011659,128.231832078248));
#215139=CARTESIAN_POINT('Ctrl Pts',(6.64140720707924,-1.3114934324544,128.240758963719));
#215140=CARTESIAN_POINT('Ctrl Pts',(6.67293928722924,-1.12435326697288,
128.24968584919));
#215141=CARTESIAN_POINT('Ctrl Pts',(6.7038462587629,-0.940923067004233,
128.258435763368));
#215142=CARTESIAN_POINT('Ctrl Pts',(6.72718554579822,-0.756217899519327,
128.267185677545));
#215143=CARTESIAN_POINT('Ctrl Pts',(6.74287786815347,-0.570865181252181,
128.275935591723));
#215144=CARTESIAN_POINT('Ctrl Pts',(6.75856988190858,-0.385516108071698,
128.284685333827));
#215145=CARTESIAN_POINT('Ctrl Pts',(6.76661520773409,-0.19951979522417,
128.293435075932));
#215146=CARTESIAN_POINT('Ctrl Pts',(6.76698651789579,-0.013508020453543,
128.302184818036));
#215147=CARTESIAN_POINT('Ctrl Pts',(6.76735782124897,0.172500343514992,
128.310934399701));
#215148=CARTESIAN_POINT('Ctrl Pts',(6.76005538995173,0.358523882212877,
128.319683981366));
#215149=CARTESIAN_POINT('Ctrl Pts',(6.74510402742346,0.543930748566255,
128.328433563031));
#215150=CARTESIAN_POINT('Ctrl Pts',(6.7301529191801,0.729334461617104,128.337182995888));
#215151=CARTESIAN_POINT('Ctrl Pts',(6.70755316306569,0.914121237636537,
128.345932428745));
#215152=CARTESIAN_POINT('Ctrl Pts',(6.67738151874544,1.09766345166306,128.354681861601));
#215153=CARTESIAN_POINT('Ctrl Pts',(6.64721034747534,1.28120278799847,128.363431157279));
#215154=CARTESIAN_POINT('Ctrl Pts',(6.60946757205101,1.46349731860511,128.372180452956));
#215155=CARTESIAN_POINT('Ctrl Pts',(6.56428138111478,1.64392790278342,128.380929748634));
#215156=CARTESIAN_POINT('Ctrl Pts',(6.51909583859801,1.82435589779231,128.389678918759));
#215157=CARTESIAN_POINT('Ctrl Pts',(6.46646716392823,2.00291972192435,128.398428088885));
#215158=CARTESIAN_POINT('Ctrl Pts',(6.40657409872828,2.17901292274827,128.407177259011));
#215159=CARTESIAN_POINT('Ctrl Pts',(6.34668181342021,2.35510383059125,128.41592631521));
#215160=CARTESIAN_POINT('Ctrl Pts',(6.27952541913996,2.52872390822712,128.424675371409));
#215161=CARTESIAN_POINT('Ctrl Pts',(6.20533299175466,2.69928350890402,128.433424427608));
#215162=CARTESIAN_POINT('Ctrl Pts',(6.12831602991496,2.87633637965736,128.442506563766));
#215163=CARTESIAN_POINT('Ctrl Pts',(6.04371690605215,3.0500908660157,128.451588699924));
#215164=CARTESIAN_POINT('Ctrl Pts',(5.95184520316575,3.21991112882838,128.460670836082));
#215165=CARTESIAN_POINT('Ctrl Pts',(5.86333549509214,3.38351691183122,128.469420616426));
#215166=CARTESIAN_POINT('Ctrl Pts',(5.76807618099303,3.5434710371211,128.47817039677));
#215167=CARTESIAN_POINT('Ctrl Pts',(5.66639083308946,3.69923018027802,128.486920177113));
#215168=CARTESIAN_POINT('Ctrl Pts',(5.56470914082125,3.85498372382159,128.495669642898));
#215169=CARTESIAN_POINT('Ctrl Pts',(5.45660203371985,4.0065423470211,128.504419108683));
#215170=CARTESIAN_POINT('Ctrl Pts',(5.34243669839128,4.15339127986783,128.513168574468));
#215171=CARTESIAN_POINT('Ctrl Pts',(5.22827486050494,4.30023571401398,128.521917772214));
#215172=CARTESIAN_POINT('Ctrl Pts',(5.10805534167005,4.44237052028592,128.53066696996));
#215173=CARTESIAN_POINT('Ctrl Pts',(4.98218644339836,4.57931296628847,128.539416167706));
#215174=CARTESIAN_POINT('Ctrl Pts',(4.85632073219448,4.71625194483504,128.548165143918));
#215175=CARTESIAN_POINT('Ctrl Pts',(4.72480612170155,4.84799861524669,128.556914120129));
#215176=CARTESIAN_POINT('Ctrl Pts',(4.58808925235122,4.9741055489866,128.565663096341));
#215177=CARTESIAN_POINT('Ctrl Pts',(4.45136349473857,5.10022068121373,128.574412641343));
#215178=CARTESIAN_POINT('Ctrl Pts',(4.30943501209888,5.22069514871992,128.583162186344));
#215179=CARTESIAN_POINT('Ctrl Pts',(4.16278587431589,5.33511975166407,128.591911731346));
#215180=CARTESIAN_POINT('Ctrl Pts',(4.01614535740256,5.44953762807983,128.600660762));
#215181=CARTESIAN_POINT('Ctrl Pts',(3.86478496657733,5.55790617532915,128.609409792653));
#215182=CARTESIAN_POINT('Ctrl Pts',(3.70921874747008,5.65985735539479,128.618158823307));
#215183=CARTESIAN_POINT('Ctrl Pts',(3.55365041605714,5.76180991977161,128.626907972757));
#215184=CARTESIAN_POINT('Ctrl Pts',(3.39387638174338,5.8573447855292,128.635657122206));
#215185=CARTESIAN_POINT('Ctrl Pts',(3.23043927904357,5.94613749121331,128.644406271656));
#215186=CARTESIAN_POINT('Ctrl Pts',(3.1869176707031,5.96978206944211,128.646736079572));
#215187=CARTESIAN_POINT('Ctrl Pts',(3.14313645919572,5.99294880633455,128.649065887488));
#215188=CARTESIAN_POINT('Ctrl Pts',(3.09910619832143,6.01563211736935,128.651395695404));
#215189=CARTESIAN_POINT('Origin',(0.,0.,4.30282021618968));
#215190=CARTESIAN_POINT('',(3.09910619832127,6.01563211736944,131.045783168526));
#215191=CARTESIAN_POINT('',(3.0991061983213,6.01563211736942,130.651283639301));
#215192=CARTESIAN_POINT('',(3.09910619832133,6.0156321173694,4.30282021618968));
#215193=CARTESIAN_POINT('',(-6.76699967917944,-0.00208374312542183,129.697179783778));
#215194=CARTESIAN_POINT('Ctrl Pts',(-6.76699967917923,-0.00208374379854805,
129.69717978381));
#215195=CARTESIAN_POINT('Ctrl Pts',(-6.766929895115,-0.228708888680955,
129.707858586294));
#215196=CARTESIAN_POINT('Ctrl Pts',(-6.7554715143949,-0.455087020649597,
129.718537388777));
#215197=CARTESIAN_POINT('Ctrl Pts',(-6.7327234342321,-0.680238309816426,
129.729216191261));
#215198=CARTESIAN_POINT('Ctrl Pts',(-6.72906175718189,-0.716480107034841,
129.730935119878));
#215199=CARTESIAN_POINT('Ctrl Pts',(-6.72510766844374,-0.75269014195336,
129.732654048496));
#215200=CARTESIAN_POINT('Ctrl Pts',(-6.72086170282627,-0.788864355566378,
129.734372977113));
#215201=CARTESIAN_POINT('Ctrl Pts',(-6.70031948464487,-0.963877216132726,
129.742689249517));
#215202=CARTESIAN_POINT('Ctrl Pts',(-6.67291698920661,-1.13825686304642,
129.751005521921));
#215203=CARTESIAN_POINT('Ctrl Pts',(-6.63870684167096,-1.31143450860163,
129.759321794325));
#215204=CARTESIAN_POINT('Ctrl Pts',(-6.60452561885537,-1.48446573225344,
129.767631035311));
#215205=CARTESIAN_POINT('Ctrl Pts',(-6.56354827886101,-1.65629663975404,
129.775940276297));
#215206=CARTESIAN_POINT('Ctrl Pts',(-6.5158790831247,-1.82636490715793,
129.784249517283));
#215207=CARTESIAN_POINT('Ctrl Pts',(-6.46824145177365,-1.99632056304762,
129.792553256265));
#215208=CARTESIAN_POINT('Ctrl Pts',(-6.41392088762249,-2.1645155705911,
129.800856995247));
#215209=CARTESIAN_POINT('Ctrl Pts',(-6.35307248181565,-2.33039890164683,
129.80916073423));
#215210=CARTESIAN_POINT('Ctrl Pts',(-6.29225321569742,-2.49620279284627,
129.817460496635));
#215211=CARTESIAN_POINT('Ctrl Pts',(-6.22491245751344,-2.659696887782,129.825760259041));
#215212=CARTESIAN_POINT('Ctrl Pts',(-6.15125486270707,-2.82034618691086,
129.834060021446));
#215213=CARTESIAN_POINT('Ctrl Pts',(-6.07761904748579,-2.98094798414818,
129.842357329721));
#215214=CARTESIAN_POINT('Ctrl Pts',(-5.9976702635514,-3.13870634635862,
129.850654637995));
#215215=CARTESIAN_POINT('Ctrl Pts',(-5.91166101819438,-3.29310689258047,
129.85895194627));
#215216=CARTESIAN_POINT('Ctrl Pts',(-5.82564308285061,-3.44752303873809,
129.867250092867));
#215217=CARTESIAN_POINT('Ctrl Pts',(-5.73356362529532,-3.59858038339801,
129.875548239464));
#215218=CARTESIAN_POINT('Ctrl Pts',(-5.63572105690231,-3.74578925845915,
129.883846386061));
#215219=CARTESIAN_POINT('Ctrl Pts',(-5.53786864982352,-3.89301293629877,
129.892145367089));
#215220=CARTESIAN_POINT('Ctrl Pts',(-5.43425216905738,-4.03638708295056,
129.900444348117));
#215221=CARTESIAN_POINT('Ctrl Pts',(-5.32521324676965,-4.17545121830312,
129.908743329145));
#215222=CARTESIAN_POINT('Ctrl Pts',(-5.21614523889757,-4.31455244831467,
129.917044523884));
#215223=CARTESIAN_POINT('Ctrl Pts',(-5.10165212143132,-4.44934110171576,
129.925345718624));
#215224=CARTESIAN_POINT('Ctrl Pts',(-4.98211578975548,-4.57938983462526,
129.933646913363));
#215225=CARTESIAN_POINT('Ctrl Pts',(-4.86252770444059,-4.70949487255171,
129.941951702132));
#215226=CARTESIAN_POINT('Ctrl Pts',(-4.7378922885946,-4.83485564394035,
129.9502564909));
#215227=CARTESIAN_POINT('Ctrl Pts',(-4.60862837475821,-4.95508158392711,
129.958561279669));
#215228=CARTESIAN_POINT('Ctrl Pts',(-4.47921121971277,-5.07545005068607,
129.96687591369));
#215229=CARTESIAN_POINT('Ctrl Pts',(-4.34515485875983,-5.19067128645063,
129.975190547711));
#215230=CARTESIAN_POINT('Ctrl Pts',(-4.20691220275123,-5.30039420405151,
129.983505181732));
#215231=CARTESIAN_POINT('Ctrl Pts',(-4.06858213468563,-5.41018650042595,
129.991825073169));
#215232=CARTESIAN_POINT('Ctrl Pts',(-3.92606077318695,-5.51447334014883,
130.000144964607));
#215233=CARTESIAN_POINT('Ctrl Pts',(-3.77983021009384,-5.6129468715517,
130.008464856045));
#215234=CARTESIAN_POINT('Ctrl Pts',(-3.63338098489388,-5.7115676528139,
130.016797188418));
#215235=CARTESIAN_POINT('Ctrl Pts',(-3.48321176947096,-5.80435757049047,
130.025129520791));
#215236=CARTESIAN_POINT('Ctrl Pts',(-3.32983063984619,-5.89105397275747,
130.033461853164));
#215237=CARTESIAN_POINT('Ctrl Pts',(-3.21435234070656,-5.95632636382545,
130.039735138363));
#215238=CARTESIAN_POINT('Ctrl Pts',(-3.09705393676772,-6.01814568291422,
130.046008423563));
#215239=CARTESIAN_POINT('Ctrl Pts',(-2.97815948344666,-6.07641794901871,
130.052281708762));
#215240=CARTESIAN_POINT('Ctrl Pts',(-2.82521570702387,-6.15137838821319,
130.060351554765));
#215241=CARTESIAN_POINT('Ctrl Pts',(-2.6691574779838,-6.22069900745924,
130.068421400769));
#215242=CARTESIAN_POINT('Ctrl Pts',(-2.51044765573,-6.28410228814265,130.076491246772));
#215243=CARTESIAN_POINT('Ctrl Pts',(-2.35193751061973,-6.34742579943437,
130.084550939882));
#215244=CARTESIAN_POINT('Ctrl Pts',(-2.19078275215329,-6.40484664854533,
130.092610632993));
#215245=CARTESIAN_POINT('Ctrl Pts',(-2.02747193673638,-6.45613247585166,
130.100670326104));
#215246=CARTESIAN_POINT('Ctrl Pts',(-1.86433074554019,-6.50736503468052,
130.108721647943));
#215247=CARTESIAN_POINT('Ctrl Pts',(-1.69903830676271,-6.55247514160329,
130.116772969782));
#215248=CARTESIAN_POINT('Ctrl Pts',(-1.53210422535143,-6.59127799767695,
130.124824291621));
#215249=CARTESIAN_POINT('Ctrl Pts',(-1.3653069505528,-6.63004905384939,
130.132869015203));
#215250=CARTESIAN_POINT('Ctrl Pts',(-1.19687107238559,-6.66252306300127,
130.140913738784));
#215251=CARTESIAN_POINT('Ctrl Pts',(-1.02732237117795,-6.68856469996944,
130.148958462366));
#215252=CARTESIAN_POINT('Ctrl Pts',(-0.857875505044011,-6.71459069569708,
130.156998354091));
#215253=CARTESIAN_POINT('Ctrl Pts',(-0.687317514268115,-6.73419195365595,
130.165038245816));
#215254=CARTESIAN_POINT('Ctrl Pts',(-0.516185308803933,-6.74728402596,130.173078137541));
#215255=CARTESIAN_POINT('Ctrl Pts',(-0.341368158127535,-6.7606580064474,
130.18129115016));
#215256=CARTESIAN_POINT('Ctrl Pts',(-0.165952171610317,-6.76723920980045,
130.18950416278));
#215257=CARTESIAN_POINT('Ctrl Pts',(0.00948324521950484,-6.76699335510684,
130.197717175399));
#215258=CARTESIAN_POINT('Ctrl Pts',(0.18116076394389,-6.76675276672093,
130.205754261942));
#215259=CARTESIAN_POINT('Ctrl Pts',(0.352856500310551,-6.75997464784988,
130.213791348486));
#215260=CARTESIAN_POINT('Ctrl Pts',(0.524026562454356,-6.74667956567097,
130.221828435029));
#215261=CARTESIAN_POINT('Ctrl Pts',(0.695213006369794,-6.73338321109083,
130.229866290758));
#215262=CARTESIAN_POINT('Ctrl Pts',(0.865873303362873,-6.7135686801116,
130.237904146488));
#215263=CARTESIAN_POINT('Ctrl Pts',(1.03546812106564,-6.68730848475355,
130.245942002218));
#215264=CARTESIAN_POINT('Ctrl Pts',(1.20511277217761,-6.66104057315111,
130.253982219775));
#215265=CARTESIAN_POINT('Ctrl Pts',(1.37369095181014,-6.62832328440613,
130.262022437333));
#215266=CARTESIAN_POINT('Ctrl Pts',(1.54067311238569,-6.58928033709083,
130.27006265489));
#215267=CARTESIAN_POINT('Ctrl Pts',(1.71396396594366,-6.54876232221805,
130.278406637017));
#215268=CARTESIAN_POINT('Ctrl Pts',(1.88553541427208,-6.5014314391498,130.286750619144));
#215269=CARTESIAN_POINT('Ctrl Pts',(2.05481349248203,-6.44748249405253,
130.29509460127));
#215270=CARTESIAN_POINT('Ctrl Pts',(2.21821293271889,-6.39540707162642,
130.303148816106));
#215271=CARTESIAN_POINT('Ctrl Pts',(2.37947529598631,-6.33716572883949,
130.311203030942));
#215272=CARTESIAN_POINT('Ctrl Pts',(2.53810585416862,-6.27298235873775,
130.319257245777));
#215273=CARTESIAN_POINT('Ctrl Pts',(2.6968551210923,-6.20875095799696,130.327317487861));
#215274=CARTESIAN_POINT('Ctrl Pts',(2.85296832305128,-6.13856882827507,
130.335377729944));
#215275=CARTESIAN_POINT('Ctrl Pts',(3.0059757622498,-6.06270556078445,130.343437972028));
#215276=CARTESIAN_POINT('Ctrl Pts',(3.15919711634376,-5.98673623124209,
130.351509482883));
#215277=CARTESIAN_POINT('Ctrl Pts',(3.30930371942944,-5.90507009388891,
130.359580993738));
#215278=CARTESIAN_POINT('Ctrl Pts',(3.45585475290609,-5.8180200177394,130.367652504592));
#215279=CARTESIAN_POINT('Ctrl Pts',(3.47121483124572,-5.80889626093328,
130.368498483199));
#215280=CARTESIAN_POINT('Ctrl Pts',(3.48653588109474,-5.79971339654704,
130.369344461805));
#215281=CARTESIAN_POINT('Ctrl Pts',(3.50181741651349,-5.79047180991349,
130.370190440411));
#215282=CARTESIAN_POINT('Ctrl Pts',(3.65046842301036,-5.70057435412382,
130.378419690146));
#215283=CARTESIAN_POINT('Ctrl Pts',(3.7958739130941,-5.60481694627283,130.386648939882));
#215284=CARTESIAN_POINT('Ctrl Pts',(3.93754041277494,-5.5034593209875,130.394878189617));
#215285=CARTESIAN_POINT('Ctrl Pts',(4.07903830627505,-5.40222232776499,
130.403097645206));
#215286=CARTESIAN_POINT('Ctrl Pts',(4.21680578145831,-5.29539859547242,
130.411317100796));
#215287=CARTESIAN_POINT('Ctrl Pts',(4.35037474427182,-5.18329321806146,
130.419536556385));
#215288=CARTESIAN_POINT('Ctrl Pts',(4.48381156222443,-5.07129875076907,
130.427747880154));
#215289=CARTESIAN_POINT('Ctrl Pts',(4.61305786707213,-4.95403327344411,
130.435959203923));
#215290=CARTESIAN_POINT('Ctrl Pts',(4.73767523971573,-4.83184460873738,
130.444170527692));
#215291=CARTESIAN_POINT('Ctrl Pts',(4.86219434083499,-4.70975230030975,
130.452375376125));
#215292=CARTESIAN_POINT('Ctrl Pts',(4.98209152537206,-4.58274478719232,
130.460580224558));
#215293=CARTESIAN_POINT('Ctrl Pts',(5.09696206426688,-4.45120957891497,
130.468785072992));
#215294=CARTESIAN_POINT('Ctrl Pts',(5.21176507239897,-4.31975169832341,
130.476985097911));
#215295=CARTESIAN_POINT('Ctrl Pts',(5.32154708645066,-4.18377169449091,
130.48518512283));
#215296=CARTESIAN_POINT('Ctrl Pts',(5.42594076321777,-4.0436933407532,130.493385147749));
#215297=CARTESIAN_POINT('Ctrl Pts',(5.53030422608991,-3.90365552886437,
130.501582799396));
#215298=CARTESIAN_POINT('Ctrl Pts',(5.62928224079385,-3.75952201458261,
130.509780451042));
#215299=CARTESIAN_POINT('Ctrl Pts',(5.72254809659069,-3.61174919979313,
130.517978102688));
#215300=CARTESIAN_POINT('Ctrl Pts',(5.81580146351725,-3.46399617269014,
130.526174656619));
#215301=CARTESIAN_POINT('Ctrl Pts',(5.90334400279473,-3.31260511847879,
130.534371210549));
#215302=CARTESIAN_POINT('Ctrl Pts',(5.98489265618446,-3.1580609389227,130.542567764479));
#215303=CARTESIAN_POINT('Ctrl Pts',(6.06644521737349,-3.00350935363261,
130.550764711187));
#215304=CARTESIAN_POINT('Ctrl Pts',(6.14200315296424,-2.8458046592573,130.558961657895));
#215305=CARTESIAN_POINT('Ctrl Pts',(6.21132962421336,-2.68545588296838,
130.567158604603));
#215306=CARTESIAN_POINT('Ctrl Pts',(6.28067202290252,-2.5250702672807,130.575357434522));
#215307=CARTESIAN_POINT('Ctrl Pts',(6.34377996349516,-2.36203968901357,
130.583556264442));
#215308=CARTESIAN_POINT('Ctrl Pts',(6.40046494410733,-2.19689269179294,
130.591755094361));
#215309=CARTESIAN_POINT('Ctrl Pts',(6.45720361264282,-2.03158927925332,
130.59996168962));
#215310=CARTESIAN_POINT('Ctrl Pts',(6.50750705057403,-1.86416578267499,
130.608168284879));
#215311=CARTESIAN_POINT('Ctrl Pts',(6.55123653024521,-1.69516634133078,
130.616374880138));
#215312=CARTESIAN_POINT('Ctrl Pts',(6.59498717523529,-1.5260851032879,130.624585447437));
#215313=CARTESIAN_POINT('Ctrl Pts',(6.63215744184712,-1.35542675002679,
130.632796014735));
#215314=CARTESIAN_POINT('Ctrl Pts',(6.66265988019255,-1.18374504048491,
130.641006582033));
#215315=CARTESIAN_POINT('Ctrl Pts',(6.69320438576726,-1.01182655728721,
130.649228472879));
#215316=CARTESIAN_POINT('Ctrl Pts',(6.71706263598801,-0.838882252680426,
130.657450363725));
#215317=CARTESIAN_POINT('Ctrl Pts',(6.73419902221055,-0.665471659245134,
130.665672254571));
#215318=CARTESIAN_POINT('Ctrl Pts',(6.74978004151143,-0.507800504533539,
130.673147893735));
#215319=CARTESIAN_POINT('Ctrl Pts',(6.75980467048279,-0.349744100864699,
130.680623532898));
#215320=CARTESIAN_POINT('Ctrl Pts',(6.76428353672316,-0.191721764064525,
130.688099172061));
#215321=CARTESIAN_POINT('Ctrl Pts',(6.76963731244371,-0.00283107060319224,
130.697035115512));
#215322=CARTESIAN_POINT('Ctrl Pts',(6.76707809647515,0.186404318632308,
130.705971058963));
#215323=CARTESIAN_POINT('Ctrl Pts',(6.75658311908621,0.375331260194678,
130.714907002414));
#215324=CARTESIAN_POINT('Ctrl Pts',(6.74610391843197,0.563974194452848,
130.723829512771));
#215325=CARTESIAN_POINT('Ctrl Pts',(6.72771277420276,0.752309349020713,
130.732752023129));
#215326=CARTESIAN_POINT('Ctrl Pts',(6.70143889179924,0.939683872097727,
130.741674533487));
#215327=CARTESIAN_POINT('Ctrl Pts',(6.67522938856135,1.12659926944415,130.750575180925));
#215328=CARTESIAN_POINT('Ctrl Pts',(6.64117573255837,1.3125584779172,130.759475828363));
#215329=CARTESIAN_POINT('Ctrl Pts',(6.59935871645636,1.4969146707583,130.768376475802));
#215330=CARTESIAN_POINT('Ctrl Pts',(6.55760632339184,1.6809859638559,130.777263368388));
#215331=CARTESIAN_POINT('Ctrl Pts',(6.50811455855815,1.86345893226053,130.786150260974));
#215332=CARTESIAN_POINT('Ctrl Pts',(6.45101544745625,2.04369486388767,130.79503715356));
#215333=CARTESIAN_POINT('Ctrl Pts',(6.39406310238482,2.22346752188896,130.803901203515));
#215334=CARTESIAN_POINT('Ctrl Pts',(6.32954250688506,2.40101437146873,130.81276525347));
#215335=CARTESIAN_POINT('Ctrl Pts',(6.25763565836037,2.57571057520381,130.821629303425));
#215336=CARTESIAN_POINT('Ctrl Pts',(6.18888692666369,2.74273419931505,130.830104048245));
#215337=CARTESIAN_POINT('Ctrl Pts',(6.11338685668269,2.9071519374485,130.838578793066));
#215338=CARTESIAN_POINT('Ctrl Pts',(6.03133770514296,3.06842866733461,130.847053537886));
#215339=CARTESIAN_POINT('Ctrl Pts',(5.95186221903356,3.22464657166756,130.855262452319));
#215340=CARTESIAN_POINT('Ctrl Pts',(5.86631780649796,3.37776640094225,130.863471366751));
#215341=CARTESIAN_POINT('Ctrl Pts',(5.77498525549678,3.52729844198003,130.871680281184));
#215342=CARTESIAN_POINT('Ctrl Pts',(5.68363099064509,3.67686603350175,130.879891147244));
#215343=CARTESIAN_POINT('Ctrl Pts',(5.58648603136028,3.82284383352606,130.888102013305));
#215344=CARTESIAN_POINT('Ctrl Pts',(5.48387501293507,3.96477033918818,130.896312879365));
#215345=CARTESIAN_POINT('Ctrl Pts',(5.38122130841649,4.10675588615177,130.904527161138));
#215346=CARTESIAN_POINT('Ctrl Pts',(5.27309722317379,4.24468649288527,130.912741442912));
#215347=CARTESIAN_POINT('Ctrl Pts',(5.15986829629692,4.37813295422489,130.920955724685));
#215348=CARTESIAN_POINT('Ctrl Pts',(5.04651192132337,4.5117296200924,130.929179252281));
#215349=CARTESIAN_POINT('Ctrl Pts',(4.92803945872198,4.64083178790609,130.937402779877));
#215350=CARTESIAN_POINT('Ctrl Pts',(4.80485466955577,4.76504570853713,130.945626307473));
#215351=CARTESIAN_POINT('Ctrl Pts',(4.68159092373097,4.88933924546,130.953855106031));
#215352=CARTESIAN_POINT('Ctrl Pts',(4.55360909002018,5.00873804713577,130.962083904588));
#215353=CARTESIAN_POINT('Ctrl Pts',(4.42134670437477,5.12288808385605,130.970312703145));
#215354=CARTESIAN_POINT('Ctrl Pts',(4.28890227013917,5.23719523896758,130.978552827985));
#215355=CARTESIAN_POINT('Ctrl Pts',(4.15216579314281,5.34623897747476,130.986792952826));
#215356=CARTESIAN_POINT('Ctrl Pts',(4.01160532518633,5.4497074889334,130.995033077666));
#215357=CARTESIAN_POINT('Ctrl Pts',(3.94920227852705,5.49564323774093,130.998691353014));
#215358=CARTESIAN_POINT('Ctrl Pts',(3.88604587658117,5.54048070588965,131.002349628362));
#215359=CARTESIAN_POINT('Ctrl Pts',(3.82217864206139,5.58419550411424,131.006007903711));
#215360=CARTESIAN_POINT('Ctrl Pts',(3.67469067372378,5.68514565210346,131.014455922524));
#215361=CARTESIAN_POINT('Ctrl Pts',(3.5230728080901,5.78033677462241,131.022903941336));
#215362=CARTESIAN_POINT('Ctrl Pts',(3.3678025770459,5.86942883098884,131.031351960149));
#215363=CARTESIAN_POINT('Ctrl Pts',(3.27938985336079,5.92015891175893,131.036162362942));
#215364=CARTESIAN_POINT('Ctrl Pts',(3.1897935246329,5.96891222998303,131.040972765734));
#215365=CARTESIAN_POINT('Ctrl Pts',(3.09910619832127,6.01563211736944,131.045783168526));
#215366=CARTESIAN_POINT('Ctrl Pts',(3.09910619832118,6.01563211736948,129.045766611327));
#215367=CARTESIAN_POINT('Ctrl Pts',(2.93295980831911,6.10122666454888,129.054564761741));
#215368=CARTESIAN_POINT('Ctrl Pts',(2.76334723714547,6.17989107528915,129.063362912156));
#215369=CARTESIAN_POINT('Ctrl Pts',(2.59088386661367,6.25136863332511,129.07216106257));
#215370=CARTESIAN_POINT('Ctrl Pts',(2.41842049608198,6.32284619136102,129.080959212985));
#215371=CARTESIAN_POINT('Ctrl Pts',(2.24310672167691,6.38713678290893,129.089757363399));
#215372=CARTESIAN_POINT('Ctrl Pts',(2.06557696693954,6.44404227124938,129.098555513813));
#215373=CARTESIAN_POINT('Ctrl Pts',(1.90133317189418,6.49668907052971,129.106695228846));
#215374=CARTESIAN_POINT('Ctrl Pts',(1.73486519293263,6.54311981293916,129.114834943879));
#215375=CARTESIAN_POINT('Ctrl Pts',(1.56668894480396,6.58314322723037,129.122974658912));
#215376=CARTESIAN_POINT('Ctrl Pts',(1.39865978261292,6.62313163728356,129.131107254999));
#215377=CARTESIAN_POINT('Ctrl Pts',(1.22892567895543,6.65672378936519,129.139239851086));
#215378=CARTESIAN_POINT('Ctrl Pts',(1.05801921841487,6.6837776992854,129.147372447173));
#215379=CARTESIAN_POINT('Ctrl Pts',(0.887229598699516,6.7108131137014,129.155499483381));
#215380=CARTESIAN_POINT('Ctrl Pts',(0.715269578040404,6.73131912826273,
129.16362651959));
#215381=CARTESIAN_POINT('Ctrl Pts',(0.542683447704755,6.74520449471973,
129.171753555798));
#215382=CARTESIAN_POINT('Ctrl Pts',(0.370179816662838,6.75908322372027,
129.179876707135));
#215383=CARTESIAN_POINT('Ctrl Pts',(0.197051036185945,6.76634757744501,
129.187999858473));
#215384=CARTESIAN_POINT('Ctrl Pts',(0.023848042362166,6.76695797762004,
129.196123009811));
#215385=CARTESIAN_POINT('Ctrl Pts',(-0.149306280132994,6.76756820626809,
129.204243878482));
#215386=CARTESIAN_POINT('Ctrl Pts',(-0.322534408546306,6.76152820516158,
129.212364747154));
#215387=CARTESIAN_POINT('Ctrl Pts',(-0.495283907157348,6.74885048369802,
129.220485615826));
#215388=CARTESIAN_POINT('Ctrl Pts',(-0.668042741812549,6.73617207708186,
129.228606923381));
#215389=CARTESIAN_POINT('Ctrl Pts',(-0.840322529454317,6.71685525627807,
129.236728230935));
#215390=CARTESIAN_POINT('Ctrl Pts',(-1.0115742687147,6.69096454174391,129.24484953849));
#215391=CARTESIAN_POINT('Ctrl Pts',(-1.10056262544168,6.67751082646585,
129.249069652206));
#215392=CARTESIAN_POINT('Ctrl Pts',(-1.18927348003949,6.66228287926408,
129.253289765922));
#215393=CARTESIAN_POINT('Ctrl Pts',(-1.27763067473819,6.64529524242287,
129.257509879638));
#215394=CARTESIAN_POINT('Ctrl Pts',(-1.46573929868794,6.60912930255511,
129.266494318163));
#215395=CARTESIAN_POINT('Ctrl Pts',(-1.65215115647333,6.56500276800371,
129.275478756689));
#215396=CARTESIAN_POINT('Ctrl Pts',(-1.83622366294872,6.51310768064118,
129.284463195214));
#215397=CARTESIAN_POINT('Ctrl Pts',(-2.02061386758355,6.46112302545534,
129.293463140344));
#215398=CARTESIAN_POINT('Ctrl Pts',(-2.20265642084614,6.40134308321685,
129.302463085474));
#215399=CARTESIAN_POINT('Ctrl Pts',(-2.38172547904874,6.33400921553245,
129.311463030604));
#215400=CARTESIAN_POINT('Ctrl Pts',(-2.56121651808352,6.26651667386047,
129.320484184336));
#215401=CARTESIAN_POINT('Ctrl Pts',(-2.73771981737689,6.19143467424104,
129.329505338068));
#215402=CARTESIAN_POINT('Ctrl Pts',(-2.91062850105638,6.10905317777136,
129.3385264918));
#215403=CARTESIAN_POINT('Ctrl Pts',(-3.08371312068443,6.02658785747966,
129.347556824627));
#215404=CARTESIAN_POINT('Ctrl Pts',(-3.25319560486031,5.9368083105328,129.356587157453));
#215405=CARTESIAN_POINT('Ctrl Pts',(-3.41849375635632,5.84005046534299,
129.36561749028));
#215406=CARTESIAN_POINT('Ctrl Pts',(-3.58402624852605,5.7431554480286,129.374660625272));
#215407=CARTESIAN_POINT('Ctrl Pts',(-3.74536234037392,5.63926247190385,
129.383703760265));
#215408=CARTESIAN_POINT('Ctrl Pts',(-3.9019469282076,5.5287520444899,129.392746895257));
#215409=CARTESIAN_POINT('Ctrl Pts',(-4.03883793299568,5.43214047078686,
129.400652678659));
#215410=CARTESIAN_POINT('Ctrl Pts',(-4.17209783550899,5.33047203388531,
129.408558462061));
#215411=CARTESIAN_POINT('Ctrl Pts',(-4.30137593202846,5.2240266166403,129.416464245463));
#215412=CARTESIAN_POINT('Ctrl Pts',(-4.44287912048788,5.10751526365335,
129.425117633692));
#215413=CARTESIAN_POINT('Ctrl Pts',(-4.57973600641257,4.9851768166606,129.433771021921));
#215414=CARTESIAN_POINT('Ctrl Pts',(-4.71147028346091,4.85740020670161,
129.442424410149));
#215415=CARTESIAN_POINT('Ctrl Pts',(-4.8430828945598,4.72974160750577,129.45106980636));
#215416=CARTESIAN_POINT('Ctrl Pts',(-4.96958211557801,4.59665507382547,
129.459715202571));
#215417=CARTESIAN_POINT('Ctrl Pts',(-5.09052595749893,4.45856865776783,
129.468360598782));
#215418=CARTESIAN_POINT('Ctrl Pts',(-5.21533233830668,4.31607222675371,
129.477282099824));
#215419=CARTESIAN_POINT('Ctrl Pts',(-5.33422236960563,4.16825146843598,
129.486203600867));
#215420=CARTESIAN_POINT('Ctrl Pts',(-5.44675115624527,4.01561836358248,
129.495125101909));
#215421=CARTESIAN_POINT('Ctrl Pts',(-5.5555896865386,3.86799069156676,129.503754032251));
#215422=CARTESIAN_POINT('Ctrl Pts',(-5.65847736139182,3.71586155715784,
129.512382962594));
#215423=CARTESIAN_POINT('Ctrl Pts',(-5.75505186027942,3.55972851289174,
129.521011892936));
#215424=CARTESIAN_POINT('Ctrl Pts',(-5.85653801117727,3.39565474732168,
129.530079679328));
#215425=CARTESIAN_POINT('Ctrl Pts',(-5.95105186775873,3.22715944719311,
129.53914746572));
#215426=CARTESIAN_POINT('Ctrl Pts',(-6.03822362058705,3.05485588985547,
129.548215252112));
#215427=CARTESIAN_POINT('Ctrl Pts',(-6.12539537341537,2.88255233251783,
129.557283038504));
#215428=CARTESIAN_POINT('Ctrl Pts',(-6.20522481478602,2.70644085053473,
129.566350824896));
#215429=CARTESIAN_POINT('Ctrl Pts',(-6.27739733281653,2.52716673884965,
129.575418611288));
#215430=CARTESIAN_POINT('Ctrl Pts',(-6.34226712862127,2.36603234399354,
129.5835688805));
#215431=CARTESIAN_POINT('Ctrl Pts',(-6.40093863369382,2.2023738437227,129.591719149711));
#215432=CARTESIAN_POINT('Ctrl Pts',(-6.45322294622245,2.03671367804805,
129.599869418923));
#215433=CARTESIAN_POINT('Ctrl Pts',(-6.50552745197575,1.87098953117558,
129.608022835928));
#215434=CARTESIAN_POINT('Ctrl Pts',(-6.55143972202865,1.70326251997774,
129.616176252934));
#215435=CARTESIAN_POINT('Ctrl Pts',(-6.59082053962587,1.53407092875321,
129.624329669939));
#215436=CARTESIAN_POINT('Ctrl Pts',(-6.63020804405421,1.36485060893274,
129.632484471388));
#215437=CARTESIAN_POINT('Ctrl Pts',(-6.66306181120303,1.19416556972321,
129.640639272837));
#215438=CARTESIAN_POINT('Ctrl Pts',(-6.68929377653724,1.02256431151308,
129.648794074286));
#215439=CARTESIAN_POINT('Ctrl Pts',(-6.71554965728286,0.850806606211075,
129.656956310383));
#215440=CARTESIAN_POINT('Ctrl Pts',(-6.73517162464069,0.678131373831475,
129.66511854648));
#215441=CARTESIAN_POINT('Ctrl Pts',(-6.74812343557283,0.505093158014219,
129.673280782577));
#215442=CARTESIAN_POINT('Ctrl Pts',(-6.76076438924186,0.336208043756621,
129.681247116311));
#215443=CARTESIAN_POINT('Ctrl Pts',(-6.76705173772872,0.166977491905592,
129.689213450045));
#215444=CARTESIAN_POINT('Ctrl Pts',(-6.76699967917944,-0.00208374312541649,
129.697179783778));
#215445=CARTESIAN_POINT('',(-6.767,6.94095388803495E-12,129.30282021619));
#215446=CARTESIAN_POINT('Ctrl Pts',(3.09910619832143,6.01563211736935,128.651395695404));
#215447=CARTESIAN_POINT('Ctrl Pts',(2.93375330764824,6.10081787314654,128.660145143307));
#215448=CARTESIAN_POINT('Ctrl Pts',(2.76488627843057,6.17918207037046,128.668894591209));
#215449=CARTESIAN_POINT('Ctrl Pts',(2.59307866646676,6.25045854554008,128.677644039111));
#215450=CARTESIAN_POINT('Ctrl Pts',(2.42127244185333,6.32173444515054,128.686393416362));
#215451=CARTESIAN_POINT('Ctrl Pts',(2.24652594672404,6.3859226274186,128.695142793612));
#215452=CARTESIAN_POINT('Ctrl Pts',(2.06943269687042,6.44280508110587,128.703892170862));
#215453=CARTESIAN_POINT('Ctrl Pts',(1.89234081821986,6.49968709436193,128.712641480368));
#215454=CARTESIAN_POINT('Ctrl Pts',(1.71290249405485,6.54926340459572,128.721390789873));
#215455=CARTESIAN_POINT('Ctrl Pts',(1.53172716624943,6.59136563150411,128.730140099378));
#215456=CARTESIAN_POINT('Ctrl Pts',(1.3505531810721,6.63346754640735,128.738889344046));
#215457=CARTESIAN_POINT('Ctrl Pts',(1.16764249714286,6.66809542395799,128.747638588713));
#215458=CARTESIAN_POINT('Ctrl Pts',(0.983616340612941,6.69513165624689,
128.75638783338));
#215459=CARTESIAN_POINT('Ctrl Pts',(0.799591486712297,6.7221676971598,128.765137016116));
#215460=CARTESIAN_POINT('Ctrl Pts',(0.614451459525037,6.74161215869387,
128.773886198851));
#215461=CARTESIAN_POINT('Ctrl Pts',(0.428825047908479,6.75339900185724,
128.782635381587));
#215462=CARTESIAN_POINT('Ctrl Pts',(0.243199888595149,6.76518576550228,
128.791384505298));
#215463=CARTESIAN_POINT('Ctrl Pts',(0.0570886373899296,6.76931499599836,
128.800133629008));
#215464=CARTESIAN_POINT('Ctrl Pts',(-0.128876626813226,6.76577266947843,
128.808882752719));
#215465=CARTESIAN_POINT('Ctrl Pts',(-0.314840698190301,6.76223036567983,
128.81763182031));
#215466=CARTESIAN_POINT('Ctrl Pts',(-0.50065849795346,6.75101660879207,
128.826380887902));
#215467=CARTESIAN_POINT('Ctrl Pts',(-0.685698951928485,6.73216948296195,
128.835129955493));
#215468=CARTESIAN_POINT('Ctrl Pts',(-0.870738280462148,6.71332247176263,
128.843878969872));
#215469=CARTESIAN_POINT('Ctrl Pts',(-1.05499998761483,6.6868422135615,128.852627984251));
#215470=CARTESIAN_POINT('Ctrl Pts',(-1.23785829161654,6.65281863948479,
128.861376998629));
#215471=CARTESIAN_POINT('Ctrl Pts',(-1.4300741291762,6.61705395368814,128.870573732328));
#215472=CARTESIAN_POINT('Ctrl Pts',(-1.6207388253599,6.5729537272774,128.879770466027));
#215473=CARTESIAN_POINT('Ctrl Pts',(-1.80913696091694,6.52068343478229,
128.888967199727));
#215474=CARTESIAN_POINT('Ctrl Pts',(-1.98838356186291,6.47095219815144,
128.89771719744));
#215475=CARTESIAN_POINT('Ctrl Pts',(-2.1655782757271,6.41382586850831,128.906467195154));
#215476=CARTESIAN_POINT('Ctrl Pts',(-2.34011918621875,6.34949849943213,
128.915217192868));
#215477=CARTESIAN_POINT('Ctrl Pts',(-2.51465655691265,6.28517243495484,
128.923967013126));
#215478=CARTESIAN_POINT('Ctrl Pts',(-2.68653996295486,6.21364572242306,
128.932716833384));
#215479=CARTESIAN_POINT('Ctrl Pts',(-2.85518555380138,6.13516132252151,
128.941466653642));
#215480=CARTESIAN_POINT('Ctrl Pts',(-3.02382794858838,6.05667841000432,
128.95021630808));
#215481=CARTESIAN_POINT('Ctrl Pts',(-3.18923239109429,5.97123819492002,
128.958965962518));
#215482=CARTESIAN_POINT('Ctrl Pts',(-3.35083705967845,5.87913088810629,
128.967715616955));
#215483=CARTESIAN_POINT('Ctrl Pts',(-3.5124388804254,5.78702520443018,128.976465117204));
#215484=CARTESIAN_POINT('Ctrl Pts',(-3.67024081223823,5.68825280605697,
128.985214617453));
#215485=CARTESIAN_POINT('Ctrl Pts',(-3.82370687544528,5.58314917682418,
128.993964117702));
#215486=CARTESIAN_POINT('Ctrl Pts',(-3.97717043817946,5.47804726007926,
129.002713475392));
#215487=CARTESIAN_POINT('Ctrl Pts',(-4.12629803722595,5.36661448084132,
129.011462833083));
#215488=CARTESIAN_POINT('Ctrl Pts',(-4.27058317207046,5.24922931204464,
129.020212190773));
#215489=CARTESIAN_POINT('Ctrl Pts',(-4.41486614774964,5.13184589986679,
129.028961417533));
#215490=CARTESIAN_POINT('Ctrl Pts',(-4.55430658194534,5.00851045722925,
129.037710644293));
#215491=CARTESIAN_POINT('Ctrl Pts',(-4.68843089001957,4.87964187103012,
129.046459871053));
#215492=CARTESIAN_POINT('Ctrl Pts',(-4.82255336917943,4.75077504207853,
129.055208978509));
#215493=CARTESIAN_POINT('Ctrl Pts',(-4.95135966065236,4.61637541907985,
129.063958085965));
#215494=CARTESIAN_POINT('Ctrl Pts',(-5.0744123086934,4.47689945401736,129.072707193421));
#215495=CARTESIAN_POINT('Ctrl Pts',(-5.19746344226516,4.33742520555397,
129.081456193198));
#215496=CARTESIAN_POINT('Ctrl Pts',(-5.31476088454869,4.19287495491208,
129.090205192974));
#215497=CARTESIAN_POINT('Ctrl Pts',(-5.42590627628957,4.04373961586568,
129.09895419275));
#215498=CARTESIAN_POINT('Ctrl Pts',(-5.53706380672776,3.89458798906581,
129.107704148045));
#215499=CARTESIAN_POINT('Ctrl Pts',(-5.64206777071976,3.74085050155115,
129.11645410334));
#215500=CARTESIAN_POINT('Ctrl Pts',(-5.74056148164123,3.58304938222977,
129.125204058634));
#215501=CARTESIAN_POINT('Ctrl Pts',(-5.8390513895199,3.425254355931,129.133953676076));
#215502=CARTESIAN_POINT('Ctrl Pts',(-5.93103139557751,3.26339625497004,
129.142703293517));
#215503=CARTESIAN_POINT('Ctrl Pts',(-6.01618907820937,3.09802485064829,
129.151452910958));
#215504=CARTESIAN_POINT('Ctrl Pts',(-6.10134392545069,2.93265895249461,
129.160202237074));
#215505=CARTESIAN_POINT('Ctrl Pts',(-6.17967677261913,2.76378023985853,
129.16895156319));
#215506=CARTESIAN_POINT('Ctrl Pts',(-6.25092157009301,2.59196229226932,
129.177700889305));
#215507=CARTESIAN_POINT('Ctrl Pts',(-6.32216437407831,2.42014915228889,
129.186449970608));
#215508=CARTESIAN_POINT('Ctrl Pts',(-6.38631941548999,2.2453972066263,129.19519905191));
#215509=CARTESIAN_POINT('Ctrl Pts',(-6.44316881037614,2.06829994947446,
129.203948133213));
#215510=CARTESIAN_POINT('Ctrl Pts',(-6.5000233452464,1.89118668024214,129.212698005555));
#215511=CARTESIAN_POINT('Ctrl Pts',(-6.54957082411157,1.71172794807471,
129.221447877897));
#215512=CARTESIAN_POINT('Ctrl Pts',(-6.59164294296136,1.53053334250113,
129.23019775024));
#215513=CARTESIAN_POINT('Ctrl Pts',(-6.63371214082178,1.34935131693382,
129.238947015095));
#215514=CARTESIAN_POINT('Ctrl Pts',(-6.66830695239726,1.16643393829557,
129.24769627995));
#215515=CARTESIAN_POINT('Ctrl Pts',(-6.69530988154017,0.982402458339035,
129.256445544805));
#215516=CARTESIAN_POINT('Ctrl Pts',(-6.72231419690506,0.798361530945111,
129.265195258812));
#215517=CARTESIAN_POINT('Ctrl Pts',(-6.74172580829295,0.613206671360537,
129.273944972819));
#215518=CARTESIAN_POINT('Ctrl Pts',(-6.75347878028192,0.42756679511147,
129.282694686826));
#215519=CARTESIAN_POINT('Ctrl Pts',(-6.76248992368208,0.285234494205815,
129.289403196614));
#215520=CARTESIAN_POINT('Ctrl Pts',(-6.76699999999985,0.142617266095155,
129.296111706402));
#215521=CARTESIAN_POINT('Ctrl Pts',(-6.767,6.94095400683209E-12,129.30282021619));
#215522=CARTESIAN_POINT('Ctrl Pts',(-6.76699998027983,-0.000516616662484787,
129.30282021619));
#215523=CARTESIAN_POINT('Ctrl Pts',(-6.76698635528968,-0.17898609850718,
129.311175751275));
#215524=CARTESIAN_POINT('Ctrl Pts',(-6.75990811182994,-0.357370256202649,
129.319531286361));
#215525=CARTESIAN_POINT('Ctrl Pts',(-6.74581131082869,-0.535087617774603,
129.327886821446));
#215526=CARTESIAN_POINT('Ctrl Pts',(-6.7317049334655,-0.712925707856396,
129.336248032686));
#215527=CARTESIAN_POINT('Ctrl Pts',(-6.71057051792594,-0.890095762078785,
129.344609243927));
#215528=CARTESIAN_POINT('Ctrl Pts',(-6.68250576114816,-1.06602333568344,
129.352970455167));
#215529=CARTESIAN_POINT('Ctrl Pts',(-6.65440001357014,-1.24220786544432,
129.361343878619));
#215530=CARTESIAN_POINT('Ctrl Pts',(-6.61934375200373,-1.41714595444067,
129.36971730207));
#215531=CARTESIAN_POINT('Ctrl Pts',(-6.57748569718429,-1.59027384539146,
129.378090725522));
#215532=CARTESIAN_POINT('Ctrl Pts',(-6.53559356498376,-1.76354268281343,
129.386470965926));
#215533=CARTESIAN_POINT('Ctrl Pts',(-6.48688868596984,-1.93499805826365,
129.394851206329));
#215534=CARTESIAN_POINT('Ctrl Pts',(-6.43156917970343,-2.10409288927293,
129.403231446732));
#215535=CARTESIAN_POINT('Ctrl Pts',(-6.3761607646608,-2.27345948725024,
129.411625155747));
#215536=CARTESIAN_POINT('Ctrl Pts',(-6.31411659565488,-2.44045764319213,
129.420018864762));
#215537=CARTESIAN_POINT('Ctrl Pts',(-6.24568284109669,-2.60456039446783,
129.428412573776));
#215538=CARTESIAN_POINT('Ctrl Pts',(-6.21110627378886,-2.68747429947737,
129.43265354589));
#215539=CARTESIAN_POINT('Ctrl Pts',(-6.17489928125139,-2.76964944403422,
129.436894518003));
#215540=CARTESIAN_POINT('Ctrl Pts',(-6.13709797108201,-2.85102043018655,
129.441135490117));
#215541=CARTESIAN_POINT('Ctrl Pts',(-6.06179770496057,-3.0131115557158,
129.449583512879));
#215542=CARTESIAN_POINT('Ctrl Pts',(-5.98000648310577,-3.17235838630767,
129.458031535642));
#215543=CARTESIAN_POINT('Ctrl Pts',(-5.89196137931734,-3.32822476774525,
129.466479558404));
#215544=CARTESIAN_POINT('Ctrl Pts',(-5.80399690105999,-3.48394841768227,
129.47491984506));
#215545=CARTESIAN_POINT('Ctrl Pts',(-5.7097901194528,-3.63629749987733,
129.483360131716));
#215546=CARTESIAN_POINT('Ctrl Pts',(-5.60962497276874,-3.7847584685009,
129.491800418372));
#215547=CARTESIAN_POINT('Ctrl Pts',(-5.50953613043959,-3.93310634171341,
129.500234275339));
#215548=CARTESIAN_POINT('Ctrl Pts',(-5.40349815741405,-4.07757173042906,
129.508668132307));
#215549=CARTESIAN_POINT('Ctrl Pts',(-5.29183963587732,-4.21766787077383,
129.517101989275));
#215550=CARTESIAN_POINT('Ctrl Pts',(-5.1802490085182,-4.35767882539246,
129.52553071802));
#215551=CARTESIAN_POINT('Ctrl Pts',(-5.06304485375228,-4.49332556828457,
129.533959446765));
#215552=CARTESIAN_POINT('Ctrl Pts',(-4.94059780221203,-4.62415206895034,
129.54238817551));
#215553=CARTESIAN_POINT('Ctrl Pts',(-4.81820640151364,-4.75491911040652,
129.550813073491));
#215554=CARTESIAN_POINT('Ctrl Pts',(-4.69057708295744,-4.88087003491284,
129.559237971471));
#215555=CARTESIAN_POINT('Ctrl Pts',(-4.55811957752833,-5.00158324103008,
129.567662869451));
#215556=CARTESIAN_POINT('Ctrl Pts',(-4.42569139840627,-5.12226972104723,
129.576085902145));
#215557=CARTESIAN_POINT('Ctrl Pts',(-4.2884374082191,-5.23772056838595,
129.584508934839));
#215558=CARTESIAN_POINT('Ctrl Pts',(-4.14680327068804,-5.34755192908035,
129.592931967534));
#215559=CARTESIAN_POINT('Ctrl Pts',(-4.0051851588989,-5.45737086248094,
129.601354047171));
#215560=CARTESIAN_POINT('Ctrl Pts',(-3.85918815125639,-5.5615713725011,
129.609776126809));
#215561=CARTESIAN_POINT('Ctrl Pts',(-3.70929022153916,-5.65981051382411,
129.618198206446));
#215562=CARTESIAN_POINT('Ctrl Pts',(-3.55938832797121,-5.75805225295013,
129.626620508795));
#215563=CARTESIAN_POINT('Ctrl Pts',(-3.40558558578551,-5.85033212661465,
129.635042811143));
#215564=CARTESIAN_POINT('Ctrl Pts',(-3.24838841911922,-5.9363508722558,
129.643465113491));
#215565=CARTESIAN_POINT('Ctrl Pts',(-3.09116515075727,-6.02238390082052,
129.651888814315));
#215566=CARTESIAN_POINT('Ctrl Pts',(-2.93054662700452,-6.10215356913166,
129.660312515138));
#215567=CARTESIAN_POINT('Ctrl Pts',(-2.76706362151651,-6.17540670032994,
129.668736215962));
#215568=CARTESIAN_POINT('Ctrl Pts',(-2.60346998558457,-6.2487094025916,
129.677165617181));
#215569=CARTESIAN_POINT('Ctrl Pts',(-2.43700829911282,-6.31548661939793,
129.6855950184));
#215570=CARTESIAN_POINT('Ctrl Pts',(-2.26822999552332,-6.37553305123645,
129.694024419619));
#215571=CARTESIAN_POINT('Ctrl Pts',(-2.09939147206966,-6.43560090755839,
129.702456828436));
#215572=CARTESIAN_POINT('Ctrl Pts',(-1.92823499958499,-6.48893308440157,
129.710889237254));
#215573=CARTESIAN_POINT('Ctrl Pts',(-1.75532745154532,-6.5353740931833,
129.719321646072));
#215574=CARTESIAN_POINT('Ctrl Pts',(-1.58225992441111,-6.58185807053765,
129.727761856799));
#215575=CARTESIAN_POINT('Ctrl Pts',(-1.40743840847123,-6.6214380602208,
129.736202067527));
#215576=CARTESIAN_POINT('Ctrl Pts',(-1.2314413453438,-6.6540094088435,129.744642278255));
#215577=CARTESIAN_POINT('Ctrl Pts',(-1.13133721906875,-6.67253543613928,
129.749442926092));
#215578=CARTESIAN_POINT('Ctrl Pts',(-1.03085294210219,-6.68879501086256,
129.754243573929));
#215579=CARTESIAN_POINT('Ctrl Pts',(-0.930095770582873,-6.70277635443283,
129.759044221766));
#215580=CARTESIAN_POINT('Ctrl Pts',(-0.759257439694681,-6.72648235335184,
129.767183936799));
#215581=CARTESIAN_POINT('Ctrl Pts',(-0.587293664602942,-6.74368299044695,
129.775323651832));
#215582=CARTESIAN_POINT('Ctrl Pts',(-0.414745515237176,-6.75427828547141,
129.783463366865));
#215583=CARTESIAN_POINT('Ctrl Pts',(-0.242348275447631,-6.76486431391442,
129.791595962952));
#215584=CARTESIAN_POINT('Ctrl Pts',(-0.0693680417233102,-6.76885647706346,
129.799728559039));
#215585=CARTESIAN_POINT('Ctrl Pts',(0.103646143768112,-6.76620621004725,
129.807861155126));
#215586=CARTESIAN_POINT('Ctrl Pts',(0.27654204748035,-6.76355775489576,
129.815988191334));
#215587=CARTESIAN_POINT('Ctrl Pts',(0.449471492083241,-6.75427591630593,
129.824115227543));
#215588=CARTESIAN_POINT('Ctrl Pts',(0.621882601247664,-6.73836412122894,
129.832242263751));
#215589=CARTESIAN_POINT('Ctrl Pts',(0.794211294781642,-6.72245993227796,
129.840365415088));
#215590=CARTESIAN_POINT('Ctrl Pts',(0.966021782391835,-6.69993213141763,
129.848488566426));
#215591=CARTESIAN_POINT('Ctrl Pts',(1.13676450063965,-6.67083618972056,
129.856611717764));
#215592=CARTESIAN_POINT('Ctrl Pts',(1.30745923891445,-6.64174842419938,
129.864732586435));
#215593=CARTESIAN_POINT('Ctrl Pts',(1.47708644491182,-6.6060962563491,129.872853455107));
#215594=CARTESIAN_POINT('Ctrl Pts',(1.64510400869592,-6.56398673068225,
129.880974323779));
#215595=CARTESIAN_POINT('Ctrl Pts',(1.81313065279243,-6.52187492925541,
129.889095631334));
#215596=CARTESIAN_POINT('Ctrl Pts',(1.97954712467904,-6.47330515799107,
129.897216938888));
#215597=CARTESIAN_POINT('Ctrl Pts',(2.14382361570506,-6.41843511338592,
129.905338246443));
#215598=CARTESIAN_POINT('Ctrl Pts',(2.22918739097763,-6.38992273083127,
129.909558360159));
#215599=CARTESIAN_POINT('Ctrl Pts',(2.31397356464635,-6.35970997104257,
129.913778473875));
#215600=CARTESIAN_POINT('Ctrl Pts',(2.39810960016221,-6.32782421892469,
129.917998587591));
#215601=CARTESIAN_POINT('Ctrl Pts',(2.57723155983313,-6.25994083970533,
129.926983026116));
#215602=CARTESIAN_POINT('Ctrl Pts',(2.75331696070877,-6.18450567964859,
129.935967464642));
#215603=CARTESIAN_POINT('Ctrl Pts',(2.92576566098836,-6.10181811405268,
129.944951903167));
#215604=CARTESIAN_POINT('Ctrl Pts',(3.09851199743215,-6.01898783465369,
129.953951848297));
#215605=CARTESIAN_POINT('Ctrl Pts',(3.26760887229161,-5.92888023450163,
129.962951793427));
#215606=CARTESIAN_POINT('Ctrl Pts',(3.43248109364044,-5.83184040777874,
129.971951738557));
#215607=CARTESIAN_POINT('Ctrl Pts',(3.59774184061054,-5.73457190421353,
129.980972892289));
#215608=CARTESIAN_POINT('Ctrl Pts',(3.75875780795001,-5.63033861015721,
129.989994046021));
#215609=CARTESIAN_POINT('Ctrl Pts',(3.91498082350201,-5.51953024736812,
129.999015199753));
#215610=CARTESIAN_POINT('Ctrl Pts',(4.07136279720394,-5.40860913619631,
130.008045532579));
#215611=CARTESIAN_POINT('Ctrl Pts',(4.22294188507482,-5.29109973396594,
130.017075865406));
#215612=CARTESIAN_POINT('Ctrl Pts',(4.36920210967447,-5.16743281763935,
130.026106198233));
#215613=CARTESIAN_POINT('Ctrl Pts',(4.51566968516852,-5.04359058060764,
130.035149333225));
#215614=CARTESIAN_POINT('Ctrl Pts',(4.65680313746559,-4.91357352917454,
130.044192468217));
#215615=CARTESIAN_POINT('Ctrl Pts',(4.7921208249499,-4.77785171380208,130.05323560321));
#215616=CARTESIAN_POINT('Ctrl Pts',(4.91041965922102,-4.65919957865099,
130.061141386612));
#215617=CARTESIAN_POINT('Ctrl Pts',(5.02427411626289,-4.53618805361324,
130.069047170014));
#215618=CARTESIAN_POINT('Ctrl Pts',(5.1333866744504,-4.40915300829707,130.076952953416));
#215619=CARTESIAN_POINT('Ctrl Pts',(5.25281738467958,-4.27010498359552,
130.085606341645));
#215620=CARTESIAN_POINT('Ctrl Pts',(5.36667148794623,-4.12611281017222,
130.094259729874));
#215621=CARTESIAN_POINT('Ctrl Pts',(5.47454641738078,-3.977641326709,130.102913118103));
#215622=CARTESIAN_POINT('Ctrl Pts',(5.58232171666579,-3.82930696719271,
130.111558514314));
#215623=CARTESIAN_POINT('Ctrl Pts',(5.68412867816535,-3.67650179399611,
130.120203910524));
#215624=CARTESIAN_POINT('Ctrl Pts',(5.77960525181488,-3.519723303499,130.128849306735));
#215625=CARTESIAN_POINT('Ctrl Pts',(5.87813102559388,-3.35793783615668,
130.137770807778));
#215626=CARTESIAN_POINT('Ctrl Pts',(5.96991515749052,-3.19192130305316,
130.14669230882));
#215627=CARTESIAN_POINT('Ctrl Pts',(6.0546071247108,-3.02225438462768,130.155613809862));
#215628=CARTESIAN_POINT('Ctrl Pts',(6.13652171310393,-2.85815150400141,
130.164242740204));
#215629=CARTESIAN_POINT('Ctrl Pts',(6.21180175270025,-2.6906341532244,130.172871670547));
#215630=CARTESIAN_POINT('Ctrl Pts',(6.28017559863909,-2.52025463996361,
130.181500600889));
#215631=CARTESIAN_POINT('Ctrl Pts',(6.35202684846474,-2.3412098487225,130.190568387281));
#215632=CARTESIAN_POINT('Ctrl Pts',(6.4162509413252,-2.15900446694894,130.199636173673));
#215633=CARTESIAN_POINT('Ctrl Pts',(6.47258869647183,-1.97430609741881,
130.208703960065));
#215634=CARTESIAN_POINT('Ctrl Pts',(6.52892645161846,-1.78960772788868,
130.217771746457));
#215635=CARTESIAN_POINT('Ctrl Pts',(6.57737772144378,-1.60241673385363,
130.226839532849));
#215636=CARTESIAN_POINT('Ctrl Pts',(6.61774319506332,-1.41342279739403,
130.235907319241));
#215637=CARTESIAN_POINT('Ctrl Pts',(6.65524709401102,-1.23782695126286,
130.244332275374));
#215638=CARTESIAN_POINT('Ctrl Pts',(6.68575477026857,-1.06075182863909,
130.252757231506));
#215639=CARTESIAN_POINT('Ctrl Pts',(6.70917194918932,-0.882780129030567,
130.261182187639));
#215640=CARTESIAN_POINT('Ctrl Pts',(6.73259456346211,-0.704767120481909,
130.269609099285));
#215641=CARTESIAN_POINT('Ctrl Pts',(6.74892335571185,-0.525857448792384,
130.278036010931));
#215642=CARTESIAN_POINT('Ctrl Pts',(6.7581158576744,-0.346639660526275,
130.286462922577));
#215643=CARTESIAN_POINT('Ctrl Pts',(6.76731174007799,-0.167355966898705,
130.294892933127));
#215644=CARTESIAN_POINT('Ctrl Pts',(6.76936608262606,0.012235738216695,
130.303322943676));
#215645=CARTESIAN_POINT('Ctrl Pts',(6.76428852229768,0.191545783331,130.311752954226));
#215646=CARTESIAN_POINT('Ctrl Pts',(6.75920628462692,0.37102100510872,130.320190730325));
#215647=CARTESIAN_POINT('Ctrl Pts',(6.74697902767285,0.550213716802047,
130.328628506424));
#215648=CARTESIAN_POINT('Ctrl Pts',(6.72766844219846,0.728537117686494,
130.337066282523));
#215649=CARTESIAN_POINT('Ctrl Pts',(6.70834772009017,0.906954125211403,
130.345508487832));
#215650=CARTESIAN_POINT('Ctrl Pts',(6.68193629732504,1.08450058339776,130.353950693142));
#215651=CARTESIAN_POINT('Ctrl Pts',(6.6485472977742,1.26059820294153,130.362392898451));
#215652=CARTESIAN_POINT('Ctrl Pts',(6.61512307466596,1.43688159578465,130.370844009823));
#215653=CARTESIAN_POINT('Ctrl Pts',(6.57470663998523,1.611712772811,130.379295121194));
#215654=CARTESIAN_POINT('Ctrl Pts',(6.52746170286202,1.78452590837726,130.387746232566));
#215655=CARTESIAN_POINT('Ctrl Pts',(6.51420233806007,1.83302618261969,130.390118050066));
#215656=CARTESIAN_POINT('Ctrl Pts',(6.50040542261883,1.88136760758521,130.392489867566));
#215657=CARTESIAN_POINT('Ctrl Pts',(6.48607526764057,1.92953792979078,130.394861685066));
#215658=CARTESIAN_POINT('Ctrl Pts',(6.43582501806462,2.09845241233877,130.403178721519));
#215659=CARTESIAN_POINT('Ctrl Pts',(6.37892343167615,2.26556646756993,130.411495757971));
#215660=CARTESIAN_POINT('Ctrl Pts',(6.31551992189105,2.43032860251392,130.419812794424));
#215661=CARTESIAN_POINT('Ctrl Pts',(6.25217157846125,2.59494738062312,130.428122594359));
#215662=CARTESIAN_POINT('Ctrl Pts',(6.18233270841608,2.75721799274781,130.436432394295));
#215663=CARTESIAN_POINT('Ctrl Pts',(6.10620249139547,2.91660421279195,130.44474219423));
#215664=CARTESIAN_POINT('Ctrl Pts',(6.02735961331197,3.08166965995505,130.453348087775));
#215665=CARTESIAN_POINT('Ctrl Pts',(5.94176887260188,3.24364100646435,130.461953981319));
#215666=CARTESIAN_POINT('Ctrl Pts',(5.84970649809143,3.40194398633883,130.470559874864));
#215667=CARTESIAN_POINT('Ctrl Pts',(5.76091870473339,3.55461626249723,130.478859664021));
#215668=CARTESIAN_POINT('Ctrl Pts',(5.66611192138681,3.70387631016144,130.487159453177));
#215669=CARTESIAN_POINT('Ctrl Pts',(5.56558115943957,3.84923308695268,130.495459242334));
#215670=CARTESIAN_POINT('Ctrl Pts',(5.46507657711748,3.9945520107937,130.503756870109));
#215671=CARTESIAN_POINT('Ctrl Pts',(5.35885118393023,4.13596940317617,130.512054497884));
#215672=CARTESIAN_POINT('Ctrl Pts',(5.24724353377759,4.27302285241131,130.520352125658));
#215673=CARTESIAN_POINT('Ctrl Pts',(5.13564640125446,4.41006338606763,130.528648971485));
#215674=CARTESIAN_POINT('Ctrl Pts',(5.01866824256713,4.54274052676302,130.536945817312));
#215675=CARTESIAN_POINT('Ctrl Pts',(4.89668826116683,4.67062448425807,130.545242663139));
#215676=CARTESIAN_POINT('Ctrl Pts',(4.77469950614701,4.79851764002625,130.553540105731));
#215677=CARTESIAN_POINT('Ctrl Pts',(4.64770845244548,4.92161667474264,130.561837548322));
#215678=CARTESIAN_POINT('Ctrl Pts',(4.5161316871342,5.03952811128804,130.570134990914));
#215679=CARTESIAN_POINT('Ctrl Pts',(4.38448221110785,5.15750470694299,130.57843701876));
#215680=CARTESIAN_POINT('Ctrl Pts',(4.2482422204802,5.27028774542234,130.586739046607));
#215681=CARTESIAN_POINT('Ctrl Pts',(4.10786250804287,5.37752309293189,130.595041074453));
#215682=CARTESIAN_POINT('Ctrl Pts',(3.9674369825844,5.484793436775,130.603345811673));
#215683=CARTESIAN_POINT('Ctrl Pts',(3.82286932331226,5.58651227583874,130.611650548892));
#215684=CARTESIAN_POINT('Ctrl Pts',(3.67464010641463,5.68236826405409,130.619955286111));
#215685=CARTESIAN_POINT('Ctrl Pts',(3.52629000069492,5.77830242793378,130.628266796286));
#215686=CARTESIAN_POINT('Ctrl Pts',(3.37427267024646,5.86836401059003,130.636578306461));
#215687=CARTESIAN_POINT('Ctrl Pts',(3.21909476324528,5.95228677948625,130.644889816635));
#215688=CARTESIAN_POINT('Ctrl Pts',(3.17930335758787,5.97380662728918,130.647021090857));
#215689=CARTESIAN_POINT('Ctrl Pts',(3.13930424687303,5.9949230681795,130.649152365079));
#215690=CARTESIAN_POINT('Ctrl Pts',(3.0991061983213,6.01563211736942,130.651283639301));
#215691=CARTESIAN_POINT('Origin',(0.,0.,4.30282021618968));
#215692=CARTESIAN_POINT('',(3.09910619832141,6.01563211736936,133.045915245968));
#215693=CARTESIAN_POINT('',(3.09910619832128,6.01563211736943,132.651465380124));
#215694=CARTESIAN_POINT('',(3.09910619832133,6.0156321173694,4.30282021618968));
#215695=CARTESIAN_POINT('',(-6.76699907392669,0.00354026487730927,131.697179783784));
#215696=CARTESIAN_POINT('Ctrl Pts',(-6.76699907392698,0.00354026431528137,
131.69717978381));
#215697=CARTESIAN_POINT('Ctrl Pts',(-6.76709497084188,-0.179760833150435,
131.705813112895));
#215698=CARTESIAN_POINT('Ctrl Pts',(-6.75973839205797,-0.363203276888397,
131.714446441981));
#215699=CARTESIAN_POINT('Ctrl Pts',(-6.74492430186807,-0.546154888350881,
131.723079771066));
#215700=CARTESIAN_POINT('Ctrl Pts',(-6.73049099454992,-0.724403893098308,
131.731491188188));
#215701=CARTESIAN_POINT('Ctrl Pts',(-6.7089788469857,-0.90218662774764,
131.739902605309));
#215702=CARTESIAN_POINT('Ctrl Pts',(-6.6804358924897,-1.0789185726158,131.748314022431));
#215703=CARTESIAN_POINT('Ctrl Pts',(-6.65076339769416,-1.26264439241631,
131.757058307498));
#215704=CARTESIAN_POINT('Ctrl Pts',(-6.6134922718676,-1.44523418945677,
131.765802592566));
#215705=CARTESIAN_POINT('Ctrl Pts',(-6.56873593024028,-1.62603729316716,
131.774546877633));
#215706=CARTESIAN_POINT('Ctrl Pts',(-6.52397958861293,-1.80684039687767,
131.7832911627));
#215707=CARTESIAN_POINT('Ctrl Pts',(-6.47173810469297,-1.98585640656563,
131.792035447767));
#215708=CARTESIAN_POINT('Ctrl Pts',(-6.41218472486434,-2.16244677488636,
131.800779732834));
#215709=CARTESIAN_POINT('Ctrl Pts',(-6.35480615025228,-2.33258831267348,
131.809204688976));
#215710=CARTESIAN_POINT('Ctrl Pts',(-6.29065631498354,-2.500430846268,131.817629645118));
#215711=CARTESIAN_POINT('Ctrl Pts',(-6.21995157621256,-2.6654251798861,
131.82605460126));
#215712=CARTESIAN_POINT('Ctrl Pts',(-6.14923042618649,-2.83045781028806,
131.834481512916));
#215713=CARTESIAN_POINT('Ctrl Pts',(-6.0719514697138,-2.9926406177891,131.842908424571));
#215714=CARTESIAN_POINT('Ctrl Pts',(-5.9883785978316,-3.15144582200494,
131.851335336227));
#215715=CARTESIAN_POINT('Ctrl Pts',(-5.90477499294191,-3.3103094250938,
131.859765346787));
#215716=CARTESIAN_POINT('Ctrl Pts',(-5.81487301206899,-3.46579265500461,
131.868195357348));
#215717=CARTESIAN_POINT('Ctrl Pts',(-5.71898192682299,-3.61739335995853,
131.876625367908));
#215718=CARTESIAN_POINT('Ctrl Pts',(-5.62300250870327,-3.76913371632938,
131.885063144018));
#215719=CARTESIAN_POINT('Ctrl Pts',(-5.52102314104431,-3.91698412176279,
131.893500920129));
#215720=CARTESIAN_POINT('Ctrl Pts',(-5.41339639226867,-4.060471462795,131.90193869624));
#215721=CARTESIAN_POINT('Ctrl Pts',(-5.30571314737572,-4.20403412411464,
131.910380901561));
#215722=CARTESIAN_POINT('Ctrl Pts',(-5.19237681409164,-4.34322889305352,
131.918823106883));
#215723=CARTESIAN_POINT('Ctrl Pts',(-5.07377984477311,-4.47761622817032,
131.927265312205));
#215724=CARTESIAN_POINT('Ctrl Pts',(-4.95505776216699,-4.61214533454318,
131.935716423589));
#215725=CARTESIAN_POINT('Ctrl Pts',(-4.83106418257116,-4.74185663299263,
131.944167534974));
#215726=CARTESIAN_POINT('Ctrl Pts',(-4.70222869586103,-4.86634711994748,
131.952618646358));
#215727=CARTESIAN_POINT('Ctrl Pts',(-4.66607081797621,-4.90128556695519,
131.954990463792));
#215728=CARTESIAN_POINT('Ctrl Pts',(-4.62953177020199,-4.93581303554232,
131.957362281225));
#215729=CARTESIAN_POINT('Ctrl Pts',(-4.59262151425912,-4.96992118919046,
131.959734098659));
#215730=CARTESIAN_POINT('Ctrl Pts',(-4.46320356918836,-5.0895141598307,
131.968050370938));
#215731=CARTESIAN_POINT('Ctrl Pts',(-4.32898587182286,-5.2041647890652,
131.976366643218));
#215732=CARTESIAN_POINT('Ctrl Pts',(-4.19037828833678,-5.31347520937435,
131.984682915498));
#215733=CARTESIAN_POINT('Ctrl Pts',(-4.05188789774753,-5.42269320757722,
131.992992156358));
#215734=CARTESIAN_POINT('Ctrl Pts',(-3.90901528784766,-5.52657977833173,
132.001301397218));
#215735=CARTESIAN_POINT('Ctrl Pts',(-3.76220534782492,-5.62477554403708,
132.009610638078));
#215736=CARTESIAN_POINT('Ctrl Pts',(-3.6154926187237,-5.72290628893476,
132.017914376934));
#215737=CARTESIAN_POINT('Ctrl Pts',(-3.46484804272415,-5.81535354453606,
132.026218115789));
#215738=CARTESIAN_POINT('Ctrl Pts',(-3.31074777697401,-5.90179956939082,
132.034521854645));
#215739=CARTESIAN_POINT('Ctrl Pts',(-3.15672130830467,-5.9882041961062,
132.042821616923));
#215740=CARTESIAN_POINT('Ctrl Pts',(-2.99924275074094,-6.06861314962715,
132.051121379201));
#215741=CARTESIAN_POINT('Ctrl Pts',(-2.83881549031413,-6.1427530971017,
132.059421141479));
#215742=CARTESIAN_POINT('Ctrl Pts',(-2.67843566613839,-6.21687112235959,
132.067718449625));
#215743=CARTESIAN_POINT('Ctrl Pts',(-2.51510919250034,-6.28472369065521,
132.076015757772));
#215744=CARTESIAN_POINT('Ctrl Pts',(-2.34936239850547,-6.34608425097624,
132.084313065918));
#215745=CARTESIAN_POINT('Ctrl Pts',(-2.18359885820913,-6.40745101088893,
132.092611212386));
#215746=CARTESIAN_POINT('Ctrl Pts',(-2.01541483259486,-6.46232432432534,
132.100909358855));
#215747=CARTESIAN_POINT('Ctrl Pts',(-1.84535545163506,-6.51052626575769,
132.109207505323));
#215748=CARTESIAN_POINT('Ctrl Pts',(-1.67527897013812,-6.55873305419751,
132.117506486223));
#215749=CARTESIAN_POINT('Ctrl Pts',(-1.50332709221133,-6.6002670380266,
132.125805467122));
#215750=CARTESIAN_POINT('Ctrl Pts',(-1.33005880005892,-6.63500057184518,
132.134104448021));
#215751=CARTESIAN_POINT('Ctrl Pts',(-1.15674428946044,-6.66974337065933,
132.142405642632));
#215752=CARTESIAN_POINT('Ctrl Pts',(-0.982113006033505,-6.69768203560138,
132.150706837243));
#215753=CARTESIAN_POINT('Ctrl Pts',(-0.80673296985677,-6.71874027741407,
132.159008031853));
#215754=CARTESIAN_POINT('Ctrl Pts',(-0.631277002325003,-6.7398076364608,
132.167312820493));
#215755=CARTESIAN_POINT('Ctrl Pts',(-0.455071981281516,-6.75398859393647,
132.175617609133));
#215756=CARTESIAN_POINT('Ctrl Pts',(-0.278690069031756,-6.76125882106454,
132.183922397773));
#215757=CARTESIAN_POINT('Ctrl Pts',(-0.10209905758523,-6.76853766698257,
132.192237031666));
#215758=CARTESIAN_POINT('Ctrl Pts',(0.074668915954113,-6.76888939950066,
132.200551665559));
#215759=CARTESIAN_POINT('Ctrl Pts',(0.251041473807029,-6.76234184128759,
132.208866299452));
#215760=CARTESIAN_POINT('Ctrl Pts',(0.427525553601578,-6.75579014299505,
132.217186190763));
#215761=CARTESIAN_POINT('Ctrl Pts',(0.603613372588242,-6.74233048058884,
132.225506082073));
#215762=CARTESIAN_POINT('Ctrl Pts',(0.778738501598195,-6.72204249809004,
132.233825973384));
#215763=CARTESIAN_POINT('Ctrl Pts',(0.954125499504187,-6.70172417847395,
132.242158305631));
#215764=CARTESIAN_POINT('Ctrl Pts',(1.12854658684618,-6.67455718662064,
132.250490637879));
#215765=CARTESIAN_POINT('Ctrl Pts',(1.3014449890108,-6.6406724012391,132.258822970127));
#215766=CARTESIAN_POINT('Ctrl Pts',(1.43161757685582,-6.61516105962769,
132.265096256854));
#215767=CARTESIAN_POINT('Ctrl Pts',(1.56092727260945,-6.5858428926111,132.271369543581));
#215768=CARTESIAN_POINT('Ctrl Pts',(1.68914275140066,-6.55279221136995,
132.277642830309));
#215769=CARTESIAN_POINT('Ctrl Pts',(1.85407689834577,-6.51027639371783,
132.285712676513));
#215770=CARTESIAN_POINT('Ctrl Pts',(2.01770936421284,-6.46145082056711,
132.293782522718));
#215771=CARTESIAN_POINT('Ctrl Pts',(2.17950805597581,-6.4064056719768,132.301852368923));
#215772=CARTESIAN_POINT('Ctrl Pts',(2.34110318440282,-6.35142977718548,
132.309912062235));
#215773=CARTESIAN_POINT('Ctrl Pts',(2.50086878054943,-6.29024999521635,
132.317971755546));
#215774=CARTESIAN_POINT('Ctrl Pts',(2.65828259754013,-6.22300752302416,
132.326031448858));
#215775=CARTESIAN_POINT('Ctrl Pts',(2.81553291527486,-6.1558348928216,132.334082770898));
#215776=CARTESIAN_POINT('Ctrl Pts',(2.97043597466164,-6.08261224893743,
132.342134092938));
#215777=CARTESIAN_POINT('Ctrl Pts',(3.12248446810918,-6.0035306067694,132.350185414977));
#215778=CARTESIAN_POINT('Ctrl Pts',(3.2744083540449,-5.92451377396869,132.358230138759));
#215779=CARTESIAN_POINT('Ctrl Pts',(3.42348200086224,-5.83964767087949,
132.366274862541));
#215780=CARTESIAN_POINT('Ctrl Pts',(3.56921798634966,-5.74917141559704,
132.374319586322));
#215781=CARTESIAN_POINT('Ctrl Pts',(3.71486643925043,-5.65874950255978,
132.382359478247));
#215782=CARTESIAN_POINT('Ctrl Pts',(3.85718090534057,-5.56272434144218,
132.390399370171));
#215783=CARTESIAN_POINT('Ctrl Pts',(3.99569859359893,-5.46138093792326,
132.398439262096));
#215784=CARTESIAN_POINT('Ctrl Pts',(4.13719894149439,-5.35785533743756,
132.40665227459));
#215785=CARTESIAN_POINT('Ctrl Pts',(4.27473679332243,-5.24878004803285,
132.414865287084));
#215786=CARTESIAN_POINT('Ctrl Pts',(4.40784969965924,-5.13450582093486,
132.423078299578));
#215787=CARTESIAN_POINT('Ctrl Pts',(4.53811127849206,-5.02267938988977,
132.431115386319));
#215788=CARTESIAN_POINT('Ctrl Pts',(4.66413527302074,-4.9058747543783,132.439152473059));
#215789=CARTESIAN_POINT('Ctrl Pts',(4.78552188066206,-4.78446123714098,
132.447189559799));
#215790=CARTESIAN_POINT('Ctrl Pts',(4.90692010555167,-4.66303610008001,
132.455227415725));
#215791=CARTESIAN_POINT('Ctrl Pts',(5.0236797955743,-4.53700146714822,132.463265271651));
#215792=CARTESIAN_POINT('Ctrl Pts',(5.13543839212052,-4.40676315686861,
132.471303127577));
#215793=CARTESIAN_POINT('Ctrl Pts',(5.24722982757857,-4.27648657763682,
132.479343345329));
#215794=CARTESIAN_POINT('Ctrl Pts',(5.35401700137793,-4.14200414581877,
132.487383563082));
#215795=CARTESIAN_POINT('Ctrl Pts',(5.45547808825628,-4.00375421680148,
132.495423780835));
#215796=CARTESIAN_POINT('Ctrl Pts',(5.5607724328051,-3.86028112669699,132.503767762595));
#215797=CARTESIAN_POINT('Ctrl Pts',(5.66033012114379,-3.7127506613426,132.512111744355));
#215798=CARTESIAN_POINT('Ctrl Pts',(5.75384181462403,-3.56168406407476,
132.520455726115));
#215799=CARTESIAN_POINT('Ctrl Pts',(5.84410606836313,-3.41586365210489,
132.528509941142));
#215800=CARTESIAN_POINT('Ctrl Pts',(5.92873708984125,-3.26674894657301,
132.536564156169));
#215801=CARTESIAN_POINT('Ctrl Pts',(6.00750464953942,-3.11483175882138,
132.544618371196));
#215802=CARTESIAN_POINT('Ctrl Pts',(6.08633115371727,-2.96280088620225,
132.552678613469));
#215803=CARTESIAN_POINT('Ctrl Pts',(6.15928530123639,-2.80796369122435,
132.560738855743));
#215804=CARTESIAN_POINT('Ctrl Pts',(6.22618559531596,-2.65083042322213,
132.568799098016));
#215805=CARTESIAN_POINT('Ctrl Pts',(6.29317942057075,-2.49347747219124,
132.576870609058));
#215806=CARTESIAN_POINT('Ctrl Pts',(6.35410237390941,-2.33382238924736,
132.5849421201));
#215807=CARTESIAN_POINT('Ctrl Pts',(6.40882304117147,-2.17238952007914,
132.593013631142));
#215808=CARTESIAN_POINT('Ctrl Pts',(6.41455832695984,-2.15546970373476,
132.593859608081));
#215809=CARTESIAN_POINT('Ctrl Pts',(6.42022552602584,-2.1385303659194,132.594705585019));
#215810=CARTESIAN_POINT('Ctrl Pts',(6.42582451980291,-2.12157211536626,
132.595551561958));
#215811=CARTESIAN_POINT('Ctrl Pts',(6.480288792434,-1.95661054936942,132.603780811795));
#215812=CARTESIAN_POINT('Ctrl Pts',(6.52847676044186,-1.78930795410407,
132.612010061631));
#215813=CARTESIAN_POINT('Ctrl Pts',(6.57018245520745,-1.62018255307363,
132.620239311468));
#215814=CARTESIAN_POINT('Ctrl Pts',(6.6118385134206,-1.4512584387472,132.62845876716));
#215815=CARTESIAN_POINT('Ctrl Pts',(6.64702757545373,-1.28051618323012,
132.636678222852));
#215816=CARTESIAN_POINT('Ctrl Pts',(6.67559245066795,-1.10849196324786,
132.644897678545));
#215817=CARTESIAN_POINT('Ctrl Pts',(6.70412906556926,-0.93663793334162,
132.653109002418));
#215818=CARTESIAN_POINT('Ctrl Pts',(6.72605448654629,-0.763504816106835,
132.661320326292));
#215819=CARTESIAN_POINT('Ctrl Pts',(6.74126185300704,-0.589641949993522,
132.669531650165));
#215820=CARTESIAN_POINT('Ctrl Pts',(6.75645722715312,-0.415916189683682,
132.677736498705));
#215821=CARTESIAN_POINT('Ctrl Pts',(6.76494506755597,-0.241462182364821,
132.685941347244));
#215822=CARTESIAN_POINT('Ctrl Pts',(6.76666991567789,-0.0668375063847751,
132.694146195783));
#215823=CARTESIAN_POINT('Ctrl Pts',(6.76839374978632,0.1076845102499,132.70234622081));
#215824=CARTESIAN_POINT('Ctrl Pts',(6.76336250840278,0.282376638002501,
132.710546245836));
#215825=CARTESIAN_POINT('Ctrl Pts',(6.75157271658027,0.456678062456395,
132.718746270862));
#215826=CARTESIAN_POINT('Ctrl Pts',(6.73978633698824,0.630929040164369,
132.726943922617));
#215827=CARTESIAN_POINT('Ctrl Pts',(6.72124532343041,0.804789182163561,
132.735141574373));
#215828=CARTESIAN_POINT('Ctrl Pts',(6.69599828685307,0.977699310862392,
132.743339226128));
#215829=CARTESIAN_POINT('Ctrl Pts',(6.67075463100586,1.15058628585447,132.751535780168));
#215830=CARTESIAN_POINT('Ctrl Pts',(6.63880679155738,1.32252314591521,132.759732334208));
#215831=CARTESIAN_POINT('Ctrl Pts',(6.60025507465575,1.49295745065993,132.767928888248));
#215832=CARTESIAN_POINT('Ctrl Pts',(6.56170151035774,1.66339992260816,132.776125835067));
#215833=CARTESIAN_POINT('Ctrl Pts',(6.51654351724407,1.83233934584685,132.784322781885));
#215834=CARTESIAN_POINT('Ctrl Pts',(6.46493220196712,1.9992350096896,132.792519728704));
#215835=CARTESIAN_POINT('Ctrl Pts',(6.41330902922189,2.16616901706283,132.800718558734));
#215836=CARTESIAN_POINT('Ctrl Pts',(6.35522968734433,2.33105798718433,132.808917388765));
#215837=CARTESIAN_POINT('Ctrl Pts',(6.29089469473621,2.4933778172872,132.817116218795));
#215838=CARTESIAN_POINT('Ctrl Pts',(6.22649876866193,2.65585138502914,132.825322814166));
#215839=CARTESIAN_POINT('Ctrl Pts',(6.15583548680489,2.81575061728925,132.833529409537));
#215840=CARTESIAN_POINT('Ctrl Pts',(6.07915332149875,2.97257193247038,132.841736004908));
#215841=CARTESIAN_POINT('Ctrl Pts',(6.00243404158102,3.12946915007523,132.849946572319));
#215842=CARTESIAN_POINT('Ctrl Pts',(5.9196902398935,3.2832851646876,132.85815713973));
#215843=CARTESIAN_POINT('Ctrl Pts',(5.83121559865078,3.43354243341361,132.866367707141));
#215844=CARTESIAN_POINT('Ctrl Pts',(5.74261893821646,3.58400692841603,132.874589598099));
#215845=CARTESIAN_POINT('Ctrl Pts',(5.6482758366476,3.73090256688787,132.882811489057));
#215846=CARTESIAN_POINT('Ctrl Pts',(5.54852311298748,3.87378113277503,132.891033380015));
#215847=CARTESIAN_POINT('Ctrl Pts',(5.45782436231733,4.003691444474,132.898509017879));
#215848=CARTESIAN_POINT('Ctrl Pts',(5.36265406615867,4.1302810409493,132.905984655743));
#215849=CARTESIAN_POINT('Ctrl Pts',(5.26329298321657,4.2532382925041,132.913460293607));
#215850=CARTESIAN_POINT('Ctrl Pts',(5.14450120317043,4.40024062328876,132.922397840407));
#215851=CARTESIAN_POINT('Ctrl Pts',(5.01947177254576,4.54235715527166,132.931335387207));
#215852=CARTESIAN_POINT('Ctrl Pts',(4.888612363018,4.67907663584895,132.940272934007));
#215853=CARTESIAN_POINT('Ctrl Pts',(4.75804937042662,4.81548642551658,132.949190235871));
#215854=CARTESIAN_POINT('Ctrl Pts',(4.62168293609941,4.94652337913678,132.958107537736));
#215855=CARTESIAN_POINT('Ctrl Pts',(4.47995901652833,5.07171136897857,132.967024839601));
#215856=CARTESIAN_POINT('Ctrl Pts',(4.33843991738055,5.19671843624111,132.975929254117));
#215857=CARTESIAN_POINT('Ctrl Pts',(4.19157897124605,5.31589323208888,132.984833668633));
#215858=CARTESIAN_POINT('Ctrl Pts',(4.03985879706266,5.42879635829117,132.99373808315));
#215859=CARTESIAN_POINT('Ctrl Pts',(3.88850419997671,5.54142743895046,133.002621042048));
#215860=CARTESIAN_POINT('Ctrl Pts',(3.7323139469524,5.64781685353747,133.011504000947));
#215861=CARTESIAN_POINT('Ctrl Pts',(3.57180300349476,5.74756577206611,133.020386959846));
#215862=CARTESIAN_POINT('Ctrl Pts',(3.41804157718929,5.84312022869689,133.028896388553));
#215863=CARTESIAN_POINT('Ctrl Pts',(3.2603155590624,5.93258100663783,133.037405817261));
#215864=CARTESIAN_POINT('Ctrl Pts',(3.09910619832141,6.01563211736936,133.045915245968));
#215865=CARTESIAN_POINT('Ctrl Pts',(3.09910619832127,6.01563211736944,131.045783168526));
#215866=CARTESIAN_POINT('Ctrl Pts',(2.94005916857604,6.09756924817982,131.054219631559));
#215867=CARTESIAN_POINT('Ctrl Pts',(2.77765505604874,6.17324937003544,131.062656094593));
#215868=CARTESIAN_POINT('Ctrl Pts',(2.61241474863898,6.24240163567625,131.071092557626));
#215869=CARTESIAN_POINT('Ctrl Pts',(2.44728583965193,6.31150728161851,131.079523333132));
#215870=CARTESIAN_POINT('Ctrl Pts',(2.27932485447001,6.37409371657269,131.087954108638));
#215871=CARTESIAN_POINT('Ctrl Pts',(2.10907500319488,6.42993714050912,131.096384884145));
#215872=CARTESIAN_POINT('Ctrl Pts',(1.93891377186047,6.48575149633839,131.10481127119));
#215873=CARTESIAN_POINT('Ctrl Pts',(1.76646636625224,6.53482973579416,131.113237658236));
#215874=CARTESIAN_POINT('Ctrl Pts',(1.59229396690954,6.57699695324116,131.121664045281));
#215875=CARTESIAN_POINT('Ctrl Pts',(1.41810494468684,6.61916819509499,131.130091236534));
#215876=CARTESIAN_POINT('Ctrl Pts',(1.24219091916096,6.65442699955921,131.138518427788));
#215877=CARTESIAN_POINT('Ctrl Pts',(1.06512733873329,6.68264863301094,131.146945619041));
#215878=CARTESIAN_POINT('Ctrl Pts',(0.888165580687034,6.71085403729844,
131.155367964144));
#215879=CARTESIAN_POINT('Ctrl Pts',(0.710055918205982,6.7320303049067,131.163790309247));
#215880=CARTESIAN_POINT('Ctrl Pts',(0.531382030646969,6.74610421928875,
131.172212654351));
#215881=CARTESIAN_POINT('Ctrl Pts',(0.352714136698274,6.76017766156176,
131.180634716927));
#215882=CARTESIAN_POINT('Ctrl Pts',(0.173482387848984,6.76714919961372,
131.189056779503));
#215883=CARTESIAN_POINT('Ctrl Pts',(-0.00572532888578081,6.7669975779964,
131.197478842078));
#215884=CARTESIAN_POINT('Ctrl Pts',(-0.184952050309111,6.76684594029986,
131.2059017978));
#215885=CARTESIAN_POINT('Ctrl Pts',(-0.36415440107678,6.75956963771297,
131.214324753523));
#215886=CARTESIAN_POINT('Ctrl Pts',(-0.542745036850973,6.74519953930005,
131.222747709245));
#215887=CARTESIAN_POINT('Ctrl Pts',(-0.721500802956766,6.73081615385724,
131.231178453088));
#215888=CARTESIAN_POINT('Ctrl Pts',(-0.899643389640689,6.70932588122367,
131.239609196931));
#215889=CARTESIAN_POINT('Ctrl Pts',(-1.07658955657966,6.68081162185132,
131.248039940774));
#215890=CARTESIAN_POINT('Ctrl Pts',(-1.25354079277129,6.65229654558653,
131.256470926145));
#215891=CARTESIAN_POINT('Ctrl Pts',(-1.42929521484197,6.61675715479673,
131.264901911517));
#215892=CARTESIAN_POINT('Ctrl Pts',(-1.60328020808028,6.5743274617544,131.273332896888));
#215893=CARTESIAN_POINT('Ctrl Pts',(-1.77744048076064,6.531855023342,131.281772375972));
#215894=CARTESIAN_POINT('Ctrl Pts',(-1.94982743830728,6.4824784923953,131.290211855056));
#215895=CARTESIAN_POINT('Ctrl Pts',(-2.11988227947715,6.4263821953848,131.298651334139));
#215896=CARTESIAN_POINT('Ctrl Pts',(-2.28958022503889,6.37040362817192,
131.307073101213));
#215897=CARTESIAN_POINT('Ctrl Pts',(-2.45695553865008,6.30773362669709,
131.315494868287));
#215898=CARTESIAN_POINT('Ctrl Pts',(-2.62147298918131,6.23860307817326,
131.32391663536));
#215899=CARTESIAN_POINT('Ctrl Pts',(-2.78048061325775,6.17178776930249,
131.33205635044));
#215900=CARTESIAN_POINT('Ctrl Pts',(-2.93713551430113,6.09880390692183,
131.340196065519));
#215901=CARTESIAN_POINT('Ctrl Pts',(-3.09092138236668,6.01984169293748,
131.348335780599));
#215902=CARTESIAN_POINT('Ctrl Pts',(-3.24457275022895,5.94094853883469,
131.356468376732));
#215903=CARTESIAN_POINT('Ctrl Pts',(-3.39535975619418,5.85608760681051,
131.364600972865));
#215904=CARTESIAN_POINT('Ctrl Pts',(-3.54278547864823,5.7654973811701,131.372733568998));
#215905=CARTESIAN_POINT('Ctrl Pts',(-3.69011041296322,5.67496908787165,
131.380860605252));
#215906=CARTESIAN_POINT('Ctrl Pts',(-3.83407832814475,5.57871949014853,
131.388987641506));
#215907=CARTESIAN_POINT('Ctrl Pts',(-3.97421640348247,5.47703322778773,
131.39711467776));
#215908=CARTESIAN_POINT('Ctrl Pts',(-4.11428749027271,5.37539557330882,
131.405237829142));
#215909=CARTESIAN_POINT('Ctrl Pts',(-4.25053208703943,5.26832664391953,
131.413360980525));
#215910=CARTESIAN_POINT('Ctrl Pts',(-4.38250592672784,5.15615465266465,
131.421484131908));
#215911=CARTESIAN_POINT('Ctrl Pts',(-4.51444268078081,5.0440141825778,131.429605000624));
#215912=CARTESIAN_POINT('Ctrl Pts',(-4.64211078986738,4.92677374443147,
131.437725869341));
#215913=CARTESIAN_POINT('Ctrl Pts',(-4.76509872085858,4.8048020958695,131.445846738057));
#215914=CARTESIAN_POINT('Ctrl Pts',(-4.88809329857753,4.68282385550348,
131.453968045656));
#215915=CARTESIAN_POINT('Ctrl Pts',(-5.0064069300545,4.556114148958,131.462089353254));
#215916=CARTESIAN_POINT('Ctrl Pts',(-5.11966451445874,4.42507901165527,
131.470210660853));
#215917=CARTESIAN_POINT('Ctrl Pts',(-5.17851708823133,4.35698860406379,
131.474430774297));
#215918=CARTESIAN_POINT('Ctrl Pts',(-5.23600505119378,4.28773083069518,
131.478650887741));
#215919=CARTESIAN_POINT('Ctrl Pts',(-5.29208000568025,4.21736626503786,
131.482871001185));
#215920=CARTESIAN_POINT('Ctrl Pts',(-5.41146115058981,4.0675631579972,131.491855439589));
#215921=CARTESIAN_POINT('Ctrl Pts',(-5.52437645878455,3.91281606115083,
131.500839877993));
#215922=CARTESIAN_POINT('Ctrl Pts',(-5.63046266527174,3.75368874242139,
131.509824316397));
#215923=CARTESIAN_POINT('Ctrl Pts',(-5.73673197018465,3.5942867794897,131.518824261402));
#215924=CARTESIAN_POINT('Ctrl Pts',(-5.83614848254495,3.43048968312826,
131.527824206408));
#215925=CARTESIAN_POINT('Ctrl Pts',(-5.92839372845277,3.26288780077432,
131.536824151413));
#215926=CARTESIAN_POINT('Ctrl Pts',(-6.02085635263005,3.09489096031943,
131.545845305018));
#215927=CARTESIAN_POINT('Ctrl Pts',(-6.10611378196859,2.92307160440881,
131.554866458623));
#215928=CARTESIAN_POINT('Ctrl Pts',(-6.18389355657347,2.74804466502441,
131.563887612228));
#215929=CARTESIAN_POINT('Ctrl Pts',(-6.26175247270942,2.5728396343556,131.572917944928));
#215930=CARTESIAN_POINT('Ctrl Pts',(-6.33211844258303,2.39442072067031,
131.581948277627));
#215931=CARTESIAN_POINT('Ctrl Pts',(-6.39476764691178,2.21342172710273,
131.590978610327));
#215932=CARTESIAN_POINT('Ctrl Pts',(-6.45750566807776,2.03216613397694,
131.600021745193));
#215933=CARTESIAN_POINT('Ctrl Pts',(-6.51250497081679,1.84832337316261,
131.60906488006));
#215934=CARTESIAN_POINT('Ctrl Pts',(-6.5595913082107,1.66254349394134,131.618108014927));
#215935=CARTESIAN_POINT('Ctrl Pts',(-6.60075561899143,1.50012906316717,
131.626013798954));
#215936=CARTESIAN_POINT('Ctrl Pts',(-6.63587296388161,1.3362344347959,131.633919582982));
#215937=CARTESIAN_POINT('Ctrl Pts',(-6.66485893493869,1.17130029342092,
131.64182536701));
#215938=CARTESIAN_POINT('Ctrl Pts',(-6.69981997936319,0.972367167034594,
131.651360823526));
#215939=CARTESIAN_POINT('Ctrl Pts',(-6.72588152660799,0.771803127922735,
131.660896280042));
#215940=CARTESIAN_POINT('Ctrl Pts',(-6.74292139287532,0.570350847728295,
131.670431736559));
#215941=CARTESIAN_POINT('Ctrl Pts',(-6.75885431812254,0.381985277783969,
131.6793477523));
#215942=CARTESIAN_POINT('Ctrl Pts',(-6.7669000369816,0.192843308266294,
131.688263768042));
#215943=CARTESIAN_POINT('Ctrl Pts',(-6.76699907392669,0.00354026487731378,
131.697179783784));
#215944=CARTESIAN_POINT('',(-6.76699797440541,-0.00523587558187145,131.302820216153));
#215945=CARTESIAN_POINT('Ctrl Pts',(3.0991061983213,6.01563211736942,130.651283639301));
#215946=CARTESIAN_POINT('Ctrl Pts',(2.94215097151982,6.09649160258211,130.659605302688));
#215947=CARTESIAN_POINT('Ctrl Pts',(2.78216153052165,6.17113635103588,130.667926966075));
#215948=CARTESIAN_POINT('Ctrl Pts',(2.6196709735354,6.23935998243539,130.676248629462));
#215949=CARTESIAN_POINT('Ctrl Pts',(2.45695092246554,6.30767996970971,130.684582045979));
#215950=CARTESIAN_POINT('Ctrl Pts',(2.2917230233006,6.36956059997624,130.692915462495));
#215951=CARTESIAN_POINT('Ctrl Pts',(2.12453663340948,6.42484498593555,130.701248879011));
#215952=CARTESIAN_POINT('Ctrl Pts',(2.04748763072223,6.45032317710359,130.705089391579));
#215953=CARTESIAN_POINT('Ctrl Pts',(1.97002282961067,6.47440110779183,130.708929904147));
#215954=CARTESIAN_POINT('Ctrl Pts',(1.89219669411109,6.49706708221449,130.712770416715));
#215955=CARTESIAN_POINT('Ctrl Pts',(1.72866515570096,6.54469377783683,130.720840262718));
#215956=CARTESIAN_POINT('Ctrl Pts',(1.56303228692083,6.58623017011433,130.728910108722));
#215957=CARTESIAN_POINT('Ctrl Pts',(1.39580167597483,6.62148221181224,130.736979954725));
#215958=CARTESIAN_POINT('Ctrl Pts',(1.22878146240835,6.65668990195779,130.745039647836));
#215959=CARTESIAN_POINT('Ctrl Pts',(1.06016786676457,6.68562889732855,130.753099340946));
#215960=CARTESIAN_POINT('Ctrl Pts',(0.89048205076826,6.70815404692376,130.761159034057));
#215961=CARTESIAN_POINT('Ctrl Pts',(0.720972480443196,6.73065580057343,
130.769210355896));
#215962=CARTESIAN_POINT('Ctrl Pts',(0.550393272684829,6.74675691681266,
130.777261677735));
#215963=CARTESIAN_POINT('Ctrl Pts',(0.37927817132368,6.75636270997623,130.785312999574));
#215964=CARTESIAN_POINT('Ctrl Pts',(0.208303303024427,6.7659606309545,130.793357723156));
#215965=CARTESIAN_POINT('Ctrl Pts',(0.0367937858360792,6.76907380268978,
130.801402446737));
#215966=CARTESIAN_POINT('Ctrl Pts',(-0.134709183319342,6.76565905407075,
130.809447170319));
#215967=CARTESIAN_POINT('Ctrl Pts',(-0.306109143619822,6.76224635643279,
130.817487062044));
#215968=CARTESIAN_POINT('Ctrl Pts',(-0.477502191633343,6.75231355100528,
130.825526953769));
#215969=CARTESIAN_POINT('Ctrl Pts',(-0.648344889022779,6.73586949880103,
130.833566845494));
#215970=CARTESIAN_POINT('Ctrl Pts',(-0.822866297722585,6.71907136110319,
130.841779858113));
#215971=CARTESIAN_POINT('Ctrl Pts',(-0.9968129878807,6.69547836327735,130.849992870733));
#215972=CARTESIAN_POINT('Ctrl Pts',(-1.16960825650072,6.66515607666657,
130.858205883353));
#215973=CARTESIAN_POINT('Ctrl Pts',(-1.33870218006575,6.63548330578907,
130.866242969896));
#215974=CARTESIAN_POINT('Ctrl Pts',(-1.50669312963795,6.5993666940462,130.874280056439));
#215975=CARTESIAN_POINT('Ctrl Pts',(-1.67304879419528,6.55691975947866,
130.882317142982));
#215976=CARTESIAN_POINT('Ctrl Pts',(-1.83942037976398,6.51446876254193,
130.890354998712));
#215977=CARTESIAN_POINT('Ctrl Pts',(-2.00415600662239,6.46568632870257,
130.898392854441));
#215978=CARTESIAN_POINT('Ctrl Pts',(-2.16673676216277,6.41073636983244,
130.906430710171));
#215979=CARTESIAN_POINT('Ctrl Pts',(-2.32936529011382,6.35577026457406,
130.914470927729));
#215980=CARTESIAN_POINT('Ctrl Pts',(-2.48983733266218,6.29463314662318,
130.922511145286));
#215981=CARTESIAN_POINT('Ctrl Pts',(-2.64765239694011,6.22753769839872,
130.930551362844));
#215982=CARTESIAN_POINT('Ctrl Pts',(-2.81142981543061,6.15790734116419,
130.93889534497));
#215983=CARTESIAN_POINT('Ctrl Pts',(-2.97234515995403,6.08185981477191,
130.947239327097));
#215984=CARTESIAN_POINT('Ctrl Pts',(-3.12986636674479,5.99968545228163,
130.955583309224));
#215985=CARTESIAN_POINT('Ctrl Pts',(-3.2819172246423,5.92036481623276,130.963637524059));
#215986=CARTESIAN_POINT('Ctrl Pts',(-3.43080544743115,5.83533599211421,
130.971691738895));
#215987=CARTESIAN_POINT('Ctrl Pts',(-3.57608202193723,5.74490438322322,
130.979745953731));
#215988=CARTESIAN_POINT('Ctrl Pts',(-3.72146731193647,5.65440510122669,
130.987806195814));
#215989=CARTESIAN_POINT('Ctrl Pts',(-3.86323526487362,5.55849519204986,
130.995866437898));
#215990=CARTESIAN_POINT('Ctrl Pts',(-4.0009693626104,5.45752078873301,131.003926679981));
#215991=CARTESIAN_POINT('Ctrl Pts',(-4.13889602206308,5.35640521627442,
131.011998190836));
#215992=CARTESIAN_POINT('Ctrl Pts',(-4.27277728439513,5.25021125280951,
131.020069701691));
#215993=CARTESIAN_POINT('Ctrl Pts',(-4.4022325033873,5.1393227166739,131.028141212546));
#215994=CARTESIAN_POINT('Ctrl Pts',(-4.41580076188398,5.1277004403816,131.028987191152));
#215995=CARTESIAN_POINT('Ctrl Pts',(-4.42932043529909,5.11602662362992,
131.029833169758));
#215996=CARTESIAN_POINT('Ctrl Pts',(-4.44279111095812,5.10430172936431,
131.030679148365));
#215997=CARTESIAN_POINT('Ctrl Pts',(-4.57265722657723,4.99126608713964,
131.038834934924));
#215998=CARTESIAN_POINT('Ctrl Pts',(-4.69841388164103,4.87309066680269,
131.046990721484));
#215999=CARTESIAN_POINT('Ctrl Pts',(-4.81962338408803,4.75010730779336,
131.055146508044));
#216000=CARTESIAN_POINT('Ctrl Pts',(-4.94068725651242,4.62727171004854,
131.063292495642));
#216001=CARTESIAN_POINT('Ctrl Pts',(-5.05721459776948,4.49963993107349,
131.071438483239));
#216002=CARTESIAN_POINT('Ctrl Pts',(-5.16880017635472,4.36758442813822,
131.079584470836));
#216003=CARTESIAN_POINT('Ctrl Pts',(-5.28027520313374,4.23565975729215,
131.087722387914));
#216004=CARTESIAN_POINT('Ctrl Pts',(-5.38681798059027,4.09932036614932,
131.095860304991));
#216005=CARTESIAN_POINT('Ctrl Pts',(-5.48805961471042,3.95897596170835,
131.103998222068));
#216006=CARTESIAN_POINT('Ctrl Pts',(-5.59112173423524,3.81610794193725,
131.112282471822));
#216007=CARTESIAN_POINT('Ctrl Pts',(-5.68868996036298,3.66908975731962,
131.120566721575));
#216008=CARTESIAN_POINT('Ctrl Pts',(-5.78041677989208,3.51839037782081,
131.128850971329));
#216009=CARTESIAN_POINT('Ctrl Pts',(-5.87040026679604,3.37055514586596,
131.136977773098));
#216010=CARTESIAN_POINT('Ctrl Pts',(-5.95476219107801,3.2191777168747,131.145104574867));
#216011=CARTESIAN_POINT('Ctrl Pts',(-6.03321733768647,3.0647312371951,131.153231376636));
#216012=CARTESIAN_POINT('Ctrl Pts',(-6.11164946317512,2.9103300767975,131.161355793755));
#216013=CARTESIAN_POINT('Ctrl Pts',(-6.18417809602116,2.75286198456227,
131.169480210873));
#216014=CARTESIAN_POINT('Ctrl Pts',(-6.25056370359283,2.59282517484846,
131.177604627992));
#216015=CARTESIAN_POINT('Ctrl Pts',(-6.31694248689683,2.43280481650213,
131.185728209942));
#216016=CARTESIAN_POINT('Ctrl Pts',(-6.37717936281698,2.27021660475608,
131.193851791892));
#216017=CARTESIAN_POINT('Ctrl Pts',(-6.43108274969321,2.10557917604596,
131.201975373842));
#216018=CARTESIAN_POINT('Ctrl Pts',(-6.48684508236007,1.93526395837273,
131.210379110701));
#216019=CARTESIAN_POINT('Ctrl Pts',(-6.53582912103941,1.76275604363099,
131.21878284756));
#216020=CARTESIAN_POINT('Ctrl Pts',(-6.57787883692022,1.58864691067497,
131.22718658442));
#216021=CARTESIAN_POINT('Ctrl Pts',(-6.61855578425189,1.42022180047233,
131.235315970182));
#216022=CARTESIAN_POINT('Ctrl Pts',(-6.65274400306477,1.25029874997547,
131.243445355945));
#216023=CARTESIAN_POINT('Ctrl Pts',(-6.68035434969251,1.07942334722959,
131.251574741708));
#216024=CARTESIAN_POINT('Ctrl Pts',(-6.70936239027104,0.899897871379726,
131.260115654116));
#216025=CARTESIAN_POINT('Ctrl Pts',(-6.73110920848742,0.719321575123651,
131.268656566523));
#216026=CARTESIAN_POINT('Ctrl Pts',(-6.74555314380781,0.538332410379065,
131.277197478931));
#216027=CARTESIAN_POINT('Ctrl Pts',(-6.7599970791282,0.357343245634606,
131.285738391338));
#216028=CARTESIAN_POINT('Ctrl Pts',(-6.76713815815236,0.175941678540549,
131.294279303746));
#216029=CARTESIAN_POINT('Ctrl Pts',(-6.76699797440541,-0.00523587558206445,
131.302820216153));
#216030=CARTESIAN_POINT('Ctrl Pts',(-6.76699797440481,-0.0052358763600726,
131.30282021619));
#216031=CARTESIAN_POINT('Ctrl Pts',(-6.76680115043988,-0.259616858714105,
131.314812020025));
#216032=CARTESIAN_POINT('Ctrl Pts',(-6.75225713895637,-0.513482533726184,
131.326803823861));
#216033=CARTESIAN_POINT('Ctrl Pts',(-6.72355946680874,-0.765530597877477,
131.338795627696));
#216034=CARTESIAN_POINT('Ctrl Pts',(-6.71574816362024,-0.834136296521997,
131.342059711802));
#216035=CARTESIAN_POINT('Ctrl Pts',(-6.70688848524606,-0.902607492201805,
131.345323795908));
#216036=CARTESIAN_POINT('Ctrl Pts',(-6.69698490228259,-0.970918234764971,
131.348587880014));
#216037=CARTESIAN_POINT('Ctrl Pts',(-6.66987228678325,-1.1579296330053,
131.357523823465));
#216038=CARTESIAN_POINT('Ctrl Pts',(-6.63490476040764,-1.34392386470323,
131.366459766916));
#216039=CARTESIAN_POINT('Ctrl Pts',(-6.59217187828101,-1.52825355461753,
131.375395710367));
#216040=CARTESIAN_POINT('Ctrl Pts',(-6.54950323501061,-1.7123061481166,
131.384318220724));
#216041=CARTESIAN_POINT('Ctrl Pts',(-6.49909258658803,-1.8946989417192,
131.393240731082));
#216042=CARTESIAN_POINT('Ctrl Pts',(-6.44108064357375,-2.0747937591432,
131.40216324144));
#216043=CARTESIAN_POINT('Ctrl Pts',(-6.38321084782317,-2.25444728837425,
131.411063888878));
#216044=CARTESIAN_POINT('Ctrl Pts',(-6.31777700975614,-2.43181383409002,
131.419964536317));
#216045=CARTESIAN_POINT('Ctrl Pts',(-6.2449696302004,-2.60627000095437,
131.428865183755));
#216046=CARTESIAN_POINT('Ctrl Pts',(-6.17227476546436,-2.78045656734307,
131.437752076341));
#216047=CARTESIAN_POINT('Ctrl Pts',(-6.09222918802415,-2.95174148937959,
131.446638968927));
#216048=CARTESIAN_POINT('Ctrl Pts',(-6.00507248150573,-3.11951815059035,
131.455525861514));
#216049=CARTESIAN_POINT('Ctrl Pts',(-5.91813980025813,-3.28686356315181,
131.464389911468));
#216050=CARTESIAN_POINT('Ctrl Pts',(-5.82413258159977,-3.45071848031863,
131.473253961423));
#216051=CARTESIAN_POINT('Ctrl Pts',(-5.7233372620906,-3.61049852296954,
131.482118011378));
#216052=CARTESIAN_POINT('Ctrl Pts',(-5.62696882821723,-3.7632610971592,
131.490592756198));
#216053=CARTESIAN_POINT('Ctrl Pts',(-5.52439583947663,-3.91229879426962,
131.499067501019));
#216054=CARTESIAN_POINT('Ctrl Pts',(-5.41590930921664,-4.05711909541002,
131.507542245839));
#216055=CARTESIAN_POINT('Ctrl Pts',(-5.31082571521176,-4.19739676575517,
131.515751160272));
#216056=CARTESIAN_POINT('Ctrl Pts',(-5.20029426297779,-4.33358166469833,
131.523960074704));
#216057=CARTESIAN_POINT('Ctrl Pts',(-5.08467554832049,-4.46523947491193,
131.532168989137));
#216058=CARTESIAN_POINT('Ctrl Pts',(-4.96902934590067,-4.5969285861016,
131.540379855197));
#216059=CARTESIAN_POINT('Ctrl Pts',(-4.84829370641897,-4.72408819672218,
131.548590721257));
#216060=CARTESIAN_POINT('Ctrl Pts',(-4.7228675867584,-4.84631930004069,
131.556801587318));
#216061=CARTESIAN_POINT('Ctrl Pts',(-4.59738928994214,-4.9686012513909,
131.565015869091));
#216062=CARTESIAN_POINT('Ctrl Pts',(-4.46721688047966,-5.08595036258548,
131.573230150864));
#216063=CARTESIAN_POINT('Ctrl Pts',(-4.33278407556525,-5.19800645964664,
131.581444432638));
#216064=CARTESIAN_POINT('Ctrl Pts',(-4.19819995591528,-5.31018868469201,
131.589667960234));
#216065=CARTESIAN_POINT('Ctrl Pts',(-4.05934613642189,-5.41706576802213,
131.59789148783));
#216066=CARTESIAN_POINT('Ctrl Pts',(-3.91668791095474,-5.51831902015287,
131.606115015426));
#216067=CARTESIAN_POINT('Ctrl Pts',(-3.77393824711408,-5.61963717167976,
131.614343813983));
#216068=CARTESIAN_POINT('Ctrl Pts',(-3.62737961373741,-5.71532411219014,
131.622572612541));
#216069=CARTESIAN_POINT('Ctrl Pts',(-3.47750376914315,-5.80510607444819,
131.630801411098));
#216070=CARTESIAN_POINT('Ctrl Pts',(-3.32742163244156,-5.89501161439311,
131.639041535938));
#216071=CARTESIAN_POINT('Ctrl Pts',(-3.17401347602669,-5.97899577119909,
131.647281660778));
#216072=CARTESIAN_POINT('Ctrl Pts',(-3.01779388326723,-6.05683160390933,
131.655521785618));
#216073=CARTESIAN_POINT('Ctrl Pts',(-2.94843883146674,-6.09138750124716,
131.659180060967));
#216074=CARTESIAN_POINT('Ctrl Pts',(-2.87852989137046,-6.12473221224536,
131.662838336315));
#216075=CARTESIAN_POINT('Ctrl Pts',(-2.80811313775106,-6.15684899973923,
131.666496611664));
#216076=CARTESIAN_POINT('Ctrl Pts',(-2.64550035440514,-6.2310160116798,
131.674944634415));
#216077=CARTESIAN_POINT('Ctrl Pts',(-2.47980626960971,-6.29880116643513,
131.683392657166));
#216078=CARTESIAN_POINT('Ctrl Pts',(-2.31155964751762,-6.35995133597485,
131.691840679918));
#216079=CARTESIAN_POINT('Ctrl Pts',(-2.14346709388374,-6.42104550847746,
131.700280966562));
#216080=CARTESIAN_POINT('Ctrl Pts',(-1.97282697409764,-6.47551669336166,
131.708721253207));
#216081=CARTESIAN_POINT('Ctrl Pts',(-1.80018895131744,-6.52315941393085,
131.717161539851));
#216082=CARTESIAN_POINT('Ctrl Pts',(-1.62768244167816,-6.57076584096677,
131.725595396808));
#216083=CARTESIAN_POINT('Ctrl Pts',(-1.45318138346915,-6.61155408513223,
131.734029253764));
#216084=CARTESIAN_POINT('Ctrl Pts',(-1.27725193784871,-6.64536804753971,
131.742463110721));
#216085=CARTESIAN_POINT('Ctrl Pts',(-1.10142946646511,-6.67916144930249,
131.750891839454));
#216086=CARTESIAN_POINT('Ctrl Pts',(-0.924180666001446,-6.70598896138486,
131.759320568188));
#216087=CARTESIAN_POINT('Ctrl Pts',(-0.746083654274415,-6.7257451766198,
131.767749296922));
#216088=CARTESIAN_POINT('Ctrl Pts',(-0.568067585684722,-6.74549241287173,
131.776174194891));
#216089=CARTESIAN_POINT('Ctrl Pts',(-0.38920440544877,-6.75817472396021,
131.78459909286));
#216090=CARTESIAN_POINT('Ctrl Pts',(-0.210079545123407,-6.76373828475945,
131.793023990828));
#216091=CARTESIAN_POINT('Ctrl Pts',(-0.030994343332114,-6.76930061377733,
131.801447023511));
#216092=CARTESIAN_POINT('Ctrl Pts',(0.148352090080952,-6.76774732196723,
131.809870056194));
#216093=CARTESIAN_POINT('Ctrl Pts',(0.327371574155583,-6.75907662720544,
131.818293088877));
#216094=CARTESIAN_POINT('Ctrl Pts',(0.506370802380278,-6.75040691352285,
131.826715168504));
#216095=CARTESIAN_POINT('Ctrl Pts',(0.685042821999834,-6.7346214184739,
131.83513724813));
#216096=CARTESIAN_POINT('Ctrl Pts',(0.862801510431626,-6.71177044851781,
131.843559327756));
#216097=CARTESIAN_POINT('Ctrl Pts',(1.04056489945689,-6.68891887429802,
131.851981630093));
#216098=CARTESIAN_POINT('Ctrl Pts',(1.21741457844043,-6.65900149556442,
131.860403932431));
#216099=CARTESIAN_POINT('Ctrl Pts',(1.39277121929909,-6.6221203047583,131.868826234768));
#216100=CARTESIAN_POINT('Ctrl Pts',(1.56815697713251,-6.58523299003981,
131.87724993558));
#216101=CARTESIAN_POINT('Ctrl Pts',(1.74204887641515,-6.54137962714381,
131.885673636393));
#216102=CARTESIAN_POINT('Ctrl Pts',(1.91387906150491,-6.49071305311929,
131.894097337206));
#216103=CARTESIAN_POINT('Ctrl Pts',(2.08582552565676,-6.44001219255946,
131.902526738414));
#216104=CARTESIAN_POINT('Ctrl Pts',(2.25570716752529,-6.38248900226481,
131.910956139622));
#216105=CARTESIAN_POINT('Ctrl Pts',(2.42297157202295,-6.31834612546422,
131.91938554083));
#216106=CARTESIAN_POINT('Ctrl Pts',(2.59029565623062,-6.25418036257319,
131.927817949638));
#216107=CARTESIAN_POINT('Ctrl Pts',(2.75500033192922,-6.18339032881242,
131.936250358445));
#216108=CARTESIAN_POINT('Ctrl Pts',(2.91655384726697,-6.10622654804031,
131.944682767252));
#216109=CARTESIAN_POINT('Ctrl Pts',(3.0782568366238,-6.02899137309014,131.953122977969));
#216110=CARTESIAN_POINT('Ctrl Pts',(3.2368025420005,-5.94537081795523,131.961563188686));
#216111=CARTESIAN_POINT('Ctrl Pts',(3.39168348224042,-5.85566154728033,
131.970003399404));
#216112=CARTESIAN_POINT('Ctrl Pts',(3.4797771206816,-5.8046364434592,131.974804047373));
#216113=CARTESIAN_POINT('Ctrl Pts',(3.56668565016117,-5.75164237058268,
131.979604695343));
#216114=CARTESIAN_POINT('Ctrl Pts',(3.65231993181012,-5.69674013061001,
131.984405343313));
#216115=CARTESIAN_POINT('Ctrl Pts',(3.79751671734005,-5.60365090735823,
131.992545058392));
#216116=CARTESIAN_POINT('Ctrl Pts',(3.93933796368613,-5.50488787645263,
132.000684773471));
#216117=CARTESIAN_POINT('Ctrl Pts',(4.07730761878017,-5.4007269493872,132.008824488551));
#216118=CARTESIAN_POINT('Ctrl Pts',(4.21515660643658,-5.29665712084747,
132.016957084684));
#216119=CARTESIAN_POINT('Ctrl Pts',(4.34916041770699,-5.18719901234504,
132.025089680817));
#216120=CARTESIAN_POINT('Ctrl Pts',(4.47887038021226,-5.07267277845292,
132.03322227695));
#216121=CARTESIAN_POINT('Ctrl Pts',(4.60849166602303,-4.95822484084321,
132.041349313204));
#216122=CARTESIAN_POINT('Ctrl Pts',(4.73382467411888,-4.83871591755658,
132.049476349458));
#216123=CARTESIAN_POINT('Ctrl Pts',(4.85445238991508,-4.71450750280957,
132.057603385712));
#216124=CARTESIAN_POINT('Ctrl Pts',(4.97502244347042,-4.59035846194261,
132.065726537095));
#216125=CARTESIAN_POINT('Ctrl Pts',(5.09089142905951,-4.46151466516838,
132.073849688477));
#216126=CARTESIAN_POINT('Ctrl Pts',(5.20167793395675,-4.3283756388959,132.08197283986));
#216127=CARTESIAN_POINT('Ctrl Pts',(5.31243330701791,-4.19527402568509,
132.090093708577));
#216128=CARTESIAN_POINT('Ctrl Pts',(5.41810881068375,-4.05787986882479,
132.098214577293));
#216129=CARTESIAN_POINT('Ctrl Pts',(5.51836223316075,-3.91662702636147,
132.10633544601));
#216130=CARTESIAN_POINT('Ctrl Pts',(5.6186210737078,-3.77536655006606,132.114456753608));
#216131=CARTESIAN_POINT('Ctrl Pts',(5.71345703244159,-3.63024726789743,
132.122578061207));
#216132=CARTESIAN_POINT('Ctrl Pts',(5.80257018197704,-3.48173351697556,
132.130699368805));
#216133=CARTESIAN_POINT('Ctrl Pts',(5.84887646896811,-3.40456061479266,
132.13491948225));
#216134=CARTESIAN_POINT('Ctrl Pts',(5.89363819746646,-3.3264716096768,132.139139595694));
#216135=CARTESIAN_POINT('Ctrl Pts',(5.93681807242065,-3.24753447633425,
132.143359709138));
#216136=CARTESIAN_POINT('Ctrl Pts',(6.02874615254374,-3.07948074467572,
132.152344147542));
#216137=CARTESIAN_POINT('Ctrl Pts',(6.11345645332912,-2.9076648672125,132.161328585946));
#216138=CARTESIAN_POINT('Ctrl Pts',(6.19068775269391,-2.73270454836334,
132.17031302435));
#216139=CARTESIAN_POINT('Ctrl Pts',(6.26805234864637,-2.55744225850405,
132.179312969356));
#216140=CARTESIAN_POINT('Ctrl Pts',(6.33791204644033,-2.37902489855576,
132.188312914361));
#216141=CARTESIAN_POINT('Ctrl Pts',(6.40005430909273,-2.19808867898082,
132.197312859367));
#216142=CARTESIAN_POINT('Ctrl Pts',(6.46234301156852,-2.01672607859981,
132.206334012972));
#216143=CARTESIAN_POINT('Ctrl Pts',(6.51687781307106,-1.83283296902651,
132.215355166577));
#216144=CARTESIAN_POINT('Ctrl Pts',(6.56349572446274,-1.64706189166021,
132.224376320181));
#216145=CARTESIAN_POINT('Ctrl Pts',(6.61016106994521,-1.46110179076443,
132.233406652881));
#216146=CARTESIAN_POINT('Ctrl Pts',(6.64889338012126,-1.27326013770002,
132.242436985581));
#216147=CARTESIAN_POINT('Ctrl Pts',(6.67958082179362,-1.08419972566262,
132.25146731828));
#216148=CARTESIAN_POINT('Ctrl Pts',(6.71031176859167,-0.894871285515337,
132.260510453147));
#216149=CARTESIAN_POINT('Ctrl Pts',(6.73297500382871,-0.704320867581619,
132.269553588014));
#216150=CARTESIAN_POINT('Ctrl Pts',(6.74751031811957,-0.513218770964102,
132.278596722881));
#216151=CARTESIAN_POINT('Ctrl Pts',(6.76021753273533,-0.346151495592786,
132.286502506908));
#216152=CARTESIAN_POINT('Ctrl Pts',(6.76671353600646,-0.178662752507999,
132.294408290935));
#216153=CARTESIAN_POINT('Ctrl Pts',(6.76699072954348,-0.0112011728232508,
132.302314074962));
#216154=CARTESIAN_POINT('Ctrl Pts',(6.7672941356706,0.172096280214045,132.310967463275));
#216155=CARTESIAN_POINT('Ctrl Pts',(6.76014593713099,0.355523123183739,
132.319620851587));
#216156=CARTESIAN_POINT('Ctrl Pts',(6.74554260586999,0.538464439301936,
132.3282742399));
#216157=CARTESIAN_POINT('Ctrl Pts',(6.73095276182253,0.721236796122272,
132.336919636194));
#216158=CARTESIAN_POINT('Ctrl Pts',(6.70892154213067,0.903524218465778,
132.345565032488));
#216159=CARTESIAN_POINT('Ctrl Pts',(6.67949743572514,1.08471332901432,132.354210428782));
#216160=CARTESIAN_POINT('Ctrl Pts',(6.64913362291565,1.27168900671169,132.363131929782));
#216161=CARTESIAN_POINT('Ctrl Pts',(6.6108968903199,1.45749473334196,132.372053430783));
#216162=CARTESIAN_POINT('Ctrl Pts',(6.56489857922134,1.64146143559257,132.380974931783));
#216163=CARTESIAN_POINT('Ctrl Pts',(6.52040873093351,1.81939515701996,132.389603862205));
#216164=CARTESIAN_POINT('Ctrl Pts',(6.46865835845453,1.99560822897561,132.398232792628));
#216165=CARTESIAN_POINT('Ctrl Pts',(6.40980027306129,2.16950442715923,132.40686172305));
#216166=CARTESIAN_POINT('Ctrl Pts',(6.34794874411817,2.35224475354242,132.415929509339));
#216167=CARTESIAN_POINT('Ctrl Pts',(6.27824773848932,2.5324260628253,132.424997295629));
#216168=CARTESIAN_POINT('Ctrl Pts',(6.20093451363,2.70937265020379,132.434065081918));
#216169=CARTESIAN_POINT('Ctrl Pts',(6.12362128877068,2.88631923758228,132.443132868208));
#216170=CARTESIAN_POINT('Ctrl Pts',(6.03869596877439,3.06003073111488,132.452200654497));
#216171=CARTESIAN_POINT('Ctrl Pts',(5.94645565075196,3.22985358702838,132.461268440787));
#216172=CARTESIAN_POINT('Ctrl Pts',(5.86075439919666,3.38763742392869,132.469693396929));
#216173=CARTESIAN_POINT('Ctrl Pts',(5.76877634762448,3.54199530509277,132.478118353071));
#216174=CARTESIAN_POINT('Ctrl Pts',(5.67082881403919,3.6924232641807,132.486543309213));
#216175=CARTESIAN_POINT('Ctrl Pts',(5.57285854588218,3.84288613905569,132.494970220868));
#216176=CARTESIAN_POINT('Ctrl Pts',(5.46891621402277,3.98941699522619,132.503397132524));
#216177=CARTESIAN_POINT('Ctrl Pts',(5.35935229455184,4.13154111475149,132.51182404418));
#216178=CARTESIAN_POINT('Ctrl Pts',(5.24974808415041,4.27371749886397,132.52025405474));
#216179=CARTESIAN_POINT('Ctrl Pts',(5.13451836654412,4.41148365264945,132.5286840653));
#216180=CARTESIAN_POINT('Ctrl Pts',(5.01405393209504,4.54439788817422,132.537114075861));
#216181=CARTESIAN_POINT('Ctrl Pts',(4.89347852831402,4.67743456152877,132.545551851971));
#216182=CARTESIAN_POINT('Ctrl Pts',(4.76765899638341,4.80561014110518,132.553989628082));
#216183=CARTESIAN_POINT('Ctrl Pts',(4.63702380340669,4.92851897091203,132.562427404193));
#216184=CARTESIAN_POINT('Ctrl Pts',(4.5063200365742,5.051492318803,132.570869609514));
#216185=CARTESIAN_POINT('Ctrl Pts',(4.37079581374232,5.16919318187508,132.579311814836));
#216186=CARTESIAN_POINT('Ctrl Pts',(4.2309131390712,5.28125581747701,132.587754020158));
#216187=CARTESIAN_POINT('Ctrl Pts',(4.09088289586226,5.39343667300373,132.596205131542));
#216188=CARTESIAN_POINT('Ctrl Pts',(3.94648527943532,5.49996721837308,132.604656242927));
#216189=CARTESIAN_POINT('Ctrl Pts',(3.79821261674009,5.60052407530192,132.613107354311));
#216190=CARTESIAN_POINT('Ctrl Pts',(3.7565996654621,5.6287455121601,132.615479171745));
#216191=CARTESIAN_POINT('Ctrl Pts',(3.71468165514017,5.65649670150209,132.617850989178));
#216192=CARTESIAN_POINT('Ctrl Pts',(3.67246982934908,5.68377113829548,132.620222806612));
#216193=CARTESIAN_POINT('Ctrl Pts',(3.52444787496525,5.77941294869373,132.628539932094));
#216194=CARTESIAN_POINT('Ctrl Pts',(3.37254386156039,5.86936147603194,132.636857057577));
#216195=CARTESIAN_POINT('Ctrl Pts',(3.21722995071989,5.95329492333371,132.645174183059));
#216196=CARTESIAN_POINT('Ctrl Pts',(3.17806936885764,5.97445775811299,132.647271248747));
#216197=CARTESIAN_POINT('Ctrl Pts',(3.13869216104785,5.99523839979182,132.649368314435));
#216198=CARTESIAN_POINT('Ctrl Pts',(3.09910619832128,6.01563211736943,132.651465380124));
#216199=CARTESIAN_POINT('Origin',(0.,0.,4.30282021618968));
#216200=CARTESIAN_POINT('',(3.09910619832134,6.0156321173694,135.045755263024));
#216201=CARTESIAN_POINT('',(3.0991061983213,6.01563211736942,134.651530974814));
#216202=CARTESIAN_POINT('',(3.09910619832133,6.0156321173694,4.30282021618968));
#216203=CARTESIAN_POINT('',(-6.767,6.55463713633477E-12,133.69717978381));
#216204=CARTESIAN_POINT('Ctrl Pts',(-6.767,6.93929656985413E-12,133.69717978381));
#216205=CARTESIAN_POINT('Ctrl Pts',(-6.76700000000019,-0.186007249519898,
133.705929295621));
#216206=CARTESIAN_POINT('Ctrl Pts',(-6.75932637294559,-0.372014355742914,
133.714678807432));
#216207=CARTESIAN_POINT('Ctrl Pts',(-6.74400518264238,-0.55738953748047,
133.723428319244));
#216208=CARTESIAN_POINT('Ctrl Pts',(-6.72868405705164,-0.742763936244698,
133.732177794099));
#216209=CARTESIAN_POINT('Ctrl Pts',(-6.70571545645824,-0.927506130235109,
133.740927268955));
#216210=CARTESIAN_POINT('Ctrl Pts',(-6.67517739404921,-1.11098863989439,
133.749676743811));
#216211=CARTESIAN_POINT('Ctrl Pts',(-6.6446394580881,-1.29447038981393,
133.758426182438));
#216212=CARTESIAN_POINT('Ctrl Pts',(-6.60653217008474,-1.47669218313153,
133.767175621065));
#216213=CARTESIAN_POINT('Ctrl Pts',(-6.56098496092805,-1.65703510598779,
133.775925059692));
#216214=CARTESIAN_POINT('Ctrl Pts',(-6.51543793658437,-1.83737729708204,
133.784674462817));
#216215=CARTESIAN_POINT('Ctrl Pts',(-6.46245112167572,-2.01584035510443,
133.793423865942));
#216216=CARTESIAN_POINT('Ctrl Pts',(-6.40220448374415,-2.19181813760319,
133.802173269067));
#216217=CARTESIAN_POINT('Ctrl Pts',(-6.34195808526676,-2.36779522066682,
133.810922637417));
#216218=CARTESIAN_POINT('Ctrl Pts',(-6.27445201433287,-2.54128677683714,
133.819672005767));
#216219=CARTESIAN_POINT('Ctrl Pts',(-6.19991555072094,-2.71170355384371,
133.828421374117));
#216220=CARTESIAN_POINT('Ctrl Pts',(-6.12537937716898,-2.88211966767039,
133.837170708419));
#216221=CARTESIAN_POINT('Ctrl Pts',(-6.0438129805274,-3.0494607637135,133.845920042721));
#216222=CARTESIAN_POINT('Ctrl Pts',(-5.95549339336065,-3.21315848374114,
133.854669377023));
#216223=CARTESIAN_POINT('Ctrl Pts',(-5.86717414255658,-3.3768555803306,
133.863418678003));
#216224=CARTESIAN_POINT('Ctrl Pts',(-5.77210188876863,-3.53690907646324,
133.872167978983));
#216225=CARTESIAN_POINT('Ctrl Pts',(-5.67059953347276,-3.69277536968857,
133.880917279963));
#216226=CARTESIAN_POINT('Ctrl Pts',(-5.56909755631678,-3.84864108224498,
133.889666548349));
#216227=CARTESIAN_POINT('Ctrl Pts',(-5.46116568197157,-4.00031938297098,
133.898415816734));
#216228=CARTESIAN_POINT('Ctrl Pts',(-5.34717048533923,-4.14729511859441,
133.907165085119));
#216229=CARTESIAN_POINT('Ctrl Pts',(-5.23317570392182,-4.29427031887494,
133.915914321636));
#216230=CARTESIAN_POINT('Ctrl Pts',(-5.11311782003887,-4.43654276189117,
133.924663558153));
#216231=CARTESIAN_POINT('Ctrl Pts',(-4.98740458985153,-4.57362924351416,
133.93341279467));
#216232=CARTESIAN_POINT('Ctrl Pts',(-4.86169180712161,-4.71071523719835,
133.942162000046));
#216233=CARTESIAN_POINT('Ctrl Pts',(-4.73032391204608,-4.84261509522811,
133.950911205421));
#216234=CARTESIAN_POINT('Ctrl Pts',(-4.59374707014054,-4.9688808453791,
133.959660410797));
#216235=CARTESIAN_POINT('Ctrl Pts',(-4.45717070301936,-5.09514615659033,
133.968409585757));
#216236=CARTESIAN_POINT('Ctrl Pts',(-4.31538563571569,-5.21577720459089,
133.977158760717));
#216237=CARTESIAN_POINT('Ctrl Pts',(-4.16887341030076,-5.33036429232443,
133.985907935678));
#216238=CARTESIAN_POINT('Ctrl Pts',(-4.02236168204279,-5.44495099123193,
133.99465708095));
#216239=CARTESIAN_POINT('Ctrl Pts',(-3.87112305348743,-5.55349359438199,
134.003406226222));
#216240=CARTESIAN_POINT('Ctrl Pts',(-3.71567117018342,-5.65562346298512,
134.012155371494));
#216241=CARTESIAN_POINT('Ctrl Pts',(-3.56021980146412,-5.75775299351277,
134.020904487804));
#216242=CARTESIAN_POINT('Ctrl Pts',(-3.40055544538953,-5.85346967463522,
134.029653604114));
#216243=CARTESIAN_POINT('Ctrl Pts',(-3.23722035987468,-5.94244842986566,
134.038402720424));
#216244=CARTESIAN_POINT('Ctrl Pts',(-3.07388580147812,-6.03142689794207,
134.047151808499));
#216245=CARTESIAN_POINT('Ctrl Pts',(-2.90688078897226,-6.11366734656473,
134.055900896574));
#216246=CARTESIAN_POINT('Ctrl Pts',(-2.73677250722034,-6.1888904695206,
134.064649984649));
#216247=CARTESIAN_POINT('Ctrl Pts',(-2.56666476032147,-6.26411335596055,
134.073399045215));
#216248=CARTESIAN_POINT('Ctrl Pts',(-2.3934540257583,-6.33231884500305,
134.082148105781));
#216249=CARTESIAN_POINT('Ctrl Pts',(-2.21772856066254,-6.39327529762497,
134.090897166347));
#216250=CARTESIAN_POINT('Ctrl Pts',(-2.04200363349168,-6.45423156364905,
134.099646200131));
#216251=CARTESIAN_POINT('Ctrl Pts',(-1.86376426189924,-6.50793874375474,
134.108395233914));
#216252=CARTESIAN_POINT('Ctrl Pts',(-1.6836157775379,-6.55421443909379,
134.117144267698));
#216253=CARTESIAN_POINT('Ctrl Pts',(-1.5034678296848,-6.60048999661712,
134.125893275426));
#216254=CARTESIAN_POINT('Ctrl Pts',(-1.32141105795712,-6.63933404237567,
134.134642283154));
#216255=CARTESIAN_POINT('Ctrl Pts',(-1.13806375487792,-6.67061465607429,
134.143391290882));
#216256=CARTESIAN_POINT('Ctrl Pts',(-0.954716982610654,-6.70189517921188,
134.15214027328));
#216257=CARTESIAN_POINT('Ctrl Pts',(-0.770079968909707,-6.72561226592142,
134.160889255678));
#216258=CARTESIAN_POINT('Ctrl Pts',(-0.584779765565736,-6.74168536983037,
134.169638238077));
#216259=CARTESIAN_POINT('Ctrl Pts',(-0.391489830658705,-6.7584515101381,
134.178764457087));
#216260=CARTESIAN_POINT('Ctrl Pts',(-0.197478578245647,-6.76689983031604,
134.187890676096));
#216261=CARTESIAN_POINT('Ctrl Pts',(-0.00346287645855221,-6.76699911397117,
134.197016895106));
#216262=CARTESIAN_POINT('Ctrl Pts',(0.184489834647668,-6.76709529501208,
134.205857919772));
#216263=CARTESIAN_POINT('Ctrl Pts',(0.372446404243251,-6.75935639738202,
134.214698944438));
#216264=CARTESIAN_POINT('Ctrl Pts',(0.559755019482324,-6.74380925873236,
134.223539969104));
#216265=CARTESIAN_POINT('Ctrl Pts',(0.745134705515861,-6.72842222659871,
134.232289947714));
#216266=CARTESIAN_POINT('Ctrl Pts',(0.929879431222757,-6.70538706057604,
134.241039926323));
#216267=CARTESIAN_POINT('Ctrl Pts',(1.11336163626255,-6.67478200894222,
134.249789904933));
#216268=CARTESIAN_POINT('Ctrl Pts',(1.29684196300168,-6.64417727061121,
134.25853979397));
#216269=CARTESIAN_POINT('Ctrl Pts',(1.47905951216979,-6.6060028489071,134.267289683006));
#216270=CARTESIAN_POINT('Ctrl Pts',(1.65939532066573,-6.5603884160736,134.276039572043));
#216271=CARTESIAN_POINT('Ctrl Pts',(1.83972934300294,-6.514774435034,134.284789374415));
#216272=CARTESIAN_POINT('Ctrl Pts',(2.01818138405761,-6.46172066062299,
134.293539176787));
#216273=CARTESIAN_POINT('Ctrl Pts',(2.194145283537,-6.4014073042365,134.302288979159));
#216274=CARTESIAN_POINT('Ctrl Pts',(2.37010749863504,-6.34109452518828,
134.311038697775));
#216275=CARTESIAN_POINT('Ctrl Pts',(2.54358134865968,-6.27352239616703,
134.319788416392));
#216276=CARTESIAN_POINT('Ctrl Pts',(2.71397759435069,-6.19892043967032,
134.328538135008));
#216277=CARTESIAN_POINT('Ctrl Pts',(2.88437226557649,-6.12431917249739,
134.337287772777));
#216278=CARTESIAN_POINT('Ctrl Pts',(3.05168912680493,-6.04268832279033,
134.346037410546));
#216279=CARTESIAN_POINT('Ctrl Pts',(3.21535986273404,-5.95430516123577,
134.354787048314));
#216280=CARTESIAN_POINT('Ctrl Pts',(3.37902914072414,-5.86592278697687,
134.363536608143));
#216281=CARTESIAN_POINT('Ctrl Pts',(3.53905210621167,-5.7707883574219,134.372286167972));
#216282=CARTESIAN_POINT('Ctrl Pts',(3.69488522831315,-5.66922500431878,
134.381035727801));
#216283=CARTESIAN_POINT('Ctrl Pts',(3.85071701406569,-5.5676625221735,134.389785212599));
#216284=CARTESIAN_POINT('Ctrl Pts',(4.00235878822045,-5.45967138329633,
134.398534697396));
#216285=CARTESIAN_POINT('Ctrl Pts',(4.14929549610978,-5.34561838199877,
134.407284182193));
#216286=CARTESIAN_POINT('Ctrl Pts',(4.29623099275755,-5.23156632087291,
134.416033594865));
#216287=CARTESIAN_POINT('Ctrl Pts',(4.43846127435706,-5.11145267305244,
134.424783007538));
#216288=CARTESIAN_POINT('Ctrl Pts',(4.57550326054133,-4.98568540050169,
134.433532420211));
#216289=CARTESIAN_POINT('Ctrl Pts',(4.71254416257476,-4.85991912290656,
134.442281763666));
#216290=CARTESIAN_POINT('Ctrl Pts',(4.84439664018462,-4.72849950385725,
134.451031107121));
#216291=CARTESIAN_POINT('Ctrl Pts',(4.97061286794451,-4.59187289861386,
134.459780450576));
#216292=CARTESIAN_POINT('Ctrl Pts',(5.09682813912402,-4.45524732885008,
134.468529727721));
#216293=CARTESIAN_POINT('Ctrl Pts',(5.21740705147567,-4.31341506236116,
134.477279004866));
#216294=CARTESIAN_POINT('Ctrl Pts',(5.33194007545436,-4.16685781276057,
134.486028282011));
#216295=CARTESIAN_POINT('Ctrl Pts',(5.44647226944229,-4.02030162522188,
134.494777495752));
#216296=CARTESIAN_POINT('Ctrl Pts',(5.55495848627862,-3.86902074888294,
134.503526709493));
#216297=CARTESIAN_POINT('Ctrl Pts',(5.65703027291542,-3.71352898081037,
134.512275923234));
#216298=CARTESIAN_POINT('Ctrl Pts',(5.75910135376767,-3.55803828789961,
134.521025076478));
#216299=CARTESIAN_POINT('Ctrl Pts',(5.85475793592538,-3.39833700107082,
134.529774229722));
#216300=CARTESIAN_POINT('Ctrl Pts',(5.94367514427199,-3.2349675082392,134.538523382966));
#216301=CARTESIAN_POINT('Ctrl Pts',(6.03259176732455,-3.07159909078089,
134.547272478619));
#216302=CARTESIAN_POINT('Ctrl Pts',(6.11476896835753,-2.90456276731794,
134.556021574272));
#216303=CARTESIAN_POINT('Ctrl Pts',(6.18992765547729,-2.73442583003406,
134.564770669925));
#216304=CARTESIAN_POINT('Ctrl Pts',(6.26508587282905,-2.56428995616535,
134.573519710893));
#216305=CARTESIAN_POINT('Ctrl Pts',(6.33322554827019,-2.39105376935576,
134.582268751861));
#216306=CARTESIAN_POINT('Ctrl Pts',(6.39411526732898,-2.21530561054463,
134.591017792829));
#216307=CARTESIAN_POINT('Ctrl Pts',(6.45500462602718,-2.03955849185506,
134.599766782018));
#216308=CARTESIAN_POINT('Ctrl Pts',(6.50864402040616,-1.86129970164976,
134.608515771207));
#216309=CARTESIAN_POINT('Ctrl Pts',(6.55485128368484,-1.68113463136514,
134.617264760396));
#216310=CARTESIAN_POINT('Ctrl Pts',(6.6019980955422,-1.49730620117337,134.626191645867));
#216311=CARTESIAN_POINT('Ctrl Pts',(6.64140720707778,-1.31149343246178,
134.635118531339));
#216312=CARTESIAN_POINT('Ctrl Pts',(6.67293928722801,-1.12435326698016,
134.64404541681));
#216313=CARTESIAN_POINT('Ctrl Pts',(6.70384625876187,-0.940923067011545,
134.652795330988));
#216314=CARTESIAN_POINT('Ctrl Pts',(6.7271855457974,-0.756217899526663,
134.661545245165));
#216315=CARTESIAN_POINT('Ctrl Pts',(6.74287786815285,-0.570865181259529,
134.670295159342));
#216316=CARTESIAN_POINT('Ctrl Pts',(6.75856988190817,-0.38551610807906,
134.679044901447));
#216317=CARTESIAN_POINT('Ctrl Pts',(6.76661520773387,-0.199519795231536,
134.687794643551));
#216318=CARTESIAN_POINT('Ctrl Pts',(6.76698651789578,-0.0135080204609056,
134.696544385656));
#216319=CARTESIAN_POINT('Ctrl Pts',(6.76735782124916,0.172500343507633,
134.705293967321));
#216320=CARTESIAN_POINT('Ctrl Pts',(6.76005538995212,0.35852388220553,134.714043548986));
#216321=CARTESIAN_POINT('Ctrl Pts',(6.74510402742405,0.543930748558928,
134.722793130651));
#216322=CARTESIAN_POINT('Ctrl Pts',(6.73015291918089,0.729334461609797,
134.731542563507));
#216323=CARTESIAN_POINT('Ctrl Pts',(6.70755316306669,0.914121237629259,
134.740291996364));
#216324=CARTESIAN_POINT('Ctrl Pts',(6.67738151874663,1.09766345165582,134.749041429221));
#216325=CARTESIAN_POINT('Ctrl Pts',(6.64721034747673,1.28120278799127,134.757790724898));
#216326=CARTESIAN_POINT('Ctrl Pts',(6.6094675720526,1.46349731859795,134.766540020576));
#216327=CARTESIAN_POINT('Ctrl Pts',(6.56428138111656,1.64392790277631,134.775289316253));
#216328=CARTESIAN_POINT('Ctrl Pts',(6.51909583860002,1.82435589778513,134.784038486379));
#216329=CARTESIAN_POINT('Ctrl Pts',(6.46646716393047,2.0029197219171,134.792787656505));
#216330=CARTESIAN_POINT('Ctrl Pts',(6.40657409873076,2.17901292274098,134.80153682663));
#216331=CARTESIAN_POINT('Ctrl Pts',(6.34668181342285,2.35510383058415,134.810285882829));
#216332=CARTESIAN_POINT('Ctrl Pts',(6.27952541914275,2.52872390822022,134.819034939028));
#216333=CARTESIAN_POINT('Ctrl Pts',(6.20533299175757,2.69928350889732,134.827783995228));
#216334=CARTESIAN_POINT('Ctrl Pts',(6.12831602991791,2.8763363796511,134.836866131386));
#216335=CARTESIAN_POINT('Ctrl Pts',(6.04371690605511,3.05009086600988,134.845948267544));
#216336=CARTESIAN_POINT('Ctrl Pts',(5.95184520316867,3.21991112882299,134.855030403702));
#216337=CARTESIAN_POINT('Ctrl Pts',(5.86333549509521,3.38351691182591,134.863780184046));
#216338=CARTESIAN_POINT('Ctrl Pts',(5.76807618099625,3.54347103711587,134.872529964389));
#216339=CARTESIAN_POINT('Ctrl Pts',(5.66639083309281,3.69923018027288,134.881279744733));
#216340=CARTESIAN_POINT('Ctrl Pts',(5.56470914082474,3.85498372381656,134.890029210518));
#216341=CARTESIAN_POINT('Ctrl Pts',(5.45660203372347,4.00654234701616,134.898778676303));
#216342=CARTESIAN_POINT('Ctrl Pts',(5.34243669839503,4.153391279863,134.907528142088));
#216343=CARTESIAN_POINT('Ctrl Pts',(5.22827486050883,4.30023571400926,134.916277339834));
#216344=CARTESIAN_POINT('Ctrl Pts',(5.10805534167406,4.44237052028131,134.92502653758));
#216345=CARTESIAN_POINT('Ctrl Pts',(4.98218644340249,4.57931296628397,134.933775735326));
#216346=CARTESIAN_POINT('Ctrl Pts',(4.85632073219899,4.71625194483038,134.942524711537));
#216347=CARTESIAN_POINT('Ctrl Pts',(4.72480612170647,4.84799861524188,134.951273687749));
#216348=CARTESIAN_POINT('Ctrl Pts',(4.58808925235655,4.97410554898168,134.960022663961));
#216349=CARTESIAN_POINT('Ctrl Pts',(4.45136349474403,5.10022068120896,134.968772208962));
#216350=CARTESIAN_POINT('Ctrl Pts',(4.30943501210447,5.22069514871531,134.977521753964));
#216351=CARTESIAN_POINT('Ctrl Pts',(4.1627858743216,5.33511975165962,134.986271298966));
#216352=CARTESIAN_POINT('Ctrl Pts',(4.01614535740829,5.44953762807562,134.995020329619));
#216353=CARTESIAN_POINT('Ctrl Pts',(3.86478496658306,5.55790617532518,135.003769360273));
#216354=CARTESIAN_POINT('Ctrl Pts',(3.7092187474758,5.65985735539104,135.012518390927));
#216355=CARTESIAN_POINT('Ctrl Pts',(3.55365041606297,5.76180991976802,135.021267540376));
#216356=CARTESIAN_POINT('Ctrl Pts',(3.3938763817493,5.85734478552577,135.030016689826));
#216357=CARTESIAN_POINT('Ctrl Pts',(3.23043927904957,5.94613749121005,135.038765839276));
#216358=CARTESIAN_POINT('Ctrl Pts',(3.18691767070709,5.96978206944,135.041095647192));
#216359=CARTESIAN_POINT('Ctrl Pts',(3.14313645919769,5.99294880633354,135.043425455108));
#216360=CARTESIAN_POINT('Ctrl Pts',(3.09910619832134,6.0156321173694,135.045755263024));
#216361=CARTESIAN_POINT('Ctrl Pts',(3.09910619832141,6.01563211736936,133.045915245968));
#216362=CARTESIAN_POINT('Ctrl Pts',(2.93176423559343,6.10184259430862,133.05474838379));
#216363=CARTESIAN_POINT('Ctrl Pts',(2.76066887234771,6.18114604978671,133.063581521611));
#216364=CARTESIAN_POINT('Ctrl Pts',(2.58638754591484,6.25323024222974,133.072414659433));
#216365=CARTESIAN_POINT('Ctrl Pts',(2.4244223041923,6.32022040056955,133.080623578493));
#216366=CARTESIAN_POINT('Ctrl Pts',(2.25986139745912,6.38091035543149,133.088832497554));
#216367=CARTESIAN_POINT('Ctrl Pts',(2.0932365976775,6.4351106863941,133.097041416615));
#216368=CARTESIAN_POINT('Ctrl Pts',(1.92657218276064,6.48932390351437,133.10525228735));
#216369=CARTESIAN_POINT('Ctrl Pts',(1.75784323582365,6.53704431267304,133.113463158085));
#216370=CARTESIAN_POINT('Ctrl Pts',(1.58759649279234,6.57813243831967,133.121674028821));
#216371=CARTESIAN_POINT('Ctrl Pts',(1.41727892642892,6.61923765679237,133.129888315312));
#216372=CARTESIAN_POINT('Ctrl Pts',(1.24544265192892,6.65370501165978,133.138102601803));
#216373=CARTESIAN_POINT('Ctrl Pts',(1.07264447500648,6.6814461630876,133.146316888293));
#216374=CARTESIAN_POINT('Ctrl Pts',(0.899651799273974,6.70921853950309,
133.154540420651));
#216375=CARTESIAN_POINT('Ctrl Pts',(0.725695410321514,6.7302495344213,133.162763953009));
#216376=CARTESIAN_POINT('Ctrl Pts',(0.551338092464835,6.74450259899107,
133.170987485366));
#216377=CARTESIAN_POINT('Ctrl Pts',(0.376869017819126,6.75876479926417,
133.179216288713));
#216378=CARTESIAN_POINT('Ctrl Pts',(0.20199885682681,6.76624039371214,133.187445092061));
#216379=CARTESIAN_POINT('Ctrl Pts',(0.0272902215745766,6.76694497124119,
133.195673895408));
#216380=CARTESIAN_POINT('Ctrl Pts',(-0.147658886335797,6.76765051856564,
133.203914025054));
#216381=CARTESIAN_POINT('Ctrl Pts',(-0.322445669605848,6.7615664459333,
133.2121541547));
#216382=CARTESIAN_POINT('Ctrl Pts',(-0.496511789836325,6.74876025967389,
133.220394284346));
#216383=CARTESIAN_POINT('Ctrl Pts',(-0.573789318755462,6.74307488892112,
133.224052531316));
#216384=CARTESIAN_POINT('Ctrl Pts',(-0.650924926912838,6.73606529465226,
133.227710778287));
#216385=CARTESIAN_POINT('Ctrl Pts',(-0.727870451698626,6.72774060183239,
133.231369025257));
#216386=CARTESIAN_POINT('Ctrl Pts',(-0.905561349639612,6.70851632405453,
133.239817043396));
#216387=CARTESIAN_POINT('Ctrl Pts',(-1.08264444933174,6.68223138116163,
133.248265061535));
#216388=CARTESIAN_POINT('Ctrl Pts',(-1.2585358525355,6.64893799849891,133.256713079674));
#216389=CARTESIAN_POINT('Ctrl Pts',(-1.43426618613749,6.61567510369285,
133.265153361682));
#216390=CARTESIAN_POINT('Ctrl Pts',(-1.60880667236696,6.57541662354257,
133.27359364369));
#216391=CARTESIAN_POINT('Ctrl Pts',(-1.78157976401296,6.52826642719639,
133.282033925697));
#216392=CARTESIAN_POINT('Ctrl Pts',(-1.95422123926741,6.48115214928314,
133.290467778004));
#216393=CARTESIAN_POINT('Ctrl Pts',(-2.12509768333322,6.42715670861028,
133.29890163031));
#216394=CARTESIAN_POINT('Ctrl Pts',(-2.29364256579097,6.36643485636913,
133.307335482616));
#216395=CARTESIAN_POINT('Ctrl Pts',(-2.46208496408001,6.30574992621342,
133.315764206695));
#216396=CARTESIAN_POINT('Ctrl Pts',(-2.62819831430491,6.23834685164277,
133.324192930775));
#216397=CARTESIAN_POINT('Ctrl Pts',(-2.79143167869532,6.16443007772627,
133.332621654855));
#216398=CARTESIAN_POINT('Ctrl Pts',(-2.95459085539805,6.0905468981338,133.341046548176));
#216399=CARTESIAN_POINT('Ctrl Pts',(-3.11487235295816,6.01015605960155,
133.349471441497));
#216400=CARTESIAN_POINT('Ctrl Pts',(-3.27174527324697,5.92351009680798,
133.357896334819));
#216401=CARTESIAN_POINT('Ctrl Pts',(-3.42858346226766,5.83688331721162,
133.36631936289));
#216402=CARTESIAN_POINT('Ctrl Pts',(-3.58201428570271,5.74400433329873,
133.374742390961));
#216403=CARTESIAN_POINT('Ctrl Pts',(-3.7315310453231,5.64517183598426,133.383165419033));
#216404=CARTESIAN_POINT('Ctrl Pts',(-3.88103088779537,5.54635052112185,
133.391587494076));
#216405=CARTESIAN_POINT('Ctrl Pts',(-4.02661727117806,5.44157721958877,
133.40000956912));
#216406=CARTESIAN_POINT('Ctrl Pts',(-4.16781185472731,5.33119436370449,
133.408431644163));
#216407=CARTESIAN_POINT('Ctrl Pts',(-4.30901017261878,5.22080858839265,
133.416853941956));
#216408=CARTESIAN_POINT('Ctrl Pts',(-4.44581619661231,5.10481316862147,
133.425276239748));
#216409=CARTESIAN_POINT('Ctrl Pts',(-4.57778381064575,4.98359151445919,
133.43369853754));
#216410=CARTESIAN_POINT('Ctrl Pts',(-4.70977333790016,4.86234973144247,
133.442122233855));
#216411=CARTESIAN_POINT('Ctrl Pts',(-4.8369226082705,4.73588020987226,133.45054593017));
#216412=CARTESIAN_POINT('Ctrl Pts',(-4.95882132357918,4.60460422629529,
133.458969626484));
#216413=CARTESIAN_POINT('Ctrl Pts',(-5.08080253038164,4.47323940542455,
133.467399023296));
#216414=CARTESIAN_POINT('Ctrl Pts',(-5.19752585490095,4.33706186760948,
133.475828420108));
#216415=CARTESIAN_POINT('Ctrl Pts',(-5.30861969906324,4.19652783747681,
133.48425781692));
#216416=CARTESIAN_POINT('Ctrl Pts',(-5.41975318212811,4.05594366401915,
133.492690221388));
#216417=CARTESIAN_POINT('Ctrl Pts',(-5.52525297777009,3.91100016420562,
133.501122625856));
#216418=CARTESIAN_POINT('Ctrl Pts',(-5.62478969626702,3.76218418910722,
133.509555030324));
#216419=CARTESIAN_POINT('Ctrl Pts',(-5.72441851057413,3.61323052283314,
133.517995236828));
#216420=CARTESIAN_POINT('Ctrl Pts',(-5.81807304384533,3.46039750321733,
133.526435443332));
#216421=CARTESIAN_POINT('Ctrl Pts',(-5.90546832877107,3.30419927030467,
133.534875649837));
#216422=CARTESIAN_POINT('Ctrl Pts',(-5.95517786491757,3.21535532738957,
133.539676352193));
#216423=CARTESIAN_POINT('Ctrl Pts',(-6.00286323972515,3.12542311443387,
133.54447705455));
#216424=CARTESIAN_POINT('Ctrl Pts',(-6.04847883432461,3.03450041864014,
133.549277756907));
#216425=CARTESIAN_POINT('Ctrl Pts',(-6.12630417289266,2.87937606597523,
133.557468295462));
#216426=CARTESIAN_POINT('Ctrl Pts',(-6.19825425152646,2.72106392792542,
133.565658834017));
#216427=CARTESIAN_POINT('Ctrl Pts',(-6.26405876161416,2.56005016182201,
133.573849372572));
#216428=CARTESIAN_POINT('Ctrl Pts',(-6.32980308573432,2.39918366175382,
133.582032419916));
#216429=CARTESIAN_POINT('Ctrl Pts',(-6.38941289688081,2.23562078529211,
133.590215467259));
#216430=CARTESIAN_POINT('Ctrl Pts',(-6.44266407163697,2.06987165303508,
133.598398514603));
#216431=CARTESIAN_POINT('Ctrl Pts',(-6.49618067748921,1.90329634231249,
133.606622350441));
#216432=CARTESIAN_POINT('Ctrl Pts',(-6.54327490417465,1.73451324334587,
133.614846186279));
#216433=CARTESIAN_POINT('Ctrl Pts',(-6.58376808304185,1.56406100543408,
133.623070022117));
#216434=CARTESIAN_POINT('Ctrl Pts',(-6.62400730407458,1.39467777920355,
133.63124228118));
#216435=CARTESIAN_POINT('Ctrl Pts',(-6.65772795357341,1.22364664624818,
133.639414540244));
#216436=CARTESIAN_POINT('Ctrl Pts',(-6.68480458637177,1.05151159861551,
133.647586799308));
#216437=CARTESIAN_POINT('Ctrl Pts',(-6.71213754830078,0.87774698251167,
133.655836423533));
#216438=CARTESIAN_POINT('Ctrl Pts',(-6.7326999430227,0.702857800600873,
133.664086047758));
#216439=CARTESIAN_POINT('Ctrl Pts',(-6.74641559389651,0.52741410147062,
133.672335671983));
#216440=CARTESIAN_POINT('Ctrl Pts',(-6.76013124477032,0.351970402340238,
133.680585296208));
#216441=CARTESIAN_POINT('Ctrl Pts',(-6.76700011584166,0.175972563260165,
133.688834920433));
#216442=CARTESIAN_POINT('Ctrl Pts',(-6.76699999999853,-4.45461812127951E-6,
133.697084544658));
#216443=CARTESIAN_POINT('',(-6.76699895518313,0.00376039232056921,133.302820216217));
#216444=CARTESIAN_POINT('Ctrl Pts',(3.09910619832128,6.01563211736943,132.651465380124));
#216445=CARTESIAN_POINT('Ctrl Pts',(2.9422829664035,6.09642360205379,132.659773088112));
#216446=CARTESIAN_POINT('Ctrl Pts',(2.78218146133116,6.17113911591494,132.6680807961));
#216447=CARTESIAN_POINT('Ctrl Pts',(2.61930798531622,6.23951237502248,132.676388504088));
#216448=CARTESIAN_POINT('Ctrl Pts',(2.4565348215353,6.30784352368617,132.684691095437));
#216449=CARTESIAN_POINT('Ctrl Pts',(2.29099340863279,6.36984006698678,132.692993686786));
#216450=CARTESIAN_POINT('Ctrl Pts',(2.12321260920816,6.42528265651399,132.701296278135));
#216451=CARTESIAN_POINT('Ctrl Pts',(1.95550439899007,6.48070125918695,132.709595277426));
#216452=CARTESIAN_POINT('Ctrl Pts',(1.78555906292883,6.52957145023807,132.717894276716));
#216453=CARTESIAN_POINT('Ctrl Pts',(1.6139235213629,6.57172274728565,132.726193276006));
#216454=CARTESIAN_POINT('Ctrl Pts',(1.44233079473145,6.61386352958199,132.73449020509));
#216455=CARTESIAN_POINT('Ctrl Pts',(1.26904904063257,6.6492886760543,132.742787134173));
#216456=CARTESIAN_POINT('Ctrl Pts',(1.09463857049795,6.67787806117918,132.751084063256));
#216457=CARTESIAN_POINT('Ctrl Pts',(0.920200817714469,6.70647191847913,
132.75938229021));
#216458=CARTESIAN_POINT('Ctrl Pts',(0.744634338483491,6.72822781539155,
132.767680517163));
#216459=CARTESIAN_POINT('Ctrl Pts',(0.568508428552313,6.74307698062724,
132.775978744117));
#216460=CARTESIAN_POINT('Ctrl Pts',(0.392357421718683,6.75792826178132,
132.784278153519));
#216461=CARTESIAN_POINT('Ctrl Pts',(0.21564717217046,6.76587082003446,132.792577562921));
#216462=CARTESIAN_POINT('Ctrl Pts',(0.0389507607491826,6.76688789904466,
132.800876972323));
#216463=CARTESIAN_POINT('Ctrl Pts',(-0.137800194472367,6.76790529201344,
132.809178943641));
#216464=CARTESIAN_POINT('Ctrl Pts',(-0.314536955050337,6.76199294298867,
132.817480914959));
#216465=CARTESIAN_POINT('Ctrl Pts',(-0.490687586842416,6.74918622443616,
132.825782886277));
#216466=CARTESIAN_POINT('Ctrl Pts',(-0.666921872883159,6.73637342395021,
132.834088800216));
#216467=CARTESIAN_POINT('Ctrl Pts',(-0.842569128580576,6.71665975372667,
132.842394714155));
#216468=CARTESIAN_POINT('Ctrl Pts',(-1.01706348563162,6.69013235042438,
132.850700628094));
#216469=CARTESIAN_POINT('Ctrl Pts',(-1.19176641434726,6.6635732391359,132.859016470023));
#216470=CARTESIAN_POINT('Ctrl Pts',(-1.36531334720724,6.63018417696049,
132.867332311952));
#216471=CARTESIAN_POINT('Ctrl Pts',(-1.53714842304668,6.59010346849919,
132.875648153881));
#216472=CARTESIAN_POINT('Ctrl Pts',(-1.7090986528531,6.54999590025647,132.883969568609));
#216473=CARTESIAN_POINT('Ctrl Pts',(-1.87933440315601,6.50318783535335,
132.892290983336));
#216474=CARTESIAN_POINT('Ctrl Pts',(-2.04731575106779,6.44986722463569,
132.900612398063));
#216475=CARTESIAN_POINT('Ctrl Pts',(-2.21553622152306,6.39647071168119,
132.908945658379));
#216476=CARTESIAN_POINT('Ctrl Pts',(-2.38149555124351,6.3365432487563,132.917278918694));
#216477=CARTESIAN_POINT('Ctrl Pts',(-2.54467344291763,6.27032104990723,
132.92561217901));
#216478=CARTESIAN_POINT('Ctrl Pts',(-2.62638946484153,6.23715837941627,
132.92978529876));
#216479=CARTESIAN_POINT('Ctrl Pts',(-2.70740833253123,6.20241784780833,
132.933958418511));
#216480=CARTESIAN_POINT('Ctrl Pts',(-2.78766713701807,6.16613338593883,
132.938131538262));
#216481=CARTESIAN_POINT('Ctrl Pts',(-2.94286905967262,6.09596764797852,
132.946201384467));
#216482=CARTESIAN_POINT('Ctrl Pts',(-3.09570670996627,6.01980878026116,
132.954271230671));
#216483=CARTESIAN_POINT('Ctrl Pts',(-3.24567133678046,5.93783685980019,
132.962341076876));
#216484=CARTESIAN_POINT('Ctrl Pts',(-3.39544728901764,5.85596807044251,
132.970400770188));
#216485=CARTESIAN_POINT('Ctrl Pts',(-3.54235708668447,5.76830095697706,
132.978460463499));
#216486=CARTESIAN_POINT('Ctrl Pts',(-3.68591042633544,5.67506416959595,
132.986520156811));
#216487=CARTESIAN_POINT('Ctrl Pts',(-3.82931466303837,5.58192422343008,
132.994571478851));
#216488=CARTESIAN_POINT('Ctrl Pts',(-3.96936906909925,5.4832263170296,133.002622800891));
#216489=CARTESIAN_POINT('Ctrl Pts',(-4.10560660096983,5.37924561979401,
133.010674122931));
#216490=CARTESIAN_POINT('Ctrl Pts',(-4.24173248280347,5.27535013731919,
133.018718846712));
#216491=CARTESIAN_POINT('Ctrl Pts',(-4.37404742114997,5.16618070606974,
133.026763570494));
#216492=CARTESIAN_POINT('Ctrl Pts',(-4.50211221102706,5.05205647626004,
133.034808294276));
#216493=CARTESIAN_POINT('Ctrl Pts',(-4.63010008206802,4.93800079224611,
133.0428481862));
#216494=CARTESIAN_POINT('Ctrl Pts',(-4.75384260851946,4.81899648151168,
133.050888078124));
#216495=CARTESIAN_POINT('Ctrl Pts',(-4.87293271969347,4.69540367906113,
133.058927970049));
#216496=CARTESIAN_POINT('Ctrl Pts',(-4.99458716234243,4.56914959004131,
133.067140982543));
#216497=CARTESIAN_POINT('Ctrl Pts',(-5.11138624186292,4.43810740421035,
133.075353995037));
#216498=CARTESIAN_POINT('Ctrl Pts',(-5.22293449680575,4.3027019699343,133.083567007532));
#216499=CARTESIAN_POINT('Ctrl Pts',(-5.3320933470238,4.17019696995537,133.091604094272));
#216500=CARTESIAN_POINT('Ctrl Pts',(-5.43622380606403,4.03351406109677,
133.099641181012));
#216501=CARTESIAN_POINT('Ctrl Pts',(-5.53499531585419,3.89308564681953,
133.107678267752));
#216502=CARTESIAN_POINT('Ctrl Pts',(-5.63377627852553,3.75264379290652,
133.115716123678));
#216503=CARTESIAN_POINT('Ctrl Pts',(-5.72719705566639,3.60845602535668,
133.123753979604));
#216504=CARTESIAN_POINT('Ctrl Pts',(-5.81497003918787,3.46098431711954,
133.13179183553));
#216505=CARTESIAN_POINT('Ctrl Pts',(-5.90276881373872,3.313469276105,133.139832053283));
#216506=CARTESIAN_POINT('Ctrl Pts',(-5.98491630043968,3.16266869459248,
133.147872271035));
#216507=CARTESIAN_POINT('Ctrl Pts',(-6.06117060009071,3.00906961644226,
133.155912488788));
#216508=CARTESIAN_POINT('Ctrl Pts',(-6.1403058306289,2.84966747760555,133.164256470548));
#216509=CARTESIAN_POINT('Ctrl Pts',(-6.21309368252874,2.68725165285073,
133.172600452309));
#216510=CARTESIAN_POINT('Ctrl Pts',(-6.2793187702202,2.52238870556469,133.180944434069));
#216511=CARTESIAN_POINT('Ctrl Pts',(-6.34324401739305,2.36325105815218,
133.188998649096));
#216512=CARTESIAN_POINT('Ctrl Pts',(-6.4010546159101,2.201833773138,133.197052864122));
#216513=CARTESIAN_POINT('Ctrl Pts',(-6.452608071421,2.03866085375488,133.205107079149));
#216514=CARTESIAN_POINT('Ctrl Pts',(-6.50420010615967,1.87536582645173,
133.213167321423));
#216515=CARTESIAN_POINT('Ctrl Pts',(-6.54952557630775,1.71031290662024,
133.221227563696));
#216516=CARTESIAN_POINT('Ctrl Pts',(-6.58849315994731,1.54403590674815,
133.22928780597));
#216517=CARTESIAN_POINT('Ctrl Pts',(-6.62751522292725,1.37752644028642,
133.237359317012));
#216518=CARTESIAN_POINT('Ctrl Pts',(-6.66016159409174,1.20978984260038,
133.245430828054));
#216519=CARTESIAN_POINT('Ctrl Pts',(-6.6863927094321,1.0413652266392,133.253502339096));
#216520=CARTESIAN_POINT('Ctrl Pts',(-6.68914199869593,1.02371260369812,
133.254348316034));
#216521=CARTESIAN_POINT('Ctrl Pts',(-6.69182086238034,1.00605242249317,
133.255194292973));
#216522=CARTESIAN_POINT('Ctrl Pts',(-6.69442928804769,0.988385303072306,
133.256040269912));
#216523=CARTESIAN_POINT('Ctrl Pts',(-6.74250861780533,0.662739350751086,
133.271633585338));
#216524=CARTESIAN_POINT('Ctrl Pts',(-6.76681562166512,0.333677441931173,
133.287226900764));
#216525=CARTESIAN_POINT('Ctrl Pts',(-6.76699895518282,0.00376039288159187,
133.30282021619));
#216526=CARTESIAN_POINT('Ctrl Pts',(-6.76699895518313,0.00376039232075853,
133.302820216217));
#216527=CARTESIAN_POINT('Ctrl Pts',(-6.76709367130421,-0.166685624388963,
133.31087623669));
#216528=CARTESIAN_POINT('Ctrl Pts',(-6.76074448764723,-0.337402547659519,
133.318932257163));
#216529=CARTESIAN_POINT('Ctrl Pts',(-6.74791638606985,-0.50785179591102,
133.326988277637));
#216530=CARTESIAN_POINT('Ctrl Pts',(-6.73510162204312,-0.6781238257745,
133.335035922157));
#216531=CARTESIAN_POINT('Ctrl Pts',(-6.71582137301528,-0.8481283643743,
133.343083566677));
#216532=CARTESIAN_POINT('Ctrl Pts',(-6.69009260406261,-1.01732489847972,
133.351131211197));
#216533=CARTESIAN_POINT('Ctrl Pts',(-6.66438491642342,-1.18638279846776,
133.35917226174));
#216534=CARTESIAN_POINT('Ctrl Pts',(-6.63223928122514,-1.35463364351775,
133.367213312282));
#216535=CARTESIAN_POINT('Ctrl Pts',(-6.59372461489781,-1.52154024031268,
133.375254362825));
#216536=CARTESIAN_POINT('Ctrl Pts',(-6.55407050051306,-1.69338473260621,
133.383533306106));
#216537=CARTESIAN_POINT('Ctrl Pts',(-6.50766470528992,-1.86380380860883,
133.391812249386));
#216538=CARTESIAN_POINT('Ctrl Pts',(-6.45463959831345,-2.03221963770749,
133.400091192667));
#216539=CARTESIAN_POINT('Ctrl Pts',(-6.40318384022079,-2.19565097533634,
133.408125109561));
#216540=CARTESIAN_POINT('Ctrl Pts',(-6.34549514090866,-2.35719557670721,
133.416159026454));
#216541=CARTESIAN_POINT('Ctrl Pts',(-6.28174561715427,-2.51633880893712,
133.424192943347));
#216542=CARTESIAN_POINT('Ctrl Pts',(-6.21800263890322,-2.67546570108328,
133.432226035356));
#216543=CARTESIAN_POINT('Ctrl Pts',(-6.14820021359972,-2.83219136695208,
133.440259127364));
#216544=CARTESIAN_POINT('Ctrl Pts',(-6.07255909613137,-2.98601993027377,
133.448292219372));
#216545=CARTESIAN_POINT('Ctrl Pts',(-5.99691068375431,-3.13986332898346,
133.4563260861));
#216546=CARTESIAN_POINT('Ctrl Pts',(-5.91542262429346,-3.29080873312182,
133.464359952829));
#216547=CARTESIAN_POINT('Ctrl Pts',(-5.82836215843078,-3.43838385730449,
133.472393819557));
#216548=CARTESIAN_POINT('Ctrl Pts',(-5.741275957439,-3.58600260478777,133.480430061101));
#216549=CARTESIAN_POINT('Ctrl Pts',(-5.64861426273166,-3.73024876760867,
133.488466302645));
#216550=CARTESIAN_POINT('Ctrl Pts',(-5.55068815627169,-3.87067823408575,
133.49650254419));
#216551=CARTESIAN_POINT('Ctrl Pts',(-5.45266859848319,-4.01124171304105,
133.504546454756));
#216552=CARTESIAN_POINT('Ctrl Pts',(-5.34937481495106,-4.14798091798835,
133.512590365322));
#216553=CARTESIAN_POINT('Ctrl Pts',(-5.24115911562539,-4.28048363210244,
133.520634275888));
#216554=CARTESIAN_POINT('Ctrl Pts',(-5.13288128729715,-4.4130624189261,
133.528682804639));
#216555=CARTESIAN_POINT('Ctrl Pts',(-5.01967616295562,-4.5413995915947,
133.53673133339));
#216556=CARTESIAN_POINT('Ctrl Pts',(-4.90193317647914,-4.6651195197265,
133.544779862142));
#216557=CARTESIAN_POINT('Ctrl Pts',(-4.78404786584367,-4.78898899676348,
133.552838119711));
#216558=CARTESIAN_POINT('Ctrl Pts',(-4.66161401386229,-4.90822983192578,
133.56089637728));
#216559=CARTESIAN_POINT('Ctrl Pts',(-4.53505477822122,-5.02250606356358,
133.56895463485));
#216560=CARTESIAN_POINT('Ctrl Pts',(-4.50890838002663,-5.04611486493982,
133.570619423753));
#216561=CARTESIAN_POINT('Ctrl Pts',(-4.48258600667227,-5.06951191744136,
133.572284212657));
#216562=CARTESIAN_POINT('Ctrl Pts',(-4.45609154241186,-5.09269448972207,
133.573949001561));
#216563=CARTESIAN_POINT('Ctrl Pts',(-4.3138795473748,-5.21712953478379,
133.582884941876));
#216564=CARTESIAN_POINT('Ctrl Pts',(-4.16636189976131,-5.33568374524025,
133.591820882191));
#216565=CARTESIAN_POINT('Ctrl Pts',(-4.01402762616934,-5.4479235692463,
133.600756822507));
#216566=CARTESIAN_POINT('Ctrl Pts',(-3.86192235100635,-5.55999466731326,
133.609679329756));
#216567=CARTESIAN_POINT('Ctrl Pts',(-3.7050151048525,-5.66577016628138,
133.618601837006));
#216568=CARTESIAN_POINT('Ctrl Pts',(-3.5438277933209,-5.76485676936438,
133.627524344256));
#216569=CARTESIAN_POINT('Ctrl Pts',(-3.38303543922898,-5.8637005804392,
133.636424988676));
#216570=CARTESIAN_POINT('Ctrl Pts',(-3.21798417041297,-5.95588807180147,
133.645325633097));
#216571=CARTESIAN_POINT('Ctrl Pts',(-3.04922410440849,-6.04106955439964,
133.654226277518));
#216572=CARTESIAN_POINT('Ctrl Pts',(-2.88072483506674,-6.12611940013066,
133.663113167154));
#216573=CARTESIAN_POINT('Ctrl Pts',(-2.70852843065635,-6.20418471810273,
133.67200005679));
#216574=CARTESIAN_POINT('Ctrl Pts',(-2.53321138391679,-6.27496048468788,
133.680886946426));
#216575=CARTESIAN_POINT('Ctrl Pts',(-2.35834496471864,-6.34555433222819,
133.689750993576));
#216576=CARTESIAN_POINT('Ctrl Pts',(-2.18037414758836,-6.4088959199107,
133.698615040725));
#216577=CARTESIAN_POINT('Ctrl Pts',(-1.99989655680842,-6.46472758606779,
133.707479087875));
#216578=CARTESIAN_POINT('Ctrl Pts',(-1.82734510126143,-6.51810726173493,
133.715953847712));
#216579=CARTESIAN_POINT('Ctrl Pts',(-1.6525025570652,-6.5646223548235,133.724428607549));
#216580=CARTESIAN_POINT('Ctrl Pts',(-1.47591029112629,-6.60408796220549,
133.732903367385));
#216581=CARTESIAN_POINT('Ctrl Pts',(-1.30485746535172,-6.64231559141512,
133.741112286446));
#216582=CARTESIAN_POINT('Ctrl Pts',(-1.13232764321828,-6.67389126433614,
133.749321205506));
#216583=CARTESIAN_POINT('Ctrl Pts',(-0.958877199700067,-6.69871954300935,
133.757530124567));
#216584=CARTESIAN_POINT('Ctrl Pts',(-0.785385518245537,-6.72355372461917,
133.765740995302));
#216585=CARTESIAN_POINT('Ctrl Pts',(-0.610973131834763,-6.74163726551333,
133.773951866038));
#216586=CARTESIAN_POINT('Ctrl Pts',(-0.436202594282811,-6.75292649869232,
133.782162736773));
#216587=CARTESIAN_POINT('Ctrl Pts',(-0.261359351486093,-6.76422042823761,
133.790377023264));
#216588=CARTESIAN_POINT('Ctrl Pts',(-0.0861580157723752,-6.76871439623117,
133.798591309754));
#216589=CARTESIAN_POINT('Ctrl Pts',(0.0888377060821969,-6.76641684069036,
133.806805596245));
#216590=CARTESIAN_POINT('Ctrl Pts',(0.264030400271302,-6.76411669905845,
133.815029128603));
#216591=CARTESIAN_POINT('Ctrl Pts',(0.43901666216046,-6.75500977012508,
133.823252660961));
#216592=CARTESIAN_POINT('Ctrl Pts',(0.613235774965258,-6.73915654101482,
133.831476193318));
#216593=CARTESIAN_POINT('Ctrl Pts',(0.787566555974475,-6.72329315055314,
133.839704996665));
#216594=CARTESIAN_POINT('Ctrl Pts',(0.961128855517095,-6.7006748859166,
133.847933800013));
#216595=CARTESIAN_POINT('Ctrl Pts',(1.13337106600222,-6.67141357035741,
133.85616260336));
#216596=CARTESIAN_POINT('Ctrl Pts',(1.30585035430655,-6.64211197890498,
133.864402733006));
#216597=CARTESIAN_POINT('Ctrl Pts',(1.47700557681594,-6.60614914596039,
133.872642862652));
#216598=CARTESIAN_POINT('Ctrl Pts',(1.6462982380752,-6.5636873105984,133.880882992298));
#216599=CARTESIAN_POINT('Ctrl Pts',(1.7214565659004,-6.54483616537771,133.884541239269));
#216600=CARTESIAN_POINT('Ctrl Pts',(1.79624802391357,-6.52470474051377,
133.88819948624));
#216601=CARTESIAN_POINT('Ctrl Pts',(1.87062672729915,-6.50331028377965,
133.89185773321));
#216602=CARTESIAN_POINT('Ctrl Pts',(2.04239004463055,-6.45390389870048,
133.900305751349));
#216603=CARTESIAN_POINT('Ctrl Pts',(2.21234394623014,-6.39764562152587,
133.908753769488));
#216604=CARTESIAN_POINT('Ctrl Pts',(2.37992213524361,-6.33468701911764,
133.917201787627));
#216605=CARTESIAN_POINT('Ctrl Pts',(2.54734686734116,-6.27178606999361,
133.925642069635));
#216606=CARTESIAN_POINT('Ctrl Pts',(2.71239991259888,-6.20219714265404,
133.934082351643));
#216607=CARTESIAN_POINT('Ctrl Pts',(2.87453008596152,-6.12612159403501,
133.942522633651));
#216608=CARTESIAN_POINT('Ctrl Pts',(3.03653675057568,-6.05010399882222,
133.950956485957));
#216609=CARTESIAN_POINT('Ctrl Pts',(3.19562468117761,-5.96760977425559,
133.959390338263));
#216610=CARTESIAN_POINT('Ctrl Pts',(3.35126227056852,-5.87888851687663,
133.967824190569));
#216611=CARTESIAN_POINT('Ctrl Pts',(3.50680522410583,-5.79022120669615,
133.976252914649));
#216612=CARTESIAN_POINT('Ctrl Pts',(3.65890173023552,-5.69533457745867,
133.984681638728));
#216613=CARTESIAN_POINT('Ctrl Pts',(3.80704406398739,-5.59452451016692,
133.993110362808));
#216614=CARTESIAN_POINT('Ctrl Pts',(3.95511906875269,-5.4937602598911,134.001535256129));
#216615=CARTESIAN_POINT('Ctrl Pts',(4.09924320935774,-5.38707812701131,
134.009960149451));
#216616=CARTESIAN_POINT('Ctrl Pts',(4.23893674913172,-5.27481793400119,
134.018385042772));
#216617=CARTESIAN_POINT('Ctrl Pts',(4.37859936110751,-5.16258259511533,
134.026808070844));
#216618=CARTESIAN_POINT('Ctrl Pts',(4.51383306664667,-5.04477186504803,
134.035231098915));
#216619=CARTESIAN_POINT('Ctrl Pts',(4.64418988453205,-4.92176688968608,
134.043654126986));
#216620=CARTESIAN_POINT('Ctrl Pts',(4.77453195313025,-4.79877583178342,
134.05207620203));
#216621=CARTESIAN_POINT('Ctrl Pts',(4.89999799161701,-4.67059192902208,
134.060498277073));
#216622=CARTESIAN_POINT('Ctrl Pts',(5.02017545619937,-4.53763455877327,
134.068920352117));
#216623=CARTESIAN_POINT('Ctrl Pts',(5.14035609925841,-4.40467367204237,
134.077342649909));
#216624=CARTESIAN_POINT('Ctrl Pts',(5.25524766621523,-4.26693931376235,
134.085764947701));
#216625=CARTESIAN_POINT('Ctrl Pts',(5.36447638677372,-4.12488570699204,
134.094187245494));
#216626=CARTESIAN_POINT('Ctrl Pts',(5.47372324476179,-3.98280851221963,
134.102610941809));
#216627=CARTESIAN_POINT('Ctrl Pts',(5.57730517887522,-3.83641090374199,
134.111034638123));
#216628=CARTESIAN_POINT('Ctrl Pts',(5.6748901988497,-3.68617826902059,134.119458334438));
#216629=CARTESIAN_POINT('Ctrl Pts',(5.77254125671401,-3.53584396863183,
134.12788773125));
#216630=CARTESIAN_POINT('Ctrl Pts',(5.86418710925702,-3.38166973601207,
134.136317128062));
#216631=CARTESIAN_POINT('Ctrl Pts',(5.94953988539577,-3.22416875366116,
134.144746524874));
#216632=CARTESIAN_POINT('Ctrl Pts',(6.03492311588055,-3.06661157408229,
134.153178929342));
#216633=CARTESIAN_POINT('Ctrl Pts',(6.11400863927412,-2.9057255740443,134.16161133381));
#216634=CARTESIAN_POINT('Ctrl Pts',(6.18655541898425,-2.74204687192554,
134.170043738277));
#216635=CARTESIAN_POINT('Ctrl Pts',(6.25916932220979,-2.57821672697324,
134.178483944782));
#216636=CARTESIAN_POINT('Ctrl Pts',(6.32523226446926,-2.41158902475306,
134.186924151286));
#216637=CARTESIAN_POINT('Ctrl Pts',(6.38455165269328,-2.24271915185374,
134.19536435779));
#216638=CARTESIAN_POINT('Ctrl Pts',(6.41829190853671,-2.14666771089225,
134.200165060147));
#216639=CARTESIAN_POINT('Ctrl Pts',(6.44985138425098,-2.04989117763733,
134.204965762503));
#216640=CARTESIAN_POINT('Ctrl Pts',(6.47920190307621,-1.95249371296647,
134.20976646486));
#216641=CARTESIAN_POINT('Ctrl Pts',(6.52896652431803,-1.78735360187953,
134.217906189267));
#216642=CARTESIAN_POINT('Ctrl Pts',(6.57247710501642,-1.62009842067415,
134.226045913675));
#216643=CARTESIAN_POINT('Ctrl Pts',(6.6095514310584,-1.45124735320821,134.234185638083));
#216644=CARTESIAN_POINT('Ctrl Pts',(6.64659333170785,-1.28254396373748,
134.242318243447));
#216645=CARTESIAN_POINT('Ctrl Pts',(6.6772101045517,-1.11224782151601,134.25045084881));
#216646=CARTESIAN_POINT('Ctrl Pts',(6.70126910669482,-0.940893915198506,
134.258583454174));
#216647=CARTESIAN_POINT('Ctrl Pts',(6.72531166052328,-0.769657157670257,
134.266710499555));
#216648=CARTESIAN_POINT('Ctrl Pts',(6.74280531900876,-0.597364436978038,
134.274837544935));
#216649=CARTESIAN_POINT('Ctrl Pts',(6.75366837228143,-0.42456155884102,
134.282964590315));
#216650=CARTESIAN_POINT('Ctrl Pts',(6.76452623258499,-0.251841287314305,
134.291087750647));
#216651=CARTESIAN_POINT('Ctrl Pts',(6.76875977664518,-0.078611708688447,
134.299210910978));
#216652=CARTESIAN_POINT('Ctrl Pts',(6.76633907293236,0.0945756316865812,
134.307334071309));
#216653=CARTESIAN_POINT('Ctrl Pts',(6.76391904948411,0.267714303068407,
134.315454948875));
#216654=CARTESIAN_POINT('Ctrl Pts',(6.75484850878356,0.440810393999221,
134.323575826441));
#216655=CARTESIAN_POINT('Ctrl Pts',(6.73914962523719,0.613311771177977,
134.331696704007));
#216656=CARTESIAN_POINT('Ctrl Pts',(6.72344989360934,0.785822467186494,
134.339818020277));
#216657=CARTESIAN_POINT('Ctrl Pts',(6.7011211330024,0.957738020181045,134.347939336548));
#216658=CARTESIAN_POINT('Ctrl Pts',(6.67223746082235,1.12851064080003,134.356060652818));
#216659=CARTESIAN_POINT('Ctrl Pts',(6.65722871038969,1.21724879111642,134.360280712107));
#216660=CARTESIAN_POINT('Ctrl Pts',(6.64045090130213,1.30567844182336,134.364500771396));
#216661=CARTESIAN_POINT('Ctrl Pts',(6.62191990559178,1.3937237042999,134.368720830685));
#216662=CARTESIAN_POINT('Ctrl Pts',(6.58246773098609,1.58117057022766,134.377705265117));
#216663=CARTESIAN_POINT('Ctrl Pts',(6.53508587936941,1.76678162433251,134.386689699548));
#216664=CARTESIAN_POINT('Ctrl Pts',(6.4799776082147,1.94991774109476,134.39567413398));
#216665=CARTESIAN_POINT('Ctrl Pts',(6.42477422283632,2.13336994198028,134.404674075113));
#216666=CARTESIAN_POINT('Ctrl Pts',(6.3618178328622,2.31433843884362,134.413674016247));
#216667=CARTESIAN_POINT('Ctrl Pts',(6.29136071496936,2.49220170815692,134.42267395738));
#216668=CARTESIAN_POINT('Ctrl Pts',(6.22073756119818,2.67048412155427,134.431695107344));
#216669=CARTESIAN_POINT('Ctrl Pts',(6.14257840135267,2.84564644294452,134.440716257309));
#216670=CARTESIAN_POINT('Ctrl Pts',(6.05718377222747,3.01708696418651,134.449737407274));
#216671=CARTESIAN_POINT('Ctrl Pts',(5.9717022519301,3.18870193044924,134.458767736484));
#216672=CARTESIAN_POINT('Ctrl Pts',(5.87897066616139,3.35658731998988,134.467798065694));
#216673=CARTESIAN_POINT('Ctrl Pts',(5.77933508011031,3.52016690397008,134.476828394905));
#216674=CARTESIAN_POINT('Ctrl Pts',(5.6795582386698,3.68397839804141,134.485871526596));
#216675=CARTESIAN_POINT('Ctrl Pts',(5.57285795009395,3.84347167641061,134.494914658287));
#216676=CARTESIAN_POINT('Ctrl Pts',(5.45962437772617,3.99809837974732,134.503957789978));
#216677=CARTESIAN_POINT('Ctrl Pts',(5.36063187673157,4.1332781127874,134.511863592155));
#216678=CARTESIAN_POINT('Ctrl Pts',(5.25664680599319,4.26473878927251,134.519769394332));
#216679=CARTESIAN_POINT('Ctrl Pts',(5.14795514502898,4.39213465467188,134.527675196509));
#216680=CARTESIAN_POINT('Ctrl Pts',(5.02897023659875,4.53159508102349,134.536329688857));
#216681=CARTESIAN_POINT('Ctrl Pts',(4.90423896087291,4.66630674144622,134.544984181205));
#216682=CARTESIAN_POINT('Ctrl Pts',(4.7741586796986,4.79580002721742,134.553638673553));
#216683=CARTESIAN_POINT('Ctrl Pts',(4.64424148225365,4.92513096518477,134.562282315625));
#216684=CARTESIAN_POINT('Ctrl Pts',(4.508988877527,5.04925637129254,134.570925957698));
#216685=CARTESIAN_POINT('Ctrl Pts',(4.36883632402047,5.16774207695385,134.57956959977));
#216686=CARTESIAN_POINT('Ctrl Pts',(4.22879280700214,5.28613560259473,134.588206517224));
#216687=CARTESIAN_POINT('Ctrl Pts',(4.08385717428778,5.39889798157439,134.596843434679));
#216688=CARTESIAN_POINT('Ctrl Pts',(3.93450038150467,5.50563309238271,134.605480352133));
#216689=CARTESIAN_POINT('Ctrl Pts',(3.78528659056306,5.61226600953039,134.614109000161));
#216690=CARTESIAN_POINT('Ctrl Pts',(3.6316603333524,5.71288299806633,134.622737648188));
#216691=CARTESIAN_POINT('Ctrl Pts',(3.47412434380166,5.80712915680414,134.631366296216));
#216692=CARTESIAN_POINT('Ctrl Pts',(3.35140667946281,5.88054519656873,134.638087855748));
#216693=CARTESIAN_POINT('Ctrl Pts',(3.22631723720771,5.95009610861492,134.644809415281));
#216694=CARTESIAN_POINT('Ctrl Pts',(3.09910619832129,6.01563211736943,134.651530974814));
#216695=CARTESIAN_POINT('Origin',(0.,0.,4.30282021618968));
#216696=CARTESIAN_POINT('',(3.0991061983214,6.01563211736937,137.045755263024));
#216697=CARTESIAN_POINT('',(3.09910619832118,6.01563211736948,136.651395695404));
#216698=CARTESIAN_POINT('',(3.09910619832133,6.0156321173694,4.30282021618968));
#216699=CARTESIAN_POINT('',(-6.767,-5.66010073996262E-10,135.697179783837));
#216700=CARTESIAN_POINT('Ctrl Pts',(-6.767,-5.65818573007036E-10,135.697179783837));
#216701=CARTESIAN_POINT('Ctrl Pts',(-6.76699999998445,-0.186007250092783,
135.705929295648));
#216702=CARTESIAN_POINT('Ctrl Pts',(-6.75932637291409,-0.372014356315282,
135.714678807459));
#216703=CARTESIAN_POINT('Ctrl Pts',(-6.74400518259517,-0.557389538051668,
135.72342831927));
#216704=CARTESIAN_POINT('Ctrl Pts',(-6.72868405698871,-0.742763936814854,
135.732177794126));
#216705=CARTESIAN_POINT('Ctrl Pts',(-6.70571545637962,-0.927506130803568,
135.740927268982));
#216706=CARTESIAN_POINT('Ctrl Pts',(-6.67517739395499,-1.11098864046051,
135.749676743838));
#216707=CARTESIAN_POINT('Ctrl Pts',(-6.64463945797831,-1.29447039037746,
135.758426182465));
#216708=CARTESIAN_POINT('Ctrl Pts',(-6.6065321699595,-1.47669218369183,
135.767175621092));
#216709=CARTESIAN_POINT('Ctrl Pts',(-6.56098496078752,-1.65703510654422,
135.775925059719));
#216710=CARTESIAN_POINT('Ctrl Pts',(-6.51543793642857,-1.83737729763449,
135.784674462844));
#216711=CARTESIAN_POINT('Ctrl Pts',(-6.46245112150483,-2.01584035565226,
135.793423865969));
#216712=CARTESIAN_POINT('Ctrl Pts',(-6.40220448355839,-2.1918181381458,
135.802173269094));
#216713=CARTESIAN_POINT('Ctrl Pts',(-6.34195808506609,-2.36779522120432,
135.810922637444));
#216714=CARTESIAN_POINT('Ctrl Pts',(-6.27445201411749,-2.54128677736892,
135.819672005794));
#216715=CARTESIAN_POINT('Ctrl Pts',(-6.19991555049112,-2.71170355436917,
135.828421374144));
#216716=CARTESIAN_POINT('Ctrl Pts',(-6.12537937692472,-2.88211966818953,
135.837170708446));
#216717=CARTESIAN_POINT('Ctrl Pts',(-6.04381298026895,-3.04946076422573,
135.845920042748));
#216718=CARTESIAN_POINT('Ctrl Pts',(-5.95549339308833,-3.21315848424588,
135.85466937705));
#216719=CARTESIAN_POINT('Ctrl Pts',(-5.86717414227038,-3.37685558082785,
135.86341867803));
#216720=CARTESIAN_POINT('Ctrl Pts',(-5.77210188846886,-3.53690907695245,
135.87216797901));
#216721=CARTESIAN_POINT('Ctrl Pts',(-5.67059953315979,-3.69277537016916,
135.88091727999));
#216722=CARTESIAN_POINT('Ctrl Pts',(-5.56909755599059,-3.84864108271698,
135.889666548376));
#216723=CARTESIAN_POINT('Ctrl Pts',(-5.46116568163254,-4.00031938343382,
135.898415816761));
#216724=CARTESIAN_POINT('Ctrl Pts',(-5.34717048498774,-4.14729511904759,
135.907165085146));
#216725=CARTESIAN_POINT('Ctrl Pts',(-5.23317570355772,-4.29427031931866,
135.915914321663));
#216726=CARTESIAN_POINT('Ctrl Pts',(-5.11311781966253,-4.43654276232491,
135.92466355818));
#216727=CARTESIAN_POINT('Ctrl Pts',(-4.98740458946339,-4.57362924393742,
135.933412794697));
#216728=CARTESIAN_POINT('Ctrl Pts',(-4.86169180672201,-4.71071523761075,
135.942162000073));
#216729=CARTESIAN_POINT('Ctrl Pts',(-4.73032391163547,-4.84261509562919,
135.950911205448));
#216730=CARTESIAN_POINT('Ctrl Pts',(-4.59374706971941,-4.96888084576842,
135.959660410824));
#216731=CARTESIAN_POINT('Ctrl Pts',(-4.45717070258735,-5.09514615696826,
135.968409585784));
#216732=CARTESIAN_POINT('Ctrl Pts',(-4.31538563527325,-5.21577720495696,
135.977158760744));
#216733=CARTESIAN_POINT('Ctrl Pts',(-4.1688734098484,-5.33036429267822,
135.985907935705));
#216734=CARTESIAN_POINT('Ctrl Pts',(-4.0223616815807,-5.44495099157329,
135.994657080977));
#216735=CARTESIAN_POINT('Ctrl Pts',(-3.87112305301613,-5.55349359471052,
136.003406226249));
#216736=CARTESIAN_POINT('Ctrl Pts',(-3.71567116970346,-5.65562346330045,
136.012155371521));
#216737=CARTESIAN_POINT('Ctrl Pts',(-3.56021980097516,-5.75775299381512,
136.020904487831));
#216738=CARTESIAN_POINT('Ctrl Pts',(-3.40055544489212,-5.8534696749242,
136.029653604141));
#216739=CARTESIAN_POINT('Ctrl Pts',(-3.23722035936936,-5.94244843014094,
136.038402720452));
#216740=CARTESIAN_POINT('Ctrl Pts',(-3.07388580096523,-6.03142689820346,
136.047151808526));
#216741=CARTESIAN_POINT('Ctrl Pts',(-2.90688078845238,-6.11366734681192,
136.055900896601));
#216742=CARTESIAN_POINT('Ctrl Pts',(-2.73677250669407,-6.18889046975332,
136.064649984676));
#216743=CARTESIAN_POINT('Ctrl Pts',(-2.56666475978868,-6.26411335617886,
136.073399045242));
#216744=CARTESIAN_POINT('Ctrl Pts',(-2.39345402521959,-6.33231884520667,
136.082148105808));
#216745=CARTESIAN_POINT('Ctrl Pts',(-2.21772856011852,-6.39327529781368,
136.090897166374));
#216746=CARTESIAN_POINT('Ctrl Pts',(-2.04200363294235,-6.45423156382285,
136.099646200158));
#216747=CARTESIAN_POINT('Ctrl Pts',(-1.86376426134522,-6.5079387439134,
136.108395233942));
#216748=CARTESIAN_POINT('Ctrl Pts',(-1.68361577697981,-6.55421443923714,
136.117144267725));
#216749=CARTESIAN_POINT('Ctrl Pts',(-1.5034678291224,-6.60048999674524,
136.125893275453));
#216750=CARTESIAN_POINT('Ctrl Pts',(-1.32141105739104,-6.63933404248835,
136.134642283181));
#216751=CARTESIAN_POINT('Ctrl Pts',(-1.13806375430879,-6.67061465617139,
136.143391290909));
#216752=CARTESIAN_POINT('Ctrl Pts',(-0.954716982039362,-6.70189517929325,
136.152140273307));
#216753=CARTESIAN_POINT('Ctrl Pts',(-0.770079968336905,-6.72561226598699,
136.160889255705));
#216754=CARTESIAN_POINT('Ctrl Pts',(-0.584779764992078,-6.74168536988013,
136.169638238104));
#216755=CARTESIAN_POINT('Ctrl Pts',(-0.391489830089624,-6.7584515101709,
136.178764457113));
#216756=CARTESIAN_POINT('Ctrl Pts',(-0.197478577681895,-6.76689983033232,
136.187890676123));
#216757=CARTESIAN_POINT('Ctrl Pts',(-0.00346287590081867,-6.76699911397146,
136.197016895133));
#216758=CARTESIAN_POINT('Ctrl Pts',(0.184489835199639,-6.76709529499687,
136.205857919798));
#216759=CARTESIAN_POINT('Ctrl Pts',(0.372446404788815,-6.7593563973518,
136.214698944464));
#216760=CARTESIAN_POINT('Ctrl Pts',(0.559755020020896,-6.74380925868766,
136.223539969129));
#216761=CARTESIAN_POINT('Ctrl Pts',(0.745134706053204,-6.72842222653921,
136.232289947739));
#216762=CARTESIAN_POINT('Ctrl Pts',(0.92987943175826,-6.70538706050178,
136.241039926349));
#216763=CARTESIAN_POINT('Ctrl Pts',(1.11336163679561,-6.67478200885331,
136.249789904959));
#216764=CARTESIAN_POINT('Ctrl Pts',(1.29684196353216,-6.64417727050766,
136.258539793995));
#216765=CARTESIAN_POINT('Ctrl Pts',(1.4790595126971,-6.60600284878903,136.267289683032));
#216766=CARTESIAN_POINT('Ctrl Pts',(1.65939532118928,-6.56038841594117,
136.276039572068));
#216767=CARTESIAN_POINT('Ctrl Pts',(1.83972934352284,-6.51477443488718,
136.28478937444));
#216768=CARTESIAN_POINT('Ctrl Pts',(2.01818138457328,-6.46172066046193,
136.293539176812));
#216769=CARTESIAN_POINT('Ctrl Pts',(2.19414528404785,-6.4014073040614,136.302288979185));
#216770=CARTESIAN_POINT('Ctrl Pts',(2.37010749914096,-6.34109452499917,
136.311038697801));
#216771=CARTESIAN_POINT('Ctrl Pts',(2.5435813491601,-6.27352239596414,136.319788416417));
#216772=CARTESIAN_POINT('Ctrl Pts',(2.71397759484504,-6.19892043945389,
136.328538135033));
#216773=CARTESIAN_POINT('Ctrl Pts',(2.88437226606477,-6.12431917226742,
136.337287772802));
#216774=CARTESIAN_POINT('Ctrl Pts',(3.05168912728658,-6.04268832254707,
136.346037410571));
#216775=CARTESIAN_POINT('Ctrl Pts',(3.21535986320854,-5.95430516097954,
136.35478704834));
#216776=CARTESIAN_POINT('Ctrl Pts',(3.3790291411916,-5.8659227867076,136.363536608169));
#216777=CARTESIAN_POINT('Ctrl Pts',(3.53905210667155,-5.77078835713988,
136.372286167998));
#216778=CARTESIAN_POINT('Ctrl Pts',(3.69488522876493,-5.66922500402434,
136.381035727827));
#216779=CARTESIAN_POINT('Ctrl Pts',(3.85071701450938,-5.56766252186664,
136.389785212624));
#216780=CARTESIAN_POINT('Ctrl Pts',(4.00235878865553,-5.45967138297739,
136.398534697421));
#216781=CARTESIAN_POINT('Ctrl Pts',(4.14929549653577,-5.34561838166811,
136.407284182218));
#216782=CARTESIAN_POINT('Ctrl Pts',(4.29623099317445,-5.23156632053054,
136.416033594891));
#216783=CARTESIAN_POINT('Ctrl Pts',(4.43846127476439,-5.11145267269874,
136.424783007563));
#216784=CARTESIAN_POINT('Ctrl Pts',(4.57550326093864,-4.98568540013707,
136.433532420236));
#216785=CARTESIAN_POINT('Ctrl Pts',(4.71254416296205,-4.85991912253102,
136.442281763691));
#216786=CARTESIAN_POINT('Ctrl Pts',(4.84439664056143,-4.72849950347121,
136.451031107146));
#216787=CARTESIAN_POINT('Ctrl Pts',(4.97061286831044,-4.59187289821775,
136.459780450602));
#216788=CARTESIAN_POINT('Ctrl Pts',(5.09682813947888,-4.45524732844411,
136.468529727747));
#216789=CARTESIAN_POINT('Ctrl Pts',(5.21740705181908,-4.31341506194578,
136.477279004891));
#216790=CARTESIAN_POINT('Ctrl Pts',(5.33194007578594,-4.16685781233627,
136.486028282036));
#216791=CARTESIAN_POINT('Ctrl Pts',(5.44647226976221,-4.02030162478847,
136.494777495777));
#216792=CARTESIAN_POINT('Ctrl Pts',(5.5549584865865,-3.86902074844091,136.503526709518));
#216793=CARTESIAN_POINT('Ctrl Pts',(5.65703027321092,-3.71352898036021,
136.512275923259));
#216794=CARTESIAN_POINT('Ctrl Pts',(5.75910135405073,-3.55803828744144,
136.521025076503));
#216795=CARTESIAN_POINT('Ctrl Pts',(5.85475793619567,-3.39833700060515,
136.529774229747));
#216796=CARTESIAN_POINT('Ctrl Pts',(5.94367514452923,-3.23496750776657,
136.538523382991));
#216797=CARTESIAN_POINT('Ctrl Pts',(6.0325917675688,-3.07159909030118,136.547272478644));
#216798=CARTESIAN_POINT('Ctrl Pts',(6.1147689685885,-2.90456276683171,136.556021574297));
#216799=CARTESIAN_POINT('Ctrl Pts',(6.18992765569473,-2.73442582954184,
136.56477066995));
#216800=CARTESIAN_POINT('Ctrl Pts',(6.26508587303301,-2.56428995566705,
136.573519710918));
#216801=CARTESIAN_POINT('Ctrl Pts',(6.33322554846041,-2.39105376885192,
136.582268751886));
#216802=CARTESIAN_POINT('Ctrl Pts',(6.39411526750526,-2.21530561003582,
136.591017792854));
#216803=CARTESIAN_POINT('Ctrl Pts',(6.45500462618948,-2.0395584913414,136.599766782043));
#216804=CARTESIAN_POINT('Ctrl Pts',(6.50864402055428,-1.86129970113184,
136.608515771232));
#216805=CARTESIAN_POINT('Ctrl Pts',(6.55485128381862,-1.68113463084354,
136.617264760421));
#216806=CARTESIAN_POINT('Ctrl Pts',(6.60199809565858,-1.49730620065882,
136.626191645892));
#216807=CARTESIAN_POINT('Ctrl Pts',(6.64140720717751,-1.31149343195513,
136.635118531363));
#216808=CARTESIAN_POINT('Ctrl Pts',(6.67293928731192,-1.12435326648217,
136.644045416834));
#216809=CARTESIAN_POINT('Ctrl Pts',(6.70384625883209,-0.940923066511241,
136.652795331011));
#216810=CARTESIAN_POINT('Ctrl Pts',(6.72718554585383,-0.756217899024617,
136.661545245189));
#216811=CARTESIAN_POINT('Ctrl Pts',(6.74287786819546,-0.570865180756313,
136.670295159366));
#216812=CARTESIAN_POINT('Ctrl Pts',(6.75856988193694,-0.385516107574673,
136.679044901471));
#216813=CARTESIAN_POINT('Ctrl Pts',(6.76661520774876,-0.199519794726551,
136.687794643575));
#216814=CARTESIAN_POINT('Ctrl Pts',(6.76698651789679,-0.0135080199558931,
136.69654438568));
#216815=CARTESIAN_POINT('Ctrl Pts',(6.76735782123629,0.172500344012673,
136.705293967345));
#216816=CARTESIAN_POINT('Ctrl Pts',(6.76005538992536,0.358523882710025,
136.71404354901));
#216817=CARTESIAN_POINT('Ctrl Pts',(6.74510402738346,0.543930749062307,
136.722793130675));
#216818=CARTESIAN_POINT('Ctrl Pts',(6.73015291912646,0.729334462112059,
136.731542563531));
#216819=CARTESIAN_POINT('Ctrl Pts',(6.70755316299847,0.914121238129835,
136.740291996388));
#216820=CARTESIAN_POINT('Ctrl Pts',(6.67738151866471,1.09766345215414,136.749041429245));
#216821=CARTESIAN_POINT('Ctrl Pts',(6.64721034738111,1.28120278848734,136.757790724922));
#216822=CARTESIAN_POINT('Ctrl Pts',(6.60946757194338,1.4634973190912,136.7665400206));
#216823=CARTESIAN_POINT('Ctrl Pts',(6.56428138099387,1.6439279032662,136.775289316277));
#216824=CARTESIAN_POINT('Ctrl Pts',(6.51909583846384,1.82435589827176,136.784038486403));
#216825=CARTESIAN_POINT('Ctrl Pts',(6.46646716378092,2.00291972239993,136.792787656528));
#216826=CARTESIAN_POINT('Ctrl Pts',(6.40657409856802,2.17901292321946,136.801536826654));
#216827=CARTESIAN_POINT('Ctrl Pts',(6.34668181324704,2.35510383105791,136.810285882853));
#216828=CARTESIAN_POINT('Ctrl Pts',(6.27952541895408,2.52872390868873,136.819034939052));
#216829=CARTESIAN_POINT('Ctrl Pts',(6.20533299155628,2.69928350936006,136.827783995251));
#216830=CARTESIAN_POINT('Ctrl Pts',(6.12831602971186,2.8763363800887,136.836866131408));
#216831=CARTESIAN_POINT('Ctrl Pts',(6.0437169058462,3.05009086642249,136.845948267566));
#216832=CARTESIAN_POINT('Ctrl Pts',(5.95184520295876,3.219911129211,136.855030403723));
#216833=CARTESIAN_POINT('Ctrl Pts',(5.86333549487463,3.38351691220815,136.863780184066));
#216834=CARTESIAN_POINT('Ctrl Pts',(5.76807618076524,3.54347103749191,136.87252996441));
#216835=CARTESIAN_POINT('Ctrl Pts',(5.66639083285165,3.69923018064229,136.881279744754));
#216836=CARTESIAN_POINT('Ctrl Pts',(5.56470914057342,3.85498372417933,136.890029210539));
#216837=CARTESIAN_POINT('Ctrl Pts',(5.45660203346228,4.00654234737189,136.898778676323));
#216838=CARTESIAN_POINT('Ctrl Pts',(5.34243669812427,4.15339128021128,136.907528142108));
#216839=CARTESIAN_POINT('Ctrl Pts',(5.22827486022857,4.30023571434999,136.916277339854));
#216840=CARTESIAN_POINT('Ctrl Pts',(5.10805534138462,4.44237052061411,136.9250265376));
#216841=CARTESIAN_POINT('Ctrl Pts',(4.98218644310422,4.57931296660848,136.933775735346));
#216842=CARTESIAN_POINT('Ctrl Pts',(4.85632073189171,4.71625194514679,136.942524711558));
#216843=CARTESIAN_POINT('Ctrl Pts',(4.72480612139051,4.84799861554981,136.95127368777));
#216844=CARTESIAN_POINT('Ctrl Pts',(4.58808925203228,4.97410554928079,136.960022663981));
#216845=CARTESIAN_POINT('Ctrl Pts',(4.45136349441154,5.10022068149915,136.968772208983));
#216846=CARTESIAN_POINT('Ctrl Pts',(4.30943501176412,5.22069514899625,136.977521753985));
#216847=CARTESIAN_POINT('Ctrl Pts',(4.16278587397379,5.335119751931,136.986271298986));
#216848=CARTESIAN_POINT('Ctrl Pts',(4.01614535705282,5.44953762833759,136.99502032964));
#216849=CARTESIAN_POINT('Ctrl Pts',(3.86478496622032,5.55790617557742,137.003769360294));
#216850=CARTESIAN_POINT('Ctrl Pts',(3.70921874710619,5.65985735563327,137.012518390948));
#216851=CARTESIAN_POINT('Ctrl Pts',(3.55365041568669,5.76180992000009,137.021267540397));
#216852=CARTESIAN_POINT('Ctrl Pts',(3.39387638136678,5.85734478574741,137.030016689847));
#216853=CARTESIAN_POINT('Ctrl Pts',(3.23043927866126,5.94613749142101,137.038765839296));
#216854=CARTESIAN_POINT('Ctrl Pts',(3.18691767044669,5.96978206957779,137.041095647206));
#216855=CARTESIAN_POINT('Ctrl Pts',(3.14313645906677,5.99294880640099,137.043425455115));
#216856=CARTESIAN_POINT('Ctrl Pts',(3.0991061983214,6.01563211736937,137.045755263024));
#216857=CARTESIAN_POINT('Ctrl Pts',(3.09910619832134,6.0156321173694,135.045755263024));
#216858=CARTESIAN_POINT('Ctrl Pts',(2.93375330764826,6.10081787314653,135.054504710927));
#216859=CARTESIAN_POINT('Ctrl Pts',(2.7648862784307,6.17918207037039,135.063254158829));
#216860=CARTESIAN_POINT('Ctrl Pts',(2.59307866646702,6.25045854553997,135.072003606731));
#216861=CARTESIAN_POINT('Ctrl Pts',(2.42127244185382,6.32173444515035,135.080752983982));
#216862=CARTESIAN_POINT('Ctrl Pts',(2.24652594672477,6.38592262741833,135.089502361232));
#216863=CARTESIAN_POINT('Ctrl Pts',(2.06943269687141,6.44280508110556,135.098251738482));
#216864=CARTESIAN_POINT('Ctrl Pts',(1.89234081822097,6.49968709436161,135.107001047988));
#216865=CARTESIAN_POINT('Ctrl Pts',(1.71290249405609,6.54926340459539,135.115750357493));
#216866=CARTESIAN_POINT('Ctrl Pts',(1.5317271662508,6.59136563150379,135.124499666998));
#216867=CARTESIAN_POINT('Ctrl Pts',(1.3505531810736,6.63346754640705,135.133248911666));
#216868=CARTESIAN_POINT('Ctrl Pts',(1.16764249714449,6.66809542395771,135.141998156333));
#216869=CARTESIAN_POINT('Ctrl Pts',(0.983616340614701,6.69513165624663,
135.150747401));
#216870=CARTESIAN_POINT('Ctrl Pts',(0.79959148671406,6.72216769715959,135.159496583736));
#216871=CARTESIAN_POINT('Ctrl Pts',(0.614451459526801,6.74161215869371,
135.168245766471));
#216872=CARTESIAN_POINT('Ctrl Pts',(0.428825047910242,6.75339900185712,
135.176994949207));
#216873=CARTESIAN_POINT('Ctrl Pts',(0.243199888596912,6.76518576550222,
135.185744072918));
#216874=CARTESIAN_POINT('Ctrl Pts',(0.057088637391689,6.76931499599835,
135.194493196628));
#216875=CARTESIAN_POINT('Ctrl Pts',(-0.128876626811471,6.76577266947846,
135.203242320339));
#216876=CARTESIAN_POINT('Ctrl Pts',(-0.314840698188552,6.76223036567991,
135.21199138793));
#216877=CARTESIAN_POINT('Ctrl Pts',(-0.500658497951714,6.7510166087922,
135.220740455522));
#216878=CARTESIAN_POINT('Ctrl Pts',(-0.685698951926748,6.73216948296213,
135.229489523113));
#216879=CARTESIAN_POINT('Ctrl Pts',(-0.870738280460292,6.71332247176287,
135.238238537492));
#216880=CARTESIAN_POINT('Ctrl Pts',(-1.05499998761286,6.68684221356181,
135.24698755187));
#216881=CARTESIAN_POINT('Ctrl Pts',(-1.23785829161446,6.65281863948517,
135.255736566249));
#216882=CARTESIAN_POINT('Ctrl Pts',(-1.43007412917413,6.61705395368859,
135.264933299948));
#216883=CARTESIAN_POINT('Ctrl Pts',(-1.62073882535785,6.57295372727791,
135.274130033647));
#216884=CARTESIAN_POINT('Ctrl Pts',(-1.80913696091492,6.52068343478286,
135.283326767346));
#216885=CARTESIAN_POINT('Ctrl Pts',(-1.9883835618609,6.47095219815205,135.29207676506));
#216886=CARTESIAN_POINT('Ctrl Pts',(-2.16557827572511,6.41382586850898,
135.300826762774));
#216887=CARTESIAN_POINT('Ctrl Pts',(-2.34011918621679,6.34949849943286,
135.309576760487));
#216888=CARTESIAN_POINT('Ctrl Pts',(-2.51465655691083,6.28517243495557,
135.318326580746));
#216889=CARTESIAN_POINT('Ctrl Pts',(-2.68653996295318,6.21364572242379,
135.327076401004));
#216890=CARTESIAN_POINT('Ctrl Pts',(-2.85518555379984,6.13516132252223,
135.335826221262));
#216891=CARTESIAN_POINT('Ctrl Pts',(-3.02382794858663,6.05667841000519,
135.3445758757));
#216892=CARTESIAN_POINT('Ctrl Pts',(-3.18923239109234,5.97123819492105,
135.353325530137));
#216893=CARTESIAN_POINT('Ctrl Pts',(-3.35083705967632,5.87913088810751,
135.362075184575));
#216894=CARTESIAN_POINT('Ctrl Pts',(-3.5124388804233,5.78702520443145,135.370824684824));
#216895=CARTESIAN_POINT('Ctrl Pts',(-3.67024081223617,5.6882528060583,135.379574185073));
#216896=CARTESIAN_POINT('Ctrl Pts',(-3.82370687544326,5.58314917682556,
135.388323685322));
#216897=CARTESIAN_POINT('Ctrl Pts',(-3.97717043817738,5.47804726008077,
135.397073043012));
#216898=CARTESIAN_POINT('Ctrl Pts',(-4.12629803722382,5.36661448084296,
135.405822400703));
#216899=CARTESIAN_POINT('Ctrl Pts',(-4.27058317206828,5.24922931204642,
135.414571758393));
#216900=CARTESIAN_POINT('Ctrl Pts',(-4.41486614774761,5.13184589986855,
135.423320985153));
#216901=CARTESIAN_POINT('Ctrl Pts',(-4.55430658194345,5.00851045723097,
135.432070211913));
#216902=CARTESIAN_POINT('Ctrl Pts',(-4.68843089001782,4.8796418710318,135.440819438673));
#216903=CARTESIAN_POINT('Ctrl Pts',(-4.82255336917773,4.75077504208025,
135.449568546129));
#216904=CARTESIAN_POINT('Ctrl Pts',(-4.95135966065071,4.61637541908161,
135.458317653585));
#216905=CARTESIAN_POINT('Ctrl Pts',(-5.07441230869181,4.47689945401916,
135.467066761041));
#216906=CARTESIAN_POINT('Ctrl Pts',(-5.1974634422637,4.33742520555572,135.475815760817));
#216907=CARTESIAN_POINT('Ctrl Pts',(-5.31476088454736,4.19287495491377,
135.484564760594));
#216908=CARTESIAN_POINT('Ctrl Pts',(-5.42590627628836,4.04373961586729,
135.49331376037));
#216909=CARTESIAN_POINT('Ctrl Pts',(-5.53706380672645,3.89458798906766,
135.502063715665));
#216910=CARTESIAN_POINT('Ctrl Pts',(-5.64206777071836,3.74085050155325,
135.51081367096));
#216911=CARTESIAN_POINT('Ctrl Pts',(-5.74056148163976,3.58304938223212,
135.519563626254));
#216912=CARTESIAN_POINT('Ctrl Pts',(-5.8390513895185,3.42525435593339,135.528313243695));
#216913=CARTESIAN_POINT('Ctrl Pts',(-5.93103139557618,3.26339625497246,
135.537062861137));
#216914=CARTESIAN_POINT('Ctrl Pts',(-6.0161890782081,3.09802485065074,135.545812478578));
#216915=CARTESIAN_POINT('Ctrl Pts',(-6.1013439254495,2.9326589524971,135.554561804693));
#216916=CARTESIAN_POINT('Ctrl Pts',(-6.17967677261801,2.76378023986105,
135.563311130809));
#216917=CARTESIAN_POINT('Ctrl Pts',(-6.25092157009195,2.59196229227185,
135.572060456925));
#216918=CARTESIAN_POINT('Ctrl Pts',(-6.32216437407728,2.42014915229157,
135.580809538228));
#216919=CARTESIAN_POINT('Ctrl Pts',(-6.386319415489,2.24539720662912,135.58955861953));
#216920=CARTESIAN_POINT('Ctrl Pts',(-6.44316881037519,2.06829994947743,
135.598307700833));
#216921=CARTESIAN_POINT('Ctrl Pts',(-6.50002334524557,1.89118668024501,
135.607057573175));
#216922=CARTESIAN_POINT('Ctrl Pts',(-6.54957082411085,1.71172794807747,
135.615807445517));
#216923=CARTESIAN_POINT('Ctrl Pts',(-6.59164294296075,1.53053334250378,
135.62455731786));
#216924=CARTESIAN_POINT('Ctrl Pts',(-6.63371214082129,1.34935131693624,
135.633306582715));
#216925=CARTESIAN_POINT('Ctrl Pts',(-6.66830695239688,1.16643393829774,
135.642055847569));
#216926=CARTESIAN_POINT('Ctrl Pts',(-6.69530988153989,0.982402458340958,
135.650805112424));
#216927=CARTESIAN_POINT('Ctrl Pts',(-6.72231419690481,0.798361530947166,
135.659554826431));
#216928=CARTESIAN_POINT('Ctrl Pts',(-6.74172580829275,0.613206671362721,
135.668304540438));
#216929=CARTESIAN_POINT('Ctrl Pts',(-6.75347878028177,0.427566795113783,
135.677054254445));
#216930=CARTESIAN_POINT('Ctrl Pts',(-6.76248992368203,0.285234494207359,
135.683762764234));
#216931=CARTESIAN_POINT('Ctrl Pts',(-6.76699999999985,0.142617266095927,
135.690471274022));
#216932=CARTESIAN_POINT('Ctrl Pts',(-6.767,6.94095400683209E-12,135.69717978381));
#216933=CARTESIAN_POINT('',(-6.767,6.93929614291322E-12,135.30282021619));
#216934=CARTESIAN_POINT('Ctrl Pts',(3.09910619832129,6.01563211736943,134.651530974814));
#216935=CARTESIAN_POINT('Ctrl Pts',(2.93600378292275,6.09965848345377,134.660148958007));
#216936=CARTESIAN_POINT('Ctrl Pts',(2.76941303260316,6.17708323365079,134.668766941199));
#216937=CARTESIAN_POINT('Ctrl Pts',(2.59988462643395,6.24763066523882,134.677384924392));
#216938=CARTESIAN_POINT('Ctrl Pts',(2.53926608414269,6.27285642274986,134.680466470373));
#216939=CARTESIAN_POINT('Ctrl Pts',(2.47827216835747,6.2972032914136,134.683548016353));
#216940=CARTESIAN_POINT('Ctrl Pts',(2.4169287797121,6.32066011376971,134.686629562334));
#216941=CARTESIAN_POINT('Ctrl Pts',(2.24921401483504,6.3847918080418,134.695054606516));
#216942=CARTESIAN_POINT('Ctrl Pts',(2.07895886568387,6.44223889516753,134.703479650697));
#216943=CARTESIAN_POINT('Ctrl Pts',(1.90672453923883,6.49281838121662,134.711904694879));
#216944=CARTESIAN_POINT('Ctrl Pts',(1.73445021098399,6.54340961446514,134.720331695797));
#216945=CARTESIAN_POINT('Ctrl Pts',(1.56019610708374,6.587129972977,134.728758696714));
#216946=CARTESIAN_POINT('Ctrl Pts',(1.38453719934345,6.62384674819958,134.737185697631));
#216947=CARTESIAN_POINT('Ctrl Pts',(1.20881367420903,6.66057702995233,134.745615798481));
#216948=CARTESIAN_POINT('Ctrl Pts',(1.03168463927251,6.6902985236657,134.754045899331));
#216949=CARTESIAN_POINT('Ctrl Pts',(0.853734211707432,6.71292982949772,
134.762476000182));
#216950=CARTESIAN_POINT('Ctrl Pts',(0.675619840749096,6.73558198525476,
134.770913867573));
#216951=CARTESIAN_POINT('Ctrl Pts',(0.496682894442441,6.75113086071185,
134.779351734965));
#216952=CARTESIAN_POINT('Ctrl Pts',(0.317512679657415,6.75954692995446,
134.787789602356));
#216953=CARTESIAN_POINT('Ctrl Pts',(0.138248403430535,6.76796741749622,
134.79623189949));
#216954=CARTESIAN_POINT('Ctrl Pts',(-0.0412490543095359,6.76924762290726,
134.804674196625));
#216955=CARTESIAN_POINT('Ctrl Pts',(-0.220390865830408,6.76341015067536,
134.813116493759));
#216956=CARTESIAN_POINT('Ctrl Pts',(-0.399721664706716,6.75756652014669,
134.821567697175));
#216957=CARTESIAN_POINT('Ctrl Pts',(-0.578695737101644,6.74459023095583,
134.830018900591));
#216958=CARTESIAN_POINT('Ctrl Pts',(-0.756728770012883,6.72455578968863,
134.838470104007));
#216959=CARTESIAN_POINT('Ctrl Pts',(-0.806682038090416,6.71893444066682,
134.840841378724));
#216960=CARTESIAN_POINT('Ctrl Pts',(-0.856561275549977,6.71275773118605,
134.843212653441));
#216961=CARTESIAN_POINT('Ctrl Pts',(-0.906353719630754,6.7060280296843,
134.845583928159));
#216962=CARTESIAN_POINT('Ctrl Pts',(-1.08097882032073,6.68242656114724,
134.853900131429));
#216963=CARTESIAN_POINT('Ctrl Pts',(-1.25485079803176,6.65197705904537,
134.862216334699));
#216964=CARTESIAN_POINT('Ctrl Pts',(-1.42740188091235,6.61474208645869,
134.870532537969));
#216965=CARTESIAN_POINT('Ctrl Pts',(-1.59980705750844,6.57753859913663,
134.878841709198));
#216966=CARTESIAN_POINT('Ctrl Pts',(-1.77089322619723,6.53356114592075,
134.887150880427));
#216967=CARTESIAN_POINT('Ctrl Pts',(-1.9400999808047,6.48292380523492,134.895460051656));
#216968=CARTESIAN_POINT('Ctrl Pts',(-2.10919468280949,6.43231999776016,
134.903763720361));
#216969=CARTESIAN_POINT('Ctrl Pts',(-2.27641211849353,6.37506519031083,
134.912067389066));
#216970=CARTESIAN_POINT('Ctrl Pts',(-2.44120406465513,6.31132408569797,
134.920371057771));
#216971=CARTESIAN_POINT('Ctrl Pts',(-2.60591708464302,6.24761350952787,
134.92867074948));
#216972=CARTESIAN_POINT('Ctrl Pts',(-2.76820660635052,6.17742295252512,
134.93697044119));
#216973=CARTESIAN_POINT('Ctrl Pts',(-2.92754129958098,6.10096639387956,
134.945270132899));
#216974=CARTESIAN_POINT('Ctrl Pts',(-3.08682887315697,6.02453244554285,
134.953567370161));
#216975=CARTESIAN_POINT('Ctrl Pts',(-3.24316304670243,5.94183633952596,
134.961864607423));
#216976=CARTESIAN_POINT('Ctrl Pts',(-3.39603394244471,5.85313953889393,
134.970161844686));
#216977=CARTESIAN_POINT('Ctrl Pts',(-3.54892028053974,5.76443377849702,
134.978459920099));
#216978=CARTESIAN_POINT('Ctrl Pts',(-3.69834233705561,5.66972628035997,
134.986757995512));
#216979=CARTESIAN_POINT('Ctrl Pts',(-3.84381574630596,5.56932397230134,
134.995056070925));
#216980=CARTESIAN_POINT('Ctrl Pts',(-3.98930378271827,5.46891156892131,
135.003354980698));
#216981=CARTESIAN_POINT('Ctrl Pts',(-4.13084209365886,5.36280341159873,
135.011653890472));
#216982=CARTESIAN_POINT('Ctrl Pts',(-4.26797625311067,5.2513491316883,135.019952800246));
#216983=CARTESIAN_POINT('Ctrl Pts',(-4.40514699306072,5.13986512138022,
135.028253923751));
#216984=CARTESIAN_POINT('Ctrl Pts',(-4.53791096991338,5.02303236570051,
135.036555047257));
#216985=CARTESIAN_POINT('Ctrl Pts',(-4.66584759328945,4.90124017328217,
135.044856170762));
#216986=CARTESIAN_POINT('Ctrl Pts',(-4.79383960942083,4.77939524846451,
135.053160888407));
#216987=CARTESIAN_POINT('Ctrl Pts',(-4.91699985457346,4.65258684715798,
135.061465606053));
#216988=CARTESIAN_POINT('Ctrl Pts',(-5.03494515810745,4.52124056591223,
135.069770323698));
#216989=CARTESIAN_POINT('Ctrl Pts',(-5.15303029447224,4.38973856399113,
135.078084887197));
#216990=CARTESIAN_POINT('Ctrl Pts',(-5.26588790351228,4.25368819222075,
135.086399450695));
#216991=CARTESIAN_POINT('Ctrl Pts',(-5.37317488258129,4.11354842942168,
135.094714014194));
#216992=CARTESIAN_POINT('Ctrl Pts',(-5.48052970397372,3.97332005002445,
135.103033835361));
#216993=CARTESIAN_POINT('Ctrl Pts',(-5.58230667026415,3.82899740668009,
135.111353656527));
#216994=CARTESIAN_POINT('Ctrl Pts',(-5.67820641843379,3.68106789799609,
135.119673477694));
#216995=CARTESIAN_POINT('Ctrl Pts',(-5.77424958151963,3.53291716560194,
135.128005740879));
#216996=CARTESIAN_POINT('Ctrl Pts',(-5.86439778375524,3.38114908719061,
135.136338004065));
#216997=CARTESIAN_POINT('Ctrl Pts',(-5.94839730981834,3.22627625050087,
135.14467026725));
#216998=CARTESIAN_POINT('Ctrl Pts',(-6.01164831454297,3.10965818151534,
135.150944398103));
#216999=CARTESIAN_POINT('Ctrl Pts',(-6.07141399149068,2.99128022710502,
135.157218528956));
#217000=CARTESIAN_POINT('Ctrl Pts',(-6.12760425966692,2.87136814722735,
135.163492659808));
#217001=CARTESIAN_POINT('Ctrl Pts',(-6.20546860883635,2.70520278870045,
135.172186889812));
#217002=CARTESIAN_POINT('Ctrl Pts',(-6.27668004813401,2.53563375665815,
135.180881119815));
#217003=CARTESIAN_POINT('Ctrl Pts',(-6.34094305750286,2.3632033643989,135.189575349818));
#217004=CARTESIAN_POINT('Ctrl Pts',(-6.40506363778926,2.19115513759997,
135.198250310397));
#217005=CARTESIAN_POINT('Ctrl Pts',(-6.46226638485983,2.01625846582904,
135.206925270975));
#217006=CARTESIAN_POINT('Ctrl Pts',(-6.51230193574305,1.83907925270158,
135.215600231554));
#217007=CARTESIAN_POINT('Ctrl Pts',(-6.56218337877673,1.66244574571772,
135.22424847354));
#217008=CARTESIAN_POINT('Ctrl Pts',(-6.60494156714428,1.48354399855786,
135.232896715525));
#217009=CARTESIAN_POINT('Ctrl Pts',(-6.64037571162132,1.30295794579476,
135.241544957511));
#217010=CARTESIAN_POINT('Ctrl Pts',(-6.67574416231199,1.12270669387829,
135.250177165929));
#217011=CARTESIAN_POINT('Ctrl Pts',(-6.70381557493082,0.940777645910259,
135.258809374347));
#217012=CARTESIAN_POINT('Ctrl Pts',(-6.72443845616014,0.757770710251219,
135.267441582765));
#217013=CARTESIAN_POINT('Ctrl Pts',(-6.74500929652179,0.575225583958943,
135.276052008212));
#217014=CARTESIAN_POINT('Ctrl Pts',(-6.75816905394779,0.391608284783801,
135.284662433659));
#217015=CARTESIAN_POINT('Ctrl Pts',(-6.76381701651168,0.207529195890568,
135.293272859106));
#217016=CARTESIAN_POINT('Ctrl Pts',(-6.76590452913319,0.139492728390334,
135.296455311468));
#217017=CARTESIAN_POINT('Ctrl Pts',(-6.76696637000047,0.0713933033251629,
135.299637763829));
#217018=CARTESIAN_POINT('Ctrl Pts',(-6.76699921371665,0.00326214013017339,
135.30282021619));
#217019=CARTESIAN_POINT('Ctrl Pts',(-6.767,6.93929656985413E-12,135.30282021619));
#217020=CARTESIAN_POINT('Ctrl Pts',(-6.76700000000019,-0.186007249520054,
135.311569728001));
#217021=CARTESIAN_POINT('Ctrl Pts',(-6.75932637294557,-0.372014355743232,
135.320319239812));
#217022=CARTESIAN_POINT('Ctrl Pts',(-6.74400518264234,-0.557389537480943,
135.329068751624));
#217023=CARTESIAN_POINT('Ctrl Pts',(-6.72868405705156,-0.742763936245454,
135.337818226479));
#217024=CARTESIAN_POINT('Ctrl Pts',(-6.7057154564581,-0.927506130236138,
135.346567701335));
#217025=CARTESIAN_POINT('Ctrl Pts',(-6.67517739404899,-1.1109886398957,
135.355317176191));
#217026=CARTESIAN_POINT('Ctrl Pts',(-6.64463945808786,-1.29447038981513,
135.364066614818));
#217027=CARTESIAN_POINT('Ctrl Pts',(-6.60653217008449,-1.47669218313263,
135.372816053445));
#217028=CARTESIAN_POINT('Ctrl Pts',(-6.5609849609278,-1.65703510598878,
135.381565492072));
#217029=CARTESIAN_POINT('Ctrl Pts',(-6.51543793658408,-1.83737729708305,
135.390314895197));
#217030=CARTESIAN_POINT('Ctrl Pts',(-6.46245112167539,-2.01584035510546,
135.399064298322));
#217031=CARTESIAN_POINT('Ctrl Pts',(-6.40220448374379,-2.19181813760425,
135.407813701447));
#217032=CARTESIAN_POINT('Ctrl Pts',(-6.34195808526632,-2.36779522066801,
135.416563069797));
#217033=CARTESIAN_POINT('Ctrl Pts',(-6.27445201433233,-2.54128677683847,
135.425312438147));
#217034=CARTESIAN_POINT('Ctrl Pts',(-6.19991555072031,-2.71170355384517,
135.434061806498));
#217035=CARTESIAN_POINT('Ctrl Pts',(-6.12537937716824,-2.88211966767197,
135.442811140799));
#217036=CARTESIAN_POINT('Ctrl Pts',(-6.04381298052655,-3.04946076371519,
135.451560475101));
#217037=CARTESIAN_POINT('Ctrl Pts',(-5.95549339335968,-3.21315848374295,
135.460309809403));
#217038=CARTESIAN_POINT('Ctrl Pts',(-5.8671741425556,-3.37685558033229,
135.469059110383));
#217039=CARTESIAN_POINT('Ctrl Pts',(-5.77210188876765,-3.53690907646483,
135.477808411363));
#217040=CARTESIAN_POINT('Ctrl Pts',(-5.6705995334718,-3.69277536969004,
135.486557712343));
#217041=CARTESIAN_POINT('Ctrl Pts',(-5.5690975563159,-3.84864108224624,
135.495306980729));
#217042=CARTESIAN_POINT('Ctrl Pts',(-5.4611656819708,-4.00031938297202,
135.504056249114));
#217043=CARTESIAN_POINT('Ctrl Pts',(-5.34717048533858,-4.14729511859525,
135.512805517499));
#217044=CARTESIAN_POINT('Ctrl Pts',(-5.23317570392105,-4.29427031887589,
135.521554754016));
#217045=CARTESIAN_POINT('Ctrl Pts',(-5.11311782003796,-4.43654276189222,
135.530303990533));
#217046=CARTESIAN_POINT('Ctrl Pts',(-4.98740458985049,-4.57362924351529,
135.53905322705));
#217047=CARTESIAN_POINT('Ctrl Pts',(-4.86169180712061,-4.71071523719938,
135.547802432426));
#217048=CARTESIAN_POINT('Ctrl Pts',(-4.73032391204511,-4.84261509522905,
135.556551637801));
#217049=CARTESIAN_POINT('Ctrl Pts',(-4.59374707013962,-4.96888084537994,
135.565300843177));
#217050=CARTESIAN_POINT('Ctrl Pts',(-4.45717070301812,-5.09514615659143,
135.574050018137));
#217051=CARTESIAN_POINT('Ctrl Pts',(-4.31538563571411,-5.21577720459222,
135.582799193098));
#217052=CARTESIAN_POINT('Ctrl Pts',(-4.16887341029881,-5.33036429232596,
135.591548368058));
#217053=CARTESIAN_POINT('Ctrl Pts',(-4.02236168204108,-5.44495099123318,
135.60029751333));
#217054=CARTESIAN_POINT('Ctrl Pts',(-3.87112305348597,-5.553493594383,135.609046658602));
#217055=CARTESIAN_POINT('Ctrl Pts',(-3.71567117018224,-5.65562346298589,
135.617795803874));
#217056=CARTESIAN_POINT('Ctrl Pts',(-3.560219801463,-5.75775299351346,135.626544920184));
#217057=CARTESIAN_POINT('Ctrl Pts',(-3.40055544538848,-5.85346967463583,
135.635294036494));
#217058=CARTESIAN_POINT('Ctrl Pts',(-3.2372203598737,-5.94244842986619,
135.644043152804));
#217059=CARTESIAN_POINT('Ctrl Pts',(-3.07388580147699,-6.03142689794265,
135.652792240879));
#217060=CARTESIAN_POINT('Ctrl Pts',(-2.90688078897097,-6.11366734656535,
135.661541328954));
#217061=CARTESIAN_POINT('Ctrl Pts',(-2.73677250721889,-6.18889046952124,
135.670290417029));
#217062=CARTESIAN_POINT('Ctrl Pts',(-2.56666476032021,-6.26411335596106,
135.679039477595));
#217063=CARTESIAN_POINT('Ctrl Pts',(-2.39345402575724,-6.33231884500344,
135.687788538161));
#217064=CARTESIAN_POINT('Ctrl Pts',(-2.21772856066169,-6.39327529762527,
135.696537598727));
#217065=CARTESIAN_POINT('Ctrl Pts',(-2.04200363349079,-6.45423156364933,
135.705286632511));
#217066=CARTESIAN_POINT('Ctrl Pts',(-1.86376426189832,-6.507938743755,135.714035666294));
#217067=CARTESIAN_POINT('Ctrl Pts',(-1.68361577753694,-6.55421443909403,
135.722784700078));
#217068=CARTESIAN_POINT('Ctrl Pts',(-1.50346782968356,-6.60048999661741,
135.731533707806));
#217069=CARTESIAN_POINT('Ctrl Pts',(-1.3214110579556,-6.63933404237598,
135.740282715534));
#217070=CARTESIAN_POINT('Ctrl Pts',(-1.13806375487611,-6.6706146560746,
135.749031723262));
#217071=CARTESIAN_POINT('Ctrl Pts',(-0.954716982609564,-6.70189517921201,
135.75778070566));
#217072=CARTESIAN_POINT('Ctrl Pts',(-0.770079968909347,-6.72561226592144,
135.766529688058));
#217073=CARTESIAN_POINT('Ctrl Pts',(-0.584779765566115,-6.74168536983034,
135.775278670457));
#217074=CARTESIAN_POINT('Ctrl Pts',(-0.391489830659183,-6.75845151013807,
135.784404889467));
#217075=CARTESIAN_POINT('Ctrl Pts',(-0.197478578246223,-6.76689983031602,
135.793531108477));
#217076=CARTESIAN_POINT('Ctrl Pts',(-0.00346287645922686,-6.76699911397117,
135.802657327486));
#217077=CARTESIAN_POINT('Ctrl Pts',(0.184489834647022,-6.7670952950121,
135.811498352152));
#217078=CARTESIAN_POINT('Ctrl Pts',(0.372446404242634,-6.75935639738206,
135.820339376818));
#217079=CARTESIAN_POINT('Ctrl Pts',(0.559755019481737,-6.74380925873241,
135.829180401484));
#217080=CARTESIAN_POINT('Ctrl Pts',(0.745134705515176,-6.72842222659879,
135.837930380094));
#217081=CARTESIAN_POINT('Ctrl Pts',(0.929879431221979,-6.70538706057615,
135.846680358703));
#217082=CARTESIAN_POINT('Ctrl Pts',(1.11336163626168,-6.67478200894237,
135.855430337313));
#217083=CARTESIAN_POINT('Ctrl Pts',(1.29684196300084,-6.64417727061137,
135.86418022635));
#217084=CARTESIAN_POINT('Ctrl Pts',(1.47905951216898,-6.60600284890728,
135.872930115386));
#217085=CARTESIAN_POINT('Ctrl Pts',(1.65939532066495,-6.5603884160738,135.881680004423));
#217086=CARTESIAN_POINT('Ctrl Pts',(1.83972934300219,-6.51477443503421,
135.890429806795));
#217087=CARTESIAN_POINT('Ctrl Pts',(2.01818138405689,-6.46172066062321,
135.899179609167));
#217088=CARTESIAN_POINT('Ctrl Pts',(2.19414528353632,-6.40140730423673,
135.907929411539));
#217089=CARTESIAN_POINT('Ctrl Pts',(2.37010749863427,-6.34109452518856,
135.916679130155));
#217090=CARTESIAN_POINT('Ctrl Pts',(2.54358134865883,-6.27352239616737,
135.925428848772));
#217091=CARTESIAN_POINT('Ctrl Pts',(2.71397759434976,-6.19892043967073,
135.934178567388));
#217092=CARTESIAN_POINT('Ctrl Pts',(2.88437226557548,-6.12431917249786,
135.942928205157));
#217093=CARTESIAN_POINT('Ctrl Pts',(3.05168912680384,-6.04268832279087,
135.951677842925));
#217094=CARTESIAN_POINT('Ctrl Pts',(3.21535986273288,-5.9543051612364,135.960427480694));
#217095=CARTESIAN_POINT('Ctrl Pts',(3.3790291407228,-5.86592278697764,135.969177040523));
#217096=CARTESIAN_POINT('Ctrl Pts',(3.53905210621016,-5.77078835742282,
135.977926600352));
#217097=CARTESIAN_POINT('Ctrl Pts',(3.69488522831148,-5.66922500431987,
135.986676160181));
#217098=CARTESIAN_POINT('Ctrl Pts',(3.85071701406418,-5.56766252217455,
135.995425644979));
#217099=CARTESIAN_POINT('Ctrl Pts',(4.00235878821909,-5.45967138329733,
136.004175129776));
#217100=CARTESIAN_POINT('Ctrl Pts',(4.14929549610857,-5.3456183819997,136.012924614573));
#217101=CARTESIAN_POINT('Ctrl Pts',(4.29623099275649,-5.23156632087378,
136.021674027245));
#217102=CARTESIAN_POINT('Ctrl Pts',(4.43846127435614,-5.11145267305324,
136.030423439918));
#217103=CARTESIAN_POINT('Ctrl Pts',(4.57550326054055,-4.9856854005024,136.039172852591));
#217104=CARTESIAN_POINT('Ctrl Pts',(4.71254416257393,-4.85991912290736,
136.047922196046));
#217105=CARTESIAN_POINT('Ctrl Pts',(4.84439664018374,-4.72849950385815,
136.056671539501));
#217106=CARTESIAN_POINT('Ctrl Pts',(4.97061286794359,-4.59187289861485,
136.065420882956));
#217107=CARTESIAN_POINT('Ctrl Pts',(5.09682813912306,-4.45524732885118,
136.074170160101));
#217108=CARTESIAN_POINT('Ctrl Pts',(5.21740705147468,-4.31341506236236,
136.082919437246));
#217109=CARTESIAN_POINT('Ctrl Pts',(5.33194007545334,-4.16685781276187,
136.091668714391));
#217110=CARTESIAN_POINT('Ctrl Pts',(5.44647226944125,-4.02030162522329,
136.100417928132));
#217111=CARTESIAN_POINT('Ctrl Pts',(5.55495848627756,-3.86902074888446,
136.109167141873));
#217112=CARTESIAN_POINT('Ctrl Pts',(5.65703027291435,-3.713528980812,136.117916355614));
#217113=CARTESIAN_POINT('Ctrl Pts',(5.75910135376652,-3.55803828790146,
136.126665508858));
#217114=CARTESIAN_POINT('Ctrl Pts',(5.85475793592416,-3.39833700107291,
136.135414662102));
#217115=CARTESIAN_POINT('Ctrl Pts',(5.94367514427073,-3.23496750824152,
136.144163815346));
#217116=CARTESIAN_POINT('Ctrl Pts',(6.03259176732325,-3.07159909078344,
136.152912910999));
#217117=CARTESIAN_POINT('Ctrl Pts',(6.1147689683562,-2.90456276732074,136.161662006652));
#217118=CARTESIAN_POINT('Ctrl Pts',(6.18992765547595,-2.73442583003709,
136.170411102304));
#217119=CARTESIAN_POINT('Ctrl Pts',(6.2650858728278,-2.5642899561684,136.179160143273));
#217120=CARTESIAN_POINT('Ctrl Pts',(6.33322554826903,-2.39105376935882,
136.187909184241));
#217121=CARTESIAN_POINT('Ctrl Pts',(6.39411526732792,-2.21530561054769,
136.196658225209));
#217122=CARTESIAN_POINT('Ctrl Pts',(6.45500462602617,-2.03955849185824,
136.205407214398));
#217123=CARTESIAN_POINT('Ctrl Pts',(6.50864402040522,-1.86129970165306,
136.214156203587));
#217124=CARTESIAN_POINT('Ctrl Pts',(6.55485128368396,-1.68113463136857,
136.222905192776));
#217125=CARTESIAN_POINT('Ctrl Pts',(6.60199809554146,-1.49730620117666,
136.231832078247));
#217126=CARTESIAN_POINT('Ctrl Pts',(6.64140720707716,-1.31149343246494,
136.240758963719));
#217127=CARTESIAN_POINT('Ctrl Pts',(6.6729392872275,-1.12435326698318,136.24968584919));
#217128=CARTESIAN_POINT('Ctrl Pts',(6.70384625876143,-0.940923067014677,
136.258435763367));
#217129=CARTESIAN_POINT('Ctrl Pts',(6.72718554579703,-0.756217899529902,
136.267185677545));
#217130=CARTESIAN_POINT('Ctrl Pts',(6.74287786815257,-0.570865181262876,
136.275935591722));
#217131=CARTESIAN_POINT('Ctrl Pts',(6.75856988190798,-0.385516108082386,
136.284685333827));
#217132=CARTESIAN_POINT('Ctrl Pts',(6.76661520773378,-0.199519795234839,
136.293435075931));
#217133=CARTESIAN_POINT('Ctrl Pts',(6.76698651789577,-0.0135080204641805,
136.302184818036));
#217134=CARTESIAN_POINT('Ctrl Pts',(6.76735782124925,0.172500343504387,
136.310934399701));
#217135=CARTESIAN_POINT('Ctrl Pts',(6.76005538995229,0.358523882202315,
136.319683981366));
#217136=CARTESIAN_POINT('Ctrl Pts',(6.74510402742431,0.543930748555749,
136.328433563031));
#217137=CARTESIAN_POINT('Ctrl Pts',(6.73015291918125,0.729334461606526,
136.337182995887));
#217138=CARTESIAN_POINT('Ctrl Pts',(6.70755316306714,0.914121237625899,
136.345932428744));
#217139=CARTESIAN_POINT('Ctrl Pts',(6.6773815187472,1.09766345165238,136.354681861601));
#217140=CARTESIAN_POINT('Ctrl Pts',(6.64721034747738,1.28120278798787,136.363431157278));
#217141=CARTESIAN_POINT('Ctrl Pts',(6.60946757205334,1.4634973185946,136.372180452956));
#217142=CARTESIAN_POINT('Ctrl Pts',(6.56428138111738,1.64392790277301,136.380929748633));
#217143=CARTESIAN_POINT('Ctrl Pts',(6.51909583860089,1.82435589778201,136.389678918759));
#217144=CARTESIAN_POINT('Ctrl Pts',(6.46646716393138,2.00291972191416,136.398428088885));
#217145=CARTESIAN_POINT('Ctrl Pts',(6.4065740987317,2.17901292273821,136.40717725901));
#217146=CARTESIAN_POINT('Ctrl Pts',(6.3466818134239,2.35510383058131,136.415926315209));
#217147=CARTESIAN_POINT('Ctrl Pts',(6.27952541914391,2.52872390821732,136.424675371408));
#217148=CARTESIAN_POINT('Ctrl Pts',(6.20533299175886,2.69928350889436,136.433424427607));
#217149=CARTESIAN_POINT('Ctrl Pts',(6.12831602991927,2.8763363796482,136.442506563766));
#217150=CARTESIAN_POINT('Ctrl Pts',(6.04371690605653,3.05009086600705,136.451588699924));
#217151=CARTESIAN_POINT('Ctrl Pts',(5.95184520317016,3.21991112882022,136.460670836082));
#217152=CARTESIAN_POINT('Ctrl Pts',(5.86333549509676,3.38351691182321,136.469420616426));
#217153=CARTESIAN_POINT('Ctrl Pts',(5.76807618099786,3.54347103711324,136.478170396769));
#217154=CARTESIAN_POINT('Ctrl Pts',(5.66639083309448,3.69923018027033,136.486920177113));
#217155=CARTESIAN_POINT('Ctrl Pts',(5.56470914082653,3.85498372381396,136.495669642898));
#217156=CARTESIAN_POINT('Ctrl Pts',(5.4566020337254,4.00654234701354,136.504419108683));
#217157=CARTESIAN_POINT('Ctrl Pts',(5.34243669839709,4.15339127986035,136.513168574467));
#217158=CARTESIAN_POINT('Ctrl Pts',(5.22827486051102,4.30023571400659,136.521917772213));
#217159=CARTESIAN_POINT('Ctrl Pts',(5.10805534167639,4.44237052027862,136.53066696996));
#217160=CARTESIAN_POINT('Ctrl Pts',(4.98218644340496,4.57931296628128,136.539416167706));
#217161=CARTESIAN_POINT('Ctrl Pts',(4.85632073220169,4.71625194482759,136.548165143917));
#217162=CARTESIAN_POINT('Ctrl Pts',(4.72480612170941,4.84799861523901,136.556914120129));
#217163=CARTESIAN_POINT('Ctrl Pts',(4.58808925235973,4.97410554897874,136.56566309634));
#217164=CARTESIAN_POINT('Ctrl Pts',(4.45136349474737,5.10022068120604,136.574412641342));
#217165=CARTESIAN_POINT('Ctrl Pts',(4.30943501210796,5.22069514871242,136.583162186344));
#217166=CARTESIAN_POINT('Ctrl Pts',(4.16278587432525,5.33511975165677,136.591911731345));
#217167=CARTESIAN_POINT('Ctrl Pts',(4.016145357412,5.44953762807288,136.600660761999));
#217168=CARTESIAN_POINT('Ctrl Pts',(3.86478496658682,5.55790617532256,136.609409792653));
#217169=CARTESIAN_POINT('Ctrl Pts',(3.70921874747961,5.65985735538855,136.618158823307));
#217170=CARTESIAN_POINT('Ctrl Pts',(3.55365041606682,5.76180991976565,136.626907972756));
#217171=CARTESIAN_POINT('Ctrl Pts',(3.39387638175318,5.85734478552352,136.635657122206));
#217172=CARTESIAN_POINT('Ctrl Pts',(3.23043927905349,5.94613749120792,136.644406271655));
#217173=CARTESIAN_POINT('Ctrl Pts',(3.18691767070967,5.96978206943863,136.646736079572));
#217174=CARTESIAN_POINT('Ctrl Pts',(3.14313645919891,5.99294880633292,136.649065887488));
#217175=CARTESIAN_POINT('Ctrl Pts',(3.09910619832119,6.01563211736948,136.651395695404));
#217176=CARTESIAN_POINT('Origin',(0.,0.,8.));
#217177=CARTESIAN_POINT('',(-7.91099969351913,0.00214482957247683,8.64224520787028));
#217178=CARTESIAN_POINT('',(3.42067962509756,7.13322310757503,8.));
#217179=CARTESIAN_POINT('Ctrl Pts',(-7.91099969351913,0.00214482957247683,
8.64224520787028));
#217180=CARTESIAN_POINT('Ctrl Pts',(-7.91037070257867,2.20309451064308,
8.55368653892647));
#217181=CARTESIAN_POINT('Ctrl Pts',(-6.94161582034834,4.38658408256068,
8.46512786998266));
#217182=CARTESIAN_POINT('Ctrl Pts',(-3.67820201488298,7.34180684107625,
8.28798176530613));
#217183=CARTESIAN_POINT('Ctrl Pts',(-1.4086817587176,8.08992666571333,8.1993943295734));
#217184=CARTESIAN_POINT('Ctrl Pts',(1.69567364519642,7.78146992497721,8.07387126256046));
#217185=CARTESIAN_POINT('Ctrl Pts',(2.59296389908063,7.53014751000291,8.03693563128023));
#217186=CARTESIAN_POINT('Ctrl Pts',(3.42067962509756,7.13322310757503,8.));
#217187=CARTESIAN_POINT('',(-3.42067962509656,7.13322310757551,8.));
#217188=CARTESIAN_POINT('Origin',(0.,0.,8.));
#217189=CARTESIAN_POINT('',(-7.911,-6.54698517621455E-12,10.3576684917633));
#217190=CARTESIAN_POINT('Ctrl Pts',(-3.42067962509657,7.13322310757551,
7.99999999999995));
#217191=CARTESIAN_POINT('Ctrl Pts',(-3.44489616196924,7.12161026257943,
8.00108062834697));
#217192=CARTESIAN_POINT('Ctrl Pts',(-3.46905336347038,7.109874194047,8.00216253476664));
#217193=CARTESIAN_POINT('Ctrl Pts',(-3.52825103437878,7.08074121098439,
8.004823170029));
#217194=CARTESIAN_POINT('Ctrl Pts',(-3.56322308571844,7.06320696896667,
8.00640312738629));
#217195=CARTESIAN_POINT('Ctrl Pts',(-3.73207987925261,6.97697250955979,
8.01406979255727));
#217196=CARTESIAN_POINT('Ctrl Pts',(-3.86411558107353,6.90472128607229,
8.02018090088184));
#217197=CARTESIAN_POINT('Ctrl Pts',(-4.1228934846205,6.75336685075825,8.0323662050104));
#217198=CARTESIAN_POINT('Ctrl Pts',(-4.24961771503789,6.67435119686245,
8.03843788348709));
#217199=CARTESIAN_POINT('Ctrl Pts',(-4.47947890501097,6.52182529976682,
8.04963551657544));
#217200=CARTESIAN_POINT('Ctrl Pts',(-4.58323415501454,6.44933340920085,
8.05476307079416));
#217201=CARTESIAN_POINT('Ctrl Pts',(-4.72079991078508,6.34822184255562,
8.06166188123683));
#217202=CARTESIAN_POINT('Ctrl Pts',(-4.75617411126229,6.32176242800932,
8.06344512348087));
#217203=CARTESIAN_POINT('Ctrl Pts',(-4.82371178017375,6.27035742417348,
8.06686785533001));
#217204=CARTESIAN_POINT('Ctrl Pts',(-4.85590799614451,6.2454571577027,8.06850757265641));
#217205=CARTESIAN_POINT('Ctrl Pts',(-4.91919182907623,6.19572880863505,
8.07174681245983));
#217206=CARTESIAN_POINT('Ctrl Pts',(-4.95028717324043,6.1709124636523,8.07334636169313));
#217207=CARTESIAN_POINT('Ctrl Pts',(-5.03093952164691,6.10554409710508,
8.07751629300772));
#217208=CARTESIAN_POINT('Ctrl Pts',(-5.08019376990848,6.06462302989733,
8.08008398698963));
#217209=CARTESIAN_POINT('Ctrl Pts',(-5.26858972302629,5.90419545879211,
8.08999106706074));
#217210=CARTESIAN_POINT('Ctrl Pts',(-5.40405659601133,5.78046146870616,
8.09729751661436));
#217211=CARTESIAN_POINT('Ctrl Pts',(-5.7305208338707,5.46075679401348,8.11545169826978));
#217212=CARTESIAN_POINT('Ctrl Pts',(-5.91588381712733,5.25937752987953,
8.12626051285213));
#217213=CARTESIAN_POINT('Ctrl Pts',(-6.16201694618838,4.96246365723223,
8.14159012515508));
#217214=CARTESIAN_POINT('Ctrl Pts',(-6.231746020937,4.87461174296043,8.14605752741075));
#217215=CARTESIAN_POINT('Ctrl Pts',(-6.30121186644715,4.78316393843605,
8.1506538525498));
#217216=CARTESIAN_POINT('Ctrl Pts',(-6.30283924957226,4.78101930992288,
8.15076161551514));
#217217=CARTESIAN_POINT('Ctrl Pts',(-6.3052682769726,4.77781484794909,8.15092258868417));
#217218=CARTESIAN_POINT('Ctrl Pts',(-6.30607074968009,4.77675564226476,
8.15097578969882));
#217219=CARTESIAN_POINT('Ctrl Pts',(-6.30725841110619,4.7751871945745,8.15105455793406));
#217220=CARTESIAN_POINT('Ctrl Pts',(-6.30764380502466,4.77467810816932,
8.15108012285505));
#217221=CARTESIAN_POINT('Ctrl Pts',(-6.3098237178123,4.77179782608195,8.15122475336233));
#217222=CARTESIAN_POINT('Ctrl Pts',(-6.31161696088066,4.76942566584106,
8.15134383319784));
#217223=CARTESIAN_POINT('Ctrl Pts',(-6.31475886559297,4.76526457697446,
8.15155265297687));
#217224=CARTESIAN_POINT('Ctrl Pts',(-6.31610810579078,4.76347608528831,
8.15164238635198));
#217225=CARTESIAN_POINT('Ctrl Pts',(-6.31845356152026,4.76036430690394,
8.1517984776924));
#217226=CARTESIAN_POINT('Ctrl Pts',(-6.31945012162097,4.75904127990884,
8.15186483170955));
#217227=CARTESIAN_POINT('Ctrl Pts',(-6.32117176135778,4.7567541473838,8.15197951986239));
#217228=CARTESIAN_POINT('Ctrl Pts',(-6.32189703617846,4.7557901887276,8.15202785174711));
#217229=CARTESIAN_POINT('Ctrl Pts',(-6.32314405624532,4.75413199208373,
8.15211098210216));
#217230=CARTESIAN_POINT('Ctrl Pts',(-6.32366590774386,4.75343783397053,
8.15214577934082));
#217231=CARTESIAN_POINT('Ctrl Pts',(-6.32455997956009,4.75224814682945,
8.15220541170329));
#217232=CARTESIAN_POINT('Ctrl Pts',(-6.32493225598301,4.75175265994797,
8.15223024617435));
#217233=CARTESIAN_POINT('Ctrl Pts',(-6.32556840365334,4.75090576246467,
8.15227269123428));
#217234=CARTESIAN_POINT('Ctrl Pts',(-6.32583230384371,4.7505543736247,8.15229030148437));
#217235=CARTESIAN_POINT('Ctrl Pts',(-6.32628240796313,4.74995494619594,
8.15232034117433));
#217236=CARTESIAN_POINT('Ctrl Pts',(-6.32646862661027,4.74970691861204,
8.15233277044376));
#217237=CARTESIAN_POINT('Ctrl Pts',(-6.32746906980883,4.74837424915331,
8.15239955174269));
#217238=CARTESIAN_POINT('Ctrl Pts',(-6.32828302993814,4.74728940895812,
8.15245390686309));
#217239=CARTESIAN_POINT('Ctrl Pts',(-6.32981681244675,4.7452440992548,8.15255637203748));
#217240=CARTESIAN_POINT('Ctrl Pts',(-6.33053669530587,4.74428367512224,
8.152604481378));
#217241=CARTESIAN_POINT('Ctrl Pts',(-6.33189056223415,4.74247657102205,
8.15269499184989));
#217242=CARTESIAN_POINT('Ctrl Pts',(-6.33252459513822,4.74162992764851,
8.15273739240259));
#217243=CARTESIAN_POINT('Ctrl Pts',(-6.33371478693054,4.74003996393019,
8.15281701085052));
#217244=CARTESIAN_POINT('Ctrl Pts',(-6.33427098691357,4.73929666999183,
8.15285422842171));
#217245=CARTESIAN_POINT('Ctrl Pts',(-6.34690696063237,4.72240402291306,
8.15369998657488));
#217246=CARTESIAN_POINT('Ctrl Pts',(-6.35892504913736,4.706208658729,8.15450925886066));
#217247=CARTESIAN_POINT('Ctrl Pts',(-6.38185619673594,4.67505884530564,
8.15606295834953));
#217248=CARTESIAN_POINT('Ctrl Pts',(-6.3927789522268,4.66011169273404,8.15680725374525));
#217249=CARTESIAN_POINT('Ctrl Pts',(-6.41586478693557,4.62828616771946,
8.15838952923648));
#217250=CARTESIAN_POINT('Ctrl Pts',(-6.42801392534389,4.61139792103343,
8.15922772072681));
#217251=CARTESIAN_POINT('Ctrl Pts',(-6.46234659646926,4.56327352471234,
8.16161206849807));
#217252=CARTESIAN_POINT('Ctrl Pts',(-6.48436997999502,4.53192395569455,
8.16316030432853));
#217253=CARTESIAN_POINT('Ctrl Pts',(-6.59396487541828,4.37348471773237,
8.1709576194927));
#217254=CARTESIAN_POINT('Ctrl Pts',(-6.67803133589984,4.24401206271492,
8.17724056167673));
#217255=CARTESIAN_POINT('Ctrl Pts',(-6.84900707012616,3.96301699898009,
8.19063853914678));
#217256=CARTESIAN_POINT('Ctrl Pts',(-6.93479615302133,3.810905977909,8.19775058869798));
#217257=CARTESIAN_POINT('Ctrl Pts',(-7.04809404058325,3.59350397157942,
8.20769640499898));
#217258=CARTESIAN_POINT('Ctrl Pts',(-7.0798670713997,3.53049326770188,8.21055424082725));
#217259=CARTESIAN_POINT('Ctrl Pts',(-7.12892538659613,3.42987691122489,
8.2150781158383));
#217260=CARTESIAN_POINT('Ctrl Pts',(-7.14676585079713,3.39254634196463,
8.21674805274142));
#217261=CARTESIAN_POINT('Ctrl Pts',(-7.17719440879838,3.3275702850262,8.21964002157895));
#217262=CARTESIAN_POINT('Ctrl Pts',(-7.18991762787208,3.29998910514304,
8.22086307439478));
#217263=CARTESIAN_POINT('Ctrl Pts',(-7.21424617641942,3.24644143645658,
8.22322887644935));
#217264=CARTESIAN_POINT('Ctrl Pts',(-7.22587094006779,3.22048428920485,
8.22437176550019));
#217265=CARTESIAN_POINT('Ctrl Pts',(-7.24859866089076,3.16899253822501,
8.22663125844302));
#217266=CARTESIAN_POINT('Ctrl Pts',(-7.25970729108622,3.14346088041579,
8.22774789415815));
#217267=CARTESIAN_POINT('Ctrl Pts',(-7.28825882046671,3.07688049422375,
8.23065030612765));
#217268=CARTESIAN_POINT('Ctrl Pts',(-7.30548980830494,3.03574190125326,
8.23243428890514));
#217269=CARTESIAN_POINT('Ctrl Pts',(-7.36594846086816,2.88790195944531,
8.23881298128726));
#217270=CARTESIAN_POINT('Ctrl Pts',(-7.40719394056845,2.78040513357046,
8.24339067858313));
#217271=CARTESIAN_POINT('Ctrl Pts',(-7.55974311846658,2.35530268793264,
8.26128696507654));
#217272=CARTESIAN_POINT('Ctrl Pts',(-7.65308059558276,2.03163092083539,
8.27444842044223));
#217273=CARTESIAN_POINT('Ctrl Pts',(-7.74957012589917,1.59391405026631,
8.29211198302982));
#217274=CARTESIAN_POINT('Ctrl Pts',(-7.77130362350533,1.48433108845941,
8.29652511896635));
#217275=CARTESIAN_POINT('Ctrl Pts',(-7.80185086684639,1.31116637868868,
8.30351442441401));
#217276=CARTESIAN_POINT('Ctrl Pts',(-7.81222398254457,1.24787441711603,
8.30607233169107));
#217277=CARTESIAN_POINT('Ctrl Pts',(-7.82476727290191,1.16504247183047,
8.30942941745381));
#217278=CARTESIAN_POINT('Ctrl Pts',(-7.82763590111199,1.14561033173175,
8.31021766186169));
#217279=CARTESIAN_POINT('Ctrl Pts',(-7.83221168575533,1.11379413843461,
8.31150956172022));
#217280=CARTESIAN_POINT('Ctrl Pts',(-7.83396191720569,1.10141633910341,
8.31201248749622));
#217281=CARTESIAN_POINT('Ctrl Pts',(-7.83730150803856,1.07738773824884,
8.31298948906482));
#217282=CARTESIAN_POINT('Ctrl Pts',(-7.83889424480481,1.06573743685103,
8.31346350363929));
#217283=CARTESIAN_POINT('Ctrl Pts',(-7.84252165388203,1.03875612518575,
8.31456207680034));
#217284=CARTESIAN_POINT('Ctrl Pts',(-7.8445373542177,1.02342262792947,8.31518698476303));
#217285=CARTESIAN_POINT('Ctrl Pts',(-7.85014022691805,0.979812160872172,
8.31696614771628));
#217286=CARTESIAN_POINT('Ctrl Pts',(-7.85361952585118,0.951521820256821,
8.318122584369));
#217287=CARTESIAN_POINT('Ctrl Pts',(-7.8937873969268,0.609675840819445,
8.33212312057686));
#217288=CARTESIAN_POINT('Ctrl Pts',(-7.91182712553228,0.294221168223732,
8.34530284940324));
#217289=CARTESIAN_POINT('Ctrl Pts',(-7.90979792715798,-0.453916304909866,
8.37668785241045));
#217290=CARTESIAN_POINT('Ctrl Pts',(-7.87316573965032,-0.885560802343966,
8.39487570545381));
#217291=CARTESIAN_POINT('Ctrl Pts',(-7.76783241553769,-1.51187307472053,
8.42111027935031));
#217292=CARTESIAN_POINT('Ctrl Pts',(-7.7265602089607,-1.71033637076335,
8.4294061156004));
#217293=CARTESIAN_POINT('Ctrl Pts',(-7.66662143851645,-1.95165412892429,
8.43949037576807));
#217294=CARTESIAN_POINT('Ctrl Pts',(-7.65514048357083,-1.996211994601,8.44135233994781));
#217295=CARTESIAN_POINT('Ctrl Pts',(-7.63732356179955,-2.06294485578655,
8.44414139215461));
#217296=CARTESIAN_POINT('Ctrl Pts',(-7.63127833121435,-2.08519632190923,
8.44507145248801));
#217297=CARTESIAN_POINT('Ctrl Pts',(-7.61932656067252,-2.128440586409,8.44687920414763));
#217298=CARTESIAN_POINT('Ctrl Pts',(-7.61343032938801,-2.14943601689064,
8.44775699248032));
#217299=CARTESIAN_POINT('Ctrl Pts',(-7.60096872045207,-2.19311494033233,
8.44958346471322));
#217300=CARTESIAN_POINT('Ctrl Pts',(-7.59438843737883,-2.2157939653495,
8.45053198828996));
#217301=CARTESIAN_POINT('Ctrl Pts',(-7.57594732406781,-2.27830426595978,
8.4531470672118));
#217302=CARTESIAN_POINT('Ctrl Pts',(-7.56387399234706,-2.31807213727665,
8.45481146952113));
#217303=CARTESIAN_POINT('Ctrl Pts',(-7.51306425492964,-2.4808078936581,
8.46162689420654));
#217304=CARTESIAN_POINT('Ctrl Pts',(-7.47163781704315,-2.60291589587731,
8.46675105322172));
#217305=CARTESIAN_POINT('Ctrl Pts',(-7.34475073858618,-2.9488909578239,
8.48133476395445));
#217306=CARTESIAN_POINT('Ctrl Pts',(-7.25207831476744,-3.16996615482062,
8.49074969533208));
#217307=CARTESIAN_POINT('Ctrl Pts',(-6.92549199415194,-3.85944990412971,
8.52039672915874));
#217308=CARTESIAN_POINT('Ctrl Pts',(-6.65509131412303,-4.30901099874273,
8.54002080608389));
#217309=CARTESIAN_POINT('Ctrl Pts',(-6.12000715349156,-5.02669967795899,
8.5733643409996));
#217310=CARTESIAN_POINT('Ctrl Pts',(-5.87700617083448,-5.30876403512616,
8.58714527828322));
#217311=CARTESIAN_POINT('Ctrl Pts',(-5.5301472547523,-5.65826214385748,
8.60618930549681));
#217312=CARTESIAN_POINT('Ctrl Pts',(-5.4432687188775,-5.74188847932049,
8.61091576102426));
#217313=CARTESIAN_POINT('Ctrl Pts',(-5.34282275833126,-5.83424530474291,
8.61636969928414));
#217314=CARTESIAN_POINT('Ctrl Pts',(-5.33109779227009,-5.84496104588815,
8.61700617691609));
#217315=CARTESIAN_POINT('Ctrl Pts',(-5.31337811782222,-5.86105782835972,
8.61796795665845));
#217316=CARTESIAN_POINT('Ctrl Pts',(-5.30740729686589,-5.86646517716934,
8.61829201846961));
#217317=CARTESIAN_POINT('Ctrl Pts',(-5.29714895474028,-5.87572694997919,
8.61884876678747));
#217318=CARTESIAN_POINT('Ctrl Pts',(-5.29286545322486,-5.87958583008033,
8.61908123953142));
#217319=CARTESIAN_POINT('Ctrl Pts',(-5.28405732787018,-5.88750338436385,
8.61955926953376));
#217320=CARTESIAN_POINT('Ctrl Pts',(-5.27953223832777,-5.89156153233657,
8.61980485198002));
#217321=CARTESIAN_POINT('Ctrl Pts',(-5.26739156119237,-5.90242420026434,
8.6204637519577));
#217322=CARTESIAN_POINT('Ctrl Pts',(-5.25976748102481,-5.90921918218692,
8.62087753703051));
#217323=CARTESIAN_POINT('Ctrl Pts',(-5.23208151202193,-5.93379834581175,
8.62238026485478));
#217324=CARTESIAN_POINT('Ctrl Pts',(-5.21194254755674,-5.9514951579442,
8.62347357727135));
#217325=CARTESIAN_POINT('Ctrl Pts',(-4.88789553212716,-6.23334042000821,
8.6410753294484));
#217326=CARTESIAN_POINT('Ctrl Pts',(-4.56440662098179,-6.47395701534081,
8.65899822507158));
#217327=CARTESIAN_POINT('Ctrl Pts',(-3.86466130504848,-6.91585285960687,
8.696577733721));
#217328=CARTESIAN_POINT('Ctrl Pts',(-3.48750813687489,-7.1135040855648,
8.71616210765956));
#217329=CARTESIAN_POINT('Ctrl Pts',(-2.82386912088756,-7.39576409731374,
8.74824627365588));
#217330=CARTESIAN_POINT('Ctrl Pts',(-2.54513820613614,-7.49625619154637,
8.76107714788845));
#217331=CARTESIAN_POINT('Ctrl Pts',(-2.15302756136409,-7.61322439324809,
8.77813941959008));
#217332=CARTESIAN_POINT('Ctrl Pts',(-2.04396038013496,-7.64322841792792,
8.78278446980245));
#217333=CARTESIAN_POINT('Ctrl Pts',(-1.9172706737058,-7.67517439757066,
8.78806561117108));
#217334=CARTESIAN_POINT('Ctrl Pts',(-1.90024273767793,-7.67940794672888,
8.78877306735934));
#217335=CARTESIAN_POINT('Ctrl Pts',(-1.87438460940062,-7.6857456196566,
8.78984382309759));
#217336=CARTESIAN_POINT('Ctrl Pts',(-1.86556470013447,-7.68789124170809,
8.7902084169985));
#217337=CARTESIAN_POINT('Ctrl Pts',(-1.84960236412615,-7.69174531735599,
8.79086712840494));
#217338=CARTESIAN_POINT('Ctrl Pts',(-1.84246122076305,-7.69345901287549,
8.79116140926346));
#217339=CARTESIAN_POINT('Ctrl Pts',(-1.82820648524223,-7.69685880688339,
8.7917480200298));
#217340=CARTESIAN_POINT('Ctrl Pts',(-1.82109292155917,-7.69854499351601,
8.79204035245549));
#217341=CARTESIAN_POINT('Ctrl Pts',(-1.80114541562527,-7.70324412044258,
8.79285896504975));
#217342=CARTESIAN_POINT('Ctrl Pts',(-1.78830623842805,-7.70623485153833,
8.7933845513515));
#217343=CARTESIAN_POINT('Ctrl Pts',(-1.73604959542368,-7.71826977568501,
8.79551842901275));
#217344=CARTESIAN_POINT('Ctrl Pts',(-1.69657021646568,-7.72704381304776,
8.79711827669385));
#217345=CARTESIAN_POINT('Ctrl Pts',(-1.08097459703194,-7.85891057407248,
8.82187726823715));
#217346=CARTESIAN_POINT('Ctrl Pts',(-0.492939563608088,-7.91758073475562,
8.8427895216776));
#217347=CARTESIAN_POINT('Ctrl Pts',(0.498700126488024,-7.90551948604952,
8.87683658463479));
#217348=CARTESIAN_POINT('Ctrl Pts',(0.900212089266585,-7.86991355186963,
8.89034209444207));
#217349=CARTESIAN_POINT('Ctrl Pts',(1.60335781328868,-7.75302857782367,
8.91555906642412));
#217350=CARTESIAN_POINT('Ctrl Pts',(1.90617520529572,-7.68418315985583,
8.92696273711215));
#217351=CARTESIAN_POINT('Ctrl Pts',(2.21931325853927,-7.59334045926619,
8.93999892752131));
#217352=CARTESIAN_POINT('Ctrl Pts',(2.23447519837941,-7.58889262350306,
8.94063325872745));
#217353=CARTESIAN_POINT('Ctrl Pts',(2.2553982569527,-7.58268659400234,8.941513059558));
#217354=CARTESIAN_POINT('Ctrl Pts',(2.2611709305597,-7.58096717462512,8.94175626436494));
#217355=CARTESIAN_POINT('Ctrl Pts',(2.27090358374208,-7.57805615014655,
8.94216710155076));
#217356=CARTESIAN_POINT('Ctrl Pts',(2.27486461068765,-7.57686802738072,
8.94233452824279));
#217357=CARTESIAN_POINT('Ctrl Pts',(2.28269272720289,-7.57451326678125,
8.94266585464807));
#217358=CARTESIAN_POINT('Ctrl Pts',(2.28655985908946,-7.57334677181498,
8.94282974583779));
#217359=CARTESIAN_POINT('Ctrl Pts',(2.29506930743921,-7.57077284073997,
8.94319085555833));
#217360=CARTESIAN_POINT('Ctrl Pts',(2.29971122277883,-7.56936409638567,
8.94338815246656));
#217361=CARTESIAN_POINT('Ctrl Pts',(2.31585486381004,-7.56444854813234,
8.94407540219058));
#217362=CARTESIAN_POINT('Ctrl Pts',(2.32734983343493,-7.56091980761333,
8.94456668127522));
#217363=CARTESIAN_POINT('Ctrl Pts',(2.45647386626368,-7.52095878618009,
8.9501073689217));
#217364=CARTESIAN_POINT('Ctrl Pts',(2.57323747096091,-7.48181327451927,
8.95532581378026));
#217365=CARTESIAN_POINT('Ctrl Pts',(2.99794759519844,-7.32830990784588,
8.9749363266347));
#217366=CARTESIAN_POINT('Ctrl Pts',(3.29959143545574,-7.1975332729554,8.99008272993728));
#217367=CARTESIAN_POINT('Ctrl Pts',(3.91938148001642,-6.88165767235397,
9.02251466157164));
#217368=CARTESIAN_POINT('Ctrl Pts',(4.23455881289234,-6.69233105866938,
9.03979261809929));
#217369=CARTESIAN_POINT('Ctrl Pts',(4.72427383600306,-6.34966685206859,
9.06703758044295));
#217370=CARTESIAN_POINT('Ctrl Pts',(4.90724289830053,-6.20934865775254,
9.07732509576453));
#217371=CARTESIAN_POINT('Ctrl Pts',(5.20430401176946,-5.96018988961546,
9.09410929961352));
#217372=CARTESIAN_POINT('Ctrl Pts',(5.32173892719841,-5.8555736394445,9.10076921216874));
#217373=CARTESIAN_POINT('Ctrl Pts',(5.49568602894485,-5.69105517716831,
9.11066798351163));
#217374=CARTESIAN_POINT('Ctrl Pts',(5.55450678978714,-5.6336603436928,9.11402177596556));
#217375=CARTESIAN_POINT('Ctrl Pts',(5.62280848796092,-5.56490456551562,
9.11792517107459));
#217376=CARTESIAN_POINT('Ctrl Pts',(5.63316383217025,-5.55442196442253,
9.11851722446226));
#217377=CARTESIAN_POINT('Ctrl Pts',(5.64899794935275,-5.53830343569123,
9.11942292278793));
#217378=CARTESIAN_POINT('Ctrl Pts',(5.65449768162376,-5.53268820254622,
9.11973757794163));
#217379=CARTESIAN_POINT('Ctrl Pts',(5.66407845598095,-5.52287701339287,
9.12028585489125));
#217380=CARTESIAN_POINT('Ctrl Pts',(5.6681632216031,-5.51868471232471,9.12051965553829));
#217381=CARTESIAN_POINT('Ctrl Pts',(5.6766979757651,-5.50990580057034,9.12100825188447));
#217382=CARTESIAN_POINT('Ctrl Pts',(5.68114706824986,-5.5053183221685,9.12126300462157));
#217383=CARTESIAN_POINT('Ctrl Pts',(5.69344541874112,-5.49260665592771,
9.12196734778831));
#217384=CARTESIAN_POINT('Ctrl Pts',(5.70128285663692,-5.48447102308259,
9.12241637344519));
#217385=CARTESIAN_POINT('Ctrl Pts',(5.73201339647766,-5.45243420681422,
9.12417767104035));
#217386=CARTESIAN_POINT('Ctrl Pts',(5.75477400728524,-5.42840607537118,
9.12548364528953));
#217387=CARTESIAN_POINT('Ctrl Pts',(6.12187832434344,-5.03595420531949,
9.14657409822095));
#217388=CARTESIAN_POINT('Ctrl Pts',(6.43038966284449,-4.63555747130408,
9.16456425362355));
#217389=CARTESIAN_POINT('Ctrl Pts',(7.08646316922651,-3.59127621927101,
9.2067079651504));
#217390=CARTESIAN_POINT('Ctrl Pts',(7.38699512295196,-2.92355531425107,
9.22973078807729));
#217391=CARTESIAN_POINT('Ctrl Pts',(7.6038522267635,-2.18338470808729,9.25998610153256));
#217392=CARTESIAN_POINT('Ctrl Pts',(7.61550460888024,-2.14238814548624,
9.26167744732356));
#217393=CARTESIAN_POINT('Ctrl Pts',(7.62891588902088,-2.09371089685046,
9.26370627919391));
#217394=CARTESIAN_POINT('Ctrl Pts',(7.63099537570652,-2.08611901300698,
9.26402328938701));
#217395=CARTESIAN_POINT('Ctrl Pts',(7.63436342753745,-2.0737503548789,9.2645407001706));
#217396=CARTESIAN_POINT('Ctrl Pts',(7.63565885283248,-2.06897543750131,
9.26474067426841));
#217397=CARTESIAN_POINT('Ctrl Pts',(7.63795803150873,-2.06046913099128,
9.26509732101109));
#217398=CARTESIAN_POINT('Ctrl Pts',(7.63896353359213,-2.0567382096906,9.26525388610885));
#217399=CARTESIAN_POINT('Ctrl Pts',(7.64107401745293,-2.04888434994692,
9.26558375412748));
#217400=CARTESIAN_POINT('Ctrl Pts',(7.64217839629818,-2.04476125224057,
9.26575709378419));
#217401=CARTESIAN_POINT('Ctrl Pts',(7.6450777929925,-2.0339014588578,9.26621408614928));
#217402=CARTESIAN_POINT('Ctrl Pts',(7.64686723993238,-2.02716329374114,
9.26649807578861));
#217403=CARTESIAN_POINT('Ctrl Pts',(7.65482219121028,-1.99704849768258,
9.26776924458624));
#217404=CARTESIAN_POINT('Ctrl Pts',(7.66088936497753,-1.97364626868803,
9.26876228375342));
#217405=CARTESIAN_POINT('Ctrl Pts',(7.70474513229622,-1.80123695377259,
9.2761146287747));
#217406=CARTESIAN_POINT('Ctrl Pts',(7.73828859033302,-1.6511924094569,9.28271278229449));
#217407=CARTESIAN_POINT('Ctrl Pts',(7.79736812662115,-1.34531744521089,
9.29643359665464));
#217408=CARTESIAN_POINT('Ctrl Pts',(7.82265325323392,-1.18950447270505,
9.30356245239264));
#217409=CARTESIAN_POINT('Ctrl Pts',(7.89758369537892,-0.620605514863718,
9.32985966080013));
#217410=CARTESIAN_POINT('Ctrl Pts',(7.91928986533777,-0.2045248942233,9.349568273859));
#217411=CARTESIAN_POINT('Ctrl Pts',(7.89264723839935,0.792453647545537,
9.39578604552791));
#217412=CARTESIAN_POINT('Ctrl Pts',(7.81311147433822,1.37016149131502,9.42163842289761));
#217413=CARTESIAN_POINT('Ctrl Pts',(7.66160148988842,1.97110300776564,9.44690877800006));
#217414=CARTESIAN_POINT('Ctrl Pts',(7.6519801942013,2.00812938300014,9.44845986946134));
#217415=CARTESIAN_POINT('Ctrl Pts',(7.6388787103723,2.05708711986375,9.45050317920551));
#217416=CARTESIAN_POINT('Ctrl Pts',(7.6356385296699,2.06908182935054,9.45100318645236));
#217417=CARTESIAN_POINT('Ctrl Pts',(7.63032679423929,2.08856274649633,9.45181428706856));
#217418=CARTESIAN_POINT('Ctrl Pts',(7.62827245397738,2.09605360171813,9.45212593929718));
#217419=CARTESIAN_POINT('Ctrl Pts',(7.6243394656068,2.11031231005066,9.45271872080262));
#217420=CARTESIAN_POINT('Ctrl Pts',(7.62246283093478,2.11708070798162,9.45299991515602));
#217421=CARTESIAN_POINT('Ctrl Pts',(7.61820010234857,2.13237581077174,9.45363492606483));
#217422=CARTESIAN_POINT('Ctrl Pts',(7.61580870054306,2.14090103348527,9.45398856976115));
#217423=CARTESIAN_POINT('Ctrl Pts',(7.60857340135766,2.16652896612847,9.45505077443395));
#217424=CARTESIAN_POINT('Ctrl Pts',(7.60368615428648,2.18361943509198,9.4557579263014));
#217425=CARTESIAN_POINT('Ctrl Pts',(7.56250933965201,2.32579824513729,9.46163107417658));
#217426=CARTESIAN_POINT('Ctrl Pts',(7.52319240390765,2.44999244817969,9.46669771973346));
#217427=CARTESIAN_POINT('Ctrl Pts',(7.38863419824306,2.84118665214395,9.48249621903437));
#217428=CARTESIAN_POINT('Ctrl Pts',(7.28210197882458,3.10407183805344,9.49286343175283));
#217429=CARTESIAN_POINT('Ctrl Pts',(7.07471645379601,3.54601451104537,9.51024887179538));
#217430=CARTESIAN_POINT('Ctrl Pts',(6.98058610601986,3.72790180133291,9.5173934847611));
#217431=CARTESIAN_POINT('Ctrl Pts',(6.57523560630917,4.44184372847885,9.54588894983493));
#217432=CARTESIAN_POINT('Ctrl Pts',(6.20937960948001,4.94037819754794,9.56679781001265));
#217433=CARTESIAN_POINT('Ctrl Pts',(5.76071160169085,5.42216672155814,9.59278744616902));
#217434=CARTESIAN_POINT('Ctrl Pts',(5.73180223121717,5.45271796575667,9.59446081963003));
#217435=CARTESIAN_POINT('Ctrl Pts',(5.69381543785865,5.49222625818714,9.59665663435051));
#217436=CARTESIAN_POINT('Ctrl Pts',(5.68495775314304,5.50139426457833,9.5971684412104));
#217437=CARTESIAN_POINT('Ctrl Pts',(5.67076897038288,5.51600927976661,9.59798790558535));
#217438=CARTESIAN_POINT('Ctrl Pts',(5.66545207416039,5.52147008367058,9.5982948950159));
#217439=CARTESIAN_POINT('Ctrl Pts',(5.65586163453775,5.53129166203543,9.59884846903116));
#217440=CARTESIAN_POINT('Ctrl Pts',(5.6515909145629,5.53565519281628,9.59909492306821));
#217441=CARTESIAN_POINT('Ctrl Pts',(5.64156153664911,5.54587882406283,9.59967355339112));
#217442=CARTESIAN_POINT('Ctrl Pts',(5.63579879814406,5.55173490084542,9.60000591557709));
#217443=CARTESIAN_POINT('Ctrl Pts',(5.61916621858536,5.56858429176758,9.60096484867161));
#217444=CARTESIAN_POINT('Ctrl Pts',(5.60827328947805,5.57955470567329,9.60159245127284));
#217445=CARTESIAN_POINT('Ctrl Pts',(5.53470338399272,5.6532148248611,9.60582808725772));
#217446=CARTESIAN_POINT('Ctrl Pts',(5.47100971574863,5.71487808433386,9.6094797680974));
#217447=CARTESIAN_POINT('Ctrl Pts',(5.25727196141003,5.91495390594267,9.62165454972014));
#217448=CARTESIAN_POINT('Ctrl Pts',(5.10290932243144,6.04862799950733,9.6303200133286));
#217449=CARTESIAN_POINT('Ctrl Pts',(4.42223601261422,6.5934544330793,9.66762994998348));
#217450=CARTESIAN_POINT('Ctrl Pts',(3.85013693435381,6.94307877578777,9.69649600156466));
#217451=CARTESIAN_POINT('Ctrl Pts',(3.14231015407456,7.26095700003366,9.72889892547154));
#217452=CARTESIAN_POINT('Ctrl Pts',(3.04278682675111,7.30322246066215,9.73339336601753));
#217453=CARTESIAN_POINT('Ctrl Pts',(2.91367789026081,7.35495488883782,9.73915505654857));
#217454=CARTESIAN_POINT('Ctrl Pts',(2.88486048458015,7.36630574005381,9.74043674199395));
#217455=CARTESIAN_POINT('Ctrl Pts',(2.84214898383273,7.38284024120973,9.74233030508017));
#217456=CARTESIAN_POINT('Ctrl Pts',(2.82830581752351,7.38815451088679,9.74294308565485));
#217457=CARTESIAN_POINT('Ctrl Pts',(2.81206961885348,7.39433512453511,9.74366072600313));
#217458=CARTESIAN_POINT('Ctrl Pts',(2.80969101912654,7.39523926943917,9.74376583329986));
#217459=CARTESIAN_POINT('Ctrl Pts',(2.53833544134911,7.49823617482062,9.7557536423545));
#217460=CARTESIAN_POINT('Ctrl Pts',(2.26398198238071,7.58558402445757,9.76755953217075));
#217461=CARTESIAN_POINT('Ctrl Pts',(1.95635801204336,7.66534339291514,9.7804277693657));
#217462=CARTESIAN_POINT('Ctrl Pts',(1.92719472409004,7.67272744901626,9.78164411088452));
#217463=CARTESIAN_POINT('Ctrl Pts',(1.87252058520879,7.6862393903802,9.78391776903705));
#217464=CARTESIAN_POINT('Ctrl Pts',(1.84702000553859,7.69240706238575,9.78497551309459));
#217465=CARTESIAN_POINT('Ctrl Pts',(1.80340324981471,7.70272699311088,9.78678009964377));
#217466=CARTESIAN_POINT('Ctrl Pts',(1.78530228686225,7.70694246498242,9.78752765334314));
#217467=CARTESIAN_POINT('Ctrl Pts',(1.74817532058392,7.71545102117662,9.78905821625662));
#217468=CARTESIAN_POINT('Ctrl Pts',(1.72914795375515,7.71973761006485,9.78984114592412));
#217469=CARTESIAN_POINT('Ctrl Pts',(1.68516052862311,7.72947654858285,9.79164774327979));
#217470=CARTESIAN_POINT('Ctrl Pts',(1.66018949870662,7.73487844484264,9.79267081545002));
#217471=CARTESIAN_POINT('Ctrl Pts',(1.58133026134982,7.7515383148923,9.79589391045869));
#217472=CARTESIAN_POINT('Ctrl Pts',(1.52735028119158,7.76235485013393,9.79808867987738));
#217473=CARTESIAN_POINT('Ctrl Pts',(1.15567060102562,7.83280500539108,9.81312519086709));
#217474=CARTESIAN_POINT('Ctrl Pts',(0.834683732020157,7.87348213233303,
9.82571745476222));
#217475=CARTESIAN_POINT('Ctrl Pts',(-0.0336831296969686,7.9298121911959,
9.85927095986215));
#217476=CARTESIAN_POINT('Ctrl Pts',(-0.581643712634404,7.908520471578,9.87984168800481));
#217477=CARTESIAN_POINT('Ctrl Pts',(-1.16169251647472,7.82533833442156,
9.90316819721011));
#217478=CARTESIAN_POINT('Ctrl Pts',(-1.20035142683879,7.81950164489381,
9.90473083611415));
#217479=CARTESIAN_POINT('Ctrl Pts',(-1.2522571329176,7.81127097136814,9.90684093613767));
#217480=CARTESIAN_POINT('Ctrl Pts',(-1.26554353129027,7.80912938064962,
9.90738211366105));
#217481=CARTESIAN_POINT('Ctrl Pts',(-1.28832949067893,7.80539690823245,
9.90831198862464));
#217482=CARTESIAN_POINT('Ctrl Pts',(-1.2978317463643,7.80382255879118,9.90870029426351));
#217483=CARTESIAN_POINT('Ctrl Pts',(-1.31635524007655,7.80071878762672,
9.90945826015159));
#217484=CARTESIAN_POINT('Ctrl Pts',(-1.32537674897428,7.79919106026147,
9.90982788088646));
#217485=CARTESIAN_POINT('Ctrl Pts',(-1.34702906569414,7.79548574338497,
9.91071610593231));
#217486=CARTESIAN_POINT('Ctrl Pts',(-1.35965725901217,7.79329310469952,
9.91123504670571));
#217487=CARTESIAN_POINT('Ctrl Pts',(-1.39784794995567,7.78656638753121,
9.91280712745014));
#217488=CARTESIAN_POINT('Ctrl Pts',(-1.42339343266007,7.78193717036247,
9.91386231549853));
#217489=CARTESIAN_POINT('Ctrl Pts',(-1.70902205249713,7.72872358544662,
9.9256994715271));
#217490=CARTESIAN_POINT('Ctrl Pts',(-1.96652822247709,7.66724755259749,
9.93672809268633));
#217491=CARTESIAN_POINT('Ctrl Pts',(-2.78182758172099,7.42882468809274,
9.97234953166494));
#217492=CARTESIAN_POINT('Ctrl Pts',(-3.32328334586225,7.20290471528132,
9.99697633622257));
#217493=CARTESIAN_POINT('Ctrl Pts',(-3.92288690088566,6.87058973624737,
10.0249691290664));
#217494=CARTESIAN_POINT('Ctrl Pts',(-4.00995457972157,6.82013999539848,
10.029057264785));
#217495=CARTESIAN_POINT('Ctrl Pts',(-4.12866891743919,6.74829377258149,
10.0346680884985));
#217496=CARTESIAN_POINT('Ctrl Pts',(-4.16115777523213,6.7283089894796,10.0362075068509));
#217497=CARTESIAN_POINT('Ctrl Pts',(-4.21298763673543,6.69590802686731,
10.0386699752365));
#217498=CARTESIAN_POINT('Ctrl Pts',(-4.23242120734334,6.68364121261004,
10.0395947820479));
#217499=CARTESIAN_POINT('Ctrl Pts',(-4.27252132323462,6.65808427841552,
10.0415063061666));
#217500=CARTESIAN_POINT('Ctrl Pts',(-4.29317996488126,6.64478220181507,
10.0424928710688));
#217501=CARTESIAN_POINT('Ctrl Pts',(-4.34147536410036,6.61336560038426,
10.0448036249742));
#217502=CARTESIAN_POINT('Ctrl Pts',(-4.36906129055225,6.59517371653357,
10.0461268964245));
#217503=CARTESIAN_POINT('Ctrl Pts',(-4.45972194159991,6.53456796249722,
10.0504876425986));
#217504=CARTESIAN_POINT('Ctrl Pts',(-4.52229963154844,6.49141775047207,
10.0535166375223));
#217505=CARTESIAN_POINT('Ctrl Pts',(-5.16806420843812,6.03226266903351,
10.0850011382433));
#217506=CARTESIAN_POINT('Ctrl Pts',(-5.69283409008161,5.53975028330331,
10.1124983806052));
#217507=CARTESIAN_POINT('Ctrl Pts',(-6.41964869114742,4.64363384768455,
10.1554422904928));
#217508=CARTESIAN_POINT('Ctrl Pts',(-6.66650918132427,4.28168792692901,
10.1714367569983));
#217509=CARTESIAN_POINT('Ctrl Pts',(-6.89831648685216,3.8727536663235,10.1894478531826));
#217510=CARTESIAN_POINT('Ctrl Pts',(-6.91427301630708,3.84419301607496,
10.1907058099702));
#217511=CARTESIAN_POINT('Ctrl Pts',(-6.98701317872356,3.7120770274598,10.1965280651845));
#217512=CARTESIAN_POINT('Ctrl Pts',(-7.04164921538346,3.60735967999222,
10.2011516576573));
#217513=CARTESIAN_POINT('Ctrl Pts',(-7.10127255207553,3.48656351853141,
10.2065326914923));
#217514=CARTESIAN_POINT('Ctrl Pts',(-7.10857907143045,3.47164235021424,
10.2071981955016));
#217515=CARTESIAN_POINT('Ctrl Pts',(-7.11925442818967,3.44966643359212,
10.2081796956698));
#217516=CARTESIAN_POINT('Ctrl Pts',(-7.12265992404065,3.44262947792414,
10.2084941861709));
#217517=CARTESIAN_POINT('Ctrl Pts',(-7.12870009848692,3.43010101950255,
10.2090544763789));
#217518=CARTESIAN_POINT('Ctrl Pts',(-7.13133887937239,3.42461149408941,
10.2093001043395));
#217519=CARTESIAN_POINT('Ctrl Pts',(-7.13682958475998,3.41315516997417,
10.2098129940607));
#217520=CARTESIAN_POINT('Ctrl Pts',(-7.13968037130188,3.40718783332111,
10.2100803037653));
#217521=CARTESIAN_POINT('Ctrl Pts',(-7.14706152367414,3.39168748258723,
10.2107750732467));
#217522=CARTESIAN_POINT('Ctrl Pts',(-7.15158029105656,3.38214898280205,
10.2112030313548));
#217523=CARTESIAN_POINT('Ctrl Pts',(-7.17077326217329,3.34142480128834,
10.2130320570353));
#217524=CARTESIAN_POINT('Ctrl Pts',(-7.18526252518813,3.3101527565099,10.2144412536191));
#217525=CARTESIAN_POINT('Ctrl Pts',(-7.28015388339508,3.10179073269101,
10.2238675213317));
#217526=CARTESIAN_POINT('Ctrl Pts',(-7.35419520899954,2.92190698075219,
10.2322134055462));
#217527=CARTESIAN_POINT('Ctrl Pts',(-7.74520097764315,1.86263999763756,
10.2820008873398));
#217528=CARTESIAN_POINT('Ctrl Pts',(-7.91095464617904,0.935317427441046,
10.327041855684));
#217529=CARTESIAN_POINT('Ctrl Pts',(-7.91099999069558,0.000383685446136151,
10.3667112445445));
#217530=CARTESIAN_POINT('',(-7.91258408968956,-0.00269315930910046,12.3576684917633));
#217531=CARTESIAN_POINT('Ctrl Pts',(-7.911,-6.54698517621455E-12,10.3576684917633));
#217532=CARTESIAN_POINT('Ctrl Pts',(-7.91099999999818,-2.20167589667329,
10.446255927496));
#217533=CARTESIAN_POINT('Ctrl Pts',(-6.9421457667201,-4.38610418339253,
10.5348433632287));
#217534=CARTESIAN_POINT('Ctrl Pts',(-3.67820201487687,-7.34180684107932,
10.7120182346942));
#217535=CARTESIAN_POINT('Ctrl Pts',(-1.40868175871086,-8.0899266657145,
10.8006056704269));
#217536=CARTESIAN_POINT('Ctrl Pts',(2.97309270521891,-7.65454228025016,
10.9777805418924));
#217537=CARTESIAN_POINT('Ctrl Pts',(5.05102072676122,-6.47444880833819,
11.0663679776251));
#217538=CARTESIAN_POINT('Ctrl Pts',(7.66951518848105,-2.93425195367096,
11.2435428490905));
#217539=CARTESIAN_POINT('Ctrl Pts',(8.18956872247118,-0.601881960092681,
11.3321302848233));
#217540=CARTESIAN_POINT('Ctrl Pts',(7.3230668976105,3.71537198233024,11.5093051562887));
#217541=CARTESIAN_POINT('Ctrl Pts',(5.94329958849758,5.66643518936975,11.5978925920214));
#217542=CARTESIAN_POINT('Ctrl Pts',(2.16154501637234,7.92205913233164,11.7750674634869));
#217543=CARTESIAN_POINT('Ctrl Pts',(-0.210816529306694,8.20894963712986,
11.8636548992196));
#217544=CARTESIAN_POINT('Ctrl Pts',(-4.42123908576965,6.91982244717493,
12.0408297706851));
#217545=CARTESIAN_POINT('Ctrl Pts',(-6.22631625634594,5.35390358803047,
12.1294172064178));
#217546=CARTESIAN_POINT('Ctrl Pts',(-7.65317280859671,2.31334857513923,
12.2645592586881));
#217547=CARTESIAN_POINT('Ctrl Pts',(-7.91100000000096,1.15702837835884,
12.3111138752257));
#217548=CARTESIAN_POINT('Ctrl Pts',(-7.911,-6.53810339201755E-12,12.3576684917633));
#217549=CARTESIAN_POINT('',(-7.91331685262984,-0.000560519916223401,14.3576684617817));
#217550=CARTESIAN_POINT('Ctrl Pts',(-7.91258408968956,-0.00269315930910046,
12.3576684917633));
#217551=CARTESIAN_POINT('Ctrl Pts',(-7.91593504939377,-0.776264288801357,
12.3886864088733));
#217552=CARTESIAN_POINT('Ctrl Pts',(-7.43681856913235,-4.19026845229773,
12.5256739031998));
#217553=CARTESIAN_POINT('Ctrl Pts',(-3.65584480504754,-7.92457769675913,
12.7156461861345));
#217554=CARTESIAN_POINT('Ctrl Pts',(1.79759080058233,-8.02852789826421,
12.9275853405675));
#217555=CARTESIAN_POINT('Ctrl Pts',(6.66378542679534,-5.62439576614873,
13.1395244950005));
#217556=CARTESIAN_POINT('Ctrl Pts',(9.26557616308506,1.35890735276843,13.4044484380419));
#217557=CARTESIAN_POINT('Ctrl Pts',(3.84357001655874,8.53192481528771,13.7223571696913));
#217558=CARTESIAN_POINT('Ctrl Pts',(-3.5690748421245,7.95640288263857,13.9872811127326));
#217559=CARTESIAN_POINT('Ctrl Pts',(-7.23560627100123,3.93118237953513,
14.1990515434295));
#217560=CARTESIAN_POINT('Ctrl Pts',(-7.91285669218149,1.3077251098878,14.3048523969097));
#217561=CARTESIAN_POINT('Ctrl Pts',(-7.91331685262984,-0.000560519916223401,
14.3576684617817));
#217562=CARTESIAN_POINT('',(-7.91099988478435,0.00135016367355217,18.3664967938599));
#217563=CARTESIAN_POINT('Ctrl Pts',(-7.91099997617816,-0.000613929265750893,
14.3563333568247));
#217564=CARTESIAN_POINT('Ctrl Pts',(-7.91099935780322,-0.00858221555712144,
14.3566531921185));
#217565=CARTESIAN_POINT('Ctrl Pts',(-7.91098670047397,-0.0165504911307802,
14.3569733132972));
#217566=CARTESIAN_POINT('Ctrl Pts',(-7.91092601335387,-0.0361311553618632,
14.3577606644224));
#217567=CARTESIAN_POINT('Ctrl Pts',(-7.91086445415868,-0.047743438954302,
14.3582282105699));
#217568=CARTESIAN_POINT('Ctrl Pts',(-7.91070448295947,-0.069064059512712,
14.3590877341926));
#217569=CARTESIAN_POINT('Ctrl Pts',(-7.91061376652499,-0.0787724397538128,
14.3594795347212));
#217570=CARTESIAN_POINT('Ctrl Pts',(-7.91039648001536,-0.0981986849055518,
14.3602643315667));
#217571=CARTESIAN_POINT('Ctrl Pts',(-7.91026987364833,-0.107916533444963,
14.3606573280512));
#217572=CARTESIAN_POINT('Ctrl Pts',(-7.9098819762533,-0.134000099461685,
14.3617132350183));
#217573=CARTESIAN_POINT('Ctrl Pts',(-7.9095878016966,-0.150365253041726,
14.3623768544412));
#217574=CARTESIAN_POINT('Ctrl Pts',(-7.90832284448457,-0.210371813784779,
14.3648141611594));
#217575=CARTESIAN_POINT('Ctrl Pts',(-7.90704164589483,-0.254005656347762,
14.3665941987198));
#217576=CARTESIAN_POINT('Ctrl Pts',(-7.8880309044882,-0.758959250380348,
14.387274724489));
#217577=CARTESIAN_POINT('Ctrl Pts',(-7.83031338981521,-1.21788090148529,
14.4068061599072));
#217578=CARTESIAN_POINT('Ctrl Pts',(-7.6498456347303,-2.05396554232061,
14.4426578333511));
#217579=CARTESIAN_POINT('Ctrl Pts',(-7.53816870490578,-2.43206548002689,
14.4589848871743));
#217580=CARTESIAN_POINT('Ctrl Pts',(-7.38111865470644,-2.84701684970282,
14.4770303286938));
#217581=CARTESIAN_POINT('Ctrl Pts',(-7.3629898367631,-2.89357879468404,
14.4790575499912));
#217582=CARTESIAN_POINT('Ctrl Pts',(-7.33274298028933,-2.9691394119104,
14.482351778737));
#217583=CARTESIAN_POINT('Ctrl Pts',(-7.32089115934277,-2.99824300302658,
14.4836217013238));
#217584=CARTESIAN_POINT('Ctrl Pts',(-7.29972140117194,-3.04935395798992,
14.4858540321543));
#217585=CARTESIAN_POINT('Ctrl Pts',(-7.29047657110277,-3.071391128832,14.4868172319709));
#217586=CARTESIAN_POINT('Ctrl Pts',(-7.27155223407225,-3.11593474258506,
14.488765678678));
#217587=CARTESIAN_POINT('Ctrl Pts',(-7.26186774619344,-3.13843879248177,
14.489750859617));
#217588=CARTESIAN_POINT('Ctrl Pts',(-7.24286345297947,-3.18204053268,14.4916613357138));
#217589=CARTESIAN_POINT('Ctrl Pts',(-7.23355561343504,-3.20314316587706,
14.4925867487731));
#217590=CARTESIAN_POINT('Ctrl Pts',(-7.21103171141795,-3.25361023657898,
14.4948018678875));
#217591=CARTESIAN_POINT('Ctrl Pts',(-7.19772837024615,-3.28293530736774,
14.4960906347056));
#217592=CARTESIAN_POINT('Ctrl Pts',(-7.14783907237772,-3.39114717316062,
14.5008529398403));
#217593=CARTESIAN_POINT('Ctrl Pts',(-7.11013207420096,-3.4695107164351,
14.5043147400745));
#217594=CARTESIAN_POINT('Ctrl Pts',(-6.78352051358068,-4.12058540043313,
14.533220115032));
#217595=CARTESIAN_POINT('Ctrl Pts',(-6.4272157762679,-4.65686164785477,
14.5579956243139));
#217596=CARTESIAN_POINT('Ctrl Pts',(-5.84158268048582,-5.34106383559166,
14.5916886329292));
#217597=CARTESIAN_POINT('Ctrl Pts',(-5.66353512370756,-5.52950463140723,
14.6012702853086));
#217598=CARTESIAN_POINT('Ctrl Pts',(-5.39514515349256,-5.78697319181438,
14.6150946386616));
#217599=CARTESIAN_POINT('Ctrl Pts',(-5.31206715749001,-5.86332603058683,
14.6192972339497));
#217600=CARTESIAN_POINT('Ctrl Pts',(-5.08087514394196,-6.06685501192869,
14.6308463942725));
#217601=CARTESIAN_POINT('Ctrl Pts',(-4.92964530888855,-6.19036467326444,
14.6382427404057));
#217602=CARTESIAN_POINT('Ctrl Pts',(-4.72463625103934,-6.34551549907018,
14.6482424482844));
#217603=CARTESIAN_POINT('Ctrl Pts',(-4.67482835626658,-6.38229851091883,
14.6506701163304));
#217604=CARTESIAN_POINT('Ctrl Pts',(-4.60446564743442,-6.43299561740641,
14.6541037678996));
#217605=CARTESIAN_POINT('Ctrl Pts',(-4.58426876575193,-6.44740384804727,
14.6550898334904));
#217606=CARTESIAN_POINT('Ctrl Pts',(-4.55358742627076,-6.46907452462936,
14.6565889659631));
#217607=CARTESIAN_POINT('Ctrl Pts',(-4.5431525378649,-6.47640708026922,
14.6570990356698));
#217608=CARTESIAN_POINT('Ctrl Pts',(-4.52614570638438,-6.48829638645187,
14.6579307558024));
#217609=CARTESIAN_POINT('Ctrl Pts',(-4.51958448315963,-6.49286847648109,
14.6582517307959));
#217610=CARTESIAN_POINT('Ctrl Pts',(-4.50688230306024,-6.50169121735234,
14.6588733313664));
#217611=CARTESIAN_POINT('Ctrl Pts',(-4.50074223523536,-6.50594313769646,
14.6591738995724));
#217612=CARTESIAN_POINT('Ctrl Pts',(-4.49007953178265,-6.51330460840188,
14.6596960387613));
#217613=CARTESIAN_POINT('Ctrl Pts',(-4.48555965819528,-6.51641816308199,
14.6599174270253));
#217614=CARTESIAN_POINT('Ctrl Pts',(-4.47615573060957,-6.52288172144017,
14.6603781645653));
#217615=CARTESIAN_POINT('Ctrl Pts',(-4.47127114907023,-6.52623094808969,
14.6606175494134));
#217616=CARTESIAN_POINT('Ctrl Pts',(-4.45935524150135,-6.53438170942558,
14.6612017058356));
#217617=CARTESIAN_POINT('Ctrl Pts',(-4.45231992534214,-6.53917737762496,
14.6615467510764));
#217618=CARTESIAN_POINT('Ctrl Pts',(-4.425636199398,-6.55730348480021,14.662856069622));
#217619=CARTESIAN_POINT('Ctrl Pts',(-4.40593567894893,-6.57055671441549,
14.6638240112931));
#217620=CARTESIAN_POINT('Ctrl Pts',(-4.1492163636711,-6.74158706222824,
14.6764576097869));
#217621=CARTESIAN_POINT('Ctrl Pts',(-3.90395243243347,-6.88651522203738,
14.688847716405));
#217622=CARTESIAN_POINT('Ctrl Pts',(-3.56053577122835,-7.06519708512882,
14.7062216485793));
#217623=CARTESIAN_POINT('Ctrl Pts',(-3.46870868321951,-7.11073021656714,
14.7108675043172));
#217624=CARTESIAN_POINT('Ctrl Pts',(-3.13091958769764,-7.27012496742601,
14.7279041342482));
#217625=CARTESIAN_POINT('Ctrl Pts',(-2.88003456556343,-7.37311156524941,
14.7404508563278));
#217626=CARTESIAN_POINT('Ctrl Pts',(-2.54472868876093,-7.49102144994287,
14.7567850368745));
#217627=CARTESIAN_POINT('Ctrl Pts',(-2.46465267895177,-7.51774792305902,
14.7606549118307));
#217628=CARTESIAN_POINT('Ctrl Pts',(-2.33620160230442,-7.55834725622247,
14.7668051339396));
#217629=CARTESIAN_POINT('Ctrl Pts',(-2.28809569355128,-7.57304887933787,
14.7690957269753));
#217630=CARTESIAN_POINT('Ctrl Pts',(-2.09890582629606,-7.62889983071797,
14.7780506426993));
#217631=CARTESIAN_POINT('Ctrl Pts',(-1.95682394954797,-7.66657422640383,
14.7846591121127));
#217632=CARTESIAN_POINT('Ctrl Pts',(-1.59098126353183,-7.7527471952586,
14.8013317641483));
#217633=CARTESIAN_POINT('Ctrl Pts',(-1.36600895248158,-7.79553335477924,
14.8112584957362));
#217634=CARTESIAN_POINT('Ctrl Pts',(-0.993698764179286,-7.84972534608339,
14.8271094233152));
#217635=CARTESIAN_POINT('Ctrl Pts',(-0.847342739479785,-7.86686967410458,
14.8331970902977));
#217636=CARTESIAN_POINT('Ctrl Pts',(-0.681702320304589,-7.88159643953867,
14.8399301348295));
#217637=CARTESIAN_POINT('Ctrl Pts',(-0.662810557941004,-7.88320763774275,
14.8406957762589));
#217638=CARTESIAN_POINT('Ctrl Pts',(-0.63446610460771,-7.88552240521146,
14.8418411223026));
#217639=CARTESIAN_POINT('Ctrl Pts',(-0.625017706542182,-7.88627692312939,
14.8422223493299));
#217640=CARTESIAN_POINT('Ctrl Pts',(-0.60878270693865,-7.88754403701043,
14.8428764383968));
#217641=CARTESIAN_POINT('Ctrl Pts',(-0.601996768830469,-7.88806485841931,
14.8431495460385));
#217642=CARTESIAN_POINT('Ctrl Pts',(-0.588036471191368,-7.88911819300989,
14.8437107997456));
#217643=CARTESIAN_POINT('Ctrl Pts',(-0.580862038931829,-7.889649678332,
14.8439989148573));
#217644=CARTESIAN_POINT('Ctrl Pts',(-0.561591662599399,-7.89105080912434,
14.8447719230641));
#217645=CARTESIAN_POINT('Ctrl Pts',(-0.549494406323064,-7.8919024301312,
14.8452562770622));
#217646=CARTESIAN_POINT('Ctrl Pts',(-0.50539440390847,-7.89490508462575,
14.8470186635983));
#217647=CARTESIAN_POINT('Ctrl Pts',(-0.47338042335452,-7.89688931181057,
14.8482917096749));
#217648=CARTESIAN_POINT('Ctrl Pts',(0.0441231675576322,-7.92580589618363,
14.8687700964924));
#217649=CARTESIAN_POINT('Ctrl Pts',(0.531083640545139,-7.90811999269952,
14.8865299364146));
#217650=CARTESIAN_POINT('Ctrl Pts',(1.27672076557734,-7.81181222259129,
14.9129498992756));
#217651=CARTESIAN_POINT('Ctrl Pts',(1.53818401177015,-7.76456167768514,
14.922082101914));
#217652=CARTESIAN_POINT('Ctrl Pts',(1.99430598686077,-7.65818547896182,
14.9382718556132));
#217653=CARTESIAN_POINT('Ctrl Pts',(2.18998775985691,-7.60453891413295,
14.9453058626977));
#217654=CARTESIAN_POINT('Ctrl Pts',(2.57078817304305,-7.48422300014504,
14.9594632038919));
#217655=CARTESIAN_POINT('Ctrl Pts',(2.75591001522079,-7.41805228471244,
14.9665725272052));
#217656=CARTESIAN_POINT('Ctrl Pts',(3.00606832804269,-7.31797725100345,
14.976696363252));
#217657=CARTESIAN_POINT('Ctrl Pts',(3.0733895327388,-7.28995981916303,14.9794735726764));
#217658=CARTESIAN_POINT('Ctrl Pts',(3.18663915665525,-7.24098056157631,
14.9842482637425));
#217659=CARTESIAN_POINT('Ctrl Pts',(3.23277234797359,-7.22050215554365,
14.9862225570641));
#217660=CARTESIAN_POINT('Ctrl Pts',(3.29759265087358,-7.19098285421745,
14.9890416794821));
#217661=CARTESIAN_POINT('Ctrl Pts',(3.31644553315007,-7.18230747782314,
14.9898670654784));
#217662=CARTESIAN_POINT('Ctrl Pts',(3.34506773786834,-7.16899991090405,
14.9911282151428));
#217663=CARTESIAN_POINT('Ctrl Pts',(3.35486223508288,-7.1644216288049,14.9915612199923));
#217664=CARTESIAN_POINT('Ctrl Pts',(3.37079127199088,-7.15693602637745,
14.9922677360995));
#217665=CARTESIAN_POINT('Ctrl Pts',(3.37693153256675,-7.15404085178162,
14.9925406409231));
#217666=CARTESIAN_POINT('Ctrl Pts',(3.38882855512097,-7.14841259540262,
14.9930704809727));
#217667=CARTESIAN_POINT('Ctrl Pts',(3.39458575694009,-7.14568045385069,
14.9933273698755));
#217668=CARTESIAN_POINT('Ctrl Pts',(3.40452756648217,-7.14094773558511,
14.9937718150547));
#217669=CARTESIAN_POINT('Ctrl Pts',(3.40871373362139,-7.13895042673583,
14.9939592130585));
#217670=CARTESIAN_POINT('Ctrl Pts',(3.41737395675531,-7.13480909721746,
14.9943474247741));
#217671=CARTESIAN_POINT('Ctrl Pts',(3.42184775607711,-7.13266454756814,
14.9945482637732));
#217672=CARTESIAN_POINT('Ctrl Pts',(3.43268559855492,-7.12745680209742,
14.9950355019325));
#217673=CARTESIAN_POINT('Ctrl Pts',(3.43904755451075,-7.12438929323911,
14.9953221051187));
#217674=CARTESIAN_POINT('Ctrl Pts',(3.46272973022396,-7.1129314774667,14.9963911443719));
#217675=CARTESIAN_POINT('Ctrl Pts',(3.48002333404723,-7.10448653832251,
14.9971761210625));
#217676=CARTESIAN_POINT('Ctrl Pts',(3.79688969567079,-6.94831748844125,
15.0116362581684));
#217677=CARTESIAN_POINT('Ctrl Pts',(4.08682696422884,-6.78183671496138,
15.0261195463624));
#217678=CARTESIAN_POINT('Ctrl Pts',(4.74915053093661,-6.34360107586198,
15.0609632208406));
#217679=CARTESIAN_POINT('Ctrl Pts',(5.110074959318,-6.05663886299537,15.0813670405938));
#217680=CARTESIAN_POINT('Ctrl Pts',(5.55323229247072,-5.63632807981863,
15.1075152519499));
#217681=CARTESIAN_POINT('Ctrl Pts',(5.65948087184041,-5.52963482973197,
15.1138876136051));
#217682=CARTESIAN_POINT('Ctrl Pts',(5.89212397978899,-5.28228403897193,
15.1280783354445));
#217683=CARTESIAN_POINT('Ctrl Pts',(6.01665189889842,-5.13999548233371,
15.1358445528358));
#217684=CARTESIAN_POINT('Ctrl Pts',(6.15539185589763,-4.96950894769468,
15.1447314757485));
#217685=CARTESIAN_POINT('Ctrl Pts',(6.17467729091905,-4.94552610446243,
15.1459724325339));
#217686=CARTESIAN_POINT('Ctrl Pts',(6.20178913010534,-4.91140474664761,
15.147725285661));
#217687=CARTESIAN_POINT('Ctrl Pts',(6.20973154220032,-4.90135891101773,
15.1482398055005));
#217688=CARTESIAN_POINT('Ctrl Pts',(6.22569404247316,-4.88106791313544,
15.1492759707693));
#217689=CARTESIAN_POINT('Ctrl Pts',(6.23371331941065,-4.87082216219094,
15.1497975970903));
#217690=CARTESIAN_POINT('Ctrl Pts',(6.24904800145695,-4.85113005620534,
15.1507971634151));
#217691=CARTESIAN_POINT('Ctrl Pts',(6.25636735234919,-4.8416868238327,15.1512751886229));
#217692=CARTESIAN_POINT('Ctrl Pts',(6.27351846519045,-4.81945508067404,
15.1523975333499));
#217693=CARTESIAN_POINT('Ctrl Pts',(6.28333256928127,-4.8066529970093,15.1530414731178));
#217694=CARTESIAN_POINT('Ctrl Pts',(6.31734106974931,-4.76200820319867,
15.1552790086126));
#217695=CARTESIAN_POINT('Ctrl Pts',(6.34133325569627,-4.7300119333516,15.1568684242194));
#217696=CARTESIAN_POINT('Ctrl Pts',(6.59392817457237,-4.38777187464092,
15.1737224558768));
#217697=CARTESIAN_POINT('Ctrl Pts',(6.79981909854397,-4.0613932197315,15.188483521749));
#217698=CARTESIAN_POINT('Ctrl Pts',(7.24808073288946,-3.22045898664596,
15.2241405309309));
#217699=CARTESIAN_POINT('Ctrl Pts',(7.46037061939149,-2.6923709677696,15.2444708611561));
#217700=CARTESIAN_POINT('Ctrl Pts',(7.66784334268925,-1.95627512409909,
15.2733511331224));
#217701=CARTESIAN_POINT('Ctrl Pts',(7.71423582310269,-1.7644810656686,15.2809369771586));
#217702=CARTESIAN_POINT('Ctrl Pts',(7.75764765228021,-1.5502513117995,15.2896280626817));
#217703=CARTESIAN_POINT('Ctrl Pts',(7.76180045457719,-1.52932335350084,
15.290479383311));
#217704=CARTESIAN_POINT('Ctrl Pts',(7.76802995338839,-1.49725086403733,
15.2917878356465));
#217705=CARTESIAN_POINT('Ctrl Pts',(7.77016745819575,-1.4861181570062,15.2922427112589));
#217706=CARTESIAN_POINT('Ctrl Pts',(7.77364420962375,-1.46779772411631,
15.2929924650061));
#217707=CARTESIAN_POINT('Ctrl Pts',(7.7749974372309,-1.46061264793973,15.2932868116689));
#217708=CARTESIAN_POINT('Ctrl Pts',(7.77739026520432,-1.44781017356194,
15.29381183258));
#217709=CARTESIAN_POINT('Ctrl Pts',(7.77843374614193,-1.44219350040737,
15.294042356937));
#217710=CARTESIAN_POINT('Ctrl Pts',(7.78043901039287,-1.43133441706998,
15.2944884156002));
#217711=CARTESIAN_POINT('Ctrl Pts',(7.78140158182625,-1.42609215344736,
15.2947039190429));
#217712=CARTESIAN_POINT('Ctrl Pts',(7.78336422694018,-1.41534223608281,
15.2951461838447));
#217713=CARTESIAN_POINT('Ctrl Pts',(7.78436375420205,-1.40983448550887,
15.2953729666738));
#217714=CARTESIAN_POINT('Ctrl Pts',(7.78674145841359,-1.39665287292741,
15.2959161782196));
#217715=CARTESIAN_POINT('Ctrl Pts',(7.78811413658624,-1.3889780352934,15.29623282615));
#217716=CARTESIAN_POINT('Ctrl Pts',(7.79301373355582,-1.36134808000553,
15.29737414253));
#217717=CARTESIAN_POINT('Ctrl Pts',(7.79647530163153,-1.3413815664667,15.2982014584043));
#217718=CARTESIAN_POINT('Ctrl Pts',(7.84291546799194,-1.0672584969498,15.309596987744));
#217719=CARTESIAN_POINT('Ctrl Pts',(7.87351566128646,-0.811215330371204,
15.3207660863788));
#217720=CARTESIAN_POINT('Ctrl Pts',(7.92935416494666,-0.0160561983133679,
15.3564238601709));
#217721=CARTESIAN_POINT('Ctrl Pts',(7.91200567443565,0.524513016241022,
15.3818093515221));
#217722=CARTESIAN_POINT('Ctrl Pts',(7.81310333305847,1.25660080367556,15.4151070653646));
#217723=CARTESIAN_POINT('Ctrl Pts',(7.77897249047789,1.4530046783481,15.4239453393603));
#217724=CARTESIAN_POINT('Ctrl Pts',(7.70306049268923,1.80943378647634,15.4397320284595));
#217725=CARTESIAN_POINT('Ctrl Pts',(7.66361099261169,1.9698381816982,15.4467414340259));
#217726=CARTESIAN_POINT('Ctrl Pts',(7.59496313033157,2.21552389567352,15.4573181082936));
#217727=CARTESIAN_POINT('Ctrl Pts',(7.5692823240326,2.30173345635525,15.460998802241));
#217728=CARTESIAN_POINT('Ctrl Pts',(7.53737181940608,2.40253955129851,15.4652674404652));
#217729=CARTESIAN_POINT('Ctrl Pts',(7.53256224607572,2.41757652462369,15.465903256478));
#217730=CARTESIAN_POINT('Ctrl Pts',(7.52513019238944,2.44057510606064,15.4668743123657));
#217731=CARTESIAN_POINT('Ctrl Pts',(7.52254003104011,2.44854706769303,15.4672106490127));
#217732=CARTESIAN_POINT('Ctrl Pts',(7.5180040542434,2.46243269910159,15.4677960341189));
#217733=CARTESIAN_POINT('Ctrl Pts',(7.51606392170615,2.46834820928785,15.4680452757413));
#217734=CARTESIAN_POINT('Ctrl Pts',(7.51168939453167,2.48163326790347,15.4686047046561));
#217735=CARTESIAN_POINT('Ctrl Pts',(7.50925113202372,2.48900154137041,15.4689147597458));
#217736=CARTESIAN_POINT('Ctrl Pts',(7.50271309900235,2.50866200583322,15.4697414824283));
#217737=CARTESIAN_POINT('Ctrl Pts',(7.49859395594341,2.52094775659288,15.4702574874924));
#217738=CARTESIAN_POINT('Ctrl Pts',(7.48082533053159,2.57351555653326,15.4724627594869));
#217739=CARTESIAN_POINT('Ctrl Pts',(7.46688118240589,2.61369765427672,15.4741419105012));
#217740=CARTESIAN_POINT('Ctrl Pts',(7.24909110562212,3.22532106457252,15.4996049523723));
#217741=CARTESIAN_POINT('Ctrl Pts',(6.98050048350745,3.77156892159659,15.5208431908311));
#217742=CARTESIAN_POINT('Ctrl Pts',(6.42534607497203,4.63404020483107,15.5554990138076));
#217743=CARTESIAN_POINT('Ctrl Pts',(6.17100647544183,4.96770107539512,15.5693129568213));
#217744=CARTESIAN_POINT('Ctrl Pts',(5.77644295054215,5.40798752966261,15.5900967330713));
#217745=CARTESIAN_POINT('Ctrl Pts',(5.65726780721133,5.53253450743778,15.5963088547547));
#217746=CARTESIAN_POINT('Ctrl Pts',(5.47009263877204,5.71577093920366,15.6061399436221));
#217747=CARTESIAN_POINT('Ctrl Pts',(5.40500041976233,5.77736274836877,15.6095717231991));
#217748=CARTESIAN_POINT('Ctrl Pts',(5.30605143347067,5.86785463765291,15.6148316812426));
#217749=CARTESIAN_POINT('Ctrl Pts',(5.27297264923195,5.89759774427823,15.6165970970495));
#217750=CARTESIAN_POINT('Ctrl Pts',(5.23341999206203,5.93256312482076,15.6187186238196));
#217751=CARTESIAN_POINT('Ctrl Pts',(5.22718592842097,5.93805669491063,15.6190533160584));
#217752=CARTESIAN_POINT('Ctrl Pts',(5.21758360611871,5.94649159671674,15.6195693371526));
#217753=CARTESIAN_POINT('Ctrl Pts',(5.2142214726166,5.949439925825,15.6197501085775));
#217754=CARTESIAN_POINT('Ctrl Pts',(5.20809330059185,5.9548046703826,15.6200797743035));
#217755=CARTESIAN_POINT('Ctrl Pts',(5.20532807369477,5.95722201493172,15.6202285940524));
#217756=CARTESIAN_POINT('Ctrl Pts',(5.19973089346847,5.96210816326705,15.6205299563838));
#217757=CARTESIAN_POINT('Ctrl Pts',(5.19689886287909,5.96457687718906,15.6206825061414));
#217758=CARTESIAN_POINT('Ctrl Pts',(5.18874628218923,5.97167336210418,15.6211218511035));
#217759=CARTESIAN_POINT('Ctrl Pts',(5.18342131667848,5.97629602493524,15.6214090590183));
#217760=CARTESIAN_POINT('Ctrl Pts',(5.1597443012597,5.99679486036049,15.6226871549473));
#217761=CARTESIAN_POINT('Ctrl Pts',(5.14132562358707,6.01259350511214,15.6236841994389));
#217762=CARTESIAN_POINT('Ctrl Pts',(4.84418429220112,6.26510319729904,15.639809123811));
#217763=CARTESIAN_POINT('Ctrl Pts',(4.54947520658831,6.48227297364153,15.6563479640861));
#217764=CARTESIAN_POINT('Ctrl Pts',(3.80204896278301,6.95690486373847,15.6973266159132));
#217765=CARTESIAN_POINT('Ctrl Pts',(3.33681832060663,7.19164918488398,15.721982862257));
#217766=CARTESIAN_POINT('Ctrl Pts',(2.49373938090724,7.51748878293906,15.762540644776));
#217767=CARTESIAN_POINT('Ctrl Pts',(2.1259339179929,7.6296682377762,15.7790206789024));
#217768=CARTESIAN_POINT('Ctrl Pts',(1.73093870865515,7.71934013293631,15.7953853349192));
#217769=CARTESIAN_POINT('Ctrl Pts',(1.71046684005026,7.72390212908402,15.7962299024903));
#217770=CARTESIAN_POINT('Ctrl Pts',(1.68100955061902,7.73034359846533,15.7974400597501));
#217771=CARTESIAN_POINT('Ctrl Pts',(1.67203871523932,7.73228891048045,15.7978079180774));
#217772=CARTESIAN_POINT('Ctrl Pts',(1.65646525765424,7.73563762166319,15.7984453498401));
#217773=CARTESIAN_POINT('Ctrl Pts',(1.64986419762829,7.73704818992347,15.7987151698813));
#217774=CARTESIAN_POINT('Ctrl Pts',(1.63716982817361,7.73974384158282,15.7992333548886));
#217775=CARTESIAN_POINT('Ctrl Pts',(1.63107679318099,7.74103018173803,15.7994817628994));
#217776=CARTESIAN_POINT('Ctrl Pts',(1.61672289272429,7.7440428272254,15.8000662315986));
#217777=CARTESIAN_POINT('Ctrl Pts',(1.60846076273674,7.74576311263946,15.8004020852574));
#217778=CARTESIAN_POINT('Ctrl Pts',(1.57990902781709,7.75166031101287,15.8015607548397));
#217779=CARTESIAN_POINT('Ctrl Pts',(1.55960569444343,7.75577076764853,15.8023812895051));
#217780=CARTESIAN_POINT('Ctrl Pts',(1.33140725767735,7.80103774250884,15.8115658896232));
#217781=CARTESIAN_POINT('Ctrl Pts',(1.12194745549349,7.83390564206428,15.8196409511701));
#217782=CARTESIAN_POINT('Ctrl Pts',(0.697165307759898,7.88317190650409,
15.8354368125971));
#217783=CARTESIAN_POINT('Ctrl Pts',(0.481989061022481,7.89924880160957,
15.8431420523301));
#217784=CARTESIAN_POINT('Ctrl Pts',(-0.22293209331493,7.92300174743003,
15.8677952867758));
#217785=CARTESIAN_POINT('Ctrl Pts',(-0.712731552397718,7.89402586215829,
15.8839332829613));
#217786=CARTESIAN_POINT('Ctrl Pts',(-1.47347829990967,7.77760783059701,
15.910780307215));
#217787=CARTESIAN_POINT('Ctrl Pts',(-1.74779483160068,7.72059012346852,
15.9208573336582));
#217788=CARTESIAN_POINT('Ctrl Pts',(-2.0813502115402,7.63257027744579,15.9342350781325));
#217789=CARTESIAN_POINT('Ctrl Pts',(-2.1440032104375,7.61520830425879,15.936797960387));
#217790=CARTESIAN_POINT('Ctrl Pts',(-2.21531496627557,7.5944970957119,15.9397801197608));
#217791=CARTESIAN_POINT('Ctrl Pts',(-2.22419192706759,7.59190205450382,
15.9401525038197));
#217792=CARTESIAN_POINT('Ctrl Pts',(-2.2376779540179,7.58793394166489,15.9407199868228));
#217793=CARTESIAN_POINT('Ctrl Pts',(-2.24229039053542,7.58657221235515,
15.9409143863981));
#217794=CARTESIAN_POINT('Ctrl Pts',(-2.25028725570714,7.58420336854743,
15.9412519654746));
#217795=CARTESIAN_POINT('Ctrl Pts',(-2.25367226177303,7.5831981910749,15.9413950267111));
#217796=CARTESIAN_POINT('Ctrl Pts',(-2.26070450327306,7.58110484265696,
15.9416925769256));
#217797=CARTESIAN_POINT('Ctrl Pts',(-2.2643516277544,7.58001630554069,15.9418470880913));
#217798=CARTESIAN_POINT('Ctrl Pts',(-2.27431983246404,7.57703331421637,
15.9422699180735));
#217799=CARTESIAN_POINT('Ctrl Pts',(-2.28063931794703,7.57513358601745,
15.9425385545351));
#217800=CARTESIAN_POINT('Ctrl Pts',(-2.30468803971605,7.56787137325946,
15.9435630262013));
#217801=CARTESIAN_POINT('Ctrl Pts',(-2.32240067627104,7.56245457311464,
15.9443220930826));
#217802=CARTESIAN_POINT('Ctrl Pts',(-2.63231164295717,7.4664875062857,15.9576802792473));
#217803=CARTESIAN_POINT('Ctrl Pts',(-2.91900929989047,7.35913379099867,
15.971234298508));
#217804=CARTESIAN_POINT('Ctrl Pts',(-3.84836935432984,6.94827102071024,
16.0176047654335));
#217805=CARTESIAN_POINT('Ctrl Pts',(-4.45647569220624,6.57483498169648,
16.0516697229704));
#217806=CARTESIAN_POINT('Ctrl Pts',(-5.17696207090427,5.9859362614302,16.0926696676948));
#217807=CARTESIAN_POINT('Ctrl Pts',(-5.34150562403159,5.83958021296413,
16.1021181678034));
#217808=CARTESIAN_POINT('Ctrl Pts',(-5.5736475534076,5.61506416284713,16.115563637908));
#217809=CARTESIAN_POINT('Ctrl Pts',(-5.64615601095024,5.54214903764875,
16.1197817764979));
#217810=CARTESIAN_POINT('Ctrl Pts',(-5.72889932244715,5.45563184961359,
16.1246203158833));
#217811=CARTESIAN_POINT('Ctrl Pts',(-5.74053517558061,5.44338701800336,
16.1253013359021));
#217812=CARTESIAN_POINT('Ctrl Pts',(-5.75820091399726,5.4246770766829,16.1263362088741));
#217813=CARTESIAN_POINT('Ctrl Pts',(-5.76425929329439,5.41823900843915,
16.1266912826983));
#217814=CARTESIAN_POINT('Ctrl Pts',(-5.77523485326303,5.40653634813208,
16.1273348585507));
#217815=CARTESIAN_POINT('Ctrl Pts',(-5.78015565456969,5.40127517381916,
16.127623514948));
#217816=CARTESIAN_POINT('Ctrl Pts',(-5.78999005917396,5.39073169065454,
16.1282006380164));
#217817=CARTESIAN_POINT('Ctrl Pts',(-5.79490363677673,5.38544936721038,
16.1284891035195));
#217818=CARTESIAN_POINT('Ctrl Pts',(-5.80873863779206,5.37053524340787,
16.1293016603914));
#217819=CARTESIAN_POINT('Ctrl Pts',(-5.8176433387451,5.36088792534746,16.1298250437338));
#217820=CARTESIAN_POINT('Ctrl Pts',(-5.85435966784315,5.32091038100809,
16.1319847542219));
#217821=CARTESIAN_POINT('Ctrl Pts',(-5.88195867339734,5.29038530087749,
16.1336121420364));
#217822=CARTESIAN_POINT('Ctrl Pts',(-6.33282587472184,4.7838268908701,16.1602693941614));
#217823=CARTESIAN_POINT('Ctrl Pts',(-6.6973134961961,4.25860960472822,16.1826227163787));
#217824=CARTESIAN_POINT('Ctrl Pts',(-7.16693673194111,3.36965827644062,
16.2174630859276));
#217825=CARTESIAN_POINT('Ctrl Pts',(-7.31602226416854,3.03238776846265,
16.2301529459766));
#217826=CARTESIAN_POINT('Ctrl Pts',(-7.51222838259756,2.48883037003805,
16.2512651639963));
#217827=CARTESIAN_POINT('Ctrl Pts',(-7.57552572331831,2.28894341957907,
16.2591846793608));
#217828=CARTESIAN_POINT('Ctrl Pts',(-7.6374228804733,2.06260044129216,16.268466281304));
#217829=CARTESIAN_POINT('Ctrl Pts',(-7.64391743189899,2.03840013547349,
16.2694619393055));
#217830=CARTESIAN_POINT('Ctrl Pts',(-7.655237853753,1.99540247054524,16.2712363700641));
#217831=CARTESIAN_POINT('Ctrl Pts',(-7.66010975199435,1.97661736221219,
16.2720134202061));
#217832=CARTESIAN_POINT('Ctrl Pts',(-7.66713534470493,1.94911192190456,
16.2731537021131));
#217833=CARTESIAN_POINT('Ctrl Pts',(-7.66934340716722,1.94040546802124,
16.2735150097861));
#217834=CARTESIAN_POINT('Ctrl Pts',(-7.67319969644353,1.92509059690481,
16.2741511872963));
#217835=CARTESIAN_POINT('Ctrl Pts',(-7.67485422805534,1.91848376735113,
16.2744258393873));
#217836=CARTESIAN_POINT('Ctrl Pts',(-7.67805613474756,1.90562757134092,
16.2749606741889));
#217837=CARTESIAN_POINT('Ctrl Pts',(-7.67960441740908,1.89937843538817,
16.2752208259352));
#217838=CARTESIAN_POINT('Ctrl Pts',(-7.68329221046285,1.88441564259427,
16.2758441478943));
#217839=CARTESIAN_POINT('Ctrl Pts',(-7.68542452632376,1.87570023055054,
16.2762075566575));
#217840=CARTESIAN_POINT('Ctrl Pts',(-7.69186412951485,1.84918431316404,
16.2773142037854));
#217841=CARTESIAN_POINT('Ctrl Pts',(-7.69612442105751,1.83137251829451,
16.2780589603471));
#217842=CARTESIAN_POINT('Ctrl Pts',(-7.7460963144361,1.61919169996095,16.2869461670382));
#217843=CARTESIAN_POINT('Ctrl Pts',(-7.78449384303411,1.42317964181873,
16.2953075273668));
#217844=CARTESIAN_POINT('Ctrl Pts',(-7.87892463966614,0.821174561950701,
16.3211556837578));
#217845=CARTESIAN_POINT('Ctrl Pts',(-7.91087598531184,0.412096929851135,
16.3389141450628));
#217846=CARTESIAN_POINT('Ctrl Pts',(-7.91122481811769,-0.743705493900177,
16.3884127477905));
#217847=CARTESIAN_POINT('Ctrl Pts',(-7.80590345515495,-1.48610707923397,
16.4193039870618));
#217848=CARTESIAN_POINT('Ctrl Pts',(-7.57736574926858,-2.27442753535988,
16.4526704896892));
#217849=CARTESIAN_POINT('Ctrl Pts',(-7.55556898687502,-2.34581962696523,
16.4556948906204));
#217850=CARTESIAN_POINT('Ctrl Pts',(-7.52445344597799,-2.44279788095363,
16.459806860129));
#217851=CARTESIAN_POINT('Ctrl Pts',(-7.51600824186062,-2.46865981103749,
16.4609037928098));
#217852=CARTESIAN_POINT('Ctrl Pts',(-7.50136310499068,-2.51273610639126,
16.4627739369616));
#217853=CARTESIAN_POINT('Ctrl Pts',(-7.49522983234375,-2.53097233014358,
16.4635478854462));
#217854=CARTESIAN_POINT('Ctrl Pts',(-7.482531161884,-2.56827864051784,16.465131581671));
#217855=CARTESIAN_POINT('Ctrl Pts',(-7.47595924021528,-2.58734636360536,
16.4659412488633));
#217856=CARTESIAN_POINT('Ctrl Pts',(-7.46061969837214,-2.63130598417239,
16.4678084326599));
#217857=CARTESIAN_POINT('Ctrl Pts',(-7.45180028644896,-2.65617958035703,
16.4688653381997));
#217858=CARTESIAN_POINT('Ctrl Pts',(-7.42360445770979,-2.73445516146129,
16.4721927296461));
#217859=CARTESIAN_POINT('Ctrl Pts',(-7.40377713792021,-2.7876930118315,
16.4744578189848));
#217860=CARTESIAN_POINT('Ctrl Pts',(-7.21371737448243,-3.28168276449015,
16.4954988710632));
#217861=CARTESIAN_POINT('Ctrl Pts',(-7.00489181316891,-3.70657094219149,
16.5137046890007));
#217862=CARTESIAN_POINT('Ctrl Pts',(-6.66297360762328,-4.2688575725084,
16.5389885353465));
#217863=CARTESIAN_POINT('Ctrl Pts',(-6.56100128272182,-4.42398277906825,
16.5461116421576));
#217864=CARTESIAN_POINT('Ctrl Pts',(-6.32360704237753,-4.7588325223663,
16.5619922547787));
#217865=CARTESIAN_POINT('Ctrl Pts',(-6.1857848884082,-4.93665401812913,
16.5707686658607));
#217866=CARTESIAN_POINT('Ctrl Pts',(-6.0246139863263,-5.12723694194316,
16.5807519238626));
#217867=CARTESIAN_POINT('Ctrl Pts',(-6.00855975003395,-5.14604139796238,
16.5817434987504));
#217868=CARTESIAN_POINT('Ctrl Pts',(-5.9843328493046,-5.1741506262578,16.583235894038));
#217869=CARTESIAN_POINT('Ctrl Pts',(-5.97622607926751,-5.18351195644496,
16.5837346077011));
#217870=CARTESIAN_POINT('Ctrl Pts',(-5.96145852556676,-5.2004841638832,
16.5846418345552));
#217871=CARTESIAN_POINT('Ctrl Pts',(-5.95480505686396,-5.20810138389114,
16.5850501261238));
#217872=CARTESIAN_POINT('Ctrl Pts',(-5.94044435150669,-5.22447873455879,
16.5859303723319));
#217873=CARTESIAN_POINT('Ctrl Pts',(-5.93273230772726,-5.23323461207253,
16.5864024680483));
#217874=CARTESIAN_POINT('Ctrl Pts',(-5.91153828586117,-5.25719020862571,
16.5876981383882));
#217875=CARTESIAN_POINT('Ctrl Pts',(-5.89801710776141,-5.27235507018253,
16.5885228302435));
#217876=CARTESIAN_POINT('Ctrl Pts',(-5.82583403600294,-5.35268781529885,
16.5929149493199));
#217877=CARTESIAN_POINT('Ctrl Pts',(-5.76615077945662,-5.41692845538449,
16.5965097636945));
#217878=CARTESIAN_POINT('Ctrl Pts',(-5.429971643884,-5.76692548361496,16.6165261898275));
#217879=CARTESIAN_POINT('Ctrl Pts',(-5.13330539865589,-6.03251126805825,
16.6333168935519));
#217880=CARTESIAN_POINT('Ctrl Pts',(-4.55191783805583,-6.47892374906174,
16.6640542837353));
#217881=CARTESIAN_POINT('Ctrl Pts',(-4.27317332956748,-6.66606394778776,
16.6780083589665));
#217882=CARTESIAN_POINT('Ctrl Pts',(-3.87686666090794,-6.89703028231194,
16.6967917186288));
#217883=CARTESIAN_POINT('Ctrl Pts',(-3.76890742286182,-6.95661262827356,
16.7018100248811));
#217884=CARTESIAN_POINT('Ctrl Pts',(-3.62296231759696,-7.03276422915456,
16.7084709861178));
#217885=CARTESIAN_POINT('Ctrl Pts',(-3.58617656520798,-7.05159317622081,
16.7101396966647));
#217886=CARTESIAN_POINT('Ctrl Pts',(-3.5281740140914,-7.08071076897187,
16.7127553417805));
#217887=CARTESIAN_POINT('Ctrl Pts',(-3.50705595473638,-7.09119421549831,
16.7137044643006));
#217888=CARTESIAN_POINT('Ctrl Pts',(-3.46628106917132,-7.1112090230155,
16.7155309870954));
#217889=CARTESIAN_POINT('Ctrl Pts',(-3.44663101121033,-7.12075367466183,
16.71640852752));
#217890=CARTESIAN_POINT('Ctrl Pts',(-3.40000197813141,-7.14316463058394,
16.7184846639398));
#217891=CARTESIAN_POINT('Ctrl Pts',(-3.37298909631384,-7.15595968091379,
16.7196824751856));
#217892=CARTESIAN_POINT('Ctrl Pts',(-3.29255097656199,-7.19350372005637,
16.7232350890006));
#217893=CARTESIAN_POINT('Ctrl Pts',(-3.23892110823703,-7.21780976571606,
16.7255851924293));
#217894=CARTESIAN_POINT('Ctrl Pts',(-2.8741555315789,-7.37824406385046,
16.7414526427757));
#217895=CARTESIAN_POINT('Ctrl Pts',(-2.55479248996414,-7.49481831616603,
16.7548217308199));
#217896=CARTESIAN_POINT('Ctrl Pts',(-1.78270437262863,-7.72153931382124,
16.7860242710609));
#217897=CARTESIAN_POINT('Ctrl Pts',(-1.32579321320553,-7.81296982832797,
16.8034911819049));
#217898=CARTESIAN_POINT('Ctrl Pts',(-0.479143300877044,-7.90593724794838,
16.8351401251896));
#217899=CARTESIAN_POINT('Ctrl Pts',(-0.0922365345026519,-7.91990494120669,
16.8493601012997));
#217900=CARTESIAN_POINT('Ctrl Pts',(0.299619445892115,-7.90532601685582,
16.8643922488431));
#217901=CARTESIAN_POINT('Ctrl Pts',(0.305114962567271,-7.90511581853389,
16.8646031977026));
#217902=CARTESIAN_POINT('Ctrl Pts',(0.328325148613027,-7.90420381182826,
16.8654947105307));
#217903=CARTESIAN_POINT('Ctrl Pts',(0.346037604667464,-7.90344818889555,
16.8661764685522));
#217904=CARTESIAN_POINT('Ctrl Pts',(0.391746202730702,-7.90134428506339,
16.8679397301249));
#217905=CARTESIAN_POINT('Ctrl Pts',(0.419737900728484,-7.89990675116246,
16.869023341465));
#217906=CARTESIAN_POINT('Ctrl Pts',(0.54744049651709,-7.89266784992797,
16.8739862156299));
#217907=CARTESIAN_POINT('Ctrl Pts',(0.647041611770897,-7.88512733702743,
16.8779105055205));
#217908=CARTESIAN_POINT('Ctrl Pts',(0.762125053221456,-7.87421955888687,
16.8825299855726));
#217909=CARTESIAN_POINT('Ctrl Pts',(0.777774819086329,-7.87268915840396,
16.8831600017052));
#217910=CARTESIAN_POINT('Ctrl Pts',(0.801244543784525,-7.87032337512253,
16.8841076961318));
#217911=CARTESIAN_POINT('Ctrl Pts',(0.809068039735018,-7.86952296867311,
16.8844240830014));
#217912=CARTESIAN_POINT('Ctrl Pts',(0.82296900940171,-7.86807983934883,
16.8849871151419));
#217913=CARTESIAN_POINT('Ctrl Pts',(0.829046963173051,-7.86744173676509,
16.8852335862202));
#217914=CARTESIAN_POINT('Ctrl Pts',(0.841808454551067,-7.86608700111764,
16.8857517159136));
#217915=CARTESIAN_POINT('Ctrl Pts',(0.848491828173234,-7.86536889156965,
16.8860234308248));
#217916=CARTESIAN_POINT('Ctrl Pts',(0.866028876139057,-7.86346197303484,
16.886737375529));
#217917=CARTESIAN_POINT('Ctrl Pts',(0.876880996434796,-7.86225921298665,
16.8871801476474));
#217918=CARTESIAN_POINT('Ctrl Pts',(0.924883247016807,-7.85683841660979,
16.889143102701));
#217919=CARTESIAN_POINT('Ctrl Pts',(0.962005287176125,-7.85237955560534,
16.8906728980387));
#217920=CARTESIAN_POINT('Ctrl Pts',(1.22096365756672,-7.81941128320379,
16.9014346404006));
#217921=CARTESIAN_POINT('Ctrl Pts',(1.44150350079323,-7.78177267628682,
16.9111032630698));
#217922=CARTESIAN_POINT('Ctrl Pts',(1.91642753726304,-7.67984005746852,
16.932694518889));
#217923=CARTESIAN_POINT('Ctrl Pts',(2.16982890755309,-7.61212659798136,
16.9446948969209));
#217924=CARTESIAN_POINT('Ctrl Pts',(2.98366944528276,-7.35070748181602,
16.9840364504983));
#217925=CARTESIAN_POINT('Ctrl Pts',(3.52585681112428,-7.10659258770302,
17.0113709298823));
#217926=CARTESIAN_POINT('Ctrl Pts',(4.22060749972608,-6.69452057109854,
17.0460336058856));
#217927=CARTESIAN_POINT('Ctrl Pts',(4.40096281659593,-6.57736031714092,
17.0550151134507));
#217928=CARTESIAN_POINT('Ctrl Pts',(4.59335558223891,-6.44091927325026,
17.064582227223));
#217929=CARTESIAN_POINT('Ctrl Pts',(4.61033208552855,-6.42877862885907,
17.0654263272162));
#217930=CARTESIAN_POINT('Ctrl Pts',(4.63546481340481,-6.41065435669106,
17.066675870371));
#217931=CARTESIAN_POINT('Ctrl Pts',(4.64365786261525,-6.40472208399058,
17.0670831950191));
#217932=CARTESIAN_POINT('Ctrl Pts',(4.65766222512379,-6.39454106398617,
17.0677794130459));
#217933=CARTESIAN_POINT('Ctrl Pts',(4.66347914934097,-6.39030007483029,
17.0680685914856));
#217934=CARTESIAN_POINT('Ctrl Pts',(4.67527099950436,-6.38167822539996,
17.0686547928282));
#217935=CARTESIAN_POINT('Ctrl Pts',(4.68124557704735,-6.37729689908686,
17.06895179811));
#217936=CARTESIAN_POINT('Ctrl Pts',(4.69494013283534,-6.36722468058036,
17.0696325658985));
#217937=CARTESIAN_POINT('Ctrl Pts',(4.70265594125082,-6.36152812482307,
17.0700161183778));
#217938=CARTESIAN_POINT('Ctrl Pts',(4.71880916420298,-6.34955680607217,
17.0708190865432));
#217939=CARTESIAN_POINT('Ctrl Pts',(4.72724446956772,-6.34327922195496,
17.0712383966277));
#217940=CARTESIAN_POINT('Ctrl Pts',(4.74947858396878,-6.32666353319766,
17.0723436303306));
#217941=CARTESIAN_POINT('Ctrl Pts',(4.76325618685626,-6.31629707857646,
17.0730284993763));
#217942=CARTESIAN_POINT('Ctrl Pts',(4.80440400848555,-6.28512570168122,
17.0750739696588));
#217943=CARTESIAN_POINT('Ctrl Pts',(4.8316727570022,-6.26418720727239,17.0764295835561));
#217944=CARTESIAN_POINT('Ctrl Pts',(5.13399232002024,-6.02890051874563,
17.0914616902129));
#217945=CARTESIAN_POINT('Ctrl Pts',(5.39472961595636,-5.79676114851014,
17.10443041916));
#217946=CARTESIAN_POINT('Ctrl Pts',(5.92997317058396,-5.25272328977008,
17.1318029862695));
#217947=CARTESIAN_POINT('Ctrl Pts',(6.19697061040851,-4.93490084494681,
17.1459677397571));
#217948=CARTESIAN_POINT('Ctrl Pts',(6.72055578030378,-4.2017496353388,17.177168162694));
#217949=CARTESIAN_POINT('Ctrl Pts',(6.96613100122361,-3.78067411618811,
17.1942237944322));
#217950=CARTESIAN_POINT('Ctrl Pts',(7.18488433895395,-3.31094684236518,
17.2147237232296));
#217951=CARTESIAN_POINT('Ctrl Pts',(7.1981332490866,-3.28204351145843,17.2159909447991));
#217952=CARTESIAN_POINT('Ctrl Pts',(7.21517264154306,-3.24427152714235,
17.2176538161701));
#217953=CARTESIAN_POINT('Ctrl Pts',(7.21912186127115,-3.23547423726308,
17.2180415868109));
#217954=CARTESIAN_POINT('Ctrl Pts',(7.22517070706325,-3.22193360599626,
17.2186391480001));
#217955=CARTESIAN_POINT('Ctrl Pts',(7.22728177850907,-3.21719536265559,
17.218848385048));
#217956=CARTESIAN_POINT('Ctrl Pts',(7.23125601214119,-3.20825164914942,
17.21924357984));
#217957=CARTESIAN_POINT('Ctrl Pts',(7.2331201706971,-3.20404662162282,17.2194294900012));
#217958=CARTESIAN_POINT('Ctrl Pts',(7.2373928035448,-3.19438600851786,17.2198568319446));
#217959=CARTESIAN_POINT('Ctrl Pts',(7.23979877639917,-3.18892932520966,
17.2200983812559));
#217960=CARTESIAN_POINT('Ctrl Pts',(7.24643837090136,-3.17382465553584,
17.2207674753057));
#217961=CARTESIAN_POINT('Ctrl Pts',(7.25065888258752,-3.16417094579374,
17.2211956263255));
#217962=CARTESIAN_POINT('Ctrl Pts',(7.27350018835718,-3.11163963760719,
17.2235281450474));
#217963=CARTESIAN_POINT('Ctrl Pts',(7.29175969894736,-3.06860662094485,
17.2254487014873));
#217964=CARTESIAN_POINT('Ctrl Pts',(7.57347273159961,-2.38796614461766,
17.2559511480148));
#217965=CARTESIAN_POINT('Ctrl Pts',(7.75279829534976,-1.71873934032661,
17.2873092424353));
#217966=CARTESIAN_POINT('Ctrl Pts',(7.89553649078866,-0.636803331712192,
17.3344857316866));
#217967=CARTESIAN_POINT('Ctrl Pts',(7.91767744205785,-0.235450646987964,
17.3513312488676));
#217968=CARTESIAN_POINT('Ctrl Pts',(7.9084831315777,0.202956362386627,17.3690919653084));
#217969=CARTESIAN_POINT('Ctrl Pts',(7.90744464334923,0.240033264658368,
17.3705894331964));
#217970=CARTESIAN_POINT('Ctrl Pts',(7.9055463365649,0.294194932724599,17.3727706581365));
#217971=CARTESIAN_POINT('Ctrl Pts',(7.90489180339208,0.311286230616918,
17.3734580557675));
#217972=CARTESIAN_POINT('Ctrl Pts',(7.90364830890303,0.341217855308203,
17.3746603411717));
#217973=CARTESIAN_POINT('Ctrl Pts',(7.90308347224003,0.354059101752278,
17.3751756484989));
#217974=CARTESIAN_POINT('Ctrl Pts',(7.90185818923262,0.380449975351676,
17.3762336993426));
#217975=CARTESIAN_POINT('Ctrl Pts',(7.90119418207741,0.393999397063265,
17.3767763797474));
#217976=CARTESIAN_POINT('Ctrl Pts',(7.89943473111563,0.428107197611385,
17.3781411559915));
#217977=CARTESIAN_POINT('Ctrl Pts',(7.89829388006276,0.448663161362323,
17.3789624785136));
#217978=CARTESIAN_POINT('Ctrl Pts',(7.89364320146484,0.526935994223997,
17.3820855982453));
#217979=CARTESIAN_POINT('Ctrl Pts',(7.88958081721388,0.584618826696907,
17.3843784221275));
#217980=CARTESIAN_POINT('Ctrl Pts',(7.83701258015053,1.22999547795197,17.4099390275444));
#217981=CARTESIAN_POINT('Ctrl Pts',(7.72357520639323,1.8105501972467,17.4318915575522));
#217982=CARTESIAN_POINT('Ctrl Pts',(7.42953922400908,2.74560134478082,17.4679417549818));
#217983=CARTESIAN_POINT('Ctrl Pts',(7.28499846947608,3.10888346147995,17.4821866086519));
#217984=CARTESIAN_POINT('Ctrl Pts',(7.04644150997162,3.59939031107713,17.5030062044131));
#217985=CARTESIAN_POINT('Ctrl Pts',(6.9745661320557,3.73675963987432,17.5090255027129));
#217986=CARTESIAN_POINT('Ctrl Pts',(6.88668389597182,3.89334164130696,17.5161861656357));
#217987=CARTESIAN_POINT('Ctrl Pts',(6.87456351411343,3.91470314238978,17.5171696564554));
#217988=CARTESIAN_POINT('Ctrl Pts',(6.85813575004615,3.94334459217472,17.5184975953473));
#217989=CARTESIAN_POINT('Ctrl Pts',(6.85391580880677,3.95067470488548,17.5188382709899));
#217990=CARTESIAN_POINT('Ctrl Pts',(6.84679248991659,3.96300227153346,17.5194126108909));
#217991=CARTESIAN_POINT('Ctrl Pts',(6.84389537152192,3.96800334520582,17.5196459995112));
#217992=CARTESIAN_POINT('Ctrl Pts',(6.83834117374544,3.97756695333956,17.5200930632562));
#217993=CARTESIAN_POINT('Ctrl Pts',(6.83568500140166,3.98213001272897,17.5203066978421));
#217994=CARTESIAN_POINT('Ctrl Pts',(6.82946160269699,3.99279666352969,17.520806866718));
#217995=CARTESIAN_POINT('Ctrl Pts',(6.82589076238279,3.99889813305984,17.5210935642522));
#217996=CARTESIAN_POINT('Ctrl Pts',(6.81563160724507,4.0163740995185,17.5219164532698));
#217997=CARTESIAN_POINT('Ctrl Pts',(6.80892302612491,4.02773662674448,17.5224535756714));
#217998=CARTESIAN_POINT('Ctrl Pts',(6.76523935690617,4.10130394393699,17.5259450988667));
#217999=CARTESIAN_POINT('Ctrl Pts',(6.72744154484847,4.16301421287914,17.5289384189671));
#218000=CARTESIAN_POINT('Ctrl Pts',(6.6147590512869,4.34144132807819,17.5378040425662));
#218001=CARTESIAN_POINT('Ctrl Pts',(6.53764835196612,4.45671406129018,17.5438005936128));
#218002=CARTESIAN_POINT('Ctrl Pts',(6.38079462798303,4.67835837220955,17.5557737039828));
#218003=CARTESIAN_POINT('Ctrl Pts',(6.30131830144144,4.78486811140937,17.5617388441873));
#218004=CARTESIAN_POINT('Ctrl Pts',(6.16331763153661,4.96040444154811,17.5718674407996));
#218005=CARTESIAN_POINT('Ctrl Pts',(6.10622152199834,5.03052232104846,17.5759969880647));
#218006=CARTESIAN_POINT('Ctrl Pts',(5.99692643556687,5.16014109508985,17.5837693013283));
#218007=CARTESIAN_POINT('Ctrl Pts',(5.945011512419,5.21986789194586,17.5874080889248));
#218008=CARTESIAN_POINT('Ctrl Pts',(5.60126735627597,5.60355556308885,17.6111186084839));
#218009=CARTESIAN_POINT('Ctrl Pts',(5.28395479734401,5.90371929368651,17.6311947158881));
#218010=CARTESIAN_POINT('Ctrl Pts',(4.70845083775999,6.36435864889453,17.6635551836821));
#218011=CARTESIAN_POINT('Ctrl Pts',(4.46283140566761,6.53893972216612,17.6763151063948));
#218012=CARTESIAN_POINT('Ctrl Pts',(4.18814210735458,6.711477303161,17.6894589220539));
#218013=CARTESIAN_POINT('Ctrl Pts',(4.16839304281629,6.72376095316463,17.69039798765));
#218014=CARTESIAN_POINT('Ctrl Pts',(4.14085334878118,6.74072229835736,17.6916993178132));
#218015=CARTESIAN_POINT('Ctrl Pts',(4.13310849644529,6.74547386897397,17.6920643893391));
#218016=CARTESIAN_POINT('Ctrl Pts',(4.11974958857148,6.75363809295936,17.6926925546024));
#218017=CARTESIAN_POINT('Ctrl Pts',(4.11413944430297,6.75705711063139,17.6929558898508));
#218018=CARTESIAN_POINT('Ctrl Pts',(4.10266703726978,6.76402921131861,17.6934934443249));
#218019=CARTESIAN_POINT('Ctrl Pts',(4.09680440141934,6.76758167199382,17.693767639835));
#218020=CARTESIAN_POINT('Ctrl Pts',(4.08321038898621,6.77579481796083,17.6944022626615));
#218021=CARTESIAN_POINT('Ctrl Pts',(4.07547563025945,6.78044990275075,17.6947624776017));
#218022=CARTESIAN_POINT('Ctrl Pts',(4.05919965605398,6.79020751816177,17.695518632824));
#218023=CARTESIAN_POINT('Ctrl Pts',(4.05065674522095,6.79530719841064,17.6959144650043));
#218024=CARTESIAN_POINT('Ctrl Pts',(4.02791270393648,6.80882609583634,17.6969654992531));
#218025=CARTESIAN_POINT('Ctrl Pts',(4.0136947656629,6.81721701916115,17.6976196330092));
#218026=CARTESIAN_POINT('Ctrl Pts',(3.97067786158824,6.84242284802061,17.6995900501004));
#218027=CARTESIAN_POINT('Ctrl Pts',(3.941798574629,6.85910031595811,17.7009011647227));
#218028=CARTESIAN_POINT('Ctrl Pts',(3.8384166002455,6.91793369623867,17.7055535399807));
#218029=CARTESIAN_POINT('Ctrl Pts',(3.7633350893431,6.95906302673103,17.7088565295266));
#218030=CARTESIAN_POINT('Ctrl Pts',(3.40329239908198,7.14876148495397,17.7243533920744));
#218031=CARTESIAN_POINT('Ctrl Pts',(3.1101104504096,7.28110057494453,17.7359504514779));
#218032=CARTESIAN_POINT('Ctrl Pts',(2.08862568196925,7.66919295046357,17.7740200046964));
#218033=CARTESIAN_POINT('Ctrl Pts',(1.33150665333911,7.83617718435891,17.7980517133665));
#218034=CARTESIAN_POINT('Ctrl Pts',(0.538504565817504,7.89268671613492,
17.8277355579075));
#218035=CARTESIAN_POINT('Ctrl Pts',(0.514687785514003,7.89427559896378,
17.8286315431259));
#218036=CARTESIAN_POINT('Ctrl Pts',(0.483124760025503,7.89623781298593,
17.8298252641054));
#218037=CARTESIAN_POINT('Ctrl Pts',(0.475384473094035,7.89670758829863,
17.8301185071108));
#218038=CARTESIAN_POINT('Ctrl Pts',(0.359055861748371,7.90359617622608,
17.834533373592));
#218039=CARTESIAN_POINT('Ctrl Pts',(0.250351708259917,7.90778576104458,
17.8387599924468));
#218040=CARTESIAN_POINT('Ctrl Pts',(0.131133523855111,7.909920011679,17.8435378505872));
#218041=CARTESIAN_POINT('Ctrl Pts',(0.1206662575226,7.91008661422039,17.8439585460098));
#218042=CARTESIAN_POINT('Ctrl Pts',(0.105154395058921,7.91030271251114,
17.8445838124572));
#218043=CARTESIAN_POINT('Ctrl Pts',(0.100109994754808,7.91036816077997,
17.8447874321589));
#218044=CARTESIAN_POINT('Ctrl Pts',(0.091488194108342,7.91047177541537,
17.8451359480434));
#218045=CARTESIAN_POINT('Ctrl Pts',(0.0879108186967583,7.91051234037162,
17.8452806999385));
#218046=CARTESIAN_POINT('Ctrl Pts',(0.0809624521533742,7.91058641606786,
17.8455621363214));
#218047=CARTESIAN_POINT('Ctrl Pts',(0.0775914646616999,7.91062019877506,
17.8456988042998));
#218048=CARTESIAN_POINT('Ctrl Pts',(0.0695428551312033,7.91069571360369,
17.8460254259222));
#218049=CARTESIAN_POINT('Ctrl Pts',(0.0648652464374623,7.91073545137829,
17.8462155001267));
#218050=CARTESIAN_POINT('Ctrl Pts',(0.0507019376084755,7.91084321017827,
17.8467917898599));
#218051=CARTESIAN_POINT('Ctrl Pts',(0.0412162212705007,7.91089831839667,
17.8471787896223));
#218052=CARTESIAN_POINT('Ctrl Pts',(-0.0493513180513969,7.91126158142155,
17.8508835022615));
#218053=CARTESIAN_POINT('Ctrl Pts',(-0.130430537977473,7.91034021487243,
17.8542744756896));
#218054=CARTESIAN_POINT('Ctrl Pts',(-0.468429134589048,7.90130154356842,
17.8686752118965));
#218055=CARTESIAN_POINT('Ctrl Pts',(-0.724875649511695,7.8819114770744,
17.8802352980139));
#218056=CARTESIAN_POINT('Ctrl Pts',(-1.18498850829019,7.82447690145656,
17.9015486843676));
#218057=CARTESIAN_POINT('Ctrl Pts',(-1.38898920206389,7.79084995150255,
17.9112052138981));
#218058=CARTESIAN_POINT('Ctrl Pts',(-1.87779738768121,7.69046550426202,
17.9345216740625));
#218059=CARTESIAN_POINT('Ctrl Pts',(-2.16068967225937,7.61582660293843,
17.9481577013894));
#218060=CARTESIAN_POINT('Ctrl Pts',(-2.61111143578272,7.46986103314748,
17.969683821983));
#218061=CARTESIAN_POINT('Ctrl Pts',(-2.78145116834839,7.40812131488053,
17.9777827967962));
#218062=CARTESIAN_POINT('Ctrl Pts',(-3.19882536764348,7.24041575186159,
17.9974450563588));
#218063=CARTESIAN_POINT('Ctrl Pts',(-3.44287123018338,7.12760562098013,
18.0087729044886));
#218064=CARTESIAN_POINT('Ctrl Pts',(-3.70021990464694,6.99233715146218,
18.0205271646795));
#218065=CARTESIAN_POINT('Ctrl Pts',(-3.71967465505053,6.98200735133162,
18.0214145976387));
#218066=CARTESIAN_POINT('Ctrl Pts',(-3.74740066349827,6.96713702209471,
18.0226777236157));
#218067=CARTESIAN_POINT('Ctrl Pts',(-3.75570724207176,6.96266279020748,
18.023055943862));
#218068=CARTESIAN_POINT('Ctrl Pts',(-3.76991834605047,6.95497533077351,
18.0237026640499));
#218069=CARTESIAN_POINT('Ctrl Pts',(-3.77582680645159,6.95176942335889,
18.0239714433805));
#218070=CARTESIAN_POINT('Ctrl Pts',(-3.78720482388141,6.94557697079396,
18.0244888387639));
#218071=CARTESIAN_POINT('Ctrl Pts',(-3.79267495083239,6.94259148681735,
18.0247374951372));
#218072=CARTESIAN_POINT('Ctrl Pts',(-3.80640154267989,6.93507872781798,
18.025361247898));
#218073=CARTESIAN_POINT('Ctrl Pts',(-3.8146534737496,6.93054316350501,18.025736026294));
#218074=CARTESIAN_POINT('Ctrl Pts',(-3.84244160334208,6.91520512203659,
18.0269974201178));
#218075=CARTESIAN_POINT('Ctrl Pts',(-3.86194025680446,6.90433463984726,
18.027881423695));
#218076=CARTESIAN_POINT('Ctrl Pts',(-4.21647187341269,6.70471179813409,
18.0439354013687));
#218077=CARTESIAN_POINT('Ctrl Pts',(-4.53736164708381,6.49185541262765,
18.0581116042004));
#218078=CARTESIAN_POINT('Ctrl Pts',(-5.50449033298963,5.74345105556112,
18.1012394415903));
#218079=CARTESIAN_POINT('Ctrl Pts',(-6.08154747687998,5.12843857623232,
18.1271523554186));
#218080=CARTESIAN_POINT('Ctrl Pts',(-6.57384695119827,4.40114530004626,
18.1616701216648));
#218081=CARTESIAN_POINT('Ctrl Pts',(-6.59617182633263,4.36761500298037,
18.1632702885342));
#218082=CARTESIAN_POINT('Ctrl Pts',(-6.62250875064856,4.3273963979237,18.1652020020667));
#218083=CARTESIAN_POINT('Ctrl Pts',(-6.62676857489583,4.32087028158809,
18.1655158413832));
#218084=CARTESIAN_POINT('Ctrl Pts',(-6.63372543031743,4.31017778613808,
18.1660306621788));
#218085=CARTESIAN_POINT('Ctrl Pts',(-6.63642821456398,4.30601511674972,
18.1662312395067));
#218086=CARTESIAN_POINT('Ctrl Pts',(-6.64125779764992,4.29856152900336,
18.1665906599341));
#218087=CARTESIAN_POINT('Ctrl Pts',(-6.64338607446431,4.29527156521906,
18.1667494000091));
#218088=CARTESIAN_POINT('Ctrl Pts',(-6.64788389208938,4.2883073434912,18.1670856193968));
#218089=CARTESIAN_POINT('Ctrl Pts',(-6.6502528321763,4.28463270105201,18.1672631400872));
#218090=CARTESIAN_POINT('Ctrl Pts',(-6.65653732615097,4.27486657842691,
18.167735241838));
#218091=CARTESIAN_POINT('Ctrl Pts',(-6.66044755655857,4.26877169493221,
18.1680301866821));
#218092=CARTESIAN_POINT('Ctrl Pts',(-6.67842522718944,4.24066503005928,
18.169391741989));
#218093=CARTESIAN_POINT('Ctrl Pts',(-6.69239180785445,4.21858925136638,
18.170465130678));
#218094=CARTESIAN_POINT('Ctrl Pts',(-6.79808284028377,4.04968668031033,
18.1787055074252));
#218095=CARTESIAN_POINT('Ctrl Pts',(-6.88506936362933,3.89996217116627,
18.1861696038195));
#218096=CARTESIAN_POINT('Ctrl Pts',(-7.03269744742566,3.62550428521574,
18.1999697160386));
#218097=CARTESIAN_POINT('Ctrl Pts',(-7.09510734782595,3.50179438647836,
18.2062311853947));
#218098=CARTESIAN_POINT('Ctrl Pts',(-7.54810672283103,2.54196902095565,
18.2547946016206));
#218099=CARTESIAN_POINT('Ctrl Pts',(-7.79304169727483,1.64462231686705,
18.2990276855453));
#218100=CARTESIAN_POINT('Ctrl Pts',(-7.88149309390995,0.683896519358582,
18.3391263512647));
#218101=CARTESIAN_POINT('Ctrl Pts',(-7.88497679169827,0.642486500084795,
18.3408433137367));
#218102=CARTESIAN_POINT('Ctrl Pts',(-7.89257334162507,0.542790049007174,
18.3449498826676));
#218103=CARTESIAN_POINT('Ctrl Pts',(-7.89636707329895,0.484481399242725,
18.3473294003498));
#218104=CARTESIAN_POINT('Ctrl Pts',(-7.90024278748618,0.412635049269635,
18.3502347043649));
#218105=CARTESIAN_POINT('Ctrl Pts',(-7.90093644115714,0.399132985684674,
18.3507795393431));
#218106=CARTESIAN_POINT('Ctrl Pts',(-7.90202878927546,0.376750620175531,
18.3516808078834));
#218107=CARTESIAN_POINT('Ctrl Pts',(-7.90244713368098,0.367871331287926,
18.3520378527977));
#218108=CARTESIAN_POINT('Ctrl Pts',(-7.90315779313715,0.352226843907147,
18.3526660630081));
#218109=CARTESIAN_POINT('Ctrl Pts',(-7.90345638917552,0.345461947958117,
18.3529374233963));
#218110=CARTESIAN_POINT('Ctrl Pts',(-7.90403589271197,0.331938788771921,
18.3534793078982));
#218111=CARTESIAN_POINT('Ctrl Pts',(-7.90431681896681,0.325180532104748,
18.3537498323726));
#218112=CARTESIAN_POINT('Ctrl Pts',(-7.90490883545092,0.310484159625379,
18.3543374935094));
#218113=CARTESIAN_POINT('Ctrl Pts',(-7.90521663713799,0.302545914787239,
18.354654527851));
#218114=CARTESIAN_POINT('Ctrl Pts',(-7.90593743813165,0.283203885276079,
18.3554260549983));
#218115=CARTESIAN_POINT('Ctrl Pts',(-7.90633772230234,0.271799629455422,
18.3558801533904));
#218116=CARTESIAN_POINT('Ctrl Pts',(-7.90777074649013,0.228286764508202,
18.3576097295215));
#218117=CARTESIAN_POINT('Ctrl Pts',(-7.90863258422699,0.196172638484583,
18.3588799192196));
#218118=CARTESIAN_POINT('Ctrl Pts',(-7.91042368178897,0.109820990047875,
18.362278829094));
#218119=CARTESIAN_POINT('Ctrl Pts',(-7.91099075449839,0.0555774990504133,
18.3643964145847));
#218120=CARTESIAN_POINT('Ctrl Pts',(-7.91099988786644,0.00133198240303771,
18.3664974980729));
#218121=CARTESIAN_POINT('',(-7.91099433110756,0.00947064855683299,22.3535317449623));
#218122=CARTESIAN_POINT('Ctrl Pts',(-7.91099988478435,0.00135016367355217,
18.3664967938599));
#218123=CARTESIAN_POINT('Ctrl Pts',(-7.91115913952513,-0.93176947257981,
18.402639240933));
#218124=CARTESIAN_POINT('Ctrl Pts',(-7.74625062688717,-1.85749765228585,
18.4325732657663));
#218125=CARTESIAN_POINT('Ctrl Pts',(-7.33513467715508,-2.97416559759076,
18.475745801834));
#218126=CARTESIAN_POINT('Ctrl Pts',(-7.23475610488461,-3.21063296551924,
18.4854408182715));
#218127=CARTESIAN_POINT('Ctrl Pts',(-7.1142579140074,-3.4600090221591,18.4964894798939));
#218128=CARTESIAN_POINT('Ctrl Pts',(-7.10541019306603,-3.47814233175404,
18.4972971599541));
#218129=CARTESIAN_POINT('Ctrl Pts',(-7.09245985157269,-3.5044282765506,
18.4984740239186));
#218130=CARTESIAN_POINT('Ctrl Pts',(-7.0884123018454,-3.51260805241907,
18.4988411003412));
#218131=CARTESIAN_POINT('Ctrl Pts',(-7.08130936149064,-3.52690025716869,
18.4994839558376));
#218132=CARTESIAN_POINT('Ctrl Pts',(-7.07826018428449,-3.53301577415346,
18.499759502394));
#218133=CARTESIAN_POINT('Ctrl Pts',(-7.07234163031472,-3.5448477789195,
18.5002935259715));
#218134=CARTESIAN_POINT('Ctrl Pts',(-7.06947323642752,-3.55056475377522,
18.5005519667374));
#218135=CARTESIAN_POINT('Ctrl Pts',(-7.06263574176736,-3.5641513806774,
18.5011671331627));
#218136=CARTESIAN_POINT('Ctrl Pts',(-7.05866041999558,-3.57201788346468,
18.5015240835875));
#218137=CARTESIAN_POINT('Ctrl Pts',(-7.04667269843559,-3.59564143994581,
18.5025983319648));
#218138=CARTESIAN_POINT('Ctrl Pts',(-7.03862064736651,-3.61137824947899,
18.5033170300506));
#218139=CARTESIAN_POINT('Ctrl Pts',(-6.95315121321176,-3.77704675309989,
18.51091491882));
#218140=CARTESIAN_POINT('Ctrl Pts',(-6.87101047988283,-3.92448794007304,
18.5179512888794));
#218141=CARTESIAN_POINT('Ctrl Pts',(-6.71256541137726,-4.18865051896204,
18.5309603610538));
#218142=CARTESIAN_POINT('Ctrl Pts',(-6.63776753007232,-4.30620120436085,
18.5369025949031));
#218143=CARTESIAN_POINT('Ctrl Pts',(-6.52916878006164,-4.46731465751185,
18.5452282556834));
#218144=CARTESIAN_POINT('Ctrl Pts',(-6.49795694959084,-4.51259356235029,
18.5475887696759));
#218145=CARTESIAN_POINT('Ctrl Pts',(-6.28527527934746,-4.8143478705476,
18.5634513492042));
#218146=CARTESIAN_POINT('Ctrl Pts',(-6.08913477802393,-5.0601455121102,
18.5769993967422));
#218147=CARTESIAN_POINT('Ctrl Pts',(-5.64215614832003,-5.55654257192806,
18.6054902147358));
#218148=CARTESIAN_POINT('Ctrl Pts',(-5.38804073534318,-5.80328534622556,
18.6203555815865));
#218149=CARTESIAN_POINT('Ctrl Pts',(-4.83845037421414,-6.26960727931723,
18.6502432655373));
#218150=CARTESIAN_POINT('Ctrl Pts',(-4.54245300336523,-6.48727296774719,
18.6653107839227));
#218151=CARTESIAN_POINT('Ctrl Pts',(-4.19253084360786,-6.70886241736414,
18.6820841447806));
#218152=CARTESIAN_POINT('Ctrl Pts',(-4.1524198290262,-6.73376264849548,
18.6839918036046));
#218153=CARTESIAN_POINT('Ctrl Pts',(-4.09116656238656,-6.77103219012437,
18.6868823373086));
#218154=CARTESIAN_POINT('Ctrl Pts',(-4.07018590320014,-6.78366475284956,
18.6878684239068));
#218155=CARTESIAN_POINT('Ctrl Pts',(-4.0319917807993,-6.80642064851768,
18.689656349691));
#218156=CARTESIAN_POINT('Ctrl Pts',(-4.01479801417763,-6.81657660948537,
18.6904585905905));
#218157=CARTESIAN_POINT('Ctrl Pts',(-3.97765771143759,-6.83832526097283,
18.6921858919366));
#218158=CARTESIAN_POINT('Ctrl Pts',(-3.95769853468321,-6.84989602526038,
18.6931106690872));
#218159=CARTESIAN_POINT('Ctrl Pts',(-3.90412178559349,-6.88064327951778,
18.6955838471163));
#218160=CARTESIAN_POINT('Ctrl Pts',(-3.87041356194284,-6.89966069714503,
18.6971302014744));
#218161=CARTESIAN_POINT('Ctrl Pts',(-3.70600453535699,-6.99083257379868,
18.704626328575));
#218162=CARTESIAN_POINT('Ctrl Pts',(-3.57341725905485,-7.05952547009614,
18.7105303120116));
#218163=CARTESIAN_POINT('Ctrl Pts',(-2.97324397932429,-7.34922940900218,
18.7366930187995));
#218164=CARTESIAN_POINT('Ctrl Pts',(-2.48660803953748,-7.52782393940463,
18.7563310566229));
#218165=CARTESIAN_POINT('Ctrl Pts',(-1.81910216947437,-7.70094331671891,
18.7829684336073));
#218166=CARTESIAN_POINT('Ctrl Pts',(-1.65080460185735,-7.738766237814,18.7896693023064));
#218167=CARTESIAN_POINT('Ctrl Pts',(-1.39977847187603,-7.78661973499417,
18.7997488734291));
#218168=CARTESIAN_POINT('Ctrl Pts',(-1.31790901964077,-7.80089367498487,
18.8030495767753));
#218169=CARTESIAN_POINT('Ctrl Pts',(-1.21752849416448,-7.81676971183015,
18.8071237155196));
#218170=CARTESIAN_POINT('Ctrl Pts',(-1.19921601069593,-7.81960007400795,
18.8078680844331));
#218171=CARTESIAN_POINT('Ctrl Pts',(-1.16980652823982,-7.8240398397127,
18.8090653669125));
#218172=CARTESIAN_POINT('Ctrl Pts',(-1.15871582910239,-7.82569002410157,
18.8095172896549));
#218173=CARTESIAN_POINT('Ctrl Pts',(-1.13754706035839,-7.82879373628687,
18.8103806325824));
#218174=CARTESIAN_POINT('Ctrl Pts',(-1.1274696145841,-7.83025139745363,
18.8107919575086));
#218175=CARTESIAN_POINT('Ctrl Pts',(-1.10442226384094,-7.83353968730601,
18.8117333947354));
#218176=CARTESIAN_POINT('Ctrl Pts',(-1.09145058039057,-7.83535756673221,
18.8122637880096));
#218177=CARTESIAN_POINT('Ctrl Pts',(-1.05760186042179,-7.84001551151188,
18.8136491308801));
#218178=CARTESIAN_POINT('Ctrl Pts',(-1.03671792768029,-7.84280439947771,
18.8145051643668));
#218179=CARTESIAN_POINT('Ctrl Pts',(-0.899734372558705,-7.86054079557132,
18.8201281243445));
#218180=CARTESIAN_POINT('Ctrl Pts',(-0.783327871189056,-7.87299308963963,
18.8249439046932));
#218181=CARTESIAN_POINT('Ctrl Pts',(-0.213703552831976,-7.92116885966793,
18.8486252761663));
#218182=CARTESIAN_POINT('Ctrl Pts',(0.24174137508306,-7.92036287116089,
18.8678721906608));
#218183=CARTESIAN_POINT('Ctrl Pts',(1.00541812397437,-7.85305160507057,
18.8998826604197));
#218184=CARTESIAN_POINT('Ctrl Pts',(1.31435854628966,-7.80728862433748,
18.9127700839643));
#218185=CARTESIAN_POINT('Ctrl Pts',(1.69253212656578,-7.72818079147799,
18.9284874713727));
#218186=CARTESIAN_POINT('Ctrl Pts',(1.76505262311285,-7.71194091742455,
18.9314994482547));
#218187=CARTESIAN_POINT('Ctrl Pts',(1.86927515056508,-7.68705469088483,
18.9358270746457));
#218188=CARTESIAN_POINT('Ctrl Pts',(1.90116861851135,-7.67922895245231,
18.937151252008));
#218189=CARTESIAN_POINT('Ctrl Pts',(1.9567910150461,-7.66521305913183,18.9394606444427));
#218190=CARTESIAN_POINT('Ctrl Pts',(1.98054157131064,-7.65911074520033,
18.9404467529206));
#218191=CARTESIAN_POINT('Ctrl Pts',(2.02653558668333,-7.6470650964517,18.9423565368898));
#218192=CARTESIAN_POINT('Ctrl Pts',(2.04878222678175,-7.64113489373845,
18.9432803358976));
#218193=CARTESIAN_POINT('Ctrl Pts',(2.10192917437701,-7.62671892516321,
18.9454875741516));
#218194=CARTESIAN_POINT('Ctrl Pts',(2.13280446483298,-7.61814235504656,
18.9467700891275));
#218195=CARTESIAN_POINT('Ctrl Pts',(2.24590940118031,-7.58598245111726,
18.9514698040529));
#218196=CARTESIAN_POINT('Ctrl Pts',(2.32780747633226,-7.56125328908962,
18.9548756841669));
#218197=CARTESIAN_POINT('Ctrl Pts',(2.93191664336227,-7.36809672603653,
18.980047653073));
#218198=CARTESIAN_POINT('Ctrl Pts',(3.43577363822072,-7.14706256497588,
19.0013884629811));
#218199=CARTESIAN_POINT('Ctrl Pts',(4.23830843990542,-6.69036722695345,
19.0362271313472));
#218200=CARTESIAN_POINT('Ctrl Pts',(4.55033791160038,-6.48218312783275,
19.0500429369366));
#218201=CARTESIAN_POINT('Ctrl Pts',(5.11648357670775,-6.0433641097861,19.0766947732885));
#218202=CARTESIAN_POINT('Ctrl Pts',(5.37266927478679,-5.81679072891381,
19.0894903356786));
#218203=CARTESIAN_POINT('Ctrl Pts',(5.63364305523964,-5.55399071943741,
19.1041214108656));
#218204=CARTESIAN_POINT('Ctrl Pts',(5.65378287549411,-5.53348770293115,
19.1052617436981));
#218205=CARTESIAN_POINT('Ctrl Pts',(5.68824582176904,-5.49801869579115,
19.1072333252215));
#218206=CARTESIAN_POINT('Ctrl Pts',(5.70262277772041,-5.4831052838322,19.1080619644604));
#218207=CARTESIAN_POINT('Ctrl Pts',(5.72294106811683,-5.46186249235418,
19.1092420701152));
#218208=CARTESIAN_POINT('Ctrl Pts',(5.72893088045403,-5.45557946700145,
19.1095910859627));
#218209=CARTESIAN_POINT('Ctrl Pts',(5.73921145993667,-5.44476003216063,
19.1101920730499));
#218210=CARTESIAN_POINT('Ctrl Pts',(5.74350722721105,-5.44022837024231,
19.1104437866939));
#218211=CARTESIAN_POINT('Ctrl Pts',(5.75168961905515,-5.43157616266721,
19.1109243756278));
#218212=CARTESIAN_POINT('Ctrl Pts',(5.75557719420145,-5.42745651720956,
19.111153201165));
#218213=CARTESIAN_POINT('Ctrl Pts',(5.76462564571406,-5.41784726024587,
19.1116869532443));
#218214=CARTESIAN_POINT('Ctrl Pts',(5.76978310471141,-5.41235445020171,
19.1119920595269));
#218215=CARTESIAN_POINT('Ctrl Pts',(5.78737933147483,-5.39356033817725,
19.1130360537816));
#218216=CARTESIAN_POINT('Ctrl Pts',(5.79977995511999,-5.38022351883813,
19.1137769817191));
#218217=CARTESIAN_POINT('Ctrl Pts',(5.96965556164268,-5.19625323140725,
19.1240003535394));
#218218=CARTESIAN_POINT('Ctrl Pts',(6.11956056867999,-5.01884264982179,
19.1339570344492));
#218219=CARTESIAN_POINT('Ctrl Pts',(6.66922081269003,-4.3070379026706,19.1737745401103));
#218220=CARTESIAN_POINT('Ctrl Pts',(7.00857184624998,-3.72948711151417,
19.2054363194764));
#218221=CARTESIAN_POINT('Ctrl Pts',(7.42077676716266,-2.7676321216702,19.2522662244487));
#218222=CARTESIAN_POINT('Ctrl Pts',(7.54490312634706,-2.40877573281266,
19.2686423991422));
#218223=CARTESIAN_POINT('Ctrl Pts',(7.65206670126215,-2.00775489843252,
19.285667207868));
#218224=CARTESIAN_POINT('Ctrl Pts',(7.66108078447154,-1.97308027937703,
19.2871293770324));
#218225=CARTESIAN_POINT('Ctrl Pts',(7.67421383668803,-1.92111396659172,
19.2893060728995));
#218226=CARTESIAN_POINT('Ctrl Pts',(7.67851052542316,-1.90386790506852,
19.2900260504147));
#218227=CARTESIAN_POINT('Ctrl Pts',(7.6853094652972,-1.8761808791694,19.2911780834312));
#218228=CARTESIAN_POINT('Ctrl Pts',(7.68784863244946,-1.86574909203476,
19.2916112711375));
#218229=CARTESIAN_POINT('Ctrl Pts',(7.69265147859991,-1.84584104174467,
19.2924363161049));
#218230=CARTESIAN_POINT('Ctrl Pts',(7.6949189022797,-1.83636570725299,19.2928282876486));
#218231=CARTESIAN_POINT('Ctrl Pts',(7.69888555652324,-1.819653113123,19.2935183961487));
#218232=CARTESIAN_POINT('Ctrl Pts',(7.70059209853602,-1.81241761105669,
19.2938167568333));
#218233=CARTESIAN_POINT('Ctrl Pts',(7.70391879305557,-1.79822336728175,
19.2944012589736));
#218234=CARTESIAN_POINT('Ctrl Pts',(7.7055397218824,-1.79126481666798,19.2946874239375));
#218235=CARTESIAN_POINT('Ctrl Pts',(7.70938724769102,-1.77464575281496,
19.2953699661643));
#218236=CARTESIAN_POINT('Ctrl Pts',(7.7116051192622,-1.76498322040901,19.2957660761962));
#218237=CARTESIAN_POINT('Ctrl Pts',(7.71947487864257,-1.73039926526118,
19.2971812326588));
#218238=CARTESIAN_POINT('Ctrl Pts',(7.72502419679118,-1.70545454149892,
19.2981971426909));
#218239=CARTESIAN_POINT('Ctrl Pts',(7.80439777401764,-1.34032523417243,
19.3129981917866));
#218240=CARTESIAN_POINT('Ctrl Pts',(7.85581443988878,-0.995643531176569,
19.3260684634179));
#218241=CARTESIAN_POINT('Ctrl Pts',(7.90742131691975,-0.368379645686695,
19.3488064406817));
#218242=CARTESIAN_POINT('Ctrl Pts',(7.91551921976296,-0.0870530682486353,
19.3586347939389));
#218243=CARTESIAN_POINT('Ctrl Pts',(7.89800906097888,0.626353289272118,
19.3833479612142));
#218244=CARTESIAN_POINT('Ctrl Pts',(7.85198267404627,1.05697837594131,19.3980564830445));
#218245=CARTESIAN_POINT('Ctrl Pts',(7.72969810845085,1.69833483242862,19.4217884829383));
#218246=CARTESIAN_POINT('Ctrl Pts',(7.67934506566328,1.91317056795507,19.430063907437));
#218247=CARTESIAN_POINT('Ctrl Pts',(7.61129410602145,2.15712626801572,19.4400823283802));
#218248=CARTESIAN_POINT('Ctrl Pts',(7.60230684550761,2.18858909984918,19.4413865434531));
#218249=CARTESIAN_POINT('Ctrl Pts',(7.5905058137588,2.22895257780103,19.4430745568355));
#218250=CARTESIAN_POINT('Ctrl Pts',(7.5878709656063,2.23790578688966,19.4434499235521));
#218251=CARTESIAN_POINT('Ctrl Pts',(7.58360268418897,2.25231520143772,19.444055535564));
#218252=CARTESIAN_POINT('Ctrl Pts',(7.5819791859609,2.25777436022152,19.4442853232697));
#218253=CARTESIAN_POINT('Ctrl Pts',(7.57887799549317,2.26816132502367,19.4447231837878));
#218254=CARTESIAN_POINT('Ctrl Pts',(7.57740138831986,2.2730894542476,19.4449312072538));
#218255=CARTESIAN_POINT('Ctrl Pts',(7.57402734311617,2.2843104004534,19.4454054899613));
#218256=CARTESIAN_POINT('Ctrl Pts',(7.57212686931596,2.29060229514045,19.4456718852432));
#218257=CARTESIAN_POINT('Ctrl Pts',(7.56644911008027,2.30931535700076,19.4464655155457));
#218258=CARTESIAN_POINT('Ctrl Pts',(7.56264909809753,2.32172956430267,19.4469937527857));
#218259=CARTESIAN_POINT('Ctrl Pts',(7.53601424635286,2.40798338908755,19.4506758101268));
#218260=CARTESIAN_POINT('Ctrl Pts',(7.51212938856055,2.48149274529982,19.453874324933));
#218261=CARTESIAN_POINT('Ctrl Pts',(7.33940042586255,2.98772929277415,19.476267391495));
#218262=CARTESIAN_POINT('Ctrl Pts',(7.15433387048857,3.40717106135049,19.4966171699505));
#218263=CARTESIAN_POINT('Ctrl Pts',(6.76768100932711,4.11118799554153,19.5319333696045));
#218264=CARTESIAN_POINT('Ctrl Pts',(6.58162534955884,4.40290818516588,19.5469758080647));
#218265=CARTESIAN_POINT('Ctrl Pts',(6.27446864134037,4.82131002998187,19.5689359944092));
#218266=CARTESIAN_POINT('Ctrl Pts',(6.16728727745257,4.95767666270367,19.5761659469251));
#218267=CARTESIAN_POINT('Ctrl Pts',(5.99111129211771,5.167260839965,19.587409994742));
#218268=CARTESIAN_POINT('Ctrl Pts',(5.92505672531264,5.24287158785245,19.5914956734813));
#218269=CARTESIAN_POINT('Ctrl Pts',(5.84092050011597,5.33555836502391,19.5965472277717));
#218270=CARTESIAN_POINT('Ctrl Pts',(5.82417478916609,5.35383258879095,19.5975453546343));
#218271=CARTESIAN_POINT('Ctrl Pts',(5.79749993295642,5.38266900851745,19.5991239664494));
#218272=CARTESIAN_POINT('Ctrl Pts',(5.78762720404809,5.39328308884937,19.599705797346));
#218273=CARTESIAN_POINT('Ctrl Pts',(5.76991758882429,5.41221790643816,19.6007451749863));
#218274=CARTESIAN_POINT('Ctrl Pts',(5.76209174468442,5.42054889980848,19.6012029815743));
#218275=CARTESIAN_POINT('Ctrl Pts',(5.74410208738454,5.43961678725398,19.6022519735008));
#218276=CARTESIAN_POINT('Ctrl Pts',(5.73392616880704,5.45034221630158,19.6028428718792));
#218277=CARTESIAN_POINT('Ctrl Pts',(5.70561494860836,5.48001523298295,19.6044800958982));
#218278=CARTESIAN_POINT('Ctrl Pts',(5.68741535867653,5.49890129410917,19.6055249214135));
#218279=CARTESIAN_POINT('Ctrl Pts',(5.60063599962763,5.58806219285022,19.610471430596));
#218280=CARTESIAN_POINT('Ctrl Pts',(5.53084484656556,5.65714755327642,19.6143455111531));
#218281=CARTESIAN_POINT('Ctrl Pts',(5.20900942805888,5.96407816705975,19.6317566789819));
#218282=CARTESIAN_POINT('Ctrl Pts',(4.94278493607555,6.18650958866493,19.6449139702574));
#218283=CARTESIAN_POINT('Ctrl Pts',(4.24926817039201,6.69251178863727,19.6769018021472));
#218284=CARTESIAN_POINT('Ctrl Pts',(3.80741566888015,6.95338434965661,19.6953251887285));
#218285=CARTESIAN_POINT('Ctrl Pts',(3.19331518712385,7.23975903988982,19.7208282012629));
#218286=CARTESIAN_POINT('Ctrl Pts',(3.04099545569801,7.30504731325001,19.7271542022879));
#218287=CARTESIAN_POINT('Ctrl Pts',(2.81638952548769,7.39307655842408,19.7365983951208));
#218288=CARTESIAN_POINT('Ctrl Pts',(2.74564559993629,7.41964020427929,19.7395895001563));
#218289=CARTESIAN_POINT('Ctrl Pts',(2.66197343911482,7.44969774688287,19.7431558737268));
#218290=CARTESIAN_POINT('Ctrl Pts',(2.64940211145755,7.45417785939972,19.7436924599653));
#218291=CARTESIAN_POINT('Ctrl Pts',(2.63012397104017,7.46099318662085,19.7445165412959));
#218292=CARTESIAN_POINT('Ctrl Pts',(2.62342521601794,7.46335122913246,19.7448031188863));
#218293=CARTESIAN_POINT('Ctrl Pts',(2.61173978571683,7.46744696521154,19.7453034363137));
#218294=CARTESIAN_POINT('Ctrl Pts',(2.60675452299177,7.46918869377547,19.7455170115554));
#218295=CARTESIAN_POINT('Ctrl Pts',(2.59554004676288,7.47309416176346,19.7459977502483));
#218296=CARTESIAN_POINT('Ctrl Pts',(2.58930986876329,7.47525510521967,19.7462650285767));
#218297=CARTESIAN_POINT('Ctrl Pts',(2.57264826612155,7.48101086995242,19.7469803833945));
#218298=CARTESIAN_POINT('Ctrl Pts',(2.56221203357467,7.4845916542505,19.7474290446012));
#218299=CARTESIAN_POINT('Ctrl Pts',(2.51732314565953,7.49988862825384,19.7493614872902));
#218300=CARTESIAN_POINT('Ctrl Pts',(2.48279773600636,7.51138872613442,19.7508544559496));
#218301=CARTESIAN_POINT('Ctrl Pts',(1.94822871550004,7.68536053016548,19.7740875340796));
#218302=CARTESIAN_POINT('Ctrl Pts',(1.43338396258432,7.79779192508504,19.7983356054488));
#218303=CARTESIAN_POINT('Ctrl Pts',(0.750881799979827,7.87693980052665,
19.8299691452143));
#218304=CARTESIAN_POINT('Ctrl Pts',(0.589920483933854,7.89062729225981,
19.8373972286174));
#218305=CARTESIAN_POINT('Ctrl Pts',(0.0926095563395046,7.9176133539248,
19.8601090107858));
#218306=CARTESIAN_POINT('Ctrl Pts',(-0.244273348460455,7.91438809406514,
19.8751423896768));
#218307=CARTESIAN_POINT('Ctrl Pts',(-0.739068114120515,7.87801718912681,
19.8963783846863));
#218308=CARTESIAN_POINT('Ctrl Pts',(-0.897801805706668,7.86150954990597,
19.9030656575271));
#218309=CARTESIAN_POINT('Ctrl Pts',(-1.10706140818153,7.83332607715578,
19.9117114817328));
#218310=CARTESIAN_POINT('Ctrl Pts',(-1.15812052083219,7.82594015999699,
19.9138076758021));
#218311=CARTESIAN_POINT('Ctrl Pts',(-1.22224268985226,7.81602332073487,
19.9164235814831));
#218312=CARTESIAN_POINT('Ctrl Pts',(-1.23537587429331,7.81395829235747,
19.9169584822217));
#218313=CARTESIAN_POINT('Ctrl Pts',(-1.25624212914935,7.81062341453613,
19.9178069580068));
#218314=CARTESIAN_POINT('Ctrl Pts',(-1.26397859693608,7.80937516820079,
19.9181212399443));
#218315=CARTESIAN_POINT('Ctrl Pts',(-1.27852982873629,7.8070051989157,19.9187117934291));
#218316=CARTESIAN_POINT('Ctrl Pts',(-1.28534499998096,7.80588604389105,
19.9189881488892));
#218317=CARTESIAN_POINT('Ctrl Pts',(-1.30063800741792,7.80335412774052,
19.9196077566529));
#218318=CARTESIAN_POINT('Ctrl Pts',(-1.30911503066057,7.80193647156822,
19.9199508478283));
#218319=CARTESIAN_POINT('Ctrl Pts',(-1.33061856793118,7.79830429132077,
19.9208202481394));
#218320=CARTESIAN_POINT('Ctrl Pts',(-1.34364189862826,7.79607093630254,
19.9213459372932));
#218321=CARTESIAN_POINT('Ctrl Pts',(-1.41493531726343,7.78366096422403,
19.9242190814441));
#218322=CARTESIAN_POINT('Ctrl Pts',(-1.47309619834195,7.77286354876746,
19.9265460185952));
#218323=CARTESIAN_POINT('Ctrl Pts',(-2.44844572863632,7.58045168564622,
19.9652958194041));
#218324=CARTESIAN_POINT('Ctrl Pts',(-3.32625998410969,7.23836562082014,
19.9949453023875));
#218325=CARTESIAN_POINT('Ctrl Pts',(-4.293346126716,6.64758972347121,20.0340323555139));
#218326=CARTESIAN_POINT('Ctrl Pts',(-4.45866952752661,6.53785359401399,
20.0410243303857));
#218327=CARTESIAN_POINT('Ctrl Pts',(-4.74865554143482,6.32925204963865,
20.0541620798706));
#218328=CARTESIAN_POINT('Ctrl Pts',(-4.8747934221936,6.23261938609712,20.0601966652247));
#218329=CARTESIAN_POINT('Ctrl Pts',(-5.01682577456608,6.11685984872732,
20.0674725081515));
#218330=CARTESIAN_POINT('Ctrl Pts',(-5.0356506361448,6.10137180530029,20.0684469015648));
#218331=CARTESIAN_POINT('Ctrl Pts',(-5.05966581824736,6.08142660914316,
20.0697032978819));
#218332=CARTESIAN_POINT('Ctrl Pts',(-5.06492253958996,6.07704923973013,
20.069979136338));
#218333=CARTESIAN_POINT('Ctrl Pts',(-5.07335737880369,6.07000684594348,
20.0704230780638));
#218334=CARTESIAN_POINT('Ctrl Pts',(-5.07653910021436,6.06734612221237,
20.0705908443267));
#218335=CARTESIAN_POINT('Ctrl Pts',(-5.08257698970345,6.0622888453903,20.0709097958613));
#218336=CARTESIAN_POINT('Ctrl Pts',(-5.08543356001441,6.05989277197123,
20.071060943235));
#218337=CARTESIAN_POINT('Ctrl Pts',(-5.09192095375131,6.05444336884073,
20.0714047742904));
#218338=CARTESIAN_POINT('Ctrl Pts',(-5.09555070241924,6.05138881123872,
20.0715975564809));
#218339=CARTESIAN_POINT('Ctrl Pts',(-5.10499414418457,6.04342731109227,
20.0721001739626));
#218340=CARTESIAN_POINT('Ctrl Pts',(-5.11080346560196,6.03851528206595,
20.0724104152236));
#218341=CARTESIAN_POINT('Ctrl Pts',(-5.14703864484835,6.00778714623434,
20.0743520040089));
#218342=CARTESIAN_POINT('Ctrl Pts',(-5.17727538420419,5.98174996867785,
20.0760007739786));
#218343=CARTESIAN_POINT('Ctrl Pts',(-5.7095678509391,5.51632803470183,20.1055127140682));
#218344=CARTESIAN_POINT('Ctrl Pts',(-6.15423095249231,5.01542018242688,
20.1376510456358));
#218345=CARTESIAN_POINT('Ctrl Pts',(-6.83867378485568,4.01424623852371,
20.193830262923));
#218346=CARTESIAN_POINT('Ctrl Pts',(-7.09921848528766,3.53311406394057,
20.2181572790312));
#218347=CARTESIAN_POINT('Ctrl Pts',(-7.32813036484757,2.98079524870643,
20.2426123867452));
#218348=CARTESIAN_POINT('Ctrl Pts',(-7.34760086507924,2.93247278468919,
20.2447259042483));
#218349=CARTESIAN_POINT('Ctrl Pts',(-7.37132186341728,2.87188148432562,
20.2473440655732));
#218350=CARTESIAN_POINT('Ctrl Pts',(-7.37602113180862,2.85979047125106,
20.2478649406148));
#218351=CARTESIAN_POINT('Ctrl Pts',(-7.38341292886023,2.84063227376752,
20.2486877794603));
#218352=CARTESIAN_POINT('Ctrl Pts',(-7.38612508911111,2.83357272030832,
20.2489904516954));
#218353=CARTESIAN_POINT('Ctrl Pts',(-7.3911902850637,2.82033170334348,20.2495571521993));
#218354=CARTESIAN_POINT('Ctrl Pts',(-7.39354569841451,2.81415116023561,
20.2498212660011));
#218355=CARTESIAN_POINT('Ctrl Pts',(-7.39879151309521,2.80033423259518,
20.2504108008889));
#218356=CARTESIAN_POINT('Ctrl Pts',(-7.40167785063667,2.79269630723452,
20.2507360755296));
#218357=CARTESIAN_POINT('Ctrl Pts',(-7.40892907955581,2.77341764838255,
20.2515555408771));
#218358=CARTESIAN_POINT('Ctrl Pts',(-7.41327837291874,2.76177104876626,
20.2520491710258));
#218359=CARTESIAN_POINT('Ctrl Pts',(-7.43633450594891,2.69958411244033,
20.2546773562784));
#218360=CARTESIAN_POINT('Ctrl Pts',(-7.45455222123624,2.64886326568902,
20.2567943716127));
#218361=CARTESIAN_POINT('Ctrl Pts',(-7.76383412578447,1.75930673492556,
20.2934736017286));
#218362=CARTESIAN_POINT('Ctrl Pts',(-7.91212168501964,0.877724371696439,
20.3218504654584));
#218363=CARTESIAN_POINT('Ctrl Pts',(-7.9109860860975,-0.0159761828078189,
20.3531105060327));
#218364=CARTESIAN_POINT('Ctrl Pts',(-7.91097190483238,-0.0219000838148015,
20.3533178653847));
#218365=CARTESIAN_POINT('Ctrl Pts',(-7.91093271805898,-0.0330417282952556,
20.3537081602693));
#218366=CARTESIAN_POINT('Ctrl Pts',(-7.91090920425387,-0.0382594749948222,
20.3538910608219));
#218367=CARTESIAN_POINT('Ctrl Pts',(-7.91085671392213,-0.0478103392606033,
20.354226080611));
#218368=CARTESIAN_POINT('Ctrl Pts',(-7.91082933931471,-0.0521434649049955,
20.3543781614645));
#218369=CARTESIAN_POINT('Ctrl Pts',(-7.91077500806176,-0.0597537649582373,
20.3546454162844));
#218370=CARTESIAN_POINT('Ctrl Pts',(-7.91074957509471,-0.0630309504684151,
20.3547605530863));
#218371=CARTESIAN_POINT('Ctrl Pts',(-7.91070375574369,-0.0684973121570124,
20.3549526868767));
#218372=CARTESIAN_POINT('Ctrl Pts',(-7.91068449704923,-0.0706864983443649,
20.355029655987));
#218373=CARTESIAN_POINT('Ctrl Pts',(-7.91065244772581,-0.0741654566928713,
20.3551520084347));
#218374=CARTESIAN_POINT('Ctrl Pts',(-7.91064025039873,-0.0754552347215277,
20.3551973769727));
#218375=CARTESIAN_POINT('Ctrl Pts',(-7.9106210391236,-0.0774354709228726,
20.3552670450185));
#218376=CARTESIAN_POINT('Ctrl Pts',(-7.91061425020951,-0.0781259314439278,
20.355291338883));
#218377=CARTESIAN_POINT('Ctrl Pts',(-7.91060389694048,-0.0791650635999006,
20.3553279042374));
#218378=CARTESIAN_POINT('Ctrl Pts',(-7.91060039993006,-0.0795137359895382,
20.3553401740347));
#218379=CARTESIAN_POINT('Ctrl Pts',(-7.91059515665141,-0.0800330975359515,
20.3553584512692));
#218380=CARTESIAN_POINT('Ctrl Pts',(-7.91059342791128,-0.0802037868481622,
20.3553644582636));
#218381=CARTESIAN_POINT('Ctrl Pts',(-7.91021163026892,-0.117780955681033,
20.3566869262875));
#218382=CARTESIAN_POINT('Ctrl Pts',(-7.90956625051917,-0.155184018494225,
20.3580100540781));
#218383=CARTESIAN_POINT('Ctrl Pts',(-7.90225486069639,-0.455438532159219,
20.3686955101006));
#218384=CARTESIAN_POINT('Ctrl Pts',(-7.88275371481392,-0.717793124483094,
20.3784232310423));
#218385=CARTESIAN_POINT('Ctrl Pts',(-7.84826578401422,-0.994433342120351,
20.3895559488599));
#218386=CARTESIAN_POINT('Ctrl Pts',(-7.84625256633663,-1.01019510695341,
20.3901932917789));
#218387=CARTESIAN_POINT('Ctrl Pts',(-7.8434751755752,-1.0314304192876,20.3910561723516));
#218388=CARTESIAN_POINT('Ctrl Pts',(-7.84275275217372,-1.03690925719923,
20.3912791757272));
#218389=CARTESIAN_POINT('Ctrl Pts',(-7.84152088491908,-1.04617676565502,
20.3916570174797));
#218390=CARTESIAN_POINT('Ctrl Pts',(-7.84101443374242,-1.04996583913891,
20.3918116782628));
#218391=CARTESIAN_POINT('Ctrl Pts',(-7.84003558043433,-1.05724903860938,
20.3921093011222));
#218392=CARTESIAN_POINT('Ctrl Pts',(-7.83956358819452,-1.06074321996108,
20.3922522390309));
#218393=CARTESIAN_POINT('Ctrl Pts',(-7.83844739542212,-1.06896501090112,
20.3925889238262));
#218394=CARTESIAN_POINT('Ctrl Pts',(-7.83780125421114,-1.07369235101253,
20.3927827842399));
#218395=CARTESIAN_POINT('Ctrl Pts',(-7.83591556603223,-1.08739613535713,
20.3933455438195));
#218396=CARTESIAN_POINT('Ctrl Pts',(-7.83466487574452,-1.0963710123131,
20.3937150890883));
#218397=CARTESIAN_POINT('Ctrl Pts',(-7.82594405801734,-1.15817409114814,
20.3962665429619));
#218398=CARTESIAN_POINT('Ctrl Pts',(-7.8179552469144,-1.21092655710541,
20.3984779802046));
#218399=CARTESIAN_POINT('Ctrl Pts',(-7.79289516786784,-1.36580635467497,
20.4050616970903));
#218400=CARTESIAN_POINT('Ctrl Pts',(-7.77435217207518,-1.46768143170529,
20.4095089520627));
#218401=CARTESIAN_POINT('Ctrl Pts',(-7.71617226515173,-1.75517060488679,
20.4223354572617));
#218402=CARTESIAN_POINT('Ctrl Pts',(-7.67184895997818,-1.93975904408205,
20.4308992465233));
#218403=CARTESIAN_POINT('Ctrl Pts',(-7.46998374039145,-2.6645429696049,
20.4653957543712));
#218404=CARTESIAN_POINT('Ctrl Pts',(-7.26163172780135,-3.18892108742889,
20.4921743115637));
#218405=CARTESIAN_POINT('Ctrl Pts',(-6.94841175843544,-3.78357927309295,
20.522525732552));
#218406=CARTESIAN_POINT('Ctrl Pts',(-6.89540485111491,-3.87934157881735,
20.5274182978205));
#218407=CARTESIAN_POINT('Ctrl Pts',(-6.79349329571786,-4.05476252758364,
20.5363789912569));
#218408=CARTESIAN_POINT('Ctrl Pts',(-6.74513128574468,-4.13471341118438,
20.5404623431943));
#218409=CARTESIAN_POINT('Ctrl Pts',(-6.57236464952416,-4.40922524714831,
20.5544735784253));
#218410=CARTESIAN_POINT('Ctrl Pts',(-6.44086245243957,-4.59918984167382,
20.5641494735474));
#218411=CARTESIAN_POINT('Ctrl Pts',(-6.2875931070313,-4.80110430606929,
20.5744235808924));
#218412=CARTESIAN_POINT('Ctrl Pts',(-6.27388031458407,-4.819009799386,20.5753346260514));
#218413=CARTESIAN_POINT('Ctrl Pts',(-6.25447069753839,-4.84413065424665,
20.5766127819941));
#218414=CARTESIAN_POINT('Ctrl Pts',(-6.24883764349203,-4.85139501666961,
20.5769823933357));
#218415=CARTESIAN_POINT('Ctrl Pts',(-6.23902481984364,-4.86400414614803,
20.5776239495327));
#218416=CARTESIAN_POINT('Ctrl Pts',(-6.2348508175237,-4.86935337800691,
20.5778961208588));
#218417=CARTESIAN_POINT('Ctrl Pts',(-6.22613685514385,-4.88049126425749,
20.578462825857));
#218418=CARTESIAN_POINT('Ctrl Pts',(-6.22159569073457,-4.8862789708418,
20.5787573116687));
#218419=CARTESIAN_POINT('Ctrl Pts',(-6.21085777022427,-4.89992519470359,
20.57945165837));
#218420=CARTESIAN_POINT('Ctrl Pts',(-6.20465415569413,-4.9077783125172,
20.5798512479867));
#218421=CARTESIAN_POINT('Ctrl Pts',(-6.18421541467847,-4.93355089657461,
20.5811626713572));
#218422=CARTESIAN_POINT('Ctrl Pts',(-6.16991737192236,-4.95142044054334,
20.5820720145653));
#218423=CARTESIAN_POINT('Ctrl Pts',(-5.96280030440594,-5.20798299811566,
20.5951296223955));
#218424=CARTESIAN_POINT('Ctrl Pts',(-5.75632365626615,-5.43533201902799,
20.6067072602713));
#218425=CARTESIAN_POINT('Ctrl Pts',(-4.98117247113122,-6.19498330335456,
20.6462154594106));
#218426=CARTESIAN_POINT('Ctrl Pts',(-4.34789877793545,-6.65473250382228,
20.6713744183327));
#218427=CARTESIAN_POINT('Ctrl Pts',(-3.49770058106296,-7.09807048669171,
20.7070399331822));
#218428=CARTESIAN_POINT('Ctrl Pts',(-3.33483808871978,-7.17602698948031,
20.713991219408));
#218429=CARTESIAN_POINT('Ctrl Pts',(-3.15171630375763,-7.25609946828432,
20.7219676330616));
#218430=CARTESIAN_POINT('Ctrl Pts',(-3.13396522925643,-7.26378393725362,
20.7227421536145));
#218431=CARTESIAN_POINT('Ctrl Pts',(-3.10803096318952,-7.27489816116355,
20.7238754961013));
#218432=CARTESIAN_POINT('Ctrl Pts',(-3.09986982759641,-7.2783794057937,
20.7242323974466));
#218433=CARTESIAN_POINT('Ctrl Pts',(-3.08542729228833,-7.28451137045385,
20.7248644289317));
#218434=CARTESIAN_POINT('Ctrl Pts',(-3.07914828203073,-7.28716771724208,
20.7251393542828));
#218435=CARTESIAN_POINT('Ctrl Pts',(-3.06613143930582,-7.29265468864227,
20.7257095844235));
#218436=CARTESIAN_POINT('Ctrl Pts',(-3.05939310369036,-7.29548409960426,
20.7260049321062));
#218437=CARTESIAN_POINT('Ctrl Pts',(-3.04207255060414,-7.3027287416812,
20.7267645071582));
#218438=CARTESIAN_POINT('Ctrl Pts',(-3.03148465404137,-7.30713030324215,
20.7272292102662));
#218439=CARTESIAN_POINT('Ctrl Pts',(-2.98773973354293,-7.32520433913742,
20.7291506646386));
#218440=CARTESIAN_POINT('Ctrl Pts',(-2.95449972592711,-7.3386741754066,
20.7306142234757));
#218441=CARTESIAN_POINT('Ctrl Pts',(-2.71248951032243,-7.43483315481171,
20.7412909332252));
#218442=CARTESIAN_POINT('Ctrl Pts',(-2.50037975844424,-7.50882401135501,
20.7507580701854));
#218443=CARTESIAN_POINT('Ctrl Pts',(-1.85276467728768,-7.7042467763377,
20.779600183233));
#218444=CARTESIAN_POINT('Ctrl Pts',(-1.40971695344449,-7.79749093084379,
20.7991934325331));
#218445=CARTESIAN_POINT('Ctrl Pts',(-0.305814160610344,-7.93260803441085,
20.8465594412363));
#218446=CARTESIAN_POINT('Ctrl Pts',(0.356984446419582,-7.93047287432116,
20.8738100242726));
#218447=CARTESIAN_POINT('Ctrl Pts',(1.08411208581547,-7.83670451579456,
20.9036081091696));
#218448=CARTESIAN_POINT('Ctrl Pts',(1.15629005288069,-7.82638039668823,
20.9065618969188));
#218449=CARTESIAN_POINT('Ctrl Pts',(1.25495293821127,-7.81087326812838,
20.9105939419744));
#218450=CARTESIAN_POINT('Ctrl Pts',(1.28156897182594,-7.80655039467753,
20.9116811003882));
#218451=CARTESIAN_POINT('Ctrl Pts',(1.32707409424849,-7.79892063387666,
20.9135388799059));
#218452=CARTESIAN_POINT('Ctrl Pts',(1.34597418553832,-7.79568099650728,
20.9143102170922));
#218453=CARTESIAN_POINT('Ctrl Pts',(1.38475611839659,-7.78888820028072,
20.9158924160856));
#218454=CARTESIAN_POINT('Ctrl Pts',(1.40463651240967,-7.78532755731211,
20.9167031899448));
#218455=CARTESIAN_POINT('Ctrl Pts',(1.45065575160813,-7.77690335365144,
20.9185793249096));
#218456=CARTESIAN_POINT('Ctrl Pts',(1.47678417343494,-7.7719840705631,20.9196440554137));
#218457=CARTESIAN_POINT('Ctrl Pts',(1.55970026469578,-7.75593995857618,
20.9230214518708));
#218458=CARTESIAN_POINT('Ctrl Pts',(1.61639110852671,-7.74432368939628,
20.9253284824738));
#218459=CARTESIAN_POINT('Ctrl Pts',(1.71449273955713,-7.7230979706777,20.9293179100728));
#218460=CARTESIAN_POINT('Ctrl Pts',(1.75596283485193,-7.71377483252006,
20.9310034712683));
#218461=CARTESIAN_POINT('Ctrl Pts',(1.87030507303023,-7.68709900773947,
20.9356492737567));
#218462=CARTESIAN_POINT('Ctrl Pts',(1.94300922772652,-7.66904475770914,
20.9386013895525));
#218463=CARTESIAN_POINT('Ctrl Pts',(2.28569722099213,-7.57876072461122,
20.9525160476721));
#218464=CARTESIAN_POINT('Ctrl Pts',(2.55198792470274,-7.49328952122857,
20.9633209280324));
#218465=CARTESIAN_POINT('Ctrl Pts',(3.24401850819709,-7.22998877782816,
20.991810314466));
#218466=CARTESIAN_POINT('Ctrl Pts',(3.65967048777963,-7.02873921173164,
21.0093232520307));
#218467=CARTESIAN_POINT('Ctrl Pts',(4.09051295773349,-6.77150615721725,
21.029296334435));
#218468=CARTESIAN_POINT('Ctrl Pts',(4.12544680429371,-6.7502800322146,21.0309299765678));
#218469=CARTESIAN_POINT('Ctrl Pts',(4.1718124884069,-6.72161345953944,21.0331186328309));
#218470=CARTESIAN_POINT('Ctrl Pts',(4.18339203115805,-6.7144127106195,21.0336669567953));
#218471=CARTESIAN_POINT('Ctrl Pts',(4.20318470605052,-6.70203354195451,
21.0346071169437));
#218472=CARTESIAN_POINT('Ctrl Pts',(4.21140704806293,-6.69686986177469,
21.0349985469051));
#218473=CARTESIAN_POINT('Ctrl Pts',(4.22739850344639,-6.68678603365406,
21.0357615004399));
#218474=CARTESIAN_POINT('Ctrl Pts',(4.23516858712259,-6.68186744891962,
21.0361329819323));
#218475=CARTESIAN_POINT('Ctrl Pts',(4.25376519610399,-6.67005003458364,
21.0370239007636));
#218476=CARTESIAN_POINT('Ctrl Pts',(4.26458352875971,-6.66313838459529,
21.037543671038));
#218477=CARTESIAN_POINT('Ctrl Pts',(4.29712739648824,-6.64223493315225,
21.0391116879193));
#218478=CARTESIAN_POINT('Ctrl Pts',(4.31880118173396,-6.62816302686519,
21.0401619414964));
#218479=CARTESIAN_POINT('Ctrl Pts',(4.54743948071369,-6.47811991304877,
21.0513028943962));
#218480=CARTESIAN_POINT('Ctrl Pts',(4.74797559055538,-6.33261129572139,
21.0616086205743));
#218481=CARTESIAN_POINT('Ctrl Pts',(5.32898445241308,-5.86789840132567,
21.0927710499984));
#218482=CARTESIAN_POINT('Ctrl Pts',(5.68658896414178,-5.52204992429265,
21.1137025848621));
#218483=CARTESIAN_POINT('Ctrl Pts',(6.03013007694855,-5.12078763435865,
21.135467962359));
#218484=CARTESIAN_POINT('Ctrl Pts',(6.05069083617393,-5.0964767394766,21.1367780052267));
#218485=CARTESIAN_POINT('Ctrl Pts',(6.16874585856948,-4.95516791145632,
21.1443432367032));
#218486=CARTESIAN_POINT('Ctrl Pts',(6.26299321364288,-4.8354970408097,21.1505546318638));
#218487=CARTESIAN_POINT('Ctrl Pts',(6.38034049097667,-4.67730386373611,
21.1585295972884));
#218488=CARTESIAN_POINT('Ctrl Pts',(6.40664825261346,-4.64120398279059,
21.1603341951164));
#218489=CARTESIAN_POINT('Ctrl Pts',(6.44832737073148,-4.58298162851746,
21.1632208448287));
#218490=CARTESIAN_POINT('Ctrl Pts',(6.46389386310364,-4.56100017759178,
21.1643053084913));
#218491=CARTESIAN_POINT('Ctrl Pts',(6.49188557198494,-4.52104194207126,
21.16626712286));
#218492=CARTESIAN_POINT('Ctrl Pts',(6.50434913068953,-4.50309237202046,
21.1671449315492));
#218493=CARTESIAN_POINT('Ctrl Pts',(6.53371666520347,-4.46042199634498,
21.1692236400733));
#218494=CARTESIAN_POINT('Ctrl Pts',(6.55055497209323,-4.43565636767066,
21.1704237493483));
#218495=CARTESIAN_POINT('Ctrl Pts',(6.60024287218715,-4.36167584358126,
21.1739902911522));
#218496=CARTESIAN_POINT('Ctrl Pts',(6.63268146300191,-4.31218724120532,
21.176351968782));
#218497=CARTESIAN_POINT('Ctrl Pts',(6.84538586891979,-3.97960421005094,
21.1920713162999));
#218498=CARTESIAN_POINT('Ctrl Pts',(7.00804105708511,-3.68563810160182,
21.2052842386913));
#218499=CARTESIAN_POINT('Ctrl Pts',(7.34758256731569,-2.96769679575803,
21.236090889135));
#218500=CARTESIAN_POINT('Ctrl Pts',(7.50722048829168,-2.53689874396757,
21.2533323760965));
#218501=CARTESIAN_POINT('Ctrl Pts',(7.72951205768504,-1.72733523885317,
21.2845384645283));
#218502=CARTESIAN_POINT('Ctrl Pts',(7.80371114555069,-1.35318819759569,
21.2985448294476));
#218503=CARTESIAN_POINT('Ctrl Pts',(7.86847397019705,-0.831809383643287,
21.3186192712006));
#218504=CARTESIAN_POINT('Ctrl Pts',(7.88235054647267,-0.687994848071836,
21.3242182200834));
#218505=CARTESIAN_POINT('Ctrl Pts',(7.89450002917865,-0.511694709694051,
21.3312287551038));
#218506=CARTESIAN_POINT('Ctrl Pts',(7.89652144218214,-0.479490630347162,
21.3325153472307));
#218507=CARTESIAN_POINT('Ctrl Pts',(7.89893019141788,-0.436955011831059,
21.3342235400982));
#218508=CARTESIAN_POINT('Ctrl Pts',(7.89949439281172,-0.426633552315023,
21.3346387280268));
#218509=CARTESIAN_POINT('Ctrl Pts',(7.90035066610369,-0.410384663632813,
21.3352934691067));
#218510=CARTESIAN_POINT('Ctrl Pts',(7.9006563014503,-0.404457940554016,
21.3355325176555));
#218511=CARTESIAN_POINT('Ctrl Pts',(7.90125331601707,-0.392622006344857,
21.3360103847259));
#218512=CARTESIAN_POINT('Ctrl Pts',(7.90154473584647,-0.386712801573303,
21.3362492015308));
#218513=CARTESIAN_POINT('Ctrl Pts',(7.90219083537574,-0.373305962584931,
21.3367915782132));
#218514=CARTESIAN_POINT('Ctrl Pts',(7.90254147350319,-0.365808145697425,
21.3370952926291));
#218515=CARTESIAN_POINT('Ctrl Pts',(7.9035418490985,-0.343743863763675,
21.3379902212282));
#218516=CARTESIAN_POINT('Ctrl Pts',(7.90416198416795,-0.32917613608675,
21.3385825890612));
#218517=CARTESIAN_POINT('Ctrl Pts',(7.90547124123999,-0.296280032940708,
21.3399237800177));
#218518=CARTESIAN_POINT('Ctrl Pts',(7.90613690255562,-0.277950848421,21.3406735479447));
#218519=CARTESIAN_POINT('Ctrl Pts',(7.91115296726171,-0.125186150170402,
21.346944248329));
#218520=CARTESIAN_POINT('Ctrl Pts',(7.91213750945838,0.00932024328144952,
21.3526193068265));
#218521=CARTESIAN_POINT('Ctrl Pts',(7.90614283229866,0.339098544217776,
21.3668687812909));
#218522=CARTESIAN_POINT('Ctrl Pts',(7.89535918553394,0.534208544160177,
21.3755744605981));
#218523=CARTESIAN_POINT('Ctrl Pts',(7.82008525248643,1.34792127042609,21.4125761989884));
#218524=CARTESIAN_POINT('Ctrl Pts',(7.68998299482453,1.95828654873776,21.4418430210699));
#218525=CARTESIAN_POINT('Ctrl Pts',(7.44215809221688,2.68701369387939,21.4758850093446));
#218526=CARTESIAN_POINT('Ctrl Pts',(7.39066539022854,2.82556674690524,21.4823255384689));
#218527=CARTESIAN_POINT('Ctrl Pts',(7.25795223941161,3.15416098080264,21.4975009748971));
#218528=CARTESIAN_POINT('Ctrl Pts',(7.17310728029139,3.3426250522858,21.5061217722289));
#218529=CARTESIAN_POINT('Ctrl Pts',(7.07074562706712,3.54809861074902,21.5154322621857));
#218530=CARTESIAN_POINT('Ctrl Pts',(7.06042495053649,3.56859173949286,21.5163598899398));
#218531=CARTESIAN_POINT('Ctrl Pts',(7.04583066941112,3.59725954760483,21.5176562390892));
#218532=CARTESIAN_POINT('Ctrl Pts',(7.04163175115944,3.60547200191611,21.5180274526292));
#218533=CARTESIAN_POINT('Ctrl Pts',(7.03391631379916,3.62049735136443,21.5187063454141));
#218534=CARTESIAN_POINT('Ctrl Pts',(7.03040423742139,3.62731250923441,21.5190141729184));
#218535=CARTESIAN_POINT('Ctrl Pts',(7.02328139103339,3.64108513302807,21.5196360504375));
#218536=CARTESIAN_POINT('Ctrl Pts',(7.01967017629657,3.64804235995725,21.5199500850606));
#218537=CARTESIAN_POINT('Ctrl Pts',(7.01078166414746,3.66510455749891,21.5207199800449));
#218538=CARTESIAN_POINT('Ctrl Pts',(7.00549284638322,3.67520352366444,21.5211754526882));
#218539=CARTESIAN_POINT('Ctrl Pts',(6.98628572076714,3.71168731209647,21.522820122082));
#218540=CARTESIAN_POINT('Ctrl Pts',(6.97223995610578,3.73800493487893,21.5240050211915));
#218541=CARTESIAN_POINT('Ctrl Pts',(6.77323418734576,4.1058587991568,21.5405475024166));
#218542=CARTESIAN_POINT('Ctrl Pts',(6.56350895449849,4.43341489518475,21.5550076613076));
#218543=CARTESIAN_POINT('Ctrl Pts',(6.22168789434987,4.88952689931979,21.5754020176109));
#218544=CARTESIAN_POINT('Ctrl Pts',(6.10785520898122,5.03100193704645,21.5817745184293));
#218545=CARTESIAN_POINT('Ctrl Pts',(5.59836509279022,5.62140586373309,21.6089026258922));
#218546=CARTESIAN_POINT('Ctrl Pts',(5.15738317849322,6.02853070226537,21.6289019173298));
#218547=CARTESIAN_POINT('Ctrl Pts',(4.56738087035909,6.46070259543378,21.6565169059394));
#218548=CARTESIAN_POINT('Ctrl Pts',(4.4580095466773,6.53665028697409,21.6616741747669));
#218549=CARTESIAN_POINT('Ctrl Pts',(4.3358291913977,6.61699915025736,21.667521513679));
#218550=CARTESIAN_POINT('Ctrl Pts',(4.32486857210806,6.62416820154599,21.6680467173917));
#218551=CARTESIAN_POINT('Ctrl Pts',(4.30833723629718,6.63492239170158,21.668839766944));
#218552=CARTESIAN_POINT('Ctrl Pts',(4.30277969889074,6.63852782987389,21.6691065306222));
#218553=CARTESIAN_POINT('Ctrl Pts',(4.29315080803214,6.64475737716687,21.6695689791331));
#218554=CARTESIAN_POINT('Ctrl Pts',(4.28908155587205,6.64738473904073,21.6697644936162));
#218555=CARTESIAN_POINT('Ctrl Pts',(4.28088084104161,6.65266896461637,21.6701586680266));
#218556=CARTESIAN_POINT('Ctrl Pts',(4.27674931113416,6.65532572136908,21.6703573333893));
#218557=CARTESIAN_POINT('Ctrl Pts',(4.2669854063907,6.66159149831317,21.670827015911));
#218558=CARTESIAN_POINT('Ctrl Pts',(4.26135092825651,6.66519722248379,21.6710982005692));
#218559=CARTESIAN_POINT('Ctrl Pts',(4.24379508170847,6.67640053825089,21.6719435858687));
#218560=CARTESIAN_POINT('Ctrl Pts',(4.23185795831254,6.6839732988507,21.67251902463));
#218561=CARTESIAN_POINT('Ctrl Pts',(4.20409311340327,6.70148277240838,21.673858767274));
#218562=CARTESIAN_POINT('Ctrl Pts',(4.18825038624189,6.71139545468534,21.674624218095));
#218563=CARTESIAN_POINT('Ctrl Pts',(4.13464737154508,6.74467076771323,21.677217023411));
#218564=CARTESIAN_POINT('Ctrl Pts',(4.096725928947,6.76777136253398,21.679056210811));
#218565=CARTESIAN_POINT('Ctrl Pts',(3.93306181694111,6.86559099389532,21.6870084533196));
#218566=CARTESIAN_POINT('Ctrl Pts',(3.80545767316003,6.93713227803034,21.693244583989));
#218567=CARTESIAN_POINT('Ctrl Pts',(3.39165803013796,7.15427515994618,21.7134246878212));
#218568=CARTESIAN_POINT('Ctrl Pts',(3.09855336687518,7.28601129607747,21.7276409876623));
#218569=CARTESIAN_POINT('Ctrl Pts',(2.67733648573444,7.44530078542147,21.7474436822204));
#218570=CARTESIAN_POINT('Ctrl Pts',(2.55530986901585,7.48805892963322,21.7531121436162));
#218571=CARTESIAN_POINT('Ctrl Pts',(1.98449402256463,7.67249366139754,21.7792481226111));
#218572=CARTESIAN_POINT('Ctrl Pts',(1.52465808512055,7.77694379217276,21.7991410679494));
#218573=CARTESIAN_POINT('Ctrl Pts',(1.0201489788642,7.84504263121774,21.819763603688));
#218574=CARTESIAN_POINT('Ctrl Pts',(0.982027729137657,7.84990569340666,
21.8213151656408));
#218575=CARTESIAN_POINT('Ctrl Pts',(0.928442124823705,7.85634506313133,
21.8234872101291));
#218576=CARTESIAN_POINT('Ctrl Pts',(0.913006435558643,7.85815384048847,
21.8241118438224));
#218577=CARTESIAN_POINT('Ctrl Pts',(0.884662989579706,7.86139052840842,
21.8252569536541));
#218578=CARTESIAN_POINT('Ctrl Pts',(0.871756864853068,7.86283216246031,
21.8257776695716));
#218579=CARTESIAN_POINT('Ctrl Pts',(0.845566530484154,7.86569238675135,
21.8268329516179));
#218580=CARTESIAN_POINT('Ctrl Pts',(0.832282159000866,7.8671091189533,21.827367483916));
#218581=CARTESIAN_POINT('Ctrl Pts',(0.79948112043046,7.8705232243456,21.8286855563566));
#218582=CARTESIAN_POINT('Ctrl Pts',(0.779960466390587,7.87248166473394,
21.8294684297796));
#218583=CARTESIAN_POINT('Ctrl Pts',(0.709111220382261,7.87932362152865,
21.8323044430253));
#218584=CARTESIAN_POINT('Ctrl Pts',(0.657742007341309,7.88377796384483,
21.8343505708884));
#218585=CARTESIAN_POINT('Ctrl Pts',(0.376724601058868,7.90537987640605,
21.845491071166));
#218586=CARTESIAN_POINT('Ctrl Pts',(0.146450258908566,7.91299629948024,
21.8544215671859));
#218587=CARTESIAN_POINT('Ctrl Pts',(-0.200421085763858,7.90932021747925,
21.8676476024266));
#218588=CARTESIAN_POINT('Ctrl Pts',(-0.316967106070901,7.90550740842303,
21.8720537432554));
#218589=CARTESIAN_POINT('Ctrl Pts',(-0.517151172562729,7.89452424920726,
21.8795761263049));
#218590=CARTESIAN_POINT('Ctrl Pts',(-0.600836856155371,7.88859643479536,
21.8827070833749));
#218591=CARTESIAN_POINT('Ctrl Pts',(-1.25053454501037,7.83217689350823,
21.9069477716208));
#218592=CARTESIAN_POINT('Ctrl Pts',(-1.80968104960947,7.72216471960022,
21.9272913244381));
#218593=CARTESIAN_POINT('Ctrl Pts',(-2.50004311591564,7.50717574209895,
21.9549589576368));
#218594=CARTESIAN_POINT('Ctrl Pts',(-2.64651248707179,7.45680035530527,
21.9609908293334));
#218595=CARTESIAN_POINT('Ctrl Pts',(-2.80616993862786,7.3965924809871,21.9678198912855));
#218596=CARTESIAN_POINT('Ctrl Pts',(-2.82091956015657,7.39097983253615,
21.9684532046756));
#218597=CARTESIAN_POINT('Ctrl Pts',(-2.8429067380082,7.38253768467095,21.9694010138659));
#218598=CARTESIAN_POINT('Ctrl Pts',(-2.85015712998586,7.37974157545378,
21.9697141662333));
#218599=CARTESIAN_POINT('Ctrl Pts',(-2.86261719516203,7.3749152575768,21.9702533897646));
#218600=CARTESIAN_POINT('Ctrl Pts',(-2.86782886427353,7.37289019770988,
21.970479249917));
#218601=CARTESIAN_POINT('Ctrl Pts',(-2.8782718849754,7.36881968208915,21.9709324699893));
#218602=CARTESIAN_POINT('Ctrl Pts',(-2.88350321315181,7.36677417670083,
21.9711598318736));
#218603=CARTESIAN_POINT('Ctrl Pts',(-2.8957210378762,7.36198186814832,21.9716916073191));
#218604=CARTESIAN_POINT('Ctrl Pts',(-2.90270580484743,7.35923069118881,
21.9719962045549));
#218605=CARTESIAN_POINT('Ctrl Pts',(-2.92395406329744,7.3508264188931,21.9729246314419));
#218606=CARTESIAN_POINT('Ctrl Pts',(-2.93820498218206,7.34514178781756,
21.9735498083944));
#218607=CARTESIAN_POINT('Ctrl Pts',(-2.97071983690408,7.33206198215857,
21.9749820690807));
#218608=CARTESIAN_POINT('Ctrl Pts',(-2.98897281342758,7.32463997546764,
21.9757903374959));
#218609=CARTESIAN_POINT('Ctrl Pts',(-3.04801954040579,7.30037298803718,
21.9784192259412));
#218610=CARTESIAN_POINT('Ctrl Pts',(-3.08869958878179,7.2832550149435,21.9802524329248));
#218611=CARTESIAN_POINT('Ctrl Pts',(-3.23355635479727,7.22086810637651,
21.9868651796408));
#218612=CARTESIAN_POINT('Ctrl Pts',(-3.33689326115389,7.17369941602656,
21.9917432591517));
#218613=CARTESIAN_POINT('Ctrl Pts',(-3.57433433654651,7.05907790442507,
22.0032688331088));
#218614=CARTESIAN_POINT('Ctrl Pts',(-3.70760718041908,6.98999948138854,
22.009978359212));
#218615=CARTESIAN_POINT('Ctrl Pts',(-4.44805180757511,6.57907438202911,
22.0483145514951));
#218616=CARTESIAN_POINT('Ctrl Pts',(-5.01004795484847,6.16190158004555,
22.081180602425));
#218617=CARTESIAN_POINT('Ctrl Pts',(-5.67190883575128,5.51943960109531,
22.1209469098375));
#218618=CARTESIAN_POINT('Ctrl Pts',(-5.8269214456974,5.35553555400147,22.1303892209941));
#218619=CARTESIAN_POINT('Ctrl Pts',(-5.98893532557489,5.16885330000307,
22.1403979110106));
#218620=CARTESIAN_POINT('Ctrl Pts',(-6.00307430571377,5.15242560946019,
22.1412726493189));
#218621=CARTESIAN_POINT('Ctrl Pts',(-6.02286875612673,5.12923489982746,
22.1424991108452));
#218622=CARTESIAN_POINT('Ctrl Pts',(-6.02858064147224,5.12252029386454,
22.1428532354283));
#218623=CARTESIAN_POINT('Ctrl Pts',(-6.03848439037269,5.11083843532389,
22.1434676269019));
#218624=CARTESIAN_POINT('Ctrl Pts',(-6.042681372483,5.10587554447732,22.143728111207));
#218625=CARTESIAN_POINT('Ctrl Pts',(-6.05141168865918,5.09552618865137,
22.1442702056203));
#218626=CARTESIAN_POINT('Ctrl Pts',(-6.05594395947538,5.09013883159554,
22.1445517705512));
#218627=CARTESIAN_POINT('Ctrl Pts',(-6.06661712052576,5.07741757286198,
22.1452151706438));
#218628=CARTESIAN_POINT('Ctrl Pts',(-6.07275191935543,5.07007856182593,
22.1455967477419));
#218629=CARTESIAN_POINT('Ctrl Pts',(-6.09283736237928,5.04596175064919,
22.1468469112061));
#218630=CARTESIAN_POINT('Ctrl Pts',(-6.10673196254756,5.02913728796018,
22.1477131299382));
#218631=CARTESIAN_POINT('Ctrl Pts',(-6.36585216210786,4.71272087137329,
22.1638939762135));
#218632=CARTESIAN_POINT('Ctrl Pts',(-6.58883964426354,4.39557145677893,
22.1782317250367));
#218633=CARTESIAN_POINT('Ctrl Pts',(-6.93729561032466,3.81348254277342,
22.2021811773027));
#218634=CARTESIAN_POINT('Ctrl Pts',(-7.07295952013767,3.55555495991087,
22.2120748894831));
#218635=CARTESIAN_POINT('Ctrl Pts',(-7.2474591786569,3.17406896853133,22.2262007549969));
#218636=CARTESIAN_POINT('Ctrl Pts',(-7.29797665220492,3.05612747356098,
22.2305031063275));
#218637=CARTESIAN_POINT('Ctrl Pts',(-7.36995885857173,2.87609649184549,
22.2370292144113));
#218638=CARTESIAN_POINT('Ctrl Pts',(-7.39355527722465,2.81488275302091,
22.2392412197324));
#218639=CARTESIAN_POINT('Ctrl Pts',(-7.4412165755555,2.68650443489874,22.2438768850733));
#218640=CARTESIAN_POINT('Ctrl Pts',(-7.46513970607562,2.61929365303851,
22.2463019169655));
#218641=CARTESIAN_POINT('Ctrl Pts',(-7.59503562179923,2.23811488765928,
22.260085018354));
#218642=CARTESIAN_POINT('Ctrl Pts',(-7.68210037590923,1.91807806255168,
22.2717634104519));
#218643=CARTESIAN_POINT('Ctrl Pts',(-7.7651139198809,1.514415685093,22.2876004533614));
#218644=CARTESIAN_POINT('Ctrl Pts',(-7.78017528097231,1.43503337894554,
22.2907674527641));
#218645=CARTESIAN_POINT('Ctrl Pts',(-7.7958270788906,1.34503259471773,22.2944307451041));
#218646=CARTESIAN_POINT('Ctrl Pts',(-7.79761563129311,1.33462466233148,
22.2948554731086));
#218647=CARTESIAN_POINT('Ctrl Pts',(-7.80021236821219,1.31933033798389,
22.2954812524248));
#218648=CARTESIAN_POINT('Ctrl Pts',(-7.8010368192283,1.31444668007342,22.2956813176428));
#218649=CARTESIAN_POINT('Ctrl Pts',(-7.80248090540606,1.3058433828348,22.2960342015207));
#218650=CARTESIAN_POINT('Ctrl Pts',(-7.8031024689808,1.30212406406063,22.2961869023084));
#218651=CARTESIAN_POINT('Ctrl Pts',(-7.80437912373904,1.29445106270511,
22.2965022263383));
#218652=CARTESIAN_POINT('Ctrl Pts',(-7.80503387022686,1.29049732478725,
22.2966648707077));
#218653=CARTESIAN_POINT('Ctrl Pts',(-7.80634767573858,1.2825262332704,22.2969931107874));
#218654=CARTESIAN_POINT('Ctrl Pts',(-7.80700663630438,1.27850887911462,
22.2971587121941));
#218655=CARTESIAN_POINT('Ctrl Pts',(-7.80861084098274,1.26868135705134,
22.2975642343431));
#218656=CARTESIAN_POINT('Ctrl Pts',(-7.80955270070102,1.26287064509135,
22.2978043632079));
#218657=CARTESIAN_POINT('Ctrl Pts',(-7.81212187000328,1.24690761731703,
22.2984650047925));
#218658=CARTESIAN_POINT('Ctrl Pts',(-7.81373586890071,1.23675320373788,
22.2988863256342));
#218659=CARTESIAN_POINT('Ctrl Pts',(-7.8785311275676,0.823906228856935,
22.3160586058685));
#218660=CARTESIAN_POINT('Ctrl Pts',(-7.91050707665273,0.416979381960712,
22.3346078413317));
#218661=CARTESIAN_POINT('Ctrl Pts',(-7.91099434492025,0.00945910354153937,
22.35353228109));
#218662=CARTESIAN_POINT('',(-7.91099777923565,-0.00592764106740733,26.3576684917633));
#218663=CARTESIAN_POINT('Ctrl Pts',(-7.91099433110756,0.00947064855683299,
22.3535317449623));
#218664=CARTESIAN_POINT('Ctrl Pts',(-7.91132738906062,-0.268738342389904,
22.3664512181225));
#218665=CARTESIAN_POINT('Ctrl Pts',(-7.89698450830174,-0.546774875940983,
22.3795297055049));
#218666=CARTESIAN_POINT('Ctrl Pts',(-7.81067683996992,-1.37140734219466,
22.4179794102181));
#218667=CARTESIAN_POINT('Ctrl Pts',(-7.69624630752847,-1.91190848755121,
22.4426006476018));
#218668=CARTESIAN_POINT('Ctrl Pts',(-7.50905049898906,-2.49024260815374,
22.4675066381919));
#218669=CARTESIAN_POINT('Ctrl Pts',(-7.4909759876114,-2.5440964185709,22.4698133677065));
#218670=CARTESIAN_POINT('Ctrl Pts',(-7.46793898366663,-2.61036138445217,
22.4726367973827));
#218671=CARTESIAN_POINT('Ctrl Pts',(-7.46352330562275,-2.62295998636552,
22.4731729327037));
#218672=CARTESIAN_POINT('Ctrl Pts',(-7.4565282840326,-2.6427571624589,22.4740143648846));
#218673=CARTESIAN_POINT('Ctrl Pts',(-7.4539703687289,-2.64996324745637,
22.4743204254822));
#218674=CARTESIAN_POINT('Ctrl Pts',(-7.44940625728032,-2.66276223478934,
22.4748636477076));
#218675=CARTESIAN_POINT('Ctrl Pts',(-7.44740420235687,-2.66835660134912,
22.4751009569242));
#218676=CARTESIAN_POINT('Ctrl Pts',(-7.44276857606013,-2.68126413116127,
22.4756481866518));
#218677=CARTESIAN_POINT('Ctrl Pts',(-7.44013052332249,-2.68857568505004,
22.4759579467845));
#218678=CARTESIAN_POINT('Ctrl Pts',(-7.43286433995909,-2.70862184382663,
22.4768066156558));
#218679=CARTESIAN_POINT('Ctrl Pts',(-7.42821425161995,-2.72134849360274,
22.477344738817));
#218680=CARTESIAN_POINT('Ctrl Pts',(-7.40526974948067,-2.7836474321062,
22.4799757048829));
#218681=CARTESIAN_POINT('Ctrl Pts',(-7.38651147292415,-2.83304809266183,
22.4820519086078));
#218682=CARTESIAN_POINT('Ctrl Pts',(-7.06340291774898,-3.65893693661997,
22.5166048658313));
#218683=CARTESIAN_POINT('Ctrl Pts',(-6.63870925191398,-4.38257078431541,
22.5437330007848));
#218684=CARTESIAN_POINT('Ctrl Pts',(-6.01865014138278,-5.13613824041793,
22.5774624884684));
#218685=CARTESIAN_POINT('Ctrl Pts',(-5.92553770890973,-5.24328775650253,
22.582432497387));
#218686=CARTESIAN_POINT('Ctrl Pts',(-5.67722987213511,-5.51396260092418,
22.5956129595548));
#218687=CARTESIAN_POINT('Ctrl Pts',(-5.51784570028461,-5.67345456356453,
22.6040033871958));
#218688=CARTESIAN_POINT('Ctrl Pts',(-5.33339807097235,-5.84289449826277,
22.6139436891075));
#218689=CARTESIAN_POINT('Ctrl Pts',(-5.31483166165228,-5.8597880081408,
22.6149467645789));
#218690=CARTESIAN_POINT('Ctrl Pts',(-5.29232173829739,-5.88007471621918,
22.6161663415352));
#218691=CARTESIAN_POINT('Ctrl Pts',(-5.28845484371562,-5.88355278855391,
22.6163759682639));
#218692=CARTESIAN_POINT('Ctrl Pts',(-5.28166968987759,-5.88964359105746,
22.6167440017176));
#218693=CARTESIAN_POINT('Ctrl Pts',(-5.27875291078135,-5.89225797546792,
22.6169022773221));
#218694=CARTESIAN_POINT('Ctrl Pts',(-5.27286611912393,-5.89752657948172,
22.6172218492687));
#218695=CARTESIAN_POINT('Ctrl Pts',(-5.2698960413717,-5.90018072425938,
22.6173831513823));
#218696=CARTESIAN_POINT('Ctrl Pts',(-5.26417790232757,-5.9052828515783,
22.6176938260265));
#218697=CARTESIAN_POINT('Ctrl Pts',(-5.26143013410749,-5.90773116249542,
22.6178431729129));
#218698=CARTESIAN_POINT('Ctrl Pts',(-5.25494853323093,-5.91349827674835,
22.6181955928357));
#218699=CARTESIAN_POINT('Ctrl Pts',(-5.25121326738718,-5.91681545902874,
22.6183987907697));
#218700=CARTESIAN_POINT('Ctrl Pts',(-5.24015968957158,-5.92661311223877,
22.6190004006471));
#218701=CARTESIAN_POINT('Ctrl Pts',(-5.23283252833325,-5.933083539202,22.6193995779622));
#218702=CARTESIAN_POINT('Ctrl Pts',(-5.16887711538896,-5.98935028218625,
22.6228870068242));
#218703=CARTESIAN_POINT('Ctrl Pts',(-5.1115532387619,-6.03834664623039,
22.6260345904189));
#218704=CARTESIAN_POINT('Ctrl Pts',(-4.85634511740895,-6.25024203055892,
22.6401085514726));
#218705=CARTESIAN_POINT('Ctrl Pts',(-4.65132340335551,-6.40427867530036,
22.6515696164034));
#218706=CARTESIAN_POINT('Ctrl Pts',(-4.31640458046204,-6.63133343766325,
22.6700839250487));
#218707=CARTESIAN_POINT('Ctrl Pts',(-4.19128877325705,-6.71111231781684,
22.6769582579013));
#218708=CARTESIAN_POINT('Ctrl Pts',(-3.95980540012706,-6.84971625345231,
22.6895168430201));
#218709=CARTESIAN_POINT('Ctrl Pts',(-3.85418175622888,-6.90970002493307,
22.6951893485242));
#218710=CARTESIAN_POINT('Ctrl Pts',(-3.53040945581009,-7.08383610865673,
22.7123384211577));
#218711=CARTESIAN_POINT('Ctrl Pts',(-3.30826906055341,-7.19026336747525,
22.7237795881239));
#218712=CARTESIAN_POINT('Ctrl Pts',(-2.6264404055016,-7.47862786741661,
22.757540212062));
#218713=CARTESIAN_POINT('Ctrl Pts',(-2.15428626939292,-7.62805549178081,
22.779061854378));
#218714=CARTESIAN_POINT('Ctrl Pts',(-1.64987825024774,-7.73707304235151,
22.7999665991115));
#218715=CARTESIAN_POINT('Ctrl Pts',(-1.6285228339128,-7.74159614631759,
22.8008480398433));
#218716=CARTESIAN_POINT('Ctrl Pts',(-1.59753759557242,-7.74802497309539,
22.8021217653868));
#218717=CARTESIAN_POINT('Ctrl Pts',(-1.58792260845171,-7.75000123506068,
22.8025162910012));
#218718=CARTESIAN_POINT('Ctrl Pts',(-1.57112729135953,-7.75342077239019,
22.8032041878312));
#218719=CARTESIAN_POINT('Ctrl Pts',(-1.56394859953637,-7.75487197945635,
22.8034978103725));
#218720=CARTESIAN_POINT('Ctrl Pts',(-1.55006863493017,-7.7576578240465,
22.804064758424));
#218721=CARTESIAN_POINT('Ctrl Pts',(-1.54336763030362,-7.758993752156,22.8043381245707));
#218722=CARTESIAN_POINT('Ctrl Pts',(-1.52746527297408,-7.76214266754479,
22.8049860393772));
#218723=CARTESIAN_POINT('Ctrl Pts',(-1.51826240065996,-7.76394797992649,
22.8053603450488));
#218724=CARTESIAN_POINT('Ctrl Pts',(-1.48586203468725,-7.77024409547664,
22.806675881429));
#218725=CARTESIAN_POINT('Ctrl Pts',(-1.46264754907615,-7.77464735205636,
22.8076143475751));
#218726=CARTESIAN_POINT('Ctrl Pts',(-1.162051151145,-7.83026960456698,22.819714006432));
#218727=CARTESIAN_POINT('Ctrl Pts',(-0.88213145939188,-7.86672399444468,
22.8303965263708));
#218728=CARTESIAN_POINT('Ctrl Pts',(-0.0333197098617335,-7.93137844934754,
22.8615555816639));
#218729=CARTESIAN_POINT('Ctrl Pts',(0.537192307667847,-7.91323538274013,
22.8807452602072));
#218730=CARTESIAN_POINT('Ctrl Pts',(1.32534613161184,-7.80248588546917,
22.9086659873577));
#218731=CARTESIAN_POINT('Ctrl Pts',(1.54840399341934,-7.76129922206249,
22.9167483955407));
#218732=CARTESIAN_POINT('Ctrl Pts',(1.86762787828406,-7.68804585092992,
22.9289110069963));
#218733=CARTESIAN_POINT('Ctrl Pts',(1.96543774556981,-7.66362422208288,
22.9327201808654));
#218734=CARTESIAN_POINT('Ctrl Pts',(2.11932888064962,-7.62206012935536,
22.9388780328626));
#218735=CARTESIAN_POINT('Ctrl Pts',(2.17573375164834,-7.6061513192077,22.9411704718224));
#218736=CARTESIAN_POINT('Ctrl Pts',(2.2562860410519,-7.58246249392462,22.9444908655487));
#218737=CARTESIAN_POINT('Ctrl Pts',(2.28058185956919,-7.57519046191902,
22.9454984528267));
#218738=CARTESIAN_POINT('Ctrl Pts',(2.31774374827146,-7.56387247439887,
22.9470486152508));
#218739=CARTESIAN_POINT('Ctrl Pts',(2.33063526652272,-7.55991019413761,
22.9475880329004));
#218740=CARTESIAN_POINT('Ctrl Pts',(2.35456108315577,-7.55248944533344,
22.9485921839809));
#218741=CARTESIAN_POINT('Ctrl Pts',(2.36559806693217,-7.54903970716123,
22.9490565981438));
#218742=CARTESIAN_POINT('Ctrl Pts',(2.38355792865656,-7.54338288819076,
22.9498142311254));
#218743=CARTESIAN_POINT('Ctrl Pts',(2.39048542004355,-7.5411904400617,22.950106931292));
#218744=CARTESIAN_POINT('Ctrl Pts',(2.40387369609309,-7.53693294778547,
22.9506735021079));
#218745=CARTESIAN_POINT('Ctrl Pts',(2.41033486692504,-7.53486913191958,
22.950947329886));
#218746=CARTESIAN_POINT('Ctrl Pts',(2.42515992144219,-7.53011271895305,
22.9515765346064));
#218747=CARTESIAN_POINT('Ctrl Pts',(2.43352198247945,-7.52741449402307,
22.9519321035013));
#218748=CARTESIAN_POINT('Ctrl Pts',(2.45937478231427,-7.51902487017744,
22.9530334414548));
#218749=CARTESIAN_POINT('Ctrl Pts',(2.47685012242444,-7.51328641696531,
22.9537807788884));
#218750=CARTESIAN_POINT('Ctrl Pts',(2.61736879920439,-7.46660016049683,
22.9598126372424));
#218751=CARTESIAN_POINT('Ctrl Pts',(2.73940562435025,-7.4226944269035,22.9651901254188));
#218752=CARTESIAN_POINT('Ctrl Pts',(3.45187544104198,-7.1464019590393,22.997249073056));
#218753=CARTESIAN_POINT('Ctrl Pts',(4.01370845633387,-6.8466557446557,23.0249985431122));
#218754=CARTESIAN_POINT('Ctrl Pts',(4.90355710499443,-6.22436658576277,
23.0710227064924));
#218755=CARTESIAN_POINT('Ctrl Pts',(5.25060485734947,-5.93454101434495,
23.0897136441153));
#218756=CARTESIAN_POINT('Ctrl Pts',(5.70374150398613,-5.48508733076998,
23.1159220734153));
#218757=CARTESIAN_POINT('Ctrl Pts',(5.83172914427766,-5.3488117412613,23.1235548263573));
#218758=CARTESIAN_POINT('Ctrl Pts',(5.98510689699571,-5.17344562679096,
23.1329881348284));
#218759=CARTESIAN_POINT('Ctrl Pts',(6.01513867865191,-5.13849695233709,
23.1348498216447));
#218760=CARTESIAN_POINT('Ctrl Pts',(6.06051113683805,-5.0847531053173,23.1376851059365));
#218761=CARTESIAN_POINT('Ctrl Pts',(6.07607345793738,-5.06614653559885,
23.1386617317339));
#218762=CARTESIAN_POINT('Ctrl Pts',(6.10304677416558,-5.03359372238583,
23.1403617644181));
#218763=CARTESIAN_POINT('Ctrl Pts',(6.11449613974235,-5.01967953645452,
23.1410857019816));
#218764=CARTESIAN_POINT('Ctrl Pts',(6.14017397110136,-4.98825557072307,
23.1427145744411));
#218765=CARTESIAN_POINT('Ctrl Pts',(6.15437528153048,-4.97072378353024,
23.143619122286));
#218766=CARTESIAN_POINT('Ctrl Pts',(6.19237580854727,-4.92339891292325,
23.1460495831962));
#218767=CARTESIAN_POINT('Ctrl Pts',(6.21603498600845,-4.89349405654072,
23.14757349581));
#218768=CARTESIAN_POINT('Ctrl Pts',(6.3223519721031,-4.75709569759269,23.1544710592942));
#218769=CARTESIAN_POINT('Ctrl Pts',(6.40249642874486,-4.64867015571946,
23.1598080732728));
#218770=CARTESIAN_POINT('Ctrl Pts',(6.70804842033338,-4.21239488764495,
23.1807536819333));
#218771=CARTESIAN_POINT('Ctrl Pts',(6.9113618840989,-3.86978930538546,23.196027616382));
#218772=CARTESIAN_POINT('Ctrl Pts',(7.25369617879374,-3.17914186783272,
23.2256442515566));
#218773=CARTESIAN_POINT('Ctrl Pts',(7.39550028729147,-2.83365618355761,
23.2399565835744));
#218774=CARTESIAN_POINT('Ctrl Pts',(7.52190510346137,-2.45067023357923,
23.2560595967062));
#218775=CARTESIAN_POINT('Ctrl Pts',(7.53124576320613,-2.42181300279579,
23.2572744662538));
#218776=CARTESIAN_POINT('Ctrl Pts',(7.54444376636864,-2.38022398091136,
23.2590281694345));
#218777=CARTESIAN_POINT('Ctrl Pts',(7.54843533335873,-2.36753499649502,
23.2595636027704));
#218778=CARTESIAN_POINT('Ctrl Pts',(7.55526946954872,-2.34561665725087,
23.2604890854947));
#218779=CARTESIAN_POINT('Ctrl Pts',(7.55812718220442,-2.33639203843616,
23.2608787703606));
#218780=CARTESIAN_POINT('Ctrl Pts',(7.56407399149598,-2.31707080925271,
23.2616953422492));
#218781=CARTESIAN_POINT('Ctrl Pts',(7.5671597793045,-2.30697320261887,23.2621223054978));
#218782=CARTESIAN_POINT('Ctrl Pts',(7.57491374088395,-2.2814170109135,23.2632034130755));
#218783=CARTESIAN_POINT('Ctrl Pts',(7.57955480890161,-2.26595027651699,
23.2638581664163));
#218784=CARTESIAN_POINT('Ctrl Pts',(7.59676134431879,-2.20796374506986,
23.2663144912943));
#218785=CARTESIAN_POINT('Ctrl Pts',(7.60901656982578,-2.16535299909108,
23.2681226697767));
#218786=CARTESIAN_POINT('Ctrl Pts',(7.71692618155002,-1.77792552160713,
23.2845846814515));
#218787=CARTESIAN_POINT('Ctrl Pts',(7.78943845978878,-1.42709787813032,
23.2996300913183));
#218788=CARTESIAN_POINT('Ctrl Pts',(7.89177819041648,-0.679240925806107,
23.3313399115327));
#218789=CARTESIAN_POINT('Ctrl Pts',(7.9159203528083,-0.282401844542897,
23.3479481870861));
#218790=CARTESIAN_POINT('Ctrl Pts',(7.90874449395551,0.213007664597464,
23.3682922702164));
#218791=CARTESIAN_POINT('Ctrl Pts',(7.90548160012989,0.31140441566165,23.3723155235435));
#218792=CARTESIAN_POINT('Ctrl Pts',(7.89657317702969,0.483182091164209,
23.3793122201177));
#218793=CARTESIAN_POINT('Ctrl Pts',(7.89173857881504,0.556592493744786,
23.3822937120554));
#218794=CARTESIAN_POINT('Ctrl Pts',(7.88327634409368,0.662529156606506,
23.3865857192254));
#218795=CARTESIAN_POINT('Ctrl Pts',(7.88046975434703,0.695116725743285,
23.3879045656946));
#218796=CARTESIAN_POINT('Ctrl Pts',(7.87520742344474,0.752083336704774,
23.3902077937332));
#218797=CARTESIAN_POINT('Ctrl Pts',(7.87284037199482,0.776470082609166,
23.3911930542105));
#218798=CARTESIAN_POINT('Ctrl Pts',(7.86802560638372,0.823787498717093,
23.3931034680931));
#218799=CARTESIAN_POINT('Ctrl Pts',(7.86559084400334,0.846719235709332,
23.3940287398877));
#218800=CARTESIAN_POINT('Ctrl Pts',(7.85951754555579,0.90163239837388,23.3962431703346));
#218801=CARTESIAN_POINT('Ctrl Pts',(7.85578402149688,0.933602939070093,
23.3975313910599));
#218802=CARTESIAN_POINT('Ctrl Pts',(7.84125686170906,1.05173786091209,23.402288366475));
#218803=CARTESIAN_POINT('Ctrl Pts',(7.82923981079504,1.13774595282398,23.4057454188129));
#218804=CARTESIAN_POINT('Ctrl Pts',(7.71935605519007,1.83966906679815,23.4339394987534));
#218805=CARTESIAN_POINT('Ctrl Pts',(7.55037928510078,2.44227265188441,23.458062001236));
#218806=CARTESIAN_POINT('Ctrl Pts',(7.19784249574146,3.29622182712517,23.4926743723737));
#218807=CARTESIAN_POINT('Ctrl Pts',(7.06760844407218,3.5669210739248,23.5037563358507));
#218808=CARTESIAN_POINT('Ctrl Pts',(6.74681534517606,4.14678552794455,23.5284160059575));
#218809=CARTESIAN_POINT('Ctrl Pts',(6.54973407530411,4.45155026875225,23.5419993385837));
#218810=CARTESIAN_POINT('Ctrl Pts',(6.32232909439529,4.75524572731487,23.5570954889225));
#218811=CARTESIAN_POINT('Ctrl Pts',(6.31214742211871,4.76875266933936,23.5577703565172));
#218812=CARTESIAN_POINT('Ctrl Pts',(6.29382758189763,4.79289418736283,23.558982972903));
#218813=CARTESIAN_POINT('Ctrl Pts',(6.28570556507965,4.80354097186587,23.5595199990598));
#218814=CARTESIAN_POINT('Ctrl Pts',(6.27313985677971,4.81992634947665,23.5603500247477));
#218815=CARTESIAN_POINT('Ctrl Pts',(6.26871521381598,4.8256795629979,23.5606421387505));
#218816=CARTESIAN_POINT('Ctrl Pts',(6.26057668873738,4.83623173011331,23.5611791731473));
#218817=CARTESIAN_POINT('Ctrl Pts',(6.25686518756732,4.84103251871604,23.5614239804994));
#218818=CARTESIAN_POINT('Ctrl Pts',(6.24885271431672,4.85137196367426,23.5619522660716));
#218819=CARTESIAN_POINT('Ctrl Pts',(6.24454989634671,4.85690917835383,23.5622358333464));
#218820=CARTESIAN_POINT('Ctrl Pts',(6.23292294590525,4.87183068861322,23.5630017503862));
#218821=CARTESIAN_POINT('Ctrl Pts',(6.22558500218917,4.88120416358291,23.563484779959));
#218822=CARTESIAN_POINT('Ctrl Pts',(6.19155479585651,4.92447271948966,23.5657234046176));
#218823=CARTESIAN_POINT('Ctrl Pts',(6.16460703934914,4.95816521511221,23.5674919902993));
#218824=CARTESIAN_POINT('Ctrl Pts',(5.58340269139946,5.6727757620947,23.6055864171149));
#218825=CARTESIAN_POINT('Ctrl Pts',(4.91994584182078,6.25689846845801,23.6481654894897));
#218826=CARTESIAN_POINT('Ctrl Pts',(3.82910546589323,6.93447208857148,23.7055327940616));
#218827=CARTESIAN_POINT('Ctrl Pts',(3.46799611524375,7.12193899185499,23.7229781519623));
#218828=CARTESIAN_POINT('Ctrl Pts',(3.07089608888263,7.29068933387601,23.740493399286));
#218829=CARTESIAN_POINT('Ctrl Pts',(3.04769828864377,7.30041703656497,23.7415109537161));
#218830=CARTESIAN_POINT('Ctrl Pts',(3.0146217872346,7.3141021122818,23.7429538649886));
#218831=CARTESIAN_POINT('Ctrl Pts',(3.00478100220456,7.31815040559034,23.7433821545098));
#218832=CARTESIAN_POINT('Ctrl Pts',(2.98781577873539,7.32508955480979,23.7441187990631));
#218833=CARTESIAN_POINT('Ctrl Pts',(2.98069525068141,7.32798989741475,23.7444274594668));
#218834=CARTESIAN_POINT('Ctrl Pts',(2.96708430414006,7.33351080483567,23.7450164781509));
#218835=CARTESIAN_POINT('Ctrl Pts',(2.96059461652865,7.33613314419733,23.7452968933152));
#218836=CARTESIAN_POINT('Ctrl Pts',(2.9454310857152,7.34223699395543,23.745951102279));
#218837=CARTESIAN_POINT('Ctrl Pts',(2.93675452747391,7.34571175599954,23.7463246789888));
#218838=CARTESIAN_POINT('Ctrl Pts',(2.90693582103706,7.3575921860718,23.7476059472233));
#218839=CARTESIAN_POINT('Ctrl Pts',(2.8857634934038,7.36592205462879,23.7485112059678));
#218840=CARTESIAN_POINT('Ctrl Pts',(2.66855034729262,7.45030035004233,23.7577531097291));
#218841=CARTESIAN_POINT('Ctrl Pts',(2.46958072402386,7.51859793258854,23.7658376899532));
#218842=CARTESIAN_POINT('Ctrl Pts',(1.52842406226246,7.8002557065653,23.8025865928719));
#218843=CARTESIAN_POINT('Ctrl Pts',(0.760377522155833,7.91213087908242,
23.8279140890067));
#218844=CARTESIAN_POINT('Ctrl Pts',(-0.169589144134691,7.91075831512624,
23.8609782525965));
#218845=CARTESIAN_POINT('Ctrl Pts',(-0.327455181626436,7.90579709125895,
23.8666904079398));
#218846=CARTESIAN_POINT('Ctrl Pts',(-0.598038368836354,7.88917505253697,
23.8767828271517));
#218847=CARTESIAN_POINT('Ctrl Pts',(-0.710849436313869,7.87981118448368,
23.8810811160126));
#218848=CARTESIAN_POINT('Ctrl Pts',(-0.886189323553663,7.86146125168594,
23.8879480214623));
#218849=CARTESIAN_POINT('Ctrl Pts',(-0.9488761648537,7.85414147724108,23.8904412671906));
#218850=CARTESIAN_POINT('Ctrl Pts',(-1.02277277304069,7.8446151397523,23.893427198762));
#218851=CARTESIAN_POINT('Ctrl Pts',(-1.03407061448032,7.84313386334491,
23.8938849600546));
#218852=CARTESIAN_POINT('Ctrl Pts',(-1.051462083779,7.84081541163407,23.8945915055022));
#218853=CARTESIAN_POINT('Ctrl Pts',(-1.05755803322652,7.83999552544475,
23.8948395162447));
#218854=CARTESIAN_POINT('Ctrl Pts',(-1.06822465264976,7.83854823141273,
23.8952740997024));
#218855=CARTESIAN_POINT('Ctrl Pts',(-1.0727957469833,7.83792393238386,23.8954605354177));
#218856=CARTESIAN_POINT('Ctrl Pts',(-1.082388951832,7.8366051872511,23.895852214784));
#218857=CARTESIAN_POINT('Ctrl Pts',(-1.08741094490711,7.8359099114665,23.896057494488));
#218858=CARTESIAN_POINT('Ctrl Pts',(-1.10139481637611,7.8339601956773,23.8966297564365));
#218859=CARTESIAN_POINT('Ctrl Pts',(-1.11035519838549,7.83269520800184,
23.8969971917991));
#218860=CARTESIAN_POINT('Ctrl Pts',(-1.14619299851865,7.82757305199663,
23.8984697273036));
#218861=CARTESIAN_POINT('Ctrl Pts',(-1.17305245260442,7.82359292095127,
23.8995799857741));
#218862=CARTESIAN_POINT('Ctrl Pts',(-1.22570373306422,7.81551363400674,
23.9017687031059));
#218863=CARTESIAN_POINT('Ctrl Pts',(-1.251496848543,7.81142487782648,23.9028467441788));
#218864=CARTESIAN_POINT('Ctrl Pts',(-1.30055829169142,7.80339836456902,
23.9049078037622));
#218865=CARTESIAN_POINT('Ctrl Pts',(-1.32383022493121,7.79948404879771,
23.9058899611385));
#218866=CARTESIAN_POINT('Ctrl Pts',(-1.63020491389335,7.7465414150172,23.9188765796201));
#218867=CARTESIAN_POINT('Ctrl Pts',(-1.9104399982384,7.68223131036253,23.9313818707812));
#218868=CARTESIAN_POINT('Ctrl Pts',(-2.50861976885112,7.51019717499976,
23.9587146320488));
#218869=CARTESIAN_POINT('Ctrl Pts',(-2.82449353229944,7.3971940140238,23.973547315303));
#218870=CARTESIAN_POINT('Ctrl Pts',(-3.53457856870992,7.09102509063753,
24.0071303848532));
#218871=CARTESIAN_POINT('Ctrl Pts',(-3.92182102906554,6.88442095650999,
24.0255959998223));
#218872=CARTESIAN_POINT('Ctrl Pts',(-4.32328892044129,6.62530488812017,
24.0449582223639));
#218873=CARTESIAN_POINT('Ctrl Pts',(-4.35642848561461,6.60356137508039,
24.0465587818311));
#218874=CARTESIAN_POINT('Ctrl Pts',(-4.40395512192688,6.5718647445142,24.0488580404523));
#218875=CARTESIAN_POINT('Ctrl Pts',(-4.41847462132928,6.56211162353109,
24.0495609913981));
#218876=CARTESIAN_POINT('Ctrl Pts',(-4.44368807215542,6.54505347844184,
24.0507826534891));
#218877=CARTESIAN_POINT('Ctrl Pts',(-4.45439663674166,6.53777021024828,
24.0513018200204));
#218878=CARTESIAN_POINT('Ctrl Pts',(-4.47501688372335,6.52367148010543,
24.0523021403465));
#218879=CARTESIAN_POINT('Ctrl Pts',(-4.48493099847679,6.51685964477934,
24.0527833678447));
#218880=CARTESIAN_POINT('Ctrl Pts',(-4.50836697485973,6.50067833736237,
24.0539216309815));
#218881=CARTESIAN_POINT('Ctrl Pts',(-4.52187523571779,6.49128923871956,
24.0545782598247));
#218882=CARTESIAN_POINT('Ctrl Pts',(-4.56882156385422,6.45844090697395,
24.0568623133264));
#218883=CARTESIAN_POINT('Ctrl Pts',(-4.60210736080558,6.43476474350345,
24.058485385381));
#218884=CARTESIAN_POINT('Ctrl Pts',(-5.06245282324008,6.10192226358925,
24.0809878398833));
#218885=CARTESIAN_POINT('Ctrl Pts',(-5.45775693711108,5.75107127150145,
24.1008530284542));
#218886=CARTESIAN_POINT('Ctrl Pts',(-6.09593885443711,5.05913775650199,
24.1356063278963));
#218887=CARTESIAN_POINT('Ctrl Pts',(-6.35231153515151,4.73323008413558,
24.1506263207329));
#218888=CARTESIAN_POINT('Ctrl Pts',(-6.67058944218628,4.25589724918746,
24.172251464074));
#218889=CARTESIAN_POINT('Ctrl Pts',(-6.7551394000578,4.12037785277874,24.1783576106507));
#218890=CARTESIAN_POINT('Ctrl Pts',(-6.87257444266999,3.91880817894615,
24.1874961017926));
#218891=CARTESIAN_POINT('Ctrl Pts',(-6.90873163945283,3.85470669998232,
24.1904103737995));
#218892=CARTESIAN_POINT('Ctrl Pts',(-6.95033606793557,3.77848184844983,
24.1938940179655));
#218893=CARTESIAN_POINT('Ctrl Pts',(-6.95665433903014,3.76683646325639,
24.1944267344584));
#218894=CARTESIAN_POINT('Ctrl Pts',(-6.96630449608345,3.74894289212901,
24.1952461012844));
#218895=CARTESIAN_POINT('Ctrl Pts',(-6.96965731386259,3.74270598197403,
24.1955318503646));
#218896=CARTESIAN_POINT('Ctrl Pts',(-6.97573747076955,3.7313591743994,24.1960520052883));
#218897=CARTESIAN_POINT('Ctrl Pts',(-6.97846758255995,3.72625076295222,
24.1962862899482));
#218898=CARTESIAN_POINT('Ctrl Pts',(-6.98438646242607,3.71514641206537,
24.1967958044797));
#218899=CARTESIAN_POINT('Ctrl Pts',(-6.98757312319085,3.70914935898864,
24.1970711269789));
#218900=CARTESIAN_POINT('Ctrl Pts',(-6.99618478085933,3.69289239062106,
24.1978179068998));
#218901=CARTESIAN_POINT('Ctrl Pts',(-7.00159491556002,3.68262465275913,
24.1982900272373));
#218902=CARTESIAN_POINT('Ctrl Pts',(-7.02684730614991,3.63444207383412,
24.2005078078407));
#218903=CARTESIAN_POINT('Ctrl Pts',(-7.04640404639417,3.59637903504548,
24.2022664615881));
#218904=CARTESIAN_POINT('Ctrl Pts',(-7.43354843992086,2.8276032463904,24.2379501882632));
#218905=CARTESIAN_POINT('Ctrl Pts',(-7.68588528680803,2.04449707151529,
24.2775250345033));
#218906=CARTESIAN_POINT('Ctrl Pts',(-7.84264991007195,1.05402552909513,
24.3223631292469));
#218907=CARTESIAN_POINT('Ctrl Pts',(-7.86514854992047,0.870385593894323,
24.3304927693579));
#218908=CARTESIAN_POINT('Ctrl Pts',(-7.89796965140514,0.493381558045493,
24.3467494714145));
#218909=CARTESIAN_POINT('Ctrl Pts',(-7.90767381607238,0.300086478573789,
24.3548534681929));
#218910=CARTESIAN_POINT('Ctrl Pts',(-7.91075720999831,0.0713253403884549,
24.3641665519708));
#218911=CARTESIAN_POINT('Ctrl Pts',(-7.91099671319619,0.0360275876546984,
24.3655958226027));
#218912=CARTESIAN_POINT('Ctrl Pts',(-7.9110010339876,-0.0108545984166303,
24.3674840000062));
#218913=CARTESIAN_POINT('Ctrl Pts',(-7.91097665939552,-0.0224383175062282,
24.3679497094544));
#218914=CARTESIAN_POINT('Ctrl Pts',(-7.91089798963952,-0.0407309266759933,
24.3686838457705));
#218915=CARTESIAN_POINT('Ctrl Pts',(-7.91086060247442,-0.0474398501254188,
24.3689528193622));
#218916=CARTESIAN_POINT('Ctrl Pts',(-7.91077194961176,-0.0603915182460814,
24.3694715465466));
#218917=CARTESIAN_POINT('Ctrl Pts',(-7.91072182858753,-0.0666342644040845,
24.3697213370205));
#218918=CARTESIAN_POINT('Ctrl Pts',(-7.9105857155312,-0.0814090955993259,
24.3703119599698));
#218919=CARTESIAN_POINT('Ctrl Pts',(-7.91049330944747,-0.0899411219108776,
24.3706525843056));
#218920=CARTESIAN_POINT('Ctrl Pts',(-7.91018172436542,-0.114970912963646,
24.3716505551158));
#218921=CARTESIAN_POINT('Ctrl Pts',(-7.90992473654661,-0.131468208588591,
24.3723066743381));
#218922=CARTESIAN_POINT('Ctrl Pts',(-7.90762753838329,-0.254267512867061,
24.3771783845604));
#218923=CARTESIAN_POINT('Ctrl Pts',(-7.9034960842377,-0.360521898386537,
24.3813255566221));
#218924=CARTESIAN_POINT('Ctrl Pts',(-7.88314449914637,-0.704926385295538,
24.3945633691707));
#218925=CARTESIAN_POINT('Ctrl Pts',(-7.85828919467957,-0.942438342881225,
24.4033702667052));
#218926=CARTESIAN_POINT('Ctrl Pts',(-7.71671606965057,-1.88220173239001,
24.4373544792518));
#218927=CARTESIAN_POINT('Ctrl Pts',(-7.51624662197628,-2.56832884594178,
24.4599268898903));
#218928=CARTESIAN_POINT('Ctrl Pts',(-7.17719781653705,-3.32965359525488,
24.4891771430719));
#218929=CARTESIAN_POINT('Ctrl Pts',(-7.12507541791424,-3.43977618596408,
24.4935282994109));
#218930=CARTESIAN_POINT('Ctrl Pts',(-7.05036059614297,-3.58864023334215,
24.4996299904059));
#218931=CARTESIAN_POINT('Ctrl Pts',(-7.02994985643906,-3.62846085429612,
24.5012841251903));
#218932=CARTESIAN_POINT('Ctrl Pts',(-6.9961428240933,-3.69306104968029,
24.5040067631413));
#218933=CARTESIAN_POINT('Ctrl Pts',(-6.98294991928229,-3.71794630510182,
24.5050651435584));
#218934=CARTESIAN_POINT('Ctrl Pts',(-6.91670089662859,-3.84131268985399,
24.5103621487923));
#218935=CARTESIAN_POINT('Ctrl Pts',(-6.86169517737788,-3.9387271538288,
24.5147045104919));
#218936=CARTESIAN_POINT('Ctrl Pts',(-6.7987475960701,-4.04488390688901,
24.5196494793193));
#218937=CARTESIAN_POINT('Ctrl Pts',(-6.79282838898946,-4.05481653965159,
24.5201142466962));
#218938=CARTESIAN_POINT('Ctrl Pts',(-6.78448037250994,-4.0687552177949,
24.5207694511315));
#218939=CARTESIAN_POINT('Ctrl Pts',(-6.78206972209699,-4.07277218019092,
24.5209586226559));
#218940=CARTESIAN_POINT('Ctrl Pts',(-6.7778604288556,-4.07977219225579,
24.5212888889154));
#218941=CARTESIAN_POINT('Ctrl Pts',(-6.77606337913362,-4.08275620330591,
24.5214298716049));
#218942=CARTESIAN_POINT('Ctrl Pts',(-6.77230116043796,-4.08899406233144,
24.5217249948599));
#218943=CARTESIAN_POINT('Ctrl Pts',(-6.77033561655297,-4.09224768172471,
24.5218791619662));
#218944=CARTESIAN_POINT('Ctrl Pts',(-6.76565839999338,-4.09997741498914,
24.522245979107));
#218945=CARTESIAN_POINT('Ctrl Pts',(-6.76294465005449,-4.10445222273462,
24.522458778058));
#218946=CARTESIAN_POINT('Ctrl Pts',(-6.7537128175157,-4.11964093720143,
24.5231825865886));
#218947=CARTESIAN_POINT('Ctrl Pts',(-6.74717374176657,-4.13034196740307,
24.5236950902292));
#218948=CARTESIAN_POINT('Ctrl Pts',(-6.60494299565158,-4.36185985154354,
24.5348376621657));
#218949=CARTESIAN_POINT('Ctrl Pts',(-6.4585175107822,-4.57587379775202,
24.5462101414511));
#218950=CARTESIAN_POINT('Ctrl Pts',(-5.93362054323009,-5.26755675728417,
24.5855297558398));
#218951=CARTESIAN_POINT('Ctrl Pts',(-5.51055126598146,-5.7086709607868,
24.6147994608072));
#218952=CARTESIAN_POINT('Ctrl Pts',(-4.87736048201414,-6.23220413840931,
24.6519098357519));
#218953=CARTESIAN_POINT('Ctrl Pts',(-4.70831640251503,-6.36087882075856,
24.6612975136818));
#218954=CARTESIAN_POINT('Ctrl Pts',(-4.3667788710594,-6.59976904046135,
24.6791993648328));
#218955=CARTESIAN_POINT('Ctrl Pts',(-4.19478175087233,-6.71040416655264,
24.6877264794834));
#218956=CARTESIAN_POINT('Ctrl Pts',(-4.00099582124599,-6.82468863831104,
24.6968158363949));
#218957=CARTESIAN_POINT('Ctrl Pts',(-3.98326946681432,-6.83504988534656,
24.6976426710025));
#218958=CARTESIAN_POINT('Ctrl Pts',(-3.95822819708615,-6.84955627909286,
24.6988042682525));
#218959=CARTESIAN_POINT('Ctrl Pts',(-3.95094678555921,-6.85375890872563,
24.699141269475));
#218960=CARTESIAN_POINT('Ctrl Pts',(-3.93826734533509,-6.86105021077644,
24.6997267802067));
#218961=CARTESIAN_POINT('Ctrl Pts',(-3.93287235493141,-6.86414413588494,
24.6999754937399));
#218962=CARTESIAN_POINT('Ctrl Pts',(-3.92160884169991,-6.87058590952261,
24.7004938852152));
#218963=CARTESIAN_POINT('Ctrl Pts',(-3.91573966552925,-6.87393260947116,
24.7007635185039));
#218964=CARTESIAN_POINT('Ctrl Pts',(-3.90185570940555,-6.88182591547928,
24.7014002019519));
#218965=CARTESIAN_POINT('Ctrl Pts',(-3.89383725048185,-6.88636605006852,
24.7017670014679));
#218966=CARTESIAN_POINT('Ctrl Pts',(-3.86736958884071,-6.90129130566539,
24.7029747709186));
#218967=CARTESIAN_POINT('Ctrl Pts',(-3.84888655231765,-6.91161642014936,
24.7038134246));
#218968=CARTESIAN_POINT('Ctrl Pts',(-3.51538507314411,-7.09616654320072,
24.7188609830471));
#218969=CARTESIAN_POINT('Ctrl Pts',(-3.18886624465887,-7.2487709143762,
24.7322040924546));
#218970=CARTESIAN_POINT('Ctrl Pts',(-2.29074197388234,-7.59604483954615,
24.7663726598042));
#218971=CARTESIAN_POINT('Ctrl Pts',(-1.70546352257685,-7.74846582425057,
24.7859460246541));
#218972=CARTESIAN_POINT('Ctrl Pts',(-0.823835515641905,-7.87324068167831,
24.8173742432762));
#218973=CARTESIAN_POINT('Ctrl Pts',(-0.537129896616979,-7.89797987771685,
24.8279251577688));
#218974=CARTESIAN_POINT('Ctrl Pts',(-0.23228753765349,-7.90760826633078,
24.8400905462782));
#218975=CARTESIAN_POINT('Ctrl Pts',(-0.214830469100922,-7.90810178640301,
24.8407905137678));
#218976=CARTESIAN_POINT('Ctrl Pts',(-0.190997205769173,-7.9086965884587,
24.8417508054288));
#218977=CARTESIAN_POINT('Ctrl Pts',(-0.184622428222553,-7.90884797043401,
24.8420081098077));
#218978=CARTESIAN_POINT('Ctrl Pts',(-0.17448734722532,-7.90907638802005,
24.842417900949));
#218979=CARTESIAN_POINT('Ctrl Pts',(-0.170727147818328,-7.90915844997314,
24.8425700922576));
#218980=CARTESIAN_POINT('Ctrl Pts',(-0.163423864046552,-7.90931262495937,
24.8428659872182));
#218981=CARTESIAN_POINT('Ctrl Pts',(-0.159880786254882,-7.9093850388499,
24.8430096732791));
#218982=CARTESIAN_POINT('Ctrl Pts',(-0.151426390271033,-7.90955214777615,
24.8433528582454));
#218983=CARTESIAN_POINT('Ctrl Pts',(-0.146515034872999,-7.90964464906047,
24.8435524842301));
#218984=CARTESIAN_POINT('Ctrl Pts',(-0.131868276137306,-7.90990686195429,
24.8441485879744));
#218985=CARTESIAN_POINT('Ctrl Pts',(-0.122132673431918,-7.91006317392594,
24.8445458345057));
#218986=CARTESIAN_POINT('Ctrl Pts',(-0.0413583157847655,-7.91121090489695,
24.8478500366152));
#218987=CARTESIAN_POINT('Ctrl Pts',(0.0296885311668372,-7.91126326767768,
24.8508097437689));
#218988=CARTESIAN_POINT('Ctrl Pts',(0.371648363382786,-7.906909019316,24.8652814699334));
#218989=CARTESIAN_POINT('Ctrl Pts',(0.642197525837218,-7.88954328864179,
24.8774108105545));
#218990=CARTESIAN_POINT('Ctrl Pts',(1.37625939628521,-7.8044170626596,24.9112730609767));
#218991=CARTESIAN_POINT('Ctrl Pts',(1.83551795534609,-7.7093390018141,24.9334554800228));
#218992=CARTESIAN_POINT('Ctrl Pts',(2.77853646681446,-7.42501143978334,
24.9786338293376));
#218993=CARTESIAN_POINT('Ctrl Pts',(3.25762435748081,-7.22766042612521,
25.0013312415204));
#218994=CARTESIAN_POINT('Ctrl Pts',(3.74370540033309,-6.96919765749632,
25.0237430468356));
#218995=CARTESIAN_POINT('Ctrl Pts',(3.77322141090087,-6.95326156089598,
25.0251018893287));
#218996=CARTESIAN_POINT('Ctrl Pts',(3.81322953016855,-6.93133086134579,
25.0269411233938));
#218997=CARTESIAN_POINT('Ctrl Pts',(3.82381035852238,-6.92549935404854,
25.0274272878759));
#218998=CARTESIAN_POINT('Ctrl Pts',(3.84050402086261,-6.91624890530693,
25.0281939342265));
#218999=CARTESIAN_POINT('Ctrl Pts',(3.8466257233662,-6.91284605637047,25.0284749869321));
#219000=CARTESIAN_POINT('Ctrl Pts',(3.85843899920075,-6.90625890210985,
25.0290171873585));
#219001=CARTESIAN_POINT('Ctrl Pts',(3.86413116851248,-6.90307568018211,
25.0292783732753));
#219002=CARTESIAN_POINT('Ctrl Pts',(3.8775999230906,-6.89552169273847,25.0298962239147));
#219003=CARTESIAN_POINT('Ctrl Pts',(3.88537307210499,-6.89114480110596,
25.0302526703099));
#219004=CARTESIAN_POINT('Ctrl Pts',(3.9081764265212,-6.87825387826642,25.0312979690574));
#219005=CARTESIAN_POINT('Ctrl Pts',(3.9231862116198,-6.86970373076358,25.0319855342826));
#219006=CARTESIAN_POINT('Ctrl Pts',(4.03552598466638,-6.80522243701821,
25.037128148783));
#219007=CARTESIAN_POINT('Ctrl Pts',(4.13168575574991,-6.74727326121044,
25.0415105145102));
#219008=CARTESIAN_POINT('Ctrl Pts',(4.44411880129165,-6.54980570291558,
25.055710864306));
#219009=CARTESIAN_POINT('Ctrl Pts',(4.65482492530766,-6.40177812230887,
25.0652199786224));
#219010=CARTESIAN_POINT('Ctrl Pts',(5.37701547321621,-5.83987644079141,
25.0981283335534));
#219011=CARTESIAN_POINT('Ctrl Pts',(5.84365389425602,-5.37290148949582,
25.1198194011806));
#219012=CARTESIAN_POINT('Ctrl Pts',(6.3976392482897,-4.6598637118227,25.1526893801091));
#219013=CARTESIAN_POINT('Ctrl Pts',(6.53904646526501,-4.45925850621323,
25.1619795408695));
#219014=CARTESIAN_POINT('Ctrl Pts',(6.68068157045178,-4.23706787199869,
25.172490887677));
#219015=CARTESIAN_POINT('Ctrl Pts',(6.69038456697445,-4.22173006447441,
25.1732171561989));
#219016=CARTESIAN_POINT('Ctrl Pts',(6.70479050270604,-4.19878379033217,
25.1743045679438));
#219017=CARTESIAN_POINT('Ctrl Pts',(6.70953349436633,-4.1912004593394,25.1746640793592));
#219018=CARTESIAN_POINT('Ctrl Pts',(6.71766400599599,-4.17815182196231,
25.1752829159307));
#219019=CARTESIAN_POINT('Ctrl Pts',(6.72105774780615,-4.17269039052995,
25.1755419940517));
#219020=CARTESIAN_POINT('Ctrl Pts',(6.72767359490597,-4.1620147249433,25.1760485485514));
#219021=CARTESIAN_POINT('Ctrl Pts',(6.73089630644967,-4.1568008710797,25.1762960010598));
#219022=CARTESIAN_POINT('Ctrl Pts',(6.7386333945356,-4.14425085787144,25.1768917635437));
#219023=CARTESIAN_POINT('Ctrl Pts',(6.74314185086959,-4.13691106713021,
25.1772402992153));
#219024=CARTESIAN_POINT('Ctrl Pts',(6.75599510237946,-4.11590906949252,
25.1782378783861));
#219025=CARTESIAN_POINT('Ctrl Pts',(6.76431040387185,-4.10222891217102,
25.1788880171649));
#219026=CARTESIAN_POINT('Ctrl Pts',(6.78353065928454,-4.07039081930573,
25.1804017587042));
#219027=CARTESIAN_POINT('Ctrl Pts',(6.79440430851134,-4.05221417390089,
25.1812664640886));
#219028=CARTESIAN_POINT('Ctrl Pts',(6.89620295312634,-3.88048347883253,
25.1894395623873));
#219029=CARTESIAN_POINT('Ctrl Pts',(6.98197836194144,-3.72394168540918,
25.1969144766021));
#219030=CARTESIAN_POINT('Ctrl Pts',(7.22370856312189,-3.24501754425016,
25.2196534681444));
#219031=CARTESIAN_POINT('Ctrl Pts',(7.36314826699406,-2.91481557483264,
25.2351396661347));
#219032=CARTESIAN_POINT('Ctrl Pts',(7.6246787059487,-2.15551973768225,25.2696227997907));
#219033=CARTESIAN_POINT('Ctrl Pts',(7.73385175208269,-1.72323901142584,
25.2884709061032));
#219034=CARTESIAN_POINT('Ctrl Pts',(7.81128592684167,-1.25250003537469,
25.3083014889854));
#219035=CARTESIAN_POINT('Ctrl Pts',(7.81628638783297,-1.22090592641171,
25.3096294948078));
#219036=CARTESIAN_POINT('Ctrl Pts',(7.83278128558146,-1.11243028148906,
25.3141797041729));
#219037=CARTESIAN_POINT('Ctrl Pts',(7.84333412809913,-1.03540989707081,
25.3173942729427));
#219038=CARTESIAN_POINT('Ctrl Pts',(7.85505517872804,-0.939356833106798,
25.3213873915063));
#219039=CARTESIAN_POINT('Ctrl Pts',(7.85729202517308,-0.920459207756815,
25.3221722474698));
#219040=CARTESIAN_POINT('Ctrl Pts',(7.89079523881774,-0.62838875677535,
25.3342917221045));
#219041=CARTESIAN_POINT('Ctrl Pts',(7.90786791627459,-0.353769153556332,
25.3455618527819));
#219042=CARTESIAN_POINT('Ctrl Pts',(7.9110116725741,-0.0382375612866903,
25.3583364229323));
#219043=CARTESIAN_POINT('Ctrl Pts',(7.91110373604007,0.00234377887646953,
25.3599761443587));
#219044=CARTESIAN_POINT('Ctrl Pts',(7.9107452451188,0.0684133312128098,
25.3626405031876));
#219045=CARTESIAN_POINT('Ctrl Pts',(7.91048375170222,0.0939017384435331,
25.3636670958938));
#219046=CARTESIAN_POINT('Ctrl Pts',(7.90979642597227,0.139440589538119,
25.3654990239649));
#219047=CARTESIAN_POINT('Ctrl Pts',(7.90941752865496,0.159491499452698,
25.3663048544668));
#219048=CARTESIAN_POINT('Ctrl Pts',(7.90853838875326,0.198218546501772,
25.3678597925179));
#219049=CARTESIAN_POINT('Ctrl Pts',(7.90804822296554,0.216894776292699,
25.3686090045103));
#219050=CARTESIAN_POINT('Ctrl Pts',(7.90651131759177,0.268485012838611,
25.3706767930177));
#219051=CARTESIAN_POINT('Ctrl Pts',(7.90532521507062,0.301394547522225,
25.3719938198419));
#219052=CARTESIAN_POINT('Ctrl Pts',(7.89979268774025,0.43220303528134,25.377221003294));
#219053=CARTESIAN_POINT('Ctrl Pts',(7.89383285467975,0.530025611400865,
25.3811127331075));
#219054=CARTESIAN_POINT('Ctrl Pts',(7.87390853319274,0.780337998346133,
25.3910346037837));
#219055=CARTESIAN_POINT('Ctrl Pts',(7.85733155752323,0.932579664573326,
25.3970339355675));
#219056=CARTESIAN_POINT('Ctrl Pts',(7.79026180895559,1.41732372848122,25.4160852667382));
#219057=CARTESIAN_POINT('Ctrl Pts',(7.72298793484054,1.74712495566934,25.4289571672772));
#219058=CARTESIAN_POINT('Ctrl Pts',(7.60799596606838,2.17092139138167,25.4458421632243));
#219059=CARTESIAN_POINT('Ctrl Pts',(7.57912505558121,2.26966198404375,25.4498026946971));
#219060=CARTESIAN_POINT('Ctrl Pts',(7.47861211052378,2.59008687786884,25.4627866038761));
#219061=CARTESIAN_POINT('Ctrl Pts',(7.3991049333707,2.80916880410323,25.4718697677481));
#219062=CARTESIAN_POINT('Ctrl Pts',(7.30055450654627,3.04736636713169,25.4821799840283));
#219063=CARTESIAN_POINT('Ctrl Pts',(7.29095117871762,3.07027177693828,25.4831760112892));
#219064=CARTESIAN_POINT('Ctrl Pts',(7.27639059424223,3.10454743237777,25.4846736650364));
#219065=CARTESIAN_POINT('Ctrl Pts',(7.27151421404099,3.11595184069142,25.4851731616243));
#219066=CARTESIAN_POINT('Ctrl Pts',(7.26270688693184,3.13641630061166,25.4860715784433));
#219067=CARTESIAN_POINT('Ctrl Pts',(7.25878575188677,3.14548055847955,25.4864702544068));
#219068=CARTESIAN_POINT('Ctrl Pts',(7.25042886510551,3.1646998392054,25.4873171404528));
#219069=CARTESIAN_POINT('Ctrl Pts',(7.24598873004309,3.1748529294128,25.4877654557867));
#219070=CARTESIAN_POINT('Ctrl Pts',(7.2367136458911,3.1959411070766,25.4886985151989));
#219071=CARTESIAN_POINT('Ctrl Pts',(7.23187521101558,3.20687462862538,25.4891833400564));
#219072=CARTESIAN_POINT('Ctrl Pts',(7.21968788403927,3.23424675784679,25.4903997320156));
#219073=CARTESIAN_POINT('Ctrl Pts',(7.21230762943266,3.25067129811652,25.4911320063211));
#219074=CARTESIAN_POINT('Ctrl Pts',(7.19122012396466,3.29717557984885,25.4932119767452));
#219075=CARTESIAN_POINT('Ctrl Pts',(7.17738037253587,3.32719471070576,25.4945624994365));
#219076=CARTESIAN_POINT('Ctrl Pts',(7.13040926050307,3.42742051297302,25.4990968945706));
#219077=CARTESIAN_POINT('Ctrl Pts',(7.09643293789722,3.49722560515425,25.5022968751233));
#219078=CARTESIAN_POINT('Ctrl Pts',(6.89905909328302,3.88801077382679,25.5204268912399));
#219079=CARTESIAN_POINT('Ctrl Pts',(6.71491863070724,4.19803628041317,25.5356224760104));
#219080=CARTESIAN_POINT('Ctrl Pts',(6.26102576116218,4.85551158733953,25.5691307109213));
#219081=CARTESIAN_POINT('Ctrl Pts',(5.98213724346328,5.19523767141024,25.5873250646001));
#219082=CARTESIAN_POINT('Ctrl Pts',(5.64180254628225,5.54585147478261,25.6071460179521));
#219083=CARTESIAN_POINT('Ctrl Pts',(5.60675453475713,5.58128194753369,25.6091625982154));
#219084=CARTESIAN_POINT('Ctrl Pts',(5.54932589252839,5.63825040348392,25.612428075788));
#219085=CARTESIAN_POINT('Ctrl Pts',(5.52714918811681,5.65999181408121,25.613679874725));
#219086=CARTESIAN_POINT('Ctrl Pts',(5.48741104182905,5.69849368914344,25.6159068792057));
#219087=CARTESIAN_POINT('Ctrl Pts',(5.46989941444212,5.71530494964329,25.6168827838942));
#219088=CARTESIAN_POINT('Ctrl Pts',(5.43580929070604,5.74773146706245,25.6187721389096));
#219089=CARTESIAN_POINT('Ctrl Pts',(5.41924019706674,5.76335625763105,25.6196857115009));
#219090=CARTESIAN_POINT('Ctrl Pts',(5.37344623946958,5.80616824823389,25.6221978623551));
#219091=CARTESIAN_POINT('Ctrl Pts',(5.3440826764968,5.83320620071678,25.6237944544804));
#219092=CARTESIAN_POINT('Ctrl Pts',(5.21856725896904,5.94703747714062,25.6305605916497));
#219093=CARTESIAN_POINT('Ctrl Pts',(5.12049551279392,6.03168510548819,25.63570283005));
#219094=CARTESIAN_POINT('Ctrl Pts',(4.84751173979438,6.25584441242179,25.6496685255382));
#219095=CARTESIAN_POINT('Ctrl Pts',(4.66868724654889,6.39040860716263,25.6584572578504));
#219096=CARTESIAN_POINT('Ctrl Pts',(4.12999990742665,6.76107143248479,25.6838643756109));
#219097=CARTESIAN_POINT('Ctrl Pts',(3.75629536910645,6.97561832569681,25.7001173469114));
#219098=CARTESIAN_POINT('Ctrl Pts',(2.97448813217734,7.34332891031433,25.7322979591062));
#219099=CARTESIAN_POINT('Ctrl Pts',(2.56748357372203,7.49533592773626,25.7481729311362));
#219100=CARTESIAN_POINT('Ctrl Pts',(2.12909288786566,7.61914434672653,25.765608404051));
#219101=CARTESIAN_POINT('Ctrl Pts',(2.10807011184755,7.62498770477838,25.766445447061));
#219102=CARTESIAN_POINT('Ctrl Pts',(2.07485610043199,7.63407180229317,25.7677696747495));
#219103=CARTESIAN_POINT('Ctrl Pts',(2.0626807793214,7.63737049784182,25.7682554755917));
#219104=CARTESIAN_POINT('Ctrl Pts',(1.93201888412045,7.67243587284948,25.7734733836137));
#219105=CARTESIAN_POINT('Ctrl Pts',(1.81281960381764,7.70147080990682,25.7782723792714));
#219106=CARTESIAN_POINT('Ctrl Pts',(1.67816650034748,7.7309707475096,25.7837782190235));
#219107=CARTESIAN_POINT('Ctrl Pts',(1.66332669103334,7.73417712603138,25.7843861573076));
#219108=CARTESIAN_POINT('Ctrl Pts',(1.6408891442759,7.7389575537035,25.7853072005107));
#219109=CARTESIAN_POINT('Ctrl Pts',(1.6332981248773,7.74056318600747,25.7856191254138));
#219110=CARTESIAN_POINT('Ctrl Pts',(1.62010578458997,7.74333332471392,25.7861617881929));
#219111=CARTESIAN_POINT('Ctrl Pts',(1.61450553184268,7.74450292906741,25.7863923318706));
#219112=CARTESIAN_POINT('Ctrl Pts',(1.60283515662178,7.74692706051798,25.786873143356));
#219113=CARTESIAN_POINT('Ctrl Pts',(1.59676482068339,7.74818053012619,25.7871234517536));
#219114=CARTESIAN_POINT('Ctrl Pts',(1.58473221214955,7.75065041426796,25.7876200479722));
#219115=CARTESIAN_POINT('Ctrl Pts',(1.57876999645954,7.75186708647838,25.7878663254889));
#219116=CARTESIAN_POINT('Ctrl Pts',(1.55850792793213,7.75597749469947,25.7887040134404));
#219117=CARTESIAN_POINT('Ctrl Pts',(1.54420152863638,7.75883854032758,25.7892967219912));
#219118=CARTESIAN_POINT('Ctrl Pts',(1.43303820497962,7.78074975059871,25.7939123453743));
#219119=CARTESIAN_POINT('Ctrl Pts',(1.33585056127449,7.79802332907676,25.7980108877753));
#219120=CARTESIAN_POINT('Ctrl Pts',(1.15757886474194,7.8262776171013,25.8056603166599));
#219121=CARTESIAN_POINT('Ctrl Pts',(1.07660814816163,7.8378265084089,25.8091802656747));
#219122=CARTESIAN_POINT('Ctrl Pts',(0.672199605143743,7.88912271075981,
25.8269452543213));
#219123=CARTESIAN_POINT('Ctrl Pts',(0.346714494306063,7.91011236524295,
25.8418212189034));
#219124=CARTESIAN_POINT('Ctrl Pts',(-0.762587769734756,7.91304050343044,
25.8928548188322));
#219125=CARTESIAN_POINT('Ctrl Pts',(-1.54218521638967,7.79870718468197,
25.928803940738));
#219126=CARTESIAN_POINT('Ctrl Pts',(-2.33945362149577,7.55733450619418,
25.9629217045627));
#219127=CARTESIAN_POINT('Ctrl Pts',(-2.38647167787547,7.54261898322933,
25.9649257826575));
#219128=CARTESIAN_POINT('Ctrl Pts',(-2.44707373976049,7.52302858842245,
25.9674988724865));
#219129=CARTESIAN_POINT('Ctrl Pts',(-2.46078561606207,7.51855459410687,
25.9680803986936));
#219130=CARTESIAN_POINT('Ctrl Pts',(-2.48256298439458,7.51138298550722,
25.9690029442039));
#219131=CARTESIAN_POINT('Ctrl Pts',(-2.49063646393958,7.50870983135632,
25.9693447296601));
#219132=CARTESIAN_POINT('Ctrl Pts',(-2.50510756887577,7.50389249623141,
25.9699569488164));
#219133=CARTESIAN_POINT('Ctrl Pts',(-2.51150678521652,7.50175314141431,
25.9702275336683));
#219134=CARTESIAN_POINT('Ctrl Pts',(-2.52642560573334,7.49674432509508,
25.9708580320195));
#219135=CARTESIAN_POINT('Ctrl Pts',(-2.53494307892034,7.49386852062725,
25.9712177457458));
#219136=CARTESIAN_POINT('Ctrl Pts',(-2.55920276136945,7.48563148872873,
25.9722415821931));
#219137=CARTESIAN_POINT('Ctrl Pts',(-2.57493303335665,7.48023511907965,
25.972904597896));
#219138=CARTESIAN_POINT('Ctrl Pts',(-2.6736230633045,7.44603068221338,25.9770590351514));
#219139=CARTESIAN_POINT('Ctrl Pts',(-2.75611674817165,7.41589200748601,
25.9805082406233));
#219140=CARTESIAN_POINT('Ctrl Pts',(-2.99817894961433,7.32285852699981,
25.990569059474));
#219141=CARTESIAN_POINT('Ctrl Pts',(-3.15622612659897,7.25614047146743,
25.9970587151788));
#219142=CARTESIAN_POINT('Ctrl Pts',(-3.63297433729236,7.03635909971397,
26.0164988608652));
#219143=CARTESIAN_POINT('Ctrl Pts',(-3.94369551238686,6.86703249493978,
26.028961394301));
#219144=CARTESIAN_POINT('Ctrl Pts',(-4.36300585777615,6.60065392374823,
26.046204784009));
#219145=CARTESIAN_POINT('Ctrl Pts',(-4.48184204138811,6.52054786404915,
26.0511465462194));
#219146=CARTESIAN_POINT('Ctrl Pts',(-4.72759217015259,6.34499696529504,
26.0615801299753));
#219147=CARTESIAN_POINT('Ctrl Pts',(-4.85394016042886,6.24887015542638,
26.0670714218476));
#219148=CARTESIAN_POINT('Ctrl Pts',(-5.27998823258973,5.90400593195878,
26.0862774113004));
#219149=CARTESIAN_POINT('Ctrl Pts',(-5.56414345744967,5.63700504895694,
26.1003112359413));
#219150=CARTESIAN_POINT('Ctrl Pts',(-5.84507556421056,5.33101217609701,
26.1168001978018));
#219151=CARTESIAN_POINT('Ctrl Pts',(-5.86259256903854,5.31174241822961,
26.1178400730554));
#219152=CARTESIAN_POINT('Ctrl Pts',(-5.88597098729484,5.28576823434068,
26.1192433036034));
#219153=CARTESIAN_POINT('Ctrl Pts',(-5.89191683180774,5.27913973451568,
26.1196015370934));
#219154=CARTESIAN_POINT('Ctrl Pts',(-5.90120952902763,5.26874486774975,
26.1201635129317));
#219155=CARTESIAN_POINT('Ctrl Pts',(-5.9045640087252,5.26498530421748,26.1203668045862));
#219156=CARTESIAN_POINT('Ctrl Pts',(-5.9109851508513,5.25777489620911,26.1207567647896));
#219157=CARTESIAN_POINT('Ctrl Pts',(-5.91405238963775,5.25432456603907,
26.1209433996392));
#219158=CARTESIAN_POINT('Ctrl Pts',(-5.92123335290712,5.24623246237463,
26.1213811846904));
#219159=CARTESIAN_POINT('Ctrl Pts',(-5.92534463861371,5.24158853613927,
26.1216324746744));
#219160=CARTESIAN_POINT('Ctrl Pts',(-5.93382148014275,5.23199075311297,
26.1221519244846));
#219161=CARTESIAN_POINT('Ctrl Pts',(-5.93818630295439,5.22703625679943,
26.1224201253125));
#219162=CARTESIAN_POINT('Ctrl Pts',(-5.94941777341498,5.21425522611201,
26.1231121250301));
#219163=CARTESIAN_POINT('Ctrl Pts',(-5.9562751689613,5.20642060496903,26.1235364346771));
#219164=CARTESIAN_POINT('Ctrl Pts',(-6.03733137419294,5.11344361171303,
26.1285731150626));
#219165=CARTESIAN_POINT('Ctrl Pts',(-6.10971212216422,5.02673770224553,
26.1332818418867));
#219166=CARTESIAN_POINT('Ctrl Pts',(-6.33177819953746,4.74883738029606,
26.1483337765984));
#219167=CARTESIAN_POINT('Ctrl Pts',(-6.47453002333946,4.55228792647149,
26.1589176161616));
#219168=CARTESIAN_POINT('Ctrl Pts',(-6.66606623623699,4.26129453619557,
26.1742173467374));
#219169=CARTESIAN_POINT('Ctrl Pts',(-6.72234803544436,4.17194282919486,
26.1788688094947));
#219170=CARTESIAN_POINT('Ctrl Pts',(-6.83269232072961,3.98872946052635,
26.188288692328));
#219171=CARTESIAN_POINT('Ctrl Pts',(-6.8866500855219,3.89482962872367,26.1930560808351));
#219172=CARTESIAN_POINT('Ctrl Pts',(-7.20699677688648,3.30986522013551,
26.2223230969753));
#219173=CARTESIAN_POINT('Ctrl Pts',(-7.42269418079283,2.79279882790139,
26.2461706717191));
#219174=CARTESIAN_POINT('Ctrl Pts',(-7.59215920201566,2.22357298943364,
26.2702337829383));
#219175=CARTESIAN_POINT('Ctrl Pts',(-7.60197058740697,2.18979483068414,
26.271654539089));
#219176=CARTESIAN_POINT('Ctrl Pts',(-7.61621293849822,2.13951242682499,
26.2737592458376));
#219177=CARTESIAN_POINT('Ctrl Pts',(-7.62081619405549,2.12305758004906,
26.2744463853379));
#219178=CARTESIAN_POINT('Ctrl Pts',(-7.6286135052345,2.0948330981062,26.2756222905566));
#219179=CARTESIAN_POINT('Ctrl Pts',(-7.63183371639946,2.08307077348754,
26.2761115307317));
#219180=CARTESIAN_POINT('Ctrl Pts',(-7.63839210264199,2.05889589331696,
26.2771154216151));
#219181=CARTESIAN_POINT('Ctrl Pts',(-7.64172725101118,2.04648255196108,
26.2776300167359));
#219182=CARTESIAN_POINT('Ctrl Pts',(-7.64827046578289,2.02188983603875,
26.2786477888843));
#219183=CARTESIAN_POINT('Ctrl Pts',(-7.65147972925777,2.00971082014847,
26.2791509856662));
#219184=CARTESIAN_POINT('Ctrl Pts',(-7.65881483943904,1.98160213714104,
26.2803104571856));
#219185=CARTESIAN_POINT('Ctrl Pts',(-7.66292009964485,1.96566714461528,
26.2809663736341));
#219186=CARTESIAN_POINT('Ctrl Pts',(-7.67339531350322,1.92447495656088,
26.2826584137667));
#219187=CARTESIAN_POINT('Ctrl Pts',(-7.67969031752528,1.89919881307823,
26.2836932852363));
#219188=CARTESIAN_POINT('Ctrl Pts',(-7.68648670856122,1.87132308026282,
26.2848309425881));
#219189=CARTESIAN_POINT('Ctrl Pts',(-7.68711174881307,1.86875385026542,
26.2849357631341));
#219190=CARTESIAN_POINT('Ctrl Pts',(-7.83651897519375,1.25327164182394,
26.3100382812323));
#219191=CARTESIAN_POINT('Ctrl Pts',(-7.91147323817745,0.624771831188963,
26.3334951089523));
#219192=CARTESIAN_POINT('Ctrl Pts',(-7.91099775207325,-0.00596378169342535,
26.3566855201154));
#219193=CARTESIAN_POINT('',(-7.91915402201384,0.00415711932536667,28.3576688734072));
#219194=CARTESIAN_POINT('Ctrl Pts',(-7.91099777923565,-0.00592764106740734,
26.3576684917633));
#219195=CARTESIAN_POINT('Ctrl Pts',(-7.91081234552831,-0.253406466168664,
26.367633558589));
#219196=CARTESIAN_POINT('Ctrl Pts',(-7.89901033771747,-0.500480502849058,
26.3775986254146));
#219197=CARTESIAN_POINT('Ctrl Pts',(-7.87572819848802,-0.74620797606343,
26.3875636922403));
#219198=CARTESIAN_POINT('Ctrl Pts',(-7.85216115441233,-0.994942430177823,
26.3976507021487));
#219199=CARTESIAN_POINT('Ctrl Pts',(-7.81683130210497,-1.24229732251291,
26.4077377120572));
#219200=CARTESIAN_POINT('Ctrl Pts',(-7.76993023616728,-1.48731473639357,
26.4178247219656));
#219201=CARTESIAN_POINT('Ctrl Pts',(-7.73756601590349,-1.65638973272377,
26.4247852932011));
#219202=CARTESIAN_POINT('Ctrl Pts',(-7.69969293076519,-1.82435207936941,
26.4317458644366));
#219203=CARTESIAN_POINT('Ctrl Pts',(-7.65638765302037,-1.99089153563854,
26.4387064356721));
#219204=CARTESIAN_POINT('Ctrl Pts',(-7.60718904108376,-2.18009503479169,
26.4466142580186));
#219205=CARTESIAN_POINT('Ctrl Pts',(-7.55090996100215,-2.36771584605453,
26.4545220803651));
#219206=CARTESIAN_POINT('Ctrl Pts',(-7.48766754116812,-2.55318542079053,
26.4624299027117));
#219207=CARTESIAN_POINT('Ctrl Pts',(-7.42448973161223,-2.73846551446555,
26.470329646199));
#219208=CARTESIAN_POINT('Ctrl Pts',(-7.35436286296112,-2.92159842557277,
26.4782293896864));
#219209=CARTESIAN_POINT('Ctrl Pts',(-7.2774547056937,-3.10202740261537,
26.4861291331738));
#219210=CARTESIAN_POINT('Ctrl Pts',(-7.20061083918178,-3.28230555150578,
26.4940222729342));
#219211=CARTESIAN_POINT('Ctrl Pts',(-7.11699711146742,-3.45988395371757,
26.5019154126945));
#219212=CARTESIAN_POINT('Ctrl Pts',(-7.02683065685917,-3.63422232669165,
26.5098085524549));
#219213=CARTESIAN_POINT('Ctrl Pts',(-6.93672283807322,-3.80844732630642,
26.5176965592559));
#219214=CARTESIAN_POINT('Ctrl Pts',(-6.8400709403987,-3.97943618940445,
26.525584566057));
#219215=CARTESIAN_POINT('Ctrl Pts',(-6.73713974615048,-4.14666963246887,
26.5334725728581));
#219216=CARTESIAN_POINT('Ctrl Pts',(-6.63425638483063,-4.31382536084861,
26.5413569140409));
#219217=CARTESIAN_POINT('Ctrl Pts',(-6.52509972210309,-4.4772288536476,
26.5492412552237));
#219218=CARTESIAN_POINT('Ctrl Pts',(-6.40998005051429,-4.63638617373584,
26.5571255964065));
#219219=CARTESIAN_POINT('Ctrl Pts',(-6.29489251299128,-4.79549906725715,
26.5650077367844));
#219220=CARTESIAN_POINT('Ctrl Pts',(-6.17384548610093,-4.95036787126117,
26.5728898771623));
#219221=CARTESIAN_POINT('Ctrl Pts',(-6.04719223232534,-5.10052812023462,
26.5807720175402));
#219222=CARTESIAN_POINT('Ctrl Pts',(-5.92052512983102,-5.25070478826553,
26.5886550197795));
#219223=CARTESIAN_POINT('Ctrl Pts',(-5.78825079265693,-5.39617160433021,
26.5965380220188));
#219224=CARTESIAN_POINT('Ctrl Pts',(-5.65076277685022,-5.53649718141028,
26.604421024258));
#219225=CARTESIAN_POINT('Ctrl Pts',(-5.51325817951605,-5.67683968223746,
26.6123049772145));
#219226=CARTESIAN_POINT('Ctrl Pts',(-5.3705388916713,-5.81203946154334,
26.6201889301709));
#219227=CARTESIAN_POINT('Ctrl Pts',(-5.22303531337968,-5.94170203857353,
26.6280728831274));
#219228=CARTESIAN_POINT('Ctrl Pts',(-5.07548913974285,-6.07140205891387,
26.6359591127723));
#219229=CARTESIAN_POINT('Ctrl Pts',(-4.92315618161962,-6.1955614627831,
26.6438453424172));
#219230=CARTESIAN_POINT('Ctrl Pts',(-4.76650006527091,-6.31382595006961,
26.6517315720621));
#219231=CARTESIAN_POINT('Ctrl Pts',(-4.6097723648779,-6.43214447833769,
26.6596214053213));
#219232=CARTESIAN_POINT('Ctrl Pts',(-4.44871784480252,-6.54456251467399,
26.6675112385805));
#219233=CARTESIAN_POINT('Ctrl Pts',(-4.2838294423279,-6.65076885097089,
26.6754010718397));
#219234=CARTESIAN_POINT('Ctrl Pts',(-4.11875088072907,-6.75709767073899,
26.6833000041244));
#219235=CARTESIAN_POINT('Ctrl Pts',(-3.94982989526002,-6.85720029469113,
26.6911989364091));
#219236=CARTESIAN_POINT('Ctrl Pts',(-3.77758538490002,-6.950810719606,26.6990978686937));
#219237=CARTESIAN_POINT('Ctrl Pts',(-3.60522710960576,-7.04448297281262,
26.7070020181056));
#219238=CARTESIAN_POINT('Ctrl Pts',(-3.42954124134811,-7.13165432588132,
26.7149061675174));
#219239=CARTESIAN_POINT('Ctrl Pts',(-3.25106724206579,-7.21210668165459,
26.7228103169293));
#219240=CARTESIAN_POINT('Ctrl Pts',(-3.07234865061488,-7.29266929447507,
26.7307252986924));
#219241=CARTESIAN_POINT('Ctrl Pts',(-2.8908346144224,-7.36649438832649,
26.7386402804554));
#219242=CARTESIAN_POINT('Ctrl Pts',(-2.7070814610296,-7.43341314359358,
26.7465552622185));
#219243=CARTESIAN_POINT('Ctrl Pts',(-2.62923165918707,-7.46176428609592,
26.7499085639196));
#219244=CARTESIAN_POINT('Ctrl Pts',(-2.55098010369695,-7.48887641831373,
26.7532618656206));
#219245=CARTESIAN_POINT('Ctrl Pts',(-2.47236966538338,-7.51473946572282,
26.7566151673216));
#219246=CARTESIAN_POINT('Ctrl Pts',(-2.29044769764609,-7.57459228650951,
26.7643754502682));
#219247=CARTESIAN_POINT('Ctrl Pts',(-2.10603030035296,-7.62794040411383,
26.7721357332148));
#219248=CARTESIAN_POINT('Ctrl Pts',(-1.91963366571878,-7.67456367420579,
26.7798960161614));
#219249=CARTESIAN_POINT('Ctrl Pts',(-1.73346136875843,-7.72113083085998,
26.7876469592193));
#219250=CARTESIAN_POINT('Ctrl Pts',(-1.54531491949835,-7.76098916388463,
26.7953979022772));
#219251=CARTESIAN_POINT('Ctrl Pts',(-1.35572989318385,-7.79396673438678,
26.8031488453351));
#219252=CARTESIAN_POINT('Ctrl Pts',(-1.16633456185022,-7.82691130819226,
26.8108920329545));
#219253=CARTESIAN_POINT('Ctrl Pts',(-0.975503869297573,-7.85298876381602,
26.818635220574));
#219254=CARTESIAN_POINT('Ctrl Pts',(-0.783788036871119,-7.87207706474331,
26.8263784081935));
#219255=CARTESIAN_POINT('Ctrl Pts',(-0.592225175822845,-7.89115013498432,
26.8341154174704));
#219256=CARTESIAN_POINT('Ctrl Pts',(-0.399778936164906,-7.90324511807012,
26.8418524267473));
#219257=CARTESIAN_POINT('Ctrl Pts',(-0.207009301238635,-7.90829110169831,
26.8495894360243));
#219258=CARTESIAN_POINT('Ctrl Pts',(-0.0143544498463088,-7.91333408072552,
26.857321838345));
#219259=CARTESIAN_POINT('Ctrl Pts',(0.178623055672807,-7.91133640881237,
26.8650542406657));
#219260=CARTESIAN_POINT('Ctrl Pts',(0.371358452897015,-7.9022790319921,
26.8727866429865));
#219261=CARTESIAN_POINT('Ctrl Pts',(0.564018081156201,-7.8932252158466,
26.8805160055121));
#219262=CARTESIAN_POINT('Ctrl Pts',(0.756435432608975,-7.87711723920013,
26.8882453680377));
#219263=CARTESIAN_POINT('Ctrl Pts',(0.948045998137956,-7.85398814523008,
26.8959747305633));
#219264=CARTESIAN_POINT('Ctrl Pts',(1.139656488908,-7.83085906028409,26.9037040900732));
#219265=CARTESIAN_POINT('Ctrl Pts',(1.33045983660178,-7.80070889512595,
26.9114334495831));
#219266=CARTESIAN_POINT('Ctrl Pts',(1.51989649849299,-7.76362258445558,
26.919162809093));
#219267=CARTESIAN_POINT('Ctrl Pts',(1.70934265562977,-7.72653441488618,
26.9268925560261));
#219268=CARTESIAN_POINT('Ctrl Pts',(1.89742163769622,-7.6825094755353,26.9346223029593));
#219269=CARTESIAN_POINT('Ctrl Pts',(2.08358411429359,-7.63168384032406,
26.9423520498924));
#219270=CARTESIAN_POINT('Ctrl Pts',(2.26979003381491,-7.58084634442937,
26.9500836006413));
#219271=CARTESIAN_POINT('Ctrl Pts',(2.45407821066096,-7.52320508683273,
26.9578151513902));
#219272=CARTESIAN_POINT('Ctrl Pts',(2.63591444857681,-7.45894603947394,
26.9655467021391));
#219273=CARTESIAN_POINT('Ctrl Pts',(2.81782644965242,-7.39466021819744,
26.9732814742851));
#219274=CARTESIAN_POINT('Ctrl Pts',(2.99728413916984,-7.32375123608585,
26.981016246431));
#219275=CARTESIAN_POINT('Ctrl Pts',(3.17377322716514,-7.24645323606865,
26.9887510185769));
#219276=CARTESIAN_POINT('Ctrl Pts',(3.35047277848795,-7.16906305814698,
26.9964950144426));
#219277=CARTESIAN_POINT('Ctrl Pts',(3.52419632934816,-7.08526879055788,
27.0042390103082));
#219278=CARTESIAN_POINT('Ctrl Pts',(3.69445320748985,-6.9953510632182,27.0119830061739));
#219279=CARTESIAN_POINT('Ctrl Pts',(3.86482059088637,-6.90537497476276,
27.0197320282813));
#219280=CARTESIAN_POINT('Ctrl Pts',(4.03171650970528,-6.80926768825034,
27.0274810503888));
#219281=CARTESIAN_POINT('Ctrl Pts',(4.19467935553526,-6.70735313698677,
27.0352300724962));
#219282=CARTESIAN_POINT('Ctrl Pts',(4.35789124698183,-6.60528283628148,
27.0429909369348));
#219283=CARTESIAN_POINT('Ctrl Pts',(4.51715776493355,-6.49738774639976,
27.0507518013734));
#219284=CARTESIAN_POINT('Ctrl Pts',(4.6720495024886,-6.38403277296538,27.0585126658121));
#219285=CARTESIAN_POINT('Ctrl Pts',(4.7785671781947,-6.30607956196428,27.0638497435318));
#219286=CARTESIAN_POINT('Ctrl Pts',(4.88301665375285,-6.22554509245537,
27.0691868212515));
#219287=CARTESIAN_POINT('Ctrl Pts',(4.98526863013735,-6.14255791062392,
27.0745238989712));
#219288=CARTESIAN_POINT('Ctrl Pts',(5.13880338537601,-6.01794988737626,
27.0825376992942));
#219289=CARTESIAN_POINT('Ctrl Pts',(5.28785309562113,-5.88742820012953,
27.0905514996173));
#219290=CARTESIAN_POINT('Ctrl Pts',(5.43194002709184,-5.7513431946005,27.0985652999404));
#219291=CARTESIAN_POINT('Ctrl Pts',(5.5758627164689,-5.6154133099141,27.106569965477));
#219292=CARTESIAN_POINT('Ctrl Pts',(5.71483365802107,-5.47393297085151,
27.1145746310137));
#219293=CARTESIAN_POINT('Ctrl Pts',(5.84840691621087,-5.3272936414672,27.1225792965504));
#219294=CARTESIAN_POINT('Ctrl Pts',(5.98185059292036,-5.18079656916062,
27.1305761966374));
#219295=CARTESIAN_POINT('Ctrl Pts',(6.1099067975314,-5.02915072602463,27.1385730967244));
#219296=CARTESIAN_POINT('Ctrl Pts',(6.23216501251044,-4.87278567729392,
27.1465699968114));
#219297=CARTESIAN_POINT('Ctrl Pts',(6.35432536491272,-4.71654579223084,
27.1545604957151));
#219298=CARTESIAN_POINT('Ctrl Pts',(6.47069677235522,-4.55559449279696,
27.1625509946188));
#219299=CARTESIAN_POINT('Ctrl Pts',(6.58090746171654,-4.3903961074513,27.1705414935225));
#219300=CARTESIAN_POINT('Ctrl Pts',(6.69104862015278,-4.22530194426977,
27.1785269512928));
#219301=CARTESIAN_POINT('Ctrl Pts',(6.79503662284419,-4.0559663136662,27.1865124090632));
#219302=CARTESIAN_POINT('Ctrl Pts',(6.89254144589137,-3.88288467723028,
27.1944978668335));
#219303=CARTESIAN_POINT('Ctrl Pts',(6.9932432187942,-3.70412810805434,27.202745148658));
#219304=CARTESIAN_POINT('Ctrl Pts',(7.08702923843833,-3.52137600817342,
27.2109924304824));
#219305=CARTESIAN_POINT('Ctrl Pts',(7.17358526280352,-3.33520546252973,
27.2192397123069));
#219306=CARTESIAN_POINT('Ctrl Pts',(7.25733666092416,-3.15506729651651,
27.2272197620904));
#219307=CARTESIAN_POINT('Ctrl Pts',(7.33431911353444,-2.97172907265719,
27.2351998118739));
#219308=CARTESIAN_POINT('Ctrl Pts',(7.40429523026887,-2.78573745048194,
27.2431798616573));
#219309=CARTESIAN_POINT('Ctrl Pts',(7.47426579002794,-2.5997605983584,27.2511592777254));
#219310=CARTESIAN_POINT('Ctrl Pts',(7.53723100496438,-2.41113108097571,
27.2591386937935));
#219311=CARTESIAN_POINT('Ctrl Pts',(7.59300213145897,-2.22041429279753,
27.2671181098617));
#219312=CARTESIAN_POINT('Ctrl Pts',(7.64877740018541,-2.02968333970634,
27.2750981185768));
#219313=CARTESIAN_POINT('Ctrl Pts',(7.6973574218759,-1.83686512805803,27.2830781272919));
#219314=CARTESIAN_POINT('Ctrl Pts',(7.73860360030138,-1.64253928945476,
27.291058136007));
#219315=CARTESIAN_POINT('Ctrl Pts',(7.77985918114683,-1.44816915261064,
27.2990399638336));
#219316=CARTESIAN_POINT('Ctrl Pts',(7.81377751748777,-1.25229103108626,
27.3070217916601));
#219317=CARTESIAN_POINT('Ctrl Pts',(7.84027123541226,-1.05549417580919,
27.3150036194866));
#219318=CARTESIAN_POINT('Ctrl Pts',(7.86678465260723,-0.858550993221867,
27.322991382161));
#219319=CARTESIAN_POINT('Ctrl Pts',(7.88586237907792,-0.660688044086383,
27.3309791448354));
#219320=CARTESIAN_POINT('Ctrl Pts',(7.89746887389976,-0.46250014679399,
27.3389669075098));
#219321=CARTESIAN_POINT('Ctrl Pts',(7.90908048063459,-0.264224960504955,
27.3469581882789));
#219322=CARTESIAN_POINT('Ctrl Pts',(7.91321428347661,-0.0656248747359486,
27.3549494690479));
#219323=CARTESIAN_POINT('Ctrl Pts',(7.90988687085329,0.13270527609249,27.362940749817));
#219324=CARTESIAN_POINT('Ctrl Pts',(7.90655632757708,0.331222029224147,
27.3709395493188));
#219325=CARTESIAN_POINT('Ctrl Pts',(7.89575056311862,0.529468006427327,
27.3789383488207));
#219326=CARTESIAN_POINT('Ctrl Pts',(7.87753809705243,0.726852481241957,
27.3869371483225));
#219327=CARTESIAN_POINT('Ctrl Pts',(7.87336720928981,0.772056051562621,
27.3887689757552));
#219328=CARTESIAN_POINT('Ctrl Pts',(7.86880807626953,0.817214474545574,
27.390600803188));
#219329=CARTESIAN_POINT('Ctrl Pts',(7.86386189895736,0.86232072578982,27.3924326306207));
#219330=CARTESIAN_POINT('Ctrl Pts',(7.84191885665016,1.06242846898338,27.4005592836538));
#219331=CARTESIAN_POINT('Ctrl Pts',(7.81231554044796,1.26186151973571,27.4086859366868));
#219332=CARTESIAN_POINT('Ctrl Pts',(7.77510704393797,1.46001077232541,27.4168125897199));
#219333=CARTESIAN_POINT('Ctrl Pts',(7.73793022096867,1.65799135138606,27.4249323249815));
#219334=CARTESIAN_POINT('Ctrl Pts',(7.69316118279052,1.85468999905893,27.4330520602431));
#219335=CARTESIAN_POINT('Ctrl Pts',(7.64090667989423,2.04950386902485,27.4411717955047));
#219336=CARTESIAN_POINT('Ctrl Pts',(7.58869007803003,2.24417643735494,27.4492856413916));
#219337=CARTESIAN_POINT('Ctrl Pts',(7.52899891914404,2.43696664675881,27.4573994872786));
#219338=CARTESIAN_POINT('Ctrl Pts',(7.46199089884747,2.62728240307689,27.4655133331655));
#219339=CARTESIAN_POINT('Ctrl Pts',(7.39503049024378,2.81746293296538,27.4736214138628));
#219340=CARTESIAN_POINT('Ctrl Pts',(7.32076369783073,3.00517221739098,27.4817294945602));
#219341=CARTESIAN_POINT('Ctrl Pts',(7.23939798117092,3.18983351763356,27.4898375752576));
#219342=CARTESIAN_POINT('Ctrl Pts',(7.15806721149645,3.37441550491707,27.4979421734934));
#219343=CARTESIAN_POINT('Ctrl Pts',(7.06964372535775,3.5559518270448,27.5060467717293));
#219344=CARTESIAN_POINT('Ctrl Pts',(6.97438333418001,3.73388512248464,27.5141513699651));
#219345=CARTESIAN_POINT('Ctrl Pts',(6.87915271862058,3.91176280116894,27.52225343494));
#219346=CARTESIAN_POINT('Ctrl Pts',(6.77708961036011,4.08603941845193,27.530355499915));
#219347=CARTESIAN_POINT('Ctrl Pts',(6.66849630597499,4.25618115418011,27.5384575648899));
#219348=CARTESIAN_POINT('Ctrl Pts',(6.61073120943118,4.34668630867486,27.5427673754085));
#219349=CARTESIAN_POINT('Ctrl Pts',(6.55111910721999,4.43602187306296,27.547077185927));
#219350=CARTESIAN_POINT('Ctrl Pts',(6.48971066688954,4.52411057115761,27.5513869964456));
#219351=CARTESIAN_POINT('Ctrl Pts',(6.37160875429003,4.69352447692362,27.559675708265));
#219352=CARTESIAN_POINT('Ctrl Pts',(6.2469109124311,4.85825186655254,27.5679644200845));
#219353=CARTESIAN_POINT('Ctrl Pts',(6.11601819192606,5.01779258997714,27.5762531319039));
#219354=CARTESIAN_POINT('Ctrl Pts',(5.98505001304714,5.17742528706926,27.5845466220847));
#219355=CARTESIAN_POINT('Ctrl Pts',(5.84788001260705,5.33186512346555,27.5928401122655));
#219356=CARTESIAN_POINT('Ctrl Pts',(5.7049483526403,5.48064643027688,27.6011336024463));
#219357=CARTESIAN_POINT('Ctrl Pts',(5.56192567655974,5.62952247814388,27.609432373761));
#219358=CARTESIAN_POINT('Ctrl Pts',(5.41313421994016,5.77273259311984,27.6177311450758));
#219359=CARTESIAN_POINT('Ctrl Pts',(5.25905028154673,5.90984865594401,27.6260299163906));
#219360=CARTESIAN_POINT('Ctrl Pts',(5.10478698055674,6.04712432977836,27.6343383479541));
#219361=CARTESIAN_POINT('Ctrl Pts',(4.9452191019751,6.17829157707465,27.6426467795176));
#219362=CARTESIAN_POINT('Ctrl Pts',(4.78085658491677,6.30296210637966,27.6509552110811));
#219363=CARTESIAN_POINT('Ctrl Pts',(4.61639267790957,6.42770954092328,27.6592687678487));
#219364=CARTESIAN_POINT('Ctrl Pts',(4.44712846544184,6.54595208638212,27.6675823246164));
#219365=CARTESIAN_POINT('Ctrl Pts',(4.27360319432333,6.65734457103351,27.675895881384));
#219366=CARTESIAN_POINT('Ctrl Pts',(4.09988820943162,6.768858840186,27.6842185272959));
#219367=CARTESIAN_POINT('Ctrl Pts',(3.92190310444567,6.87350792750676,27.6925411732078));
#219368=CARTESIAN_POINT('Ctrl Pts',(3.74021347826065,6.97099161791473,27.7008638191197));
#219369=CARTESIAN_POINT('Ctrl Pts',(3.67124617746068,7.00799531009367,27.7040230001699));
#219370=CARTESIAN_POINT('Ctrl Pts',(3.60174533351802,7.04396704201864,27.7071821812201));
#219371=CARTESIAN_POINT('Ctrl Pts',(3.53174268526238,7.0788921877011,27.7103413622702));
#219372=CARTESIAN_POINT('Ctrl Pts',(3.3390033883788,7.17505209293512,27.7190395808307));
#219373=CARTESIAN_POINT('Ctrl Pts',(3.14228745469956,7.26336011798245,27.7277377993912));
#219374=CARTESIAN_POINT('Ctrl Pts',(2.9422257820067,7.34351608207506,27.7364360179517));
#219375=CARTESIAN_POINT('Ctrl Pts',(2.74233989031145,7.42360161840836,27.7451265939612));
#219376=CARTESIAN_POINT('Ctrl Pts',(2.5391143416163,7.4955493109218,27.7538171699706));
#219377=CARTESIAN_POINT('Ctrl Pts',(2.33320040946053,7.55910688172176,27.7625077459801));
#219378=CARTESIAN_POINT('Ctrl Pts',(2.12234812839698,7.62418872752853,27.7714067444897));
#219379=CARTESIAN_POINT('Ctrl Pts',(1.90867711533581,7.6804728782617,27.7803057429993));
#219380=CARTESIAN_POINT('Ctrl Pts',(1.6929071988585,7.72774133987759,27.7892047415089));
#219381=CARTESIAN_POINT('Ctrl Pts',(1.48281167866957,7.77376671817802,27.7978697108964));
#219382=CARTESIAN_POINT('Ctrl Pts',(1.27072649096759,7.81124450237042,27.806534680284));
#219383=CARTESIAN_POINT('Ctrl Pts',(1.05733189541374,7.8400236136724,27.8151996496715));
#219384=CARTESIAN_POINT('Ctrl Pts',(0.835292050071472,7.86996865237403,
27.8242156627421));
#219385=CARTESIAN_POINT('Ctrl Pts',(0.611834712781352,7.8904954553862,27.8332316758127));
#219386=CARTESIAN_POINT('Ctrl Pts',(0.387740269425987,7.90149216815821,
27.8422476888833));
#219387=CARTESIAN_POINT('Ctrl Pts',(0.163645826070641,7.91248888093021,
27.8512637019539));
#219388=CARTESIAN_POINT('Ctrl Pts',(-0.0610854473386478,7.91395542263523,
27.8602797150245));
#219389=CARTESIAN_POINT('Ctrl Pts',(-0.285662862010668,7.90584073513171,
27.8692957280951));
#219390=CARTESIAN_POINT('Ctrl Pts',(-0.480211015268739,7.8988110991802,
27.8771061692972));
#219391=CARTESIAN_POINT('Ctrl Pts',(-0.674559784868564,7.88459373706153,
27.8849166104994));
#219392=CARTESIAN_POINT('Ctrl Pts',(-0.868135493372626,7.86322209816985,
27.8927270517016));
#219393=CARTESIAN_POINT('Ctrl Pts',(-1.06169724545758,7.84185200013034,
27.9005369297867));
#219394=CARTESIAN_POINT('Ctrl Pts',(-1.25448569742344,7.81332869140897,
27.9083468078717));
#219395=CARTESIAN_POINT('Ctrl Pts',(-1.44593247985462,7.77773747716529,
27.9161566859568));
#219396=CARTESIAN_POINT('Ctrl Pts',(-1.63739925074674,7.74214254693544,
27.923967379451));
#219397=CARTESIAN_POINT('Ctrl Pts',(-1.82752372698342,7.69947830650449,
27.9317780729451));
#219398=CARTESIAN_POINT('Ctrl Pts',(-2.01574776697818,7.64988117162106,
27.9395887664393));
#219399=CARTESIAN_POINT('Ctrl Pts',(-2.20410538122401,7.60024883985127,
27.9474050028361));
#219400=CARTESIAN_POINT('Ctrl Pts',(-2.39055952383616,7.54367387406576,
27.9552212392329));
#219401=CARTESIAN_POINT('Ctrl Pts',(-2.57456640881466,7.48034282680969,
27.9630374756298));
#219402=CARTESIAN_POINT('Ctrl Pts',(-2.75864132380225,7.41698836514866,
27.9708566018023));
#219403=CARTESIAN_POINT('Ctrl Pts',(-2.94026684866335,7.34687296844819,
27.9786757279749));
#219404=CARTESIAN_POINT('Ctrl Pts',(-3.11891909844799,7.27023140328672,
27.9864948541474));
#219405=CARTESIAN_POINT('Ctrl Pts',(-3.29777000429548,7.19350461495227,
27.994322674959));
#219406=CARTESIAN_POINT('Ctrl Pts',(-3.47364071051776,7.11023730843021,
28.0021504957706));
#219407=CARTESIAN_POINT('Ctrl Pts',(-3.64603087473383,7.02071078029053,
28.0099783165822));
#219408=CARTESIAN_POINT('Ctrl Pts',(-3.7801624877571,6.95105287560464,28.016068909028));
#219409=CARTESIAN_POINT('Ctrl Pts',(-3.91218747058962,6.87760662874013,
28.0221595014739));
#219410=CARTESIAN_POINT('Ctrl Pts',(-4.04188246519154,6.80052256356651,
28.0282500939197));
#219411=CARTESIAN_POINT('Ctrl Pts',(-4.21472797360549,6.69779204203449,
28.0363670729217));
#219412=CARTESIAN_POINT('Ctrl Pts',(-4.38377786317178,6.58839489746363,
28.0444840519237));
#219413=CARTESIAN_POINT('Ctrl Pts',(-4.54850427346319,6.47263701085478,
28.0526010309257));
#219414=CARTESIAN_POINT('Ctrl Pts',(-4.71311019210323,6.35696379712196,
28.0607120726393));
#219415=CARTESIAN_POINT('Ctrl Pts',(-4.87339867558365,6.23493930186843,
28.0688231143529));
#219416=CARTESIAN_POINT('Ctrl Pts',(-5.02886943702191,6.10691355640367,
28.0769341560665));
#219417=CARTESIAN_POINT('Ctrl Pts',(-5.18424858218529,5.97896325433277,
28.0850404180811));
#219418=CARTESIAN_POINT('Ctrl Pts',(-5.33481541949327,5.84501895723589,
28.0931466800958));
#219419=CARTESIAN_POINT('Ctrl Pts',(-5.48010099593342,5.70547229196405,
28.1012529421105));
#219420=CARTESIAN_POINT('Ctrl Pts',(-5.62532159301977,5.565988039303,28.1093555785783));
#219421=CARTESIAN_POINT('Ctrl Pts',(-5.76526540890448,5.42090663721578,
28.1174582150462));
#219422=CARTESIAN_POINT('Ctrl Pts',(-5.89949834397028,5.27065843035687,
28.125560851514));
#219423=CARTESIAN_POINT('Ctrl Pts',(-6.03369029242549,5.12045610020283,
28.1336610139272));
#219424=CARTESIAN_POINT('Ctrl Pts',(-6.16217462460431,4.96509035080169,
28.1417611763405));
#219425=CARTESIAN_POINT('Ctrl Pts',(-6.28455534534605,4.8050270666545,28.1498613387537));
#219426=CARTESIAN_POINT('Ctrl Pts',(-6.40812811406901,4.64340468795731,
28.1580404007044));
#219427=CARTESIAN_POINT('Ctrl Pts',(-6.52547751237483,4.47699302135058,
28.166219462655));
#219428=CARTESIAN_POINT('Ctrl Pts',(-6.63623817174748,4.30630513640658,
28.1743985246057));
#219429=CARTESIAN_POINT('Ctrl Pts',(-6.74592977371789,4.13726472402103,
28.1824986425814));
#219430=CARTESIAN_POINT('Ctrl Pts',(-6.8491591054058,3.96403056200219,28.190598760557));
#219431=CARTESIAN_POINT('Ctrl Pts',(-6.94561521639302,3.78712955492808,
28.1986988785327));
#219432=CARTESIAN_POINT('Ctrl Pts',(-7.04208430867657,3.61020474008927,
28.2068000866418));
#219433=CARTESIAN_POINT('Ctrl Pts',(-7.13177820871898,3.42961237766244,
28.2149012947509));
#219434=CARTESIAN_POINT('Ctrl Pts',(-7.21443201372118,3.24590383705294,
28.22300250286));
#219435=CARTESIAN_POINT('Ctrl Pts',(-7.29710761715152,3.06214684667854,
28.2311058475145));
#219436=CARTESIAN_POINT('Ctrl Pts',(-7.37273929120307,2.87527233165193,
28.239209192169));
#219437=CARTESIAN_POINT('Ctrl Pts',(-7.44111013701217,2.68585199310289,
28.2473125368234));
#219438=CARTESIAN_POINT('Ctrl Pts',(-7.51061029049638,2.49330292564002,
28.2555497275523));
#219439=CARTESIAN_POINT('Ctrl Pts',(-7.57260753909675,2.29812352187236,
28.2637869182811));
#219440=CARTESIAN_POINT('Ctrl Pts',(-7.62692677239108,2.100930510175,28.2720241090099));
#219441=CARTESIAN_POINT('Ctrl Pts',(-7.68043295853602,1.90668907209746,
28.2801380059432));
#219442=CARTESIAN_POINT('Ctrl Pts',(-7.72648932949952,1.71049420536543,
28.2882519028766));
#219443=CARTESIAN_POINT('Ctrl Pts',(-7.76498004321694,1.51294610890233,
28.2963657998099));
#219444=CARTESIAN_POINT('Ctrl Pts',(-7.80434807881021,1.31089528308394,
28.3046646374365));
#219445=CARTESIAN_POINT('Ctrl Pts',(-7.83580140239664,1.10742915874967,
28.312963475063));
#219446=CARTESIAN_POINT('Ctrl Pts',(-7.85927207572049,0.903196235488287,
28.3212623126896));
#219447=CARTESIAN_POINT('Ctrl Pts',(-7.88274274904433,0.698963312226884,
28.3295611503162));
#219448=CARTESIAN_POINT('Ctrl Pts',(-7.898230780354,0.493963947803846,28.3378599879427));
#219449=CARTESIAN_POINT('Ctrl Pts',(-7.90572501483226,0.288847693180128,
28.3461588255693));
#219450=CARTESIAN_POINT('Ctrl Pts',(-7.9091896019269,0.194022380370513,
28.3499953809673));
#219451=CARTESIAN_POINT('Ctrl Pts',(-7.91094894867227,0.0991112522795639,
28.3538319363653));
#219452=CARTESIAN_POINT('Ctrl Pts',(-7.9109989050297,0.00416228529412779,
28.3576684917633));
#219453=CARTESIAN_POINT('',(-7.90357832657621,0.00116160200912298,30.3576684917633));
#219454=CARTESIAN_POINT('Ctrl Pts',(-7.92069697714534,0.00415614191964403,
28.3576689456146));
#219455=CARTESIAN_POINT('Ctrl Pts',(-7.91973006024624,-1.21367684137233,
28.4068170275411));
#219456=CARTESIAN_POINT('Ctrl Pts',(-7.29458056008006,-3.75569163334529,
28.5089498980758));
#219457=CARTESIAN_POINT('Ctrl Pts',(-3.85135548505637,-7.82348539955324,
28.717052345827));
#219458=CARTESIAN_POINT('Ctrl Pts',(3.55328581504252,-8.66439214142531,
28.9819762888683));
#219459=CARTESIAN_POINT('Ctrl Pts',(9.20702352837811,-1.6725696989809,29.2998850205178));
#219460=CARTESIAN_POINT('Ctrl Pts',(6.86085464277753,5.38250085615541,29.5648089635592));
#219461=CARTESIAN_POINT('Ctrl Pts',(2.06639954247995,7.97215553854543,29.776748117992));
#219462=CARTESIAN_POINT('Ctrl Pts',(-2.00486737260903,8.00605902378823,
29.9357024838169));
#219463=CARTESIAN_POINT('Ctrl Pts',(-5.57344547750851,6.06317035785365,
30.0946568496417));
#219464=CARTESIAN_POINT('Ctrl Pts',(-7.57769228948297,3.04117976839579,
30.2353121856238));
#219465=CARTESIAN_POINT('Ctrl Pts',(-7.90592795537224,0.863866818058979,
30.3229827329977));
#219466=CARTESIAN_POINT('Ctrl Pts',(-7.89949422726844,0.0018008241519719,
30.3576684917633));
#219467=CARTESIAN_POINT('',(-7.911,-6.8273164899324E-12,32.3576684917633));
#219468=CARTESIAN_POINT('Ctrl Pts',(-7.911,-6.88560319872522E-12,30.3576684917633));
#219469=CARTESIAN_POINT('Ctrl Pts',(-7.91099999999808,-2.20167589667365,
30.446255927496));
#219470=CARTESIAN_POINT('Ctrl Pts',(-6.9421457667199,-4.38610418339286,
30.5348433632287));
#219471=CARTESIAN_POINT('Ctrl Pts',(-3.6782020148765,-7.34180684107951,
30.7120182346942));
#219472=CARTESIAN_POINT('Ctrl Pts',(-1.40868175871044,-8.08992666571458,
30.8006056704269));
#219473=CARTESIAN_POINT('Ctrl Pts',(2.97309270521935,-7.65454228025,30.9777805418924));
#219474=CARTESIAN_POINT('Ctrl Pts',(5.05102072676161,-6.4744488083379,31.0663679776251));
#219475=CARTESIAN_POINT('Ctrl Pts',(7.66951518848124,-2.93425195367047,
31.2435428490906));
#219476=CARTESIAN_POINT('Ctrl Pts',(8.18956872247123,-0.601881960092137,
31.3321302848233));
#219477=CARTESIAN_POINT('Ctrl Pts',(7.32306689761024,3.71537198233077,31.5093051562887));
#219478=CARTESIAN_POINT('Ctrl Pts',(5.94329958849717,5.66643518937019,31.5978925920215));
#219479=CARTESIAN_POINT('Ctrl Pts',(2.16154501637172,7.92205913233182,31.7750674634869));
#219480=CARTESIAN_POINT('Ctrl Pts',(-0.210816529307356,8.20894963712984,
31.8636548992196));
#219481=CARTESIAN_POINT('Ctrl Pts',(-4.42123908577025,6.91982244717456,
32.0408297706851));
#219482=CARTESIAN_POINT('Ctrl Pts',(-6.22631625634641,5.35390358802993,
32.1294172064178));
#219483=CARTESIAN_POINT('Ctrl Pts',(-7.65317280859686,2.31334857513867,
32.2645592586881));
#219484=CARTESIAN_POINT('Ctrl Pts',(-7.911000000001,1.15702837835841,32.3111138752257));
#219485=CARTESIAN_POINT('Ctrl Pts',(-7.911,-6.8273164899324E-12,32.3576684917633));
#219486=CARTESIAN_POINT('',(-7.91204594914714,-0.00281928559808421,34.3576684917633));
#219487=CARTESIAN_POINT('Ctrl Pts',(-7.91099999939128,-9.81387723526022E-5,
32.3576684917633));
#219488=CARTESIAN_POINT('Ctrl Pts',(-7.91099751585164,-0.200297118282624,
32.3656923392676));
#219489=CARTESIAN_POINT('Ctrl Pts',(-7.90339122720327,-0.40042256281032,
32.373716186772));
#219490=CARTESIAN_POINT('Ctrl Pts',(-7.88822379333303,-0.599871974920195,
32.3817400342763));
#219491=CARTESIAN_POINT('Ctrl Pts',(-7.87290732035448,-0.801281228278693,
32.389842726171));
#219492=CARTESIAN_POINT('Ctrl Pts',(-7.84988034736886,-1.00200075216182,
32.3979454180657));
#219493=CARTESIAN_POINT('Ctrl Pts',(-7.81924013616528,-1.20141778452877,
32.4060481099605));
#219494=CARTESIAN_POINT('Ctrl Pts',(-7.78884737466464,-1.39922432912552,
32.4140853646854));
#219495=CARTESIAN_POINT('Ctrl Pts',(-7.75096400576114,-1.59574903115637,
32.4221226194104));
#219496=CARTESIAN_POINT('Ctrl Pts',(-7.70573595741653,-1.79040619820696,
32.4301598741354));
#219497=CARTESIAN_POINT('Ctrl Pts',(-7.65995555713476,-1.9874406348334,
32.438295284615));
#219498=CARTESIAN_POINT('Ctrl Pts',(-7.60665000850472,-2.18256128921893,
32.4464306950946));
#219499=CARTESIAN_POINT('Ctrl Pts',(-7.54602201322522,-2.37517847243538,
32.4545661055742));
#219500=CARTESIAN_POINT('Ctrl Pts',(-7.48539401794571,-2.56779565565183,
32.4627015160538));
#219501=CARTESIAN_POINT('Ctrl Pts',(-7.41744373511158,-2.75790905979931,
32.4708369265334));
#219502=CARTESIAN_POINT('Ctrl Pts',(-7.34242339731225,-2.94495155386327,
32.4789723370131));
#219503=CARTESIAN_POINT('Ctrl Pts',(-7.26757302459109,-3.13157028694375,
32.487089316015));
#219504=CARTESIAN_POINT('Ctrl Pts',(-7.18555049878641,-3.31546674058872,
32.495206295017));
#219505=CARTESIAN_POINT('Ctrl Pts',(-7.09657665040477,-3.49607220247663,
32.503323274019));
#219506=CARTESIAN_POINT('Ctrl Pts',(-7.00766788330481,-3.67654555773826,
32.5114343157326));
#219507=CARTESIAN_POINT('Ctrl Pts',(-6.91181807296472,-3.85373243432938,
32.5195453574462));
#219508=CARTESIAN_POINT('Ctrl Pts',(-6.80929592384273,-4.02708455604533,
32.5276563991598));
#219509=CARTESIAN_POINT('Ctrl Pts',(-6.70683418927916,-4.20033452430493,
32.5357626611745));
#219510=CARTESIAN_POINT('Ctrl Pts',(-6.59770811918204,-4.36975396842767,
32.5438689231892));
#219511=CARTESIAN_POINT('Ctrl Pts',(-6.48223234756314,-4.53481915760773,
32.5519751852039));
#219512=CARTESIAN_POINT('Ctrl Pts',(-6.36680822278493,-4.69981052095046,
32.5600778216717));
#219513=CARTESIAN_POINT('Ctrl Pts',(-6.24504024355459,-4.86045125074867,
32.5681804581395));
#219514=CARTESIAN_POINT('Ctrl Pts',(-6.11728667280101,-5.01624608275662,
32.5762830946073));
#219515=CARTESIAN_POINT('Ctrl Pts',(-5.98957211025251,-5.1719933444562,
32.5843832570206));
#219516=CARTESIAN_POINT('Ctrl Pts',(-5.85587580458666,-5.32289741184233,
32.5924834194338));
#219517=CARTESIAN_POINT('Ctrl Pts',(-5.71659700898962,-5.46849518942926,
32.600583581847));
#219518=CARTESIAN_POINT('Ctrl Pts',(-5.57596156991047,-5.61551116046858,
32.6087626437977));
#219519=CARTESIAN_POINT('Ctrl Pts',(-5.42963451903887,-5.75711666265266,
32.6169417057483));
#219520=CARTESIAN_POINT('Ctrl Pts',(-5.27806645274836,-5.89287158526065,
32.625120767699));
#219521=CARTESIAN_POINT('Ctrl Pts',(-5.12796131530042,-6.02731620684901,
32.6332208856746));
#219522=CARTESIAN_POINT('Ctrl Pts',(-4.97271614545482,-6.15602248894394,
32.6413210036503));
#219523=CARTESIAN_POINT('Ctrl Pts',(-4.81280360002459,-6.27860195486147,
32.649421121626));
#219524=CARTESIAN_POINT('Ctrl Pts',(-4.65286953317809,-6.40119791781935,
32.6575223297351));
#219525=CARTESIAN_POINT('Ctrl Pts',(-4.48826709261825,-6.51766522496317,
32.6656235378442));
#219526=CARTESIAN_POINT('Ctrl Pts',(-4.31950020762517,-6.62765712422769,
32.6737247459533));
#219527=CARTESIAN_POINT('Ctrl Pts',(-4.15068881345533,-6.73767803184233,
32.6818280906077));
#219528=CARTESIAN_POINT('Ctrl Pts',(-3.97771105325729,-6.84121995071108,
32.6899314352621));
#219529=CARTESIAN_POINT('Ctrl Pts',(-3.80109834675442,-6.93798042360317,
32.6980347799166));
#219530=CARTESIAN_POINT('Ctrl Pts',(-3.62156845994399,-7.03633912660939,
32.7062719706454));
#219531=CARTESIAN_POINT('Ctrl Pts',(-3.43828279823117,-7.12769023333335,
32.7145091613742));
#219532=CARTESIAN_POINT('Ctrl Pts',(-3.25182371357782,-7.21176563234087,
32.7227463521031));
#219533=CARTESIAN_POINT('Ctrl Pts',(-3.06815553774374,-7.29458259562771,
32.7308602490364));
#219534=CARTESIAN_POINT('Ctrl Pts',(-2.88140858540826,-7.37034004299627,
32.7389741459697));
#219535=CARTESIAN_POINT('Ctrl Pts',(-2.69215801552766,-7.43883097129046,
32.7470880429031));
#219536=CARTESIAN_POINT('Ctrl Pts',(-2.49859384247002,-7.50888301871932,
32.7553868805296));
#219537=CARTESIAN_POINT('Ctrl Pts',(-2.30241090357604,-7.57133323731986,
32.7636857181562));
#219538=CARTESIAN_POINT('Ctrl Pts',(-2.10423946725972,-7.62601450722634,
32.7719845557828));
#219539=CARTESIAN_POINT('Ctrl Pts',(-1.90606803094339,-7.68069577713281,
32.7802833934094));
#219540=CARTESIAN_POINT('Ctrl Pts',(-1.70590845196345,-7.72760805133005,
32.788582231036));
#219541=CARTESIAN_POINT('Ctrl Pts',(-1.50440079314152,-7.76664015218905,
32.7968810686625));
#219542=CARTESIAN_POINT('Ctrl Pts',(-1.31199505282891,-7.80390920839087,
32.8048050553071));
#219543=CARTESIAN_POINT('Ctrl Pts',(-1.11794724197646,-7.83407388985267,
32.8127290419516));
#219544=CARTESIAN_POINT('Ctrl Pts',(-0.922822870368844,-7.85699172393125,
32.8206530285961));
#219545=CARTESIAN_POINT('Ctrl Pts',(-0.72790742030301,-7.87988501966442,
32.8285685309519));
#219546=CARTESIAN_POINT('Ctrl Pts',(-0.531918042238157,-7.89554688301356,
32.8364840333077));
#219547=CARTESIAN_POINT('Ctrl Pts',(-0.33543177697902,-7.90388553326734,
32.8443995356635));
#219548=CARTESIAN_POINT('Ctrl Pts',(-0.13912347375537,-7.91221663101779,
32.8523078687706));
#219549=CARTESIAN_POINT('Ctrl Pts',(0.0576804802670977,-7.91323771422012,
32.8602162018777));
#219550=CARTESIAN_POINT('Ctrl Pts',(0.254396269709758,-7.90690859552314,
32.8681245349847));
#219551=CARTESIAN_POINT('Ctrl Pts',(0.450938590661315,-7.90058505798807,
32.8760258943424));
#219552=CARTESIAN_POINT('Ctrl Pts',(0.647392561310094,-7.88692425101804,
32.8839272537001));
#219553=CARTESIAN_POINT('Ctrl Pts',(0.843172661556533,-7.86593801544378,
32.8918286130578));
#219554=CARTESIAN_POINT('Ctrl Pts',(1.03885195967599,-7.84496258514126,
32.8997259042092));
#219555=CARTESIAN_POINT('Ctrl Pts',(1.23385773914795,-7.81666927600717,
32.9076231953607));
#219556=CARTESIAN_POINT('Ctrl Pts',(1.42760726097397,-7.78112193121367,
32.9155204865121));
#219557=CARTESIAN_POINT('Ctrl Pts',(1.62129091441759,-7.7455866713331,32.9234150928477));
#219558=CARTESIAN_POINT('Ctrl Pts',(1.81371882481146,-7.70280235050061,
32.9313096991832));
#219559=CARTESIAN_POINT('Ctrl Pts',(2.00431583579567,-7.65288436018595,
32.9392043055188));
#219560=CARTESIAN_POINT('Ctrl Pts',(2.13815588371267,-7.61783120703767,
32.944748015175));
#219561=CARTESIAN_POINT('Ctrl Pts',(2.27109324457853,-7.57926148210648,
32.9502917248312));
#219562=CARTESIAN_POINT('Ctrl Pts',(2.40293217908638,-7.53723012403835,
32.9558354344874));
#219563=CARTESIAN_POINT('Ctrl Pts',(2.60554771556565,-7.47263459165091,
32.9643552371562));
#219564=CARTESIAN_POINT('Ctrl Pts',(2.80536580397596,-7.39992595719343,
32.972875039825));
#219565=CARTESIAN_POINT('Ctrl Pts',(3.00176547501411,-7.31938009895738,
32.9813948424938));
#219566=CARTESIAN_POINT('Ctrl Pts',(3.1985203517524,-7.23868856660783,32.9899300539587));
#219567=CARTESIAN_POINT('Ctrl Pts',(3.39184422391902,-7.15013157600585,
32.9984652654236));
#219568=CARTESIAN_POINT('Ctrl Pts',(3.58113923516166,-7.05403166837134,
33.0070004768884));
#219569=CARTESIAN_POINT('Ctrl Pts',(3.78035301829711,-6.95289627112467,
33.0159829205071));
#219570=CARTESIAN_POINT('Ctrl Pts',(3.97510414562345,-6.84340654501848,
33.0249653641257));
#219571=CARTESIAN_POINT('Ctrl Pts',(4.16473106960945,-6.72598960137687,
33.0339478077443));
#219572=CARTESIAN_POINT('Ctrl Pts',(4.34567291235788,-6.61395045785329,
33.0425188474816));
#219573=CARTESIAN_POINT('Ctrl Pts',(4.52194926412814,-6.49469414161851,
33.0510898872189));
#219574=CARTESIAN_POINT('Ctrl Pts',(4.69301903899192,-6.36863355042974,
33.0596609269561));
#219575=CARTESIAN_POINT('Ctrl Pts',(4.86430347557559,-6.24241477593048,
33.0682427218027));
#219576=CARTESIAN_POINT('Ctrl Pts',(5.03036808583398,-6.10937482078115,
33.0768245166493));
#219577=CARTESIAN_POINT('Ctrl Pts',(5.1907054161778,-5.96996635522031,33.0854063114959));
#219578=CARTESIAN_POINT('Ctrl Pts',(5.35131094072339,-5.83032470290213,
33.094002461001));
#219579=CARTESIAN_POINT('Ctrl Pts',(5.50616984471472,-5.68429340668538,
33.1025986105061));
#219580=CARTESIAN_POINT('Ctrl Pts',(5.65481044660595,-5.53236295021904,
33.1111947600111));
#219581=CARTESIAN_POINT('Ctrl Pts',(5.67553169914019,-5.51118307529908,
33.1123931067781));
#219582=CARTESIAN_POINT('Ctrl Pts',(5.69613216964715,-5.48988861109374,
33.1135914535451));
#219583=CARTESIAN_POINT('Ctrl Pts',(5.71661064203229,-5.46848093782937,
33.114789800312));
#219584=CARTESIAN_POINT('Ctrl Pts',(5.8517469197889,-5.32721291617385,33.1226976226586));
#219585=CARTESIAN_POINT('Ctrl Pts',(5.98181649645736,-5.180751969505,33.1306054450051));
#219586=CARTESIAN_POINT('Ctrl Pts',(6.10639715746423,-5.02949647134908,
33.1385132673516));
#219587=CARTESIAN_POINT('Ctrl Pts',(6.23085054327868,-4.8783955001677,33.146413010839));
#219588=CARTESIAN_POINT('Ctrl Pts',(6.34982596579197,-4.72250999835522,
33.1543127543264));
#219589=CARTESIAN_POINT('Ctrl Pts',(6.46293785533335,-4.56227523041948,
33.1622124978138));
#219590=CARTESIAN_POINT('Ctrl Pts',(6.57595518990039,-4.40217440944928,
33.1701056375742));
#219591=CARTESIAN_POINT('Ctrl Pts',(6.68311855829631,-4.23773184540781,
33.1779987773345));
#219592=CARTESIAN_POINT('Ctrl Pts',(6.78408233919181,-4.06941615162,33.1858919170949));
#219593=CARTESIAN_POINT('Ctrl Pts',(6.88498046269459,-3.90120991460482,
33.193779923896));
#219594=CARTESIAN_POINT('Ctrl Pts',(6.97968685448573,-3.7291358608326,33.2016679306971));
#219595=CARTESIAN_POINT('Ctrl Pts',(7.0678987945588,-3.55369211241974,33.2095559374981));
#219596=CARTESIAN_POINT('Ctrl Pts',(7.1560697418556,-3.37832989408455,33.217440278681));
#219597=CARTESIAN_POINT('Ctrl Pts',(7.2377520967932,-3.19960140903364,33.2253246198638));
#219598=CARTESIAN_POINT('Ctrl Pts',(7.31268861647481,-3.01803018515052,
33.2332089610466));
#219599=CARTESIAN_POINT('Ctrl Pts',(7.38760421866241,-2.83650964436564,
33.2410911014245));
#219600=CARTESIAN_POINT('Ctrl Pts',(7.45577760722682,-2.65214826482966,
33.2489732418025));
#219601=CARTESIAN_POINT('Ctrl Pts',(7.51699919169613,-2.46549065137951,
33.2568553821804));
#219602=CARTESIAN_POINT('Ctrl Pts',(7.57822747035189,-2.27881262812,33.2647383844197));
#219603=CARTESIAN_POINT('Ctrl Pts',(7.63250231191321,-2.08983819486411,
33.2726213866589));
#219604=CARTESIAN_POINT('Ctrl Pts',(7.67966344111192,-1.89912886114897,
33.2805043888982));
#219605=CARTESIAN_POINT('Ctrl Pts',(7.72683025810499,-1.70839652723239,
33.2883883418546));
#219606=CARTESIAN_POINT('Ctrl Pts',(7.76688156967074,-1.51592921081426,
33.2962722948111));
#219607=CARTESIAN_POINT('Ctrl Pts',(7.79970786024444,-1.32230037995951,
33.3041562477676));
#219608=CARTESIAN_POINT('Ctrl Pts',(7.83254363023004,-1.12861563394007,
33.3120424774125));
#219609=CARTESIAN_POINT('Ctrl Pts',(7.85815016386974,-0.933769045222951,
33.3199287070574));
#219610=CARTESIAN_POINT('Ctrl Pts',(7.87646959053683,-0.738341241803896,
33.3278149367023));
#219611=CARTESIAN_POINT('Ctrl Pts',(7.8947973882697,-0.542824137609977,
33.3357047699615));
#219612=CARTESIAN_POINT('Ctrl Pts',(7.90583141148543,-0.34672563261261,
33.3435946032207));
#219613=CARTESIAN_POINT('Ctrl Pts',(7.9095658546241,-0.150628653862828,
33.3514844364799));
#219614=CARTESIAN_POINT('Ctrl Pts',(7.91330460454496,0.0456944755994065,
33.3593833687646));
#219615=CARTESIAN_POINT('Ctrl Pts',(7.90972695288974,0.242015730339113,
33.3672823010493));
#219616=CARTESIAN_POINT('Ctrl Pts',(7.89887919719827,0.437753844150282,
33.375181233334));
#219617=CARTESIAN_POINT('Ctrl Pts',(7.88802427672569,0.633621240071249,
33.3830853827458));
#219618=CARTESIAN_POINT('Ctrl Pts',(7.86988971147021,0.828904384874831,
33.3909895321577));
#219619=CARTESIAN_POINT('Ctrl Pts',(7.84457336390429,1.02302968594434,33.3988936815696));
#219620=CARTESIAN_POINT('Ctrl Pts',(7.81922232119861,1.21742102872598,33.4068086633326));
#219621=CARTESIAN_POINT('Ctrl Pts',(7.78666989428001,1.41065101945937,33.4147236450957));
#219622=CARTESIAN_POINT('Ctrl Pts',(7.74706473490351,1.60215760561012,33.4226386268588));
#219623=CARTESIAN_POINT('Ctrl Pts',(7.73028541029121,1.68329226647263,33.4259919285598));
#219624=CARTESIAN_POINT('Ctrl Pts',(7.71224078485991,1.76411778931457,33.4293452302607));
#219625=CARTESIAN_POINT('Ctrl Pts',(7.69294481085428,1.8445924040693,33.4326985319616));
#219626=CARTESIAN_POINT('Ctrl Pts',(7.6482896526346,2.03082848904188,33.4404588149082));
#219627=CARTESIAN_POINT('Ctrl Pts',(7.59678883034721,2.21577027280105,33.4482190978548));
#219628=CARTESIAN_POINT('Ctrl Pts',(7.5385262387593,2.39886288635627,33.4559793808014));
#219629=CARTESIAN_POINT('Ctrl Pts',(7.48033376911482,2.5817351387923,33.4637303238593));
#219630=CARTESIAN_POINT('Ctrl Pts',(7.41539583586916,2.76276231328958,33.4714812669172));
#219631=CARTESIAN_POINT('Ctrl Pts',(7.34384753351423,2.94139837568748,33.4792322099751));
#219632=CARTESIAN_POINT('Ctrl Pts',(7.27237082095791,3.11985569841846,33.4869753975945));
#219633=CARTESIAN_POINT('Ctrl Pts',(7.1942970382658,3.29592634153664,33.494718585214));
#219634=CARTESIAN_POINT('Ctrl Pts',(7.10981143473723,3.46907802773011,33.5024617728334));
#219635=CARTESIAN_POINT('Ctrl Pts',(7.02539324285138,3.64209155500512,33.5101987821104));
#219636=CARTESIAN_POINT('Ctrl Pts',(6.93457357238678,3.81219044163001,33.5179357913873));
#219637=CARTESIAN_POINT('Ctrl Pts',(6.83758630096032,3.97886096476362,33.5256728006642));
#219638=CARTESIAN_POINT('Ctrl Pts',(6.7406567800286,4.14543224492414,33.533405202985));
#219639=CARTESIAN_POINT('Ctrl Pts',(6.63756715092253,4.30857891727795,33.5411376053057));
#219640=CARTESIAN_POINT('Ctrl Pts',(6.52859792619909,4.46781043890953,33.5488700076264));
#219641=CARTESIAN_POINT('Ctrl Pts',(6.41967153992414,4.62697936276311,33.556599370152));
#219642=CARTESIAN_POINT('Ctrl Pts',(6.30487036406361,4.78223590553231,33.5643287326775));
#219643=CARTESIAN_POINT('Ctrl Pts',(6.18451910530415,4.93311711153586,33.5720580952031));
#219644=CARTESIAN_POINT('Ctrl Pts',(6.06416789350083,5.08399825867174,33.579787454713));
#219645=CARTESIAN_POINT('Ctrl Pts',(5.93826681802207,5.23050378465456,33.5875168142229));
#219646=CARTESIAN_POINT('Ctrl Pts',(5.80718212848568,5.37220222316664,33.5952461737328));
#219647=CARTESIAN_POINT('Ctrl Pts',(5.67609086851405,5.51390776411316,33.602975920666));
#219648=CARTESIAN_POINT('Ctrl Pts',(5.53981572038103,5.65080547330261,33.6107056675991));
#219649=CARTESIAN_POINT('Ctrl Pts',(5.39876108033296,5.78249944206501,33.6184354145323));
#219650=CARTESIAN_POINT('Ctrl Pts',(5.25767352373744,5.91422414296617,33.6261669652812));
#219651=CARTESIAN_POINT('Ctrl Pts',(5.11180451665938,6.04074243996941,33.6338985160301));
#219652=CARTESIAN_POINT('Ctrl Pts',(4.96159295997803,6.16169751768913,33.641630066779));
#219653=CARTESIAN_POINT('Ctrl Pts',(4.81131881675027,6.28270299206776,33.6493648389249));
#219654=CARTESIAN_POINT('Ctrl Pts',(4.65669880047748,6.39814040644776,33.6570996110708));
#219655=CARTESIAN_POINT('Ctrl Pts',(4.49820233994311,6.5076951917657,33.6648343832167));
#219656=CARTESIAN_POINT('Ctrl Pts',(4.33951687229848,6.61738062122115,33.6725783790824));
#219657=CARTESIAN_POINT('Ctrl Pts',(4.17694602386429,6.72116920750912,33.680322374948));
#219658=CARTESIAN_POINT('Ctrl Pts',(4.01098636851405,6.8187909010025,33.6880663708137));
#219659=CARTESIAN_POINT('Ctrl Pts',(3.84491899702214,6.91647595587214,33.6958153929211));
#219660=CARTESIAN_POINT('Ctrl Pts',(3.67545875205341,7.00798597507403,33.7035644150286));
#219661=CARTESIAN_POINT('Ctrl Pts',(3.50312378239829,7.09309838964578,33.711313437136));
#219662=CARTESIAN_POINT('Ctrl Pts',(3.33052544431363,7.17834087603641,33.7190743015746));
#219663=CARTESIAN_POINT('Ctrl Pts',(3.15504393341909,7.25716608453744,33.7268351660132));
#219664=CARTESIAN_POINT('Ctrl Pts',(2.97721534149284,7.32940037181621,33.7345960304519));
#219665=CARTESIAN_POINT('Ctrl Pts',(2.85492419423598,7.37907525124317,33.7399331081716));
#219666=CARTESIAN_POINT('Ctrl Pts',(2.73152339249698,7.42563420155241,33.7452701858914));
#219667=CARTESIAN_POINT('Ctrl Pts',(2.60719024406889,7.46903474561687,33.7506072636111));
#219668=CARTESIAN_POINT('Ctrl Pts',(2.42049987204106,7.53420211103824,33.7586210639342));
#219669=CARTESIAN_POINT('Ctrl Pts',(2.23113424949472,7.59244632073761,33.7666348642572));
#219670=CARTESIAN_POINT('Ctrl Pts',(2.03964247063132,7.64354496238473,33.7746486645803));
#219671=CARTESIAN_POINT('Ctrl Pts',(1.8483689697918,7.69458535761214,33.782653330117));
#219672=CARTESIAN_POINT('Ctrl Pts',(1.65497446234548,7.73849632921086,33.7906579956536));
#219673=CARTESIAN_POINT('Ctrl Pts',(1.4600263215984,7.77510412407704,33.7986626611903));
#219674=CARTESIAN_POINT('Ctrl Pts',(1.26526730305292,7.81167640515615,33.8066595612773));
#219675=CARTESIAN_POINT('Ctrl Pts',(1.06895798155994,7.84095956712274,33.8146564613643));
#219676=CARTESIAN_POINT('Ctrl Pts',(0.87167954054783,7.86283001079067,33.8226533614514));
#219677=CARTESIAN_POINT('Ctrl Pts',(0.674559012659043,7.8846829480851,33.830643860355));
#219678=CARTESIAN_POINT('Ctrl Pts',(0.476471242419789,7.89913495629219,
33.8386343592587));
#219679=CARTESIAN_POINT('Ctrl Pts',(0.278006635571342,7.90611366668721,
33.8466248581624));
#219680=CARTESIAN_POINT('Ctrl Pts',(0.0796672382447334,7.91308797427709,
33.8546103159327));
#219681=CARTESIAN_POINT('Ctrl Pts',(-0.119048188392748,7.91259837046145,
33.8625957737031));
#219682=CARTESIAN_POINT('Ctrl Pts',(-0.317544683696693,7.90462436639819,
33.8705812314734));
#219683=CARTESIAN_POINT('Ctrl Pts',(-0.522549404154987,7.89638891382046,
33.8788285132979));
#219684=CARTESIAN_POINT('Ctrl Pts',(-0.727320230152651,7.88016990300526,
33.8870757951224));
#219685=CARTESIAN_POINT('Ctrl Pts',(-0.931201043011376,7.85600315793563,
33.8953230769468));
#219686=CARTESIAN_POINT('Ctrl Pts',(-1.12847562039773,7.83261947433359,
33.9033031267303));
#219687=CARTESIAN_POINT('Ctrl Pts',(-1.32491660216615,7.80179508432112,
33.9112831765138));
#219688=CARTESIAN_POINT('Ctrl Pts',(-1.51993413497656,7.76361521620779,
33.9192632262972));
#219689=CARTESIAN_POINT('Ctrl Pts',(-1.71493618096541,7.72543838005161,
33.9272426423654));
#219690=CARTESIAN_POINT('Ctrl Pts',(-1.90851467496671,7.67990729418527,
33.9352220584335));
#219691=CARTESIAN_POINT('Ctrl Pts',(-2.10008938177088,7.62715842162553,
33.9432014745016));
#219692=CARTESIAN_POINT('Ctrl Pts',(-2.2916783172079,7.57440563130256,33.9511814832167));
#219693=CARTESIAN_POINT('Ctrl Pts',(-2.48126284631228,7.51443407491835,
33.9591614919319));
#219694=CARTESIAN_POINT('Ctrl Pts',(-2.66827696741949,7.44743036389993,
33.967141500647));
#219695=CARTESIAN_POINT('Ctrl Pts',(-2.8553337199984,7.38041137881133,33.9751233284735));
#219696=CARTESIAN_POINT('Ctrl Pts',(-3.03981858195051,7.30635715717243,
33.9831051563001));
#219697=CARTESIAN_POINT('Ctrl Pts',(-3.22118427901842,7.22550294724212,
33.9910869841266));
#219698=CARTESIAN_POINT('Ctrl Pts',(-3.40268482963671,7.14458861857134,
33.999074746801));
#219699=CARTESIAN_POINT('Ctrl Pts',(-3.58106127676926,7.05686433803137,
34.0070625094754));
#219700=CARTESIAN_POINT('Ctrl Pts',(-3.75578884196494,6.96261238146801,
34.0150502721498));
#219701=CARTESIAN_POINT('Ctrl Pts',(-3.93059336339302,6.86831891299172,
34.0230415529188));
#219702=CARTESIAN_POINT('Ctrl Pts',(-4.10174550842667,6.76749220202758,
34.0310328336879));
#219703=CARTESIAN_POINT('Ctrl Pts',(-4.26874787360661,6.66045888746256,
34.039024114457));
#219704=CARTESIAN_POINT('Ctrl Pts',(-4.43590736580849,6.55332486877909,
34.0470229139588));
#219705=CARTESIAN_POINT('Ctrl Pts',(-4.59890900402786,6.43997277148666,
34.0550217134607));
#219706=CARTESIAN_POINT('Ctrl Pts',(-4.75728616458605,6.32077126213551,
34.0630205129625));
#219707=CARTESIAN_POINT('Ctrl Pts',(-4.79355656083256,6.29347259127849,
34.0648523403952));
#219708=CARTESIAN_POINT('Ctrl Pts',(-4.82958456007265,6.26586729955871,
34.0666841678279));
#219709=CARTESIAN_POINT('Ctrl Pts',(-4.86536481653062,6.23796009942882,
34.0685159952606));
#219710=CARTESIAN_POINT('Ctrl Pts',(-5.02409905343179,6.11415360514417,
34.0766426482937));
#219711=CARTESIAN_POINT('Ctrl Pts',(-5.17823453496432,5.98418379559127,
34.0847693013268));
#219712=CARTESIAN_POINT('Ctrl Pts',(-5.32728194534809,5.84841757014393,
34.0928959543598));
#219713=CARTESIAN_POINT('Ctrl Pts',(-5.47620247989274,5.71276691499556,
34.1010156896214));
#219714=CARTESIAN_POINT('Ctrl Pts',(-5.62004334347727,5.57132989459795,
34.109135424883));
#219715=CARTESIAN_POINT('Ctrl Pts',(-5.75834768658442,5.42451407228407,
34.1172551601446));
#219716=CARTESIAN_POINT('Ctrl Pts',(-5.89655171532517,5.27780473784946,
34.1253690060315));
#219717=CARTESIAN_POINT('Ctrl Pts',(-6.02922701250107,5.12572461156609,
34.1334828519184));
#219718=CARTESIAN_POINT('Ctrl Pts',(-6.15595264358235,4.96871895461712,
34.1415966978053));
#219719=CARTESIAN_POINT('Ctrl Pts',(-6.28258823138525,4.81182485603212,
34.1497047785027));
#219720=CARTESIAN_POINT('Ctrl Pts',(-6.40328238722698,4.65001245644391,
34.1578128592001));
#219721=CARTESIAN_POINT('Ctrl Pts',(-6.51765338771445,4.48376129132834,
34.1659209398974));
#219722=CARTESIAN_POINT('Ctrl Pts',(-6.63197526528062,4.31758153192632,
34.1740255381332));
#219723=CARTESIAN_POINT('Ctrl Pts',(-6.73997922220622,4.14696707052053,
34.1821301363691));
#219724=CARTESIAN_POINT('Ctrl Pts',(-6.84132542625956,3.97242840237738,
34.1902347346049));
#219725=CARTESIAN_POINT('Ctrl Pts',(-6.94263995244727,3.79794428992803,
34.1983367995798));
#219726=CARTESIAN_POINT('Ctrl Pts',(-7.03730071617164,3.61953869245295,
34.2064388645547));
#219727=CARTESIAN_POINT('Ctrl Pts',(-7.12501233872718,3.43774928884954,
34.2145409295297));
#219728=CARTESIAN_POINT('Ctrl Pts',(-7.17166963839849,3.34104827667042,
34.2188507400483));
#219729=CARTESIAN_POINT('Ctrl Pts',(-7.21636137211169,3.24339022665641,
34.2231605505669));
#219730=CARTESIAN_POINT('Ctrl Pts',(-7.25904840949159,3.14485885035522,
34.2274703610855));
#219731=CARTESIAN_POINT('Ctrl Pts',(-7.3397234526633,2.95864252978646,34.2356155538885));
#219732=CARTESIAN_POINT('Ctrl Pts',(-7.41321019089491,2.76936358343293,
34.2437607466915));
#219733=CARTESIAN_POINT('Ctrl Pts',(-7.47929653081031,2.57760439249488,
34.2519059394945));
#219734=CARTESIAN_POINT('Ctrl Pts',(-7.54540914024934,2.38576897668789,
34.2600543700367));
#219735=CARTESIAN_POINT('Ctrl Pts',(-7.60411538130517,2.19145164546105,
34.268202800579));
#219736=CARTESIAN_POINT('Ctrl Pts',(-7.65525293737596,1.99525022611117,
34.2763512311212));
#219737=CARTESIAN_POINT('Ctrl Pts',(-7.70643729736452,1.79886923237797,
34.2845071195575));
#219738=CARTESIAN_POINT('Ctrl Pts',(-7.75003905080395,1.60060100786197,
34.2926630079937));
#219739=CARTESIAN_POINT('Ctrl Pts',(-7.7859466513297,1.40105522469594,34.30081889643));
#219740=CARTESIAN_POINT('Ctrl Pts',(-7.82187261808719,1.20140737667341,
34.3089789564882));
#219741=CARTESIAN_POINT('Ctrl Pts',(-7.85009653171284,1.00048097534893,
34.3171390165465));
#219742=CARTESIAN_POINT('Ctrl Pts',(-7.87055857554369,0.798892176038643,
34.3252990766047));
#219743=CARTESIAN_POINT('Ctrl Pts',(-7.89104121973609,0.597100425244778,
34.3334673518828));
#219744=CARTESIAN_POINT('Ctrl Pts',(-7.90374635618476,0.394645255978008,
34.3416356271609));
#219745=CARTESIAN_POINT('Ctrl Pts',(-7.90866620186477,0.192145537241679,
34.3498039024389));
#219746=CARTESIAN_POINT('Ctrl Pts',(-7.91024517924965,0.127155190567017,
34.3524254322137));
#219747=CARTESIAN_POINT('Ctrl Pts',(-7.91102265168034,0.0621602421645904,
34.3550469619885));
#219748=CARTESIAN_POINT('Ctrl Pts',(-7.91099949777088,-0.00281891271787961,
34.3576684917633));
#219749=CARTESIAN_POINT('',(-7.91647471845545,0.00302621288097889,36.3576684917633));
#219750=CARTESIAN_POINT('Ctrl Pts',(-7.91204594914714,-0.00281928559808421,
34.3576684917633));
#219751=CARTESIAN_POINT('Ctrl Pts',(-7.91263194564264,-0.240441980020169,
34.3672539034789));
#219752=CARTESIAN_POINT('Ctrl Pts',(-7.84556028379859,-1.79088486701073,
34.4298241038026));
#219753=CARTESIAN_POINT('Ctrl Pts',(-6.85004567783285,-4.57189276894299,
34.5453790927351));
#219754=CARTESIAN_POINT('Ctrl Pts',(-2.81663569969601,-8.25789292523349,
34.7573182471679));
#219755=CARTESIAN_POINT('Ctrl Pts',(3.1111528735023,-8.15382484340564,34.969257401601));
#219756=CARTESIAN_POINT('Ctrl Pts',(6.99765226366875,-4.32682987995013,
35.1811965560339));
#219757=CARTESIAN_POINT('Ctrl Pts',(8.68015910443019,0.833487127119469,
35.3931357104671));
#219758=CARTESIAN_POINT('Ctrl Pts',(5.50527049693975,7.57558763524673,35.6580596535081));
#219759=CARTESIAN_POINT('Ctrl Pts',(-3.41422952378675,8.71262350896433,
35.9759683851579));
#219760=CARTESIAN_POINT('Ctrl Pts',(-7.61324989218557,3.69250539781279,
36.2091713312427));
#219761=CARTESIAN_POINT('Ctrl Pts',(-7.91879245460977,0.531856155555196,
36.3364047001113));
#219762=CARTESIAN_POINT('Ctrl Pts',(-7.91647471845545,0.00302621288097889,
36.3576684917633));
#219763=CARTESIAN_POINT('',(-7.91099900736828,0.00390977488672659,38.3579590976759));
#219764=CARTESIAN_POINT('Ctrl Pts',(-7.91099942198829,0.00302411985178654,
36.3576684917633));
#219765=CARTESIAN_POINT('Ctrl Pts',(-7.91107476249638,-0.194064205058786,
36.3655987410024));
#219766=CARTESIAN_POINT('Ctrl Pts',(-7.90378024015271,-0.391324740971317,
36.3735289902414));
#219767=CARTESIAN_POINT('Ctrl Pts',(-7.88910633031748,-0.588151603708371,
36.3814592394805));
#219768=CARTESIAN_POINT('Ctrl Pts',(-7.87478977333831,-0.780185153528796,
36.3891963638301));
#219769=CARTESIAN_POINT('Ctrl Pts',(-7.85344908612159,-0.971805523534133,
36.3969334881797));
#219770=CARTESIAN_POINT('Ctrl Pts',(-7.82512812677067,-1.16245034286313,
36.4046706125293));
#219771=CARTESIAN_POINT('Ctrl Pts',(-7.79574679629921,-1.36023313581051,
36.4126974242131));
#219772=CARTESIAN_POINT('Ctrl Pts',(-7.75885239555156,-1.55696551137542,
36.4207242358969));
#219773=CARTESIAN_POINT('Ctrl Pts',(-7.71455283276676,-1.75202613863217,
36.4287510475807));
#219774=CARTESIAN_POINT('Ctrl Pts',(-7.67025326998196,-1.94708676588892,
36.4367778592645));
#219775=CARTESIAN_POINT('Ctrl Pts',(-7.61854863814548,-2.14047522170225,
36.4448046709482));
#219776=CARTESIAN_POINT('Ctrl Pts',(-7.55960584956221,-2.33158323875963,
36.452831482632));
#219777=CARTESIAN_POINT('Ctrl Pts',(-7.49873986595021,-2.52892675972155,
36.4611201944515));
#219778=CARTESIAN_POINT('Ctrl Pts',(-7.43016362405057,-2.72381637900719,
36.469408906271));
#219779=CARTESIAN_POINT('Ctrl Pts',(-7.35410670943481,-2.91565352987044,
36.4776976180904));
#219780=CARTESIAN_POINT('Ctrl Pts',(-7.27800594875152,-3.10760127297521,
36.4859911082712));
#219781=CARTESIAN_POINT('Ctrl Pts',(-7.19441601513058,-3.29649276321212,
36.494284598452));
#219782=CARTESIAN_POINT('Ctrl Pts',(-7.10361425212294,-3.48175035823016,
36.5025780886328));
#219783=CARTESIAN_POINT('Ctrl Pts',(-7.01275466831001,-3.66712592169922,
36.5108768599476));
#219784=CARTESIAN_POINT('Ctrl Pts',(-6.91467421693679,-3.84886270843548,
36.5191756312624));
#219785=CARTESIAN_POINT('Ctrl Pts',(-6.80969610124306,-4.02640782940763,
36.5274744025772));
#219786=CARTESIAN_POINT('Ctrl Pts',(-6.70459578496448,-4.20415962314656,
36.5357828341408));
#219787=CARTESIAN_POINT('Ctrl Pts',(-6.59258190386947,-4.3777097458219,
36.5440912657043));
#219788=CARTESIAN_POINT('Ctrl Pts',(-6.47402183736757,-4.54653299221372,
36.5523996972678));
#219789=CARTESIAN_POINT('Ctrl Pts',(-6.35538863497532,-4.71546038023435,
36.5607132540355));
#219790=CARTESIAN_POINT('Ctrl Pts',(-6.23020135994754,-4.87965483613968,
36.5690268108031));
#219791=CARTESIAN_POINT('Ctrl Pts',(-6.09886844427265,-5.03862329406112,
36.5773403675708));
#219792=CARTESIAN_POINT('Ctrl Pts',(-5.9673919433846,-5.19776555091025,
36.5856630134827));
#219793=CARTESIAN_POINT('Ctrl Pts',(-5.82975656394132,-5.35167016877368,
36.5939856593946));
#219794=CARTESIAN_POINT('Ctrl Pts',(-5.68640953514584,-5.49987887126639,
36.6023083053066));
#219795=CARTESIAN_POINT('Ctrl Pts',(-5.63199664509257,-5.55613719696339,
36.6054674863567));
#219796=CARTESIAN_POINT('Ctrl Pts',(-5.57676114621976,-5.61157520261264,
36.6086266674068));
#219797=CARTESIAN_POINT('Ctrl Pts',(-5.52072881163643,-5.66616928694929,
36.6117858484569));
#219798=CARTESIAN_POINT('Ctrl Pts',(-5.36645418003708,-5.8164839634869,
36.6204840670173));
#219799=CARTESIAN_POINT('Ctrl Pts',(-5.20599955280558,-5.9605317973859,
36.6291822855778));
#219800=CARTESIAN_POINT('Ctrl Pts',(-5.03987436346181,-6.09783464850601,
36.6378805041383));
#219801=CARTESIAN_POINT('Ctrl Pts',(-4.87389513736593,-6.235016860666,36.6465710801477));
#219802=CARTESIAN_POINT('Ctrl Pts',(-4.70225547389765,-6.36546577796639,
36.6552616561572));
#219803=CARTESIAN_POINT('Ctrl Pts',(-4.52549880935453,-6.48874267686204,
36.6639522321667));
#219804=CARTESIAN_POINT('Ctrl Pts',(-4.34450306262691,-6.61497607477977,
36.6728512306762));
#219805=CARTESIAN_POINT('Ctrl Pts',(-4.158141977721,-6.73368897837097,36.6817502291858));
#219806=CARTESIAN_POINT('Ctrl Pts',(-3.96703473233668,-6.84445442912979,
36.6906492276954));
#219807=CARTESIAN_POINT('Ctrl Pts',(-3.78095329528384,-6.9523069294971,
36.6993141970829));
#219808=CARTESIAN_POINT('Ctrl Pts',(-3.5903723669704,-7.05262452971617,
36.7079791664705));
#219809=CARTESIAN_POINT('Ctrl Pts',(-3.39589382665893,-7.14505606122582,
36.716644135858));
#219810=CARTESIAN_POINT('Ctrl Pts',(-3.19353638222078,-7.24123226900607,
36.7256601489286));
#219811=CARTESIAN_POINT('Ctrl Pts',(-2.98695913188559,-7.328869994186,36.7346761619992));
#219812=CARTESIAN_POINT('Ctrl Pts',(-2.77687127158161,-7.40762491903206,
36.7436921750698));
#219813=CARTESIAN_POINT('Ctrl Pts',(-2.56678341127766,-7.48637984387811,
36.7527081881404));
#219814=CARTESIAN_POINT('Ctrl Pts',(-2.35318517926386,-7.55625180730678,
36.761724201211));
#219815=CARTESIAN_POINT('Ctrl Pts',(-2.13681410900475,-7.61695125779063,
36.7707402142816));
#219816=CARTESIAN_POINT('Ctrl Pts',(-1.94937499274797,-7.66953431033245,
36.7785506554837));
#219817=CARTESIAN_POINT('Ctrl Pts',(-1.75993569387107,-7.7152106682391,
36.7863610966859));
#219818=CARTESIAN_POINT('Ctrl Pts',(-1.56905280285689,-7.75383739201738,
36.7941715378881));
#219819=CARTESIAN_POINT('Ctrl Pts',(-1.37818367411464,-7.7924613308867,
36.8019814159732));
#219820=CARTESIAN_POINT('Ctrl Pts',(-1.18587150572844,-7.82403657819518,
36.8097912940583));
#219821=CARTESIAN_POINT('Ctrl Pts',(-0.992683632905888,-7.84847120176667,
36.8176011721434));
#219822=CARTESIAN_POINT('Ctrl Pts',(-0.799475589840243,-7.87290837649363,
36.8254118656376));
#219823=CARTESIAN_POINT('Ctrl Pts',(-0.605392009731172,-7.89020339912567,
36.8332225591317));
#219824=CARTESIAN_POINT('Ctrl Pts',(-0.411006059591829,-7.90031613411633,
36.8410332526259));
#219825=CARTESIAN_POINT('Ctrl Pts',(-0.216482162367165,-7.91043604566639,
36.8488494890227));
#219826=CARTESIAN_POINT('Ctrl Pts',(-0.0216558185432678,-7.91336346825983,
36.8566657254195));
#219827=CARTESIAN_POINT('Ctrl Pts',(0.172898201252367,-7.90911039321134,
36.8644819618164));
#219828=CARTESIAN_POINT('Ctrl Pts',(0.367524150485898,-7.90485574573944,
36.8723010879889));
#219829=CARTESIAN_POINT('Ctrl Pts',(0.56187722347289,-7.89341532808239,
36.8801202141615));
#219830=CARTESIAN_POINT('Ctrl Pts',(0.755386913604808,-7.87485311677333,
36.8879393403341));
#219831=CARTESIAN_POINT('Ctrl Pts',(0.94911178083699,-7.85627026482968,
36.8957671611457));
#219832=CARTESIAN_POINT('Ctrl Pts',(1.14199104226654,-7.83054984195504,
36.9035949819573));
#219833=CARTESIAN_POINT('Ctrl Pts',(1.33346243678921,-7.79780731550044,
36.9114228027688));
#219834=CARTESIAN_POINT('Ctrl Pts',(1.48244058245026,-7.77233133833098,
36.9175133952147));
#219835=CARTESIAN_POINT('Ctrl Pts',(1.63056657029824,-7.74260527242311,
36.9236039876605));
#219836=CARTESIAN_POINT('Ctrl Pts',(1.77758179887016,-7.70870442735519,
36.9296945801064));
#219837=CARTESIAN_POINT('Ctrl Pts',(1.97351011518767,-7.66352451259113,
36.9378115591084));
#219838=CARTESIAN_POINT('Ctrl Pts',(2.16785460434091,-7.61083846189088,
36.9459285381104));
#219839=CARTESIAN_POINT('Ctrl Pts',(2.3600193048635,-7.55077677333078,36.9540455171123));
#219840=CARTESIAN_POINT('Ctrl Pts',(2.55204344357796,-7.49075901781104,
36.9621565588259));
#219841=CARTESIAN_POINT('Ctrl Pts',(2.74189066777335,-7.42337647672146,
36.9702676005396));
#219842=CARTESIAN_POINT('Ctrl Pts',(2.92897782587097,-7.34881010065957,
36.9783786422531));
#219843=CARTESIAN_POINT('Ctrl Pts',(3.11595473668884,-7.27428766529466,
36.9864849042678));
#219844=CARTESIAN_POINT('Ctrl Pts',(3.30017452750588,-7.1925899548432,36.9945911662825));
#219845=CARTESIAN_POINT('Ctrl Pts',(3.48107121658169,-7.10394708490192,
37.0026974282972));
#219846=CARTESIAN_POINT('Ctrl Pts',(3.66188699914079,-7.01534386071576,
37.010800064765));
#219847=CARTESIAN_POINT('Ctrl Pts',(3.83938235647035,-6.91980181257708,
37.0189027012329));
#219848=CARTESIAN_POINT('Ctrl Pts',(4.01301270567736,-6.81759855257495,
37.0270053377007));
#219849=CARTESIAN_POINT('Ctrl Pts',(4.18659003868975,-6.7154264992596,37.035105500114));
#219850=CARTESIAN_POINT('Ctrl Pts',(4.35630444132757,-6.60659745331978,
37.0432056625273));
#219851=CARTESIAN_POINT('Ctrl Pts',(4.52163679433242,-6.49143448708675,
37.0513058249406));
#219852=CARTESIAN_POINT('Ctrl Pts',(4.68857956518987,-6.37514977732676,
37.0594848868912));
#219853=CARTESIAN_POINT('Ctrl Pts',(4.85105417908993,-6.25240726674657,
37.0676639488419));
#219854=CARTESIAN_POINT('Ctrl Pts',(5.00855630989813,-6.12358430092864,
37.0758430107925));
#219855=CARTESIAN_POINT('Ctrl Pts',(5.16453823651368,-5.99600472916347,
37.0839431287682));
#219856=CARTESIAN_POINT('Ctrl Pts',(5.31564300693685,-5.86246178413592,
37.0920432467439));
#219857=CARTESIAN_POINT('Ctrl Pts',(5.46141391000008,-5.72336256964886,
37.1001433647196));
#219858=CARTESIAN_POINT('Ctrl Pts',(5.60720443126282,-5.58424463485422,
37.1082445728287));
#219859=CARTESIAN_POINT('Ctrl Pts',(5.74765942143414,-5.43956916074917,
37.1163457809378));
#219860=CARTESIAN_POINT('Ctrl Pts',(5.8823585729742,-5.28978058325267,37.1244469890468));
#219861=CARTESIAN_POINT('Ctrl Pts',(6.01709324894984,-5.1399525017607,37.1325503337013));
#219862=CARTESIAN_POINT('Ctrl Pts',(6.14606884454866,-4.98500886611857,
37.1406536783557));
#219863=CARTESIAN_POINT('Ctrl Pts',(6.26890457849805,-4.82542810387702,
37.1487570230102));
#219864=CARTESIAN_POINT('Ctrl Pts',(6.39376923772251,-4.6632114845317,37.156994213739));
#219865=CARTESIAN_POINT('Ctrl Pts',(6.51228922050543,-4.49620348421384,
37.1652314044678));
#219866=CARTESIAN_POINT('Ctrl Pts',(6.62410982722577,-4.32493814948271,
37.1734685951966));
#219867=CARTESIAN_POINT('Ctrl Pts',(6.73425670955768,-4.15623630439844,
37.1815824921299));
#219868=CARTESIAN_POINT('Ctrl Pts',(6.83790322831374,-3.98340397470245,
37.1896963890633));
#219869=CARTESIAN_POINT('Ctrl Pts',(6.93475617045278,-3.80697752244048,
37.1978102859966));
#219870=CARTESIAN_POINT('Ctrl Pts',(7.03381668934642,-3.6265297681271,37.2061091236232));
#219871=CARTESIAN_POINT('Ctrl Pts',(7.12577008698459,-3.44232241762529,
37.2144079612497));
#219872=CARTESIAN_POINT('Ctrl Pts',(7.21035405914917,-3.254952433095,37.2227067988763));
#219873=CARTESIAN_POINT('Ctrl Pts',(7.29493803131375,-3.06758244856471,
37.2310056365028));
#219874=CARTESIAN_POINT('Ctrl Pts',(7.37215247685052,-2.87705017327259,
37.2393044741294));
#219875=CARTESIAN_POINT('Ctrl Pts',(7.44178885452159,-2.683970872554,37.2476033117559));
#219876=CARTESIAN_POINT('Ctrl Pts',(7.50827982006027,-2.49961278903974,
37.2555272984004));
#219877=CARTESIAN_POINT('Ctrl Pts',(7.56800456966879,-2.31253682802811,
37.263451285045));
#219878=CARTESIAN_POINT('Ctrl Pts',(7.62073513691692,-2.12327976794391,
37.2713752716895));
#219879=CARTESIAN_POINT('Ctrl Pts',(7.6734092450396,-1.93422534721395,37.2792907740453));
#219880=CARTESIAN_POINT('Ctrl Pts',(7.71910399549655,-1.74299480556682,
37.2872062764011));
#219881=CARTESIAN_POINT('Ctrl Pts',(7.75763972954911,-1.55014413088628,
37.2951217787569));
#219882=CARTESIAN_POINT('Ctrl Pts',(7.79614056091922,-1.35746812540629,
37.3030301118639));
#219883=CARTESIAN_POINT('Ctrl Pts',(7.82749522594396,-1.16317524362569,
37.310938444971));
#219884=CARTESIAN_POINT('Ctrl Pts',(7.85157399763482,-0.967836122318609,
37.318846778078));
#219885=CARTESIAN_POINT('Ctrl Pts',(7.8756315361131,-0.772669255524447,
37.3267481374357));
#219886=CARTESIAN_POINT('Ctrl Pts',(7.892425930422,-0.576458326801188,37.3346494967933));
#219887=CARTESIAN_POINT('Ctrl Pts',(7.90187859668068,-0.379783679638453,
37.342550856151));
#219888=CARTESIAN_POINT('Ctrl Pts',(7.91132639600518,-0.183210295181699,
37.3504481473024));
#219889=CARTESIAN_POINT('Ctrl Pts',(7.91343998100059,0.013825991140516,
37.3583454384539));
#219890=CARTESIAN_POINT('Ctrl Pts',(7.90819257704468,0.210739565282478,
37.3662427296053));
#219891=CARTESIAN_POINT('Ctrl Pts',(7.90294695703129,0.407586195369699,
37.3741373359408));
#219892=CARTESIAN_POINT('Ctrl Pts',(7.89034534262739,0.604309854653562,
37.3820319422764));
#219893=CARTESIAN_POINT('Ctrl Pts',(7.870413060219,0.800324472657258,37.3899265486119));
#219894=CARTESIAN_POINT('Ctrl Pts',(7.85641631588982,0.937968844574584,
37.3954702582682));
#219895=CARTESIAN_POINT('Ctrl Pts',(7.838805867321,1.0752635556771,37.4010139679244));
#219896=CARTESIAN_POINT('Ctrl Pts',(7.81760581450124,1.21200673639894,37.4065576775806));
#219897=CARTESIAN_POINT('Ctrl Pts',(7.7850246950356,1.42215932163486,37.4150774802494));
#219898=CARTESIAN_POINT('Ctrl Pts',(7.74399615321713,1.63079889778628,37.4235972829182));
#219899=CARTESIAN_POINT('Ctrl Pts',(7.69469701891557,1.83726938337627,37.4321170855871));
#219900=CARTESIAN_POINT('Ctrl Pts',(7.64530872288838,2.04411328860228,37.440652297052));
#219901=CARTESIAN_POINT('Ctrl Pts',(7.58761999670923,2.24878002015923,37.4491875085169));
#219902=CARTESIAN_POINT('Ctrl Pts',(7.52185733897788,2.4506291380102,37.4577227199818));
#219903=CARTESIAN_POINT('Ctrl Pts',(7.4526488175824,2.66305484392548,37.4667051636004));
#219904=CARTESIAN_POINT('Ctrl Pts',(7.37449776855023,2.87235944314116,37.475687607219));
#219905=CARTESIAN_POINT('Ctrl Pts',(7.28772418927061,3.0778234421617,37.4846700508377));
#219906=CARTESIAN_POINT('Ctrl Pts',(7.20492491685308,3.27387700786832,37.493241090575));
#219907=CARTESIAN_POINT('Ctrl Pts',(7.11427539764419,3.46643371593889,37.5018121303123));
#219908=CARTESIAN_POINT('Ctrl Pts',(7.01610015978658,3.65489528548257,37.5103831700496));
#219909=CARTESIAN_POINT('Ctrl Pts',(6.91780172970799,3.84359334031346,37.5189649648963));
#219910=CARTESIAN_POINT('Ctrl Pts',(6.81195883449633,4.02818577239186,37.527546759743));
#219911=CARTESIAN_POINT('Ctrl Pts',(6.69894048499784,4.20810139830981,37.5361285545897));
#219912=CARTESIAN_POINT('Ctrl Pts',(6.58573309115283,4.38831796679222,37.5447247040947));
#219913=CARTESIAN_POINT('Ctrl Pts',(6.46532638008344,4.5638418784101,37.5533208535998));
#219914=CARTESIAN_POINT('Ctrl Pts',(6.33813223962513,4.7341314634286,37.5619170031049));
#219915=CARTESIAN_POINT('Ctrl Pts',(6.32040073240938,4.75787069382586,37.5631153498717));
#219916=CARTESIAN_POINT('Ctrl Pts',(6.30253738256674,4.78150825552507,37.5643136966385));
#219917=CARTESIAN_POINT('Ctrl Pts',(6.28454336630384,4.80504273415403,37.5655120434053));
#219918=CARTESIAN_POINT('Ctrl Pts',(6.16580187356797,4.96034542380006,37.5734198657519));
#219919=CARTESIAN_POINT('Ctrl Pts',(6.04114830945474,5.11144271903652,37.5813276880984));
#219920=CARTESIAN_POINT('Ctrl Pts',(5.91091118070632,5.25785602824963,37.589235510445));
#219921=CARTESIAN_POINT('Ctrl Pts',(5.78080710596087,5.40411975740776,37.5971352539323));
#219922=CARTESIAN_POINT('Ctrl Pts',(5.64513105637164,5.54570877677501,37.6050349974197));
#219923=CARTESIAN_POINT('Ctrl Pts',(5.50425363886146,5.68217501306325,37.6129347409071));
#219924=CARTESIAN_POINT('Ctrl Pts',(5.3634939866952,5.81852717149903,37.6208278806675));
#219925=CARTESIAN_POINT('Ctrl Pts',(5.21754187482366,5.94976483924279,37.6287210204279));
#219926=CARTESIAN_POINT('Ctrl Pts',(5.06680701991465,6.07547427144117,37.6366141601883));
#219927=CARTESIAN_POINT('Ctrl Pts',(4.9161701888471,6.20110195399076,37.6445021669893));
#219928=CARTESIAN_POINT('Ctrl Pts',(4.76075707549972,6.32120834360865,37.6523901737904));
#219929=CARTESIAN_POINT('Ctrl Pts',(4.60101316751264,6.43541753364732,37.6602781805914));
#219930=CARTESIAN_POINT('Ctrl Pts',(4.44134349376458,6.54957364978527,37.6681625217742));
#219931=CARTESIAN_POINT('Ctrl Pts',(4.27734731577844,6.65783782706723,37.676046862957));
#219932=CARTESIAN_POINT('Ctrl Pts',(4.10950223537964,6.75987517469145,37.6839312041398));
#219933=CARTESIAN_POINT('Ctrl Pts',(3.94170400661599,6.86188403999989,37.6918133445177));
#219934=CARTESIAN_POINT('Ctrl Pts',(3.77005931122769,6.95766936099216,37.6996954848956));
#219935=CARTESIAN_POINT('Ctrl Pts',(3.59507392359959,7.04694007948516,37.7075776252735));
#219936=CARTESIAN_POINT('Ctrl Pts',(3.42006940244416,7.13622055915739,37.7154606275128));
#219937=CARTESIAN_POINT('Ctrl Pts',(3.24172376327543,7.21898485001104,37.7233436297521));
#219938=CARTESIAN_POINT('Ctrl Pts',(3.06056708707034,7.2949880127072,37.7312266319914));
#219939=CARTESIAN_POINT('Ctrl Pts',(2.87938856274774,7.3710003416459,37.7391105849478));
#219940=CARTESIAN_POINT('Ctrl Pts',(2.69539864384964,7.44024978345649,37.7469945379042));
#219941=CARTESIAN_POINT('Ctrl Pts',(2.50914705365698,7.50253970753401,37.7548784908607));
#219942=CARTESIAN_POINT('Ctrl Pts',(2.3228416786623,7.56484761938404,37.7627647205056));
#219943=CARTESIAN_POINT('Ctrl Pts',(2.13427365805966,7.62019189917519,37.7706509501505));
#219944=CARTESIAN_POINT('Ctrl Pts',(1.94400775272161,7.66842583959435,37.7785371797954));
#219945=CARTESIAN_POINT('Ctrl Pts',(1.75365490533875,7.71668182052256,37.7864270130546));
#219946=CARTESIAN_POINT('Ctrl Pts',(1.56160296125589,7.75782090296864,37.7943168463138));
#219947=CARTESIAN_POINT('Ctrl Pts',(1.36842698097498,7.79174746752869,37.802206679573));
#219948=CARTESIAN_POINT('Ctrl Pts',(1.17502821865124,7.82571315822309,37.8101056118577));
#219949=CARTESIAN_POINT('Ctrl Pts',(0.9805031706794,7.85244965697262,37.8180045441423));
#219950=CARTESIAN_POINT('Ctrl Pts',(0.78543329051248,7.87191308044968,37.825903476427));
#219951=CARTESIAN_POINT('Ctrl Pts',(0.590234569593391,7.89138935922822,
37.8338076258389));
#219952=CARTESIAN_POINT('Ctrl Pts',(0.39449064227463,7.90358296490442,37.8417117752508));
#219953=CARTESIAN_POINT('Ctrl Pts',(0.198783331142212,7.90850214561898,
37.8496159246627));
#219954=CARTESIAN_POINT('Ctrl Pts',(0.00280781021079834,7.91342806789298,
37.8575309064257));
#219955=CARTESIAN_POINT('Ctrl Pts',(-0.193130650653157,7.91105965676954,
37.8654458881888));
#219956=CARTESIAN_POINT('Ctrl Pts',(-0.388453799583046,7.90145712167,37.8733608699519));
#219957=CARTESIAN_POINT('Ctrl Pts',(-0.471205404976599,7.89738886248163,
37.8767141716529));
#219958=CARTESIAN_POINT('Ctrl Pts',(-0.553846669945976,7.89202276760672,
37.8800674733539));
#219959=CARTESIAN_POINT('Ctrl Pts',(-0.636334172624782,7.88536618177938,
37.8834207750549));
#219960=CARTESIAN_POINT('Ctrl Pts',(-0.827228526136434,7.86996136763375,
37.8911810580015));
#219961=CARTESIAN_POINT('Ctrl Pts',(-1.01789961082983,7.84759318625714,
37.8989413409481));
#219962=CARTESIAN_POINT('Ctrl Pts',(-1.20778625754698,7.81825897218049,
37.9067016238947));
#219963=CARTESIAN_POINT('Ctrl Pts',(-1.3974443661861,7.78896006329786,37.9144525669526));
#219964=CARTESIAN_POINT('Ctrl Pts',(-1.58631956594894,7.75271186340924,
37.9222035100104));
#219965=CARTESIAN_POINT('Ctrl Pts',(-1.77385152220997,7.70956365672879,
37.9299544530683));
#219966=CARTESIAN_POINT('Ctrl Pts',(-1.9611958377506,7.66645862327997,37.9376976406878));
#219967=CARTESIAN_POINT('Ctrl Pts',(-2.14719923865808,7.61646740642545,
37.9454408283072));
#219968=CARTESIAN_POINT('Ctrl Pts',(-2.33130724911348,7.55969096658263,
37.9531840159267));
#219969=CARTESIAN_POINT('Ctrl Pts',(-2.51526835852451,7.50295982905059,
37.9609210252036));
#219970=CARTESIAN_POINT('Ctrl Pts',(-2.69733674743482,7.43945435264161,
37.9686580344805));
#219971=CARTESIAN_POINT('Ctrl Pts',(-2.87696877445214,7.36932640550189,
37.9763950437574));
#219972=CARTESIAN_POINT('Ctrl Pts',(-3.056493840646,7.29924021563173,37.9841274460782));
#219973=CARTESIAN_POINT('Ctrl Pts',(-3.23358510038085,7.22253953731047,
37.9918598483989));
#219974=CARTESIAN_POINT('Ctrl Pts',(-3.40771462419382,7.13942589008777,
37.9995922507196));
#219975=CARTESIAN_POINT('Ctrl Pts',(-3.58177569346296,7.05634491685787,
38.0073216132452));
#219976=CARTESIAN_POINT('Ctrl Pts',(-3.75287702226877,6.96685615034051,
38.0150509757708));
#219977=CARTESIAN_POINT('Ctrl Pts',(-3.92051112403433,6.87120902944475,
38.0227803382964));
#219978=CARTESIAN_POINT('Ctrl Pts',(-4.08814516039471,6.77556194586727,
38.0305096978063));
#219979=CARTESIAN_POINT('Ctrl Pts',(-4.25231165492579,6.67375668066268,
38.0382390573162));
#219980=CARTESIAN_POINT('Ctrl Pts',(-4.41252782819546,6.5660885742884,38.0459684168261));
#219981=CARTESIAN_POINT('Ctrl Pts',(-4.57275203207569,6.45841507120158,
38.0536981637593));
#219982=CARTESIAN_POINT('Ctrl Pts',(-4.72902522157414,6.34487834135559,
38.0614279106924));
#219983=CARTESIAN_POINT('Ctrl Pts',(-4.88089386772019,6.22581689837176,
38.0691576576256));
#219984=CARTESIAN_POINT('Ctrl Pts',(-5.03279795397306,6.1067276711786,38.0768892083745));
#219985=CARTESIAN_POINT('Ctrl Pts',(-5.18029516725317,5.98211138501453,
38.0846207591234));
#219986=CARTESIAN_POINT('Ctrl Pts',(-5.32296528397476,5.85234667339517,
38.0923523098723));
#219987=CARTESIAN_POINT('Ctrl Pts',(-5.46569484505672,5.72252789452993,
38.1000870820183));
#219988=CARTESIAN_POINT('Ctrl Pts',(-5.60359303920781,5.58755666010915,
38.1078218541642));
#219989=CARTESIAN_POINT('Ctrl Pts',(-5.73627667674065,5.44784828054905,
38.1155566263102));
#219990=CARTESIAN_POINT('Ctrl Pts',(-5.86911853957823,5.3079732986758,38.1233006221758));
#219991=CARTESIAN_POINT('Ctrl Pts',(-5.99673317963242,5.16335015029389,
38.1310446180414));
#219992=CARTESIAN_POINT('Ctrl Pts',(-6.11877720864985,5.01442783086038,
38.1387886139071));
#219993=CARTESIAN_POINT('Ctrl Pts',(-6.2409004503644,4.86540885337093,38.1465376360145));
#219994=CARTESIAN_POINT('Ctrl Pts',(-6.35744566258698,4.71208543132804,
38.1542866581219));
#219995=CARTESIAN_POINT('Ctrl Pts',(-6.46811304319438,4.55493519827217,
38.1620356802293));
#219996=CARTESIAN_POINT('Ctrl Pts',(-6.57894954962902,4.39754480264065,
38.169796544668));
#219997=CARTESIAN_POINT('Ctrl Pts',(-6.68389008910803,4.23631621542687,
38.1775574091066));
#219998=CARTESIAN_POINT('Ctrl Pts',(-6.78268043334072,4.07175234256418,
38.1853182735452));
#219999=CARTESIAN_POINT('Ctrl Pts',(-6.85061767787057,3.95858322509337,
38.1906553512649));
#220000=CARTESIAN_POINT('Ctrl Pts',(-6.9156473584285,3.84383726930316,38.1959924289847));
#220001=CARTESIAN_POINT('Ctrl Pts',(-6.97770016626062,3.72768311284188,
38.2013295067044));
#220002=CARTESIAN_POINT('Ctrl Pts',(-7.07871441134965,3.53859860822715,
38.2100176047241));
#220003=CARTESIAN_POINT('Ctrl Pts',(-7.17210872623232,3.34527559886758,
38.2187057027438));
#220004=CARTESIAN_POINT('Ctrl Pts',(-7.25754798714799,3.14831990341581,
38.2273938007634));
#220005=CARTESIAN_POINT('Ctrl Pts',(-7.34282980133001,2.95172715622213,
38.2360658884309));
#220006=CARTESIAN_POINT('Ctrl Pts',(-7.42018572299943,2.75151529464273,
38.2447379760985));
#220007=CARTESIAN_POINT('Ctrl Pts',(-7.48932709473185,2.54831329865765,
38.253410063766));
#220008=CARTESIAN_POINT('Ctrl Pts',(-7.55859694649434,2.3447337082179,38.2620982660991));
#220009=CARTESIAN_POINT('Ctrl Pts',(-7.61962154043449,2.13815305182341,
38.2707864684322));
#220010=CARTESIAN_POINT('Ctrl Pts',(-7.67215758315153,1.929227570633,38.2794746707653));
#220011=CARTESIAN_POINT('Ctrl Pts',(-7.72432902666704,1.72175202856402,
38.2881025771289));
#220012=CARTESIAN_POINT('Ctrl Pts',(-7.76812926263982,1.51196432347098,
38.2967304834924));
#220013=CARTESIAN_POINT('Ctrl Pts',(-7.80336783994071,1.30052733711331,
38.3053583898559));
#220014=CARTESIAN_POINT('Ctrl Pts',(-7.83897581349406,1.08687391534949,
38.3140767401738));
#220015=CARTESIAN_POINT('Ctrl Pts',(-7.86584148296301,0.87153664402298,
38.3227950904917));
#220016=CARTESIAN_POINT('Ctrl Pts',(-7.88381960402942,0.655217102280911,
38.3315134408096));
#220017=CARTESIAN_POINT('Ctrl Pts',(-7.90179772509583,0.438897560538843,
38.3402317911275));
#220018=CARTESIAN_POINT('Ctrl Pts',(-7.91088819026632,0.221595984180793,
38.3489501414454));
#220019=CARTESIAN_POINT('Ctrl Pts',(-7.91099897442464,0.00402823191254809,
38.3576684917633));
#220020=CARTESIAN_POINT('',(-7.92439853970512,0.00241054887052533,42.3578451112103));
#220021=CARTESIAN_POINT('Ctrl Pts',(-7.91099999125534,0.000371964958585618,
38.3666382661385));
#220022=CARTESIAN_POINT('Ctrl Pts',(-7.91100271520357,-0.0575613265987164,
38.3690406849655));
#220023=CARTESIAN_POINT('Ctrl Pts',(-7.9103690600493,-0.115493823804628,
38.3714232920843));
#220024=CARTESIAN_POINT('Ctrl Pts',(-7.90838440824614,-0.206009619986472,
38.3751157245008));
#220025=CARTESIAN_POINT('Ctrl Pts',(-7.90746825211672,-0.238599637850203,
38.3764390523976));
#220026=CARTESIAN_POINT('Ctrl Pts',(-7.90596219549245,-0.282508723941569,
38.3782138863615));
#220027=CARTESIAN_POINT('Ctrl Pts',(-7.90554940551862,-0.293833309801218,
38.3786709066768));
#220028=CARTESIAN_POINT('Ctrl Pts',(-7.90480709229007,-0.313062983095493,
38.3794457228368));
#220029=CARTESIAN_POINT('Ctrl Pts',(-7.90449004101174,-0.320968518269954,
38.379763906663));
#220030=CARTESIAN_POINT('Ctrl Pts',(-7.90388018161711,-0.335625904036209,
38.3803531916325));
#220031=CARTESIAN_POINT('Ctrl Pts',(-7.90359058040864,-0.342377876603587,
38.3806243923135));
#220032=CARTESIAN_POINT('Ctrl Pts',(-7.90299231014186,-0.355921003355959,
38.3811678576104));
#220033=CARTESIAN_POINT('Ctrl Pts',(-7.90268353872469,-0.362712147380527,
38.3814401188041));
#220034=CARTESIAN_POINT('Ctrl Pts',(-7.90194822328956,-0.378437955671679,
38.3820699835571));
#220035=CARTESIAN_POINT('Ctrl Pts',(-7.90151527853552,-0.387372319072966,
38.3824273878951));
#220036=CARTESIAN_POINT('Ctrl Pts',(-7.90038089752371,-0.409988231430878,
38.3833309855707));
#220037=CARTESIAN_POINT('Ctrl Pts',(-7.89965907279563,-0.423668752526804,
38.3838765454769));
#220038=CARTESIAN_POINT('Ctrl Pts',(-7.89555229742595,-0.497840948260592,
38.3868288902424));
#220039=CARTESIAN_POINT('Ctrl Pts',(-7.8915080159501,-0.558294839597717,
38.3892151939417));
#220040=CARTESIAN_POINT('Ctrl Pts',(-7.88350108713109,-0.6603622260029,
38.393212241086));
#220041=CARTESIAN_POINT('Ctrl Pts',(-7.87990242229589,-0.702001096365646,
38.3948338789408));
#220042=CARTESIAN_POINT('Ctrl Pts',(-7.78940110074119,-1.66054947662174,
38.4319683124899));
#220043=CARTESIAN_POINT('Ctrl Pts',(-7.54340726935622,-2.55517792037413,
38.4615223651022));
#220044=CARTESIAN_POINT('Ctrl Pts',(-7.11896055711377,-3.45098212916863,
38.4975134515376));
#220045=CARTESIAN_POINT('Ctrl Pts',(-7.08796926483968,-3.51419528037316,
38.5000954516352));
#220046=CARTESIAN_POINT('Ctrl Pts',(-6.98097220032684,-3.72526300089221,
38.5088835234331));
#220047=CARTESIAN_POINT('Ctrl Pts',(-6.90116232317098,-3.87111269627868,
38.515250026745));
#220048=CARTESIAN_POINT('Ctrl Pts',(-6.80002871001735,-4.0428484989135,
38.523151571807));
#220049=CARTESIAN_POINT('Ctrl Pts',(-6.78307074601405,-4.07123637943482,
38.5244703690638));
#220050=CARTESIAN_POINT('Ctrl Pts',(-6.76017316436285,-4.10902706686521,
38.5262422827698));
#220051=CARTESIAN_POINT('Ctrl Pts',(-6.7543908401765,-4.11852510312975,
38.5266890071502));
#220052=CARTESIAN_POINT('Ctrl Pts',(-6.74481490552963,-4.13418011093671,
38.5274275699904));
#220053=CARTESIAN_POINT('Ctrl Pts',(-6.741032833677,-4.14034414444287,38.5277189519936));
#220054=CARTESIAN_POINT('Ctrl Pts',(-6.73365166125648,-4.1523370810343,
38.5282869916163));
#220055=CARTESIAN_POINT('Ctrl Pts',(-6.73005343015131,-4.15816651382083,
38.528563615347));
#220056=CARTESIAN_POINT('Ctrl Pts',(-6.72167408808717,-4.17170237453172,
38.5292071201259));
#220057=CARTESIAN_POINT('Ctrl Pts',(-6.71688729251227,-4.17940526236564,
38.5295742180452));
#220058=CARTESIAN_POINT('Ctrl Pts',(-6.70128749956797,-4.20441234950533,
38.530768869808));
#220059=CARTESIAN_POINT('Ctrl Pts',(-6.690420837446,-4.22168288320633,38.5315984245083));
#220060=CARTESIAN_POINT('Ctrl Pts',(-6.57057832438846,-4.41052538393717,
38.5407172316674));
#220061=CARTESIAN_POINT('Ctrl Pts',(-6.4550989127875,-4.57787355432885,
38.5492327207875));
#220062=CARTESIAN_POINT('Ctrl Pts',(-6.04559034718836,-5.12496746765744,
38.5782338796753));
#220063=CARTESIAN_POINT('Ctrl Pts',(-5.72347520198491,-5.48236237008008,
38.5990891690844));
#220064=CARTESIAN_POINT('Ctrl Pts',(-4.87310576715638,-6.26869387387898,
38.6484651614694));
#220065=CARTESIAN_POINT('Ctrl Pts',(-4.31813371183424,-6.66314139238969,
38.6764608749002));
#220066=CARTESIAN_POINT('Ctrl Pts',(-3.6565655008636,-7.01559423391413,
38.7069170972005));
#220067=CARTESIAN_POINT('Ctrl Pts',(-3.59300596085827,-7.04835739684581,
38.7098130697934));
#220068=CARTESIAN_POINT('Ctrl Pts',(-3.50316297181426,-7.09313782991565,
38.7138647255688));
#220069=CARTESIAN_POINT('Ctrl Pts',(-3.47724487160706,-7.10587948053701,
38.715028728308));
#220070=CARTESIAN_POINT('Ctrl Pts',(-3.432733747905,-7.12745984222853,38.7170195510794));
#220071=CARTESIAN_POINT('Ctrl Pts',(-3.41417496050453,-7.13636841317174,
38.7178471910449));
#220072=CARTESIAN_POINT('Ctrl Pts',(-3.37877152905703,-7.15319301776245,
38.719421435893));
#220073=CARTESIAN_POINT('Ctrl Pts',(-3.3619333131652,-7.16112224409712,
38.7201681945741));
#220074=CARTESIAN_POINT('Ctrl Pts',(-3.32264080803551,-7.17945621241007,
38.721906228771));
#220075=CARTESIAN_POINT('Ctrl Pts',(-3.30016534542252,-7.18981516751878,
38.7228969428637));
#220076=CARTESIAN_POINT('Ctrl Pts',(-3.26052548909528,-7.20786016832306,
38.7246382596247));
#220077=CARTESIAN_POINT('Ctrl Pts',(-3.24338162372294,-7.21559078082115,
38.7253893981968));
#220078=CARTESIAN_POINT('Ctrl Pts',(-3.12052734476668,-7.27046264375817,
38.7307581977238));
#220079=CARTESIAN_POINT('Ctrl Pts',(-3.01382024168068,-7.31534045871677,
38.7353475410548));
#220080=CARTESIAN_POINT('Ctrl Pts',(-2.23422058661147,-7.6232622653596,
38.7683875594053));
#220081=CARTESIAN_POINT('Ctrl Pts',(-1.52911817523031,-7.79535729482972,
38.7953257885712));
#220082=CARTESIAN_POINT('Ctrl Pts',(-0.720756914736055,-7.87861481531954,
38.8273359660099));
#220083=CARTESIAN_POINT('Ctrl Pts',(-0.630854176453375,-7.88632262198436,
38.830916309755));
#220084=CARTESIAN_POINT('Ctrl Pts',(-0.521912899122263,-7.89378792888539,
38.8352930736138));
#220085=CARTESIAN_POINT('Ctrl Pts',(-0.502980753681077,-7.89501686495704,
38.8360550966044));
#220086=CARTESIAN_POINT('Ctrl Pts',(-0.472764132041824,-7.89686917682917,
38.8372736385121));
#220087=CARTESIAN_POINT('Ctrl Pts',(-0.461482510633819,-7.8975364900623,
38.8377290975011));
#220088=CARTESIAN_POINT('Ctrl Pts',(-0.440053325420325,-7.89875796252408,
38.8385951670821));
#220089=CARTESIAN_POINT('Ctrl Pts',(-0.429906042740363,-7.89931674725418,
38.8390056720697));
#220090=CARTESIAN_POINT('Ctrl Pts',(-0.406840797752764,-7.90054231578217,
38.8399396514505));
#220091=CARTESIAN_POINT('Ctrl Pts',(-0.393922229818125,-7.90119697220654,
38.8404633910863));
#220092=CARTESIAN_POINT('Ctrl Pts',(-0.360495683730597,-7.90280870036098,
38.8418201318137));
#220093=CARTESIAN_POINT('Ctrl Pts',(-0.339985519612715,-7.90371762738879,
38.8426541459414));
#220094=CARTESIAN_POINT('Ctrl Pts',(-0.212138288763526,-7.9088847327349,
38.8478619099687));
#220095=CARTESIAN_POINT('Ctrl Pts',(-0.104728643885638,-7.91103606682353,
38.8522768196841));
#220096=CARTESIAN_POINT('Ctrl Pts',(0.269888492743345,-7.91090869061913,
38.8677759941054));
#220097=CARTESIAN_POINT('Ctrl Pts',(0.536907991786122,-7.89728071512809,
38.878998287945));
#220098=CARTESIAN_POINT('Ctrl Pts',(1.17548499987085,-7.83214875715672,
38.9059645797674));
#220099=CARTESIAN_POINT('Ctrl Pts',(1.54508422159397,-7.76769239284312,
38.9216646679157));
#220100=CARTESIAN_POINT('Ctrl Pts',(2.08565917721932,-7.63329463885581,
38.9446156192098));
#220101=CARTESIAN_POINT('Ctrl Pts',(2.26102071893566,-7.58320173009643,
38.9520632859458));
#220102=CARTESIAN_POINT('Ctrl Pts',(2.47767115759562,-7.51313021395045,
38.9612838798034));
#220103=CARTESIAN_POINT('Ctrl Pts',(2.52072430977822,-7.49879516725812,
38.9631172610841));
#220104=CARTESIAN_POINT('Ctrl Pts',(2.58927957279897,-7.47531177522488,
38.9660388729488));
#220105=CARTESIAN_POINT('Ctrl Pts',(2.61486203976945,-7.46640150018851,
38.9671296217264));
#220106=CARTESIAN_POINT('Ctrl Pts',(2.66326573892189,-7.44926339170212,
38.9691945080094));
#220107=CARTESIAN_POINT('Ctrl Pts',(2.68609586863034,-7.44106164897747,
38.9701689080954));
#220108=CARTESIAN_POINT('Ctrl Pts',(2.73794074019937,-7.42216664331352,
38.9723829014106));
#220109=CARTESIAN_POINT('Ctrl Pts',(2.76693126057956,-7.41140800292276,
38.9736217986367));
#220110=CARTESIAN_POINT('Ctrl Pts',(2.85592775459304,-7.37778564684661,
38.9774281968979));
#220111=CARTESIAN_POINT('Ctrl Pts',(2.91571920133957,-7.35436101920162,
38.9799899307979));
#220112=CARTESIAN_POINT('Ctrl Pts',(3.0604552529429,-7.29561489774216,38.986205572551));
#220113=CARTESIAN_POINT('Ctrl Pts',(3.1450819346465,-7.25953461951917,38.9898520929798));
#220114=CARTESIAN_POINT('Ctrl Pts',(3.41976419997844,-7.13671998058995,
39.0017453460508));
#220115=CARTESIAN_POINT('Ctrl Pts',(3.60701978363886,-7.04393144972072,
39.0099542913002));
#220116=CARTESIAN_POINT('Ctrl Pts',(4.31233168883667,-6.65892784241672,
39.0412100602678));
#220117=CARTESIAN_POINT('Ctrl Pts',(4.8004908165499,-6.31607764594432,39.0633350943303));
#220118=CARTESIAN_POINT('Ctrl Pts',(5.46689748272606,-5.72576036371308,
39.0963879917825));
#220119=CARTESIAN_POINT('Ctrl Pts',(5.677001770324,-5.51751216030138,39.1073702202544));
#220120=CARTESIAN_POINT('Ctrl Pts',(5.97080660544676,-5.19171217778812,
39.1242178287143));
#220121=CARTESIAN_POINT('Ctrl Pts',(6.06375507665267,-5.08284159513783,
39.1297998753315));
#220122=CARTESIAN_POINT('Ctrl Pts',(6.16368103374691,-4.9591541183792,39.1361541653297));
#220123=CARTESIAN_POINT('Ctrl Pts',(6.17362877195611,-4.94676472427187,
39.1367907973691));
#220124=CARTESIAN_POINT('Ctrl Pts',(6.18839703962758,-4.92825767805735,
39.1377421230619));
#220125=CARTESIAN_POINT('Ctrl Pts',(6.19324600090646,-4.92216269876513,
39.138055480075));
#220126=CARTESIAN_POINT('Ctrl Pts',(6.20152423659714,-4.91172563937437,
39.1385921830369));
#220127=CARTESIAN_POINT('Ctrl Pts',(6.20495797692332,-4.90738709681956,
39.138815315389));
#220128=CARTESIAN_POINT('Ctrl Pts',(6.21197910980657,-4.89849672123536,
39.1392726230588));
#220129=CARTESIAN_POINT('Ctrl Pts',(6.21556605670109,-4.89394454230649,
39.1395068196496));
#220130=CARTESIAN_POINT('Ctrl Pts',(6.22412194577437,-4.88306172105563,
39.1400668133257));
#220131=CARTESIAN_POINT('Ctrl Pts',(6.22908623061827,-4.87672743737101,
39.1403928380221));
#220132=CARTESIAN_POINT('Ctrl Pts',(6.24406681195771,-4.8575524554928,39.1413800576716));
#220133=CARTESIAN_POINT('Ctrl Pts',(6.25405309401799,-4.84468844219225,
39.1420427453491));
#220134=CARTESIAN_POINT('Ctrl Pts',(6.39114836767435,-4.66695636702513,
39.1512051820283));
#220135=CARTESIAN_POINT('Ctrl Pts',(6.51171854436379,-4.49719444148638,
39.1600827168072));
#220136=CARTESIAN_POINT('Ctrl Pts',(7.05173089917422,-3.6695488224066,39.2035578025975));
#220137=CARTESIAN_POINT('Ctrl Pts',(7.379054417748,-2.95672873120676,39.2409017257229));
#220138=CARTESIAN_POINT('Ctrl Pts',(7.68024011589105,-1.9202371514314,39.2884241153686));
#220139=CARTESIAN_POINT('Ctrl Pts',(7.74735464126035,-1.62847140738848,
39.301174309276));
#220140=CARTESIAN_POINT('Ctrl Pts',(7.80310647979635,-1.30247694968702,
39.314709516951));
#220141=CARTESIAN_POINT('Ctrl Pts',(7.80824025664181,-1.27133829603604,
39.3159954471475));
#220142=CARTESIAN_POINT('Ctrl Pts',(7.81572572646455,-1.2241791143627,39.3179325925056));
#220143=CARTESIAN_POINT('Ctrl Pts',(7.81821476286821,-1.20818088915252,
39.3185879432793));
#220144=CARTESIAN_POINT('Ctrl Pts',(7.82217286480417,-1.18221578633447,
39.319648669934));
#220145=CARTESIAN_POINT('Ctrl Pts',(7.82367202981318,-1.17225358314323,
39.3200549525274));
#220146=CARTESIAN_POINT('Ctrl Pts',(7.82651310842613,-1.15312591211613,
39.3208337000043));
#220147=CARTESIAN_POINT('Ctrl Pts',(7.82785796130529,-1.14396090139137,
39.321206252941));
#220148=CARTESIAN_POINT('Ctrl Pts',(7.83024356812774,-1.12750208245547,
39.3218742526899));
#220149=CARTESIAN_POINT('Ctrl Pts',(7.83129023488242,-1.12020914990784,
39.3221698772805));
#220150=CARTESIAN_POINT('Ctrl Pts',(7.83335681930409,-1.10566521083275,
39.3227586973428));
#220151=CARTESIAN_POINT('Ctrl Pts',(7.83437686073325,-1.098414230298,39.3230518962471));
#220152=CARTESIAN_POINT('Ctrl Pts',(7.83684417182053,-1.08069702626316,
39.323767425465));
#220153=CARTESIAN_POINT('Ctrl Pts',(7.83828054565859,-1.07022928600295,
39.3241894275831));
#220154=CARTESIAN_POINT('Ctrl Pts',(7.84367300623051,-1.03033789156443,
39.3257947926687));
#220155=CARTESIAN_POINT('Ctrl Pts',(7.84748444372987,-1.00089476382841,
39.3269738031868));
#220156=CARTESIAN_POINT('Ctrl Pts',(7.90924919453521,-0.501710311019217,
39.3468651678445));
#220157=CARTESIAN_POINT('Ctrl Pts',(7.92510132197997,-0.027706405577548,
39.3642113656409));
#220158=CARTESIAN_POINT('Ctrl Pts',(7.86938845878505,0.961356924089496,
39.3991103625044));
#220159=CARTESIAN_POINT('Ctrl Pts',(7.78971844561418,1.4736817027025,39.4164568344321));
#220160=CARTESIAN_POINT('Ctrl Pts',(7.64562512745606,2.03271899099538,39.4370736695871));
#220161=CARTESIAN_POINT('Ctrl Pts',(7.6299685321875,2.09072000372798,39.4392345089688));
#220162=CARTESIAN_POINT('Ctrl Pts',(7.55235467016894,2.36575607206893,39.4496049411629));
#220163=CARTESIAN_POINT('Ctrl Pts',(7.48179207598633,2.58023984417568,39.4580605834728));
#220164=CARTESIAN_POINT('Ctrl Pts',(7.3904863048398,2.82236216501128,39.4682943514352));
#220165=CARTESIAN_POINT('Ctrl Pts',(7.37861624582227,2.85325046568614,39.4696131354601));
#220166=CARTESIAN_POINT('Ctrl Pts',(7.36313698551467,2.89278802037589,39.4713174113298));
#220167=CARTESIAN_POINT('Ctrl Pts',(7.35970550930436,2.90150712793873,39.4716942651444));
#220168=CARTESIAN_POINT('Ctrl Pts',(7.35416030718162,2.91552391681494,39.4723017025418));
#220169=CARTESIAN_POINT('Ctrl Pts',(7.35205632132558,2.92082546227149,39.4725318234672));
#220170=CARTESIAN_POINT('Ctrl Pts',(7.34804438438703,2.93090279155142,39.4729699432471));
#220171=CARTESIAN_POINT('Ctrl Pts',(7.34613750542787,2.93567900145971,39.4731778918163));
#220172=CARTESIAN_POINT('Ctrl Pts',(7.34178859231193,2.94654106827947,39.4736514840893));
#220173=CARTESIAN_POINT('Ctrl Pts',(7.33934364775402,2.95262575025401,39.4739172623778));
#220174=CARTESIAN_POINT('Ctrl Pts',(7.33206199778297,2.97068251169752,39.4747073987852));
#220175=CARTESIAN_POINT('Ctrl Pts',(7.32720355836226,2.98264576109962,39.4752327462041));
#220176=CARTESIAN_POINT('Ctrl Pts',(7.29357638235363,3.06487011503149,39.478856003977));
#220177=CARTESIAN_POINT('Ctrl Pts',(7.2638273512309,3.13472438617163,39.4819970277138));
#220178=CARTESIAN_POINT('Ctrl Pts',(7.22201098502701,3.22912139496021,39.4863174093829));
#220179=CARTESIAN_POINT('Ctrl Pts',(7.21081446849818,3.2540470696945,39.4874654820911));
#220180=CARTESIAN_POINT('Ctrl Pts',(7.18864687072568,3.30272031208883,39.4897209708892));
#220181=CARTESIAN_POINT('Ctrl Pts',(7.17768667474293,3.32647249719887,39.4908280191946));
#220182=CARTESIAN_POINT('Ctrl Pts',(7.15174932842089,3.38195709427862,39.4934283779987));
#220183=CARTESIAN_POINT('Ctrl Pts',(7.13667849656462,3.41364500864425,39.494924501378));
#220184=CARTESIAN_POINT('Ctrl Pts',(7.11700818813409,3.45430413118417,39.4968575736647));
#220185=CARTESIAN_POINT('Ctrl Pts',(7.1126015894661,3.46336847727902,39.4972893838175));
#220186=CARTESIAN_POINT('Ctrl Pts',(7.05330795713899,3.58474467753427,39.503082877715));
#220187=CARTESIAN_POINT('Ctrl Pts',(6.99578455521396,3.69574686964681,39.5085110742401));
#220188=CARTESIAN_POINT('Ctrl Pts',(6.78731004033436,4.07571518047886,39.5274538392275));
#220189=CARTESIAN_POINT('Ctrl Pts',(6.6232802705237,4.33718713788831,39.5411189842109));
#220190=CARTESIAN_POINT('Ctrl Pts',(6.14315761159606,5.01151661952922,39.5773561037032));
#220191=CARTESIAN_POINT('Ctrl Pts',(5.8009572889213,5.40394872300416,39.5994473775974));
#220192=CARTESIAN_POINT('Ctrl Pts',(5.39233664908235,5.78864138728636,39.6222005742356));
#220193=CARTESIAN_POINT('Ctrl Pts',(5.36171576013608,5.81701536834967,39.6238869032296));
#220194=CARTESIAN_POINT('Ctrl Pts',(5.31767323420031,5.85718289459712,39.6262864342426));
#220195=CARTESIAN_POINT('Ctrl Pts',(5.30443416596084,5.8691752630627,39.627004425174));
#220196=CARTESIAN_POINT('Ctrl Pts',(5.28147865477692,5.88982797914241,39.6282437393928));
#220197=CARTESIAN_POINT('Ctrl Pts',(5.27178126336351,5.89850936399747,39.628765556259));
#220198=CARTESIAN_POINT('Ctrl Pts',(5.25314535711491,5.91511009771673,39.6297650880353));
#220199=CARTESIAN_POINT('Ctrl Pts',(5.24421025113421,5.92303321397659,39.630242888993));
#220200=CARTESIAN_POINT('Ctrl Pts',(5.22316430207539,5.94161054399292,39.6313649834139));
#220201=CARTESIAN_POINT('Ctrl Pts',(5.21103873587482,5.95224801888364,39.6320088967503));
#220202=CARTESIAN_POINT('Ctrl Pts',(5.16947504556207,5.98848651671236,39.6342074015884));
#220203=CARTESIAN_POINT('Ctrl Pts',(5.13987995853597,6.0139069702918,39.6357580517973));
#220204=CARTESIAN_POINT('Ctrl Pts',(4.84207088466704,6.26590340091852,39.6512180939256));
#220205=CARTESIAN_POINT('Ctrl Pts',(4.55923559092939,6.47461083434499,39.6647163939174));
#220206=CARTESIAN_POINT('Ctrl Pts',(3.9335669978444,6.8749070762322,39.6926293775717));
#220207=CARTESIAN_POINT('Ctrl Pts',(3.58845862270875,7.0611801730281,39.7069267604959));
#220208=CARTESIAN_POINT('Ctrl Pts',(2.8740147650569,7.38084607139559,39.7357542371441));
#220209=CARTESIAN_POINT('Ctrl Pts',(2.50572392121636,7.51386460852727,39.7502518971484));
#220210=CARTESIAN_POINT('Ctrl Pts',(2.08442051882942,7.63159667229031,39.7675485415777));
#220211=CARTESIAN_POINT('Ctrl Pts',(2.03959589143796,7.6436983954947,39.7693978818927));
#220212=CARTESIAN_POINT('Ctrl Pts',(1.98353662064013,7.6583050208189,39.771724332625));
#220213=CARTESIAN_POINT('Ctrl Pts',(1.97239906432514,7.66118106081746,39.7721872070834));
#220214=CARTESIAN_POINT('Ctrl Pts',(1.95476535337692,7.66569359491175,39.7729211614091));
#220215=CARTESIAN_POINT('Ctrl Pts',(1.94827330074194,7.66734615255485,39.7731916109767));
#220216=CARTESIAN_POINT('Ctrl Pts',(1.93610291201317,7.6704276803579,39.7736990643508));
#220217=CARTESIAN_POINT('Ctrl Pts',(1.93042507035832,7.67185859704151,39.773935990572));
#220218=CARTESIAN_POINT('Ctrl Pts',(1.91773826393014,7.67504092133412,39.774465808676));
#220219=CARTESIAN_POINT('Ctrl Pts',(1.91072848345521,7.67678903286731,39.7747588328634));
#220220=CARTESIAN_POINT('Ctrl Pts',(1.89305550956257,7.68117064495437,39.7754983412253));
#220221=CARTESIAN_POINT('Ctrl Pts',(1.88238922872612,7.68379153993196,39.7759453391509));
#220222=CARTESIAN_POINT('Ctrl Pts',(1.82561207215154,7.69761737991473,39.7783284695209));
#220223=CARTESIAN_POINT('Ctrl Pts',(1.77940722168193,7.70842931880425,39.7802809489069));
#220224=CARTESIAN_POINT('Ctrl Pts',(0.948814859251304,7.89492232092405,
39.8156503759892));
#220225=CARTESIAN_POINT('Ctrl Pts',(0.142344382455355,7.95044911474386,
39.8544822232692));
#220226=CARTESIAN_POINT('Ctrl Pts',(-1.0248819715523,7.85293830026884,39.9069327330826));
#220227=CARTESIAN_POINT('Ctrl Pts',(-1.38861581272634,7.79684655180978,
39.9228169576492));
#220228=CARTESIAN_POINT('Ctrl Pts',(-1.79734250557897,7.7042928213546,39.939975799354));
#220229=CARTESIAN_POINT('Ctrl Pts',(-1.84740927995367,7.69244090304661,
39.94206624299));
#220230=CARTESIAN_POINT('Ctrl Pts',(-1.91025195217123,7.67691571485802,
39.9446759829438));
#220231=CARTESIAN_POINT('Ctrl Pts',(-1.92313837206761,7.67369768872882,
39.9452103822742));
#220232=CARTESIAN_POINT('Ctrl Pts',(-1.94361219817025,7.66853010625162,
39.9460582464532));
#220233=CARTESIAN_POINT('Ctrl Pts',(-1.95120489009336,7.66660171423512,
39.9463724164409));
#220234=CARTESIAN_POINT('Ctrl Pts',(-1.96548643812819,7.66295189631464,
39.9469628715697));
#220235=CARTESIAN_POINT('Ctrl Pts',(-1.97217592523177,7.66123298327091,
39.9472392403276));
#220236=CARTESIAN_POINT('Ctrl Pts',(-1.9871886150494,7.65735439611999,39.9478590238896));
#220237=CARTESIAN_POINT('Ctrl Pts',(-1.99551057103304,7.65518990627137,
39.9482022771631));
#220238=CARTESIAN_POINT('Ctrl Pts',(-2.01662415088057,7.64966162480336,
39.9490723596271));
#220239=CARTESIAN_POINT('Ctrl Pts',(-2.02941092152446,7.64627930785708,
39.9495985671355));
#220240=CARTESIAN_POINT('Ctrl Pts',(-2.09949205655606,7.62755348477661,
39.9524786103381));
#220241=CARTESIAN_POINT('Ctrl Pts',(-2.1566216854424,7.61159787202896,39.9548118121544));
#220242=CARTESIAN_POINT('Ctrl Pts',(-3.18384901983735,7.31221188895279,
39.996514440083));
#220243=CARTESIAN_POINT('Ctrl Pts',(-4.09073894759682,6.84622257074285,
40.0277405781552));
#220244=CARTESIAN_POINT('Ctrl Pts',(-5.11674070738103,6.04064065632391,
40.073635032168));
#220245=CARTESIAN_POINT('Ctrl Pts',(-5.33768091836027,5.84632416592615,
40.0844259993587));
#220246=CARTESIAN_POINT('Ctrl Pts',(-5.55791189271404,5.62972104465172,
40.0967720866748));
#220247=CARTESIAN_POINT('Ctrl Pts',(-5.56852046932466,5.61922800965859,
40.0973709143779));
#220248=CARTESIAN_POINT('Ctrl Pts',(-5.58312226727767,5.60470328812776,
40.0982009465838));
#220249=CARTESIAN_POINT('Ctrl Pts',(-5.58714099214233,5.60069716489918,
40.0984299981913));
#220250=CARTESIAN_POINT('Ctrl Pts',(-5.59390839776516,5.59393644766466,
40.0988167487078));
#220251=CARTESIAN_POINT('Ctrl Pts',(-5.59665936807869,5.59118413761223,
40.0989742529439));
#220252=CARTESIAN_POINT('Ctrl Pts',(-5.60209085489987,5.58574198060863,
40.0992858017266));
#220253=CARTESIAN_POINT('Ctrl Pts',(-5.60477146783886,5.58305223096501,
40.0994398379317));
#220254=CARTESIAN_POINT('Ctrl Pts',(-5.61067328222019,5.5771217665209,40.0997795874119));
#220255=CARTESIAN_POINT('Ctrl Pts',(-5.61389359422322,5.57388020959251,
40.0999653748072));
#220256=CARTESIAN_POINT('Ctrl Pts',(-5.62497167677132,5.5627097037452,40.1006058853756));
#220257=CARTESIAN_POINT('Ctrl Pts',(-5.63281542718606,5.55476695940392,
40.1010618029628));
#220258=CARTESIAN_POINT('Ctrl Pts',(-5.71360813305525,5.4726074939307,40.1057824964462));
#220259=CARTESIAN_POINT('Ctrl Pts',(-5.78509965841184,5.39697792538076,
40.1101673970241));
#220260=CARTESIAN_POINT('Ctrl Pts',(-5.87744926672617,5.29533927831622,
40.116080981103));
#220261=CARTESIAN_POINT('Ctrl Pts',(-5.89966736616873,5.27057424480898,
40.1175234538636));
#220262=CARTESIAN_POINT('Ctrl Pts',(-6.0374092888227,5.11508024181091,40.1265856923867));
#220263=CARTESIAN_POINT('Ctrl Pts',(-6.14873376321625,4.9807051936094,40.1344392800865));
#220264=CARTESIAN_POINT('Ctrl Pts',(-6.60146831300707,4.39589701321909,
40.1682930351166));
#220265=CARTESIAN_POINT('Ctrl Pts',(-6.89854733621004,3.9132363277899,40.1952973119054));
#220266=CARTESIAN_POINT('Ctrl Pts',(-7.22288530682164,3.23256725133725,
40.2293079155267));
#220267=CARTESIAN_POINT('Ctrl Pts',(-7.29797212619905,3.05927643789607,
40.237661179588));
#220268=CARTESIAN_POINT('Ctrl Pts',(-7.42232802915468,2.74156616301702,
40.2523816933558));
#220269=CARTESIAN_POINT('Ctrl Pts',(-7.47375679305211,2.59809573945222,
40.2588185355707));
#220270=CARTESIAN_POINT('Ctrl Pts',(-7.54530838423873,2.37873520591927,
40.2683427038426));
#220271=CARTESIAN_POINT('Ctrl Pts',(-7.56849760516399,2.30388895001688,
40.2715376683309));
#220272=CARTESIAN_POINT('Ctrl Pts',(-7.59472275158966,2.21457093857108,
40.2752869711011));
#220273=CARTESIAN_POINT('Ctrl Pts',(-7.59883439912788,2.20042129906829,
40.2758790536387));
#220274=CARTESIAN_POINT('Ctrl Pts',(-7.60510337470772,2.17862040125772,
40.2767884269391));
#220275=CARTESIAN_POINT('Ctrl Pts',(-7.60728873148677,2.17097727972219,
40.2771066994569));
#220276=CARTESIAN_POINT('Ctrl Pts',(-7.61109214888292,2.15759885350793,
40.2776628543255));
#220277=CARTESIAN_POINT('Ctrl Pts',(-7.6127152544861,2.15186499710866,40.2779009130775));
#220278=CARTESIAN_POINT('Ctrl Pts',(-7.6163668019076,2.13890953636076,40.2784381154137));
#220279=CARTESIAN_POINT('Ctrl Pts',(-7.61839145592972,2.1316868650393,40.2787371264134));
#220280=CARTESIAN_POINT('Ctrl Pts',(-7.62381538778137,2.11223131565829,
40.2795412797663));
#220281=CARTESIAN_POINT('Ctrl Pts',(-7.62719550144084,2.09999309110522,
40.2800457527841));
#220282=CARTESIAN_POINT('Ctrl Pts',(-7.64192742605976,2.0461490934733,40.2822592882439));
#220283=CARTESIAN_POINT('Ctrl Pts',(-7.65296847740238,2.00445864551502,
40.2839575193772));
#220284=CARTESIAN_POINT('Ctrl Pts',(-7.82779901257981,1.32179844281649,
40.3115158432425));
#220285=CARTESIAN_POINT('Ctrl Pts',(-7.91089925752325,0.662823887569133,
40.3342043247919));
#220286=CARTESIAN_POINT('Ctrl Pts',(-7.91108201108098,-0.538491210849919,
40.37501585252));
#220287=CARTESIAN_POINT('Ctrl Pts',(-7.85593626646437,-1.07671278173625,
40.3932271424114));
#220288=CARTESIAN_POINT('Ctrl Pts',(-7.73952615419851,-1.63854383578707,
40.4158612029801));
#220289=CARTESIAN_POINT('Ctrl Pts',(-7.73236927171654,-1.67199173718399,
40.4172229274171));
#220290=CARTESIAN_POINT('Ctrl Pts',(-7.72340608793648,-1.7125927078554,
40.4188943852793));
#220291=CARTESIAN_POINT('Ctrl Pts',(-7.72180630492352,-1.71979149043264,
40.4191914537871));
#220292=CARTESIAN_POINT('Ctrl Pts',(-7.7191413648481,-1.73170463689244,
40.41968423049));
#220293=CARTESIAN_POINT('Ctrl Pts',(-7.7180819449022,-1.73642029804808,
40.4198795914765));
#220294=CARTESIAN_POINT('Ctrl Pts',(-7.71615850065117,-1.74494534322553,
40.4202333103217));
#220295=CARTESIAN_POINT('Ctrl Pts',(-7.71529597389651,-1.7487550694953,
40.420391578355));
#220296=CARTESIAN_POINT('Ctrl Pts',(-7.71344347478094,-1.75690939350378,
40.4207307518267));
#220297=CARTESIAN_POINT('Ctrl Pts',(-7.71245265305085,-1.76125379486147,
40.4209117078258));
#220298=CARTESIAN_POINT('Ctrl Pts',(-7.70975832953071,-1.77302157596164,
40.4214025504843));
#220299=CARTESIAN_POINT('Ctrl Pts',(-7.70804778081875,-1.78044332019545,
40.4217128533897));
#220300=CARTESIAN_POINT('Ctrl Pts',(-7.69950107351774,-1.8172826828606,
40.4232567250017));
#220301=CARTESIAN_POINT('Ctrl Pts',(-7.69250729438803,-1.84666310110749,
40.4244994697214));
#220302=CARTESIAN_POINT('Ctrl Pts',(-7.63154129672951,-2.09642011987007,
40.4351572841536));
#220303=CARTESIAN_POINT('Ctrl Pts',(-7.56828327969176,-2.31440545813413,
40.4450785239092));
#220304=CARTESIAN_POINT('Ctrl Pts',(-7.36903943095525,-2.90486563161531,
40.4731184376421));
#220305=CARTESIAN_POINT('Ctrl Pts',(-7.21429198763766,-3.27031549342397,
40.4917630167172));
#220306=CARTESIAN_POINT('Ctrl Pts',(-6.87031834605332,-3.93809295397977,
40.5267444415144));
#220307=CARTESIAN_POINT('Ctrl Pts',(-6.68676627239349,-4.24229146828261,
40.5430806355035));
#220308=CARTESIAN_POINT('Ctrl Pts',(-6.47723856000872,-4.5419618196085,
40.5592768463925));
#220309=CARTESIAN_POINT('Ctrl Pts',(-6.47106140393932,-4.55075827105341,
40.5597523856308));
#220310=CARTESIAN_POINT('Ctrl Pts',(-6.41199761958388,-4.63450340596798,
40.5642807770836));
#220311=CARTESIAN_POINT('Ctrl Pts',(-6.35782810761078,-4.70854093618355,
40.5682925432195));
#220312=CARTESIAN_POINT('Ctrl Pts',(-6.16060544065873,-4.96848887811672,
40.5824011250004));
#220313=CARTESIAN_POINT('Ctrl Pts',(-6.01058144986155,-5.14896730418382,
40.5922352962012));
#220314=CARTESIAN_POINT('Ctrl Pts',(-5.83751511302868,-5.33927438751271,
40.6026612032246));
#220315=CARTESIAN_POINT('Ctrl Pts',(-5.82220934662197,-5.35596041949393,
40.6035758852737));
#220316=CARTESIAN_POINT('Ctrl Pts',(-5.80057857059859,-5.37933955388652,
40.6048582889587));
#220317=CARTESIAN_POINT('Ctrl Pts',(-5.79431326239355,-5.38608759747377,
40.6052285332949));
#220318=CARTESIAN_POINT('Ctrl Pts',(-5.78340820776284,-5.39779182562199,
40.605870882739));
#220319=CARTESIAN_POINT('Ctrl Pts',(-5.77877384275295,-5.40275299870337,
40.6061432156969));
#220320=CARTESIAN_POINT('Ctrl Pts',(-5.76910639553429,-5.41307550959544,
40.6067099644696));
#220321=CARTESIAN_POINT('Ctrl Pts',(-5.76407221127928,-5.4184358092643,
40.6070043330004));
#220322=CARTESIAN_POINT('Ctrl Pts',(-5.75218089085048,-5.43106212575577,
40.6076978844572));
#220323=CARTESIAN_POINT('Ctrl Pts',(-5.74531744274403,-5.43832219511873,
40.6080967978567));
#220324=CARTESIAN_POINT('Ctrl Pts',(-5.72275241163505,-5.46210080786379,
40.6094037668562));
#220325=CARTESIAN_POINT('Ctrl Pts',(-5.70699313414145,-5.47856457276963,
40.6103093554362));
#220326=CARTESIAN_POINT('Ctrl Pts',(-5.448101584998,-5.74670008974927,40.6250700818318));
#220327=CARTESIAN_POINT('Ctrl Pts',(-5.1885959736697,-5.98204608301881,
40.6381746923237));
#220328=CARTESIAN_POINT('Ctrl Pts',(-4.72124973395091,-6.35251392425787,
40.6596742533094));
#220329=CARTESIAN_POINT('Ctrl Pts',(-4.52111215866887,-6.49647458446487,
40.6683096877142));
#220330=CARTESIAN_POINT('Ctrl Pts',(-4.1214291799933,-6.75654085336454,
40.6848810477597));
#220331=CARTESIAN_POINT('Ctrl Pts',(-3.92288210991624,-6.87371933955018,
40.6928191560776));
#220332=CARTESIAN_POINT('Ctrl Pts',(-3.66502063653614,-7.01108805613906,
40.7030323030737));
#220333=CARTESIAN_POINT('Ctrl Pts',(-3.61019872986792,-7.03947420186448,
40.7051985147615));
#220334=CARTESIAN_POINT('Ctrl Pts',(-3.22853913631383,-7.23146199755547,
40.72027477787));
#220335=CARTESIAN_POINT('Ctrl Pts',(-2.89103775692214,-7.37288417780481,
40.7336328639309));
#220336=CARTESIAN_POINT('Ctrl Pts',(-2.52002064136027,-7.49894062262285,
40.7492130867442));
#220337=CARTESIAN_POINT('Ctrl Pts',(-2.49504425864787,-7.50728770076862,
40.7502650204757));
#220338=CARTESIAN_POINT('Ctrl Pts',(-2.46106023124157,-7.51845679796498,
40.751700166845));
#220339=CARTESIAN_POINT('Ctrl Pts',(-2.45208837107114,-7.5213876847459,
40.752079411001));
#220340=CARTESIAN_POINT('Ctrl Pts',(-2.43686760089633,-7.5263298087165,
40.7527233926932));
#220341=CARTESIAN_POINT('Ctrl Pts',(-2.43062138174445,-7.52834934047339,
40.7529878357527));
#220342=CARTESIAN_POINT('Ctrl Pts',(-2.4185822937369,-7.53222528155159,
40.7534978468833));
#220343=CARTESIAN_POINT('Ctrl Pts',(-2.41278978197055,-7.53408278899374,
40.7537433764912));
#220344=CARTESIAN_POINT('Ctrl Pts',(-2.39911006385869,-7.5384521235378,
40.7543235515642));
#220345=CARTESIAN_POINT('Ctrl Pts',(-2.39122105327994,-7.54095825417148,
40.7546583915292));
#220346=CARTESIAN_POINT('Ctrl Pts',(-2.36818304438918,-7.54823703515138,
40.75563693857));
#220347=CARTESIAN_POINT('Ctrl Pts',(-2.35302362921683,-7.55297643760833,
40.7562817541365));
#220348=CARTESIAN_POINT('Ctrl Pts',(-2.24236509798363,-7.58720696817183,
40.7609949470691));
#220349=CARTESIAN_POINT('Ctrl Pts',(-2.1463307324269,-7.61493101660534,
40.7651191011544));
#220350=CARTESIAN_POINT('Ctrl Pts',(-1.818167507871,-7.70296711661536,40.7792826212084));
#220351=CARTESIAN_POINT('Ctrl Pts',(-1.58383502304826,-7.75454039850525,
40.7895113506033));
#220352=CARTESIAN_POINT('Ctrl Pts',(-0.814949133076653,-7.88745178877353,
40.8229963049838));
#220353=CARTESIAN_POINT('Ctrl Pts',(-0.274309553465448,-7.92469760869911,
40.8463010789948));
#220354=CARTESIAN_POINT('Ctrl Pts',(0.335384128893991,-7.90419331282219,
40.8719167344252));
#220355=CARTESIAN_POINT('Ctrl Pts',(0.404834304556967,-7.90094068605221,
40.8748272482128));
#220356=CARTESIAN_POINT('Ctrl Pts',(0.908082551452367,-7.87071860796951,
40.8958739064551));
#220357=CARTESIAN_POINT('Ctrl Pts',(1.33906373592302,-7.80895323040188,
40.9137387684529));
#220358=CARTESIAN_POINT('Ctrl Pts',(1.82125838895418,-7.6987360311632,40.9338064528476));
#220359=CARTESIAN_POINT('Ctrl Pts',(1.87957671003879,-7.68470624387322,
40.9362332491362));
#220360=CARTESIAN_POINT('Ctrl Pts',(1.9635703156367,-7.66348634430565,40.9397281815936));
#220361=CARTESIAN_POINT('Ctrl Pts',(1.98937742553456,-7.65682759363849,
40.9408019660878));
#220362=CARTESIAN_POINT('Ctrl Pts',(2.0347587269758,-7.64487338589867,40.9426901642683));
#220363=CARTESIAN_POINT('Ctrl Pts',(2.05434710700069,-7.63963285309747,
40.9435051758945));
#220364=CARTESIAN_POINT('Ctrl Pts',(2.09478505724481,-7.62864760357231,
40.945187676698));
#220365=CARTESIAN_POINT('Ctrl Pts',(2.11563166134352,-7.62289258565481,
40.9460550426494));
#220366=CARTESIAN_POINT('Ctrl Pts',(2.16907465960688,-7.60790272752859,
40.9482786988633));
#220367=CARTESIAN_POINT('Ctrl Pts',(2.20163585725308,-7.59854383126085,
40.9496335519723));
#220368=CARTESIAN_POINT('Ctrl Pts',(2.33813513322191,-7.55835949700753,
40.9553137690073));
#220369=CARTESIAN_POINT('Ctrl Pts',(2.44149476556681,-7.52560814285373,
40.9596161189062));
#220370=CARTESIAN_POINT('Ctrl Pts',(2.70817216971802,-7.43503405254023,
40.9707309891727));
#220371=CARTESIAN_POINT('Ctrl Pts',(2.8703225289261,-7.37395266505057,40.9775027729984));
#220372=CARTESIAN_POINT('Ctrl Pts',(3.47687404875542,-7.12242583750333,
41.0029992525202));
#220373=CARTESIAN_POINT('Ctrl Pts',(3.90548841926288,-6.89672025093036,
41.0213029038865));
#220374=CARTESIAN_POINT('Ctrl Pts',(4.44457424347299,-6.54638300702135,
41.046350561226));
#220375=CARTESIAN_POINT('Ctrl Pts',(4.57567577731252,-6.45542869991477,
41.0526238538909));
#220376=CARTESIAN_POINT('Ctrl Pts',(4.72234670403155,-6.34695887931542,
41.0599239047219));
#220377=CARTESIAN_POINT('Ctrl Pts',(4.7406993924828,-6.33326256174149,41.0608425597413));
#220378=CARTESIAN_POINT('Ctrl Pts',(4.76877484565758,-6.31211988471779,
41.0622561541049));
#220379=CARTESIAN_POINT('Ctrl Pts',(4.7785401904589,-6.30473033638202,41.0627493701661));
#220380=CARTESIAN_POINT('Ctrl Pts',(4.79633378708911,-6.29120062918059,
41.0636508375065));
#220381=CARTESIAN_POINT('Ctrl Pts',(4.80436751289362,-6.28506769686039,
41.0640588814064));
#220382=CARTESIAN_POINT('Ctrl Pts',(4.82173909713339,-6.27175349047567,
41.064943432507));
#220383=CARTESIAN_POINT('Ctrl Pts',(4.83107270920755,-6.26456672431373,
41.0654200922201));
#220384=CARTESIAN_POINT('Ctrl Pts',(4.85686294025399,-6.24461664969128,
41.0667410099732));
#220385=CARTESIAN_POINT('Ctrl Pts',(4.8732852286146,-6.23180919130501,41.0675864576568));
#220386=CARTESIAN_POINT('Ctrl Pts',(4.96433863619142,-6.16021819455948,
41.072297762244));
#220387=CARTESIAN_POINT('Ctrl Pts',(5.03795590015163,-6.10015952217814,
41.0761958344638));
#220388=CARTESIAN_POINT('Ctrl Pts',(5.44846570641175,-5.75275565522514,
41.0984012099495));
#220389=CARTESIAN_POINT('Ctrl Pts',(5.76184621752423,-5.43885116326933,
41.1171385065488));
#220390=CARTESIAN_POINT('Ctrl Pts',(6.22086327210754,-4.8946135113089,41.1469272337747));
#220391=CARTESIAN_POINT('Ctrl Pts',(6.38379933645567,-4.68011672686343,
41.1581022538579));
#220392=CARTESIAN_POINT('Ctrl Pts',(6.54772380283569,-4.43978666836273,
41.1700292862554));
#220393=CARTESIAN_POINT('Ctrl Pts',(6.55988748812866,-4.42179474932165,
41.1709187760289));
#220394=CARTESIAN_POINT('Ctrl Pts',(6.63678071393931,-4.30704251078201,
41.1765704304468));
#220395=CARTESIAN_POINT('Ctrl Pts',(6.69944242153006,-4.20891258887597,
41.181306346304));
#220396=CARTESIAN_POINT('Ctrl Pts',(6.78087228530435,-4.07496251945919,
41.1876480776934));
#220397=CARTESIAN_POINT('Ctrl Pts',(6.80156439396075,-4.04033046915947,
41.1892769066331));
#220398=CARTESIAN_POINT('Ctrl Pts',(6.83383169090829,-3.9853748036672,41.1918450406949));
#220399=CARTESIAN_POINT('Ctrl Pts',(6.84558316382334,-3.96515561566891,
41.192786396983));
#220400=CARTESIAN_POINT('Ctrl Pts',(6.86816602078005,-3.92590068287647,
41.1946073451946));
#220401=CARTESIAN_POINT('Ctrl Pts',(6.87900834942608,-3.90687148399961,
41.1954870556991));
#220402=CARTESIAN_POINT('Ctrl Pts',(6.9046779314019,-3.86138106009618,41.1975830073545));
#220403=CARTESIAN_POINT('Ctrl Pts',(6.91943231099754,-3.8348790762309,41.1987984191924));
#220404=CARTESIAN_POINT('Ctrl Pts',(6.96346256409352,-3.75471001293163,
41.2024584876864));
#220405=CARTESIAN_POINT('Ctrl Pts',(6.99226922471156,-3.70078766129468,
41.2048980064924));
#220406=CARTESIAN_POINT('Ctrl Pts',(7.19015650595692,-3.31980769766959,
41.221987628562));
#220407=CARTESIAN_POINT('Ctrl Pts',(7.33685605418884,-2.9816156434677,41.2364668014338));
#220408=CARTESIAN_POINT('Ctrl Pts',(7.63687285613083,-2.13211085690407,
41.271280868553));
#220409=CARTESIAN_POINT('Ctrl Pts',(7.76308427169009,-1.6131531459468,41.2910642235314));
#220410=CARTESIAN_POINT('Ctrl Pts',(7.89494829331881,-0.661183439387172,
41.3267458755949));
#220411=CARTESIAN_POINT('Ctrl Pts',(7.91915967737508,-0.232877693956832,
41.3426309331704));
#220412=CARTESIAN_POINT('Ctrl Pts',(7.90804139615672,0.21747848682177,41.3605743133562));
#220413=CARTESIAN_POINT('Ctrl Pts',(7.90739875941743,0.239709122353434,
41.3614633513774));
#220414=CARTESIAN_POINT('Ctrl Pts',(7.90636380494532,0.270949640312946,
41.3627176842484));
#220415=CARTESIAN_POINT('Ctrl Pts',(7.90604980584113,0.279962123280698,
41.3630801251431));
#220416=CARTESIAN_POINT('Ctrl Pts',(7.90549211774436,0.295219294359333,
41.3636947106507));
#220417=CARTESIAN_POINT('Ctrl Pts',(7.90525643759748,0.301464278188743,
41.3639465565419));
#220418=CARTESIAN_POINT('Ctrl Pts',(7.90477522771567,0.313826513213213,
41.3644456756055));
#220419=CARTESIAN_POINT('Ctrl Pts',(7.90452999637114,0.319943772097463,
41.3646929373109));
#220420=CARTESIAN_POINT('Ctrl Pts',(7.90392160733752,0.334692177593052,
41.3652897608273));
#220421=CARTESIAN_POINT('Ctrl Pts',(7.90355141283754,0.343323014875956,
41.3656395929061));
#220422=CARTESIAN_POINT('Ctrl Pts',(7.90225653096316,0.372399800166932,
41.3668201171148));
#220423=CARTESIAN_POINT('Ctrl Pts',(7.90126664086971,0.392842654933553,
41.3676533679189));
#220424=CARTESIAN_POINT('Ctrl Pts',(7.8852524735081,0.698966067963113,41.380182642444));
#220425=CARTESIAN_POINT('Ctrl Pts',(7.85482572920474,0.983572604281911,
41.3926097470657));
#220426=CARTESIAN_POINT('Ctrl Pts',(7.65043768365785,2.24443644992404,41.449891458383));
#220427=CARTESIAN_POINT('Ctrl Pts',(7.30918761736838,3.18486130846244,41.4971408822131));
#220428=CARTESIAN_POINT('Ctrl Pts',(6.77571982784173,4.08367421582991,41.540008583662));
#220429=CARTESIAN_POINT('Ctrl Pts',(6.74799159735284,4.12933212863205,41.5421832711266));
#220430=CARTESIAN_POINT('Ctrl Pts',(6.71204451494971,4.18719423577374,41.5449359569383));
#220431=CARTESIAN_POINT('Ctrl Pts',(6.7042514950107,4.1996605854889,41.5455288255349));
#220432=CARTESIAN_POINT('Ctrl Pts',(6.69181667839155,4.21942951282276,41.5464686900694));
#220433=CARTESIAN_POINT('Ctrl Pts',(6.68719759135799,4.22674629539127,41.5468164835685));
#220434=CARTESIAN_POINT('Ctrl Pts',(6.67856158556983,4.24037641502107,41.5474642560565));
#220435=CARTESIAN_POINT('Ctrl Pts',(6.67454769801821,4.24669165593355,41.5477643413729));
#220436=CARTESIAN_POINT('Ctrl Pts',(6.66561609809459,4.26070022456332,41.5484298940697));
#220437=CARTESIAN_POINT('Ctrl Pts',(6.66069401124881,4.2683907576479,41.5487952063302));
#220438=CARTESIAN_POINT('Ctrl Pts',(6.6464136015203,4.29061838687088,41.5498508637549));
#220439=CARTESIAN_POINT('Ctrl Pts',(6.63702089926751,4.30513338835862,41.550539990002));
#220440=CARTESIAN_POINT('Ctrl Pts',(6.57244489428123,4.40421222518066,41.5552424584642));
#220441=CARTESIAN_POINT('Ctrl Pts',(6.51569343417278,4.48774522206117,41.5591995337757));
#220442=CARTESIAN_POINT('Ctrl Pts',(6.35453243946062,4.715455330846,41.5699790903228));
#220443=CARTESIAN_POINT('Ctrl Pts',(6.24683111850503,4.85723241383463,41.5766812082956));
#220444=CARTESIAN_POINT('Ctrl Pts',(6.023050648152,5.1320462388652,41.5897364929209));
#220445=CARTESIAN_POINT('Ctrl Pts',(5.90712016905897,5.2650709439302,41.5960885985373));
#220446=CARTESIAN_POINT('Ctrl Pts',(5.68994763933128,5.49805497148893,41.6073796448948));
#220447=CARTESIAN_POINT('Ctrl Pts',(5.59027474376821,5.5993697722298,41.6123514034159));
#220448=CARTESIAN_POINT('Ctrl Pts',(5.4535979885375,5.73100877098024,41.6189466392761));
#220449=CARTESIAN_POINT('Ctrl Pts',(5.41897183773035,5.76376064689435,41.6205993148689));
#220450=CARTESIAN_POINT('Ctrl Pts',(5.35387141337888,5.82423202378489,41.6236758602257));
#220451=CARTESIAN_POINT('Ctrl Pts',(5.32347252886368,5.85203024770597,41.6251002923482));
#220452=CARTESIAN_POINT('Ctrl Pts',(5.26574915612239,5.90399332994155,41.6277843320518));
#220453=CARTESIAN_POINT('Ctrl Pts',(5.23847196168647,5.92820908232838,41.6290441023104));
#220454=CARTESIAN_POINT('Ctrl Pts',(5.18522572474764,5.97482478721945,41.6314881897212));
#220455=CARTESIAN_POINT('Ctrl Pts',(5.15927657852703,5.9972462213741,41.6326724876556));
#220456=CARTESIAN_POINT('Ctrl Pts',(5.1086062635638,6.04045579855471,41.6349731706584));
#220457=CARTESIAN_POINT('Ctrl Pts',(5.08390195689247,6.06126266549168,41.6360894768823));
#220458=CARTESIAN_POINT('Ctrl Pts',(5.0355485660153,6.1014840642528,41.6382650616517));
#220459=CARTESIAN_POINT('Ctrl Pts',(5.01191290297839,6.12091383664271,41.6393242264894));
#220460=CARTESIAN_POINT('Ctrl Pts',(4.61684476853867,6.44185829776546,41.6569652991833));
#220461=CARTESIAN_POINT('Ctrl Pts',(4.2189603037467,6.70917871269953,41.6737852942337));
#220462=CARTESIAN_POINT('Ctrl Pts',(3.77328353440653,6.95321079794561,41.6939104568213));
#220463=CARTESIAN_POINT('Ctrl Pts',(3.74706508671286,6.96737484493203,41.6950989140428));
#220464=CARTESIAN_POINT('Ctrl Pts',(3.71263693429395,6.98572350423005,41.6966647805266));
#220465=CARTESIAN_POINT('Ctrl Pts',(3.70449880711223,6.99004252279446,41.6970353038563));
#220466=CARTESIAN_POINT('Ctrl Pts',(3.69136555731544,6.99698314606487,41.6976338470275));
#220467=CARTESIAN_POINT('Ctrl Pts',(3.68637512669243,6.99961364998906,41.6978614224354));
#220468=CARTESIAN_POINT('Ctrl Pts',(3.67693480431925,7.00457683859597,41.6982921786328));
#220469=CARTESIAN_POINT('Ctrl Pts',(3.67248549357513,7.00691062753917,41.6984953050114));
#220470=CARTESIAN_POINT('Ctrl Pts',(3.6624019328315,7.01218749670569,41.6989558914722));
#220471=CARTESIAN_POINT('Ctrl Pts',(3.65676635702034,7.01512802565935,41.6992134749696));
#220472=CARTESIAN_POINT('Ctrl Pts',(3.64015674522534,7.02376913034822,41.6999731247799));
#220473=CARTESIAN_POINT('Ctrl Pts',(3.62917291122858,7.02945075409312,41.7004760922341));
#220474=CARTESIAN_POINT('Ctrl Pts',(3.54487551154266,7.07280515276999,41.7043406622659));
#220475=CARTESIAN_POINT('Ctrl Pts',(3.47099211339649,7.10935498005472,41.707753551548));
#220476=CARTESIAN_POINT('Ctrl Pts',(3.21041319145589,7.23323209310508,41.7198463035516));
#220477=CARTESIAN_POINT('Ctrl Pts',(3.02089232249659,7.3144106419306,41.728738253241));
#220478=CARTESIAN_POINT('Ctrl Pts',(2.36015294890875,7.56736526403759,41.7596208291027));
#220479=CARTESIAN_POINT('Ctrl Pts',(1.87586435508062,7.70172146626963,41.7819601915515));
#220480=CARTESIAN_POINT('Ctrl Pts',(1.04187134182631,7.84970308737852,41.8183001021839));
#220481=CARTESIAN_POINT('Ctrl Pts',(0.698020577031019,7.88771995460522,
41.8327226117628));
#220482=CARTESIAN_POINT('Ctrl Pts',(0.319519857606371,7.9046148298508,41.8480649197127));
#220483=CARTESIAN_POINT('Ctrl Pts',(0.286263940302587,7.90588904074924,
41.8494086808059));
#220484=CARTESIAN_POINT('Ctrl Pts',(0.236392962909805,7.90748477521783,
41.851417759828));
#220485=CARTESIAN_POINT('Ctrl Pts',(0.219783438972896,7.90796385586357,
41.852085879521));
#220486=CARTESIAN_POINT('Ctrl Pts',(0.191105754536285,7.90870060710512,
41.8532377603289));
#220487=CARTESIAN_POINT('Ctrl Pts',(0.179038304844068,7.90898299331668,
41.8537219529738));
#220488=CARTESIAN_POINT('Ctrl Pts',(0.154053817537983,7.90951043551615,
41.8547233876408));
#220489=CARTESIAN_POINT('Ctrl Pts',(0.141136728312348,7.90975147101862,
41.8552405586643));
#220490=CARTESIAN_POINT('Ctrl Pts',(0.110917285840395,7.91024132290573,
41.8564491670535));
#220491=CARTESIAN_POINT('Ctrl Pts',(0.0936145758183488,7.91046501444356,
41.85714017413));
#220492=CARTESIAN_POINT('Ctrl Pts',(0.0379336129200809,7.91100215015645,
41.8593607597468));
#220493=CARTESIAN_POINT('Ctrl Pts',(-0.000446417369137525,7.91109308534335,
41.8608866579435));
#220494=CARTESIAN_POINT('Ctrl Pts',(-0.657937600988395,7.90786620402613,
41.8869514640247));
#220495=CARTESIAN_POINT('Ctrl Pts',(-1.27455985327542,7.83216355241303,
41.9100206344112));
#220496=CARTESIAN_POINT('Ctrl Pts',(-2.20124744488796,7.60595003412247,
41.945101943823));
#220497=CARTESIAN_POINT('Ctrl Pts',(-2.52105686132487,7.50601280044812,
41.9573365152083));
#220498=CARTESIAN_POINT('Ctrl Pts',(-3.03620611225692,7.3083842404825,41.9781632766603));
#220499=CARTESIAN_POINT('Ctrl Pts',(-3.23555335730512,7.22234129958856,
41.9865189460275));
#220500=CARTESIAN_POINT('Ctrl Pts',(-3.44777701216067,7.12018940735029,
41.9959388376127));
#220501=CARTESIAN_POINT('Ctrl Pts',(-3.46442478062121,7.11210408068141,
41.9966813697875));
#220502=CARTESIAN_POINT('Ctrl Pts',(-3.48830836144234,7.10040077873328,
41.9977519813274));
#220503=CARTESIAN_POINT('Ctrl Pts',(-3.49556730482277,7.0968299725994,41.9980780843184));
#220504=CARTESIAN_POINT('Ctrl Pts',(-3.50813239344269,7.0906250220969,41.9986438132672));
#220505=CARTESIAN_POINT('Ctrl Pts',(-3.51344108842076,7.08799603638857,
41.9988832188529));
#220506=CARTESIAN_POINT('Ctrl Pts',(-3.52366358699059,7.08291931781152,
41.9993449763496));
#220507=CARTESIAN_POINT('Ctrl Pts',(-3.5285778068292,7.08047242759022,41.9995672917061));
#220508=CARTESIAN_POINT('Ctrl Pts',(-3.54104333922466,7.07424938431496,
42.0001320849182));
#220509=CARTESIAN_POINT('Ctrl Pts',(-3.5485911497255,7.07046625995094,42.0004748683441));
#220510=CARTESIAN_POINT('Ctrl Pts',(-3.5743521539647,7.05750265190446,42.0016475912794));
#220511=CARTESIAN_POINT('Ctrl Pts',(-3.59253579578981,7.04826386760933,
42.0024801362335));
#220512=CARTESIAN_POINT('Ctrl Pts',(-3.88395218019158,6.89877970283401,
42.0159020361551));
#220513=CARTESIAN_POINT('Ctrl Pts',(-4.14876607418192,6.74284158376022,
42.0293556189183));
#220514=CARTESIAN_POINT('Ctrl Pts',(-5.03575823288574,6.14847532580657,
42.0775826492922));
#220515=CARTESIAN_POINT('Ctrl Pts',(-5.60347049897522,5.63596163035518,
42.1135700742141));
#220516=CARTESIAN_POINT('Ctrl Pts',(-6.20226648627755,4.91397583051021,
42.1534922700765));
#220517=CARTESIAN_POINT('Ctrl Pts',(-6.31069038605238,4.77393552077865,
42.1608489967513));
#220518=CARTESIAN_POINT('Ctrl Pts',(-6.42647438413755,4.61354295450916,
42.1688539988249));
#220519=CARTESIAN_POINT('Ctrl Pts',(-6.43855390252691,4.59667001819435,
42.1696910832619));
#220520=CARTESIAN_POINT('Ctrl Pts',(-6.45544927921385,4.57287291865571,
42.1708646628838));
#220521=CARTESIAN_POINT('Ctrl Pts',(-6.46032061342598,4.56598835948938,
42.171203360242));
#220522=CARTESIAN_POINT('Ctrl Pts',(-6.46924188268018,4.55333725062501,
42.1718242479178));
#220523=CARTESIAN_POINT('Ctrl Pts',(-6.47329513734873,4.54757305820301,
42.1721065697476));
#220524=CARTESIAN_POINT('Ctrl Pts',(-6.48149829068946,4.53587404490415,
42.1726784143019));
#220525=CARTESIAN_POINT('Ctrl Pts',(-6.48564775297144,4.52993892543764,
42.172967919629));
#220526=CARTESIAN_POINT('Ctrl Pts',(-6.49585093667497,4.51530220179238,
42.1736803963505));
#220527=CARTESIAN_POINT('Ctrl Pts',(-6.50189533768921,4.50659410019524,
42.1741029990117));
#220528=CARTESIAN_POINT('Ctrl Pts',(-6.52391183469455,4.47473868249381,
42.1756442633853));
#220529=CARTESIAN_POINT('Ctrl Pts',(-6.53977806301494,4.45151825915932,
42.1767587465458));
#220530=CARTESIAN_POINT('Ctrl Pts',(-6.76906668787332,4.11207974731767,
42.1929209174369));
#220531=CARTESIAN_POINT('Ctrl Pts',(-6.95947556188112,3.78090014648215,
42.2070243362292));
#220532=CARTESIAN_POINT('Ctrl Pts',(-7.46143197580483,2.74036550525493,
42.2477766617882));
#220533=CARTESIAN_POINT('Ctrl Pts',(-7.693510719254,1.99805136147197,42.2718825976976));
#220534=CARTESIAN_POINT('Ctrl Pts',(-7.81782820231704,1.21079849749936,
42.3010003059383));
#220535=CARTESIAN_POINT('Ctrl Pts',(-7.82138259187117,1.18762163155551,
42.3018609750709));
#220536=CARTESIAN_POINT('Ctrl Pts',(-7.8362578405834,1.08766164772221,42.3055890127478));
#220537=CARTESIAN_POINT('Ctrl Pts',(-7.84655118492198,1.01073176742203,
42.3084988746579));
#220538=CARTESIAN_POINT('Ctrl Pts',(-7.86649340689596,0.842941019962311,
42.3149567807464));
#220539=CARTESIAN_POINT('Ctrl Pts',(-7.87570326841956,0.752040486649506,
42.3185260399074));
#220540=CARTESIAN_POINT('Ctrl Pts',(-7.88416991522032,0.651064694886736,
42.3225881851356));
#220541=CARTESIAN_POINT('Ctrl Pts',(-7.88498452584095,0.641123634296307,
42.3229891469778));
#220542=CARTESIAN_POINT('Ctrl Pts',(-7.88617309362215,0.62627403825458,
42.3235896813882));
#220543=CARTESIAN_POINT('Ctrl Pts',(-7.88656127600493,0.621366617358638,
42.3237884026503));
#220544=CARTESIAN_POINT('Ctrl Pts',(-7.88722110434174,0.612924805331908,
42.3241306968172));
#220545=CARTESIAN_POINT('Ctrl Pts',(-7.88749495612917,0.609390583054566,
42.3242741366023));
#220546=CARTESIAN_POINT('Ctrl Pts',(-7.88803964793819,0.602299128213421,
42.3245622249174));
#220547=CARTESIAN_POINT('Ctrl Pts',(-7.88831045732677,0.59874189433717,
42.3247068752623));
#220548=CARTESIAN_POINT('Ctrl Pts',(-7.88885279295259,0.591553774577943,
42.3249994533008));
#220549=CARTESIAN_POINT('Ctrl Pts',(-7.88912421887864,0.587922882866159,
42.325147387155));
#220550=CARTESIAN_POINT('Ctrl Pts',(-7.88974226027719,0.57957778614266,
42.3254877288672));
#220551=CARTESIAN_POINT('Ctrl Pts',(-7.89008715612654,0.574863472767717,
42.3256802409768));
#220552=CARTESIAN_POINT('Ctrl Pts',(-7.89096650305754,0.562693978209425,
42.3261778201668));
#220553=CARTESIAN_POINT('Ctrl Pts',(-7.89149461315194,0.555238359001871,
42.3264832712027));
#220554=CARTESIAN_POINT('Ctrl Pts',(-7.89236009415005,0.542769190243475,
42.326995129068));
#220555=CARTESIAN_POINT('Ctrl Pts',(-7.89270325669091,0.537756033157323,
42.3272011903006));
#220556=CARTESIAN_POINT('Ctrl Pts',(-7.90496435960736,0.356097193764284,
42.3346778608755));
#220557=CARTESIAN_POINT('Ctrl Pts',(-7.91095283143479,0.179114742897442,
42.3422953872974));
#220558=CARTESIAN_POINT('Ctrl Pts',(-7.91099972245079,0.00209556283347154,
42.3501361000675));
#220559=CARTESIAN_POINT('',(-7.90023482472552,0.00384550184740459,44.3576663208611));
#220560=CARTESIAN_POINT('Ctrl Pts',(-7.92439853970512,0.00241054887052533,
42.3578451112103));
#220561=CARTESIAN_POINT('Ctrl Pts',(-7.90901013703974,-2.42537430455476,
42.4559139907394));
#220562=CARTESIAN_POINT('Ctrl Pts',(-5.39991474507588,-7.5142952426176,
42.6599524474851));
#220563=CARTESIAN_POINT('Ctrl Pts',(1.73928624701431,-8.54502927126578,
42.9169756928389));
#220564=CARTESIAN_POINT('Ctrl Pts',(6.20214295403129,-5.4183663384529,43.128914847272));
#220565=CARTESIAN_POINT('Ctrl Pts',(8.05603662777276,-1.79352951637783,
43.2878692130968));
#220566=CARTESIAN_POINT('Ctrl Pts',(7.91736572010992,2.26730000951632,43.4468235789215));
#220567=CARTESIAN_POINT('Ctrl Pts',(5.19886495601264,7.00699902943489,43.6587627333544));
#220568=CARTESIAN_POINT('Ctrl Pts',(-0.478760874683204,8.7140644824411,
43.8707018877876));
#220569=CARTESIAN_POINT('Ctrl Pts',(-5.3465309654218,6.25325520421469,44.0826410422206));
#220570=CARTESIAN_POINT('Ctrl Pts',(-7.51352671913395,3.24846515819994,
44.2273006934993));
#220571=CARTESIAN_POINT('Ctrl Pts',(-7.90127645816085,0.967839502849978,
44.3189755561699));
#220572=CARTESIAN_POINT('Ctrl Pts',(-7.89681039064019,0.00386106567456798,
44.3576656302323));
#220573=CARTESIAN_POINT('',(-7.9087893072687,-0.00562351359541763,46.3576688933213));
#220574=CARTESIAN_POINT('Ctrl Pts',(-7.91099908898921,0.0037965789759559,
44.3576684917633));
#220575=CARTESIAN_POINT('Ctrl Pts',(-7.91109982716945,-0.206113357618994,
44.3660783104271));
#220576=CARTESIAN_POINT('Ctrl Pts',(-7.90284075888705,-0.415997733834797,
44.3744881290909));
#220577=CARTESIAN_POINT('Ctrl Pts',(-7.88625968517452,-0.625163321053882,
44.3828979477547));
#220578=CARTESIAN_POINT('Ctrl Pts',(-7.87039289892966,-0.825318372513329,
44.3909454842056));
#220579=CARTESIAN_POINT('Ctrl Pts',(-7.84690610496436,-1.02481493022194,
44.3989930206565));
#220580=CARTESIAN_POINT('Ctrl Pts',(-7.81588547481346,-1.22305161158475,
44.4070405571074));
#220581=CARTESIAN_POINT('Ctrl Pts',(-7.78485066183586,-1.42137892800182,
44.4150917729425));
#220582=CARTESIAN_POINT('Ctrl Pts',(-7.74627519257816,-1.61844489821876,
44.4231429887776));
#220583=CARTESIAN_POINT('Ctrl Pts',(-7.70029643748892,-1.81365811960124,
44.4311942046126));
#220584=CARTESIAN_POINT('Ctrl Pts',(-7.65429036665681,-2.00898731615855,
44.4392502036337));
#220585=CARTESIAN_POINT('Ctrl Pts',(-7.60087231183685,-2.20246125254749,
44.4473062026549));
#220586=CARTESIAN_POINT('Ctrl Pts',(-7.54022973211643,-2.39350299496519,
44.455362201676));
#220587=CARTESIAN_POINT('Ctrl Pts',(-7.47954281728029,-2.58468440587652,
44.4634240903485));
#220588=CARTESIAN_POINT('Ctrl Pts',(-7.41162094061861,-2.77342976716646,
44.4714859790209));
#220589=CARTESIAN_POINT('Ctrl Pts',(-7.33670013772784,-2.95918098281675,
44.4795478676933));
#220590=CARTESIAN_POINT('Ctrl Pts',(-7.26167017368218,-3.14520284181893,
44.4876215027038));
#220591=CARTESIAN_POINT('Ctrl Pts',(-7.17962102796923,-3.32822153676562,
44.4956951377143));
#220592=CARTESIAN_POINT('Ctrl Pts',(-7.09083592370065,-3.50770108520613,
44.5037687727248));
#220593=CARTESIAN_POINT('Ctrl Pts',(-7.00197608919707,-3.68733170120405,
44.5118492032969));
#220594=CARTESIAN_POINT('Ctrl Pts',(-6.90636913929137,-3.86341694329685,
44.5199296338689));
#220595=CARTESIAN_POINT('Ctrl Pts',(-6.80434263566374,-4.03544821506715,
44.528010064441));
#220596=CARTESIAN_POINT('Ctrl Pts',(-6.70216180642607,-4.2077397018798,
44.5361027174977));
#220597=CARTESIAN_POINT('Ctrl Pts',(-6.59354219716093,-4.37596469417913,
44.5441953705544));
#220598=CARTESIAN_POINT('Ctrl Pts',(-6.47885362489306,-4.5396449979277,
44.5522880236112));
#220599=CARTESIAN_POINT('Ctrl Pts',(-6.44476484316526,-4.58829554817254,
44.554693395639));
#220600=CARTESIAN_POINT('Ctrl Pts',(-6.41014015950638,-4.63654483022345,
44.5570987676669));
#220601=CARTESIAN_POINT('Ctrl Pts',(-6.3749899338597,-4.68438089219777,
44.5595041396948));
#220602=CARTESIAN_POINT('Ctrl Pts',(-6.2615872279606,-4.83871102145419,
44.5672644226414));
#220603=CARTESIAN_POINT('Ctrl Pts',(-6.14237699780792,-4.98919264526007,
44.575024705588));
#220604=CARTESIAN_POINT('Ctrl Pts',(-6.01765181233345,-5.13534688852856,
44.5827849885346));
#220605=CARTESIAN_POINT('Ctrl Pts',(-5.89307673985873,-5.28132522785431,
44.5905359315925));
#220606=CARTESIAN_POINT('Ctrl Pts',(-5.76300015346301,-5.4229862837319,
44.5982868746503));
#220607=CARTESIAN_POINT('Ctrl Pts',(-5.62775838536374,-5.55987918537517,
44.6060378177082));
#220608=CARTESIAN_POINT('Ctrl Pts',(-5.4926519374696,-5.69663511472216,
44.6137810053277));
#220609=CARTESIAN_POINT('Ctrl Pts',(-5.35239084601381,-5.82863213414115,
44.6215241929472));
#220610=CARTESIAN_POINT('Ctrl Pts',(-5.20735233406623,-5.95545150839926,
44.6292673805666));
#220611=CARTESIAN_POINT('Ctrl Pts',(-5.06242954934239,-6.08216969260859,
44.6370043898436));
#220612=CARTESIAN_POINT('Ctrl Pts',(-4.91273720216241,-6.20371822188837,
44.6447413991205));
#220613=CARTESIAN_POINT('Ctrl Pts',(-4.75869013840848,-6.31971432634529,
44.6524784083974));
#220614=CARTESIAN_POINT('Ctrl Pts',(-4.6047348010644,-6.43564136161024,
44.6602108107181));
#220615=CARTESIAN_POINT('Ctrl Pts',(-4.44643019630563,-6.54602234023068,
44.6679432130388));
#220616=CARTESIAN_POINT('Ctrl Pts',(-4.28422516124588,-6.65051394763952,
44.6756756153595));
#220617=CARTESIAN_POINT('Ctrl Pts',(-4.12208389292393,-6.75496447686031,
44.683404977885));
#220618=CARTESIAN_POINT('Ctrl Pts',(-3.95604554959901,-6.85353005197379,
44.6911343404106));
#220619=CARTESIAN_POINT('Ctrl Pts',(-3.78658900026213,-6.94590992909452,
44.6988637029362));
#220620=CARTESIAN_POINT('Ctrl Pts',(-3.61713251704006,-7.03828977017251,
44.7065930624461));
#220621=CARTESIAN_POINT('Ctrl Pts',(-3.44425814018197,-7.12448373618032,
44.714322421956));
#220622=CARTESIAN_POINT('Ctrl Pts',(-3.26847081325667,-7.20423622203556,
44.7220517814659));
#220623=CARTESIAN_POINT('Ctrl Pts',(-3.0926746752393,-7.28399270537179,
44.7297815283991));
#220624=CARTESIAN_POINT('Ctrl Pts',(-2.91396562323699,-7.3573069162215,
44.7375112753322));
#220625=CARTESIAN_POINT('Ctrl Pts',(-2.73286996688449,-7.42397082053134,
44.7452410222654));
#220626=CARTESIAN_POINT('Ctrl Pts',(-2.55173205000262,-7.4906502815472,
44.7529725730143));
#220627=CARTESIAN_POINT('Ctrl Pts',(-2.36820675677898,-7.55067622135483,
44.7607041237632));
#220628=CARTESIAN_POINT('Ctrl Pts',(-2.18283703457222,-7.60389002290932,
44.7684356745121));
#220629=CARTESIAN_POINT('Ctrl Pts',(-1.99739007695806,-7.65712599631364,
44.776170446658));
#220630=CARTESIAN_POINT('Ctrl Pts',(-1.81009750496497,-7.70354408058446,
44.783905218804));
#220631=CARTESIAN_POINT('Ctrl Pts',(-1.62151401522891,-7.74303643917657,
44.7916399909499));
#220632=CARTESIAN_POINT('Ctrl Pts',(-1.43270563958536,-7.78257589242641,
44.7993839868156));
#220633=CARTESIAN_POINT('Ctrl Pts',(-1.24260362336187,-7.81517305230361,
44.8071279826812));
#220634=CARTESIAN_POINT('Ctrl Pts',(-1.05177041277071,-7.84077164562393,
44.8148719785469));
#220635=CARTESIAN_POINT('Ctrl Pts',(-0.860813341852577,-7.86638685371549,
44.8226210006543));
#220636=CARTESIAN_POINT('Ctrl Pts',(-0.669124487209044,-7.88499441252165,
44.8303700227618));
#220637=CARTESIAN_POINT('Ctrl Pts',(-0.477267761920374,-7.89659018079522,
44.8381190448693));
#220638=CARTESIAN_POINT('Ctrl Pts',(-0.285117834361302,-7.90820367013424,
44.8458799093079));
#220639=CARTESIAN_POINT('Ctrl Pts',(-0.0927998811833496,-7.91278395903853,
44.8536407737465));
#220640=CARTESIAN_POINT('Ctrl Pts',(0.0991246257200402,-7.9103789611229,
44.8614016381851));
#220641=CARTESIAN_POINT('Ctrl Pts',(0.231109408828784,-7.90872506536257,
44.8667387159048));
#220642=CARTESIAN_POINT('Ctrl Pts',(0.362908228918708,-7.90376878181581,
44.8720757936246));
#220643=CARTESIAN_POINT('Ctrl Pts',(0.494341184836341,-7.89553974044679,
44.8774128713443));
#220644=CARTESIAN_POINT('Ctrl Pts',(0.691692154768313,-7.88318356018403,
44.8854266716674));
#220645=CARTESIAN_POINT('Ctrl Pts',(0.888823270522177,-7.86340857175364,
44.8934404719905));
#220646=CARTESIAN_POINT('Ctrl Pts',(1.08514215758107,-7.8362227825554,44.9014542723135));
#220647=CARTESIAN_POINT('Ctrl Pts',(1.28123726428257,-7.80906798194778,
44.9094589378502));
#220648=CARTESIAN_POINT('Ctrl Pts',(1.476521658544,-7.77451925845426,44.9174636033868));
#220649=CARTESIAN_POINT('Ctrl Pts',(1.67040499389583,-7.73263655918005,
44.9254682689235));
#220650=CARTESIAN_POINT('Ctrl Pts',(1.8641002400297,-7.69079449095924,44.9334651690105));
#220651=CARTESIAN_POINT('Ctrl Pts',(2.05639681089065,-7.64163269568441,
44.9414620690975));
#220652=CARTESIAN_POINT('Ctrl Pts',(2.24671108690782,-7.58526270421569,
44.9494589691845));
#220653=CARTESIAN_POINT('Ctrl Pts',(2.43687302432396,-7.52893783456242,
44.9574494680882));
#220654=CARTESIAN_POINT('Ctrl Pts',(2.62505550996796,-7.46541636294701,
44.9654399669918));
#220655=CARTESIAN_POINT('Ctrl Pts',(2.81068629733434,-7.39486061653477,
44.9734304658955));
#220656=CARTESIAN_POINT('Ctrl Pts',(2.99619997191894,-7.32434938310365,
44.9814159236658));
#220657=CARTESIAN_POINT('Ctrl Pts',(3.17916484529946,-7.24681283943503,
44.9894013814361));
#220658=CARTESIAN_POINT('Ctrl Pts',(3.35902459788108,-7.16246289699499,
44.9973868392064));
#220659=CARTESIAN_POINT('Ctrl Pts',(3.54478152141502,-7.07534732175913,
45.0056341210309));
#220660=CARTESIAN_POINT('Ctrl Pts',(3.72722590038802,-6.98096408133548,
45.0138814028554));
#220661=CARTESIAN_POINT('Ctrl Pts',(3.90576689097264,-6.87960071467683,
45.0221286846798));
#220662=CARTESIAN_POINT('Ctrl Pts',(4.07852271811378,-6.78152176825905,
45.0301087344633));
#220663=CARTESIAN_POINT('Ctrl Pts',(4.24762384174879,-6.67690813471623,
45.0380887842467));
#220664=CARTESIAN_POINT('Ctrl Pts',(4.41255965923379,-6.56606718315482,
45.0460688340302));
#220665=CARTESIAN_POINT('Ctrl Pts',(4.57748237876047,-6.45523503374557,
45.0540482500983));
#220666=CARTESIAN_POINT('Ctrl Pts',(4.7382401736902,-6.33817673848495,45.0620276661664));
#220667=CARTESIAN_POINT('Ctrl Pts',(4.89435118121349,-6.21524315815191,
45.0700070822345));
#220668=CARTESIAN_POINT('Ctrl Pts',(5.05047378340941,-6.09230044729924,
45.0779870909496));
#220669=CARTESIAN_POINT('Ctrl Pts',(5.20194864763116,-5.96348178887062,
45.0859670996647));
#220670=CARTESIAN_POINT('Ctrl Pts',(5.34832648350908,-5.82917874368211,
45.0939471083798));
#220671=CARTESIAN_POINT('Ctrl Pts',(5.49473768746913,-5.69484508296349,
45.1019289362063));
#220672=CARTESIAN_POINT('Ctrl Pts',(5.63604930102413,-5.5550247700403,45.1099107640327));
#220673=CARTESIAN_POINT('Ctrl Pts',(5.77184816184117,-5.41014692930337,
45.1178925918592));
#220674=CARTESIAN_POINT('Ctrl Pts',(5.90774799521772,-5.26516136537711,
45.1258803545336));
#220675=CARTESIAN_POINT('Ctrl Pts',(6.03812665892673,-5.11511100604018,
45.1338681172079));
#220676=CARTESIAN_POINT('Ctrl Pts',(6.16260996772766,-4.96045959419726,
45.1418558798823));
#220677=CARTESIAN_POINT('Ctrl Pts',(6.28714810340438,-4.80574006837321,
45.1498471606514));
#220678=CARTESIAN_POINT('Ctrl Pts',(6.40578550402128,-4.64641571502952,
45.1578384414205));
#220679=CARTESIAN_POINT('Ctrl Pts',(6.51819042492076,-4.48298054696553,
45.1658297221896));
#220680=CARTESIAN_POINT('Ctrl Pts',(6.63070110390533,-4.31939160813888,
45.1738285216914));
#220681=CARTESIAN_POINT('Ctrl Pts',(6.73696740993568,-4.15168441024629,
45.1818273211931));
#220682=CARTESIAN_POINT('Ctrl Pts',(6.83670227117521,-3.9803797626995,45.1898261206949));
#220683=CARTESIAN_POINT('Ctrl Pts',(6.85954283053687,-3.94114880651634,
45.1916579481279));
#220684=CARTESIAN_POINT('Ctrl Pts',(6.88204103031947,-3.90172926989703,
45.1934897755608));
#220685=CARTESIAN_POINT('Ctrl Pts',(6.90419377139895,-3.86212757000282,
45.1953216029938));
#220686=CARTESIAN_POINT('Ctrl Pts',(7.00247139146564,-3.68644001954424,
45.2034482560269));
#220687=CARTESIAN_POINT('Ctrl Pts',(7.09411950613567,-3.50685571861464,
45.21157490906));
#220688=CARTESIAN_POINT('Ctrl Pts',(7.17882944288115,-3.32390265050328,
45.2197015620931));
#220689=CARTESIAN_POINT('Ctrl Pts',(7.26346727072994,-3.14110532024741,
45.2278212973548));
#220690=CARTESIAN_POINT('Ctrl Pts',(7.34117856188255,-2.95494522784442,
45.2359410326164));
#220691=CARTESIAN_POINT('Ctrl Pts',(7.41170034204722,-2.7659752420615,45.244060767878));
#220692=CARTESIAN_POINT('Ctrl Pts',(7.48217097162953,-2.57714231925115,
45.252174613765));
#220693=CARTESIAN_POINT('Ctrl Pts',(7.54546237646609,-2.38550386443243,
45.2602884596519));
#220694=CARTESIAN_POINT('Ctrl Pts',(7.60135930856294,-2.1916335601837,45.2684023055389));
#220695=CARTESIAN_POINT('Ctrl Pts',(7.65721652380877,-1.99790100800299,
45.2765103862363));
#220696=CARTESIAN_POINT('Ctrl Pts',(7.70568966018132,-1.80194007576001,
45.2846184669337));
#220697=CARTESIAN_POINT('Ctrl Pts',(7.7466129059657,-1.60434082573676,45.2927265476311));
#220698=CARTESIAN_POINT('Ctrl Pts',(7.78751857500983,-1.40682644558694,
45.3008311458669));
#220699=CARTESIAN_POINT('Ctrl Pts',(7.8208807545832,-1.20767546234247,45.3089357441028));
#220700=CARTESIAN_POINT('Ctrl Pts',(7.84658425365761,-1.00749022340289,
45.3170403423387));
#220701=CARTESIAN_POINT('Ctrl Pts',(7.87227971856832,-0.807367556526994,
45.3251424073137));
#220702=CARTESIAN_POINT('Ctrl Pts',(7.89032123671649,-0.606211594589851,
45.3332444722887));
#220703=CARTESIAN_POINT('Ctrl Pts',(7.90064513463664,-0.404632495658001,
45.3413465372637));
#220704=CARTESIAN_POINT('Ctrl Pts',(7.90613682644405,-0.297404557653095,
45.345656347782));
#220705=CARTESIAN_POINT('Ctrl Pts',(7.90944561592449,-0.190057001995731,
45.3499661583004));
#220706=CARTESIAN_POINT('Ctrl Pts',(7.91056791006032,-0.0826821644845067,
45.3542759688187));
#220707=CARTESIAN_POINT('Ctrl Pts',(7.9127263280764,0.123823221542817,45.3625646806382));
#220708=CARTESIAN_POINT('Ctrl Pts',(7.90679341923676,0.330340691145279,
45.3708533924576));
#220709=CARTESIAN_POINT('Ctrl Pts',(7.89280547003969,0.536230185751951,
45.3791421042771));
#220710=CARTESIAN_POINT('Ctrl Pts',(7.8788094569267,0.742238373638703,45.3874355944578));
#220711=CARTESIAN_POINT('Ctrl Pts',(7.85674915431576,0.947617572038266,
45.3957290846386));
#220712=CARTESIAN_POINT('Ctrl Pts',(7.8267127113667,1.15173310004138,45.4040225748193));
#220713=CARTESIAN_POINT('Ctrl Pts',(7.79665714179197,1.35597860486316,45.4123213461342));
#220714=CARTESIAN_POINT('Ctrl Pts',(7.75861533609209,1.55895854380817,45.420620117449));
#220715=CARTESIAN_POINT('Ctrl Pts',(7.71272666472887,1.76004783888968,45.4289188887638));
#220716=CARTESIAN_POINT('Ctrl Pts',(7.66678457630412,1.9613712135148,45.4372273203274));
#220717=CARTESIAN_POINT('Ctrl Pts',(7.6129774292099,2.16079925958702,45.4455357518909));
#220718=CARTESIAN_POINT('Ctrl Pts',(7.55149510465868,2.35771980615085,45.4538441834544));
#220719=CARTESIAN_POINT('Ctrl Pts',(7.48997485363959,2.55476182666408,45.4621577402221));
#220720=CARTESIAN_POINT('Ctrl Pts',(7.42077006778067,2.7492929830202,45.4704712969897));
#220721=CARTESIAN_POINT('Ctrl Pts',(7.34411952157781,2.94071920672133,45.4787848537574));
#220722=CARTESIAN_POINT('Ctrl Pts',(7.2673851739534,3.13235471516291,45.4871074996693));
#220723=CARTESIAN_POINT('Ctrl Pts',(7.18318891056288,3.32087823705202,45.4954301455813));
#220724=CARTESIAN_POINT('Ctrl Pts',(7.09181705855585,3.50571701766931,45.5037527914932));
#220725=CARTESIAN_POINT('Ctrl Pts',(7.05713335022302,3.57587970141391,45.5069119725433));
#220726=CARTESIAN_POINT('Ctrl Pts',(7.02141619908188,3.64551171933842,45.5100711535933));
#220727=CARTESIAN_POINT('Ctrl Pts',(6.98468296144834,3.71458273942758,45.5132303346434));
#220728=CARTESIAN_POINT('Ctrl Pts',(6.88354481067239,3.90475697110615,45.5219285532038));
#220729=CARTESIAN_POINT('Ctrl Pts',(6.77461103495292,4.09084538653731,45.5306267717642));
#220730=CARTESIAN_POINT('Ctrl Pts',(6.65822115543557,4.27223735825975,45.5393249903246));
#220731=CARTESIAN_POINT('Ctrl Pts',(6.54193354002888,4.45346995282031,45.548015566334));
#220732=CARTESIAN_POINT('Ctrl Pts',(6.41820302540795,4.63001415083212,45.5567061423434));
#220733=CARTESIAN_POINT('Ctrl Pts',(6.28741352878674,4.80128650655525,45.5653967183529));
#220734=CARTESIAN_POINT('Ctrl Pts',(6.15348736160973,4.97666641654763,45.5742957168625));
#220735=CARTESIAN_POINT('Ctrl Pts',(6.0121595041008,5.14651824650132,45.5831947153721));
#220736=CARTESIAN_POINT('Ctrl Pts',(5.86388959808269,5.31024667802708,45.5920937138817));
#220737=CARTESIAN_POINT('Ctrl Pts',(5.7195189483578,5.46966931929405,45.6007586832692));
#220738=CARTESIAN_POINT('Ctrl Pts',(5.56856689393716,5.62328633793491,45.6094236526567));
#220739=CARTESIAN_POINT('Ctrl Pts',(5.41149969380398,5.77057987241832,45.6180886220442));
#220740=CARTESIAN_POINT('Ctrl Pts',(5.248069234209,5.92384070609705,45.6271046351148));
#220741=CARTESIAN_POINT('Ctrl Pts',(5.07801796646155,6.07025483645696,45.6361206481855));
#220742=CARTESIAN_POINT('Ctrl Pts',(4.90191645063256,6.20927822786336,45.6451366612562));
#220743=CARTESIAN_POINT('Ctrl Pts',(4.72581493480356,6.34830161926976,45.6541526743268));
#220744=CARTESIAN_POINT('Ctrl Pts',(4.54366334874069,6.47993404570182,45.6631686873975));
#220745=CARTESIAN_POINT('Ctrl Pts',(4.35607592972436,6.60367499915585,45.6721847004682));
#220746=CARTESIAN_POINT('Ctrl Pts',(4.1935716725746,6.71086999029916,45.6799951416704));
#220747=CARTESIAN_POINT('Ctrl Pts',(4.02705788775809,6.81209615834343,45.6878055828726));
#220748=CARTESIAN_POINT('Ctrl Pts',(3.85702114597265,6.90704776873013,45.6956160240748));
#220749=CARTESIAN_POINT('Ctrl Pts',(3.68699666349458,7.00199253329653,45.7034259021599));
#220750=CARTESIAN_POINT('Ctrl Pts',(3.51345003746774,7.09066346960936,45.711235780245));
#220751=CARTESIAN_POINT('Ctrl Pts',(3.33689361421739,7.17280015108432,45.7190456583301));
#220752=CARTESIAN_POINT('Ctrl Pts',(3.1603187571691,7.25494540823702,45.7268563518243));
#220753=CARTESIAN_POINT('Ctrl Pts',(2.98073379664296,7.33055490386447,45.7346670453185));
#220754=CARTESIAN_POINT('Ctrl Pts',(2.79867241578842,7.39941576809311,45.7424777388127));
#220755=CARTESIAN_POINT('Ctrl Pts',(2.61648183404873,7.46832549982221,45.7502939752096));
#220756=CARTESIAN_POINT('Ctrl Pts',(2.43181165073282,7.53047690725006,45.7581102116064));
#220757=CARTESIAN_POINT('Ctrl Pts',(2.24521295929854,7.5857062800637,45.7659264480033));
#220758=CARTESIAN_POINT('Ctrl Pts',(2.05854527962687,7.64095607197596,45.7737455741759));
#220759=CARTESIAN_POINT('Ctrl Pts',(1.86994801126352,7.68927863918557,45.7815647003485));
#220760=CARTESIAN_POINT('Ctrl Pts',(1.67998402619482,7.73056108388843,45.7893838265211));
#220761=CARTESIAN_POINT('Ctrl Pts',(1.48980880674577,7.77188943345912,45.7972116473327));
#220762=CARTESIAN_POINT('Ctrl Pts',(1.29826418053113,7.80616195614139,45.8050394681443));
#220763=CARTESIAN_POINT('Ctrl Pts',(1.10592085526108,7.83331730889912,45.8128672889559));
#220764=CARTESIAN_POINT('Ctrl Pts',(0.956264286457905,7.85444607389607,
45.8189578814016));
#220765=CARTESIAN_POINT('Ctrl Pts',(0.806124361235694,7.87126719524561,
45.8250484738473));
#220766=CARTESIAN_POINT('Ctrl Pts',(0.655770330981767,7.88377360614852,
45.8311390662929));
#220767=CARTESIAN_POINT('Ctrl Pts',(0.455392368194894,7.90044099533835,
45.8392560452949));
#220768=CARTESIAN_POINT('Ctrl Pts',(0.254235815865489,7.90947658372479,
45.8473730242969));
#220769=CARTESIAN_POINT('Ctrl Pts',(0.0529080594121575,7.91082307584042,
45.8554900032989));
#220770=CARTESIAN_POINT('Ctrl Pts',(-0.148272432775386,7.9121685830438,
45.8636010450124));
#220771=CARTESIAN_POINT('Ctrl Pts',(-0.349623559861184,7.90583620596543,
45.871712086726));
#220772=CARTESIAN_POINT('Ctrl Pts',(-0.55053476441224,7.89182060573944,
45.8798231284396));
#220773=CARTESIAN_POINT('Ctrl Pts',(-0.751327575407982,7.87781326466825,
45.8879293904543));
#220774=CARTESIAN_POINT('Ctrl Pts',(-0.951680661696556,7.85613175097405,
45.8960356524689));
#220775=CARTESIAN_POINT('Ctrl Pts',(-1.15098483876664,7.82682278456139,
45.9041419144836));
#220776=CARTESIAN_POINT('Ctrl Pts',(-1.35019987652316,7.79752692666049,
45.9122445509514));
#220777=CARTESIAN_POINT('Ctrl Pts',(-1.54836662387694,7.76061046584511,
45.9203471874192));
#220778=CARTESIAN_POINT('Ctrl Pts',(-1.74488180554461,7.71617188019288,
45.928449823887));
#220779=CARTESIAN_POINT('Ctrl Pts',(-1.94133698337312,7.67174686339434,
45.9365499863002));
#220780=CARTESIAN_POINT('Ctrl Pts',(-2.13614128887116,7.61980437345477,
45.9446501487134));
#220781=CARTESIAN_POINT('Ctrl Pts',(-2.32870184792713,7.5604939457327,45.9527503111266));
#220782=CARTESIAN_POINT('Ctrl Pts',(-2.52313804086199,7.50060580548137,
45.9609293730772));
#220783=CARTESIAN_POINT('Ctrl Pts',(-2.71528622065873,7.43320550083424,
45.9691084350279));
#220784=CARTESIAN_POINT('Ctrl Pts',(-2.90455106595427,7.35849876708992,
45.9772874969785));
#220785=CARTESIAN_POINT('Ctrl Pts',(-3.0919891346209,7.28451309971699,45.9853876149542));
#220786=CARTESIAN_POINT('Ctrl Pts',(-3.27659898816238,7.20336156377171,
45.9934877329298));
#220787=CARTESIAN_POINT('Ctrl Pts',(-3.45782158877621,7.11529274592361,
46.0015878509055));
#220788=CARTESIAN_POINT('Ctrl Pts',(-3.6390685787649,7.02721207556151,46.0096890590145));
#220789=CARTESIAN_POINT('Ctrl Pts',(-3.81692711812746,6.9322124068927,46.0177902671236));
#220790=CARTESIAN_POINT('Ctrl Pts',(-3.99086146664235,6.83058897563521,
46.0258914752327));
#220791=CARTESIAN_POINT('Ctrl Pts',(-4.16484168715849,6.72893874305754,
46.0339948198871));
#220792=CARTESIAN_POINT('Ctrl Pts',(-4.33489537597066,6.62066142591515,
46.0420981645416));
#220793=CARTESIAN_POINT('Ctrl Pts',(-4.50051408243206,6.50609667879526,
46.050201509196));
#220794=CARTESIAN_POINT('Ctrl Pts',(-4.66886837705556,6.38963962148463,
46.0584386999249));
#220795=CARTESIAN_POINT('Ctrl Pts',(-4.83263961466782,6.26668580812152,
46.0666758906538));
#220796=CARTESIAN_POINT('Ctrl Pts',(-4.99132723906832,6.13763581458973,
46.0749130813826));
#220797=CARTESIAN_POINT('Ctrl Pts',(-5.14763963626277,6.01051743391519,
46.0830269783159));
#220798=CARTESIAN_POINT('Ctrl Pts',(-5.29901931862242,5.87748432973878,
46.0911408752493));
#220799=CARTESIAN_POINT('Ctrl Pts',(-5.44502358725628,5.73895801816173,
46.0992547721826));
#220800=CARTESIAN_POINT('Ctrl Pts',(-5.59435574271114,5.59727426542921,
46.1075536098092));
#220801=CARTESIAN_POINT('Ctrl Pts',(-5.7380642686248,5.449844163697,46.1158524474359));
#220802=CARTESIAN_POINT('Ctrl Pts',(-5.87571744045468,5.29715636544144,
46.1241512850625));
#220803=CARTESIAN_POINT('Ctrl Pts',(-6.01337061228458,5.14446856718585,
46.1324501226891));
#220804=CARTESIAN_POINT('Ctrl Pts',(-6.14496822909381,4.9865233685294,46.1407489603158));
#220805=CARTESIAN_POINT('Ctrl Pts',(-6.27012419589844,4.82384323625976,
46.1490477979425));
#220806=CARTESIAN_POINT('Ctrl Pts',(-6.38962698099469,4.66851121827937,
46.156971784587));
#220807=CARTESIAN_POINT('Ctrl Pts',(-6.50351342195307,4.50852890841244,
46.1648957712315));
#220808=CARTESIAN_POINT('Ctrl Pts',(-6.61140283708434,4.34433809984825,
46.1728197578761));
#220809=CARTESIAN_POINT('Ctrl Pts',(-6.71917673398114,4.180323091962,46.1807352602319));
#220810=CARTESIAN_POINT('Ctrl Pts',(-6.82096620798325,4.01210884387182,
46.1886507625878));
#220811=CARTESIAN_POINT('Ctrl Pts',(-6.91643073493292,3.84017016405202,
46.1965662649436));
#220812=CARTESIAN_POINT('Ctrl Pts',(-7.01180879751107,3.66838721296585,
46.2044745980508));
#220813=CARTESIAN_POINT('Ctrl Pts',(-7.10087315974315,3.49288684740855,
46.2123829311579));
#220814=CARTESIAN_POINT('Ctrl Pts',(-7.1833263914318,3.31417304227757,46.220291264265));
#220815=CARTESIAN_POINT('Ctrl Pts',(-7.26570691397072,3.13561683107651,
46.2281926236228));
#220816=CARTESIAN_POINT('Ctrl Pts',(-7.3414877853863,2.9538531389966,46.2360939829805));
#220817=CARTESIAN_POINT('Ctrl Pts',(-7.41041732906845,2.76941076928686,
46.2439953423382));
#220818=CARTESIAN_POINT('Ctrl Pts',(-7.47931138270548,2.58506336419856,
46.2518926334897));
#220819=CARTESIAN_POINT('Ctrl Pts',(-7.54136101623707,2.39804034864094,
46.2597899246412));
#220820=CARTESIAN_POINT('Ctrl Pts',(-7.59636229280378,2.20889133197376,
46.2676872157926));
#220821=CARTESIAN_POINT('Ctrl Pts',(-7.65134487076883,2.01980661967077,
46.2755818221282));
#220822=CARTESIAN_POINT('Ctrl Pts',(-7.69928377003174,1.82859767441595,
46.2834764284638));
#220823=CARTESIAN_POINT('Ctrl Pts',(-7.74002453821444,1.63583041536658,
46.2913710347994));
#220824=CARTESIAN_POINT('Ctrl Pts',(-7.76863330987008,1.50046638707689,
46.2969147444554));
#220825=CARTESIAN_POINT('Ctrl Pts',(-7.79369367148229,1.3643343046367,46.3024584541113));
#220826=CARTESIAN_POINT('Ctrl Pts',(-7.81516706782015,1.22763378173597,
46.3080021637673));
#220827=CARTESIAN_POINT('Ctrl Pts',(-7.845367225673,1.03537833666277,46.3157988301198));
#220828=CARTESIAN_POINT('Ctrl Pts',(-7.8684564505306,0.842086412083351,
46.3235954964722));
#220829=CARTESIAN_POINT('Ctrl Pts',(-7.88438896608291,0.648329878619016,
46.3313921628247));
#220830=CARTESIAN_POINT('Ctrl Pts',(-7.90033187838918,0.454446909438875,
46.3391939168874));
#220831=CARTESIAN_POINT('Ctrl Pts',(-7.90910873931268,0.260099077667802,
46.34699567095));
#220832=CARTESIAN_POINT('Ctrl Pts',(-7.91072585228101,0.0658596238445143,
46.3547974250127));
#220833=CARTESIAN_POINT('Ctrl Pts',(-7.91092421960704,0.0420327411094098,
46.3557544472629));
#220834=CARTESIAN_POINT('Ctrl Pts',(-7.91101491610168,0.0182074856072361,
46.3567114695131));
#220835=CARTESIAN_POINT('Ctrl Pts',(-7.91099800725439,-0.00561508833863839,
46.3576684917633));
#220836=CARTESIAN_POINT('',(-7.919264176172,0.00076404157701636,48.3576684917633));
#220837=CARTESIAN_POINT('Ctrl Pts',(-7.9087893072687,-0.00562351359541763,
46.3576688933213));
#220838=CARTESIAN_POINT('Ctrl Pts',(-7.91252992283379,-0.912183692134236,
46.3940981054115));
#220839=CARTESIAN_POINT('Ctrl Pts',(-7.33081702863261,-4.44677843272281,
46.5364968947182));
#220840=CARTESIAN_POINT('Ctrl Pts',(-2.13546797111051,-9.11796621008134,
46.7848652612416));
#220841=CARTESIAN_POINT('Ctrl Pts',(6.52665753302942,-6.70593118787837,
47.1027739928909));
#220842=CARTESIAN_POINT('Ctrl Pts',(8.71102287534456,0.400901934475626,
47.3676979359323));
#220843=CARTESIAN_POINT('Ctrl Pts',(6.30989378669818,5.29249576291848,47.5796370903652));
#220844=CARTESIAN_POINT('Ctrl Pts',(3.0142647445543,7.68314273743952,47.7385914561901));
#220845=CARTESIAN_POINT('Ctrl Pts',(-1.01938237615656,8.17228174075617,
47.8975458220149));
#220846=CARTESIAN_POINT('Ctrl Pts',(-5.98723647190021,6.26859805905107,
48.1039048338725));
#220847=CARTESIAN_POINT('Ctrl Pts',(-7.90588447844806,2.48564124360112,
48.2572790571221));
#220848=CARTESIAN_POINT('Ctrl Pts',(-7.919264176172,0.00076404157701636,
48.3576684917633));
#220849=CARTESIAN_POINT('',(-7.91099885442289,0.00182802643405098,52.3592849490288));
#220850=CARTESIAN_POINT('Ctrl Pts',(-7.91099999257641,0.000342718611354188,
48.3529178502397));
#220851=CARTESIAN_POINT('Ctrl Pts',(-7.91100661574924,-0.152540487811379,
48.3586348317909));
#220852=CARTESIAN_POINT('Ctrl Pts',(-7.90658148115475,-0.305390842585058,
48.3645117988981));
#220853=CARTESIAN_POINT('Ctrl Pts',(-7.89699780615803,-0.470644912774039,
48.3711132231136));
#220854=CARTESIAN_POINT('Ctrl Pts',(-7.89623522578758,-0.483270359723247,
48.3716190656282));
#220855=CARTESIAN_POINT('Ctrl Pts',(-7.89496833725055,-0.503441299715581,
48.3724295463481));
#220856=CARTESIAN_POINT('Ctrl Pts',(-7.89448348037355,-0.51098802917705,
48.3727332989232));
#220857=CARTESIAN_POINT('Ctrl Pts',(-7.89363240401814,-0.523944529531292,
48.3732556724732));
#220858=CARTESIAN_POINT('Ctrl Pts',(-7.89327144179119,-0.529354650288003,
48.3734740584775));
#220859=CARTESIAN_POINT('Ctrl Pts',(-7.89258197691212,-0.539530871591092,
48.3738853241614));
#220860=CARTESIAN_POINT('Ctrl Pts',(-7.89225471827215,-0.544297056250423,
48.374078148934));
#220861=CARTESIAN_POINT('Ctrl Pts',(-7.8915630985206,-0.554238011260211,
48.3744807466072));
#220862=CARTESIAN_POINT('Ctrl Pts',(-7.89119796448472,-0.5594127243683,
48.3746905530849));
#220863=CARTESIAN_POINT('Ctrl Pts',(-7.89034505126172,-0.571333279638533,
48.3751744054809));
#220864=CARTESIAN_POINT('Ctrl Pts',(-7.88985371088079,-0.578078856981754,
48.375448604309));
#220865=CARTESIAN_POINT('Ctrl Pts',(-7.88826100268444,-0.599564710918577,
48.3763232246957));
#220866=CARTESIAN_POINT('Ctrl Pts',(-7.88712697675256,-0.614302480473204,
48.3769250246693));
#220867=CARTESIAN_POINT('Ctrl Pts',(-7.87670620086609,-0.744943040559715,
48.3822756802667));
#220868=CARTESIAN_POINT('Ctrl Pts',(-7.86490678359015,-0.860627858398803,
48.3871259461307));
#220869=CARTESIAN_POINT('Ctrl Pts',(-7.84570162601393,-1.01510558565293,
48.3937177240286));
#220870=CARTESIAN_POINT('Ctrl Pts',(-7.84054873943716,-1.05416733342591,
48.3953944606311));
#220871=CARTESIAN_POINT('Ctrl Pts',(-7.83045833566371,-1.12648730171445,
48.3985154460787));
#220872=CARTESIAN_POINT('Ctrl Pts',(-7.82560015480292,-1.15975582612675,
48.3999576987699));
#220873=CARTESIAN_POINT('Ctrl Pts',(-7.71367378093027,-1.89347697473503,
48.4318978521123));
#220874=CARTESIAN_POINT('Ctrl Pts',(-7.51319161944449,-2.57645980247717,
48.463848760742));
#220875=CARTESIAN_POINT('Ctrl Pts',(-7.14652961386596,-3.3981688616766,
48.5017989064571));
#220876=CARTESIAN_POINT('Ctrl Pts',(-7.06236223474376,-3.56980125007885,
48.5097265543574));
#220877=CARTESIAN_POINT('Ctrl Pts',(-6.95046144749486,-3.77850443661812,
48.5193885177295));
#220878=CARTESIAN_POINT('Ctrl Pts',(-6.92851456981222,-3.81859869865115,
48.5212458626885));
#220879=CARTESIAN_POINT('Ctrl Pts',(-6.8889585147471,-3.88939896178052,
48.5245285959484));
#220880=CARTESIAN_POINT('Ctrl Pts',(-6.87148847872423,-3.92018109442377,
48.5259568473936));
#220881=CARTESIAN_POINT('Ctrl Pts',(-6.84547039708444,-3.96531651357632,
48.528052946124));
#220882=CARTESIAN_POINT('Ctrl Pts',(-6.83708259566889,-3.97976149947496,
48.5287240594627));
#220883=CARTESIAN_POINT('Ctrl Pts',(-6.82217211084606,-4.00525320805384,
48.5299089619354));
#220884=CARTESIAN_POINT('Ctrl Pts',(-6.81566819705766,-4.01631081956556,
48.5304231273273));
#220885=CARTESIAN_POINT('Ctrl Pts',(-6.80289571202452,-4.0379055530394,
48.5314276503735));
#220886=CARTESIAN_POINT('Ctrl Pts',(-6.79662948550272,-4.04844401735975,
48.5319180529909));
#220887=CARTESIAN_POINT('Ctrl Pts',(-6.78144746443217,-4.07384236225726,
48.5331004310319));
#220888=CARTESIAN_POINT('Ctrl Pts',(-6.77250728407431,-4.08868761281229,
48.5337919230438));
#220889=CARTESIAN_POINT('Ctrl Pts',(-6.74485538591721,-4.1342643074334,
48.5359162262893));
#220890=CARTESIAN_POINT('Ctrl Pts',(-6.72598264041988,-4.1648977279389,
48.5373459514208));
#220891=CARTESIAN_POINT('Ctrl Pts',(-6.51753243772125,-4.49813282197162,
48.5529221407399));
#220892=CARTESIAN_POINT('Ctrl Pts',(-6.30787906436848,-4.78770396647052,
48.566641454316));
#220893=CARTESIAN_POINT('Ctrl Pts',(-5.76291319535767,-5.44218113988198,
48.5986218239133));
#220894=CARTESIAN_POINT('Ctrl Pts',(-5.41152229067082,-5.79171153527603,
48.616493264834));
#220895=CARTESIAN_POINT('Ctrl Pts',(-4.87011634372129,-6.23768315747306,
48.6425651874563));
#220896=CARTESIAN_POINT('Ctrl Pts',(-4.70533327230349,-6.36290484720138,
48.65034589399));
#220897=CARTESIAN_POINT('Ctrl Pts',(-4.4720880165956,-6.52613239690935,
48.6613578592977));
#220898=CARTESIAN_POINT('Ctrl Pts',(-4.40768484202316,-6.56980130598483,
48.664398523612));
#220899=CARTESIAN_POINT('Ctrl Pts',(-4.31831240962476,-6.62849505238604,
48.6686299082087));
#220900=CARTESIAN_POINT('Ctrl Pts',(-4.29388776915809,-6.64434319754351,
48.6697875039874));
#220901=CARTESIAN_POINT('Ctrl Pts',(-4.25741760587972,-6.66772210806573,
48.6715184502886));
#220902=CARTESIAN_POINT('Ctrl Pts',(-4.24543824605021,-6.67535593635639,
48.672087406372));
#220903=CARTESIAN_POINT('Ctrl Pts',(-4.22363483013553,-6.6891676985892,
48.6731237611976));
#220904=CARTESIAN_POINT('Ctrl Pts',(-4.21381760120947,-6.69535636841934,
48.6735906877806));
#220905=CARTESIAN_POINT('Ctrl Pts',(-4.19832699576839,-6.7050739053632,
48.6743279637802));
#220906=CARTESIAN_POINT('Ctrl Pts',(-4.19266268389706,-6.70861723893145,
48.6745976646051));
#220907=CARTESIAN_POINT('Ctrl Pts',(-4.18247363878874,-6.71497309334601,
48.6750830097549));
#220908=CARTESIAN_POINT('Ctrl Pts',(-4.17795053635783,-6.71778822969965,
48.6752985352102));
#220909=CARTESIAN_POINT('Ctrl Pts',(-4.16759861972971,-6.72421666634182,
48.6757919740803));
#220910=CARTESIAN_POINT('Ctrl Pts',(-4.16176794872268,-6.72782695761993,
48.676070025062));
#220911=CARTESIAN_POINT('Ctrl Pts',(-4.14581290907523,-6.7376774756889,
48.67683123804));
#220912=CARTESIAN_POINT('Ctrl Pts',(-4.13567917643111,-6.74390244524758,
48.6773151069841));
#220913=CARTESIAN_POINT('Ctrl Pts',(-4.08656069818263,-6.77392269573197,
48.6796624711196));
#220914=CARTESIAN_POINT('Ctrl Pts',(-4.04738496354369,-6.7974025817451,
48.6815408735513));
#220915=CARTESIAN_POINT('Ctrl Pts',(-3.6679549366365,-7.02037004560078,
48.6998107317642));
#220916=CARTESIAN_POINT('Ctrl Pts',(-3.31348985693382,-7.19445401575491,
48.7176023183945));
#220917=CARTESIAN_POINT('Ctrl Pts',(-2.9141862889199,-7.35477635369745,
48.7373327793731));
#220918=CARTESIAN_POINT('Ctrl Pts',(-2.88068818691423,-7.36796121709828,
48.738985779723));
#220919=CARTESIAN_POINT('Ctrl Pts',(-2.80985012154015,-7.39528616231137,
48.7424753433348));
#220920=CARTESIAN_POINT('Ctrl Pts',(-2.77249070714876,-7.40937314467989,
48.7443122092073));
#220921=CARTESIAN_POINT('Ctrl Pts',(-2.69292466414668,-7.4386887908924,
48.7482150643918));
#220922=CARTESIAN_POINT('Ctrl Pts',(-2.65069181886143,-7.45384243552452,
48.7502812025828));
#220923=CARTESIAN_POINT('Ctrl Pts',(-2.56010914456161,-7.48547735812721,
48.7546986866358));
#220924=CARTESIAN_POINT('Ctrl Pts',(-2.51172387818537,-7.50185132387944,
48.7570498189509));
#220925=CARTESIAN_POINT('Ctrl Pts',(-2.40702621195399,-7.53615538552259,
48.7621156655851));
#220926=CARTESIAN_POINT('Ctrl Pts',(-2.35066444220565,-7.55392546382175,
48.7648293831232));
#220927=CARTESIAN_POINT('Ctrl Pts',(-2.22715058391424,-7.59135141477335,
48.7707424381434));
#220928=CARTESIAN_POINT('Ctrl Pts',(-2.15992583994453,-7.61075137773288,
48.7739390257932));
#220929=CARTESIAN_POINT('Ctrl Pts',(-2.00949524559602,-7.65200949873924,
48.7810366857959));
#220930=CARTESIAN_POINT('Ctrl Pts',(-1.92617181449688,-7.67340752345283,
48.7849306016099));
#220931=CARTESIAN_POINT('Ctrl Pts',(-1.54067935108595,-7.7657297325216,
48.8027503669159));
#220932=CARTESIAN_POINT('Ctrl Pts',(-1.23483391434615,-7.82019585537871,
48.8163241561035));
#220933=CARTESIAN_POINT('Ctrl Pts',(-0.802353418988295,-7.87120008959691,
48.8345719702348));
#220934=CARTESIAN_POINT('Ctrl Pts',(-0.677817434831919,-7.8829009458555,
48.839720123879));
#220935=CARTESIAN_POINT('Ctrl Pts',(-0.535937842065803,-7.89284397233831,
48.845465888752));
#220936=CARTESIAN_POINT('Ctrl Pts',(-0.518819484888331,-7.89398769249893,
48.8461571756467));
#220937=CARTESIAN_POINT('Ctrl Pts',(-0.493046164904217,-7.89562547405645,
48.847195035469));
#220938=CARTESIAN_POINT('Ctrl Pts',(-0.484393944219274,-7.89616100739766,
48.8475429514724));
#220939=CARTESIAN_POINT('Ctrl Pts',(-0.469491370421446,-7.89705882279947,
48.8481413462082));
#220940=CARTESIAN_POINT('Ctrl Pts',(-0.463241444858093,-7.89742790797418,
48.848392045345));
#220941=CARTESIAN_POINT('Ctrl Pts',(-0.450350636799203,-7.89817381089004,
48.8489085929236));
#220942=CARTESIAN_POINT('Ctrl Pts',(-0.443709703530657,-7.8985496733487,
48.8491744101444));
#220943=CARTESIAN_POINT('Ctrl Pts',(-0.427691631236518,-7.89943599629352,
48.8498148655461));
#220944=CARTESIAN_POINT('Ctrl Pts',(-0.418314030716937,-7.89993813668887,
48.8501892333271));
#220945=CARTESIAN_POINT('Ctrl Pts',(-0.389442718001976,-7.9014325509617,
48.8513400421727));
#220946=CARTESIAN_POINT('Ctrl Pts',(-0.369946140895122,-7.90236938190622,
48.8521146810402));
#220947=CARTESIAN_POINT('Ctrl Pts',(-0.143619541678384,-7.91240518455315,
48.8610784356172));
#220948=CARTESIAN_POINT('Ctrl Pts',(0.0634951013188367,-7.91345428530354,
48.8690003584402));
#220949=CARTESIAN_POINT('Ctrl Pts',(0.958808634332102,-7.88283171187693,
48.9022430620205));
#220950=CARTESIAN_POINT('Ctrl Pts',(1.64112210893485,-7.76949561552535,
48.9247075830862));
#220951=CARTESIAN_POINT('Ctrl Pts',(2.55939489953236,-7.49044948587877,
48.9572919195504));
#220952=CARTESIAN_POINT('Ctrl Pts',(2.8144105518948,-7.39840622688852,48.9666562515675));
#220953=CARTESIAN_POINT('Ctrl Pts',(3.18828566343891,-7.24133096905835,
48.9814903459293));
#220954=CARTESIAN_POINT('Ctrl Pts',(3.31102771276401,-7.18603729132512,
48.9865472699021));
#220955=CARTESIAN_POINT('Ctrl Pts',(3.48456177873523,-7.10247250317492,
48.9940452198641));
#220956=CARTESIAN_POINT('Ctrl Pts',(3.53655007621673,-7.07672944793297,
48.996337293225));
#220957=CARTESIAN_POINT('Ctrl Pts',(3.59618510664614,-7.04637871312041,
48.9990246692971));
#220958=CARTESIAN_POINT('Ctrl Pts',(3.60411408443478,-7.04232645899623,
48.9993831733879));
#220959=CARTESIAN_POINT('Ctrl Pts',(3.61536070831833,-7.03655469048941,
48.9998934031931));
#220960=CARTESIAN_POINT('Ctrl Pts',(3.61868402995509,-7.03484618557877,
49.0000443871616));
#220961=CARTESIAN_POINT('Ctrl Pts',(3.62537367615581,-7.03140107348601,
49.0003487414055));
#220962=CARTESIAN_POINT('Ctrl Pts',(3.62873996635609,-7.02966440197925,
49.0005021160366));
#220963=CARTESIAN_POINT('Ctrl Pts',(3.63521377196227,-7.02631867181486,
49.0007975023784));
#220964=CARTESIAN_POINT('Ctrl Pts',(3.63832147032344,-7.02470996726983,
49.0009394898793));
#220965=CARTESIAN_POINT('Ctrl Pts',(3.64566064517282,-7.02090465615061,
49.0012752596173));
#220966=CARTESIAN_POINT('Ctrl Pts',(3.64989117851192,-7.01870629925154,
49.0014691627196));
#220967=CARTESIAN_POINT('Ctrl Pts',(3.66257068361196,-7.0121029496636,49.0020513784108));
#220968=CARTESIAN_POINT('Ctrl Pts',(3.67101365357332,-7.00768653285817,
49.0024404738746));
#220969=CARTESIAN_POINT('Ctrl Pts',(3.75204687743676,-6.96511238904207,
49.0061883098611));
#220970=CARTESIAN_POINT('Ctrl Pts',(3.82404517609923,-6.92584463465615,
49.0096217384498));
#220971=CARTESIAN_POINT('Ctrl Pts',(4.10019653383469,-6.76961341188309,
49.023150644087));
#220972=CARTESIAN_POINT('Ctrl Pts',(4.29969268660219,-6.64469000790777,
49.0336938035138));
#220973=CARTESIAN_POINT('Ctrl Pts',(4.81087167482887,-6.29192386670885,
49.0621469682306));
#220974=CARTESIAN_POINT('Ctrl Pts',(5.11197234620048,-6.04983747216701,
49.0803915568301));
#220975=CARTESIAN_POINT('Ctrl Pts',(5.79360790095394,-5.41444004763659,
49.1235575187725));
#220976=CARTESIAN_POINT('Ctrl Pts',(6.15343820265702,-5.00174152867317,
49.1479000756468));
#220977=CARTESIAN_POINT('Ctrl Pts',(6.49767599167211,-4.51295882524471,
49.1723497541839));
#220978=CARTESIAN_POINT('Ctrl Pts',(6.52701293761932,-4.47042424230836,
49.1744457630141));
#220979=CARTESIAN_POINT('Ctrl Pts',(6.56317149771846,-4.41688444873617,
49.1770452393478));
#220980=CARTESIAN_POINT('Ctrl Pts',(6.57038523763264,-4.40614640851522,
49.1775646616262));
#220981=CARTESIAN_POINT('Ctrl Pts',(6.58176998967304,-4.38910946259454,
49.1783857293413));
#220982=CARTESIAN_POINT('Ctrl Pts',(6.58595835720279,-4.38282221738789,
49.1786880780354));
#220983=CARTESIAN_POINT('Ctrl Pts',(6.59379725704169,-4.3710184729439,49.1792544867366));
#220984=CARTESIAN_POINT('Ctrl Pts',(6.59744988676893,-4.36550337872447,
49.179518631434));
#220985=CARTESIAN_POINT('Ctrl Pts',(6.60560174291223,-4.35316131842645,
49.1801086382622));
#220986=CARTESIAN_POINT('Ctrl Pts',(6.61009731478669,-4.34633194082252,
49.180434352858));
#220987=CARTESIAN_POINT('Ctrl Pts',(6.62142130366424,-4.32907107378963,
49.1812556644296));
#220988=CARTESIAN_POINT('Ctrl Pts',(6.6282356752216,-4.31863037064045,49.1817506963699));
#220989=CARTESIAN_POINT('Ctrl Pts',(6.66460157881149,-4.26262318136732,
49.1843968292002));
#220990=CARTESIAN_POINT('Ctrl Pts',(6.69370832717306,-4.21676885540567,
49.1865301064493));
#220991=CARTESIAN_POINT('Ctrl Pts',(7.18236075874533,-3.42914255465011,
49.2226236523381));
#220992=CARTESIAN_POINT('Ctrl Pts',(7.51647601648318,-2.6168184078806,49.2506467358803));
#220993=CARTESIAN_POINT('Ctrl Pts',(7.76012010158495,-1.55315726001384,
49.288681172093));
#220994=CARTESIAN_POINT('Ctrl Pts',(7.80009135965436,-1.33803083913816,
49.2964923040738));
#220995=CARTESIAN_POINT('Ctrl Pts',(7.84739975800822,-1.00770155530242,
49.3090344547507));
#220996=CARTESIAN_POINT('Ctrl Pts',(7.86121808071381,-0.893528611771507,
49.3134685427911));
#220997=CARTESIAN_POINT('Ctrl Pts',(7.8744931619752,-0.759388439814313,
49.3188372586612));
#220998=CARTESIAN_POINT('Ctrl Pts',(7.87636987804081,-0.739669456558147,
49.3196305034297));
#220999=CARTESIAN_POINT('Ctrl Pts',(7.87875954302258,-0.713519916311099,
49.3206879967775));
#221000=CARTESIAN_POINT('Ctrl Pts',(7.87933870628537,-0.707095579741262,
49.3209482394462));
#221001=CARTESIAN_POINT('Ctrl Pts',(7.88023410046405,-0.697025760990089,
49.321356840038));
#221002=CARTESIAN_POINT('Ctrl Pts',(7.88055566156894,-0.693380742756694,
49.3215048833921));
#221003=CARTESIAN_POINT('Ctrl Pts',(7.88121598036788,-0.685835981546097,
49.3218116044132));
#221004=CARTESIAN_POINT('Ctrl Pts',(7.881554372733,-0.681936208406209,49.3219703034383));
#221005=CARTESIAN_POINT('Ctrl Pts',(7.88231206479833,-0.673128352011628,
49.3223290919668));
#221006=CARTESIAN_POINT('Ctrl Pts',(7.88272967468943,-0.668220128954483,
49.3225292796412));
#221007=CARTESIAN_POINT('Ctrl Pts',(7.8837866334746,-0.65565867543255,49.323042249917));
#221008=CARTESIAN_POINT('Ctrl Pts',(7.88441942124602,-0.648004915003598,
49.3233554100142));
#221009=CARTESIAN_POINT('Ctrl Pts',(7.88795309570027,-0.604492529093342,
49.3251391459016));
#221010=CARTESIAN_POINT('Ctrl Pts',(7.89062045419689,-0.568615886238823,
49.3266229476336));
#221011=CARTESIAN_POINT('Ctrl Pts',(7.90138341779411,-0.409147349534968,
49.3332726872491));
#221012=CARTESIAN_POINT('Ctrl Pts',(7.90682024283162,-0.285398510364241,
49.3385778210243));
#221013=CARTESIAN_POINT('Ctrl Pts',(7.91122346572789,-0.0698592169688464,
49.3480116480563));
#221014=CARTESIAN_POINT('Ctrl Pts',(7.91150157955322,0.0218839090433246,
49.3520881194122));
#221015=CARTESIAN_POINT('Ctrl Pts',(7.90001394010572,0.821729758698371,
49.3880471709652));
#221016=CARTESIAN_POINT('Ctrl Pts',(7.79481102396731,1.52529913615493,49.4222083583846));
#221017=CARTESIAN_POINT('Ctrl Pts',(7.49231567967891,2.56730278294983,49.4707495100454));
#221018=CARTESIAN_POINT('Ctrl Pts',(7.36157543239759,2.92114643119724,49.4869112064786));
#221019=CARTESIAN_POINT('Ctrl Pts',(7.19421130595928,3.29060401180695,49.5033888048121));
#221020=CARTESIAN_POINT('Ctrl Pts',(7.1821794788057,3.31678293447481,49.5045543432817));
#221021=CARTESIAN_POINT('Ctrl Pts',(7.16536237469439,3.35285307468195,49.5061575634714));
#221022=CARTESIAN_POINT('Ctrl Pts',(7.16069917739773,3.36280076620141,49.5065994271673));
#221023=CARTESIAN_POINT('Ctrl Pts',(7.15279799122516,3.37956488973098,49.5073435964196));
#221024=CARTESIAN_POINT('Ctrl Pts',(7.14957095061672,3.38638644718539,49.5076462773202));
#221025=CARTESIAN_POINT('Ctrl Pts',(7.14317094308289,3.39986533045488,49.5082440940921));
#221026=CARTESIAN_POINT('Ctrl Pts',(7.1399984185725,3.40652285629643,49.5085392447022));
#221027=CARTESIAN_POINT('Ctrl Pts',(7.13299188686917,3.42117323835114,49.5091884746106));
#221028=CARTESIAN_POINT('Ctrl Pts',(7.12915374228704,3.42916411162583,49.5095424112388));
#221029=CARTESIAN_POINT('Ctrl Pts',(7.11573851096625,3.4569742501357,49.5107735848593));
#221030=CARTESIAN_POINT('Ctrl Pts',(7.10609210361164,3.47676006469464,49.511648435281));
#221031=CARTESIAN_POINT('Ctrl Pts',(7.00945630452051,3.67288809452217,49.5203101663974));
#221032=CARTESIAN_POINT('Ctrl Pts',(6.91600070138897,3.84597520775397,49.5278692045383));
#221033=CARTESIAN_POINT('Ctrl Pts',(6.48971679090423,4.56959566521287,49.5593190800551));
#221034=CARTESIAN_POINT('Ctrl Pts',(6.09689795915771,5.08187614184098,49.5809863835182));
#221035=CARTESIAN_POINT('Ctrl Pts',(5.5038362838196,5.68622301205579,49.6106286371034));
#221036=CARTESIAN_POINT('Ctrl Pts',(5.35573175650464,5.82593153716105,49.6178479706202));
#221037=CARTESIAN_POINT('Ctrl Pts',(5.144136819712,6.01063730125885,49.6281469277709));
#221038=CARTESIAN_POINT('Ctrl Pts',(5.08512139320036,6.06064718944004,49.6310179914204));
#221039=CARTESIAN_POINT('Ctrl Pts',(4.92297921660238,6.19401143922407,49.6389281361451));
#221040=CARTESIAN_POINT('Ctrl Pts',(4.81848699848259,6.27564194572297,49.644060491067));
#221041=CARTESIAN_POINT('Ctrl Pts',(4.69663331035553,6.36599733077107,49.6500871031609));
#221042=CARTESIAN_POINT('Ctrl Pts',(4.68123603394261,6.37732825360064,49.650849158632));
#221043=CARTESIAN_POINT('Ctrl Pts',(4.65692972641367,6.39507991474747,49.6520528362937));
#221044=CARTESIAN_POINT('Ctrl Pts',(4.64804808264866,6.40153814428547,49.6524928099804));
#221045=CARTESIAN_POINT('Ctrl Pts',(4.63303220259765,6.41240911909503,49.6532368684981));
#221046=CARTESIAN_POINT('Ctrl Pts',(4.62690502448526,6.41683161653042,49.6535405380033));
#221047=CARTESIAN_POINT('Ctrl Pts',(4.61486127033237,6.42549838341937,49.6541375430188));
#221048=CARTESIAN_POINT('Ctrl Pts',(4.60894515104571,6.42974327745645,49.6544308521191));
#221049=CARTESIAN_POINT('Ctrl Pts',(4.59763868522363,6.4378321935656,49.6549914865852));
#221050=CARTESIAN_POINT('Ctrl Pts',(4.5922493550361,6.44167763034238,49.6552587540299));
#221051=CARTESIAN_POINT('Ctrl Pts',(4.57980057475314,6.45053661853814,49.6558761868436));
#221052=CARTESIAN_POINT('Ctrl Pts',(4.57273771412904,6.45554535022041,49.6562265439412));
#221053=CARTESIAN_POINT('Ctrl Pts',(4.55165348068188,6.47044558223827,49.6572725739305));
#221054=CARTESIAN_POINT('Ctrl Pts',(4.53760817494482,6.48030303973213,49.6579695664457));
#221055=CARTESIAN_POINT('Ctrl Pts',(4.43694161994981,6.55046640374775,49.6629658732885));
#221056=CARTESIAN_POINT('Ctrl Pts',(4.34915486146927,6.60907800669358,49.6673268371874));
#221057=CARTESIAN_POINT('Ctrl Pts',(3.88349400070891,6.9066845115384,49.690400873529));
#221058=CARTESIAN_POINT('Ctrl Pts',(3.48703597589635,7.11508183160246,49.7097881305069));
#221059=CARTESIAN_POINT('Ctrl Pts',(2.54662273391097,7.51183341385169,49.7536213046553));
#221060=CARTESIAN_POINT('Ctrl Pts',(1.99543921507439,7.67666592210404,49.7777368059601));
#221061=CARTESIAN_POINT('Ctrl Pts',(1.15421249347565,7.83141581900206,49.8130058032926));
#221062=CARTESIAN_POINT('Ctrl Pts',(0.874621814571236,7.86754873002635,
49.8245534133192));
#221063=CARTESIAN_POINT('Ctrl Pts',(0.550173865377027,7.89196647060808,
49.8377225142882));
#221064=CARTESIAN_POINT('Ctrl Pts',(0.506623502239162,7.89488180459686,
49.839485464602));
#221065=CARTESIAN_POINT('Ctrl Pts',(0.439345026522528,7.89882654939033,
49.842201726678));
#221066=CARTESIAN_POINT('Ctrl Pts',(0.415632774466015,7.90010976574574,
49.8431576891077));
#221067=CARTESIAN_POINT('Ctrl Pts',(0.373961018304702,7.90217674425358,
49.8448352900434));
#221068=CARTESIAN_POINT('Ctrl Pts',(0.356003968542585,7.90300609369197,
49.845557413228));
#221069=CARTESIAN_POINT('Ctrl Pts',(0.315107312811892,7.90475524261024,
49.8472002650276));
#221070=CARTESIAN_POINT('Ctrl Pts',(0.292166199282699,7.9056364057672,49.8481205656482));
#221071=CARTESIAN_POINT('Ctrl Pts',(0.23033713514553,7.90774174803181,49.8505975449528));
#221072=CARTESIAN_POINT('Ctrl Pts',(0.191443376698478,7.9087789324712,49.8521521330745));
#221073=CARTESIAN_POINT('Ctrl Pts',(0.00458423463766006,7.9123827036578,
49.8596044685682));
#221074=CARTESIAN_POINT('Ctrl Pts',(-0.14342747607543,7.91108403921816,
49.8654573361658));
#221075=CARTESIAN_POINT('Ctrl Pts',(-0.304709530693521,7.90514090296338,
49.871794149227));
#221076=CARTESIAN_POINT('Ctrl Pts',(-0.318100437902277,7.90461338117633,
49.8723199797568));
#221077=CARTESIAN_POINT('Ctrl Pts',(-1.02673932222282,7.87489360253939,
49.9001313274641));
#221078=CARTESIAN_POINT('Ctrl Pts',(-1.71506856455189,7.75413479406379,
49.9260768847217));
#221079=CARTESIAN_POINT('Ctrl Pts',(-2.42154685907048,7.53140441058269,
49.9553849848351));
#221080=CARTESIAN_POINT('Ctrl Pts',(-2.46430143181564,7.51752352732088,
49.9571706617528));
#221081=CARTESIAN_POINT('Ctrl Pts',(-2.53692159645602,7.49326026388894,
49.9602266022773));
#221082=CARTESIAN_POINT('Ctrl Pts',(-2.56684766294533,7.48306178161918,
49.9614925989072));
#221083=CARTESIAN_POINT('Ctrl Pts',(-2.60945912356887,7.46825456194679,
49.9633054870285));
#221084=CARTESIAN_POINT('Ctrl Pts',(-2.62219519606525,7.463792298262,49.9638486442149));
#221085=CARTESIAN_POINT('Ctrl Pts',(-2.64457279545448,7.45588764250573,
49.9648052420404));
#221086=CARTESIAN_POINT('Ctrl Pts',(-2.65421918854743,7.45245907781669,
49.9652183454056));
#221087=CARTESIAN_POINT('Ctrl Pts',(-2.67298221972546,7.44574918547511,
49.966023285584));
#221088=CARTESIAN_POINT('Ctrl Pts',(-2.6820995410196,7.44246981394094,49.9664150755907));
#221089=CARTESIAN_POINT('Ctrl Pts',(-2.70645963948871,7.43365725455341,
49.9674636055986));
#221090=CARTESIAN_POINT('Ctrl Pts',(-2.7216914419776,7.42809394463044,49.9681210370287));
#221091=CARTESIAN_POINT('Ctrl Pts',(-2.77694172355167,7.40772140767843,
49.9705121724703));
#221092=CARTESIAN_POINT('Ctrl Pts',(-2.81685711203906,7.39263537272083,
49.9722519241893));
#221093=CARTESIAN_POINT('Ctrl Pts',(-3.2356632050271,7.23046310318623,49.9906282851724));
#221094=CARTESIAN_POINT('Ctrl Pts',(-3.60279850662276,7.05471090422539,
50.0077673043186));
#221095=CARTESIAN_POINT('Ctrl Pts',(-4.23543921280448,6.68954246540859,
50.0384355816507));
#221096=CARTESIAN_POINT('Ctrl Pts',(-4.50587094352013,6.51045764238882,
50.0519689907399));
#221097=CARTESIAN_POINT('Ctrl Pts',(-4.9022445261573,6.21141422585282,50.0724063327205));
#221098=CARTESIAN_POINT('Ctrl Pts',(-5.03649660314221,6.10306248354741,
50.0794474542288));
#221099=CARTESIAN_POINT('Ctrl Pts',(-5.20087533890208,5.96127554062813,
50.0882367416149));
#221100=CARTESIAN_POINT('Ctrl Pts',(-5.23440243413324,5.93185818673869,
50.0900386748054));
#221101=CARTESIAN_POINT('Ctrl Pts',(-5.28776368598536,5.88423324802794,
50.0929220874912));
#221102=CARTESIAN_POINT('Ctrl Pts',(-5.30775670867709,5.86620528480842,
50.0940059690077));
#221103=CARTESIAN_POINT('Ctrl Pts',(-5.345615820904,5.83171524187965,50.096065358478));
#221104=CARTESIAN_POINT('Ctrl Pts',(-5.36349885759869,5.81527223575232,
50.097041108542));
#221105=CARTESIAN_POINT('Ctrl Pts',(-5.40419455632999,5.77750614585633,
50.0992685795209));
#221106=CARTESIAN_POINT('Ctrl Pts',(-5.42695729807266,5.75612982496213,
50.100519572694));
#221107=CARTESIAN_POINT('Ctrl Pts',(-5.49731689498937,5.68926729310164,
50.104402742031));
#221108=CARTESIAN_POINT('Ctrl Pts',(-5.54447306914706,5.64332117096459,
50.1070288060158));
#221109=CARTESIAN_POINT('Ctrl Pts',(-5.69019741966563,5.49774630353738,
50.1152234795968));
#221110=CARTESIAN_POINT('Ctrl Pts',(-5.78669559525153,5.39608336162977,
50.1207664804448));
#221111=CARTESIAN_POINT('Ctrl Pts',(-6.04285138454884,5.11143956168988,
50.1358577302533));
#221112=CARTESIAN_POINT('Ctrl Pts',(-6.19686849361963,4.92358531291668,
50.1453447110581));
#221113=CARTESIAN_POINT('Ctrl Pts',(-6.88006779501779,4.00734379429515,
50.1894024851266));
#221114=CARTESIAN_POINT('Ctrl Pts',(-7.29095677095426,3.19932370315164,
50.2209451943107));
#221115=CARTESIAN_POINT('Ctrl Pts',(-7.57364965574357,2.28623773066557,
50.2585424156923));
#221116=CARTESIAN_POINT('Ctrl Pts',(-7.58963090453476,2.23261161578721,
50.2607614420685));
#221117=CARTESIAN_POINT('Ctrl Pts',(-7.60849007438963,2.16678484274719,
50.2635030380398));
#221118=CARTESIAN_POINT('Ctrl Pts',(-7.61190988036006,2.15474029478054,
50.2640054001461));
#221119=CARTESIAN_POINT('Ctrl Pts',(-7.61721833305808,2.13587358588345,
50.2647935008947));
#221120=CARTESIAN_POINT('Ctrl Pts',(-7.61912644935336,2.12905689372577,
50.2650784919022));
#221121=CARTESIAN_POINT('Ctrl Pts',(-7.62248920621045,2.11698112299754,
50.2655837985381));
#221122=CARTESIAN_POINT('Ctrl Pts',(-7.62394756113775,2.11172307813934,
50.2658039689641));
#221123=CARTESIAN_POINT('Ctrl Pts',(-7.62728579590833,2.09963866435772,
50.2663103311243));
#221124=CARTESIAN_POINT('Ctrl Pts',(-7.62916195188494,2.09281127788031,
50.2665966698636));
#221125=CARTESIAN_POINT('Ctrl Pts',(-7.63424475844412,2.07421713126053,
50.2673772232649));
#221126=CARTESIAN_POINT('Ctrl Pts',(-7.63743336093345,2.06244548886669,
50.2678721627985));
#221127=CARTESIAN_POINT('Ctrl Pts',(-7.65252025215243,2.00623312193516,
50.2702395409895));
#221128=CARTESIAN_POINT('Ctrl Pts',(-7.66405778238667,1.96169715531895,
50.2721268620331));
#221129=CARTESIAN_POINT('Ctrl Pts',(-7.83174917306884,1.29032357800861,
50.3007852269654));
#221130=CARTESIAN_POINT('Ctrl Pts',(-7.91091770692492,0.646847282851201,
50.3311032181041));
#221131=CARTESIAN_POINT('Ctrl Pts',(-7.9110781458086,-0.613265661808885,
50.3889607529025));
#221132=CARTESIAN_POINT('Ctrl Pts',(-7.83961221315099,-1.22553469161474,
50.4163053721436));
#221133=CARTESIAN_POINT('Ctrl Pts',(-7.68892047427846,-1.86171179354981,
50.4429917766574));
#221134=CARTESIAN_POINT('Ctrl Pts',(-7.67956668600615,-1.89992748100339,
50.4445889437121));
#221135=CARTESIAN_POINT('Ctrl Pts',(-7.66669637470578,-1.95086178829899,
50.4467099645235));
#221136=CARTESIAN_POINT('Ctrl Pts',(-7.66343263670222,-1.9636433596231,
50.4472415690704));
#221137=CARTESIAN_POINT('Ctrl Pts',(-7.658286695103,-1.98358784621849,50.4480700861503));
#221138=CARTESIAN_POINT('Ctrl Pts',(-7.65642638431928,-1.9907563562427,
50.4483676716273));
#221139=CARTESIAN_POINT('Ctrl Pts',(-7.65285141875138,-2.00445297235825,
50.4489358723899));
#221140=CARTESIAN_POINT('Ctrl Pts',(-7.65113847101483,-2.01098151496095,
50.4492065399394));
#221141=CARTESIAN_POINT('Ctrl Pts',(-7.64711834734946,-2.0262238857487,
50.4498380862094));
#221142=CARTESIAN_POINT('Ctrl Pts',(-7.64480462699974,-2.03493598651649,
50.4501987628552));
#221143=CARTESIAN_POINT('Ctrl Pts',(-7.6381508891065,-2.05981851448924,
50.4512280452428));
#221144=CARTESIAN_POINT('Ctrl Pts',(-7.63377440979884,-2.07597918629055,
50.4518955251838));
#221145=CARTESIAN_POINT('Ctrl Pts',(-7.60556724247679,-2.17884214348994,
50.4561376725646));
#221146=CARTESIAN_POINT('Ctrl Pts',(-7.58031069865209,-2.26514823178452,
50.4596680187682));
#221147=CARTESIAN_POINT('Ctrl Pts',(-7.50124455436533,-2.5191811308906,
50.4699831922148));
#221148=CARTESIAN_POINT('Ctrl Pts',(-7.4432980986143,-2.6855653091354,50.4766391382225));
#221149=CARTESIAN_POINT('Ctrl Pts',(-7.25853460608201,-3.16401509616062,
50.4955984443591));
#221150=CARTESIAN_POINT('Ctrl Pts',(-7.11728867606135,-3.47009130871819,
50.5074852468541));
#221151=CARTESIAN_POINT('Ctrl Pts',(-6.63093218700432,-4.36848345296698,
50.542976746542));
#221152=CARTESIAN_POINT('Ctrl Pts',(-6.22812000437783,-4.92577038368863,
50.5657375972308));
#221153=CARTESIAN_POINT('Ctrl Pts',(-5.73111295294465,-5.45342842424301,
50.59428384968));
#221154=CARTESIAN_POINT('Ctrl Pts',(-5.70332658931703,-5.48248145479456,
50.5958818908981));
#221155=CARTESIAN_POINT('Ctrl Pts',(-5.66809643280397,-5.51875994646949,
50.5979098638502));
#221156=CARTESIAN_POINT('Ctrl Pts',(-5.66085804235525,-5.52618446499029,
50.5983266162829));
#221157=CARTESIAN_POINT('Ctrl Pts',(-5.64941556507517,-5.53787510215853,
50.5989855221022));
#221158=CARTESIAN_POINT('Ctrl Pts',(-5.64522117710273,-5.54215073192017,
50.5992270740518));
#221159=CARTESIAN_POINT('Ctrl Pts',(-5.63779748682326,-5.54970104145597,
50.5996546304427));
#221160=CARTESIAN_POINT('Ctrl Pts',(-5.63457017334984,-5.55297767989755,
50.5998405131253));
#221161=CARTESIAN_POINT('Ctrl Pts',(-5.62716437177296,-5.56048356524843,
50.6002670827712));
#221162=CARTESIAN_POINT('Ctrl Pts',(-5.62298397313339,-5.56471091647651,
50.6005078855522));
#221163=CARTESIAN_POINT('Ctrl Pts',(-5.61144035032726,-5.57635790305297,
50.6011728600856));
#221164=CARTESIAN_POINT('Ctrl Pts',(-5.60406719590833,-5.58376764653519,
50.6015976259967));
#221165=CARTESIAN_POINT('Ctrl Pts',(-5.56444556777176,-5.62342836842772,
50.6038802858695));
#221166=CARTESIAN_POINT('Ctrl Pts',(-5.53193374440984,-5.65541422218535,
50.6057535686657));
#221167=CARTESIAN_POINT('Ctrl Pts',(-5.00264858932352,-6.16720558405938,
50.6362271789454));
#221168=CARTESIAN_POINT('Ctrl Pts',(-4.44541680323696,-6.58021745856812,
50.6676222125593));
#221169=CARTESIAN_POINT('Ctrl Pts',(-3.49029581516804,-7.11078553694575,
50.7148572245285));
#221170=CARTESIAN_POINT('Ctrl Pts',(-3.12459714627059,-7.27889873369191,
50.7317256310915));
#221171=CARTESIAN_POINT('Ctrl Pts',(-2.71265007469027,-7.4314767202868,
50.7495184547133));
#221172=CARTESIAN_POINT('Ctrl Pts',(-2.67752549716521,-7.44420404830618,
50.7510267054452));
#221173=CARTESIAN_POINT('Ctrl Pts',(-2.62759340962983,-7.46189772844314,
50.7531587116978));
#221174=CARTESIAN_POINT('Ctrl Pts',(-2.61285948021649,-7.46706971808667,
50.753786338776));
#221175=CARTESIAN_POINT('Ctrl Pts',(-2.58582625646578,-7.47646926780171,
50.754935212084));
#221176=CARTESIAN_POINT('Ctrl Pts',(-2.57353167521449,-7.48071018412298,
50.75545670412));
#221177=CARTESIAN_POINT('Ctrl Pts',(-2.54860953546499,-7.48923816337282,
50.7565117982853));
#221178=CARTESIAN_POINT('Ctrl Pts',(-2.5359814822688,-7.49352365411644,
50.7570453703211));
#221179=CARTESIAN_POINT('Ctrl Pts',(-2.50485960326084,-7.50399758018336,
50.7583578324285));
#221180=CARTESIAN_POINT('Ctrl Pts',(-2.48635359234213,-7.51014960790015,
50.7591360683082));
#221181=CARTESIAN_POINT('Ctrl Pts',(-2.41952424389723,-7.53209186697771,
50.7619387493956));
#221182=CARTESIAN_POINT('Ctrl Pts',(-2.37107127965403,-7.54748478093516,
50.7639563930259));
#221183=CARTESIAN_POINT('Ctrl Pts',(-2.10741176231317,-7.62845661047556,
50.7748600864445));
#221184=CARTESIAN_POINT('Ctrl Pts',(-1.88962625364266,-7.68530107065886,
50.7835902013705));
#221185=CARTESIAN_POINT('Ctrl Pts',(-1.35922573791527,-7.7998282154574,
50.8042984441705));
#221186=CARTESIAN_POINT('Ctrl Pts',(-1.04498338704565,-7.84811016597931,
50.8161073988341));
#221187=CARTESIAN_POINT('Ctrl Pts',(-0.207903721103711,-7.92554276268818,
50.8470925886929));
#221188=CARTESIAN_POINT('Ctrl Pts',(0.316337605352563,-7.92195174394789,
50.865972636626));
#221189=CARTESIAN_POINT('Ctrl Pts',(0.928553727129594,-7.85686367788499,
50.8899343797249));
#221190=CARTESIAN_POINT('Ctrl Pts',(1.02057731670896,-7.84544071648079,
50.8935900097282));
#221191=CARTESIAN_POINT('Ctrl Pts',(1.12726926054586,-7.83028807118377,
50.8979081171873));
#221192=CARTESIAN_POINT('Ctrl Pts',(1.14215574734217,-7.8281305244904,50.8985124250607));
#221193=CARTESIAN_POINT('Ctrl Pts',(1.16451267898166,-7.8248251318643,50.8994228105157));
#221194=CARTESIAN_POINT('Ctrl Pts',(1.17198782723061,-7.82370900890905,
50.8997276762696));
#221195=CARTESIAN_POINT('Ctrl Pts',(1.1852844575232,-7.821704189895,50.900270822695));
#221196=CARTESIAN_POINT('Ctrl Pts',(1.19110657470778,-7.82081970172647,
50.9005089398191));
#221197=CARTESIAN_POINT('Ctrl Pts',(1.20334533267836,-7.81894642272051,
50.9010101131069));
#221198=CARTESIAN_POINT('Ctrl Pts',(1.20976175251835,-7.81795623247324,
50.9012732241577));
#221199=CARTESIAN_POINT('Ctrl Pts',(1.22662957610809,-7.81533190500662,
50.9019658664896));
#221200=CARTESIAN_POINT('Ctrl Pts',(1.23707891235629,-7.81368470476932,
50.9023959184921));
#221201=CARTESIAN_POINT('Ctrl Pts',(1.28356969169995,-7.80626044965329,
50.9043137141617));
#221202=CARTESIAN_POINT('Ctrl Pts',(1.31957380868606,-7.80025501258658,
50.9058107651023));
#221203=CARTESIAN_POINT('Ctrl Pts',(1.57048580536669,-7.75661633244477,
50.9163328450662));
#221204=CARTESIAN_POINT('Ctrl Pts',(1.78376257117131,-7.71036227864182,
50.9257815686554));
#221205=CARTESIAN_POINT('Ctrl Pts',(2.42664186170662,-7.54284117060676,
50.9553694721891));
#221206=CARTESIAN_POINT('Ctrl Pts',(2.84815251033658,-7.3939885097737,50.9762124233281));
#221207=CARTESIAN_POINT('Ctrl Pts',(3.59400176165992,-7.05730305501481,
51.0136176912277));
#221208=CARTESIAN_POINT('Ctrl Pts',(3.92194185326242,-6.88046428132935,
51.0302762608795));
#221209=CARTESIAN_POINT('Ctrl Pts',(4.39363317978894,-6.58138594154004,
51.0541081547688));
#221210=CARTESIAN_POINT('Ctrl Pts',(4.547458196659,-6.47605464462263,51.0618636365923));
#221211=CARTESIAN_POINT('Ctrl Pts',(4.71266346588171,-6.35413901633539,
51.0701733093627));
#221212=CARTESIAN_POINT('Ctrl Pts',(4.72785968284902,-6.34284024767907,
51.0709374985991));
#221213=CARTESIAN_POINT('Ctrl Pts',(4.75041597862298,-6.32594297608029,
51.072071584344));
#221214=CARTESIAN_POINT('Ctrl Pts',(4.7578069907328,-6.32038599661947,51.0724431531572));
#221215=CARTESIAN_POINT('Ctrl Pts',(4.77046670412028,-6.31083292063964,
51.0730795360119));
#221216=CARTESIAN_POINT('Ctrl Pts',(4.77574016153975,-6.30684315938723,
51.0733446061722));
#221217=CARTESIAN_POINT('Ctrl Pts',(4.78600890076762,-6.29905383300283,
51.0738607306304));
#221218=CARTESIAN_POINT('Ctrl Pts',(4.79100467568514,-6.29525492630163,
51.0741118114144));
#221219=CARTESIAN_POINT('Ctrl Pts',(4.80297275199537,-6.28613161694719,
51.0747132749856));
#221220=CARTESIAN_POINT('Ctrl Pts',(4.80994073462674,-6.28080154853001,
51.0750634265904));
#221221=CARTESIAN_POINT('Ctrl Pts',(4.83091374697876,-6.26470314269561,
51.0761172702566));
#221222=CARTESIAN_POINT('Ctrl Pts',(4.84489163058013,-6.25389943876369,
51.0768195151905));
#221223=CARTESIAN_POINT('Ctrl Pts',(4.97133355543121,-6.15549235669783,
51.0831710719581));
#221224=CARTESIAN_POINT('Ctrl Pts',(5.08144987315789,-6.06490835568331,
51.0886957186609));
#221225=CARTESIAN_POINT('Ctrl Pts',(5.35892877845868,-5.82378290359019,
51.1026344550917));
#221226=CARTESIAN_POINT('Ctrl Pts',(5.52242547354013,-5.66898495797105,
51.1108620717518));
#221227=CARTESIAN_POINT('Ctrl Pts',(5.99339894599743,-5.18332940834571,
51.1348995119455));
#221228=CARTESIAN_POINT('Ctrl Pts',(6.2793790958365,-4.8329230006552,51.1499216900156));
#221229=CARTESIAN_POINT('Ctrl Pts',(6.82363446786695,-4.03559532756613,
51.1824267232602));
#221230=CARTESIAN_POINT('Ctrl Pts',(7.07128122062639,-3.58397456001204,
51.1999062801039));
#221231=CARTESIAN_POINT('Ctrl Pts',(7.28663647422192,-3.08058248197096,
51.2215118530094));
#221232=CARTESIAN_POINT('Ctrl Pts',(7.29970936240751,-3.04947580635208,
51.2228553307206));
#221233=CARTESIAN_POINT('Ctrl Pts',(7.31535572090004,-3.01156844589331,
51.2245037334189));
#221234=CARTESIAN_POINT('Ctrl Pts',(7.31811951398557,-3.00484618673897,
51.2247964778157));
#221235=CARTESIAN_POINT('Ctrl Pts',(7.32264532027286,-2.99379497596358,
51.2252784565775));
#221236=CARTESIAN_POINT('Ctrl Pts',(7.3244127728528,-2.98946824322873,51.2254673391091));
#221237=CARTESIAN_POINT('Ctrl Pts',(7.32758071117033,-2.98169344029259,
51.2258070733931));
#221238=CARTESIAN_POINT('Ctrl Pts',(7.32898260139996,-2.97824593995863,
51.2259578336435));
#221239=CARTESIAN_POINT('Ctrl Pts',(7.3319561285575,-2.97091868812755,51.2262785041984));
#221240=CARTESIAN_POINT('Ctrl Pts',(7.3335271192361,-2.96703867751138,51.226448456726));
#221241=CARTESIAN_POINT('Ctrl Pts',(7.33775565707316,-2.95657121920158,
51.2269073549054));
#221242=CARTESIAN_POINT('Ctrl Pts',(7.34040740631352,-2.94998145176252,
51.2271966822495));
#221243=CARTESIAN_POINT('Ctrl Pts',(7.35355119609214,-2.91719083622515,
51.2286384670204));
#221244=CARTESIAN_POINT('Ctrl Pts',(7.36391172199688,-2.89093785441998,
51.2297994417603));
#221245=CARTESIAN_POINT('Ctrl Pts',(7.45109231496194,-2.66651757213358,
51.2397764882567));
#221246=CARTESIAN_POINT('Ctrl Pts',(7.52003283004686,-2.46539761670041,
51.2490649921619));
#221247=CARTESIAN_POINT('Ctrl Pts',(7.7453106022586,-1.71033048793827,51.2845060583133));
#221248=CARTESIAN_POINT('Ctrl Pts',(7.84917815459769,-1.1425921410738,51.3121148467833));
#221249=CARTESIAN_POINT('Ctrl Pts',(7.92376928653246,-0.107455863215498,
51.3595018041555));
#221250=CARTESIAN_POINT('Ctrl Pts',(7.91651540116999,0.355741900989444,
51.3796904883554));
#221251=CARTESIAN_POINT('Ctrl Pts',(7.86557507855181,0.84714107187943,51.3997467850635));
#221252=CARTESIAN_POINT('Ctrl Pts',(7.86212888889296,0.87854919009609,51.4010231026232));
#221253=CARTESIAN_POINT('Ctrl Pts',(7.85720545556633,0.921069511043594,
51.4027435211936));
#221254=CARTESIAN_POINT('Ctrl Pts',(7.85589265232685,0.932200220829996,
51.4031931886683));
#221255=CARTESIAN_POINT('Ctrl Pts',(7.8537869074029,0.949733559674308,51.4039004297629));
#221256=CARTESIAN_POINT('Ctrl Pts',(7.85300978283221,0.956138050846054,
51.404158539072));
#221257=CARTESIAN_POINT('Ctrl Pts',(7.85149744012159,0.968475444926297,
51.4046553141591));
#221258=CARTESIAN_POINT('Ctrl Pts',(7.85076332967054,0.974408477683425,
51.4048940172912));
#221259=CARTESIAN_POINT('Ctrl Pts',(7.84901469924289,0.988410536810985,
51.4054569018433));
#221260=CARTESIAN_POINT('Ctrl Pts',(7.84799445978118,0.996478849751861,
51.4057808891804));
#221261=CARTESIAN_POINT('Ctrl Pts',(7.84498150058779,1.02001444218521,51.4067249291445));
#221262=CARTESIAN_POINT('Ctrl Pts',(7.84295547827992,1.03547746299875,51.4073438526169));
#221263=CARTESIAN_POINT('Ctrl Pts',(7.83829573786301,1.0702431734016,51.4087324598477));
#221264=CARTESIAN_POINT('Ctrl Pts',(7.83563641174783,1.08954236021146,51.4095012740764));
#221265=CARTESIAN_POINT('Ctrl Pts',(7.81260586231883,1.25223263785313,51.4159654449639));
#221266=CARTESIAN_POINT('Ctrl Pts',(7.78837121374084,1.39505326231059,51.4215288095821));
#221267=CARTESIAN_POINT('Ctrl Pts',(7.70536079225613,1.81413195357768,51.4375805343184));
#221268=CARTESIAN_POINT('Ctrl Pts',(7.63569988046149,2.0880041636256,51.4477088983109));
#221269=CARTESIAN_POINT('Ctrl Pts',(7.46312542582521,2.64077602578509,51.4679071480701));
#221270=CARTESIAN_POINT('Ctrl Pts',(7.35884965397134,2.91877954939865,51.4779319646777));
#221271=CARTESIAN_POINT('Ctrl Pts',(7.03822376863279,3.64632842248934,51.5049712475368));
#221272=CARTESIAN_POINT('Ctrl Pts',(6.79461702771615,4.08232351738125,51.5220151060109));
#221273=CARTESIAN_POINT('Ctrl Pts',(6.49385402679533,4.51827011516617,51.5429450989516));
#221274=CARTESIAN_POINT('Ctrl Pts',(6.4758877379527,4.54398315484607,51.5441951960781));
#221275=CARTESIAN_POINT('Ctrl Pts',(6.4532314067712,4.57600121584495,51.5457723623038));
#221276=CARTESIAN_POINT('Ctrl Pts',(6.44868405341011,4.58240730349968,51.5460889512797));
#221277=CARTESIAN_POINT('Ctrl Pts',(6.44148417213284,4.59251820048186,51.5465902532252));
#221278=CARTESIAN_POINT('Ctrl Pts',(6.438837961864,4.59622752507792,51.546774508435));
#221279=CARTESIAN_POINT('Ctrl Pts',(6.43414840242404,4.60278911599557,51.5471010547285));
#221280=CARTESIAN_POINT('Ctrl Pts',(6.43210635535538,4.60564231612314,51.547243252158));
#221281=CARTESIAN_POINT('Ctrl Pts',(6.42741406828286,4.6121892917171,51.5475700065591));
#221282=CARTESIAN_POINT('Ctrl Pts',(6.42476254324614,4.61588214001647,51.547754655433));
#221283=CARTESIAN_POINT('Ctrl Pts',(6.41742310120222,4.62608539720852,51.5482657767697));
#221284=CARTESIAN_POINT('Ctrl Pts',(6.41272847291706,4.63259094825321,51.5485927256276));
#221285=CARTESIAN_POINT('Ctrl Pts',(6.38729957637856,4.66771615651435,51.5503636961705));
#221286=CARTESIAN_POINT('Ctrl Pts',(6.36638389438506,4.69620336336403,51.5518204239993));
#221287=CARTESIAN_POINT('Ctrl Pts',(6.04847316960574,5.12317153045162,51.573951318478));
#221288=CARTESIAN_POINT('Ctrl Pts',(5.71479022107682,5.49290431171215,51.5969875042569));
#221289=CARTESIAN_POINT('Ctrl Pts',(5.15457249096666,6.00697129978001,51.632450132198));
#221290=CARTESIAN_POINT('Ctrl Pts',(4.95168881088706,6.17528177636811,51.6447655609537));
#221291=CARTESIAN_POINT('Ctrl Pts',(4.31431316721881,6.65239915056125,51.6813685007465));
#221292=CARTESIAN_POINT('Ctrl Pts',(3.85664452218045,6.92778102496164,51.7048305115745));
#221293=CARTESIAN_POINT('Ctrl Pts',(3.34335201789069,7.16987586097758,51.7279440336819));
#221294=CARTESIAN_POINT('Ctrl Pts',(3.31190332904333,7.18445676139648,51.7293486614492));
#221295=CARTESIAN_POINT('Ctrl Pts',(3.26921581274263,7.20390858760205,51.7312399236168));
#221296=CARTESIAN_POINT('Ctrl Pts',(3.25806026271668,7.20896069451518,51.731732758106));
#221297=CARTESIAN_POINT('Ctrl Pts',(3.24047625381636,7.21687495831333,51.7325073845961));
#221298=CARTESIAN_POINT('Ctrl Pts',(3.2340556527941,7.2197544660765,51.7327897683564));
#221299=CARTESIAN_POINT('Ctrl Pts',(3.22168486445983,7.22528269718834,51.7333329596235));
#221300=CARTESIAN_POINT('Ctrl Pts',(3.21573523279332,7.22793264585477,51.733593808706));
#221301=CARTESIAN_POINT('Ctrl Pts',(3.20169452538161,7.23416556826426,51.7342084668592));
#221302=CARTESIAN_POINT('Ctrl Pts',(3.19360068950142,7.23774232337614,51.734562064444));
#221303=CARTESIAN_POINT('Ctrl Pts',(3.17000216809267,7.2481234777252,51.7355909166724));
#221304=CARTESIAN_POINT('Ctrl Pts',(3.1544815743588,7.25489170805623,51.7362649454632));
#221305=CARTESIAN_POINT('Ctrl Pts',(3.04365887101114,7.30279647515724,51.7410591091237));
#221306=CARTESIAN_POINT('Ctrl Pts',(2.94757504752495,7.34210446787291,51.7451173363025));
#221307=CARTESIAN_POINT('Ctrl Pts',(2.64085365278465,7.46059252142293,51.7577832761653));
#221308=CARTESIAN_POINT('Ctrl Pts',(2.42759347594129,7.5326852359243,51.7661614800352));
#221309=CARTESIAN_POINT('Ctrl Pts',(1.81932403050469,7.70978964033411,51.7891548467233));
#221310=CARTESIAN_POINT('Ctrl Pts',(1.41884239132787,7.7934391603952,51.8032253428223));
#221311=CARTESIAN_POINT('Ctrl Pts',(0.504071196503408,7.91162956739007,
51.8352107630675));
#221312=CARTESIAN_POINT('Ctrl Pts',(-0.0107690511506302,7.92766572568367,
51.8531772405592));
#221313=CARTESIAN_POINT('Ctrl Pts',(-0.559038632226526,7.89130301784501,
51.8749293513342));
#221314=CARTESIAN_POINT('Ctrl Pts',(-0.594532066426574,7.88870832799293,
51.876347317049));
#221315=CARTESIAN_POINT('Ctrl Pts',(-0.641855534574459,7.88492763252809,
51.8782500900988));
#221316=CARTESIAN_POINT('Ctrl Pts',(-0.653702457337308,7.88395429927047,
51.8787274496849));
#221317=CARTESIAN_POINT('Ctrl Pts',(-0.672183163184198,7.88239399841931,
51.8794736663263));
#221318=CARTESIAN_POINT('Ctrl Pts',(-0.678818500791426,7.88182534657297,
51.8797419019709));
#221319=CARTESIAN_POINT('Ctrl Pts',(-0.692102931663866,7.88066996433184,
51.8802795477937));
#221320=CARTESIAN_POINT('Ctrl Pts',(-0.698752015983833,7.88008319591775,
51.8805489590296));
#221321=CARTESIAN_POINT('Ctrl Pts',(-0.713738016078834,7.87874159485013,
51.8811568601622));
#221322=CARTESIAN_POINT('Ctrl Pts',(-0.722074487042778,7.87798194391178,
51.8814955074101));
#221323=CARTESIAN_POINT('Ctrl Pts',(-0.746670719876964,7.87570127224605,
51.8824960620968));
#221324=CARTESIAN_POINT('Ctrl Pts',(-0.762926949777184,7.87414313806338,
51.8831591546484));
#221325=CARTESIAN_POINT('Ctrl Pts',(-0.890657268889658,7.86150112621064,
51.8883829814816));
#221326=CARTESIAN_POINT('Ctrl Pts',(-1.00188710518627,7.84810113607214,
51.8930138278287));
#221327=CARTESIAN_POINT('Ctrl Pts',(-1.4173907905058,7.78906782060753,51.9105526401867));
#221328=CARTESIAN_POINT('Ctrl Pts',(-1.71919973981018,7.72806047636063,
51.923764983382));
#221329=CARTESIAN_POINT('Ctrl Pts',(-2.15833879410559,7.61228982175401,
51.9433029058731));
#221330=CARTESIAN_POINT('Ctrl Pts',(-2.29893252332808,7.57101658615155,
51.9496094193611));
#221331=CARTESIAN_POINT('Ctrl Pts',(-3.1397074359222,7.29861450688728,51.9875468585231));
#221332=CARTESIAN_POINT('Ctrl Pts',(-3.80593010888782,6.9744177836307,52.0182039409521));
#221333=CARTESIAN_POINT('Ctrl Pts',(-4.51715674106673,6.49566132404436,
52.0532203229488));
#221334=CARTESIAN_POINT('Ctrl Pts',(-4.61516770633612,6.4263946810876,52.0580986816982));
#221335=CARTESIAN_POINT('Ctrl Pts',(-4.74069260370534,6.33333003531172,
52.0644152510801));
#221336=CARTESIAN_POINT('Ctrl Pts',(-4.76967063906559,6.31153528937594,
52.0658783857615));
#221337=CARTESIAN_POINT('Ctrl Pts',(-4.81610291973277,6.27611057959156,
52.0682308341278));
#221338=CARTESIAN_POINT('Ctrl Pts',(-4.83365150353797,6.26260524754771,
52.0691217861421));
#221339=CARTESIAN_POINT('Ctrl Pts',(-4.86644478718618,6.2371476955178,52.0707902615155));
#221340=CARTESIAN_POINT('Ctrl Pts',(-4.88170273341824,6.22521282105096,
52.0715680141047));
#221341=CARTESIAN_POINT('Ctrl Pts',(-4.91658743398862,6.19771863637366,
52.0733495740153));
#221342=CARTESIAN_POINT('Ctrl Pts',(-4.93618445945907,6.18212190749689,
52.0743528502155));
#221343=CARTESIAN_POINT('Ctrl Pts',(-4.99500979439336,6.13484641409477,
52.0773719565386));
#221344=CARTESIAN_POINT('Ctrl Pts',(-5.03400974699968,6.10288532424101,
52.0793837118689));
#221345=CARTESIAN_POINT('Ctrl Pts',(-5.12244505268295,6.02898663855011,
52.0839696579611));
#221346=CARTESIAN_POINT('Ctrl Pts',(-5.17167592738975,5.98680978468854,
52.0865401855486));
#221347=CARTESIAN_POINT('Ctrl Pts',(-5.33316153641293,5.84498405226461,
52.0950340762327));
#221348=CARTESIAN_POINT('Ctrl Pts',(-5.44309929502286,5.74274512833629,
52.1009175962134));
#221349=CARTESIAN_POINT('Ctrl Pts',(-5.74076968088533,5.44968842352764,
52.1171866084284));
#221350=CARTESIAN_POINT('Ctrl Pts',(-5.92182762584419,5.25238045739707,
52.1274752605463));
#221351=CARTESIAN_POINT('Ctrl Pts',(-6.33807021666432,4.74983664057066,
52.1525459708026));
#221352=CARTESIAN_POINT('Ctrl Pts',(-6.56163101543227,4.43588335381606,
52.167277404458));
#221353=CARTESIAN_POINT('Ctrl Pts',(-6.783098461993,4.07126960118406,52.1842540684907));
#221354=CARTESIAN_POINT('Ctrl Pts',(-6.80447051966529,4.03544815461553,
52.1859208580246));
#221355=CARTESIAN_POINT('Ctrl Pts',(-6.83250411751814,3.98760545342949,
52.188147086145));
#221356=CARTESIAN_POINT('Ctrl Pts',(-6.8394191790698,3.97573327299858,52.1886995413469));
#221357=CARTESIAN_POINT('Ctrl Pts',(-6.8511815742741,3.95541740248493,52.1896449113731));
#221358=CARTESIAN_POINT('Ctrl Pts',(-6.85604432307434,3.94698264892919,
52.1900374091311));
#221359=CARTESIAN_POINT('Ctrl Pts',(-6.86546461324758,3.93057260720118,
52.1908010041881));
#221360=CARTESIAN_POINT('Ctrl Pts',(-6.87002386076315,3.92259831339526,
52.1911720563455));
#221361=CARTESIAN_POINT('Ctrl Pts',(-6.87944923989044,3.90604613579889,
52.191942212168));
#221362=CARTESIAN_POINT('Ctrl Pts',(-6.8843132401745,3.89746705819821,52.1923413688658));
#221363=CARTESIAN_POINT('Ctrl Pts',(-6.89533705725171,3.87793833175498,
52.1932499136883));
#221364=CARTESIAN_POINT('Ctrl Pts',(-6.90148685382313,3.86698306735794,
52.1937595456643));
#221365=CARTESIAN_POINT('Ctrl Pts',(-6.91710291469134,3.8390086647724,52.1950607347738));
#221366=CARTESIAN_POINT('Ctrl Pts',(-6.92653246322216,3.82196916419084,
52.1958531497359));
#221367=CARTESIAN_POINT('Ctrl Pts',(-7.01557173815238,3.6596605055552,52.2033991550164));
#221368=CARTESIAN_POINT('Ctrl Pts',(-7.09066176988678,3.51196177598958,
52.2102493619808));
#221369=CARTESIAN_POINT('Ctrl Pts',(-7.38279973148594,2.88971137013535,
52.2388873792428));
#221370=CARTESIAN_POINT('Ctrl Pts',(-7.55727388721529,2.39662130011934,
52.2609806885891));
#221371=CARTESIAN_POINT('Ctrl Pts',(-7.71816766020533,1.7426469761399,52.2888577329158));
#221372=CARTESIAN_POINT('Ctrl Pts',(-7.75016264639936,1.59433702197289,
52.2950957528323));
#221373=CARTESIAN_POINT('Ctrl Pts',(-7.79607812790603,1.34722554614238,
52.3053578060762));
#221374=CARTESIAN_POINT('Ctrl Pts',(-7.81242954179104,1.2489178596798,52.309406401178));
#221375=CARTESIAN_POINT('Ctrl Pts',(-7.83244073755938,1.11276000862184,
52.3149711377105));
#221376=CARTESIAN_POINT('Ctrl Pts',(-7.83769142509056,1.07515388962323,
52.3165036351529));
#221377=CARTESIAN_POINT('Ctrl Pts',(-7.84567886659451,1.01477587126273,
52.3189573249605));
#221378=CARTESIAN_POINT('Ctrl Pts',(-7.848587679112,0.992027415754827,52.3198802521722));
#221379=CARTESIAN_POINT('Ctrl Pts',(-7.85424943783336,0.946165195015163,
52.3217379273752));
#221380=CARTESIAN_POINT('Ctrl Pts',(-7.85699937265996,0.923051282302919,
52.3226726364649));
#221381=CARTESIAN_POINT('Ctrl Pts',(-7.86238184616331,0.876042566886318,
52.3245706389048));
#221382=CARTESIAN_POINT('Ctrl Pts',(-7.86500756444916,0.852147222655544,
52.3255338561054));
#221383=CARTESIAN_POINT('Ctrl Pts',(-7.87083848874207,0.796758777953407,
52.3277630797707));
#221384=CARTESIAN_POINT('Ctrl Pts',(-7.87396366651727,0.765257638552243,
52.3290283088682));
#221385=CARTESIAN_POINT('Ctrl Pts',(-7.88514882816963,0.6451816253484,52.3338418596193));
#221386=CARTESIAN_POINT('Ctrl Pts',(-7.89190400436654,0.556491449336632,
52.3373780185071));
#221387=CARTESIAN_POINT('Ctrl Pts',(-7.90634940986654,0.312582307885866,
52.3470621327352));
#221388=CARTESIAN_POINT('Ctrl Pts',(-7.9109639325235,0.15722082092995,52.3531904209946));
#221389=CARTESIAN_POINT('Ctrl Pts',(-7.91099978939441,0.00182543188703851,
52.3592866701075));
#221390=CARTESIAN_POINT('',(-7.91934491493686,0.00236459517639777,56.3576684917633));
#221391=CARTESIAN_POINT('Ctrl Pts',(-7.9109997887806,0.00182809008343179,
52.3592865658249));
#221392=CARTESIAN_POINT('Ctrl Pts',(-7.91119646617743,-0.849286884464968,
52.3926762906361));
#221393=CARTESIAN_POINT('Ctrl Pts',(-7.7740466783572,-1.69487562970979,
52.423722529026));
#221394=CARTESIAN_POINT('Ctrl Pts',(-7.44295841195928,-2.6878487431774,
52.4630109752596));
#221395=CARTESIAN_POINT('Ctrl Pts',(-7.37424828576619,-2.87099608398839,
52.4704332882737));
#221396=CARTESIAN_POINT('Ctrl Pts',(-7.26632607255126,-3.12914139336323,
52.4813427238853));
#221397=CARTESIAN_POINT('Ctrl Pts',(-7.23258701250455,-3.20635384665817,
52.4846650845882));
#221398=CARTESIAN_POINT('Ctrl Pts',(-7.19177196686032,-3.29583611258907,
52.4885992268777));
#221399=CARTESIAN_POINT('Ctrl Pts',(-7.18588787205115,-3.30864552220287,
52.4891644266056));
#221400=CARTESIAN_POINT('Ctrl Pts',(-7.17685456187478,-3.32817286885108,
52.4900292331509));
#221401=CARTESIAN_POINT('Ctrl Pts',(-7.1737300632019,-3.33490225150739,
52.4903278359422));
#221402=CARTESIAN_POINT('Ctrl Pts',(-7.16803267913505,-3.34712792403135,
52.4908713944099));
#221403=CARTESIAN_POINT('Ctrl Pts',(-7.1654629249818,-3.35262567242916,
52.4911162202184));
#221404=CARTESIAN_POINT('Ctrl Pts',(-7.15991313359746,-3.3644634037863,
52.4916442369079));
#221405=CARTESIAN_POINT('Ctrl Pts',(-7.15693099750073,-3.37080239300474,
52.49192751608));
#221406=CARTESIAN_POINT('Ctrl Pts',(-7.14887160078172,-3.38787497175459,
52.4926919146789));
#221407=CARTESIAN_POINT('Ctrl Pts',(-7.14377860001328,-3.39860107995461,
52.493173709312));
#221408=CARTESIAN_POINT('Ctrl Pts',(-7.1201924955951,-3.44798730080933,
52.4953993509368));
#221409=CARTESIAN_POINT('Ctrl Pts',(-7.10140982208081,-3.48650771356148,
52.4971560054075));
#221410=CARTESIAN_POINT('Ctrl Pts',(-6.83843456813954,-4.01488806981178,
52.521561416813));
#221411=CARTESIAN_POINT('Ctrl Pts',(-6.54439384039041,-4.4781963339638,
52.5468120377884));
#221412=CARTESIAN_POINT('Ctrl Pts',(-6.11888112045396,-5.01622080723766,
52.5784190523372));
#221413=CARTESIAN_POINT('Ctrl Pts',(-6.029951030074,-5.12277936971555,52.5848094843894));
#221414=CARTESIAN_POINT('Ctrl Pts',(-5.91001079051183,-5.25904192237671,
52.5931219020823));
#221415=CARTESIAN_POINT('Ctrl Pts',(-5.88149804853277,-5.29091015055192,
52.5950764406383));
#221416=CARTESIAN_POINT('Ctrl Pts',(-5.81272016056783,-5.36653905115986,
52.5997386153237));
#221417=CARTESIAN_POINT('Ctrl Pts',(-5.77221707065414,-5.41008015153635,
52.6024420373466));
#221418=CARTESIAN_POINT('Ctrl Pts',(-5.38751487540486,-5.81439895944724,
52.6277144984721));
#221419=CARTESIAN_POINT('Ctrl Pts',(-5.01038963351085,-6.14236584293915,
52.6493971512202));
#221420=CARTESIAN_POINT('Ctrl Pts',(-4.5864839144347,-6.44582007393821,
52.6705380287873));
#221421=CARTESIAN_POINT('Ctrl Pts',(-4.56806232492975,-6.45888827346036,
52.6714510474623));
#221422=CARTESIAN_POINT('Ctrl Pts',(-4.54125490759907,-6.47773328750249,
52.6727714948196));
#221423=CARTESIAN_POINT('Ctrl Pts',(-4.53291357146582,-6.48357302992665,
52.673181218036));
#221424=CARTESIAN_POINT('Ctrl Pts',(-4.51832015166986,-6.49374790764697,
52.6738960503734));
#221425=CARTESIAN_POINT('Ctrl Pts',(-4.51207305480041,-6.49809015246708,
52.6742014178902));
#221426=CARTESIAN_POINT('Ctrl Pts',(-4.49997928226364,-6.50647046780809,
52.6747913551646));
#221427=CARTESIAN_POINT('Ctrl Pts',(-4.49413341296765,-6.51050968481054,
52.6750759663727));
#221428=CARTESIAN_POINT('Ctrl Pts',(-4.48024109875156,-6.52008098461047,
52.6757510197887));
#221429=CARTESIAN_POINT('Ctrl Pts',(-4.47218982891529,-6.52560606256914,
52.6761412081885));
#221430=CARTESIAN_POINT('Ctrl Pts',(-4.44376467379382,-6.54503513653207,
52.6775151324094));
#221431=CARTESIAN_POINT('Ctrl Pts',(-4.42333591904498,-6.55885880128651,
52.6784959674633));
#221432=CARTESIAN_POINT('Ctrl Pts',(-4.15522084767664,-6.73846365612211,
52.6912837185592));
#221433=CARTESIAN_POINT('Ctrl Pts',(-3.89841284420971,-6.89022133476271,
52.7025731614423));
#221434=CARTESIAN_POINT('Ctrl Pts',(-3.30337905130952,-7.19790528298636,
52.7270625360408));
#221435=CARTESIAN_POINT('Ctrl Pts',(-2.96148521637809,-7.34518715173454,
52.7400060225158));
#221436=CARTESIAN_POINT('Ctrl Pts',(-2.42815231856111,-7.53162060067291,
52.7595337157709));
#221437=CARTESIAN_POINT('Ctrl Pts',(-2.2435377630356,-7.58866061725906,
52.7661838452677));
#221438=CARTESIAN_POINT('Ctrl Pts',(-1.86262541601725,-7.69123383801406,
52.7799311814493));
#221439=CARTESIAN_POINT('Ctrl Pts',(-1.66630635933668,-7.73614051193638,
52.7870306085686));
#221440=CARTESIAN_POINT('Ctrl Pts',(-1.2531059643277,-7.81419825148433,
52.8023220801888));
#221441=CARTESIAN_POINT('Ctrl Pts',(-1.03613198034881,-7.84591535733134,
52.8105490664315));
#221442=CARTESIAN_POINT('Ctrl Pts',(-0.785689960523596,-7.8719550539589,
52.8205096169565));
#221443=CARTESIAN_POINT('Ctrl Pts',(-0.75322464998402,-7.87512778504,52.8218098358847));
#221444=CARTESIAN_POINT('Ctrl Pts',(-0.711457395074118,-7.87894893282157,
52.8234933859347));
#221445=CARTESIAN_POINT('Ctrl Pts',(-0.702172093536987,-7.87978186633176,
52.8238683415471));
#221446=CARTESIAN_POINT('Ctrl Pts',(-0.687214092755923,-7.88109701772237,
52.8244734489482));
#221447=CARTESIAN_POINT('Ctrl Pts',(-0.681542288638739,-7.88158953007479,
52.8247031445438));
#221448=CARTESIAN_POINT('Ctrl Pts',(-0.670743673371047,-7.88251548661697,
52.8251409338568));
#221449=CARTESIAN_POINT('Ctrl Pts',(-0.665616959167033,-7.88295005284269,
52.8253489784883));
#221450=CARTESIAN_POINT('Ctrl Pts',(-0.653935908396738,-7.8839287213393,
52.825823454277));
#221451=CARTESIAN_POINT('Ctrl Pts',(-0.647381315194075,-7.88446965165159,
52.8260900218814));
#221452=CARTESIAN_POINT('Ctrl Pts',(-0.627866225437084,-7.88605567250676,
52.8268846293151));
#221453=CARTESIAN_POINT('Ctrl Pts',(-0.614903858146825,-7.88707698132475,
52.827413674992));
#221454=CARTESIAN_POINT('Ctrl Pts',(-0.524487526524967,-7.89397666013232,
52.8311123630761));
#221455=CARTESIAN_POINT('Ctrl Pts',(-0.446954764783016,-7.89874582316162,
52.8343271527586));
#221456=CARTESIAN_POINT('Ctrl Pts',(-0.341818402105852,-7.90366002039431,
52.8387339909716));
#221457=CARTESIAN_POINT('Ctrl Pts',(-0.31426426536002,-7.90480357054582,
52.8398933559037));
#221458=CARTESIAN_POINT('Ctrl Pts',(-0.253604906586833,-7.90700338954029,
52.8424546257411));
#221459=CARTESIAN_POINT('Ctrl Pts',(-0.220497938893828,-7.90799586980192,
52.8438584074659));
#221460=CARTESIAN_POINT('Ctrl Pts',(-0.185011916436274,-7.90883665465911,
52.8453687456014));
#221461=CARTESIAN_POINT('Ctrl Pts',(-0.182637837061959,-7.90889183512866,
52.8454698172215));
#221462=CARTESIAN_POINT('Ctrl Pts',(0.425420965005026,-7.92275094494516,
52.8713636159861));
#221463=CARTESIAN_POINT('Ctrl Pts',(1.03069311791269,-7.8669367083047,52.8986734608375));
#221464=CARTESIAN_POINT('Ctrl Pts',(1.88356150178577,-7.68808326487359,
52.9362743536675));
#221465=CARTESIAN_POINT('Ctrl Pts',(2.14053999471102,-7.62053328988184,
52.9475197554204));
#221466=CARTESIAN_POINT('Ctrl Pts',(2.47924432325361,-7.51301099576739,
52.9622222051086));
#221467=CARTESIAN_POINT('Ctrl Pts',(2.56437567350824,-7.48438136862762,
52.9659081796846));
#221468=CARTESIAN_POINT('Ctrl Pts',(2.70594550314423,-7.43407236636109,
52.9720265941409));
#221469=CARTESIAN_POINT('Ctrl Pts',(2.76265546285147,-7.41318473615827,
52.97447448468));
#221470=CARTESIAN_POINT('Ctrl Pts',(2.83837856524004,-7.38430449791696,
52.9777406354176));
#221471=CARTESIAN_POINT('Ctrl Pts',(2.85760738896977,-7.37688456008501,
52.9785698184246));
#221472=CARTESIAN_POINT('Ctrl Pts',(2.88932765143184,-7.36450184178956,
52.979937400091));
#221473=CARTESIAN_POINT('Ctrl Pts',(2.90183579801819,-7.35958223390965,
52.9804766082397));
#221474=CARTESIAN_POINT('Ctrl Pts',(2.9143346659203,-7.3546294573573,52.9810153669147));
#221475=CARTESIAN_POINT('Ctrl Pts',(2.91433796399321,-7.35462815046692,
52.9810155090768));
#221476=CARTESIAN_POINT('Ctrl Pts',(2.91434456184307,-7.35462553600578,
52.9810157934745));
#221477=CARTESIAN_POINT('Ctrl Pts',(2.91434785918889,-7.35462422939838,
52.9810159356052));
#221478=CARTESIAN_POINT('Ctrl Pts',(2.91435445255371,-7.35462161670421,
52.9810162198095));
#221479=CARTESIAN_POINT('Ctrl Pts',(2.91435775226989,-7.3546203091524,52.9810163620425));
#221480=CARTESIAN_POINT('Ctrl Pts',(2.91436434982926,-7.35461769478583,
52.9810166464276));
#221481=CARTESIAN_POINT('Ctrl Pts',(2.91436764912413,-7.35461638739583,
52.9810167886423));
#221482=CARTESIAN_POINT('Ctrl Pts',(2.91437425057796,-7.35461377147575,
52.9810170731953));
#221483=CARTESIAN_POINT('Ctrl Pts',(2.91437754820863,-7.35461246474007,
52.9810172153383));
#221484=CARTESIAN_POINT('Ctrl Pts',(2.91438414645053,-7.35460985008249,
52.9810174997528));
#221485=CARTESIAN_POINT('Ctrl Pts',(2.91438744534538,-7.35460854284073,
52.9810176419503));
#221486=CARTESIAN_POINT('Ctrl Pts',(2.9143940417932,-7.35460592888381,52.9810179262874));
#221487=CARTESIAN_POINT('Ctrl Pts',(2.9143973427108,-7.35460462083536,52.9810180685721));
#221488=CARTESIAN_POINT('Ctrl Pts',(2.91440394373701,-7.35460200505389,
52.9810183531066));
#221489=CARTESIAN_POINT('Ctrl Pts',(2.91440724386871,-7.35460069731173,
52.9810184953574));
#221490=CARTESIAN_POINT('Ctrl Pts',(2.91441384477225,-7.35459808156859,
52.9810187798866));
#221491=CARTESIAN_POINT('Ctrl Pts',(2.9144171450662,-7.35459677375699,52.9810189221444));
#221492=CARTESIAN_POINT('Ctrl Pts',(2.91442374758804,-7.35459415736229,
52.9810192067433));
#221493=CARTESIAN_POINT('Ctrl Pts',(2.91442704764742,-7.3545928496385,52.981019348991));
#221494=CARTESIAN_POINT('Ctrl Pts',(2.91443364709967,-7.3545902344499,52.9810196334576));
#221495=CARTESIAN_POINT('Ctrl Pts',(2.91443694906994,-7.35458892596374,
52.9810197757876));
#221496=CARTESIAN_POINT('Ctrl Pts',(2.91444355359865,-7.35458630875319,
52.981020060473));
#221497=CARTESIAN_POINT('Ctrl Pts',(2.9144468544801,-7.35458500069335,52.9810202027561));
#221498=CARTESIAN_POINT('Ctrl Pts',(2.91445345652773,-7.35458238445571,
52.9810204873345));
#221499=CARTESIAN_POINT('Ctrl Pts',(2.9144567585994,-7.35458107591907,52.9810206296689));
#221500=CARTESIAN_POINT('Ctrl Pts',(2.9144633624289,-7.35457845896502,52.9810209143241));
#221501=CARTESIAN_POINT('Ctrl Pts',(2.91446666469943,-7.35457715034443,
52.9810210566671));
#221502=CARTESIAN_POINT('Ctrl Pts',(2.91447326748367,-7.3545745337943,52.9810213412773));
#221503=CARTESIAN_POINT('Ctrl Pts',(2.91447657087126,-7.3545732247259,52.9810214836684));
#221504=CARTESIAN_POINT('Ctrl Pts',(2.91448317833929,-7.35457060630938,
52.9810217684804));
#221505=CARTESIAN_POINT('Ctrl Pts',(2.91448648043816,-7.35456929774653,
52.9810219108159));
#221506=CARTESIAN_POINT('Ctrl Pts',(2.91449308627621,-7.35456667996564,
52.9810221955577));
#221507=CARTESIAN_POINT('Ctrl Pts',(2.91449638904102,-7.35456537113373,
52.9810223379219));
#221508=CARTESIAN_POINT('Ctrl Pts',(2.91450299337868,-7.35456275393713,
52.981022622599));
#221509=CARTESIAN_POINT('Ctrl Pts',(2.91450629772253,-7.35456144447433,
52.9810227650313));
#221510=CARTESIAN_POINT('Ctrl Pts',(2.91451290647998,-7.35455882551593,
52.9810230498989));
#221511=CARTESIAN_POINT('Ctrl Pts',(2.91451620989901,-7.35455751641447,
52.9810231922913));
#221512=CARTESIAN_POINT('Ctrl Pts',(2.91452281742994,-7.35455489793182,
52.981023477106));
#221513=CARTESIAN_POINT('Ctrl Pts',(2.91452612149604,-7.35455358856878,
52.9810236195263));
#221514=CARTESIAN_POINT('Ctrl Pts',(2.91453273151748,-7.35455096908886,
52.9810239044484));
#221515=CARTESIAN_POINT('Ctrl Pts',(2.91453603515875,-7.35454965988902,
52.9810240468504));
#221516=CARTESIAN_POINT('Ctrl Pts',(2.91454264288666,-7.3545470413077,52.9810243316735));
#221517=CARTESIAN_POINT('Ctrl Pts',(2.9145459479584,-7.35454573153583,52.9810244741372));
#221518=CARTESIAN_POINT('Ctrl Pts',(2.91455255838938,-7.354543111873,52.9810247590768));
#221519=CARTESIAN_POINT('Ctrl Pts',(2.91455586332221,-7.35454180215102,
52.9810249015345));
#221520=CARTESIAN_POINT('Ctrl Pts',(2.91456247215089,-7.35453918311286,
52.9810251864051));
#221521=CARTESIAN_POINT('Ctrl Pts',(2.91456577831281,-7.35453787289865,
52.9810253289157));
#221522=CARTESIAN_POINT('Ctrl Pts',(2.91457239009006,-7.35453525268167,
52.9810256139134));
#221523=CARTESIAN_POINT('Ctrl Pts',(2.91457569588938,-7.35453394260599,
52.9810257564083));
#221524=CARTESIAN_POINT('Ctrl Pts',(2.91458230879692,-7.35453132193076,
52.9810260414547));
#221525=CARTESIAN_POINT('Ctrl Pts',(2.91458561434799,-7.35453001194831,
52.981026183939));
#221526=CARTESIAN_POINT('Ctrl Pts',(2.91459222526276,-7.3545273920525,52.9810264688994));
#221527=CARTESIAN_POINT('Ctrl Pts',(2.91459553218407,-7.35452608152186,
52.9810266114428));
#221528=CARTESIAN_POINT('Ctrl Pts',(2.91460214775043,-7.35452345977231,
52.9810268966037));
#221529=CARTESIAN_POINT('Ctrl Pts',(2.91460545352993,-7.35452214968901,
52.9810270390978));
#221530=CARTESIAN_POINT('Ctrl Pts',(2.9146120675619,-7.35451952853721,52.9810273241926));
#221531=CARTESIAN_POINT('Ctrl Pts',(2.91461537403595,-7.3545182181735,52.9810274667167));
#221532=CARTESIAN_POINT('Ctrl Pts',(2.91462198598216,-7.35451559783797,
52.9810277517215));
#221533=CARTESIAN_POINT('Ctrl Pts',(2.91462529434583,-7.35451428672024,
52.981027894327));
#221534=CARTESIAN_POINT('Ctrl Pts',(2.91463190910869,-7.35451166525814,
52.9810281794533));
#221535=CARTESIAN_POINT('Ctrl Pts',(2.91463521750736,-7.35451035412137,
52.9810283220603));
#221536=CARTESIAN_POINT('Ctrl Pts',(2.91464183561226,-7.35450773132448,
52.9810286073306));
#221537=CARTESIAN_POINT('Ctrl Pts',(2.91464514285756,-7.35450642063963,
52.9810287498879));
#221538=CARTESIAN_POINT('Ctrl Pts',(2.91465175799495,-7.35450379900844,
52.9810290350303));
#221539=CARTESIAN_POINT('Ctrl Pts',(2.91465506664666,-7.35450248776106,
52.9810291776482));
#221540=CARTESIAN_POINT('Ctrl Pts',(2.9146616827465,-7.35449986573812,52.981029462832));
#221541=CARTESIAN_POINT('Ctrl Pts',(2.91466499212062,-7.35449855419927,
52.981029605481));
#221542=CARTESIAN_POINT('Ctrl Pts',(2.91467161061857,-7.3544959312156,52.9810298907682));
#221543=CARTESIAN_POINT('Ctrl Pts',(2.91467491965505,-7.3544946198054,52.9810300334027));
#221544=CARTESIAN_POINT('Ctrl Pts',(2.91468153956378,-7.35449199625228,
52.9810303187507));
#221545=CARTESIAN_POINT('Ctrl Pts',(2.91468484822723,-7.35449068498474,
52.9810304613691));
#221546=CARTESIAN_POINT('Ctrl Pts',(2.92671562101463,-7.34972271957208,
52.9815490420874));
#221547=CARTESIAN_POINT('Ctrl Pts',(2.9387313940353,-7.34492656026756,52.9820669305185));
#221548=CARTESIAN_POINT('Ctrl Pts',(2.96661305715445,-7.33371807551113,
52.9832685793568));
#221549=CARTESIAN_POINT('Ctrl Pts',(2.98247002806966,-7.32728369698994,
52.9839519324171));
#221550=CARTESIAN_POINT('Ctrl Pts',(3.02538151917038,-7.30970886645019,
52.9858011499504));
#221551=CARTESIAN_POINT('Ctrl Pts',(3.05239537216224,-7.29846967185571,
52.9869652357231));
#221552=CARTESIAN_POINT('Ctrl Pts',(3.23295511706357,-7.22216943614654,
52.9947468429668));
#221553=CARTESIAN_POINT('Ctrl Pts',(3.3844757542567,-7.15241611371773,53.0012794331881));
#221554=CARTESIAN_POINT('Ctrl Pts',(4.20685679633496,-6.74183914528896,
53.0368212952316));
#221555=CARTESIAN_POINT('Ctrl Pts',(4.828608559283,-6.31145959244081,53.0635973285695));
#221556=CARTESIAN_POINT('Ctrl Pts',(5.53379228580312,-5.6572925709027,53.0996258844541));
#221557=CARTESIAN_POINT('Ctrl Pts',(5.68166524440177,-5.50876482387663,
53.1075986853947));
#221558=CARTESIAN_POINT('Ctrl Pts',(5.86524467170673,-5.30910882763804,
53.1182653268251));
#221559=CARTESIAN_POINT('Ctrl Pts',(5.90649263824944,-5.26318117431992,
53.1207158651883));
#221560=CARTESIAN_POINT('Ctrl Pts',(5.95550269338952,-5.20730902310365,
53.1236985004562));
#221561=CARTESIAN_POINT('Ctrl Pts',(5.96378453495471,-5.19782200651623,
53.1242049993396));
#221562=CARTESIAN_POINT('Ctrl Pts',(5.9765948052464,-5.18307666256742,53.1249923708119));
#221563=CARTESIAN_POINT('Ctrl Pts',(5.98113904815341,-5.17783206008257,
53.1252724488482));
#221564=CARTESIAN_POINT('Ctrl Pts',(5.98912011610344,-5.16859642214904,
53.1257657188648));
#221565=CARTESIAN_POINT('Ctrl Pts',(5.99255987098294,-5.16460791664533,
53.1259787616843));
#221566=CARTESIAN_POINT('Ctrl Pts',(5.99981288201078,-5.15618081751876,
53.1264289344631));
#221567=CARTESIAN_POINT('Ctrl Pts',(6.0036252002764,-5.15174142367923,53.1266661122774));
#221568=CARTESIAN_POINT('Ctrl Pts',(6.01434757127685,-5.1392273001011,53.1273347746767));
#221569=CARTESIAN_POINT('Ctrl Pts',(6.02124626716762,-5.13114288817535,
53.1277668469999));
#221570=CARTESIAN_POINT('Ctrl Pts',(6.04956908506887,-5.09781630175962,
53.1295484986411));
#221571=CARTESIAN_POINT('Ctrl Pts',(6.07085072683781,-5.07245389992766,
53.1309055785729));
#221572=CARTESIAN_POINT('Ctrl Pts',(6.38457475645071,-4.6937707908609,53.1511959039074));
#221573=CARTESIAN_POINT('Ctrl Pts',(6.64584835604746,-4.31587833869546,
53.1720573887208));
#221574=CARTESIAN_POINT('Ctrl Pts',(7.12990765384459,-3.46665975050171,
53.2170098457722));
#221575=CARTESIAN_POINT('Ctrl Pts',(7.34195941994329,-2.99149422545371,
53.240965374298));
#221576=CARTESIAN_POINT('Ctrl Pts',(7.55886183626264,-2.33999921054791,
53.2707248202692));
#221577=CARTESIAN_POINT('Ctrl Pts',(7.60672215287401,-2.17939697399912,
53.2778374648674));
#221578=CARTESIAN_POINT('Ctrl Pts',(7.67228031744532,-1.93081637273955,
53.2884950348853));
#221579=CARTESIAN_POINT('Ctrl Pts',(7.69364129372632,-1.84386048548167,
53.2921586057735));
#221580=CARTESIAN_POINT('Ctrl Pts',(7.71702306430708,-1.74118483730677,
53.2964097636407));
#221581=CARTESIAN_POINT('Ctrl Pts',(7.72047811409645,-1.72580048277422,
53.2970447750595));
#221582=CARTESIAN_POINT('Ctrl Pts',(7.7256985196037,-1.70222606429507,53.2980148586746));
#221583=CARTESIAN_POINT('Ctrl Pts',(7.72749688798299,-1.69404339866473,
53.2983510242385));
#221584=CARTESIAN_POINT('Ctrl Pts',(7.73060884397527,-1.67977577468526,
53.2989362204085));
#221585=CARTESIAN_POINT('Ctrl Pts',(7.73192825243453,-1.67369210167542,
53.2991854437687));
#221586=CARTESIAN_POINT('Ctrl Pts',(7.73467029510905,-1.66097634965166,
53.2997057256528));
#221587=CARTESIAN_POINT('Ctrl Pts',(7.73609158374099,-1.65434398370694,
53.2999767394061));
#221588=CARTESIAN_POINT('Ctrl Pts',(7.73999427849783,-1.63601726266065,
53.3007246242328));
#221589=CARTESIAN_POINT('Ctrl Pts',(7.7424577142747,-1.62431907556484,53.3012008991494));
#221590=CARTESIAN_POINT('Ctrl Pts',(7.75198752207222,-1.57855034413763,
53.3030599888307));
#221591=CARTESIAN_POINT('Ctrl Pts',(7.75885564729814,-1.54443867346927,
53.30443622465));
#221592=CARTESIAN_POINT('Ctrl Pts',(7.86647901737055,-0.991065962559473,
53.3266130344015));
#221593=CARTESIAN_POINT('Ctrl Pts',(7.91513755553762,-0.463019939003818,
53.3455218999271));
#221594=CARTESIAN_POINT('Ctrl Pts',(7.90691203355497,0.523064402191629,
53.3792121188147));
#221595=CARTESIAN_POINT('Ctrl Pts',(7.86349305738964,0.978932304835636,
53.3941799175719));
#221596=CARTESIAN_POINT('Ctrl Pts',(7.71791560243968,1.7718921920976,53.4221423440559));
#221597=CARTESIAN_POINT('Ctrl Pts',(7.63221175647553,2.11071493466494,53.4347592732188));
#221598=CARTESIAN_POINT('Ctrl Pts',(7.52055111934445,2.45466684629179,53.4492388750309));
#221599=CARTESIAN_POINT('Ctrl Pts',(7.5166480646286,2.46659285937464,53.4497430674054));
#221600=CARTESIAN_POINT('Ctrl Pts',(7.51105909535235,2.48353382458279,53.4504623746172));
#221601=CARTESIAN_POINT('Ctrl Pts',(7.5093964813866,2.48855650464053,53.4506760236377));
#221602=CARTESIAN_POINT('Ctrl Pts',(7.50652629278005,2.49719814411378,53.4510442852934));
#221603=CARTESIAN_POINT('Ctrl Pts',(7.50532113454581,2.50081791068478,53.4511987444298));
#221604=CARTESIAN_POINT('Ctrl Pts',(7.50301578044834,2.50772550703525,53.4514938896054));
#221605=CARTESIAN_POINT('Ctrl Pts',(7.50191604043297,2.51101348911296,53.4516345464708));
#221606=CARTESIAN_POINT('Ctrl Pts',(7.49934122706226,2.51869482819077,53.4519635447833));
#221607=CARTESIAN_POINT('Ctrl Pts',(7.49786446361801,2.52308758516975,53.4521519950838));
#221608=CARTESIAN_POINT('Ctrl Pts',(7.49350833780352,2.53600764921127,53.4527071635878));
#221609=CARTESIAN_POINT('Ctrl Pts',(7.49061829611375,2.54453130184913,53.4530745665352));
#221610=CARTESIAN_POINT('Ctrl Pts',(7.46595341234014,2.61686971717652,53.456202244861));
#221611=CARTESIAN_POINT('Ctrl Pts',(7.44337868640597,2.68040680986584,53.4590129131883));
#221612=CARTESIAN_POINT('Ctrl Pts',(7.26465512515369,3.16375201773333,53.4808340436628));
#221613=CARTESIAN_POINT('Ctrl Pts',(7.07392806428874,3.56987715633135,53.5016737064763));
#221614=CARTESIAN_POINT('Ctrl Pts',(6.64980333807219,4.30395125281107,53.5412757944525));
#221615=CARTESIAN_POINT('Ctrl Pts',(6.42373344697784,4.63460541644503,53.5599647166545));
#221616=CARTESIAN_POINT('Ctrl Pts',(6.0663315835851,5.08064745274554,53.5855550069576));
#221617=CARTESIAN_POINT('Ctrl Pts',(5.95471733042043,5.21101753800589,53.5930930277341));
#221618=CARTESIAN_POINT('Ctrl Pts',(5.70161638419597,5.48788845325515,53.609193272877));
#221619=CARTESIAN_POINT('Ctrl Pts',(5.55853341985669,5.63276700151686,53.6176777546798));
#221620=CARTESIAN_POINT('Ctrl Pts',(5.39560899731263,5.78547442201284,53.6266944099865));
#221621=CARTESIAN_POINT('Ctrl Pts',(5.38115453462074,5.79892116018955,53.627489064347));
#221622=CARTESIAN_POINT('Ctrl Pts',(5.36007088403791,5.81838820463012,53.6286405361458));
#221623=CARTESIAN_POINT('Ctrl Pts',(5.35348163032309,5.82445152921869,53.6289993282473));
#221624=CARTESIAN_POINT('Ctrl Pts',(5.3419351589508,5.83504025780954,53.6296261704756));
#221625=CARTESIAN_POINT('Ctrl Pts',(5.33698245706216,5.83957055835489,53.6298944444511));
#221626=CARTESIAN_POINT('Ctrl Pts',(5.32738150249499,5.84833025920204,53.6304133401011));
#221627=CARTESIAN_POINT('Ctrl Pts',(5.32273396555444,5.85256043334828,53.630663997002));
#221628=CARTESIAN_POINT('Ctrl Pts',(5.31166995101668,5.86260678626034,53.6312594705137));
#221629=CARTESIAN_POINT('Ctrl Pts',(5.30524894690136,5.86841798195408,53.6316040605701));
#221630=CARTESIAN_POINT('Ctrl Pts',(5.282482700742,5.88895419477228,53.6328223336542));
#221631=CARTESIAN_POINT('Ctrl Pts',(5.26608551752779,5.90362162782722,53.6336934097733));
#221632=CARTESIAN_POINT('Ctrl Pts',(5.04870342348825,6.09644562941048,53.6451582399578));
#221633=CARTESIAN_POINT('Ctrl Pts',(4.83882593018278,6.26433042915619,53.6552816843423));
#221634=CARTESIAN_POINT('Ctrl Pts',(4.53439283331565,6.48340459753419,53.6689044957035));
#221635=CARTESIAN_POINT('Ctrl Pts',(4.44673795587198,6.54383495197679,53.6727132047741));
#221636=CARTESIAN_POINT('Ctrl Pts',(3.90006845053592,6.90465773114763,53.6958627326938));
#221637=CARTESIAN_POINT('Ctrl Pts',(3.41209070958504,7.15838194321465,53.7138267259914));
#221638=CARTESIAN_POINT('Ctrl Pts',(2.59289696593736,7.48138121527582,53.7446043561623));
#221639=CARTESIAN_POINT('Ctrl Pts',(2.27665585312476,7.58359902652599,53.7566589582212));
#221640=CARTESIAN_POINT('Ctrl Pts',(1.94288720592805,7.6687199511353,53.7704535844457));
#221641=CARTESIAN_POINT('Ctrl Pts',(1.93080150053543,7.67177176061324,53.7709545358457));
#221642=CARTESIAN_POINT('Ctrl Pts',(1.91345082602626,7.67610945121032,53.7716758177732));
#221643=CARTESIAN_POINT('Ctrl Pts',(1.90819183961635,7.67741846413984,53.7718947123061));
#221644=CARTESIAN_POINT('Ctrl Pts',(1.89906304779282,7.67968075018061,53.7722751501183));
#221645=CARTESIAN_POINT('Ctrl Pts',(1.89519385345344,7.68063650629995,53.7724365434568));
#221646=CARTESIAN_POINT('Ctrl Pts',(1.88775337878041,7.68246846415364,53.7727471830486));
#221647=CARTESIAN_POINT('Ctrl Pts',(1.88418220556449,7.68334510079831,53.7728964032048));
#221648=CARTESIAN_POINT('Ctrl Pts',(1.8757698053407,7.68540392383284,53.773248201615));
#221649=CARTESIAN_POINT('Ctrl Pts',(1.87092807499982,7.68658402497788,53.7734509036962));
#221650=CARTESIAN_POINT('Ctrl Pts',(1.85420175949626,7.69064408049221,53.7741519327338));
#221651=CARTESIAN_POINT('Ctrl Pts',(1.84231166648745,7.69350104036191,53.7746516116642));
#221652=CARTESIAN_POINT('Ctrl Pts',(1.70993435261513,7.72498428189403,53.7802293270365));
#221653=CARTESIAN_POINT('Ctrl Pts',(1.58880311180231,7.75080378720844,53.7854674400192));
#221654=CARTESIAN_POINT('Ctrl Pts',(1.15229894869493,7.83318401914403,53.8047012158067));
#221655=CARTESIAN_POINT('Ctrl Pts',(0.83417617697899,7.87341656915547,53.8193747289654));
#221656=CARTESIAN_POINT('Ctrl Pts',(-0.03065438921563,7.92978268497122,
53.8596186226031));
#221657=CARTESIAN_POINT('Ctrl Pts',(-0.578093233013222,7.9087479508543,
53.8853695287536));
#221658=CARTESIAN_POINT('Ctrl Pts',(-1.33131877502286,7.80112213093109,
53.9191452088183));
#221659=CARTESIAN_POINT('Ctrl Pts',(-1.54231498046819,7.76216399866891,
53.9284390305732));
#221660=CARTESIAN_POINT('Ctrl Pts',(-1.88812614898245,7.68365379446863,
53.9433656909064));
#221661=CARTESIAN_POINT('Ctrl Pts',(-2.02392937984187,7.64900441396915,
53.9491488711969));
#221662=CARTESIAN_POINT('Ctrl Pts',(-2.17625846638252,7.60579722761481,
53.9555524817733));
#221663=CARTESIAN_POINT('Ctrl Pts',(-2.19375432593834,7.6007693257507,53.9562867300508));
#221664=CARTESIAN_POINT('Ctrl Pts',(-2.21998217786313,7.59313394917978,
53.9573855992714));
#221665=CARTESIAN_POINT('Ctrl Pts',(-2.22872721557096,7.5905717202012,53.9577516838276));
#221666=CARTESIAN_POINT('Ctrl Pts',(-2.24374849884163,7.58614240247529,
53.9583799822557));
#221667=CARTESIAN_POINT('Ctrl Pts',(-2.25002687925856,7.58428262392344,
53.9586424324572));
#221668=CARTESIAN_POINT('Ctrl Pts',(-2.26294114735719,7.58043971885191,
53.9591819566745));
#221669=CARTESIAN_POINT('Ctrl Pts',(-2.26957675467967,7.57845566870044,
53.959459000461));
#221670=CARTESIAN_POINT('Ctrl Pts',(-2.28552684237528,7.57366375646814,
53.96012451749));
#221671=CARTESIAN_POINT('Ctrl Pts',(-2.29483877649414,7.57084741848953,
53.960512715921));
#221672=CARTESIAN_POINT('Ctrl Pts',(-2.32333884389236,7.56217033316017,
53.9616997992994));
#221673=CARTESIAN_POINT('Ctrl Pts',(-2.34250996312598,7.55625374186349,
53.9624968751169));
#221674=CARTESIAN_POINT('Ctrl Pts',(-2.55846270306019,7.48870556111712,
53.9714596967271));
#221675=CARTESIAN_POINT('Ctrl Pts',(-2.75279164653053,7.41947355374272,
53.9793737261645));
#221676=CARTESIAN_POINT('Ctrl Pts',(-3.3955273646696,7.16175663551943,54.0052355033074));
#221677=CARTESIAN_POINT('Ctrl Pts',(-3.82922184575607,6.93955709537523,
54.0220953470999));
#221678=CARTESIAN_POINT('Ctrl Pts',(-4.69015958428299,6.39303645141051,
54.0574284590475));
#221679=CARTESIAN_POINT('Ctrl Pts',(-5.11047850810296,6.06230397285203,
54.0758764021775));
#221680=CARTESIAN_POINT('Ctrl Pts',(-5.53067736776218,5.65668494604445,
54.0988492504295));
#221681=CARTESIAN_POINT('Ctrl Pts',(-5.56671212823633,5.62122697116766,
54.1008569842762));
#221682=CARTESIAN_POINT('Ctrl Pts',(-5.61156564497577,5.57623711776027,
54.1034014557561));
#221683=CARTESIAN_POINT('Ctrl Pts',(-5.62070460393262,5.56702516020896,
54.1039222978428));
#221684=CARTESIAN_POINT('Ctrl Pts',(-5.6351921783673,5.55234982403144,54.104751743595));
#221685=CARTESIAN_POINT('Ctrl Pts',(-5.64055563048404,5.54690108389462,
54.1050596406219));
#221686=CARTESIAN_POINT('Ctrl Pts',(-5.65063097395156,5.53663580139107,
54.1056395780295));
#221687=CARTESIAN_POINT('Ctrl Pts',(-5.65534462960088,5.53182099503976,
54.1059115360356));
#221688=CARTESIAN_POINT('Ctrl Pts',(-5.66591169030453,5.52099955259648,
54.1065226389316));
#221689=CARTESIAN_POINT('Ctrl Pts',(-5.67176170214238,5.51498962244065,
54.1068619375626));
#221690=CARTESIAN_POINT('Ctrl Pts',(-5.68659917213833,5.49969797173558,
54.107724996355));
#221691=CARTESIAN_POINT('Ctrl Pts',(-5.69557345448984,5.49040353228363,
54.1082493384872));
#221692=CARTESIAN_POINT('Ctrl Pts',(-5.74511552548725,5.43884186790284,
54.1111567085762));
#221693=CARTESIAN_POINT('Ctrl Pts',(-5.78523512131532,5.3961474850898,54.1135586569343));
#221694=CARTESIAN_POINT('Ctrl Pts',(-5.84706139113431,5.32887127290308,
54.1173310314572));
#221695=CARTESIAN_POINT('Ctrl Pts',(-5.86909609507175,5.30459300556864,
54.1186898985648));
#221696=CARTESIAN_POINT('Ctrl Pts',(-5.9600096526759,5.2031627499176,54.1243548977835));
#221697=CARTESIAN_POINT('Ctrl Pts',(-6.02752226395053,5.12480168981251,
54.1287024776697));
#221698=CARTESIAN_POINT('Ctrl Pts',(-6.29579401683741,4.80078536201363,
54.1465123012092));
#221699=CARTESIAN_POINT('Ctrl Pts',(-6.48322654416945,4.54448375102178,
54.1602053430769));
#221700=CARTESIAN_POINT('Ctrl Pts',(-6.9690666613559,3.78865538307987,54.1988431745692));
#221701=CARTESIAN_POINT('Ctrl Pts',(-7.2285361651983,3.26651468749628,54.2234085490936));
#221702=CARTESIAN_POINT('Ctrl Pts',(-7.5029764598599,2.51718457331221,54.2563829748878));
#221703=CARTESIAN_POINT('Ctrl Pts',(-7.56910680964462,2.31073542341048,
54.2652904526933));
#221704=CARTESIAN_POINT('Ctrl Pts',(-7.65831524081857,1.98703496228163,
54.2790002288049));
#221705=CARTESIAN_POINT('Ctrl Pts',(-7.68735643862039,1.87153726676206,
54.2838396326363));
#221706=CARTESIAN_POINT('Ctrl Pts',(-7.72150907181092,1.72146217345042,
54.2900595690303));
#221707=CARTESIAN_POINT('Ctrl Pts',(-7.72901408993107,1.68744646487597,
54.2914648921472));
#221708=CARTESIAN_POINT('Ctrl Pts',(-7.74085679063939,1.63203361669875,
54.2937470005079));
#221709=CARTESIAN_POINT('Ctrl Pts',(-7.74533097960332,1.61066619726802,
54.2946252516648));
#221710=CARTESIAN_POINT('Ctrl Pts',(-7.75377484409917,1.56949186855227,
54.2963142929539));
#221711=CARTESIAN_POINT('Ctrl Pts',(-7.75775721264313,1.54968773978843,
54.2971252168167));
#221712=CARTESIAN_POINT('Ctrl Pts',(-7.76672275293462,1.50420179989738,
54.2989843862186));
#221713=CARTESIAN_POINT('Ctrl Pts',(-7.77165448062265,1.47851006610452,
54.3000320485255));
#221714=CARTESIAN_POINT('Ctrl Pts',(-7.78447213923758,1.40990021978572,
54.3028234018497));
#221715=CARTESIAN_POINT('Ctrl Pts',(-7.79213058136303,1.36694043295633,
54.3045644926613));
#221716=CARTESIAN_POINT('Ctrl Pts',(-7.87393163691742,0.885036544939357,
54.3240226939874));
#221717=CARTESIAN_POINT('Ctrl Pts',(-7.91125398658139,0.440643456825135,
54.3412395963992));
#221718=CARTESIAN_POINT('Ctrl Pts',(-7.91086706386801,-0.234087545961717,
54.3671770834644));
#221719=CARTESIAN_POINT('Ctrl Pts',(-7.90074428252544,-0.46352253225071,
54.3759721012671));
#221720=CARTESIAN_POINT('Ctrl Pts',(-7.86129618668486,-0.912643246804813,
54.3934206776831));
#221721=CARTESIAN_POINT('Ctrl Pts',(-7.83269150091399,-1.13218111851608,
54.402060868805));
#221722=CARTESIAN_POINT('Ctrl Pts',(-7.79071161378515,-1.37453345827551,
54.4118989447882));
#221723=CARTESIAN_POINT('Ctrl Pts',(-7.78638710016935,-1.39882293362783,
54.4128883681082));
#221724=CARTESIAN_POINT('Ctrl Pts',(-7.77972307662556,-1.43526407699927,
54.414378221559));
#221725=CARTESIAN_POINT('Ctrl Pts',(-7.77746856669707,-1.44743110799853,
54.4148765561077));
#221726=CARTESIAN_POINT('Ctrl Pts',(-7.77331959517379,-1.46953249404212,
54.4157833824846));
#221727=CARTESIAN_POINT('Ctrl Pts',(-7.77143461063091,-1.47946861127073,
54.4161916536715));
#221728=CARTESIAN_POINT('Ctrl Pts',(-7.7673324638568,-1.5008676524494,54.4170721809818));
#221729=CARTESIAN_POINT('Ctrl Pts',(-7.7651089690174,-1.51232933333855,
54.4175445789451));
#221730=CARTESIAN_POINT('Ctrl Pts',(-7.75894019326233,-1.54375588693335,
54.418841917555));
#221731=CARTESIAN_POINT('Ctrl Pts',(-7.75494324185829,-1.5637104819137,
54.4196679801569));
#221732=CARTESIAN_POINT('Ctrl Pts',(-7.7332242437255,-1.67000997002164,
54.4240803529691));
#221733=CARTESIAN_POINT('Ctrl Pts',(-7.71413721812039,-1.75606865396703,
54.4276943446451));
#221734=CARTESIAN_POINT('Ctrl Pts',(-7.6516523701087,-2.0170835511992,54.4387650364541));
#221735=CARTESIAN_POINT('Ctrl Pts',(-7.6037101729826,-2.19089021926288,
54.4462870303886));
#221736=CARTESIAN_POINT('Ctrl Pts',(-7.41194139651707,-2.8036233699511,
54.4731937489262));
#221737=CARTESIAN_POINT('Ctrl Pts',(-7.23567939862982,-3.23143001827603,
54.4926573018446));
#221738=CARTESIAN_POINT('Ctrl Pts',(-7.00125805147646,-3.68355257673471,
54.5136840094165));
#221739=CARTESIAN_POINT('Ctrl Pts',(-6.97903134270909,-3.72549264374597,
54.5156396413139));
#221740=CARTESIAN_POINT('Ctrl Pts',(-6.88085214365688,-3.90678673052697,
54.5241160556178));
#221741=CARTESIAN_POINT('Ctrl Pts',(-6.80109250648502,-4.04403891838817,
54.5305915993251));
#221742=CARTESIAN_POINT('Ctrl Pts',(-6.69338959760291,-4.21716710002389,
54.538847930818));
#221743=CARTESIAN_POINT('Ctrl Pts',(-6.66919350359408,-4.25532850618024,
54.540673536942));
#221744=CARTESIAN_POINT('Ctrl Pts',(-6.62999295380238,-4.31599884320318,
54.5435857055036));
#221745=CARTESIAN_POINT('Ctrl Pts',(-6.6151977487487,-4.33864164607268,
54.5446747572055));
#221746=CARTESIAN_POINT('Ctrl Pts',(-6.5882515373331,-4.37942225393369,
54.5466403262516));
#221747=CARTESIAN_POINT('Ctrl Pts',(-6.57614103070698,-4.39758646814392,
54.5475173149181));
#221748=CARTESIAN_POINT('Ctrl Pts',(-6.54734012708687,-4.44039912161655,
54.549588023646));
#221749=CARTESIAN_POINT('Ctrl Pts',(-6.53058547562071,-4.46500397002371,
54.5507809712487));
#221750=CARTESIAN_POINT('Ctrl Pts',(-6.48062742095259,-4.53748651870606,
54.5543042049303));
#221751=CARTESIAN_POINT('Ctrl Pts',(-6.44703343617735,-4.58509275844188,
54.5566299084139));
#221752=CARTESIAN_POINT('Ctrl Pts',(-6.21838340084642,-4.90163228966447,
54.572179911753));
#221753=CARTESIAN_POINT('Ctrl Pts',(-6.00707170675512,-5.15842908038931,
54.5852613213391));
#221754=CARTESIAN_POINT('Ctrl Pts',(-5.60904732433313,-5.58438728797675,
54.6078867167073));
#221755=CARTESIAN_POINT('Ctrl Pts',(-5.42923799794173,-5.7593552614092,
54.6174778847388));
#221756=CARTESIAN_POINT('Ctrl Pts',(-4.73596972671233,-6.37258868107269,
54.6524278010461));
#221757=CARTESIAN_POINT('Ctrl Pts',(-4.17544233568427,-6.75313522176013,
54.6765714295174));
#221758=CARTESIAN_POINT('Ctrl Pts',(-3.49568977349531,-7.09730080246153,
54.7062397503744));
#221759=CARTESIAN_POINT('Ctrl Pts',(-3.41724431650202,-7.1354023243537,
54.709674515105));
#221760=CARTESIAN_POINT('Ctrl Pts',(-3.32569721832532,-7.17801147898649,
54.7137110346409));
#221761=CARTESIAN_POINT('Ctrl Pts',(-3.31319255663347,-7.18379188592281,
54.7142629960643));
#221762=CARTESIAN_POINT('Ctrl Pts',(-3.29329178320488,-7.19292820723781,
54.7151424686008));
#221763=CARTESIAN_POINT('Ctrl Pts',(-3.28590546146572,-7.196305459158,54.7154691193393));
#221764=CARTESIAN_POINT('Ctrl Pts',(-3.27289843750078,-7.20222846700842,
54.7160447591127));
#221765=CARTESIAN_POINT('Ctrl Pts',(-3.26727992608159,-7.20477903599653,
54.7162935502082));
#221766=CARTESIAN_POINT('Ctrl Pts',(-3.25569369712998,-7.21002235884941,
54.7168068896717));
#221767=CARTESIAN_POINT('Ctrl Pts',(-3.24972561061869,-7.21271428243209,
54.7170714723439));
#221768=CARTESIAN_POINT('Ctrl Pts',(-3.2345118760153,-7.21955376795084,
54.7177463657334));
#221769=CARTESIAN_POINT('Ctrl Pts',(-3.22526160448074,-7.22369097247584,
54.7181571137681));
#221770=CARTESIAN_POINT('Ctrl Pts',(-3.18803904983219,-7.24025309259574,
54.7198116304288));
#221771=CARTESIAN_POINT('Ctrl Pts',(-3.16000295443897,-7.25253328979102,
54.721061647384));
#221772=CARTESIAN_POINT('Ctrl Pts',(-2.98589340877544,-7.32759445087228,
54.7288520001625));
#221773=CARTESIAN_POINT('Ctrl Pts',(-2.8380462943876,-7.3861141699198,54.7356076042871));
#221774=CARTESIAN_POINT('Ctrl Pts',(-2.58992900809067,-7.47577315816816,
54.74710723741));
#221775=CARTESIAN_POINT('Ctrl Pts',(-2.4906141491953,-7.50944449366486,
54.7517494897539));
#221776=CARTESIAN_POINT('Ctrl Pts',(-1.43726275669575,-7.84337414811336,
54.8012165261127));
#221777=CARTESIAN_POINT('Ctrl Pts',(-0.434792823876008,-7.96216655253596,
54.8489632567107));
#221778=CARTESIAN_POINT('Ctrl Pts',(0.616449503353414,-7.88712575600834,
54.8921867569514));
#221779=CARTESIAN_POINT('Ctrl Pts',(0.669582528429679,-7.88279278289727,
54.8943569718477));
#221780=CARTESIAN_POINT('Ctrl Pts',(0.737297255389228,-7.87658108334241,
54.8971047884567));
#221781=CARTESIAN_POINT('Ctrl Pts',(0.751922427519911,-7.87519837662244,
54.8976971969171));
#221782=CARTESIAN_POINT('Ctrl Pts',(0.775153156405917,-7.87293677157096,
54.8986364956258));
#221783=CARTESIAN_POINT('Ctrl Pts',(0.783761236428558,-7.87208448569377,
54.8989841818111));
#221784=CARTESIAN_POINT('Ctrl Pts',(0.799813335686963,-7.87046857715947,
54.8996318538304));
#221785=CARTESIAN_POINT('Ctrl Pts',(0.807257698493105,-7.86970850823591,
54.8999319457178));
#221786=CARTESIAN_POINT('Ctrl Pts',(0.823786502598141,-7.8679972184551,
54.9005976373648));
#221787=CARTESIAN_POINT('Ctrl Pts',(0.832870403531804,-7.86704082378435,
54.9009630816766));
#221788=CARTESIAN_POINT('Ctrl Pts',(0.85915886929496,-7.86422701117024,
54.9020194943953));
#221789=CARTESIAN_POINT('Ctrl Pts',(0.876359068959876,-7.86232886826909,
54.9027092411659));
#221790=CARTESIAN_POINT('Ctrl Pts',(0.994221373760253,-7.84893049708849,
54.9074258349511));
#221791=CARTESIAN_POINT('Ctrl Pts',(1.09466266891507,-7.83555362637779,
54.9113960245377));
#221792=CARTESIAN_POINT('Ctrl Pts',(1.37897901975434,-7.7921141856775,54.9225084722948));
#221793=CARTESIAN_POINT('Ctrl Pts',(1.56209040980258,-7.75748058331131,
54.9295137451526));
#221794=CARTESIAN_POINT('Ctrl Pts',(2.25792280637528,-7.60023094988118,
54.955736439059));
#221795=CARTESIAN_POINT('Ctrl Pts',(2.75914757479126,-7.43295687460698,
54.9737008228036));
#221796=CARTESIAN_POINT('Ctrl Pts',(3.68135926837173,-7.01894369588516,
55.0087212779305));
#221797=CARTESIAN_POINT('Ctrl Pts',(4.10356977213113,-6.78075220247433,
55.0257052435565));
#221798=CARTESIAN_POINT('Ctrl Pts',(4.52604174807477,-6.48843354093584,
55.0460505242683));
#221799=CARTESIAN_POINT('Ctrl Pts',(4.55065131485444,-6.47119743852568,
55.0472486735376));
#221800=CARTESIAN_POINT('Ctrl Pts',(4.58285692998871,-6.44836664068558,
55.0488331527018));
#221801=CARTESIAN_POINT('Ctrl Pts',(4.59054226993995,-6.44289776732519,
55.0492125058542));
#221802=CARTESIAN_POINT('Ctrl Pts',(4.6024042942724,-6.43442477471288,55.0497999230572));
#221803=CARTESIAN_POINT('Ctrl Pts',(4.60658787749039,-6.43143029163432,
55.0500074638262));
#221804=CARTESIAN_POINT('Ctrl Pts',(4.61484158300029,-6.42551035234188,
55.0504176355482));
#221805=CARTESIAN_POINT('Ctrl Pts',(4.61891185250142,-6.42258510437476,
55.0506202553047));
#221806=CARTESIAN_POINT('Ctrl Pts',(4.62789955109062,-6.4161128035415,55.0510684264516));
#221807=CARTESIAN_POINT('Ctrl Pts',(4.63281568345979,-6.41256396502293,
55.0513140725527));
#221808=CARTESIAN_POINT('Ctrl Pts',(4.64302421396867,-6.40517680402366,
55.0518252045324));
#221809=CARTESIAN_POINT('Ctrl Pts',(4.64831594371214,-6.40133756564769,
55.0520907383148));
#221810=CARTESIAN_POINT('Ctrl Pts',(4.66189686041151,-6.39145866381124,
55.0527736978922));
#221811=CARTESIAN_POINT('Ctrl Pts',(4.67017905681166,-6.38540944374524,
55.0531916161231));
#221812=CARTESIAN_POINT('Ctrl Pts',(4.69421276456808,-6.36778373115723,
55.0544084345532));
#221813=CARTESIAN_POINT('Ctrl Pts',(4.70993309386602,-6.35616498904592,
55.0552094590927));
#221814=CARTESIAN_POINT('Ctrl Pts',(5.29193362977246,-5.92266940393472,
55.0850504672423));
#221815=CARTESIAN_POINT('Ctrl Pts',(5.79923763835632,-5.42692318221993,
55.1172000364732));
#221816=CARTESIAN_POINT('Ctrl Pts',(6.48358919502754,-4.55096972711259,
55.1652773749016));
#221817=CARTESIAN_POINT('Ctrl Pts',(6.70825066077856,-4.21279796056472,
55.1822983748031));
#221818=CARTESIAN_POINT('Ctrl Pts',(6.92425700366949,-3.82622330959298,
55.2002345752718));
#221819=CARTESIAN_POINT('Ctrl Pts',(6.9422692131843,-3.79344409058826,55.2017445629007));
#221820=CARTESIAN_POINT('Ctrl Pts',(6.96747478046474,-3.7467933298125,55.2038786024422));
#221821=CARTESIAN_POINT('Ctrl Pts',(6.97486046265915,-3.73302646671918,
55.2045065359381));
#221822=CARTESIAN_POINT('Ctrl Pts',(6.98832055818766,-3.70775753901179,
55.2056557949338));
#221823=CARTESIAN_POINT('Ctrl Pts',(6.99440747229689,-3.69626220724765,
55.2061773668574));
#221824=CARTESIAN_POINT('Ctrl Pts',(7.00667617124315,-3.67295355242057,
55.2072324440797));
#221825=CARTESIAN_POINT('Ctrl Pts',(7.01285649846355,-3.66113950841705,
55.2077659196643));
#221826=CARTESIAN_POINT('Ctrl Pts',(7.02799754695141,-3.63201752973426,
55.2090778166863));
#221827=CARTESIAN_POINT('Ctrl Pts',(7.0369242413197,-3.61469197607792,55.2098555851904));
#221828=CARTESIAN_POINT('Ctrl Pts',(7.06887103757555,-3.55212054298723,
55.2126549217877));
#221829=CARTESIAN_POINT('Ctrl Pts',(7.09151973038163,-3.50668591169718,
55.2146697092169));
#221830=CARTESIAN_POINT('Ctrl Pts',(7.21192339744033,-3.25921114755375,
55.2255497534726));
#221831=CARTESIAN_POINT('Ctrl Pts',(7.30148584487766,-3.05329431063649,
55.2342598561714));
#221832=CARTESIAN_POINT('Ctrl Pts',(7.4949716180313,-2.55103523509234,55.254802660372));
#221833=CARTESIAN_POINT('Ctrl Pts',(7.59025087707266,-2.25177272638997,
55.2664734339752));
#221834=CARTESIAN_POINT('Ctrl Pts',(7.80112650043722,-1.42159167739227,
55.2980519045625));
#221835=CARTESIAN_POINT('Ctrl Pts',(7.88024951926195,-0.883227583544129,
55.3176140994103));
#221836=CARTESIAN_POINT('Ctrl Pts',(7.90703841821882,-0.262412077518545,
55.3419046805517));
#221837=CARTESIAN_POINT('Ctrl Pts',(7.90925787588008,-0.183728086002174,
55.345016780243));
#221838=CARTESIAN_POINT('Ctrl Pts',(7.91047595157171,-0.0919853300617438,
55.3486948175989));
#221839=CARTESIAN_POINT('Ctrl Pts',(7.91061684255294,-0.0789445954374625,
55.3492187952998));
#221840=CARTESIAN_POINT('Ctrl Pts',(7.91079014638393,-0.058142111105068,
55.3500565647246));
#221841=CARTESIAN_POINT('Ctrl Pts',(7.91084338405457,-0.0503805282363616,
55.3503695708268));
#221842=CARTESIAN_POINT('Ctrl Pts',(7.91091652925125,-0.0368033760274333,
55.3509178676722));
#221843=CARTESIAN_POINT('Ctrl Pts',(7.91094144683786,-0.0309878320969655,
55.3511529661507));
#221844=CARTESIAN_POINT('Ctrl Pts',(7.91097961879299,-0.0189914274697496,
55.351638443931));
#221845=CARTESIAN_POINT('Ctrl Pts',(7.91099204223478,-0.0128105694601785,
55.3518888553203));
#221846=CARTESIAN_POINT('Ctrl Pts',(7.91100512741119,0.0028034951340082,
55.3525221640952));
#221847=CARTESIAN_POINT('Ctrl Pts',(7.91099616028461,0.0122366844166195,
55.3529054397927));
#221848=CARTESIAN_POINT('Ctrl Pts',(7.91094053542195,0.0325435852834091,
55.3537319842501));
#221849=CARTESIAN_POINT('Ctrl Pts',(7.91088833067868,0.0434172528264745,
55.3541754747805));
#221850=CARTESIAN_POINT('Ctrl Pts',(7.91067702513212,0.0742070115765184,
55.3554338852622));
#221851=CARTESIAN_POINT('Ctrl Pts',(7.91046513226251,0.0941225662792637,
55.3562509684261));
#221852=CARTESIAN_POINT('Ctrl Pts',(7.90790191464639,0.27192022472201,55.3635746764319));
#221853=CARTESIAN_POINT('Ctrl Pts',(7.90090009270303,0.429675636351487,
55.370299442748));
#221854=CARTESIAN_POINT('Ctrl Pts',(7.88141634415975,0.691485561427953,
55.381777868643));
#221855=CARTESIAN_POINT('Ctrl Pts',(7.87157821093175,0.795695425339125,
55.3864265097527));
#221856=CARTESIAN_POINT('Ctrl Pts',(7.75383859127071,1.82428202577128,55.4329098480358));
#221857=CARTESIAN_POINT('Ctrl Pts',(7.485607250148,2.72332626818989,55.477213874366));
#221858=CARTESIAN_POINT('Ctrl Pts',(7.04436380502909,3.60047786289725,55.5174219828695));
#221859=CARTESIAN_POINT('Ctrl Pts',(7.02109529922987,3.64564441326285,55.5194868007979));
#221860=CARTESIAN_POINT('Ctrl Pts',(6.99099690496271,3.70271133776944,55.5220887725884));
#221861=CARTESIAN_POINT('Ctrl Pts',(6.98456927220815,3.71482180734349,55.5226405548882));
#221862=CARTESIAN_POINT('Ctrl Pts',(6.97433644049507,3.73398130428023,55.5235128891819));
#221863=CARTESIAN_POINT('Ctrl Pts',(6.97055197703984,3.74104133922951,55.5238341999685));
#221864=CARTESIAN_POINT('Ctrl Pts',(6.96349182650797,3.75416436396925,55.5244311985998));
#221865=CARTESIAN_POINT('Ctrl Pts',(6.96021892973312,3.76022884144655,55.5247069885492));
#221866=CARTESIAN_POINT('Ctrl Pts',(6.95295629677151,3.77364408584432,55.525316848845));
#221867=CARTESIAN_POINT('Ctrl Pts',(6.94896281667145,3.78099282259753,55.5256507808675));
#221868=CARTESIAN_POINT('Ctrl Pts',(6.93743911383342,3.80211862687295,55.5266103448307));
#221869=CARTESIAN_POINT('Ctrl Pts',(6.92987950091776,3.8158796649663,55.5272348902411));
#221870=CARTESIAN_POINT('Ctrl Pts',(6.87961244810827,3.90674056717534,55.5313553786714));
#221871=CARTESIAN_POINT('Ctrl Pts',(6.83565926072647,3.98314604550887,55.5348047653676));
#221872=CARTESIAN_POINT('Ctrl Pts',(6.70753364389809,4.19750211085642,55.5444454890998));
#221873=CARTESIAN_POINT('Ctrl Pts',(6.62039734600867,4.33363290545073,55.5505234029967));
#221874=CARTESIAN_POINT('Ctrl Pts',(6.44756714864027,4.58624831506854,55.5617693887955));
#221875=CARTESIAN_POINT('Ctrl Pts',(6.36273176013428,4.70323743725388,55.5669636651061));
#221876=CARTESIAN_POINT('Ctrl Pts',(6.21989164740532,4.88927186892742,55.57524845031));
#221877=CARTESIAN_POINT('Ctrl Pts',(6.1638292366516,4.95976219725351,55.5783939022713));
#221878=CARTESIAN_POINT('Ctrl Pts',(6.06118459520204,5.08439377004502,55.583982441492));
#221879=CARTESIAN_POINT('Ctrl Pts',(6.01505006641264,5.13889010961267,55.5864357677979));
#221880=CARTESIAN_POINT('Ctrl Pts',(5.65044116183605,5.55794569938099,55.6054155013654));
#221881=CARTESIAN_POINT('Ctrl Pts',(5.29986617697838,5.89318520828578,55.6212173823318));
#221882=CARTESIAN_POINT('Ctrl Pts',(4.84985227492496,6.25068634738431,55.641288792889));
#221883=CARTESIAN_POINT('Ctrl Pts',(4.77787352705255,6.30587589948935,55.6444955047424));
#221884=CARTESIAN_POINT('Ctrl Pts',(4.69398335766373,6.36793748210256,55.6482471553391));
#221885=CARTESIAN_POINT('Ctrl Pts',(4.68298251854409,6.37603185896641,55.6487394023981));
#221886=CARTESIAN_POINT('Ctrl Pts',(4.49712898061499,6.51204175245371,55.6570612951302));
#221887=CARTESIAN_POINT('Ctrl Pts',(4.31712767229245,6.63274089344022,55.6652044103897));
#221888=CARTESIAN_POINT('Ctrl Pts',(4.12078984027477,6.75301399004028,55.6744139692693));
#221889=CARTESIAN_POINT('Ctrl Pts',(4.1091463895922,6.76010523599476,55.6749613153992));
#221890=CARTESIAN_POINT('Ctrl Pts',(4.09314504405239,6.76979396923635,55.6757152303537));
#221891=CARTESIAN_POINT('Ctrl Pts',(4.08880283291325,6.77241745102042,55.6759199889666));
#221892=CARTESIAN_POINT('Ctrl Pts',(4.08138761075529,6.77688785692618,55.6762699553073));
#221893=CARTESIAN_POINT('Ctrl Pts',(4.07831585748665,6.77873687504273,55.6764150161143));
#221894=CARTESIAN_POINT('Ctrl Pts',(4.07235573382361,6.78231900780226,55.6766966490261));
#221895=CARTESIAN_POINT('Ctrl Pts',(4.06946751122572,6.78405236723615,55.6768332037838));
#221896=CARTESIAN_POINT('Ctrl Pts',(4.06350569662145,6.78762515789051,55.6771152401273));
#221897=CARTESIAN_POINT('Ctrl Pts',(4.06043195786432,6.78946434897916,55.6772607389915));
#221898=CARTESIAN_POINT('Ctrl Pts',(4.05081979674586,6.79520698449249,55.6777160227102));
#221899=CARTESIAN_POINT('Ctrl Pts',(4.04427701171192,6.79910306139824,55.6780263298881));
#221900=CARTESIAN_POINT('Ctrl Pts',(4.007496446712,6.82093316076346,55.6797729606704));
#221901=CARTESIAN_POINT('Ctrl Pts',(3.97714546095821,6.83867464189511,55.681222699086));
#221902=CARTESIAN_POINT('Ctrl Pts',(3.88928541947689,6.88924997713737,55.6854410384317));
#221903=CARTESIAN_POINT('Ctrl Pts',(3.83148209662901,6.92156418626674,55.6882428045681));
#221904=CARTESIAN_POINT('Ctrl Pts',(3.61021145596674,7.04164165693944,55.6990455965559));
#221905=CARTESIAN_POINT('Ctrl Pts',(3.44408715668642,7.12436663781493,55.7073142573033));
#221906=CARTESIAN_POINT('Ctrl Pts',(3.0852830946315,7.28755702932442,55.725245810854));
#221907=CARTESIAN_POINT('Ctrl Pts',(2.89200826596929,7.36639281472405,55.734946317405));
#221908=CARTESIAN_POINT('Ctrl Pts',(2.433950147589,7.5324239312153,55.7576900166131));
#221909=CARTESIAN_POINT('Ctrl Pts',(2.167213369983,7.61345630018782,55.770743645551));
#221910=CARTESIAN_POINT('Ctrl Pts',(1.41041541625579,7.80035901900882,55.8065585580959));
#221911=CARTESIAN_POINT('Ctrl Pts',(0.913718627602875,7.87401551902733,
55.8285887029286));
#221912=CARTESIAN_POINT('Ctrl Pts',(0.380234885885243,7.90192636349685,
55.8502898363374));
#221913=CARTESIAN_POINT('Ctrl Pts',(0.347135910286013,7.90344959621687,
55.8516287716143));
#221914=CARTESIAN_POINT('Ctrl Pts',(0.302608450095644,7.90521851304922,
55.8534201137061));
#221915=CARTESIAN_POINT('Ctrl Pts',(0.291187844994659,7.90564742785708,
55.8538786896639));
#221916=CARTESIAN_POINT('Ctrl Pts',(0.273274757894683,7.90628130664492,
55.8545965954802));
#221917=CARTESIAN_POINT('Ctrl Pts',(0.266782907955704,7.90650302430878,
55.854856489271));
#221918=CARTESIAN_POINT('Ctrl Pts',(0.254325869587166,7.90691311263696,
55.8553546549386));
#221919=CARTESIAN_POINT('Ctrl Pts',(0.248360728385151,7.90710272903696,
55.8555929685846));
#221920=CARTESIAN_POINT('Ctrl Pts',(0.234357082804797,7.90753200641666,
55.8561518755499));
#221921=CARTESIAN_POINT('Ctrl Pts',(0.226318408897982,7.90776616074927,
55.8564722833496));
#221922=CARTESIAN_POINT('Ctrl Pts',(0.203117438986491,7.90840656298365,
55.857395804963));
#221923=CARTESIAN_POINT('Ctrl Pts',(0.187954273129431,7.90878146456195,
55.8579978640955));
#221924=CARTESIAN_POINT('Ctrl Pts',(0.0859150395957425,7.91101071154047,
55.8620392710231));
#221925=CARTESIAN_POINT('Ctrl Pts',(-0.000987040249993028,7.91147720328216,
55.8654317933009));
#221926=CARTESIAN_POINT('Ctrl Pts',(-0.219174209855252,7.90905327265437,
55.8738342414234));
#221927=CARTESIAN_POINT('Ctrl Pts',(-0.350413887905194,7.90432622629885,
55.8787832286093));
#221928=CARTESIAN_POINT('Ctrl Pts',(-0.715355012722817,7.88207393163809,
55.8923005511797));
#221929=CARTESIAN_POINT('Ctrl Pts',(-0.948488714424283,7.85742956072827,
55.9006523087725));
#221930=CARTESIAN_POINT('Ctrl Pts',(-1.24601193570906,7.81254157969881,
55.9111367234525));
#221931=CARTESIAN_POINT('Ctrl Pts',(-1.31170287182357,7.80178103866956,
55.9134409910735));
#221932=CARTESIAN_POINT('Ctrl Pts',(-1.43117515333971,7.78065918940041,
55.917620260368));
#221933=CARTESIAN_POINT('Ctrl Pts',(-1.48499944668865,7.77056603047045,
55.919498817032));
#221934=CARTESIAN_POINT('Ctrl Pts',(-1.58405744677661,7.7509238027929,55.9229529984494));
#221935=CARTESIAN_POINT('Ctrl Pts',(-1.62932049762711,7.74153554068138,
55.9245301347176));
#221936=CARTESIAN_POINT('Ctrl Pts',(-1.71325995073063,7.7233564103393,55.9274557488279));
#221937=CARTESIAN_POINT('Ctrl Pts',(-1.75195750340065,7.71467036324937,
55.928804845002));
#221938=CARTESIAN_POINT('Ctrl Pts',(-1.8241025079016,7.69790587777259,55.9313226805811));
#221939=CARTESIAN_POINT('Ctrl Pts',(-1.85756571872462,7.68989950940108,
55.9324916157818));
#221940=CARTESIAN_POINT('Ctrl Pts',(-2.1596775417065,7.61552951954678,55.9430614639445));
#221941=CARTESIAN_POINT('Ctrl Pts',(-2.42471646702756,7.53533268053587,
55.9524452512352));
#221942=CARTESIAN_POINT('Ctrl Pts',(-2.95607903622881,7.34360731760556,
55.9723801599168));
#221943=CARTESIAN_POINT('Ctrl Pts',(-3.22158867360532,7.23106554033772,
55.9829510820967));
#221944=CARTESIAN_POINT('Ctrl Pts',(-3.49606027988588,7.09660410990899,
55.9951418009379));
#221945=CARTESIAN_POINT('Ctrl Pts',(-3.51175327603105,7.08885155030967,
55.995843337483));
#221946=CARTESIAN_POINT('Ctrl Pts',(-3.53313260041945,7.07820144900475,
55.9968054142405));
#221947=CARTESIAN_POINT('Ctrl Pts',(-3.53884123849446,7.07534906651966,
55.9970629196426));
#221948=CARTESIAN_POINT('Ctrl Pts',(-3.54790973421809,7.07080417428842,
55.997472951894));
#221949=CARTESIAN_POINT('Ctrl Pts',(-3.55127185748557,7.06911616451666,
55.9976251826567));
#221950=CARTESIAN_POINT('Ctrl Pts',(-3.55779838601845,7.0658335814399,55.9979211023692));
#221951=CARTESIAN_POINT('Ctrl Pts',(-3.56096292715563,7.06423927875445,
55.9980647736179));
#221952=CARTESIAN_POINT('Ctrl Pts',(-3.56750351977011,7.06093860233166,
55.9983621050999));
#221953=CARTESIAN_POINT('Ctrl Pts',(-3.57087942036125,7.0592319323435,55.998515784577));
#221954=CARTESIAN_POINT('Ctrl Pts',(-3.57853197278513,7.05535632791345,
55.9988646290135));
#221955=CARTESIAN_POINT('Ctrl Pts',(-3.58280787566428,7.0531859269385,55.999059888622));
#221956=CARTESIAN_POINT('Ctrl Pts',(-3.603381548481,7.04271942214215,56.0000010204206));
#221957=CARTESIAN_POINT('Ctrl Pts',(-3.61965237131838,7.0343707709444,56.0007502558238));
#221958=CARTESIAN_POINT('Ctrl Pts',(-3.66031519777789,7.01332800916777,
56.0026347901358));
#221959=CARTESIAN_POINT('Ctrl Pts',(-3.68467008840576,7.00056307849199,
56.0037744742592));
#221960=CARTESIAN_POINT('Ctrl Pts',(-3.78099729385834,6.94943395466464,
56.0083241469871));
#221961=CARTESIAN_POINT('Ctrl Pts',(-3.85243910919269,6.91008573813601,
56.011791970731));
#221962=CARTESIAN_POINT('Ctrl Pts',(-4.13745763107289,6.74731143776999,
56.0259677778496));
#221963=CARTESIAN_POINT('Ctrl Pts',(-4.34580693950223,6.61503701137007,
56.0371090797736));
#221964=CARTESIAN_POINT('Ctrl Pts',(-5.30920869592848,5.93822335211284,
56.0912800273718));
#221965=CARTESIAN_POINT('Ctrl Pts',(-5.97066924491027,5.27277118452364,
56.1355515754416));
#221966=CARTESIAN_POINT('Ctrl Pts',(-6.5341371864934,4.46007924211345,56.176158837364));
#221967=CARTESIAN_POINT('Ctrl Pts',(-6.56651967412693,4.41226417757633,
56.1785102187326));
#221968=CARTESIAN_POINT('Ctrl Pts',(-6.6065287644229,4.35177171854595,56.1814386607794));
#221969=CARTESIAN_POINT('Ctrl Pts',(-6.61464681290655,4.33942242113643,
56.1820340913721));
#221970=CARTESIAN_POINT('Ctrl Pts',(-6.62736485325176,4.31995693252685,
56.1829688848917));
#221971=CARTESIAN_POINT('Ctrl Pts',(-6.63198807868977,4.31285600521238,
56.1833091116291));
#221972=CARTESIAN_POINT('Ctrl Pts',(-6.64012398252134,4.3003158512327,56.183908574154));
#221973=CARTESIAN_POINT('Ctrl Pts',(-6.6436414044089,4.29487972049184,56.1841679856497));
#221974=CARTESIAN_POINT('Ctrl Pts',(-6.65166890616065,4.28243986012553,
56.1847605788891));
#221975=CARTESIAN_POINT('Ctrl Pts',(-6.65617460908818,4.27543330747374,
56.1850935986572));
#221976=CARTESIAN_POINT('Ctrl Pts',(-6.66851293711726,4.2561799235453,56.1860066602377));
#221977=CARTESIAN_POINT('Ctrl Pts',(-6.67632290228966,4.24391857147661,
56.1865858668019));
#221978=CARTESIAN_POINT('Ctrl Pts',(-6.7171592949207,4.17941526557387,56.1896210763298));
#221979=CARTESIAN_POINT('Ctrl Pts',(-6.74960687384587,4.12680847860903,
56.192055848706));
#221980=CARTESIAN_POINT('Ctrl Pts',(-7.08204139587035,3.57342620551511,
56.2172590565886));
#221981=CARTESIAN_POINT('Ctrl Pts',(-7.32635415445363,3.0412647168216,56.2378565042868));
#221982=CARTESIAN_POINT('Ctrl Pts',(-7.66838630813713,2.00846680578221,
56.2755917055936));
#221983=CARTESIAN_POINT('Ctrl Pts',(-7.7807572772411,1.51585918976673,56.2928000614765));
#221984=CARTESIAN_POINT('Ctrl Pts',(-7.84981220511726,0.982599014530777,
56.3131926255566));
#221985=CARTESIAN_POINT('Ctrl Pts',(-7.85391919466974,0.949213209538551,
56.3144767962577));
#221986=CARTESIAN_POINT('Ctrl Pts',(-7.86923715244024,0.817781333682439,
56.3195646681704));
#221987=CARTESIAN_POINT('Ctrl Pts',(-7.8788254213886,0.719560665028929,
56.323440829787));
#221988=CARTESIAN_POINT('Ctrl Pts',(-7.88790269596649,0.604316621768899,
56.3280597818904));
#221989=CARTESIAN_POINT('Ctrl Pts',(-7.88917767045129,0.587437825892734,
56.3287380505002));
#221990=CARTESIAN_POINT('Ctrl Pts',(-7.89101957623093,0.561965493110897,
56.3297642134599));
#221991=CARTESIAN_POINT('Ctrl Pts',(-7.89162666633343,0.553374851673178,
56.330110731003));
#221992=CARTESIAN_POINT('Ctrl Pts',(-7.89266831739549,0.538284558459132,
56.3307201797341));
#221993=CARTESIAN_POINT('Ctrl Pts',(-7.89310888095752,0.531785320748647,
56.3309829097867));
#221994=CARTESIAN_POINT('Ctrl Pts',(-7.89396160508928,0.518971312901581,
56.3315013913042));
#221995=CARTESIAN_POINT('Ctrl Pts',(-7.89437421714418,0.512656576740334,
56.3317571277389));
#221996=CARTESIAN_POINT('Ctrl Pts',(-7.89524826889938,0.499028526229135,
56.3323095279262));
#221997=CARTESIAN_POINT('Ctrl Pts',(-7.89570712487282,0.491715055083747,
56.3326062748875));
#221998=CARTESIAN_POINT('Ctrl Pts',(-7.89679491331828,0.473983160246461,
56.3333264730549));
#221999=CARTESIAN_POINT('Ctrl Pts',(-7.89741338941203,0.463564121619056,
56.3337502545563));
#222000=CARTESIAN_POINT('Ctrl Pts',(-7.89904055939394,0.435203580163036,
56.3349053804877));
#222001=CARTESIAN_POINT('Ctrl Pts',(-7.90000874154438,0.417259863033981,
56.3356379667097));
#222002=CARTESIAN_POINT('Ctrl Pts',(-7.90760136725193,0.267030132472929,
56.3417852675347));
#222003=CARTESIAN_POINT('Ctrl Pts',(-7.91096353872841,0.134603956130085,
56.3472937751941));
#222004=CARTESIAN_POINT('Ctrl Pts',(-7.91099970505067,0.00216025190750625,
56.3528639154922));
#222005=CARTESIAN_POINT('',(-7.90376924347838,0.00391285016959399,58.3576684917633));
#222006=CARTESIAN_POINT('Ctrl Pts',(-7.91934491493686,0.00236459517639777,
56.3576684917633));
#222007=CARTESIAN_POINT('Ctrl Pts',(-7.91655862145948,-1.0192215766598,
56.3988061866928));
#222008=CARTESIAN_POINT('Ctrl Pts',(-7.44280733691386,-3.36276887012757,
56.4929286702307));
#222009=CARTESIAN_POINT('Ctrl Pts',(-5.2119713477239,-6.39936160446072,
56.6400359423766));
#222010=CARTESIAN_POINT('Ctrl Pts',(-1.51916769345754,-8.09428556441302,
56.7989903082015));
#222011=CARTESIAN_POINT('Ctrl Pts',(3.93614139152782,-7.78672095142199,
57.0109294626343));
#222012=CARTESIAN_POINT('Ctrl Pts',(8.00548149351692,-3.47511119767746,
57.2228686170676));
#222013=CARTESIAN_POINT('Ctrl Pts',(7.98567764449062,1.97927930609152,57.4348077715004));
#222014=CARTESIAN_POINT('Ctrl Pts',(5.47176008357,6.78967631460865,57.6467469259335));
#222015=CARTESIAN_POINT('Ctrl Pts',(-1.56877482900821,9.23236030490876,
57.9116708689747));
#222016=CARTESIAN_POINT('Ctrl Pts',(-7.21413900831743,4.76026128847,58.1663063204541));
#222017=CARTESIAN_POINT('Ctrl Pts',(-7.90544983343671,1.06880511690692,
58.3149721947169));
#222018=CARTESIAN_POINT('Ctrl Pts',(-7.8990614508284,0.00646042416755821,
58.3576684917633));
#222019=CARTESIAN_POINT('',(-7.90710165646731,-0.00603558549463476,60.3576684917633));
#222020=CARTESIAN_POINT('Ctrl Pts',(-7.911,-6.63413768364762E-12,58.3576684917633));
#222021=CARTESIAN_POINT('Ctrl Pts',(-7.91099999999815,-2.20167589667336,
58.446255927496));
#222022=CARTESIAN_POINT('Ctrl Pts',(-6.94214576672008,-4.38610418339256,
58.5348433632287));
#222023=CARTESIAN_POINT('Ctrl Pts',(-3.67820201487687,-7.34180684107931,
58.7120182346942));
#222024=CARTESIAN_POINT('Ctrl Pts',(-1.40868175871089,-8.08992666571449,
58.8006056704269));
#222025=CARTESIAN_POINT('Ctrl Pts',(2.97309270521885,-7.65454228025018,
58.9777805418924));
#222026=CARTESIAN_POINT('Ctrl Pts',(5.05102072676115,-6.47444880833824,
59.0663679776251));
#222027=CARTESIAN_POINT('Ctrl Pts',(7.66951518848099,-2.93425195367107,
59.2435428490905));
#222028=CARTESIAN_POINT('Ctrl Pts',(8.18956872247117,-0.601881960092826,
59.3321302848233));
#222029=CARTESIAN_POINT('Ctrl Pts',(7.32306689761058,3.71537198233008,59.5093051562887));
#222030=CARTESIAN_POINT('Ctrl Pts',(5.94329958849772,5.6664351893696,59.5978925920214));
#222031=CARTESIAN_POINT('Ctrl Pts',(2.16154501637257,7.92205913233158,59.7750674634869));
#222032=CARTESIAN_POINT('Ctrl Pts',(-0.21081652930643,8.20894963712986,
59.8636548992196));
#222033=CARTESIAN_POINT('Ctrl Pts',(-4.4212390857694,6.91982244717508,60.040829770685));
#222034=CARTESIAN_POINT('Ctrl Pts',(-6.22631625634573,5.35390358803071,
60.1294172064178));
#222035=CARTESIAN_POINT('Ctrl Pts',(-7.65317280859665,2.31334857513947,
60.2645592586881));
#222036=CARTESIAN_POINT('Ctrl Pts',(-7.91100000000094,1.157028378359,60.3111138752257));
#222037=CARTESIAN_POINT('Ctrl Pts',(-7.911,-6.46316333785535E-12,60.3576684917633));
#222038=CARTESIAN_POINT('',(-7.92241601769487,0.00219170473266906,62.357667929495));
#222039=CARTESIAN_POINT('Ctrl Pts',(-7.90475974663917,-0.00966143243572837,
60.3576684917633));
#222040=CARTESIAN_POINT('Ctrl Pts',(-7.91126008640382,-0.81782965792324,
60.3900925685658));
#222041=CARTESIAN_POINT('Ctrl Pts',(-7.42667005382225,-4.25751452650637,
60.5284862225846));
#222042=CARTESIAN_POINT('Ctrl Pts',(-3.54336063882975,-7.96788788067822,
60.7198646652124));
#222043=CARTESIAN_POINT('Ctrl Pts',(1.90559845092771,-8.01211367516218,
60.931803819645));
#222044=CARTESIAN_POINT('Ctrl Pts',(5.51918048952775,-6.13637686246202,
61.09075818547));
#222045=CARTESIAN_POINT('Ctrl Pts',(7.76323891949608,-2.74908180270005,
61.2497125512946));
#222046=CARTESIAN_POINT('Ctrl Pts',(8.30052305478131,2.68841017079816,61.4616517057278));
#222047=CARTESIAN_POINT('Ctrl Pts',(4.66794071633822,7.37390407097891,61.6735908601605));
#222048=CARTESIAN_POINT('Ctrl Pts',(-0.724272964357983,8.19536592754439,
61.8855300145938));
#222049=CARTESIAN_POINT('Ctrl Pts',(-5.82656564660765,6.46618994551645,
62.095894041246));
#222050=CARTESIAN_POINT('Ctrl Pts',(-7.92243276554659,2.58340903040866,
62.2532732792902));
#222051=CARTESIAN_POINT('Ctrl Pts',(-7.92649243633973,0.002197789429415,
62.3576677287261));
#222052=CARTESIAN_POINT('',(-7.90269638755491,0.00610913357140485,64.3576684865946));
#222053=CARTESIAN_POINT('Ctrl Pts',(-7.91099970110201,0.00217466408241333,
62.3576684917633));
#222054=CARTESIAN_POINT('Ctrl Pts',(-7.91101038434451,-0.0366888684033183,
62.3592433651982));
#222055=CARTESIAN_POINT('Ctrl Pts',(-7.91073468951299,-0.0755529221471149,
62.3608182386331));
#222056=CARTESIAN_POINT('Ctrl Pts',(-7.910172578582,-0.114414933681696,
62.362393112068));
#222057=CARTESIAN_POINT('Ctrl Pts',(-7.90740274338427,-0.305909817463608,
62.3701533950146));
#222058=CARTESIAN_POINT('Ctrl Pts',(-7.8976699909024,-0.49764158740683,
62.3779136779612));
#222059=CARTESIAN_POINT('Ctrl Pts',(-7.8809346174063,-0.689050474324599,
62.3856739609078));
#222060=CARTESIAN_POINT('Ctrl Pts',(-7.86421938576937,-0.880228991072,62.3934249039657));
#222061=CARTESIAN_POINT('Ctrl Pts',(-7.84051833923485,-1.07108504540069,
62.4011758470236));
#222062=CARTESIAN_POINT('Ctrl Pts',(-7.80984366553306,-1.26105627151729,
62.4089267900815));
#222063=CARTESIAN_POINT('Ctrl Pts',(-7.77919968429556,-1.45083741622899,
62.4166699777009));
#222064=CARTESIAN_POINT('Ctrl Pts',(-7.74159602285949,-1.63973514400386,
62.4244131653204));
#222065=CARTESIAN_POINT('Ctrl Pts',(-7.69709681919609,-1.82718952381012,
62.4321563529399));
#222066=CARTESIAN_POINT('Ctrl Pts',(-7.65263312175257,-2.01449433248074,
62.4398933622168));
#222067=CARTESIAN_POINT('Ctrl Pts',(-7.60128491870243,-2.20035773882507,
62.4476303714938));
#222068=CARTESIAN_POINT('Ctrl Pts',(-7.54316785991181,-2.38422726206908,
62.4553673807707));
#222069=CARTESIAN_POINT('Ctrl Pts',(-7.48508540657878,-2.5679873012972,
62.4630997830914));
#222070=CARTESIAN_POINT('Ctrl Pts',(-7.42024223106417,-2.74975548035633,
62.4708321854121));
#222071=CARTESIAN_POINT('Ctrl Pts',(-7.34880456351915,-2.92899171852707,
62.4785645877328));
#222072=CARTESIAN_POINT('Ctrl Pts',(-7.27739497985612,-3.10815749457977,
62.4862939502584));
#222073=CARTESIAN_POINT('Ctrl Pts',(-7.19939620021256,-3.28479297919593,
62.494023312784));
#222074=CARTESIAN_POINT('Ctrl Pts',(-7.11502361905996,-3.45837532668434,
62.5017526753095));
#222075=CARTESIAN_POINT('Ctrl Pts',(-7.03065107082583,-3.63195760644853,
62.5094820348194));
#222076=CARTESIAN_POINT('Ctrl Pts',(-6.93990487267707,-3.80248642357877,
62.5172113943294));
#222077=CARTESIAN_POINT('Ctrl Pts',(-6.84304785148925,-3.96946055557029,
62.5249407538393));
#222078=CARTESIAN_POINT('Ctrl Pts',(-6.7461859754797,-4.13644305690495,
62.5326705007724));
#222079=CARTESIAN_POINT('Ctrl Pts',(-6.64321284592823,-4.299870206946,62.5404002477056));
#222080=CARTESIAN_POINT('Ctrl Pts',(-6.53443629959605,-4.45926711988882,
62.5481299946388));
#222081=CARTESIAN_POINT('Ctrl Pts',(-6.42563436914082,-4.61870122973656,
62.5558615453877));
#222082=CARTESIAN_POINT('Ctrl Pts',(-6.31102652740491,-4.77410293280094,
62.5635930961366));
#222083=CARTESIAN_POINT('Ctrl Pts',(-6.19096284210019,-4.92502792760962,
62.5713246468855));
#222084=CARTESIAN_POINT('Ctrl Pts',(-6.07084913154013,-5.07601580622355,
62.5790594190315));
#222085=CARTESIAN_POINT('Ctrl Pts',(-5.94527527420421,-5.2225229815602,
62.5867941911774));
#222086=CARTESIAN_POINT('Ctrl Pts',(-5.81463037939895,-5.36413968414049,
62.5945289633234));
#222087=CARTESIAN_POINT('Ctrl Pts',(-5.68382969049035,-5.50592526471045,
62.602272959189));
#222088=CARTESIAN_POINT('Ctrl Pts',(-5.54794613065987,-5.64280846153232,
62.6100169550547));
#222089=CARTESIAN_POINT('Ctrl Pts',(-5.40740504816606,-5.77441699611902,
62.6177609509203));
#222090=CARTESIAN_POINT('Ctrl Pts',(-5.26677274745945,-5.90611095124683,
62.6255099730278));
#222091=CARTESIAN_POINT('Ctrl Pts',(-5.12147717238078,-6.03252318998137,
62.6332589951353));
#222092=CARTESIAN_POINT('Ctrl Pts',(-4.9719751240282,-6.15332303442983,
62.6410080172427));
#222093=CARTESIAN_POINT('Ctrl Pts',(-4.82224460132833,-6.2743074894968,
62.6487688816814));
#222094=CARTESIAN_POINT('Ctrl Pts',(-4.6682950524527,-6.38966220575165,
62.65652974612));
#222095=CARTESIAN_POINT('Ctrl Pts',(-4.51061150420258,-6.49910031143968,
62.6642906105586));
#222096=CARTESIAN_POINT('Ctrl Pts',(-4.40217392501625,-6.57435992719061,
62.6696276882783));
#222097=CARTESIAN_POINT('Ctrl Pts',(-4.29197101186985,-6.64682241167096,
62.6749647659979));
#222098=CARTESIAN_POINT('Ctrl Pts',(-4.18016645934941,-6.71640747514102,
62.6803018437175));
#222099=CARTESIAN_POINT('Ctrl Pts',(-4.01228819221994,-6.82089177036964,
62.6883156440406));
#222100=CARTESIAN_POINT('Ctrl Pts',(-3.84028294266886,-6.91920718672284,
62.6963294443637));
#222101=CARTESIAN_POINT('Ctrl Pts',(-3.66463773976345,-7.01101641962857,
62.7043432446867));
#222102=CARTESIAN_POINT('Ctrl Pts',(-3.48919275165567,-7.10272100084623,
62.7123479102234));
#222103=CARTESIAN_POINT('Ctrl Pts',(-3.31011637171477,-7.18793402264737,
62.72035257576));
#222104=CARTESIAN_POINT('Ctrl Pts',(-3.12792412429923,-7.26636165303014,
62.7283572412967));
#222105=CARTESIAN_POINT('Ctrl Pts',(-2.94590862439637,-7.34471319955757,
62.7363541413837));
#222106=CARTESIAN_POINT('Ctrl Pts',(-2.76078358620477,-7.41629234117269,
62.7443510414708));
#222107=CARTESIAN_POINT('Ctrl Pts',(-2.57308899641308,-7.48085115588714,
62.7523479415578));
#222108=CARTESIAN_POINT('Ctrl Pts',(-2.38554464827369,-7.54535829397625,
62.7603384404615));
#222109=CARTESIAN_POINT('Ctrl Pts',(-2.19543516287578,-7.60285619673152,
62.7683289393651));
#222110=CARTESIAN_POINT('Ctrl Pts',(-2.00332074872912,-7.65314490766452,
62.7763194382688));
#222111=CARTESIAN_POINT('Ctrl Pts',(-1.81132753782506,-7.70340189190561,
62.7843048960392));
#222112=CARTESIAN_POINT('Ctrl Pts',(-1.61733224222847,-7.74645866584448,
62.7922903538095));
#222113=CARTESIAN_POINT('Ctrl Pts',(-1.42191088052068,-7.78216489467146,
62.8002758115798));
#222114=CARTESIAN_POINT('Ctrl Pts',(-1.22008211993164,-7.81904184531023,
62.8085230934043));
#222115=CARTESIAN_POINT('Ctrl Pts',(-1.01673253755762,-7.84807794077574,
62.8167703752288));
#222116=CARTESIAN_POINT('Ctrl Pts',(-0.812510161289643,-7.86916439260237,
62.8250176570533));
#222117=CARTESIAN_POINT('Ctrl Pts',(-0.61490508798135,-7.88956759197336,
62.8329977068367));
#222118=CARTESIAN_POINT('Ctrl Pts',(-0.416483253234442,-7.90252821824812,
62.8409777566202));
#222119=CARTESIAN_POINT('Ctrl Pts',(-0.217838852862356,-7.90800020448809,
62.8489578064037));
#222120=CARTESIAN_POINT('Ctrl Pts',(-0.0192102273301515,-7.91347175618418,
62.8569372224718));
#222121=CARTESIAN_POINT('Ctrl Pts',(0.179640594185305,-7.9114558438232,
62.8649166385399));
#222122=CARTESIAN_POINT('Ctrl Pts',(0.378117575871898,-7.90195849766479,
62.872896054608));
#222123=CARTESIAN_POINT('Ctrl Pts',(0.57660929883652,-7.89246044611969,
62.8808760633231));
#222124=CARTESIAN_POINT('Ctrl Pts',(0.774726792436858,-7.87547986956123,
62.8888560720383));
#222125=CARTESIAN_POINT('Ctrl Pts',(0.971876922139844,-7.85107484668259,
62.8968360807534));
#222126=CARTESIAN_POINT('Ctrl Pts',(1.16907199390426,-7.82666426046986,
62.9048179085799));
#222127=CARTESIAN_POINT('Ctrl Pts',(1.36529893034396,-7.79482589607605,
62.9127997364064));
#222128=CARTESIAN_POINT('Ctrl Pts',(1.5599722140535,-7.75566939028354,62.9207815642329));
#222129=CARTESIAN_POINT('Ctrl Pts',(1.7547902461029,-7.71648376986831,62.9287693269073));
#222130=CARTESIAN_POINT('Ctrl Pts',(1.94805198961005,-7.66996920457517,
62.9367570895817));
#222131=CARTESIAN_POINT('Ctrl Pts',(2.13918357370322,-7.61628614470323,
62.9447448522561));
#222132=CARTESIAN_POINT('Ctrl Pts',(2.33039933894324,-7.56257944090258,
62.9527361330252));
#222133=CARTESIAN_POINT('Ctrl Pts',(2.51948275470099,-7.50169804572053,
62.9607274137943));
#222134=CARTESIAN_POINT('Ctrl Pts',(2.70587694104146,-7.43385169208669,
62.9687186945635));
#222135=CARTESIAN_POINT('Ctrl Pts',(2.89244649952837,-7.3659415040549,62.9767174940653));
#222136=CARTESIAN_POINT('Ctrl Pts',(3.07632146455346,-7.29105339244926,
62.9847162935671));
#222137=CARTESIAN_POINT('Ctrl Pts',(3.2569657808282,-7.20944484010483,62.992715093069));
#222138=CARTESIAN_POINT('Ctrl Pts',(3.29833564064755,-7.19075543741466,
62.9945469205017));
#222139=CARTESIAN_POINT('Ctrl Pts',(3.33953616636706,-7.17171375837726,
62.9963787479343));
#222140=CARTESIAN_POINT('Ctrl Pts',(3.38056110967398,-7.1523232298156,62.998210575367));
#222141=CARTESIAN_POINT('Ctrl Pts',(3.56256268580738,-7.06629978954222,
63.0063372284001));
#222142=CARTESIAN_POINT('Ctrl Pts',(3.74142748038145,-6.97325526619819,
63.0144638814331));
#222143=CARTESIAN_POINT('Ctrl Pts',(3.91659768441751,-6.87344044699708,
63.0225905344662));
#222144=CARTESIAN_POINT('Ctrl Pts',(4.09161877572136,-6.77371059464572,
63.0307102697278));
#222145=CARTESIAN_POINT('Ctrl Pts',(4.26295127071939,-6.66722209323163,
63.0388300049894));
#222146=CARTESIAN_POINT('Ctrl Pts',(4.43006012935157,-6.55427251877197,
63.046949740251));
#222147=CARTESIAN_POINT('Ctrl Pts',(4.59704778123877,-6.44140486845674,
63.0550635861379));
#222148=CARTESIAN_POINT('Ctrl Pts',(4.75981764161475,-6.32208566696624,
63.0631774320248));
#222149=CARTESIAN_POINT('Ctrl Pts',(4.91786145409672,-6.19665714061297,
63.0712912779117));
#222150=CARTESIAN_POINT('Ctrl Pts',(5.07579297056634,-6.07131773589707,
63.0793993586091));
#222151=CARTESIAN_POINT('Ctrl Pts',(5.22900488937254,-5.93987786428078,
63.0875074393064));
#222152=CARTESIAN_POINT('Ctrl Pts',(5.37701970391702,-5.80272178410167,
63.0956155200038));
#222153=CARTESIAN_POINT('Ctrl Pts',(5.52497094535221,-5.66562461315069,
63.1037201182396));
#222154=CARTESIAN_POINT('Ctrl Pts',(5.66772929983764,-5.52281634526398,
63.1118247164754));
#222155=CARTESIAN_POINT('Ctrl Pts',(5.80485135161792,-5.37472062395988,
63.1199293147112));
#222156=CARTESIAN_POINT('Ctrl Pts',(5.94193054304696,-5.22667119305581,
63.1280313796861));
#222157=CARTESIAN_POINT('Ctrl Pts',(6.07337672896945,-5.07333783854438,
63.136133444661));
#222158=CARTESIAN_POINT('Ctrl Pts',(6.19878391186954,-4.91518046606098,
63.144235509636));
#222159=CARTESIAN_POINT('Ctrl Pts',(6.26549297895872,-4.83105027090261,
63.1485453201546));
#222160=CARTESIAN_POINT('Ctrl Pts',(6.33049389698373,-4.74555567194487,
63.1528551306732));
#222161=CARTESIAN_POINT('Ctrl Pts',(6.39373014667625,-4.65876977446657,
63.1571649411919));
#222162=CARTESIAN_POINT('Ctrl Pts',(6.51534733796135,-4.49186144031034,
63.1654536530113));
#222163=CARTESIAN_POINT('Ctrl Pts',(6.63038262704873,-4.32024691026366,
63.1737423648308));
#222164=CARTESIAN_POINT('Ctrl Pts',(6.73849406084604,-4.14446845710552,
63.1820310766503));
#222165=CARTESIAN_POINT('Ctrl Pts',(6.84666781982837,-3.968588669387,63.1903245668312));
#222166=CARTESIAN_POINT('Ctrl Pts',(6.94790960294631,-3.7885404163034,63.198618057012));
#222167=CARTESIAN_POINT('Ctrl Pts',(7.04192281111767,-3.60489169355483,
63.2069115471929));
#222168=CARTESIAN_POINT('Ctrl Pts',(7.13599588507806,-3.42112602685865,
63.2152103185075));
#222169=CARTESIAN_POINT('Ctrl Pts',(7.22283106273601,-3.23375557424026,
63.2235090898222));
#222170=CARTESIAN_POINT('Ctrl Pts',(7.30217902916827,-3.04337024135664,
63.2318078611369));
#222171=CARTESIAN_POINT('Ctrl Pts',(7.38161936121375,-2.8527632889557,63.2401162927004));
#222172=CARTESIAN_POINT('Ctrl Pts',(7.4535549480545,-2.65913471156,63.2484247242639));
#222173=CARTESIAN_POINT('Ctrl Pts',(7.51778509807714,-2.46309322177,63.2567331558274));
#222174=CARTESIAN_POINT('Ctrl Pts',(7.58205486961288,-2.26693080029209,
63.2650467125951));
#222175=CARTESIAN_POINT('Ctrl Pts',(7.63860963153772,-2.06835277511666,
63.2733602693627));
#222176=CARTESIAN_POINT('Ctrl Pts',(7.68729901393674,-1.86798149624863,
63.2816738261303));
#222177=CARTESIAN_POINT('Ctrl Pts',(7.73604162804305,-1.66739115308481,
63.2899964720422));
#222178=CARTESIAN_POINT('Ctrl Pts',(7.77690161275452,-1.46500392344011,
63.2983191179541));
#222179=CARTESIAN_POINT('Ctrl Pts',(7.80977969206544,-1.2614524015603,63.306641763866));
#222180=CARTESIAN_POINT('Ctrl Pts',(7.82225983434539,-1.18418657558744,
63.3098009449162));
#222181=CARTESIAN_POINT('Ctrl Pts',(7.8335904169355,-1.10675305116369,63.3129601259664));
#222182=CARTESIAN_POINT('Ctrl Pts',(7.84376796813824,-1.02918660213224,
63.3161193070166));
#222183=CARTESIAN_POINT('Ctrl Pts',(7.8717899660437,-0.815621783936255,
63.3248175255771));
#222184=CARTESIAN_POINT('Ctrl Pts',(7.8910923602589,-0.600859395635776,
63.3335157441376));
#222185=CARTESIAN_POINT('Ctrl Pts',(7.90159720958278,-0.38559374672525,
63.3422139626981));
#222186=CARTESIAN_POINT('Ctrl Pts',(7.91209282898842,-0.170517237542343,
63.3509045387076));
#222187=CARTESIAN_POINT('Ctrl Pts',(7.91380632695787,0.0450614210154638,
63.3595951147171));
#222188=CARTESIAN_POINT('Ctrl Pts',(7.90671169159671,0.260444285727001,
63.3682856907266));
#222189=CARTESIAN_POINT('Ctrl Pts',(7.89944690852185,0.480992588849226,
63.3771846892362));
#222190=CARTESIAN_POINT('Ctrl Pts',(7.88294619330481,0.70133535329489,63.3860836877457));
#222191=CARTESIAN_POINT('Ctrl Pts',(7.85723830688212,0.920721015761098,
63.3949826862553));
#222192=CARTESIAN_POINT('Ctrl Pts',(7.83220649587203,1.1343371937263,63.4036476556428));
#222193=CARTESIAN_POINT('Ctrl Pts',(7.79844563548479,1.34704571601964,63.4123126250303));
#222194=CARTESIAN_POINT('Ctrl Pts',(7.75603483252731,1.5581542531544,63.4209775944178));
#222195=CARTESIAN_POINT('Ctrl Pts',(7.71190584179489,1.77781542505187,63.4299936074884));
#222196=CARTESIAN_POINT('Ctrl Pts',(7.65841145220673,1.99574404068841,63.439009620559));
#222197=CARTESIAN_POINT('Ctrl Pts',(7.5957005129222,2.21116591824166,63.4480256336296));
#222198=CARTESIAN_POINT('Ctrl Pts',(7.53298957363764,2.42658779579498,63.4570416467002));
#222199=CARTESIAN_POINT('Ctrl Pts',(7.46106209829464,2.63950264798602,63.4660576597708));
#222200=CARTESIAN_POINT('Ctrl Pts',(7.3801277674481,2.84914638727839,63.4750736728413));
#222201=CARTESIAN_POINT('Ctrl Pts',(7.31001553187736,3.03075771440566,63.4828841140435));
#222202=CARTESIAN_POINT('Ctrl Pts',(7.23317384894474,3.20983572364905,63.4906945552457));
#222203=CARTESIAN_POINT('Ctrl Pts',(7.14982148808359,3.38584903510747,63.4985049964478));
#222204=CARTESIAN_POINT('Ctrl Pts',(7.06647513675998,3.56184965636021,63.5063148745329));
#222205=CARTESIAN_POINT('Ctrl Pts',(6.97661919325035,3.73478570167088,63.514124752618));
#222206=CARTESIAN_POINT('Ctrl Pts',(6.88051971414148,3.90414772560037,63.5219346307031));
#222207=CARTESIAN_POINT('Ctrl Pts',(6.78441020153603,4.07352743217809,63.5297453241972));
#222208=CARTESIAN_POINT('Ctrl Pts',(6.68205602943363,4.23933206820721,63.5375560176913));
#222209=CARTESIAN_POINT('Ctrl Pts',(6.57376823218394,4.40107853026155,63.5453667111854));
#222210=CARTESIAN_POINT('Ctrl Pts',(6.46540358788814,4.56293977660503,63.5531829475822));
#222211=CARTESIAN_POINT('Ctrl Pts',(6.35109710195647,4.72073680232081,63.560999183979));
#222212=CARTESIAN_POINT('Ctrl Pts',(6.2312025193915,4.87401643024816,63.5688154203759));
#222213=CARTESIAN_POINT('Ctrl Pts',(6.11126361006417,5.02735272787231,63.5766345465484));
#222214=CARTESIAN_POINT('Ctrl Pts',(5.98573271174946,5.1761680285087,63.5844536727209));
#222215=CARTESIAN_POINT('Ctrl Pts',(5.85500265344306,5.32004369607757,63.5922727988935));
#222216=CARTESIAN_POINT('Ctrl Pts',(5.72412722714509,5.46407934917006,63.600100619705));
#222217=CARTESIAN_POINT('Ctrl Pts',(5.58804133517596,5.60316414219001,63.6079284405166));
#222218=CARTESIAN_POINT('Ctrl Pts',(5.44717411064738,5.73691687305062,63.6157562613282));
#222219=CARTESIAN_POINT('Ctrl Pts',(5.33756955093011,5.84098585876409,63.6218468537741));
#222220=CARTESIAN_POINT('Ctrl Pts',(5.22507114904329,5.94182760034021,63.6279374462201));
#222221=CARTESIAN_POINT('Ctrl Pts',(5.10989405962437,6.03928006466132,63.6340280386661));
#222222=CARTESIAN_POINT('Ctrl Pts',(4.95639667417045,6.16915570707249,63.642145017668));
#222223=CARTESIAN_POINT('Ctrl Pts',(4.79783563040531,6.29326854203543,63.65026199667));
#222224=CARTESIAN_POINT('Ctrl Pts',(4.63467227805463,6.4112193750512,63.658378975672));
#222225=CARTESIAN_POINT('Ctrl Pts',(4.47162827403193,6.52908393112732,63.6664900173856));
#222226=CARTESIAN_POINT('Ctrl Pts',(4.30398893260069,6.64079528499523,63.6746010590992));
#222227=CARTESIAN_POINT('Ctrl Pts',(4.13224834309014,6.74599471027281,63.6827121008128));
#222228=CARTESIAN_POINT('Ctrl Pts',(3.96060895738772,6.8511321433185,63.6908183628275));
#222229=CARTESIAN_POINT('Ctrl Pts',(3.78487341560353,6.94976513260468,63.6989246248422));
#222230=CARTESIAN_POINT('Ctrl Pts',(3.60556490494635,7.04157814102913,63.7070308868569));
#222231=CARTESIAN_POINT('Ctrl Pts',(3.42633659048856,7.13335008584593,63.7151335233247));
#222232=CARTESIAN_POINT('Ctrl Pts',(3.24353877899788,7.21830798689402,63.7232361597926));
#222233=CARTESIAN_POINT('Ctrl Pts',(3.05771988709311,7.29618188452531,63.7313387962604));
#222234=CARTESIAN_POINT('Ctrl Pts',(2.87195773302711,7.37403200418331,63.7394389586737));
#222235=CARTESIAN_POINT('Ctrl Pts',(2.68317663386522,7.44480231082203,63.747539121087));
#222236=CARTESIAN_POINT('Ctrl Pts',(2.49194617095313,7.50827045870566,63.7556392835002));
#222237=CARTESIAN_POINT('Ctrl Pts',(2.29885302995061,7.57235681734244,63.7638183454509));
#222238=CARTESIAN_POINT('Ctrl Pts',(2.10326286058131,7.62899787763967,63.7719974074015));
#222239=CARTESIAN_POINT('Ctrl Pts',(1.90577985651915,7.6780156380725,63.7801764693522));
#222240=CARTESIAN_POINT('Ctrl Pts',(1.7102029504211,7.72656028106512,63.7882765873278));
#222241=CARTESIAN_POINT('Ctrl Pts',(1.51276990884496,7.76762807751141,63.7963767053035));
#222242=CARTESIAN_POINT('Ctrl Pts',(1.31408025082597,7.80109698019382,63.8044768232792));
#222243=CARTESIAN_POINT('Ctrl Pts',(1.11536385267232,7.83457038720209,63.8125780313883));
#222244=CARTESIAN_POINT('Ctrl Pts',(0.915390817151028,7.86044280758088,
63.8206792394974));
#222245=CARTESIAN_POINT('Ctrl Pts',(0.714768767622149,7.87864370363528,
63.8287804476065));
#222246=CARTESIAN_POINT('Ctrl Pts',(0.51409380770184,7.8968493998427,63.8368837922609));
#222247=CARTESIAN_POINT('Ctrl Pts',(0.312769811839722,7.9073795079036,63.8449871369153));
#222248=CARTESIAN_POINT('Ctrl Pts',(0.111407962529794,7.91021550059699,
63.8530904815697));
#222249=CARTESIAN_POINT('Ctrl Pts',(-0.0932798582425197,7.91309833647741,
63.8613276722986));
#222250=CARTESIAN_POINT('Ctrl Pts',(-0.298006449285327,7.90803065365533,
63.8695648630274));
#222251=CARTESIAN_POINT('Ctrl Pts',(-0.502131696847686,7.89504811632082,
63.8778020537562));
#222252=CARTESIAN_POINT('Ctrl Pts',(-0.703201609483169,7.88225990085599,
63.8859159506895));
#222253=CARTESIAN_POINT('Ctrl Pts',(-0.903687737140456,7.86179217858119,
63.8940298476228));
#222254=CARTESIAN_POINT('Ctrl Pts',(-1.1029849262459,7.83373124714362,63.9021437445562));
#222255=CARTESIAN_POINT('Ctrl Pts',(-1.30682471191427,7.80503072068078,
63.9104425821827));
#222256=CARTESIAN_POINT('Ctrl Pts',(-1.50942036041786,7.76838677815455,
63.9187414198093));
#222257=CARTESIAN_POINT('Ctrl Pts',(-1.71013668760003,7.72394675730772,
63.9270402574359));
#222258=CARTESIAN_POINT('Ctrl Pts',(-1.91085301478221,7.67950673646089,
63.9353390950625));
#222259=CARTESIAN_POINT('Ctrl Pts',(-2.10968968514138,7.62727076180396,
63.9436379326891));
#222260=CARTESIAN_POINT('Ctrl Pts',(-2.30602904505396,7.56744019093429,
63.9519367703157));
#222261=CARTESIAN_POINT('Ctrl Pts',(-2.49349993383965,7.51031211278181,
63.9598607569602));
#222262=CARTESIAN_POINT('Ctrl Pts',(-2.67909644624304,7.4461373865409,63.9677847436047));
#222263=CARTESIAN_POINT('Ctrl Pts',(-2.86225216123665,7.37505481779601,
63.9757087302493));
#222264=CARTESIAN_POINT('Ctrl Pts',(-3.04521176964433,7.30404835784126,
63.9836242326051));
#222265=CARTESIAN_POINT('Ctrl Pts',(-3.22573546964,7.22614890971879,63.9915397349609));
#222266=CARTESIAN_POINT('Ctrl Pts',(-3.40327037852688,7.14154547213987,
63.9994552373167));
#222267=CARTESIAN_POINT('Ctrl Pts',(-3.58064449004641,7.05701866180073,
64.0073635704236));
#222268=CARTESIAN_POINT('Ctrl Pts',(-3.7550348959095,6.96580010408428,64.0152719035306));
#222269=CARTESIAN_POINT('Ctrl Pts',(-3.92590687688866,6.86812756098766,
64.0231802366376));
#222270=CARTESIAN_POINT('Ctrl Pts',(-4.09662817904104,6.77054114777681,
64.0310815959953));
#222271=CARTESIAN_POINT('Ctrl Pts',(-4.26383694567463,6.66651226432804,
64.0389829553529));
#222272=CARTESIAN_POINT('Ctrl Pts',(-4.42702130471118,6.55632544704984,
64.0468843147106));
#222273=CARTESIAN_POINT('Ctrl Pts',(-4.59012164432531,6.44619536212517,
64.0547816058619));
#222274=CARTESIAN_POINT('Ctrl Pts',(-4.7492014211138,6.32991385033155,64.0626788970133));
#222275=CARTESIAN_POINT('Ctrl Pts',(-4.90377556210006,6.20781009991045,
64.0705761881646));
#222276=CARTESIAN_POINT('Ctrl Pts',(-5.05829715303041,6.08574786069473,
64.0784707945001));
#222277=CARTESIAN_POINT('Ctrl Pts',(-5.20831589148195,5.95786753804494,
64.0863654008357));
#222278=CARTESIAN_POINT('Ctrl Pts',(-5.3533775340894,5.82454032327933,64.0942600071712));
#222279=CARTESIAN_POINT('Ctrl Pts',(-5.45524197098643,5.73091597565009,
64.0998037168276));
#222280=CARTESIAN_POINT('Ctrl Pts',(-5.55466266542029,5.6346066245214,64.105347426484));
#222281=CARTESIAN_POINT('Ctrl Pts',(-5.651492361676,5.53575244080856,64.1108911361403));
#222282=CARTESIAN_POINT('Ctrl Pts',(-5.80030425041226,5.38382923587623,
64.1194109388091));
#222283=CARTESIAN_POINT('Ctrl Pts',(-5.94284646280459,5.22604605658933,
64.1279307414778));
#222284=CARTESIAN_POINT('Ctrl Pts',(-6.07869939272208,5.06293735818647,
64.1364505441465));
#222285=CARTESIAN_POINT('Ctrl Pts',(-6.21479802434825,4.89953366367332,
64.1449857556112));
#222286=CARTESIAN_POINT('Ctrl Pts',(-6.3441830342779,4.73078539157157,64.1535209670759));
#222287=CARTESIAN_POINT('Ctrl Pts',(-6.46647708311045,4.55725741357753,
64.1620561785405));
#222288=CARTESIAN_POINT('Ctrl Pts',(-6.5951791548858,4.37463683234712,64.1710386221592));
#222289=CARTESIAN_POINT('Ctrl Pts',(-6.71602711881429,4.18672256643622,
64.180021065778));
#222290=CARTESIAN_POINT('Ctrl Pts',(-6.82863630027726,3.99420170729217,
64.1890035093967));
#222291=CARTESIAN_POINT('Ctrl Pts',(-6.93608788139017,3.81049847418549,
64.1975745491338));
#222292=CARTESIAN_POINT('Ctrl Pts',(-7.03603839763765,3.6226013867786,64.206145588871));
#222293=CARTESIAN_POINT('Ctrl Pts',(-7.12820297121017,3.43112859001677,
64.2147166286082));
#222294=CARTESIAN_POINT('Ctrl Pts',(-7.22048319470356,3.23941552942108,
64.2232984234547));
#222295=CARTESIAN_POINT('Ctrl Pts',(-7.30495785393249,3.04411802202887,
64.2318802183012));
#222296=CARTESIAN_POINT('Ctrl Pts',(-7.38139040831873,2.84587361630489,
64.2404620131477));
#222297=CARTESIAN_POINT('Ctrl Pts',(-7.45795081046058,2.64729760970042,
64.2490581626526));
#222298=CARTESIAN_POINT('Ctrl Pts',(-7.52644212449434,2.44576508249835,
64.2576543121575));
#222299=CARTESIAN_POINT('Ctrl Pts',(-7.5866771208844,2.24193025392163,64.2662504616625));
#222300=CARTESIAN_POINT('Ctrl Pts',(-7.59507418438069,2.21351464670172,
64.26744880843));
#222301=CARTESIAN_POINT('Ctrl Pts',(-7.60331087730045,2.18505431498424,
64.2686471551975));
#222302=CARTESIAN_POINT('Ctrl Pts',(-7.61138677106328,2.1565510476877,64.2698455019651));
#222303=CARTESIAN_POINT('Ctrl Pts',(-7.67423591751027,1.93472965266338,
64.2791714135853));
#222304=CARTESIAN_POINT('Ctrl Pts',(-7.72742685236606,1.71000847173687,
64.2884973252056));
#222305=CARTESIAN_POINT('Ctrl Pts',(-7.77072390541452,1.48316249474539,
64.2978232368259));
#222306=CARTESIAN_POINT('Ctrl Pts',(-7.81383118656715,1.25731078845093,
64.307108272779));
#222307=CARTESIAN_POINT('Ctrl Pts',(-7.84713105685815,1.02935293352636,
64.3163933087322));
#222308=CARTESIAN_POINT('Ctrl Pts',(-7.87043857397434,0.80007352993134,
64.3256783446853));
#222309=CARTESIAN_POINT('Ctrl Pts',(-7.89357025557444,0.572523845639279,
64.3348933328903));
#222310=CARTESIAN_POINT('Ctrl Pts',(-7.90685971761943,0.34367255329281,
64.3441083210953));
#222311=CARTESIAN_POINT('Ctrl Pts',(-7.91017416660382,0.114305091721668,
64.3533233093003));
#222312=CARTESIAN_POINT('Ctrl Pts',(-7.91069511936109,0.0782539676598749,
64.3547716868545));
#222313=CARTESIAN_POINT('Ctrl Pts',(-7.91096974389411,0.0421901279273608,
64.3562200644088));
#222314=CARTESIAN_POINT('Ctrl Pts',(-7.91099763534554,0.00611666226964039,
64.357668441963));
#222315=CARTESIAN_POINT('',(-7.90615846952848,-0.00382583299217227,66.3576684917633));
#222316=CARTESIAN_POINT('Ctrl Pts',(-7.90173504288081,0.00610826169356984,
64.3576684917633));
#222317=CARTESIAN_POINT('Ctrl Pts',(-7.88678469063768,-1.90184896929262,
64.4343637390471));
#222318=CARTESIAN_POINT('Ctrl Pts',(-6.25273451541879,-6.46756077205388,
64.6170285635472));
#222319=CARTESIAN_POINT('Ctrl Pts',(1.42253012608145,-9.24895559998287,
64.9056629652644));
#222320=CARTESIAN_POINT('Ctrl Pts',(7.32623646320802,-4.72957727296922,
65.1705869083054));
#222321=CARTESIAN_POINT('Ctrl Pts',(8.21012473050356,0.647397026181004,
65.3825260627385));
#222322=CARTESIAN_POINT('Ctrl Pts',(6.91400940569619,4.50698881871914,65.5414804285633));
#222323=CARTESIAN_POINT('Ctrl Pts',(3.91324198025052,7.24650719196005,65.7004347943879));
#222324=CARTESIAN_POINT('Ctrl Pts',(-1.37637619322111,8.61578904130303,
65.9123739488212));
#222325=CARTESIAN_POINT('Ctrl Pts',(-6.56595387401644,5.74912006338756,
66.1243131032538));
#222326=CARTESIAN_POINT('Ctrl Pts',(-7.85360726975729,1.67313532969439,
66.2904062137708));
#222327=CARTESIAN_POINT('Ctrl Pts',(-7.90579410487209,0.174089764566414,
66.3505297470712));
#222328=CARTESIAN_POINT('Ctrl Pts',(-7.90615846952848,-0.00382583299217227,
66.3576684917633));
#222329=CARTESIAN_POINT('',(-7.91099999947648,-9.10112777354474E-5,68.357571168238));
#222330=CARTESIAN_POINT('Ctrl Pts',(-7.9109990733941,-0.00382893689472276,
66.3576685222996));
#222331=CARTESIAN_POINT('Ctrl Pts',(-7.91089361564559,-0.221716087729338,
66.366405760205));
#222332=CARTESIAN_POINT('Ctrl Pts',(-7.90178236265442,-0.439340629505819,
66.3751429981104));
#222333=CARTESIAN_POINT('Ctrl Pts',(-7.8837549931329,-0.655994061140797,
66.3838802360158));
#222334=CARTESIAN_POINT('Ctrl Pts',(-7.8656770179853,-0.873255672606956,
66.392642000705));
#222335=CARTESIAN_POINT('Ctrl Pts',(-7.8386328733282,-1.0895405155915,66.4014037653942));
#222336=CARTESIAN_POINT('Ctrl Pts',(-7.8027635950725,-1.30414772146843,
66.4101655300834));
#222337=CARTESIAN_POINT('Ctrl Pts',(-7.76676534922295,-1.51952654518409,
66.4189587976007));
#222338=CARTESIAN_POINT('Ctrl Pts',(-7.72187846929606,-1.733215449891,66.4277520651181));
#222339=CARTESIAN_POINT('Ctrl Pts',(-7.66829529032727,-1.9445226510238,
66.4365453326355));
#222340=CARTESIAN_POINT('Ctrl Pts',(-7.6146169970211,-2.15620493898057,
66.445354208891));
#222341=CARTESIAN_POINT('Ctrl Pts',(-7.55221159940958,-2.36549687437015,
66.4541630851466));
#222342=CARTESIAN_POINT('Ctrl Pts',(-7.48132101428588,-2.571722551366,66.4629719614022));
#222343=CARTESIAN_POINT('Ctrl Pts',(-7.41027988377687,-2.77838617543128,
66.4717995444532));
#222344=CARTESIAN_POINT('Ctrl Pts',(-7.33071758631889,-2.9819703215386,
66.4806271275041));
#222345=CARTESIAN_POINT('Ctrl Pts',(-7.24292485520071,-3.18181717606712,
66.4894547105551));
#222346=CARTESIAN_POINT('Ctrl Pts',(-7.22385673864273,-3.22522285518611,
66.491372014874));
#222347=CARTESIAN_POINT('Ctrl Pts',(-7.20440053691037,-3.26845232266537,
66.4932893191929));
#222348=CARTESIAN_POINT('Ctrl Pts',(-7.18455951561155,-3.31149899088547,
66.4952066235118));
#222349=CARTESIAN_POINT('Ctrl Pts',(-7.10272625102719,-3.48904274414686,
66.503114445859));
#222350=CARTESIAN_POINT('Ctrl Pts',(-7.01420322113214,-3.66377847849524,
66.5110222682062));
#222351=CARTESIAN_POINT('Ctrl Pts',(-6.91920610262592,-3.83516725963605,
66.5189300905533));
#222352=CARTESIAN_POINT('Ctrl Pts',(-6.82430603591275,-4.00638094506046,
66.5268298340414));
#222353=CARTESIAN_POINT('Ctrl Pts',(-6.72294522106175,-4.17425418907617,
66.5347295775294));
#222354=CARTESIAN_POINT('Ctrl Pts',(-6.61538709815423,-4.33826861104458,
66.5426293210174));
#222355=CARTESIAN_POINT('Ctrl Pts',(-6.50791888759448,-4.50214592647606,
66.5505224607785));
#222356=CARTESIAN_POINT('Ctrl Pts',(-6.39426387747894,-4.66217055919256,
66.5584156005395));
#222357=CARTESIAN_POINT('Ctrl Pts',(-6.2747311881986,-4.81784905490487,
66.5663087403005));
#222358=CARTESIAN_POINT('Ctrl Pts',(-6.15527623179081,-4.97342631189548,
66.5741967471022));
#222359=CARTESIAN_POINT('Ctrl Pts',(-6.02995142100922,-5.12466279041883,
66.5820847539039));
#222360=CARTESIAN_POINT('Ctrl Pts',(-5.89910906780965,-5.27109411850006,
66.5899727607056));
#222361=CARTESIAN_POINT('Ctrl Pts',(-5.76832751807179,-5.41745739880141,
66.5978571018891));
#222362=CARTESIAN_POINT('Ctrl Pts',(-5.63203376460771,-5.55901972164596,
66.6057414430726));
#222363=CARTESIAN_POINT('Ctrl Pts',(-5.49062043914128,-5.69534969894597,
66.613625784256));
#222364=CARTESIAN_POINT('Ctrl Pts',(-5.34924658725096,-5.83164162161629,
66.6215079246346));
#222365=CARTESIAN_POINT('Ctrl Pts',(-5.20275625972483,-5.96270387064153,
66.6293900650131));
#222366=CARTESIAN_POINT('Ctrl Pts',(-5.0515791792801,-6.08814165369563,
66.6372722053917));
#222367=CARTESIAN_POINT('Ctrl Pts',(-4.90038556859353,-6.21359315256489,
66.6451552076316));
#222368=CARTESIAN_POINT('Ctrl Pts',(-4.74450444202807,-6.33341873095843,
66.6530382098716));
#222369=CARTESIAN_POINT('Ctrl Pts',(-4.58439934210815,-6.44726326995248,
66.6609212121115));
#222370=CARTESIAN_POINT('Ctrl Pts',(-4.42427493296259,-6.56112153898944,
66.6688051650686));
#222371=CARTESIAN_POINT('Ctrl Pts',(-4.25992581625462,-6.66899713071645,
66.6766891180257));
#222372=CARTESIAN_POINT('Ctrl Pts',(-4.09184528309732,-6.77057775815286,
66.6845730709828));
#222373=CARTESIAN_POINT('Ctrl Pts',(-3.92371621248503,-6.87218771953437,
66.6924593006283));
#222374=CARTESIAN_POINT('Ctrl Pts',(-3.7518538734144,-6.96749891570094,
66.7003455302739));
#222375=CARTESIAN_POINT('Ctrl Pts',(-3.57677716645369,-7.05624447574881,
66.7082317599195));
#222376=CARTESIAN_POINT('Ctrl Pts',(-3.40162045815588,-7.14503058809851,
66.7161215931793));
#222377=CARTESIAN_POINT('Ctrl Pts',(-3.2232467624788,-7.22724493007648,
66.7240114264391));
#222378=CARTESIAN_POINT('Ctrl Pts',(-3.0421962217268,-7.30266822117171,
66.731901259699));
#222379=CARTESIAN_POINT('Ctrl Pts',(-2.86093688271062,-7.37817849489728,
66.7398001919843));
#222380=CARTESIAN_POINT('Ctrl Pts',(-2.67699485087025,-7.44688194155259,
66.7476991242696));
#222381=CARTESIAN_POINT('Ctrl Pts',(-2.49092784047274,-7.50860835931385,
66.755598056555));
#222382=CARTESIAN_POINT('Ctrl Pts',(-2.30473793558527,-7.57037554645498,
66.7635022059675));
#222383=CARTESIAN_POINT('Ctrl Pts',(-2.11642058433851,-7.62515642201285,
66.77140635538));
#222384=CARTESIAN_POINT('Ctrl Pts',(-1.92654528210323,-7.67283156833289,
66.7793105047925));
#222385=CARTESIAN_POINT('Ctrl Pts',(-1.73640976262606,-7.72057205171856,
66.7872254865562));
#222386=CARTESIAN_POINT('Ctrl Pts',(-1.54471236372734,-7.76118728382085,
66.7951404683199));
#222387=CARTESIAN_POINT('Ctrl Pts',(-1.35203048045524,-7.79460932824218,
66.8030554500836));
#222388=CARTESIAN_POINT('Ctrl Pts',(-1.27039788740664,-7.80876908267662,
66.8064087517762));
#222389=CARTESIAN_POINT('Ctrl Pts',(-1.18858862504131,-7.82163835642003,
66.8097620534687));
#222390=CARTESIAN_POINT('Ctrl Pts',(-1.10664666945898,-7.83321480293853,
66.8131153551613));
#222391=CARTESIAN_POINT('Ctrl Pts',(-0.917014832310649,-7.8600052646178,
66.8208756381074));
#222392=CARTESIAN_POINT('Ctrl Pts',(-0.726075308837745,-7.8799526064951,
66.8286359210535));
#222393=CARTESIAN_POINT('Ctrl Pts',(-0.534375051767953,-7.89293128717386,
66.8363962039996));
#222394=CARTESIAN_POINT('Ctrl Pts',(-0.342905515546799,-7.9058943473612,
66.844147147057));
#222395=CARTESIAN_POINT('Ctrl Pts',(-0.150677421537793,-7.91190541633262,
66.8518980901143));
#222396=CARTESIAN_POINT('Ctrl Pts',(0.0417517106779919,-7.91088982319028,
66.8596490331717));
#222397=CARTESIAN_POINT('Ctrl Pts',(0.233988302157394,-7.90987524623009,
66.8673922207907));
#222398=CARTESIAN_POINT('Ctrl Pts',(0.426425175715994,-7.90184800493826,
66.8751354084096));
#222399=CARTESIAN_POINT('Ctrl Pts',(0.618499207052614,-7.88678513279494,
66.8828785960286));
#222400=CARTESIAN_POINT('Ctrl Pts',(0.810419981201786,-7.87173427942066,
66.890615605305));
#222401=CARTESIAN_POINT('Ctrl Pts',(1.00197813373313,-7.84965899983031,
66.8983526145815));
#222402=CARTESIAN_POINT('Ctrl Pts',(1.19260995872977,-7.82058837213279,
66.9060896238579));
#222403=CARTESIAN_POINT('Ctrl Pts',(1.3831282731383,-7.79153505436789,66.9138220261781));
#222404=CARTESIAN_POINT('Ctrl Pts',(1.57272100461281,-7.75549473670529,
66.9215544284983));
#222405=CARTESIAN_POINT('Ctrl Pts',(1.76082889986946,-7.71254838463815,
66.9292868308185));
#222406=CARTESIAN_POINT('Ctrl Pts',(1.94886284534487,-7.66961891582482,
66.9370161933436));
#222407=CARTESIAN_POINT('Ctrl Pts',(2.1354127677142,-7.61978889965393,66.9447455558687));
#222408=CARTESIAN_POINT('Ctrl Pts',(2.3199288618094,-7.56319053549121,66.9524749183938));
#222409=CARTESIAN_POINT('Ctrl Pts',(2.50444488391394,-7.50659219341086,
66.9602042779032));
#222410=CARTESIAN_POINT('Ctrl Pts',(2.68692673275618,-7.4432256029294,66.9679336374127));
#222411=CARTESIAN_POINT('Ctrl Pts',(2.8668386540124,-7.37327316270463,66.9756629969221));
#222412=CARTESIAN_POINT('Ctrl Pts',(3.04675959310001,-7.30331721621243,
66.9833927438548));
#222413=CARTESIAN_POINT('Ctrl Pts',(3.22411001279397,-7.22677489190614,
66.9911224907874));
#222414=CARTESIAN_POINT('Ctrl Pts',(3.39837324029387,-7.14387712097952,
66.9988522377201));
#222415=CARTESIAN_POINT('Ctrl Pts',(3.57267713390611,-7.06096000500739,
67.0065837884685));
#222416=CARTESIAN_POINT('Ctrl Pts',(3.74389207622142,-6.97168464319702,
67.0143153392169));
#222417=CARTESIAN_POINT('Ctrl Pts',(3.9115251012887,-6.87632840853231,67.0220468899654));
#222418=CARTESIAN_POINT('Ctrl Pts',(4.07922797166176,-6.78093244312024,
67.0297816621108));
#222419=CARTESIAN_POINT('Ctrl Pts',(4.24334564106713,-6.67945073710558,
67.0375164342563));
#222420=CARTESIAN_POINT('Ctrl Pts',(4.40341324262927,-6.5722045627504,67.0452512064017));
#222421=CARTESIAN_POINT('Ctrl Pts',(4.56367172488819,-6.46483049727742,
67.0529952022669));
#222422=CARTESIAN_POINT('Ctrl Pts',(4.71987019539429,-6.35167843493897,
67.0607391981321));
#222423=CARTESIAN_POINT('Ctrl Pts',(4.87157524210685,-6.23311123440707,
67.0684831939973));
#222424=CARTESIAN_POINT('Ctrl Pts',(5.0233787530051,-6.11446707781403,67.0762322161042));
#222425=CARTESIAN_POINT('Ctrl Pts',(5.17068275718742,-5.99040101240313,
67.0839812382112));
#222426=CARTESIAN_POINT('Ctrl Pts',(5.31309009588742,-5.86131338805417,
67.0917302603182));
#222427=CARTESIAN_POINT('Ctrl Pts',(5.45571506654717,-5.73202848740665,
67.0994911247564));
#222428=CARTESIAN_POINT('Ctrl Pts',(5.5934281701958,-5.59770695063796,67.1072519891945));
#222429=CARTESIAN_POINT('Ctrl Pts',(5.72587117811032,-5.4587837703728,67.1150128536327));
#222430=CARTESIAN_POINT('Ctrl Pts',(5.81695106143292,-5.363247529928,67.1203499313587));
#222431=CARTESIAN_POINT('Ctrl Pts',(5.90553946723006,-5.26553576951593,
67.1256870090848));
#222432=CARTESIAN_POINT('Ctrl Pts',(5.99153182540679,-5.16579784594186,
67.1310240868108));
#222433=CARTESIAN_POINT('Ctrl Pts',(6.12065222105285,-5.01603802511763,
67.139037887132));
#222434=CARTESIAN_POINT('Ctrl Pts',(6.24431386483648,-4.86124937952612,
67.1470516874533));
#222435=CARTESIAN_POINT('Ctrl Pts',(6.36210838962077,-4.70186110372446,
67.1550654877745));
#222436=CARTESIAN_POINT('Ctrl Pts',(6.47976864255138,-4.54265451174288,
67.1630701533093));
#222437=CARTESIAN_POINT('Ctrl Pts',(6.59157490549445,-4.37885900360627,
67.1710748188441));
#222438=CARTESIAN_POINT('Ctrl Pts',(6.69715737020913,-4.21093863154684,
67.179079484379));
#222439=CARTESIAN_POINT('Ctrl Pts',(6.80263740774437,-4.0431811616334,67.1870763844641));
#222440=CARTESIAN_POINT('Ctrl Pts',(6.90190550233217,-3.8713070837191,67.1950732845494));
#222441=CARTESIAN_POINT('Ctrl Pts',(6.99463343477549,-3.69581169881811,
67.2030701846345));
#222442=CARTESIAN_POINT('Ctrl Pts',(7.08728714239552,-3.52045679061698,
67.2110606835364));
#222443=CARTESIAN_POINT('Ctrl Pts',(7.1734109661304,-3.34148664722052,67.2190511824382));
#222444=CARTESIAN_POINT('Ctrl Pts',(7.25272096058811,-3.15942394557075,
67.2270416813401));
#222445=CARTESIAN_POINT('Ctrl Pts',(7.33198091908907,-2.9774761056295,67.2350271391086));
#222446=CARTESIAN_POINT('Ctrl Pts',(7.40443548388706,-2.79243990236596,
67.2430125968771));
#222447=CARTESIAN_POINT('Ctrl Pts',(7.46984730002809,-2.60486128503287,
67.2509980546456));
#222448=CARTESIAN_POINT('Ctrl Pts',(7.53740381313978,-2.41113241357003,
67.2592453364712));
#222449=CARTESIAN_POINT('Ctrl Pts',(7.59744774193219,-2.21469190318688,
67.2674926182968));
#222450=CARTESIAN_POINT('Ctrl Pts',(7.6497716776,-2.01616325742459,67.2757399001224));
#222451=CARTESIAN_POINT('Ctrl Pts',(7.7004001901487,-1.82406742394096,67.2837199499041));
#222452=CARTESIAN_POINT('Ctrl Pts',(7.7438010761231,-1.63001700415982,67.2916999996857));
#222453=CARTESIAN_POINT('Ctrl Pts',(7.77983719867239,-1.43459198455637,
67.2996800494674));
#222454=CARTESIAN_POINT('Ctrl Pts',(7.81587045950469,-1.23918248413365,
67.3076594655337));
#222455=CARTESIAN_POINT('Ctrl Pts',(7.84454006182957,-1.04239893043744,
67.3156388816));
#222456=CARTESIAN_POINT('Ctrl Pts',(7.8657600592359,-0.844831160960169,
67.3236182976663));
#222457=CARTESIAN_POINT('Ctrl Pts',(7.88698163269343,-0.647248717733632,
67.3315983063796));
#222458=CARTESIAN_POINT('Ctrl Pts',(7.90075246300295,-0.448882275345031,
67.3395783150929));
#222459=CARTESIAN_POINT('Ctrl Pts',(7.9070384770834,-0.250326830209312,
67.3475583238062));
#222460=CARTESIAN_POINT('Ctrl Pts',(7.91332592411466,-0.0517261226573362,
67.355540151631));
#222461=CARTESIAN_POINT('Ctrl Pts',(7.91212514395374,0.147063339189747,
67.3635219794557));
#222462=CARTESIAN_POINT('Ctrl Pts',(7.90345417952032,0.345446135052728,
67.3715038072804));
#222463=CARTESIAN_POINT('Ctrl Pts',(7.89477676783494,0.543976437444913,
67.3794915699531));
#222464=CARTESIAN_POINT('Ctrl Pts',(7.87861809117559,0.742099135384174,
67.3874793326257));
#222465=CARTESIAN_POINT('Ctrl Pts',(7.85504819410101,0.939222480752311,
67.3954670952983));
#222466=CARTESIAN_POINT('Ctrl Pts',(7.83146791600566,1.13643264625102,67.4034583760657));
#222467=CARTESIAN_POINT('Ctrl Pts',(7.80046995710848,1.33264225080553,67.411449656833));
#222468=CARTESIAN_POINT('Ctrl Pts',(7.76217567509884,1.52726873499851,67.4194409376004));
#222469=CARTESIAN_POINT('Ctrl Pts',(7.72384536326102,1.72207833683767,67.4274397371005));
#222470=CARTESIAN_POINT('Ctrl Pts',(7.67820509114356,1.91530151755185,67.4354385366006));
#222471=CARTESIAN_POINT('Ctrl Pts',(7.62542660630291,2.10636893062153,67.4434373361007));
#222472=CARTESIAN_POINT('Ctrl Pts',(7.61333965782149,2.15012581347302,67.4452691635539));
#222473=CARTESIAN_POINT('Ctrl Pts',(7.60087853581273,2.19376970588041,67.4471009910071));
#222474=CARTESIAN_POINT('Ctrl Pts',(7.58804566267132,2.23729390586374,67.4489328184604));
#222475=CARTESIAN_POINT('Ctrl Pts',(7.53111436847256,2.43038309226115,67.4570594715109));
#222476=CARTESIAN_POINT('Ctrl Pts',(7.46676228830706,2.62145561255573,67.4651861245613));
#222477=CARTESIAN_POINT('Ctrl Pts',(7.39515119991861,2.80992165911123,67.4733127776118));
#222478=CARTESIAN_POINT('Ctrl Pts',(7.32360107010053,2.99822727491472,67.4814325128907));
#222479=CARTESIAN_POINT('Ctrl Pts',(7.24480436383578,3.18393054367065,67.4895522481696));
#222480=CARTESIAN_POINT('Ctrl Pts',(7.15897259892058,3.36645693985596,67.4976719834486));
#222481=CARTESIAN_POINT('Ctrl Pts',(7.0732030891675,3.54885094670502,67.5057858293526));
#222482=CARTESIAN_POINT('Ctrl Pts',(6.98040882999578,3.72807238773233,67.5138996752567));
#222483=CARTESIAN_POINT('Ctrl Pts',(6.88084958536843,3.90356631601604,67.5220135211608));
#222484=CARTESIAN_POINT('Ctrl Pts',(6.781361081294,4.07893554932477,67.530121601875));
#222485=CARTESIAN_POINT('Ctrl Pts',(6.67511733837263,4.25058227714498,67.5382296825893));
#222486=CARTESIAN_POINT('Ctrl Pts',(6.56242439132248,4.41797545355062,67.5463377633035));
#222487=CARTESIAN_POINT('Ctrl Pts',(6.44977984646348,4.58529673373972,67.554442361556));
#222488=CARTESIAN_POINT('Ctrl Pts',(6.33069179825181,4.74836784121332,67.5625469598086));
#222489=CARTESIAN_POINT('Ctrl Pts',(6.20551045213857,4.90668534026781,67.5706515580611));
#222490=CARTESIAN_POINT('Ctrl Pts',(6.08036823406626,5.06495335388555,67.5787536230524));
#222491=CARTESIAN_POINT('Ctrl Pts',(5.94913671409405,5.21847047257917,67.5868556880437));
#222492=CARTESIAN_POINT('Ctrl Pts',(5.81220769575312,5.36676464002552,67.594957753035));
#222493=CARTESIAN_POINT('Ctrl Pts',(5.73936970812569,5.44564820221379,67.5992675634517));
#222494=CARTESIAN_POINT('Ctrl Pts',(5.66492024938762,5.52305442511757,67.6035773738683));
#222495=CARTESIAN_POINT('Ctrl Pts',(5.58892283565255,5.59891619307893,67.607887184285));
#222496=CARTESIAN_POINT('Ctrl Pts',(5.4427631216407,5.74481503048304,67.6161758960581));
#222497=CARTESIAN_POINT('Ctrl Pts',(5.29093861110085,5.88493634288509,67.6244646078311));
#222498=CARTESIAN_POINT('Ctrl Pts',(5.13393236485294,6.01885865202993,67.6327533196042));
#222499=CARTESIAN_POINT('Ctrl Pts',(4.97683560604934,6.15285816606791,67.641046809738));
#222500=CARTESIAN_POINT('Ctrl Pts',(4.81455137147102,6.28065135377505,67.6493402998718));
#222501=CARTESIAN_POINT('Ctrl Pts',(4.64759513050342,6.40185758221166,67.6576337900056));
#222502=CARTESIAN_POINT('Ctrl Pts',(4.48053257504112,6.5231409924227,67.665932561273));
#222503=CARTESIAN_POINT('Ctrl Pts',(4.30879231126388,6.63782889902091,67.6742313325405));
#222504=CARTESIAN_POINT('Ctrl Pts',(4.1329187473739,6.74558400938016,67.6825301038079));
#222505=CARTESIAN_POINT('Ctrl Pts',(3.95684045650926,6.85346455290435,67.6908385353238));
#222506=CARTESIAN_POINT('Ctrl Pts',(3.77661949784773,6.9543960158946,67.6991469668397));
#222507=CARTESIAN_POINT('Ctrl Pts',(3.59282635899221,7.04808624763707,67.7074553983556));
#222508=CARTESIAN_POINT('Ctrl Pts',(3.40891984406263,7.14183427386914,67.7157689550757));
#222509=CARTESIAN_POINT('Ctrl Pts',(3.22143701376419,7.22833202552435,67.7240825117957));
#222510=CARTESIAN_POINT('Ctrl Pts',(3.03096958926497,7.30733496898499,67.7323960685157));
#222511=CARTESIAN_POINT('Ctrl Pts',(2.84029392826499,7.38642428572727,67.7407187143803));
#222512=CARTESIAN_POINT('Ctrl Pts',(2.64662742391201,7.45800231085157,67.7490413602449));
#222513=CARTESIAN_POINT('Ctrl Pts',(2.45057979742485,7.52187341401417,67.7573640061095));
#222514=CARTESIAN_POINT('Ctrl Pts',(2.3761623570886,7.54611815542717,67.760523187443));
#222515=CARTESIAN_POINT('Ctrl Pts',(2.30140196972341,7.56925294275549,67.7636823687765));
#222516=CARTESIAN_POINT('Ctrl Pts',(2.2263324580011,7.59126898393482,67.7668415501099));
#222517=CARTESIAN_POINT('Ctrl Pts',(2.01964250937032,7.65188606157403,67.7755397687682));
#222518=CARTESIAN_POINT('Ctrl Pts',(1.81042481073598,7.70407247221576,67.7842379874265));
#222519=CARTESIAN_POINT('Ctrl Pts',(1.59935335019757,7.74764414910828,67.7929362060847));
#222520=CARTESIAN_POINT('Ctrl Pts',(1.3884673442381,7.79117754244048,67.8016267821916));
#222521=CARTESIAN_POINT('Ctrl Pts',(1.17573105250927,7.8261112696819,67.8103173582985));
#222522=CARTESIAN_POINT('Ctrl Pts',(0.961830060516146,7.85231201205655,
67.8190079344054));
#222523=CARTESIAN_POINT('Ctrl Pts',(0.742799172910187,7.8791411155814,67.8279069328662));
#222524=CARTESIAN_POINT('Ctrl Pts',(0.52254724978505,7.89681304929409,67.836805931327));
#222525=CARTESIAN_POINT('Ctrl Pts',(0.301821301022647,7.90524034436961,
67.8457049297878));
#222526=CARTESIAN_POINT('Ctrl Pts',(0.0869000806119238,7.91344601548598,
67.8543698992684));
#222527=CARTESIAN_POINT('Ctrl Pts',(-0.128470297376114,7.91288707579814,
67.8630348687491));
#222528=CARTESIAN_POINT('Ctrl Pts',(-0.343593585467,7.90353493368796,67.8716998382298));
#222529=CARTESIAN_POINT('Ctrl Pts',(-0.567432152443107,7.89380390871769,
67.8807158511806));
#222530=CARTESIAN_POINT('Ctrl Pts',(-0.791002962238243,7.87455234026838,
67.8897318641314));
#222531=CARTESIAN_POINT('Ctrl Pts',(-1.01351814020634,7.8458079239472,67.8987478770822));
#222532=CARTESIAN_POINT('Ctrl Pts',(-1.23603331817452,7.81706350762602,
67.907763890033));
#222533=CARTESIAN_POINT('Ctrl Pts',(-1.45749257836948,7.77882621261139,
67.9167799029838));
#222534=CARTESIAN_POINT('Ctrl Pts',(-1.67710863993402,7.73118539487048,
67.9257959159346));
#222535=CARTESIAN_POINT('Ctrl Pts',(-1.86735884610759,7.68991484601848,
67.933606357077));
#222536=CARTESIAN_POINT('Ctrl Pts',(-2.05614366473886,7.64160470917383,
67.9414167982193));
#222537=CARTESIAN_POINT('Ctrl Pts',(-2.24290433812382,7.58638920238247,
67.9492272393616));
#222538=CARTESIAN_POINT('Ctrl Pts',(-2.42965154643451,7.53117767651968,
67.9570371173865));
#222539=CARTESIAN_POINT('Ctrl Pts',(-2.61437456247086,7.46906187225572,
67.9648469954115));
#222540=CARTESIAN_POINT('Ctrl Pts',(-2.79652900932253,7.40022611141157,
67.9726568734365));
#222541=CARTESIAN_POINT('Ctrl Pts',(-2.97870247444238,7.33138316360611,
67.9804675668704));
#222542=CARTESIAN_POINT('Ctrl Pts',(-3.15830650705467,7.25581898698974,
67.9882782603043));
#222543=CARTESIAN_POINT('Ctrl Pts',(-3.33481582197461,7.17376640500008,
67.9960889537381));
#222544=CARTESIAN_POINT('Ctrl Pts',(-3.51145039772298,7.09165559393396,
68.0039051900745));
#222545=CARTESIAN_POINT('Ctrl Pts',(-3.68498554836475,7.00304732691777,
68.011721426411));
#222546=CARTESIAN_POINT('Ctrl Pts',(-3.85491897140076,6.90822124167535,
68.0195376627474));
#222547=CARTESIAN_POINT('Ctrl Pts',(-4.02491522128161,6.81336009785741,
68.0273567888594));
#222548=CARTESIAN_POINT('Ctrl Pts',(-4.19130678757497,6.7122767350376,68.0351759149715));
#222549=CARTESIAN_POINT('Ctrl Pts',(-4.35361946929871,6.60529473351063,
68.0429950410835));
#222550=CARTESIAN_POINT('Ctrl Pts',(-4.51611263796829,6.49819377113284,
68.0508228618347));
#222551=CARTESIAN_POINT('Ctrl Pts',(-4.67451757258652,6.38518126845022,
68.0586506825859));
#222552=CARTESIAN_POINT('Ctrl Pts',(-4.82839146064093,6.26662244776321,
68.0664785033371));
#222553=CARTESIAN_POINT('Ctrl Pts',(-4.94811612292252,6.17437538137183,
68.0725690961445));
#222554=CARTESIAN_POINT('Ctrl Pts',(-5.0650983463964,6.07877146212607,68.0786596889519));
#222555=CARTESIAN_POINT('Ctrl Pts',(-5.17914486036435,5.97999828723734,
68.0847502817594));
#222556=CARTESIAN_POINT('Ctrl Pts',(-5.32878187294105,5.85040096506739,
68.0927415660241));
#222557=CARTESIAN_POINT('Ctrl Pts',(-5.47368874160669,5.71506514973898,
68.1007328502889));
#222558=CARTESIAN_POINT('Ctrl Pts',(-5.61340759243505,5.57436778488758,
68.1087241345537));
#222559=CARTESIAN_POINT('Ctrl Pts',(-5.75301402109007,5.43378362955262,
68.1167089887803));
#222560=CARTESIAN_POINT('Ctrl Pts',(-5.88744051612372,5.28784675950667,
68.1246938430069));
#222561=CARTESIAN_POINT('Ctrl Pts',(-6.01626352534858,5.13697325217489,
68.1326786972335));
#222562=CARTESIAN_POINT('Ctrl Pts',(-6.1450049258841,4.9861953224054,68.1406584930975));
#222563=CARTESIAN_POINT('Ctrl Pts',(-6.26814969893185,4.83048724323403,
68.1486382889615));
#222564=CARTESIAN_POINT('Ctrl Pts',(-6.38531203854047,4.67030097215053,
68.1566180848256));
#222565=CARTESIAN_POINT('Ctrl Pts',(-6.50824821074617,4.50222062250324,
68.1649911299677));
#222566=CARTESIAN_POINT('Ctrl Pts',(-6.62459715263853,4.32920982727371,
68.1733641751099));
#222567=CARTESIAN_POINT('Ctrl Pts',(-6.73396102446077,4.15182970761606,
68.1817372202521));
#222568=CARTESIAN_POINT('Ctrl Pts',(-6.83811830582926,3.98289429298126,
68.1897116418253));
#222569=CARTESIAN_POINT('Ctrl Pts',(-6.93593994293605,3.80999622431243,
68.1976860633985));
#222570=CARTESIAN_POINT('Ctrl Pts',(-7.02712676734891,3.63364973485455,
68.2056604849716));
#222571=CARTESIAN_POINT('Ctrl Pts',(-7.11830686206389,3.45731625998077,
68.2136343180229));
#222572=CARTESIAN_POINT('Ctrl Pts',(-7.20285296571857,3.27753516944541,
68.2216081510741));
#222573=CARTESIAN_POINT('Ctrl Pts',(-7.28051203477752,3.09484498989201,
68.2295819841253));
#222574=CARTESIAN_POINT('Ctrl Pts',(-7.35817741734007,2.91213995804744,
68.2375564654308));
#222575=CARTESIAN_POINT('Ctrl Pts',(-7.4289545182984,2.72652567467862,68.2455309467363));
#222576=CARTESIAN_POINT('Ctrl Pts',(-7.49263843978814,2.5385606572641,68.2535054280418));
#222577=CARTESIAN_POINT('Ctrl Pts',(-7.55633741607271,2.35055120516801,
68.2614817945042));
#222578=CARTESIAN_POINT('Ctrl Pts',(-7.61293976347384,2.16019022921051,
68.2694581609665));
#222579=CARTESIAN_POINT('Ctrl Pts',(-7.66229033963456,1.96805176536161,
68.2774345274288));
#222580=CARTESIAN_POINT('Ctrl Pts',(-7.7116793054823,1.77576383749292,68.2854170986862));
#222581=CARTESIAN_POINT('Ctrl Pts',(-7.75380514743358,1.58169598472964,
68.2933996699437));
#222582=CARTESIAN_POINT('Ctrl Pts',(-7.78856355251007,1.38643383849056,
68.3013822412011));
#222583=CARTESIAN_POINT('Ctrl Pts',(-7.82333757724496,1.19108394576213,
68.3093683996494));
#222584=CARTESIAN_POINT('Ctrl Pts',(-7.85073751366954,0.994539020857734,
68.3173545580978));
#222585=CARTESIAN_POINT('Ctrl Pts',(-7.87071083101772,0.797390753959685,
68.3253407165462));
#222586=CARTESIAN_POINT('Ctrl Pts',(-7.89070412513149,0.600045304758576,
68.3333348625317));
#222587=CARTESIAN_POINT('Ctrl Pts',(-7.90325593885016,0.402095642404761,
68.3413290085173));
#222588=CARTESIAN_POINT('Ctrl Pts',(-7.90836580526636,0.204135469954951,
68.3493231545028));
#222589=CARTESIAN_POINT('Ctrl Pts',(-7.91012318491482,0.136053224758531,
68.3520724924145));
#222590=CARTESIAN_POINT('Ctrl Pts',(-7.91100078247404,0.0679697153253449,
68.3548218303263));
#222591=CARTESIAN_POINT('Ctrl Pts',(-7.91099999947649,-9.10112777354474E-5,
68.357571168238));
#222592=CARTESIAN_POINT('',(-7.911,-5.21527265817667E-12,72.3576684917632));
#222593=CARTESIAN_POINT('Ctrl Pts',(-7.91099999855147,-0.000151389195569007,
68.3558388064656));
#222594=CARTESIAN_POINT('Ctrl Pts',(-7.91099267116411,-0.383051642702635,
68.3692832323818));
#222595=CARTESIAN_POINT('Ctrl Pts',(-7.88318610730695,-0.765434127276486,
68.3831365286044));
#222596=CARTESIAN_POINT('Ctrl Pts',(-7.82570790785023,-1.15863156054466,
68.3989553848451));
#222597=CARTESIAN_POINT('Ctrl Pts',(-7.82357060661066,-1.1729766882449,
68.3995346283287));
#222598=CARTESIAN_POINT('Ctrl Pts',(-7.82014362030889,-1.19555181953054,
68.4004494428244));
#222599=CARTESIAN_POINT('Ctrl Pts',(-7.81888035569568,-1.20378585219969,
68.4007837929193));
#222600=CARTESIAN_POINT('Ctrl Pts',(-7.81672501576949,-1.21768795291669,
68.4013494332849));
#222601=CARTESIAN_POINT('Ctrl Pts',(-7.81583977327504,-1.22335708649469,
68.4015804140919));
#222602=CARTESIAN_POINT('Ctrl Pts',(-7.81407557906146,-1.23457499010191,
68.402038095322));
#222603=CARTESIAN_POINT('Ctrl Pts',(-7.81319688273769,-1.24012379737284,
68.4022647842345));
#222604=CARTESIAN_POINT('Ctrl Pts',(-7.81149905296429,-1.25077184924765,
68.4027003696608));
#222605=CARTESIAN_POINT('Ctrl Pts',(-7.81068083490817,-1.25587123876143,
68.402909225789));
#222606=CARTESIAN_POINT('Ctrl Pts',(-7.80880327587672,-1.2674999617876,
68.4033860752584));
#222607=CARTESIAN_POINT('Ctrl Pts',(-7.80774073900184,-1.27402876993698,
68.4036542073709));
#222608=CARTESIAN_POINT('Ctrl Pts',(-7.80491844125137,-1.29123437701826,
68.4043618947425));
#222609=CARTESIAN_POINT('Ctrl Pts',(-7.80314496437676,-1.30190888862316,
68.4048020358127));
#222610=CARTESIAN_POINT('Ctrl Pts',(-7.79165457493977,-1.37020230018491,
68.4076247768268));
#222611=CARTESIAN_POINT('Ctrl Pts',(-7.78132158893045,-1.42771476599643,
68.4100329197169));
#222612=CARTESIAN_POINT('Ctrl Pts',(-7.76735303439255,-1.50080083637552,
68.4131283185282));
#222613=CARTESIAN_POINT('Ctrl Pts',(-7.76430591961106,-1.51648603477537,
68.4137947005674));
#222614=CARTESIAN_POINT('Ctrl Pts',(-7.68561737290302,-1.91508520955995,
68.4307800253249));
#222615=CARTESIAN_POINT('Ctrl Pts',(-7.58179044984547,-2.29187687176655,
68.4479969538861));
#222616=CARTESIAN_POINT('Ctrl Pts',(-7.42143069826756,-2.74113287224135,
68.4690066971408));
#222617=CARTESIAN_POINT('Ctrl Pts',(-7.39093334107457,-2.8223301461755,
68.4728256097494));
#222618=CARTESIAN_POINT('Ctrl Pts',(-7.3312520235115,-2.9736218218695,68.4799717258169));
#222619=CARTESIAN_POINT('Ctrl Pts',(-7.30238205928943,-3.04382971719106,
68.4833004782112));
#222620=CARTESIAN_POINT('Ctrl Pts',(-7.20486734381686,-3.27159619849965,
68.4941311044133));
#222621=CARTESIAN_POINT('Ctrl Pts',(-7.13209748889981,-3.4273375706699,
68.5015854153323));
#222622=CARTESIAN_POINT('Ctrl Pts',(-6.90353947332873,-3.87763214491744,
68.5232233510192));
#222623=CARTESIAN_POINT('Ctrl Pts',(-6.73415091316401,-4.16486754002624,
68.5371195904191));
#222624=CARTESIAN_POINT('Ctrl Pts',(-6.5320027790225,-4.46291257803096,
68.5517117487156));
#222625=CARTESIAN_POINT('Ctrl Pts',(-6.51674357505487,-4.48516467615891,
68.5528024463055));
#222626=CARTESIAN_POINT('Ctrl Pts',(-6.49174591880461,-4.5212212174636,
68.55457198989));
#222627=CARTESIAN_POINT('Ctrl Pts',(-6.4820766006714,-4.53507324276247,
68.5552523404065));
#222628=CARTESIAN_POINT('Ctrl Pts',(-6.4632510976959,-4.56185898063703,
68.5565690373003));
#222629=CARTESIAN_POINT('Ctrl Pts',(-6.45410027725383,-4.57479635878669,
68.557205495623));
#222630=CARTESIAN_POINT('Ctrl Pts',(-6.43822743721823,-4.59709487385287,
68.5583033893215));
#222631=CARTESIAN_POINT('Ctrl Pts',(-6.43152373007514,-4.60646896471027,
68.5587652134299));
#222632=CARTESIAN_POINT('Ctrl Pts',(-6.41760422149165,-4.62584361320477,
68.5597203269337));
#222633=CARTESIAN_POINT('Ctrl Pts',(-6.41038547042436,-4.63584201619037,
68.5602135523368));
#222634=CARTESIAN_POINT('Ctrl Pts',(-6.39281228645006,-4.66006239733254,
68.5614091968327));
#222635=CARTESIAN_POINT('Ctrl Pts',(-6.38243372549041,-4.67426681087956,
68.5621111089101));
#222636=CARTESIAN_POINT('Ctrl Pts',(-6.35006682320306,-4.71825634865552,
68.5642871852062));
#222637=CARTESIAN_POINT('Ctrl Pts',(-6.32791659535625,-4.74792198950683,
68.565758062387));
#222638=CARTESIAN_POINT('Ctrl Pts',(-5.92415346049836,-5.28083437618242,
68.5922461044926));
#222639=CARTESIAN_POINT('Ctrl Pts',(-5.48383614965457,-5.73675913105012,
68.6157207141508));
#222640=CARTESIAN_POINT('Ctrl Pts',(-4.81573601843965,-6.28055924018325,
68.6473916385621));
#222641=CARTESIAN_POINT('Ctrl Pts',(-4.63126144119365,-6.41779970849139,
68.6558191605972));
#222642=CARTESIAN_POINT('Ctrl Pts',(-4.26509920350076,-6.66618844531353,
68.6722879951277));
#222643=CARTESIAN_POINT('Ctrl Pts',(-4.08438534066451,-6.77841649412097,
68.6803051892477));
#222644=CARTESIAN_POINT('Ctrl Pts',(-3.84148541821903,-6.91602037258903,
68.6911535938341));
#222645=CARTESIAN_POINT('Ctrl Pts',(-3.78318320161178,-6.94808409577938,
68.6937629200508));
#222646=CARTESIAN_POINT('Ctrl Pts',(-3.70155245617908,-6.99164544597577,
68.6974312947829));
#222647=CARTESIAN_POINT('Ctrl Pts',(-3.67856048631828,-7.00376965341143,
68.6984661567266));
#222648=CARTESIAN_POINT('Ctrl Pts',(-3.63895051481667,-7.02440807363235,
68.7002523512833));
#222649=CARTESIAN_POINT('Ctrl Pts',(-3.62236127977562,-7.03297720639666,
68.7010014425127));
#222650=CARTESIAN_POINT('Ctrl Pts',(-3.59998266934696,-7.04443664513221,
68.7020134717656));
#222651=CARTESIAN_POINT('Ctrl Pts',(-3.59421978260699,-7.04737873403146,
68.7022742222193));
#222652=CARTESIAN_POINT('Ctrl Pts',(-3.58280999475297,-7.05318606295414,
68.7027907523536));
#222653=CARTESIAN_POINT('Ctrl Pts',(-3.57716324970943,-7.05605159999429,
68.7030465190522));
#222654=CARTESIAN_POINT('Ctrl Pts',(-3.5662129094974,-7.06159201365216,
68.7035427785839));
#222655=CARTESIAN_POINT('Ctrl Pts',(-3.56090972896128,-7.06426770338445,
68.7037832359767));
#222656=CARTESIAN_POINT('Ctrl Pts',(-3.54865717673049,-7.07043235656505,
68.704339083303));
#222657=CARTESIAN_POINT('Ctrl Pts',(-3.54170567128436,-7.07391704815259,
68.7046546598619));
#222658=CARTESIAN_POINT('Ctrl Pts',(-3.52306543037367,-7.08322677394313,
68.7055014696299));
#222659=CARTESIAN_POINT('Ctrl Pts',(-3.51136742059046,-7.08903310703499,
68.7060335324084));
#222660=CARTESIAN_POINT('Ctrl Pts',(-3.42954000370042,-7.12939609386607,
68.7097600120389));
#222661=CARTESIAN_POINT('Ctrl Pts',(-3.35891695323342,-7.16294003450221,
68.7130004460642));
#222662=CARTESIAN_POINT('Ctrl Pts',(-3.22304749508098,-7.22502287513372,
68.7192973931093));
#222663=CARTESIAN_POINT('Ctrl Pts',(-3.15789102889086,-7.25373796443689,
68.72234318374));
#222664=CARTESIAN_POINT('Ctrl Pts',(-2.91452953112833,-7.35708942044556,
68.7337914899018));
#222665=CARTESIAN_POINT('Ctrl Pts',(-2.73400217071512,-7.42606710366668,
68.7424250757653));
#222666=CARTESIAN_POINT('Ctrl Pts',(-2.25624090499895,-7.58883107296132,
68.7653231090039));
#222667=CARTESIAN_POINT('Ctrl Pts',(-1.95566689615631,-7.67178893398544,
68.7797685144795));
#222668=CARTESIAN_POINT('Ctrl Pts',(-1.61085615867597,-7.74536940370806,
68.7959373903439));
#222669=CARTESIAN_POINT('Ctrl Pts',(-1.57065983744819,-7.75362060349462,
68.79781641557));
#222670=CARTESIAN_POINT('Ctrl Pts',(-1.48298861968049,-7.77090735270843,
68.8019004650449));
#222671=CARTESIAN_POINT('Ctrl Pts',(-1.43549132550243,-7.77982140128291,
68.8041040025682));
#222672=CARTESIAN_POINT('Ctrl Pts',(-1.33072105479945,-7.79849200249259,
68.8089424089125));
#222673=CARTESIAN_POINT('Ctrl Pts',(-1.27341604509132,-7.80805402934875,
68.8115742725154));
#222674=CARTESIAN_POINT('Ctrl Pts',(-1.01693628396925,-7.84795203404889,
68.8232817349391));
#222675=CARTESIAN_POINT('Ctrl Pts',(-0.816744777269923,-7.87130516574341,
68.8322239127042));
#222676=CARTESIAN_POINT('Ctrl Pts',(-0.448488523544445,-7.90006120217563,
68.848233701133));
#222677=CARTESIAN_POINT('Ctrl Pts',(-0.280725844923976,-7.90780035781369,
68.8553617724685));
#222678=CARTESIAN_POINT('Ctrl Pts',(-0.023395804265896,-7.91147109826808,
68.8660305133032));
#222679=CARTESIAN_POINT('Ctrl Pts',(0.0660621300034966,-7.91122991747475,
68.8696906404969));
#222680=CARTESIAN_POINT('Ctrl Pts',(0.171259219025422,-7.90916176129038,
68.873938282075));
#222681=CARTESIAN_POINT('Ctrl Pts',(0.18701872281499,-7.90880480777876,
68.8745731311813));
#222682=CARTESIAN_POINT('Ctrl Pts',(0.211151443637993,-7.90818602735886,
68.8755430186653));
#222683=CARTESIAN_POINT('Ctrl Pts',(0.219525441755695,-7.90795800168826,
68.8758791497306));
#222684=CARTESIAN_POINT('Ctrl Pts',(0.234788091929472,-7.90751813464895,
68.8764910315976));
#222685=CARTESIAN_POINT('Ctrl Pts',(0.241676853825557,-7.90731059188653,
68.876766921324));
#222686=CARTESIAN_POINT('Ctrl Pts',(0.25656066684261,-7.90684270822007,
68.8773623998683));
#222687=CARTESIAN_POINT('Ctrl Pts',(0.264555616015933,-7.9065792423045,
68.8776818870771));
#222688=CARTESIAN_POINT('Ctrl Pts',(0.286204496454357,-7.90583295095865,
68.8785459797097));
#222689=CARTESIAN_POINT('Ctrl Pts',(0.299857628101998,-7.90532687923897,
68.8790898302436));
#222690=CARTESIAN_POINT('Ctrl Pts',(0.36379316573564,-7.90279115023373,
68.8816314823334));
#222691=CARTESIAN_POINT('Ctrl Pts',(0.414057314165239,-7.90031708827669,
68.8836148153806));
#222692=CARTESIAN_POINT('Ctrl Pts',(1.18707292050748,-7.8548706140366,68.9138953598185));
#222693=CARTESIAN_POINT('Ctrl Pts',(1.90056243693366,-7.71337058912142,
68.938425648029));
#222694=CARTESIAN_POINT('Ctrl Pts',(2.8807247211722,-7.3745043618532,68.9732787214039));
#222695=CARTESIAN_POINT('Ctrl Pts',(3.17020330597196,-7.25476991758539,
68.9837986703218));
#222696=CARTESIAN_POINT('Ctrl Pts',(3.58942916883665,-7.05147573013782,
69.000281574889));
#222697=CARTESIAN_POINT('Ctrl Pts',(3.72507333268752,-6.98076906052019,
69.0058223942346));
#222698=CARTESIAN_POINT('Ctrl Pts',(3.93614406620698,-6.86284093269931,
69.0149015035908));
#222699=CARTESIAN_POINT('Ctrl Pts',(4.01297284516761,-6.81820091398579,
69.018305525603));
#222700=CARTESIAN_POINT('Ctrl Pts',(4.12686057970146,-6.74943668443656,
69.0235251388711));
#222701=CARTESIAN_POINT('Ctrl Pts',(4.1644974755192,-6.72627938985658,69.0252790628599));
#222702=CARTESIAN_POINT('Ctrl Pts',(4.2089645106925,-6.69840335668968,69.0273881769384));
#222703=CARTESIAN_POINT('Ctrl Pts',(4.21598439557585,-6.69398725397687,
69.0277222368543));
#222704=CARTESIAN_POINT('Ctrl Pts',(4.22677575800657,-6.6871748637095,69.0282374866888));
#222705=CARTESIAN_POINT('Ctrl Pts',(4.23055218990476,-6.68478639409126,
69.0284181218006));
#222706=CARTESIAN_POINT('Ctrl Pts',(4.23742894821586,-6.68042890823025,
69.0287476461064));
#222707=CARTESIAN_POINT('Ctrl Pts',(4.24052993338372,-6.67846092846852,
69.0288964610994));
#222708=CARTESIAN_POINT('Ctrl Pts',(4.24728066833008,-6.67417010876501,
69.0292209084398));
#222709=CARTESIAN_POINT('Ctrl Pts',(4.25092988785623,-6.67184643144703,
69.0293966012091));
#222710=CARTESIAN_POINT('Ctrl Pts',(4.26094571556994,-6.66545719897486,
69.0298796657077));
#222711=CARTESIAN_POINT('Ctrl Pts',(4.26730838626577,-6.66138553141146,
69.0301874806836));
#222712=CARTESIAN_POINT('Ctrl Pts',(4.29898312434527,-6.64105189335956,
69.0317245061905));
#222713=CARTESIAN_POINT('Ctrl Pts',(4.32420779092285,-6.62465494083208,
69.0329633777252));
#222714=CARTESIAN_POINT('Ctrl Pts',(4.7360508373138,-6.35358752296343,69.0534252411683));
#222715=CARTESIAN_POINT('Ctrl Pts',(5.09964201529366,-6.06562659517763,
69.0748468048089));
#222716=CARTESIAN_POINT('Ctrl Pts',(5.78957145143553,-5.41310521750574,
69.1191708386676));
#222717=CARTESIAN_POINT('Ctrl Pts',(6.11161874692291,-5.04668612007073,
69.1419679397868));
#222718=CARTESIAN_POINT('Ctrl Pts',(6.45585263016582,-4.5733552155204,69.1678168702819));
#222719=CARTESIAN_POINT('Ctrl Pts',(6.5122608449502,-4.49266855296762,69.1721131791636));
#222720=CARTESIAN_POINT('Ctrl Pts',(6.67613615065987,-4.24868615481598,
69.1847715256489));
#222721=CARTESIAN_POINT('Ctrl Pts',(6.77907586512952,-4.08243385150327,
69.1929609192879));
#222722=CARTESIAN_POINT('Ctrl Pts',(6.89313802199598,-3.88198458271381,
69.2023346454192));
#222723=CARTESIAN_POINT('Ctrl Pts',(6.91031547873694,-3.85132394377513,
69.203755124983));
#222724=CARTESIAN_POINT('Ctrl Pts',(6.93272861315077,-3.81068522443658,
69.205620516761));
#222725=CARTESIAN_POINT('Ctrl Pts',(6.93814795430447,-3.80080923869968,
69.2060724969384));
#222726=CARTESIAN_POINT('Ctrl Pts',(6.94698731077291,-3.78461885410698,
69.2068112661683));
#222727=CARTESIAN_POINT('Ctrl Pts',(6.9504198467011,-3.77831133204551,69.2070985355975));
#222728=CARTESIAN_POINT('Ctrl Pts',(6.95703735435253,-3.76611167003633,
69.2076531090742));
#222729=CARTESIAN_POINT('Ctrl Pts',(6.96022344000786,-3.76022014335748,
69.2079204556589));
#222730=CARTESIAN_POINT('Ctrl Pts',(6.96753713534063,-3.74665493339144,
69.2085349393069));
#222731=CARTESIAN_POINT('Ctrl Pts',(6.97165956053072,-3.73897845607445,
69.2088818780199));
#222732=CARTESIAN_POINT('Ctrl Pts',(6.98262218688279,-3.71848349414215,
69.2098060389638));
#222733=CARTESIAN_POINT('Ctrl Pts',(6.98943978687597,-3.70565292083379,
69.2103823993173));
#222734=CARTESIAN_POINT('Ctrl Pts',(7.01103092801316,-3.66474730170878,
69.2122129709258));
#222735=CARTESIAN_POINT('Ctrl Pts',(7.02567104195463,-3.63660197175208,
69.2134621200273));
#222736=CARTESIAN_POINT('Ctrl Pts',(7.31090912016085,-3.08008560910539,
69.2379603604112));
#222737=CARTESIAN_POINT('Ctrl Pts',(7.52136943827937,-2.5229752637,69.2587061061502));
#222738=CARTESIAN_POINT('Ctrl Pts',(7.75354823923443,-1.60888252737453,
69.2908190019049));
#222739=CARTESIAN_POINT('Ctrl Pts',(7.81703368902067,-1.26490395938088,
69.3025508367558));
#222740=CARTESIAN_POINT('Ctrl Pts',(7.87488659003489,-0.769644385982223,
69.3201719177187));
#222741=CARTESIAN_POINT('Ctrl Pts',(7.88800296910085,-0.620964750366225,
69.3255572171987));
#222742=CARTESIAN_POINT('Ctrl Pts',(7.90281241697206,-0.373196587133696,
69.3348184871047));
#222743=CARTESIAN_POINT('Ctrl Pts',(7.90686322027276,-0.27428532286279,
69.3385915466291));
#222744=CARTESIAN_POINT('Ctrl Pts',(7.91012528879533,-0.127132962586155,
69.3443524357003));
#222745=CARTESIAN_POINT('Ctrl Pts',(7.91075310362411,-0.0789304516088896,
69.3462630678072));
#222746=CARTESIAN_POINT('Ctrl Pts',(7.91097386826388,-0.0220911882680467,
69.3485470334868));
#222747=CARTESIAN_POINT('Ctrl Pts',(7.91099326849609,-0.0134561739420375,
69.3488948591021));
#222748=CARTESIAN_POINT('Ctrl Pts',(7.91100138283853,-0.000141531331991104,
69.3494324715951));
#222749=CARTESIAN_POINT('Ctrl Pts',(7.91100008244892,0.00453812880742098,
69.3496216699129));
#222750=CARTESIAN_POINT('Ctrl Pts',(7.910990130612,0.0130791191128701,69.3499674255897));
#222751=CARTESIAN_POINT('Ctrl Pts',(7.91098280436475,0.0169404525733413,
69.3501239054311));
#222752=CARTESIAN_POINT('Ctrl Pts',(7.91096222122711,0.024768277940188,
69.3504414603468));
#222753=CARTESIAN_POINT('Ctrl Pts',(7.91094880821848,0.0287347684210849,
69.3506025444539));
#222754=CARTESIAN_POINT('Ctrl Pts',(7.91090184056813,0.040096964525484,
69.3510644716996));
#222755=CARTESIAN_POINT('Ctrl Pts',(7.9108608980438,0.0474926179049623,
69.3513657401058));
#222756=CARTESIAN_POINT('Ctrl Pts',(7.91063898918875,0.0794754370881539,
69.3526711511801));
#222757=CARTESIAN_POINT('Ctrl Pts',(7.91035376829573,0.10406150645942,69.3536812069608));
#222758=CARTESIAN_POINT('Ctrl Pts',(7.903898176097,0.500992636726142,69.3700895447515));
#222759=CARTESIAN_POINT('Ctrl Pts',(7.87155893965766,0.872413598769646,
69.3868710105261));
#222760=CARTESIAN_POINT('Ctrl Pts',(7.73899210649224,1.70762216107917,69.4259117223213));
#222761=CARTESIAN_POINT('Ctrl Pts',(7.62297811994877,2.1675356329989,69.4483032668793));
#222762=CARTESIAN_POINT('Ctrl Pts',(7.31544024044349,3.04587027786733,69.4906324823488));
#222763=CARTESIAN_POINT('Ctrl Pts',(7.12719550235307,3.46354837109602,69.5105457574904));
#222764=CARTESIAN_POINT('Ctrl Pts',(6.8858686679488,3.89488075553801,69.5306867679188));
#222765=CARTESIAN_POINT('Ctrl Pts',(6.86762098931882,3.92696643828317,69.5321828122469));
#222766=CARTESIAN_POINT('Ctrl Pts',(6.84309197543201,3.96940294309177,69.5341587725822));
#222767=CARTESIAN_POINT('Ctrl Pts',(6.83701063533985,3.97986847556331,69.5346458567571));
#222768=CARTESIAN_POINT('Ctrl Pts',(6.82697740350053,3.99704405438516,69.5354448874105));
#222769=CARTESIAN_POINT('Ctrl Pts',(6.82303959127708,4.0037622777726,69.5357573395872));
#222770=CARTESIAN_POINT('Ctrl Pts',(6.8153839180573,4.01677937499464,69.5363625726592));
#222771=CARTESIAN_POINT('Ctrl Pts',(6.81166722943277,4.02307892710757,69.5366553953119));
#222772=CARTESIAN_POINT('Ctrl Pts',(6.80305778786671,4.03762525289804,69.5373313801535));
#222773=CARTESIAN_POINT('Ctrl Pts',(6.79815876243496,4.04586831093772,69.5377143157143));
#222774=CARTESIAN_POINT('Ctrl Pts',(6.78239460038087,4.0722834822811,69.5389410439332));
#222775=CARTESIAN_POINT('Ctrl Pts',(6.77147145341944,4.09042096118371,69.539782741335));
#222776=CARTESIAN_POINT('Ctrl Pts',(6.67205524229193,4.25400828041303,69.5473691017637));
#222777=CARTESIAN_POINT('Ctrl Pts',(6.57895847681344,4.39661428572872,69.5539441114009));
#222778=CARTESIAN_POINT('Ctrl Pts',(6.10735555924581,5.07045444105337,69.5849770522167));
#222779=CARTESIAN_POINT('Ctrl Pts',(5.66876101765411,5.55647903212384,69.6070192854743));
#222780=CARTESIAN_POINT('Ctrl Pts',(4.97868738477628,6.15339729266858,69.6388855746637));
#222781=CARTESIAN_POINT('Ctrl Pts',(4.77362263612577,6.31380566900336,69.648104308806));
#222782=CARTESIAN_POINT('Ctrl Pts',(4.47839859854395,6.52212362037798,69.6615227950873));
#222783=CARTESIAN_POINT('Ctrl Pts',(4.3946512411819,6.57884411079101,69.6653450507036));
#222784=CARTESIAN_POINT('Ctrl Pts',(4.23434513926404,6.68298942724517,69.6727313189785));
#222785=CARTESIAN_POINT('Ctrl Pts',(4.15801849158751,6.7307434800034,69.6762770553784));
#222786=CARTESIAN_POINT('Ctrl Pts',(4.06763452276068,6.78516838491791,69.6804965061603));
#222787=CARTESIAN_POINT('Ctrl Pts',(4.05435000539511,6.79311465031172,69.6811171939526));
#222788=CARTESIAN_POINT('Ctrl Pts',(4.03399922461893,6.80520671059323,69.6820687465038));
#222789=CARTESIAN_POINT('Ctrl Pts',(4.02694966151494,6.80938062830892,69.6823984966464));
#222790=CARTESIAN_POINT('Ctrl Pts',(4.01410185384773,6.81696065179618,69.6829996873944));
#222791=CARTESIAN_POINT('Ctrl Pts',(4.00830572043572,6.82037033249869,69.6832709894562));
#222792=CARTESIAN_POINT('Ctrl Pts',(3.99665737169282,6.82720270803515,69.6838163748187));
#222793=CARTESIAN_POINT('Ctrl Pts',(3.99080509021004,6.83062527847498,69.6840904624925));
#222794=CARTESIAN_POINT('Ctrl Pts',(3.97418339086418,6.84031743883636,69.6848691403089));
#222795=CARTESIAN_POINT('Ctrl Pts',(3.96340357073975,6.84656909859529,69.6853743950252));
#222796=CARTESIAN_POINT('Ctrl Pts',(3.91778800794991,6.87287960113444,69.687513365312));
#222797=CARTESIAN_POINT('Ctrl Pts',(3.88281469160793,6.8926980855669,69.6891556397315));
#222798=CARTESIAN_POINT('Ctrl Pts',(3.81846529933082,6.92851807039484,69.6921800107935));
#222799=CARTESIAN_POINT('Ctrl Pts',(3.78913572325624,6.94460152450603,69.6935594785057));
#222800=CARTESIAN_POINT('Ctrl Pts',(3.75297540581836,6.96413347861145,69.6952608525216));
#222801=CARTESIAN_POINT('Ctrl Pts',(3.74624031964666,6.96775881985767,69.6955777710755));
#222802=CARTESIAN_POINT('Ctrl Pts',(3.41025500094192,7.14798398481803,69.7113885773152));
#222803=CARTESIAN_POINT('Ctrl Pts',(3.06891934335209,7.30104346016771,69.7274724741248));
#222804=CARTESIAN_POINT('Ctrl Pts',(2.1556924354718,7.63514874499331,69.7693158043987));
#222805=CARTESIAN_POINT('Ctrl Pts',(1.57175606567315,7.77638412284417,69.7947861802248));
#222806=CARTESIAN_POINT('Ctrl Pts',(0.622803894818848,7.89454100181482,
69.8344114306702));
#222807=CARTESIAN_POINT('Ctrl Pts',(0.265534713305808,7.9146171906137,69.8490851990332));
#222808=CARTESIAN_POINT('Ctrl Pts',(-0.138667298695609,7.90992307022863,
69.8654544432408));
#222809=CARTESIAN_POINT('Ctrl Pts',(-0.185462374825714,7.90896423916535,
69.8673455919368));
#222810=CARTESIAN_POINT('Ctrl Pts',(-0.256642227807109,7.90687368299679,
69.8702162927225));
#222811=CARTESIAN_POINT('Ctrl Pts',(-0.281034701086563,7.90604428102136,
69.8711989901411));
#222812=CARTESIAN_POINT('Ctrl Pts',(-0.323444047688881,7.90440574560732,
69.8729057215475));
#222813=CARTESIAN_POINT('Ctrl Pts',(-0.341462694661206,7.90364785863238,
69.8736302997199));
#222814=CARTESIAN_POINT('Ctrl Pts',(-0.379073405326805,7.90193704755114,
69.8751415586107));
#222815=CARTESIAN_POINT('Ctrl Pts',(-0.398664840305231,7.90097285767418,
69.8759281115913));
#222816=CARTESIAN_POINT('Ctrl Pts',(-0.452873237435632,7.89810285984614,
69.8781026630388));
#222817=CARTESIAN_POINT('Ctrl Pts',(-0.487481631477381,7.8960423394796,
69.8794889375054));
#222818=CARTESIAN_POINT('Ctrl Pts',(-0.626410018028492,7.88685392315334,
69.8850460762369));
#222819=CARTESIAN_POINT('Ctrl Pts',(-0.730598347615395,7.87788555069864,
69.889195835196));
#222820=CARTESIAN_POINT('Ctrl Pts',(-1.39482507476343,7.80741903953486,
69.9155627540954));
#222821=CARTESIAN_POINT('Ctrl Pts',(-1.94711386526339,7.68830796928129,
69.936954011173));
#222822=CARTESIAN_POINT('Ctrl Pts',(-2.65134425786079,7.45560737536659,
69.965587502651));
#222823=CARTESIAN_POINT('Ctrl Pts',(-2.81868809754911,7.39396395741821,
69.9725099945296));
#222824=CARTESIAN_POINT('Ctrl Pts',(-3.06242320530185,7.2947029671966,69.98288680094));
#222825=CARTESIAN_POINT('Ctrl Pts',(-3.14052183444556,7.2614220024738,69.986257760095));
#222826=CARTESIAN_POINT('Ctrl Pts',(-3.23510100330352,7.21930676186637,
69.9904080302097));
#222827=CARTESIAN_POINT('Ctrl Pts',(-3.25210634313778,7.21166228773418,
69.9911569773442));
#222828=CARTESIAN_POINT('Ctrl Pts',(-3.27931597899883,7.19931482495235,
69.9923597665165));
#222829=CARTESIAN_POINT('Ctrl Pts',(-3.28953748680595,7.19465012080496,
69.9928125999241));
#222830=CARTESIAN_POINT('Ctrl Pts',(-3.30899806132569,7.18571891971241,
69.9936766175625));
#222831=CARTESIAN_POINT('Ctrl Pts',(-3.31823890538068,7.18145633761492,
69.9940877038156));
#222832=CARTESIAN_POINT('Ctrl Pts',(-3.33931474275092,7.17168518969149,
69.9950271021966));
#222833=CARTESIAN_POINT('Ctrl Pts',(-3.35114436866679,7.16616514113917,
69.9955556910536));
#222834=CARTESIAN_POINT('Ctrl Pts',(-3.38733423748395,7.14916868540159,
69.9971767496466));
#222835=CARTESIAN_POINT('Ctrl Pts',(-3.41164951593606,7.13759719352427,
69.9982714285053));
#222836=CARTESIAN_POINT('Ctrl Pts',(-3.73852173339539,6.97998880130868,
70.0130594415364));
#222837=CARTESIAN_POINT('Ctrl Pts',(-4.03153001636447,6.81495005697474,
70.0271386478852));
#222838=CARTESIAN_POINT('Ctrl Pts',(-4.35192622129461,6.60657238437597,
70.0431916716659));
#222839=CARTESIAN_POINT('Ctrl Pts',(-4.39047968199022,6.58101425816762,
70.0451349881296));
#222840=CARTESIAN_POINT('Ctrl Pts',(-4.75731807393134,6.33316883693342,
70.0637333821983));
#222841=CARTESIAN_POINT('Ctrl Pts',(-5.06868790616475,6.08683170055626,
70.0803209690402));
#222842=CARTESIAN_POINT('Ctrl Pts',(-5.43342449658723,5.75080082891796,
70.1006879592206));
#222843=CARTESIAN_POINT('Ctrl Pts',(-5.50529118371559,5.68204023481666,
70.1047530957996));
#222844=CARTESIAN_POINT('Ctrl Pts',(-5.62844860799349,5.55967503615597,
70.1118155983288));
#222845=CARTESIAN_POINT('Ctrl Pts',(-5.68031712735868,5.50667029186173,
70.1148212252642));
#222846=CARTESIAN_POINT('Ctrl Pts',(-5.7540491384615,5.42917268713113,70.1191413959629));
#222847=CARTESIAN_POINT('Ctrl Pts',(-5.77651718671456,5.4052610258065,70.1204644269423));
#222848=CARTESIAN_POINT('Ctrl Pts',(-5.81551236097219,5.36323950898299,
70.1227724530622));
#222849=CARTESIAN_POINT('Ctrl Pts',(-5.83210524297471,5.34519134275688,
70.1237583386237));
#222850=CARTESIAN_POINT('Ctrl Pts',(-5.86412151426685,5.31004051084356,
70.1256681474333));
#222851=CARTESIAN_POINT('Ctrl Pts',(-5.87955464526416,5.29294705602304,
70.126592193162));
#222852=CARTESIAN_POINT('Ctrl Pts',(-5.91630085494447,5.25188858823575,
70.128800754827));
#222853=CARTESIAN_POINT('Ctrl Pts',(-5.93754329663954,5.22786085884446,
70.1300843438165));
#222854=CARTESIAN_POINT('Ctrl Pts',(-6.01507482827396,5.13908133473645,
70.1347952230515));
#222855=CARTESIAN_POINT('Ctrl Pts',(-6.07045584296581,5.07354394643626,
70.1382111182776));
#222856=CARTESIAN_POINT('Ctrl Pts',(-6.49114753581666,4.55894941591987,
70.1645903234642));
#222857=CARTESIAN_POINT('Ctrl Pts',(-6.80726010890783,4.0718907899914,70.1870590371129));
#222858=CARTESIAN_POINT('Ctrl Pts',(-7.27669376322296,3.13856880300413,
70.2263595207206));
#222859=CARTESIAN_POINT('Ctrl Pts',(-7.4488261141157,2.704784773958,70.2433794464231));
#222860=CARTESIAN_POINT('Ctrl Pts',(-7.63315808487446,2.08595100320572,
70.2676810524803));
#222861=CARTESIAN_POINT('Ctrl Pts',(-7.67862295448836,1.91181583995978,
70.2745321638661));
#222862=CARTESIAN_POINT('Ctrl Pts',(-7.7355394031686,1.65881205484539,70.2846578370269));
#222863=CARTESIAN_POINT('Ctrl Pts',(-7.75180071658034,1.58107952410888,
70.2877920762707));
#222864=CARTESIAN_POINT('Ctrl Pts',(-7.76952508051071,1.48949439331139,
70.2915240136778));
#222865=CARTESIAN_POINT('Ctrl Pts',(-7.772125583798,1.4758649772674,70.2920804049426));
#222866=CARTESIAN_POINT('Ctrl Pts',(-7.77605287287183,1.45498352902487,
70.2929344851342));
#222867=CARTESIAN_POINT('Ctrl Pts',(-7.77740540757182,1.44773632863859,
70.2932312079769));
#222868=CARTESIAN_POINT('Ctrl Pts',(-7.77974522226511,1.43510113992445,
70.2937490732413));
#222869=CARTESIAN_POINT('Ctrl Pts',(-7.78073704160769,1.42971399039587,
70.2939700421648));
#222870=CARTESIAN_POINT('Ctrl Pts',(-7.7827980377082,1.4184538552255,70.2944322734439));
#222871=CARTESIAN_POINT('Ctrl Pts',(-7.78386616337178,1.4125806828686,70.2946735762766));
#222872=CARTESIAN_POINT('Ctrl Pts',(-7.7867998884772,1.39634500000254,70.2953412154704));
#222873=CARTESIAN_POINT('Ctrl Pts',(-7.78865144518479,1.38597998767521,
70.295768102483));
#222874=CARTESIAN_POINT('Ctrl Pts',(-7.79581537742497,1.34540858094252,
70.2974417299759));
#222875=CARTESIAN_POINT('Ctrl Pts',(-7.80097272174366,1.31517535194466,
70.2986946986105));
#222876=CARTESIAN_POINT('Ctrl Pts',(-7.87588585811102,0.860071845863508,
70.3176523236553));
#222877=CARTESIAN_POINT('Ctrl Pts',(-7.91100437914619,0.430312242319449,
70.3370166920242));
#222878=CARTESIAN_POINT('Ctrl Pts',(-7.91099157029255,-0.828455852205915,
70.3947334112468));
#222879=CARTESIAN_POINT('Ctrl Pts',(-7.78086560444916,-1.65189306722651,
70.4331033463336));
#222880=CARTESIAN_POINT('Ctrl Pts',(-7.50795410839227,-2.49353042565992,
70.469423264854));
#222881=CARTESIAN_POINT('Ctrl Pts',(-7.49008065500436,-2.54671569306175,
70.471708634733));
#222882=CARTESIAN_POINT('Ctrl Pts',(-7.46672124334167,-2.61385140325897,
70.4745815199327));
#222883=CARTESIAN_POINT('Ctrl Pts',(-7.46175963141329,-2.62798182835505,
70.4751855194328));
#222884=CARTESIAN_POINT('Ctrl Pts',(-7.4538467285934,-2.65031430724814,
70.4761390629174));
#222885=CARTESIAN_POINT('Ctrl Pts',(-7.45092196702358,-2.65852568588199,
70.4764894442036));
#222886=CARTESIAN_POINT('Ctrl Pts',(-7.4454866211128,-2.6737062004203,70.4771367874842));
#222887=CARTESIAN_POINT('Ctrl Pts',(-7.44297981006352,-2.6806766717922,
70.4774338684247));
#222888=CARTESIAN_POINT('Ctrl Pts',(-7.43739822157482,-2.6961287218434,
70.4780920789659));
#222889=CARTESIAN_POINT('Ctrl Pts',(-7.43431871643164,-2.70460858798668,
70.4784530583023));
#222890=CARTESIAN_POINT('Ctrl Pts',(-7.42547048555206,-2.72884418543444,
70.4794840714559));
#222891=CARTESIAN_POINT('Ctrl Pts',(-7.41966611666459,-2.74458689817808,
70.4801529734319));
#222892=CARTESIAN_POINT('Ctrl Pts',(-7.38219876330018,-2.84521899854418,
70.4844236960742));
#222893=CARTESIAN_POINT('Ctrl Pts',(-7.34912896718946,-2.9295791169623,
70.4879804969658));
#222894=CARTESIAN_POINT('Ctrl Pts',(-7.24699587358815,-3.17749700386068,
70.4983740594362));
#222895=CARTESIAN_POINT('Ctrl Pts',(-7.17386722885993,-3.33932173581964,
70.5050798721963));
#222896=CARTESIAN_POINT('Ctrl Pts',(-6.94302632394983,-3.80748581263191,
70.5243649622279));
#222897=CARTESIAN_POINT('Ctrl Pts',(-6.77068147873238,-4.10614798780795,
70.5365040480709));
#222898=CARTESIAN_POINT('Ctrl Pts',(-6.20413711655041,-4.95473431817849,
70.5719205789795));
#222899=CARTESIAN_POINT('Ctrl Pts',(-5.7584184554071,-5.4663623039457,70.59443801509));
#222900=CARTESIAN_POINT('Ctrl Pts',(-5.22371792587205,-5.94123270220873,
70.622612218416));
#222901=CARTESIAN_POINT('Ctrl Pts',(-5.19404908804392,-5.96718768738708,
70.6241795543267));
#222902=CARTESIAN_POINT('Ctrl Pts',(-5.15638480129399,-5.99964356275094,
70.6261735230437));
#222903=CARTESIAN_POINT('Ctrl Pts',(-5.14856868111659,-6.00635227350239,
70.6265875319608));
#222904=CARTESIAN_POINT('Ctrl Pts',(-5.13619904930809,-6.01692745592559,
70.6272430482233));
#222905=CARTESIAN_POINT('Ctrl Pts',(-5.13165420381323,-6.02080408385659,
70.6274839645454));
#222906=CARTESIAN_POINT('Ctrl Pts',(-5.12360203253522,-6.02765662340119,
70.6279109109085));
#222907=CARTESIAN_POINT('Ctrl Pts',(-5.12009649012831,-6.03063463402343,
70.6280968208214));
#222908=CARTESIAN_POINT('Ctrl Pts',(-5.11204177255391,-6.03746515124704,
70.6285240691954));
#222909=CARTESIAN_POINT('Ctrl Pts',(-5.10749083980277,-6.04131557344143,
70.62876552497));
#222910=CARTESIAN_POINT('Ctrl Pts',(-5.09489270867644,-6.05195010461731,
70.6294340895036));
#222911=CARTESIAN_POINT('Ctrl Pts',(-5.08683633483922,-6.05872328818189,
70.6298618029537));
#222912=CARTESIAN_POINT('Ctrl Pts',(-5.0430409582497,-6.09539416640215,
70.6321877293022));
#222913=CARTESIAN_POINT('Ctrl Pts',(-5.00705231907065,-6.12499135530667,
70.6341020235493));
#222914=CARTESIAN_POINT('Ctrl Pts',(-4.43402532228738,-6.58782546603999,
70.6646011078195));
#222915=CARTESIAN_POINT('Ctrl Pts',(-3.84282802481101,-6.94930014431599,
70.6959645917874));
#222916=CARTESIAN_POINT('Ctrl Pts',(-2.84537196036472,-7.39249097282537,
70.7431489256086));
#222917=CARTESIAN_POINT('Ctrl Pts',(-2.46663670591237,-7.52733723690445,
70.7599971427778));
#222918=CARTESIAN_POINT('Ctrl Pts',(-2.04323877770246,-7.64267567665813,
70.7777709488822));
#222919=CARTESIAN_POINT('Ctrl Pts',(-2.00713039340839,-7.65223783046748,
70.7792789435391));
#222920=CARTESIAN_POINT('Ctrl Pts',(-1.95583392937872,-7.66543400165097,
70.7814106391181));
#222921=CARTESIAN_POINT('Ctrl Pts',(-1.94070089253754,-7.66927929082834,
70.7820382102926));
#222922=CARTESIAN_POINT('Ctrl Pts',(-1.9129428567909,-7.67624515967114,
70.7831870023427));
#222923=CARTESIAN_POINT('Ctrl Pts',(-1.9003213672853,-7.67937945584948,
70.7837084689452));
#222924=CARTESIAN_POINT('Ctrl Pts',(-1.87474213025496,-7.68566462800248,
70.7847635330229));
#222925=CARTESIAN_POINT('Ctrl Pts',(-1.86178402872431,-7.68881389166745,
70.7852971003599));
#222926=CARTESIAN_POINT('Ctrl Pts',(-1.82985556900204,-7.6964881565451,
70.7866095898017));
#222927=CARTESIAN_POINT('Ctrl Pts',(-1.81087629924963,-7.7009758069879,
70.7873878575732));
#222928=CARTESIAN_POINT('Ctrl Pts',(-1.74235803554529,-7.71690965259505,
70.7901908235108));
#222929=CARTESIAN_POINT('Ctrl Pts',(-1.69272511652909,-7.72794848989756,
70.7922087178548));
#222930=CARTESIAN_POINT('Ctrl Pts',(-1.42286918634173,-7.78524252255262,
70.803114679966));
#222931=CARTESIAN_POINT('Ctrl Pts',(-1.20085078209283,-7.82256483455634,
70.8118467231437));
#222932=CARTESIAN_POINT('Ctrl Pts',(-0.662017941131162,-7.88966090973433,
70.8325687972571));
#222933=CARTESIAN_POINT('Ctrl Pts',(-0.344412789612312,-7.90989289001028,
70.8443890479029));
#222934=CARTESIAN_POINT('Ctrl Pts',(0.494584770115002,-7.91269750895233,
70.875312482633));
#222935=CARTESIAN_POINT('Ctrl Pts',(1.01448141026288,-7.86296135942484,
70.8941239740843));
#222936=CARTESIAN_POINT('Ctrl Pts',(1.57414399919336,-7.75296277109719,
70.9163127209722));
#222937=CARTESIAN_POINT('Ctrl Pts',(1.62252282230501,-7.7429826708429,70.9182476458554));
#222938=CARTESIAN_POINT('Ctrl Pts',(1.71934670691455,-7.72206152957189,
70.9221584352453));
#222939=CARTESIAN_POINT('Ctrl Pts',(1.76778850440719,-7.71111606966892,
70.9241343755342));
#222940=CARTESIAN_POINT('Ctrl Pts',(1.82697858869865,-7.69715496970321,
70.9265752540666));
#222941=CARTESIAN_POINT('Ctrl Pts',(1.83782833432807,-7.6945716192099,70.9270237701683));
#222942=CARTESIAN_POINT('Ctrl Pts',(1.855741721388,-7.69026634930908,70.9277661413006));
#222943=CARTESIAN_POINT('Ctrl Pts',(1.8628085362989,-7.68855761612406,70.9280594827564));
#222944=CARTESIAN_POINT('Ctrl Pts',(1.87556537495691,-7.68545443322404,
70.9285898896411));
#222945=CARTESIAN_POINT('Ctrl Pts',(1.88125622955397,-7.68406339897233,
70.9288268197784));
#222946=CARTESIAN_POINT('Ctrl Pts',(1.89341841672263,-7.68107623481638,
70.9293338545063));
#222947=CARTESIAN_POINT('Ctrl Pts',(1.89988928485461,-7.67947824599973,
70.9296040334775));
#222948=CARTESIAN_POINT('Ctrl Pts',(1.91737625297983,-7.67513636283403,
70.9303352985852));
#222949=CARTESIAN_POINT('Ctrl Pts',(1.92838845318024,-7.67237693647971,
70.9307970162469));
#222950=CARTESIAN_POINT('Ctrl Pts',(1.98266504523857,-7.65865212471821,
70.9330788353388));
#222951=CARTESIAN_POINT('Ctrl Pts',(2.02584144979125,-7.64734459482731,
70.9349131849894));
#222952=CARTESIAN_POINT('Ctrl Pts',(2.57118063346461,-7.49958253244396,
70.9583467681856));
#222953=CARTESIAN_POINT('Ctrl Pts',(3.05870345832054,-7.31429129332358,
70.9823703445208));
#222954=CARTESIAN_POINT('Ctrl Pts',(3.97906444526342,-6.85630008518049,
71.0296999326365));
#222955=CARTESIAN_POINT('Ctrl Pts',(4.41091153929234,-6.58678714778771,
71.0528574581757));
#222956=CARTESIAN_POINT('Ctrl Pts',(4.96120297657999,-6.16480424524337,
71.0824408895058));
#222957=CARTESIAN_POINT('Ctrl Pts',(5.10442545407705,-6.04675065114256,
71.0901609842244));
#222958=CARTESIAN_POINT('Ctrl Pts',(5.25753396170436,-5.91122790774098,
71.0984362422111));
#222959=CARTESIAN_POINT('Ctrl Pts',(5.27165177157368,-5.89864105889531,
71.0991995240868));
#222960=CARTESIAN_POINT('Ctrl Pts',(5.29260030553449,-5.87982894404224,
71.100332485919));
#222961=CARTESIAN_POINT('Ctrl Pts',(5.29946542880635,-5.87364218990048,
71.1007038336044));
#222962=CARTESIAN_POINT('Ctrl Pts',(5.31122315147431,-5.86300889849365,
71.1013399384213));
#222963=CARTESIAN_POINT('Ctrl Pts',(5.31612103953301,-5.8585682382226,71.1016049511629));
#222964=CARTESIAN_POINT('Ctrl Pts',(5.32617418602407,-5.84943058581738,
71.102148969611));
#222965=CARTESIAN_POINT('Ctrl Pts',(5.33132881260921,-5.84473290496227,
71.1024279448225));
#222966=CARTESIAN_POINT('Ctrl Pts',(5.34323760036355,-5.83385094168014,
71.1030725507106));
#222967=CARTESIAN_POINT('Ctrl Pts',(5.34998725492793,-5.82766172976289,
71.1034379645731));
#222968=CARTESIAN_POINT('Ctrl Pts',(5.37116407182459,-5.80817548514979,
71.1045846484303));
#222969=CARTESIAN_POINT('Ctrl Pts',(5.38555257530667,-5.79483644451969,
71.1053640652281));
#222970=CARTESIAN_POINT('Ctrl Pts',(5.58839771817655,-5.60537828368679,
71.1163567572089));
#222971=CARTESIAN_POINT('Ctrl Pts',(5.7681882766061,-5.42019129965922,71.1261499494144));
#222972=CARTESIAN_POINT('Ctrl Pts',(6.27578539534948,-4.84343731462605,
71.1542603424725));
#222973=CARTESIAN_POINT('Ctrl Pts',(6.5750997769323,-4.42859570005681,71.1714013390723));
#222974=CARTESIAN_POINT('Ctrl Pts',(7.11471399516983,-3.50406826544196,
71.2073795007907));
#222975=CARTESIAN_POINT('Ctrl Pts',(7.34485239707152,-2.99176142641056,
71.2261554397885));
#222976=CARTESIAN_POINT('Ctrl Pts',(7.52990797772028,-2.42603571719051,
71.2496216496714));
#222977=CARTESIAN_POINT('Ctrl Pts',(7.54064256190323,-2.39246173051011,
71.2510243341122));
#222978=CARTESIAN_POINT('Ctrl Pts',(7.55335365062155,-2.35177042630304,
71.2527376812737));
#222979=CARTESIAN_POINT('Ctrl Pts',(7.55554517551398,-2.34472015589461,
71.2530350215957));
#222980=CARTESIAN_POINT('Ctrl Pts',(7.5591184472608,-2.33316769207849,71.253523042413));
#222981=CARTESIAN_POINT('Ctrl Pts',(7.56050605285211,-2.32866730205098,
71.2537133558606));
#222982=CARTESIAN_POINT('Ctrl Pts',(7.56298413646254,-2.32060462610301,
71.2540546735051));
#222983=CARTESIAN_POINT('Ctrl Pts',(7.56407611943898,-2.31704280027612,
71.2542055827151));
#222984=CARTESIAN_POINT('Ctrl Pts',(7.56638345373586,-2.30949773205644,
71.2545255257389));
#222985=CARTESIAN_POINT('Ctrl Pts',(7.56759817607682,-2.30551430024735,
71.2546945993788));
#222986=CARTESIAN_POINT('Ctrl Pts',(7.57084708041395,-2.29482995561991,
71.2551485190671));
#222987=CARTESIAN_POINT('Ctrl Pts',(7.57287550586153,-2.28812731555784,
71.2554337324246));
#222988=CARTESIAN_POINT('Ctrl Pts',(7.58269993320535,-2.25550774529017,
71.2568239491827));
#222989=CARTESIAN_POINT('Ctrl Pts',(7.59037171603507,-2.22955391105535,
71.257936756496));
#222990=CARTESIAN_POINT('Ctrl Pts',(7.65214872964639,-2.01654593088892,
71.2671210529241));
#222991=CARTESIAN_POINT('Ctrl Pts',(7.69946044412186,-1.8276038611942,71.2755900200433));
#222992=CARTESIAN_POINT('Ctrl Pts',(7.80535664015676,-1.32696352028802,
71.2984853038982));
#222993=CARTESIAN_POINT('Ctrl Pts',(7.85225665101399,-1.0131511786666,71.3132818361687));
#222994=CARTESIAN_POINT('Ctrl Pts',(7.91309322995383,-0.32572013567189,
71.345525892849));
#222995=CARTESIAN_POINT('Ctrl Pts',(7.91965158157489,0.0478278269703545,
71.3629266662739));
#222996=CARTESIAN_POINT('Ctrl Pts',(7.89154285788762,0.575949664985327,
71.3866453844034));
#222997=CARTESIAN_POINT('Ctrl Pts',(7.878677905796,0.73116667710807,71.3935125826961));
#222998=CARTESIAN_POINT('Ctrl Pts',(7.83605033322369,1.10942854801582,71.4099570442083));
#222999=CARTESIAN_POINT('Ctrl Pts',(7.80133853702477,1.33178280281065,71.4193721069612));
#223000=CARTESIAN_POINT('Ctrl Pts',(7.75306265166879,1.57301745356591,71.429314063165));
#223001=CARTESIAN_POINT('Ctrl Pts',(7.74884824351197,1.59364842376209,71.4301621640269));
#223002=CARTESIAN_POINT('Ctrl Pts',(7.74281716663155,1.62258299129979,71.4313486176197));
#223003=CARTESIAN_POINT('Ctrl Pts',(7.74106943101313,1.63090076472523,71.4316893379124));
#223004=CARTESIAN_POINT('Ctrl Pts',(7.73801466791903,1.64532336511804,71.4322795302557));
#223005=CARTESIAN_POINT('Ctrl Pts',(7.73671381390792,1.651429483412,71.4325292143487));
#223006=CARTESIAN_POINT('Ctrl Pts',(7.73399357829743,1.6641243212275,71.4330479302875));
#223007=CARTESIAN_POINT('Ctrl Pts',(7.7325730017871,1.67071278141943,71.4333169208035));
#223008=CARTESIAN_POINT('Ctrl Pts',(7.72921101956874,1.68620910140554,71.4339490903886));
#223009=CARTESIAN_POINT('Ctrl Pts',(7.72726262951738,1.69511544560198,71.4343120288363));
#223010=CARTESIAN_POINT('Ctrl Pts',(7.72313891453043,1.71381062530068,71.4350730457539));
#223011=CARTESIAN_POINT('Ctrl Pts',(7.72096036435933,1.72359873680813,71.4354710126182));
#223012=CARTESIAN_POINT('Ctrl Pts',(7.71503546507564,1.74998234756904,71.4365424556139));
#223013=CARTESIAN_POINT('Ctrl Pts',(7.71125417248284,1.76656999195839,71.4372147298258));
#223014=CARTESIAN_POINT('Ctrl Pts',(7.61095239261569,2.20011169342071,71.4547507322307));
#223015=CARTESIAN_POINT('Ctrl Pts',(7.48080403500993,2.60858433050395,71.4703688143833));
#223016=CARTESIAN_POINT('Ctrl Pts',(7.2114079641856,3.26475630405798,71.4951327822622));
#223017=CARTESIAN_POINT('Ctrl Pts',(7.09077726743393,3.51907938583672,71.504659573355));
#223018=CARTESIAN_POINT('Ctrl Pts',(6.75570443059019,4.13798078226517,71.5285775372291));
#223019=CARTESIAN_POINT('Ctrl Pts',(6.52512572917753,4.49278362904718,71.5429571990857));
#223020=CARTESIAN_POINT('Ctrl Pts',(6.19368462287517,4.92308485777645,71.5634174895336));
#223021=CARTESIAN_POINT('Ctrl Pts',(6.1178443584561,5.01701818022746,71.5680896686679));
#223022=CARTESIAN_POINT('Ctrl Pts',(6.03294769566524,5.11738005206377,71.5733563490854));
#223023=CARTESIAN_POINT('Ctrl Pts',(6.02599041812151,5.12557079506963,71.5737882182886));
#223024=CARTESIAN_POINT('Ctrl Pts',(6.0156242090462,5.13772456443133,71.5744321028692));
#223025=CARTESIAN_POINT('Ctrl Pts',(6.01222809808811,5.14169832066524,71.5746431112));
#223026=CARTESIAN_POINT('Ctrl Pts',(6.00639507990508,5.148509797536,71.5750056337904));
#223027=CARTESIAN_POINT('Ctrl Pts',(6.00396009025109,5.15134916558816,71.5751569994675));
#223028=CARTESIAN_POINT('Ctrl Pts',(5.99920946646611,5.15688078084582,71.5754523696088));
#223029=CARTESIAN_POINT('Ctrl Pts',(5.99689403089543,5.15957319867772,71.5755963587804));
#223030=CARTESIAN_POINT('Ctrl Pts',(5.99133684732384,5.16602636792826,71.5759420039353));
#223031=CARTESIAN_POINT('Ctrl Pts',(5.98809337312693,5.16978562483354,71.5761437921706));
#223032=CARTESIAN_POINT('Ctrl Pts',(5.9783078788401,5.18110566089641,71.5767527297861));
#223033=CARTESIAN_POINT('Ctrl Pts',(5.97175508422018,5.18865706863606,71.577160698198));
#223034=CARTESIAN_POINT('Ctrl Pts',(5.91266598286916,5.25649084540286,71.5808411160431));
#223035=CARTESIAN_POINT('Ctrl Pts',(5.85923448934556,5.31598395347245,71.5841805354665));
#223036=CARTESIAN_POINT('Ctrl Pts',(5.65045994989739,5.54147152182264,71.5972366174554));
#223037=CARTESIAN_POINT('Ctrl Pts',(5.48889821859864,5.70154252001349,71.6073546406233));
#223038=CARTESIAN_POINT('Ctrl Pts',(4.98105913775226,6.16308233597734,71.6386049207332));
#223039=CARTESIAN_POINT('Ctrl Pts',(4.61522563577888,6.4416017270678,71.6603496219915));
#223040=CARTESIAN_POINT('Ctrl Pts',(3.95188749017471,6.86095327751132,71.6965434586497));
#223041=CARTESIAN_POINT('Ctrl Pts',(3.66595629059359,7.01789761495503,71.7112583315734));
#223042=CARTESIAN_POINT('Ctrl Pts',(3.14614603478404,7.2627502210597,71.7361935944456));
#223043=CARTESIAN_POINT('Ctrl Pts',(2.91626804767273,7.35806844619734,71.746643509954));
#223044=CARTESIAN_POINT('Ctrl Pts',(2.66064294656456,7.45019653283647,71.7576581973014));
#223045=CARTESIAN_POINT('Ctrl Pts',(2.63898633870715,7.45789517107288,71.7585867680611));
#223046=CARTESIAN_POINT('Ctrl Pts',(2.60855142823489,7.46856521158115,71.7598853465347));
#223047=CARTESIAN_POINT('Ctrl Pts',(2.59980109090375,7.47161569955595,71.7602579628025));
#223048=CARTESIAN_POINT('Ctrl Pts',(2.58461730231572,7.47687907392358,71.7609032616196));
#223049=CARTESIAN_POINT('Ctrl Pts',(2.57818632750207,7.47909904644293,71.7611761772865));
#223050=CARTESIAN_POINT('Ctrl Pts',(2.56480975184804,7.48369733716626,71.761743028615));
#223051=CARTESIAN_POINT('Ctrl Pts',(2.55786368607432,7.48607428906018,71.7620369191849));
#223052=CARTESIAN_POINT('Ctrl Pts',(2.54151905395885,7.49164203710807,71.7627273917477));
#223053=CARTESIAN_POINT('Ctrl Pts',(2.53211776190156,7.49482482480951,71.7631237107888));
#223054=CARTESIAN_POINT('Ctrl Pts',(2.50144890816817,7.50514340880997,71.7644138746114));
#223055=CARTESIAN_POINT('Ctrl Pts',(2.48015689393075,7.51220646807339,71.7653053394764));
#223056=CARTESIAN_POINT('Ctrl Pts',(2.07088663585798,7.64604129939103,71.7823606298767));
#223057=CARTESIAN_POINT('Ctrl Pts',(1.67368805803971,7.74269540356035,71.7974868025735));
#223058=CARTESIAN_POINT('Ctrl Pts',(0.973651664704941,7.85662401868755,
71.8227571713165));
#223059=CARTESIAN_POINT('Ctrl Pts',(0.674011368291598,7.88798147197124,
71.8331581214453));
#223060=CARTESIAN_POINT('Ctrl Pts',(-0.157416664472316,7.9272594460788,
71.8620047659941));
#223061=CARTESIAN_POINT('Ctrl Pts',(-0.689337248274834,7.89880153920904,
71.8804813650044));
#223062=CARTESIAN_POINT('Ctrl Pts',(-1.25111560064042,7.81153072482053,
71.9029706469464));
#223063=CARTESIAN_POINT('Ctrl Pts',(-1.28780271249366,7.80556638738845,
71.9044509848803));
#223064=CARTESIAN_POINT('Ctrl Pts',(-1.33636181684843,7.79732032012387,
71.9064248480477));
#223065=CARTESIAN_POINT('Ctrl Pts',(-1.348272901174,7.79526954391305,71.9069101753331));
#223066=CARTESIAN_POINT('Ctrl Pts',(-1.36677328278422,7.79204059280609,
71.9076657492807));
#223067=CARTESIAN_POINT('Ctrl Pts',(-1.37336588997148,7.79088133258608,
71.907935345499));
#223068=CARTESIAN_POINT('Ctrl Pts',(-1.38657690877119,7.78854098496303,
71.9084762815399));
#223069=CARTESIAN_POINT('Ctrl Pts',(-1.39319530180666,7.78735982532539,
71.9087476236088));
#223070=CARTESIAN_POINT('Ctrl Pts',(-1.40798684636991,7.78470057392633,
71.909354815265));
#223071=CARTESIAN_POINT('Ctrl Pts',(-1.41615918704046,7.78321804536101,
71.9096908117686));
#223072=CARTESIAN_POINT('Ctrl Pts',(-1.44011781342516,7.77883277339254,
71.9106773530511));
#223073=CARTESIAN_POINT('Ctrl Pts',(-1.45589757405786,7.77589486058238,
71.9113290372067));
#223074=CARTESIAN_POINT('Ctrl Pts',(-1.57454820754044,7.75343037941236,
71.9162432057093));
#223075=CARTESIAN_POINT('Ctrl Pts',(-1.67702929151945,7.73191157069865,
71.920567030218));
#223076=CARTESIAN_POINT('Ctrl Pts',(-1.93194104340771,7.67307926361051,
71.9314843229525));
#223077=CARTESIAN_POINT('Ctrl Pts',(-2.08374502194059,7.63325267321287,
71.938131662078));
#223078=CARTESIAN_POINT('Ctrl Pts',(-2.42685656466533,7.53223714827264,
71.9533973911316));
#223079=CARTESIAN_POINT('Ctrl Pts',(-2.61722276979147,7.46822423516205,
71.9620407646658));
#223080=CARTESIAN_POINT('Ctrl Pts',(-2.94437925591308,7.34416700173195,
71.9770980241227));
#223081=CARTESIAN_POINT('Ctrl Pts',(-3.08229022865552,7.28736204004305,
71.9835111389092));
#223082=CARTESIAN_POINT('Ctrl Pts',(-3.9015094674697,6.9225107432412,72.0219308591963));
#223083=CARTESIAN_POINT('Ctrl Pts',(-4.53796070296965,6.52302937767378,
72.0528960236787));
#223084=CARTESIAN_POINT('Ctrl Pts',(-5.16558010832075,5.99218018713211,
72.086310519397));
#223085=CARTESIAN_POINT('Ctrl Pts',(-5.22162953362689,5.94340192047556,
72.0893208720212));
#223086=CARTESIAN_POINT('Ctrl Pts',(-5.29720552792464,5.87573581033753,
72.0934162959694));
#223087=CARTESIAN_POINT('Ctrl Pts',(-5.31733395891755,5.85752655083411,
72.0945106448856));
#223088=CARTESIAN_POINT('Ctrl Pts',(-5.35154991008816,5.82625125707545,
72.0963771141525));
#223089=CARTESIAN_POINT('Ctrl Pts',(-5.36568424990266,5.8132368507921,72.0971499672951));
#223090=CARTESIAN_POINT('Ctrl Pts',(-5.39425491760438,5.78673700283436,
72.0987159267158));
#223091=CARTESIAN_POINT('Ctrl Pts',(-5.40868842780447,5.77324871710554,
72.0995089843347));
#223092=CARTESIAN_POINT('Ctrl Pts',(-5.43382503352709,5.74958126025726,
72.10089358198));
#223093=CARTESIAN_POINT('Ctrl Pts',(-5.44455041556772,5.73942592396704,
72.1014854755283));
#223094=CARTESIAN_POINT('Ctrl Pts',(-5.47222447673021,5.71307533787036,
72.1030155931375));
#223095=CARTESIAN_POINT('Ctrl Pts',(-5.48912974322961,5.6968346655181,72.1039531179759));
#223096=CARTESIAN_POINT('Ctrl Pts',(-5.53122212288266,5.65603574099872,
72.1062946137568));
#223097=CARTESIAN_POINT('Ctrl Pts',(-5.55631812750907,5.63138414216991,
72.1076971126576));
#223098=CARTESIAN_POINT('Ctrl Pts',(-5.62655310562677,5.56146631645238,
72.1116408926125));
#223099=CARTESIAN_POINT('Ctrl Pts',(-5.67130918682736,5.51581903562978,
72.1141760187627));
#223100=CARTESIAN_POINT('Ctrl Pts',(-5.81726065000472,5.36330670187768,
72.1225198004269));
#223101=CARTESIAN_POINT('Ctrl Pts',(-5.91602808554049,5.25415957983556,
72.1282901708205));
#223102=CARTESIAN_POINT('Ctrl Pts',(-6.44153883999227,4.63980453477771,
72.1597869003572));
#223103=CARTESIAN_POINT('Ctrl Pts',(-6.80665855149192,4.08540427680142,
72.1844683217585));
#223104=CARTESIAN_POINT('Ctrl Pts',(-7.11640740702316,3.45576416596647,
72.2124003032842));
#223105=CARTESIAN_POINT('Ctrl Pts',(-7.13400084120414,3.41929704852806,
72.2140185152756));
#223106=CARTESIAN_POINT('Ctrl Pts',(-7.15707583306152,3.37051452030001,
72.2161852263665));
#223107=CARTESIAN_POINT('Ctrl Pts',(-7.16280706343204,3.358317671269,72.2167271340219));
#223108=CARTESIAN_POINT('Ctrl Pts',(-7.17255477876143,3.3374347221852,72.2176552548076));
#223109=CARTESIAN_POINT('Ctrl Pts',(-7.17658671916797,3.32875586981402,
72.2180410598546));
#223110=CARTESIAN_POINT('Ctrl Pts',(-7.18440603692826,3.31184435283327,
72.218792979462));
#223111=CARTESIAN_POINT('Ctrl Pts',(-7.18819503677124,3.30361245209955,
72.2191590524219));
#223112=CARTESIAN_POINT('Ctrl Pts',(-7.19602549777607,3.286522908259,72.2199191478036));
#223113=CARTESIAN_POINT('Ctrl Pts',(-7.20006476785826,3.27766427951054,
72.2203132231805));
#223114=CARTESIAN_POINT('Ctrl Pts',(-7.20922715744471,3.25747133606334,
72.2212116398839));
#223115=CARTESIAN_POINT('Ctrl Pts',(-7.21433991602449,3.24613235831654,
72.2217162261814));
#223116=CARTESIAN_POINT('Ctrl Pts',(-7.22732903215772,3.21714308514874,
72.2230064543193));
#223117=CARTESIAN_POINT('Ctrl Pts',(-7.23516747304474,3.19947592612922,
72.2237929578117));
#223118=CARTESIAN_POINT('Ctrl Pts',(-7.32395778147548,2.99735544136753,
72.2327923230002));
#223119=CARTESIAN_POINT('Ctrl Pts',(-7.39789943580156,2.80990708683299,
72.2411502310389));
#223120=CARTESIAN_POINT('Ctrl Pts',(-7.67523641657879,2.01970372487532,
72.2761574661352));
#223121=CARTESIAN_POINT('Ctrl Pts',(-7.81273495777942,1.39631261206159,
72.3030619631906));
#223122=CARTESIAN_POINT('Ctrl Pts',(-7.88418812074589,0.659116211714981,
72.3333280215586));
#223123=CARTESIAN_POINT('Ctrl Pts',(-7.89221192187817,0.55484038951926,
72.3375789131369));
#223124=CARTESIAN_POINT('Ctrl Pts',(-7.90033749776537,0.412362324693237,
72.3433504849001));
#223125=CARTESIAN_POINT('Ctrl Pts',(-7.90223349597277,0.37427404171455,
72.3448898318507));
#223126=CARTESIAN_POINT('Ctrl Pts',(-7.90481343563123,0.31361646145783,
72.347336013787));
#223127=CARTESIAN_POINT('Ctrl Pts',(-7.90567628115004,0.291055455714753,
72.3482446799303));
#223128=CARTESIAN_POINT('Ctrl Pts',(-7.90721753802288,0.245668989415847,
72.3500704149669));
#223129=CARTESIAN_POINT('Ctrl Pts',(-7.90789372403584,0.222843664899516,
72.3509874527183));
#223130=CARTESIAN_POINT('Ctrl Pts',(-7.90905917344906,0.176762665795935,
72.3528366219436));
#223131=CARTESIAN_POINT('Ctrl Pts',(-7.90954471620337,0.153507118007278,
72.3537687074326));
#223132=CARTESIAN_POINT('Ctrl Pts',(-7.91064206092113,0.0868665379281315,
72.3564366156031));
#223133=CARTESIAN_POINT('Ctrl Pts',(-7.91099951148764,0.0434781555137821,
72.3581699259418));
#223134=CARTESIAN_POINT('Ctrl Pts',(-7.91099999949962,8.89775508417708E-5,
72.3598999971));
#223135=CARTESIAN_POINT('',(-7.911,-5.26911847487099E-12,74.3576684917632));
#223136=CARTESIAN_POINT('Ctrl Pts',(-7.911,-5.21527265817667E-12,72.3576684917632));
#223137=CARTESIAN_POINT('Ctrl Pts',(-7.91099999999855,-2.20167589667201,
72.446255927496));
#223138=CARTESIAN_POINT('Ctrl Pts',(-6.94214576672079,-4.38610418339146,
72.5348433632287));
#223139=CARTESIAN_POINT('Ctrl Pts',(-3.67820201487792,-7.34180684107881,
72.7120182346941));
#223140=CARTESIAN_POINT('Ctrl Pts',(-1.40868175871195,-8.08992666571433,
72.8006056704269));
#223141=CARTESIAN_POINT('Ctrl Pts',(2.97309270521799,-7.65454228025054,
72.9777805418923));
#223142=CARTESIAN_POINT('Ctrl Pts',(5.05102072676049,-6.47444880833878,
73.066367977625));
#223143=CARTESIAN_POINT('Ctrl Pts',(7.66951518848077,-2.93425195367174,
73.2435428490905));
#223144=CARTESIAN_POINT('Ctrl Pts',(8.18956872247114,-0.601881960093438,
73.3321302848232));
#223145=CARTESIAN_POINT('Ctrl Pts',(7.32306689761081,3.71537198232967,73.5093051562887));
#223146=CARTESIAN_POINT('Ctrl Pts',(5.943299588498,5.66643518936933,73.5978925920214));
#223147=CARTESIAN_POINT('Ctrl Pts',(2.1615450163728,7.92205913233153,73.7750674634868));
#223148=CARTESIAN_POINT('Ctrl Pts',(-0.210816529306286,8.20894963712988,
73.8636548992196));
#223149=CARTESIAN_POINT('Ctrl Pts',(-4.42123908576941,6.9198224471751,74.040829770685));
#223150=CARTESIAN_POINT('Ctrl Pts',(-6.2263162563458,5.35390358803066,74.1294172064178));
#223151=CARTESIAN_POINT('Ctrl Pts',(-7.65317280859651,2.31334857513973,
74.2645592586881));
#223152=CARTESIAN_POINT('Ctrl Pts',(-7.91100000000077,1.15702837835974,
74.3111138752257));
#223153=CARTESIAN_POINT('Ctrl Pts',(-7.911,-5.26911847487099E-12,74.3576684917632));
#223154=CARTESIAN_POINT('',(-7.911,-4.92828000631107E-12,78.3576684917632));
#223155=CARTESIAN_POINT('Ctrl Pts',(-7.91099999987772,4.39868550092259E-5,
74.3589457483061));
#223156=CARTESIAN_POINT('Ctrl Pts',(-7.91100255781545,-0.459999029859075,
74.37478896162));
#223157=CARTESIAN_POINT('Ctrl Pts',(-7.87087669527066,-0.919148178927294,
74.3902122431434));
#223158=CARTESIAN_POINT('Ctrl Pts',(-7.75556910623801,-1.57384771154762,
74.4143390289438));
#223159=CARTESIAN_POINT('Ctrl Pts',(-7.71223846080161,-1.77403948953629,
74.422021749972));
#223160=CARTESIAN_POINT('Ctrl Pts',(-7.65405480674869,-2.00004655857829,
74.4312663779502));
#223161=CARTESIAN_POINT('Ctrl Pts',(-7.64676414644965,-2.02774240737943,
74.4324091659388));
#223162=CARTESIAN_POINT('Ctrl Pts',(-7.63738158098275,-2.06261470997046,
74.4338612661042));
#223163=CARTESIAN_POINT('Ctrl Pts',(-7.63542959584612,-2.06982891599108,
74.4341623830335));
#223164=CARTESIAN_POINT('Ctrl Pts',(-7.63230658350073,-2.08130650391784,
74.434642602861));
#223165=CARTESIAN_POINT('Ctrl Pts',(-7.63114219597235,-2.08557170399325,
74.4348213112727));
#223166=CARTESIAN_POINT('Ctrl Pts',(-7.62893900387383,-2.09361554074054,
74.435158823249));
#223167=CARTESIAN_POINT('Ctrl Pts',(-7.62790096985216,-2.09739437188012,
74.4353175805888));
#223168=CARTESIAN_POINT('Ctrl Pts',(-7.62554061076717,-2.10596203074823,
74.4356779824742));
#223169=CARTESIAN_POINT('Ctrl Pts',(-7.62421658422282,-2.1107503779696,
74.4358797283332));
#223170=CARTESIAN_POINT('Ctrl Pts',(-7.62079555479545,-2.12307732786204,
74.4363999193981));
#223171=CARTESIAN_POINT('Ctrl Pts',(-7.61869188086996,-2.13061405504613,
74.4367187592679));
#223172=CARTESIAN_POINT('Ctrl Pts',(-7.60630760249972,-2.17472972287422,
74.4385896606587));
#223173=CARTESIAN_POINT('Ctrl Pts',(-7.59577491134693,-2.21123678406558,
74.440156402358));
#223174=CARTESIAN_POINT('Ctrl Pts',(-7.40284776344447,-2.86228927489958,
74.4684098051805));
#223175=CARTESIAN_POINT('Ctrl Pts',(-7.14669633365192,-3.45246665168654,
74.4988232229369));
#223176=CARTESIAN_POINT('Ctrl Pts',(-6.77221950229717,-4.0903175426112,
74.5328593659256));
#223177=CARTESIAN_POINT('Ctrl Pts',(-6.72068200122676,-4.17445666937669,
74.5373797254462));
#223178=CARTESIAN_POINT('Ctrl Pts',(-6.61604537604343,-4.3383216824764,
74.5462276282956));
#223179=CARTESIAN_POINT('Ctrl Pts',(-6.56304510840782,-4.41809132188313,
74.5505562222393));
#223180=CARTESIAN_POINT('Ctrl Pts',(-6.3492767697925,-4.72749125692134,
74.5674067966865));
#223181=CARTESIAN_POINT('Ctrl Pts',(-6.17779273714898,-4.94948342987304,
74.5796228457744));
#223182=CARTESIAN_POINT('Ctrl Pts',(-5.911662629768,-5.25855769531768,74.5967279283866));
#223183=CARTESIAN_POINT('Ctrl Pts',(-5.82612465619924,-5.35317266712475,
74.6019804187158));
#223184=CARTESIAN_POINT('Ctrl Pts',(-5.72900440892965,-5.45551218153069,
74.607683425037));
#223185=CARTESIAN_POINT('Ctrl Pts',(-5.71964976374926,-5.46531895343892,
74.6082301523073));
#223186=CARTESIAN_POINT('Ctrl Pts',(-5.70213029593801,-5.48359092285748,
74.6092492619851));
#223187=CARTESIAN_POINT('Ctrl Pts',(-5.69397171556912,-5.49206203761088,
74.6097219150718));
#223188=CARTESIAN_POINT('Ctrl Pts',(-5.6805051471627,-5.50598221379641,
74.6104989106774));
#223189=CARTESIAN_POINT('Ctrl Pts',(-5.6752081502598,-5.51144185465401,
74.6108037348877));
#223190=CARTESIAN_POINT('Ctrl Pts',(-5.66490037473644,-5.52203551328437,
74.611395358321));
#223191=CARTESIAN_POINT('Ctrl Pts',(-5.65989047218949,-5.52717037088918,
74.6116821955945));
#223192=CARTESIAN_POINT('Ctrl Pts',(-5.64826694583571,-5.5390514313789,
74.6123460494215));
#223193=CARTESIAN_POINT('Ctrl Pts',(-5.64164820239469,-5.54579262252948,
74.6127228393201));
#223194=CARTESIAN_POINT('Ctrl Pts',(-5.62025410432703,-5.56750457891165,
74.6139368180659));
#223195=CARTESIAN_POINT('Ctrl Pts',(-5.60543105633025,-5.58242833495877,
74.6147718916182));
#223196=CARTESIAN_POINT('Ctrl Pts',(-5.46659889325157,-5.72109321662509,
74.622537401475));
#223197=CARTESIAN_POINT('Ctrl Pts',(-5.33856726614387,-5.84074612380135,
74.6292841902116));
#223198=CARTESIAN_POINT('Ctrl Pts',(-4.91547034767126,-6.2106089416447,
74.6503990477461));
#223199=CARTESIAN_POINT('Ctrl Pts',(-4.60599155065285,-6.44347577305572,
74.664073811501));
#223200=CARTESIAN_POINT('Ctrl Pts',(-4.08188854207762,-6.78070807296753,
74.6856549478911));
#223201=CARTESIAN_POINT('Ctrl Pts',(-3.87743546093855,-6.89966012133398,
74.6937350477193));
#223202=CARTESIAN_POINT('Ctrl Pts',(-3.43081695122265,-7.13337612355974,
74.7111755778941));
#223203=CARTESIAN_POINT('Ctrl Pts',(-3.18753496248547,-7.24535496022746,
74.720552883012));
#223204=CARTESIAN_POINT('Ctrl Pts',(-2.78789572095369,-7.40527295776753,
74.7364073513357));
#223205=CARTESIAN_POINT('Ctrl Pts',(-2.63490896036442,-7.46107763215647,
74.7425794297122));
#223206=CARTESIAN_POINT('Ctrl Pts',(-2.44992900290924,-7.5221534847238,
74.7502804100549));
#223207=CARTESIAN_POINT('Ctrl Pts',(-2.41947978599846,-7.53200256763053,
74.7515556753191));
#223208=CARTESIAN_POINT('Ctrl Pts',(-2.38150194279796,-7.54403280071772,
74.7531566545599));
#223209=CARTESIAN_POINT('Ctrl Pts',(-2.37402833663229,-7.54638800080179,
74.7534722093428));
#223210=CARTESIAN_POINT('Ctrl Pts',(-2.36216191967191,-7.55010815981622,
74.7539740495719));
#223211=CARTESIAN_POINT('Ctrl Pts',(-2.35777141050801,-7.55148039362454,
74.7541599027669));
#223212=CARTESIAN_POINT('Ctrl Pts',(-2.3494894962841,-7.55406094163649,
74.7545108083172));
#223213=CARTESIAN_POINT('Ctrl Pts',(-2.34559834772306,-7.55527008082113,
74.7546758125245));
#223214=CARTESIAN_POINT('Ctrl Pts',(-2.3368372213771,-7.55798510088525,
74.7550476310431));
#223215=CARTESIAN_POINT('Ctrl Pts',(-2.33196672249307,-7.55948928099117,
74.7552545434696));
#223216=CARTESIAN_POINT('Ctrl Pts',(-2.31955290473075,-7.56330996258342,
74.7557824470207));
#223217=CARTESIAN_POINT('Ctrl Pts',(-2.31200758376753,-7.56561988205167,
74.7561038135544));
#223218=CARTESIAN_POINT('Ctrl Pts',(-2.26993121056785,-7.57843229148842,
74.7578986330891));
#223219=CARTESIAN_POINT('Ctrl Pts',(-2.23533252576648,-7.58870951617319,
74.7593847002442));
#223220=CARTESIAN_POINT('Ctrl Pts',(-1.62050637068699,-7.76676862332133,
74.7859576510475));
#223221=CARTESIAN_POINT('Ctrl Pts',(-1.02304451363722,-7.86778569835948,
74.814236618596));
#223222=CARTESIAN_POINT('Ctrl Pts',(-0.0659459552973449,-7.91866435171381,
74.8580827739364));
#223223=CARTESIAN_POINT('Ctrl Pts',(0.288942814869212,-7.91366777144239,
74.8740599113042));
#223224=CARTESIAN_POINT('Ctrl Pts',(0.894844434015389,-7.86430962641148,
74.9003569623192));
#223225=CARTESIAN_POINT('Ctrl Pts',(1.1462463730478,-7.83161841484737,74.9109813593004));
#223226=CARTESIAN_POINT('Ctrl Pts',(1.4156646610637,-7.78333010412937,74.9220525573507));
#223227=CARTESIAN_POINT('Ctrl Pts',(1.43565311544551,-7.77966799307198,
74.9228721011929));
#223228=CARTESIAN_POINT('Ctrl Pts',(1.46515615226902,-7.77414512532751,
74.924079063536));
#223229=CARTESIAN_POINT('Ctrl Pts',(1.47468170510054,-7.77234384530687,
74.924468337338));
#223230=CARTESIAN_POINT('Ctrl Pts',(1.49143149282617,-7.76914456329789,
74.9251521144648));
#223231=CARTESIAN_POINT('Ctrl Pts',(1.49865712356671,-7.76775398487626,
74.925446849356));
#223232=CARTESIAN_POINT('Ctrl Pts',(1.51271076223718,-7.76502901165071,
74.9260196408041));
#223233=CARTESIAN_POINT('Ctrl Pts',(1.51953896971166,-7.76369568709483,
74.9262977305323));
#223234=CARTESIAN_POINT('Ctrl Pts',(1.53777219721394,-7.76011036100972,
74.9270397471734));
#223235=CARTESIAN_POINT('Ctrl Pts',(1.54917404631814,-7.75784222069808,
74.9275031686034));
#223236=CARTESIAN_POINT('Ctrl Pts',(1.59017377593742,-7.74959225866892,
74.9291674878776));
#223237=CARTESIAN_POINT('Ctrl Pts',(1.61974251569416,-7.74346608574651,
74.9303638605007));
#223238=CARTESIAN_POINT('Ctrl Pts',(2.09173180150072,-7.64285560803748,
74.9493998775935));
#223239=CARTESIAN_POINT('Ctrl Pts',(2.52529576691775,-7.51076034656274,
74.9659577279597));
#223240=CARTESIAN_POINT('Ctrl Pts',(3.22649636901077,-7.22948705169856,
74.9925398244361));
#223241=CARTESIAN_POINT('Ctrl Pts',(3.50105071584739,-7.10059206025086,
75.0029127712537));
#223242=CARTESIAN_POINT('Ctrl Pts',(4.03248942627739,-6.81276339169449,
75.0238089169988));
#223243=CARTESIAN_POINT('Ctrl Pts',(4.28902032581565,-6.65424709862905,
75.0343167711192));
#223244=CARTESIAN_POINT('Ctrl Pts',(4.67717872089305,-6.3826065876698,75.0517723991173));
#223245=CARTESIAN_POINT('Ctrl Pts',(4.81520633394387,-6.27912805811054,
75.0583185506745));
#223246=CARTESIAN_POINT('Ctrl Pts',(4.97021192529077,-6.15480328849698,
75.0662010274249));
#223247=CARTESIAN_POINT('Ctrl Pts',(4.9906075725137,-6.13827713045954,75.0672491692675));
#223248=CARTESIAN_POINT('Ctrl Pts',(5.01663804408551,-6.11696970166405,
75.0686015168016));
#223249=CARTESIAN_POINT('Ctrl Pts',(5.02234913894389,-6.1122814662213,75.0688991305419));
#223250=CARTESIAN_POINT('Ctrl Pts',(5.03151651934753,-6.10473444419738,
75.069378332311));
#223251=CARTESIAN_POINT('Ctrl Pts',(5.03497696746959,-6.10188069823834,
75.0695595573356));
#223252=CARTESIAN_POINT('Ctrl Pts',(5.04154624502855,-6.09645378439796,
75.0699042409071));
#223253=CARTESIAN_POINT('Ctrl Pts',(5.04465553739504,-6.09388117663758,
75.0700676587275));
#223254=CARTESIAN_POINT('Ctrl Pts',(5.05171530255322,-6.08803086815133,
75.070439336512));
#223255=CARTESIAN_POINT('Ctrl Pts',(5.05566455297499,-6.08475170217899,
75.0706477039822));
#223256=CARTESIAN_POINT('Ctrl Pts',(5.06773675797528,-6.07470796778211,
75.0712860359159));
#223257=CARTESIAN_POINT('Ctrl Pts',(5.07584927910152,-6.06793101757252,
75.0717169236208));
#223258=CARTESIAN_POINT('Ctrl Pts',(5.13758427735328,-6.01614906913351,
75.075010472847));
#223259=CARTESIAN_POINT('Ctrl Pts',(5.19061938504279,-5.97045154659893,
75.0779237779166));
#223260=CARTESIAN_POINT('Ctrl Pts',(5.59905548075049,-5.60896846508895,
75.1009689887324));
#223261=CARTESIAN_POINT('Ctrl Pts',(5.92592111326226,-5.26244732300141,
75.1230039316853));
#223262=CARTESIAN_POINT('Ctrl Pts',(6.39763600440487,-4.66230657695339,
75.1582869219465));
#223263=CARTESIAN_POINT('Ctrl Pts',(6.56310353028825,-4.42634526081582,
75.1715615034023));
#223264=CARTESIAN_POINT('Ctrl Pts',(6.87847552078114,-3.91991507693336,
75.1983872471724));
#223265=CARTESIAN_POINT('Ctrl Pts',(7.0261515530736,-3.6486136016874,75.2118644934768));
#223266=CARTESIAN_POINT('Ctrl Pts',(7.20953427929696,-3.25904899450842,
75.2298744374987));
#223267=CARTESIAN_POINT('Ctrl Pts',(7.25890441416499,-3.14755355400882,
75.2348852948041));
#223268=CARTESIAN_POINT('Ctrl Pts',(7.31224406567963,-3.01915559934486,
75.2404964122261));
#223269=CARTESIAN_POINT('Ctrl Pts',(7.31875748479892,-3.00333193182822,
75.2411852039126));
#223270=CARTESIAN_POINT('Ctrl Pts',(7.32851703815783,-2.97940183055967,
75.242222783988));
#223271=CARTESIAN_POINT('Ctrl Pts',(7.33180115527293,-2.97131100134406,
75.242572890325));
#223272=CARTESIAN_POINT('Ctrl Pts',(7.33743021191441,-2.95737696727229,
75.2431746397299));
#223273=CARTESIAN_POINT('Ctrl Pts',(7.33978158023324,-2.95153637889914,
75.2434265054638));
#223274=CARTESIAN_POINT('Ctrl Pts',(7.34461312728542,-2.93949377046904,
75.2439450760217));
#223275=CARTESIAN_POINT('Ctrl Pts',(7.3470924292694,-2.93329140253549,75.2442117503577));
#223276=CARTESIAN_POINT('Ctrl Pts',(7.35375179750237,-2.91657052244639,
75.2449295786337));
#223277=CARTESIAN_POINT('Ctrl Pts',(7.35791715731509,-2.90604614883611,
75.2453802237446));
#223278=CARTESIAN_POINT('Ctrl Pts',(7.3731352263746,-2.86735305974536,75.2470327671426));
#223279=CARTESIAN_POINT('Ctrl Pts',(7.38404894492617,-2.83912976822201,
75.2482298670331));
#223280=CARTESIAN_POINT('Ctrl Pts',(7.55501982078598,-2.38933768778958,
75.2671782273451));
#223281=CARTESIAN_POINT('Ctrl Pts',(7.67891604551075,-1.95488237722311,
75.2836011282009));
#223282=CARTESIAN_POINT('Ctrl Pts',(7.8691786430854,-0.977889573176178,
75.3183638326138));
#223283=CARTESIAN_POINT('Ctrl Pts',(7.91780052232114,-0.434299729356681,
75.3362857174874));
#223284=CARTESIAN_POINT('Ctrl Pts',(7.90695354038161,0.346105018583208,
75.3642587005676));
#223285=CARTESIAN_POINT('Ctrl Pts',(7.89309717197793,0.58198291796844,75.3730263858001));
#223286=CARTESIAN_POINT('Ctrl Pts',(7.86558100841814,0.84703983716694,75.3835743083525));
#223287=CARTESIAN_POINT('Ctrl Pts',(7.8622754531318,0.877191961548501,75.3847844476465));
#223288=CARTESIAN_POINT('Ctrl Pts',(7.85793372159408,0.914797918671408,
75.3863073499697));
#223289=CARTESIAN_POINT('Ctrl Pts',(7.85706016727825,0.922270639228235,
75.3866106388035));
#223290=CARTESIAN_POINT('Ctrl Pts',(7.85566133366451,0.934090565715141,
75.3870914419696));
#223291=CARTESIAN_POINT('Ctrl Pts',(7.85514310086212,0.938438617607111,
75.3872685400263));
#223292=CARTESIAN_POINT('Ctrl Pts',(7.85416544655165,0.946583734814029,
75.3876007305111));
#223293=CARTESIAN_POINT('Ctrl Pts',(7.85370688063013,0.950380903565148,
75.3877557719475));
#223294=CARTESIAN_POINT('Ctrl Pts',(7.85267688791865,0.958858135240187,
75.3881023038262));
#223295=CARTESIAN_POINT('Ctrl Pts',(7.85210403098808,0.963538019969806,
75.3882938800158));
#223296=CARTESIAN_POINT('Ctrl Pts',(7.85064008321831,0.975409553846123,
75.3887805508474));
#223297=CARTESIAN_POINT('Ctrl Pts',(7.84974329562271,0.982600481423201,
75.3890759899834));
#223298=CARTESIAN_POINT('Ctrl Pts',(7.84467859607688,1.02276252953264,75.3907296305616));
#223299=CARTESIAN_POINT('Ctrl Pts',(7.84031289116645,1.05570790017319,75.3920996244686));
#223300=CARTESIAN_POINT('Ctrl Pts',(7.76585879186209,1.5916163440472,75.4145931992722));
#223301=CARTESIAN_POINT('Ctrl Pts',(7.64771406160099,2.08666720844628,75.4383037912463));
#223302=CARTESIAN_POINT('Ctrl Pts',(7.33381503755783,3.00172930986357,75.4836730363999));
#223303=CARTESIAN_POINT('Ctrl Pts',(7.14703653488529,3.42274068644863,75.505218539365));
#223304=CARTESIAN_POINT('Ctrl Pts',(6.80754038572666,4.03733386179259,75.5364445360822));
#223305=CARTESIAN_POINT('Ctrl Pts',(6.68064724138917,4.24401195603253,75.5469167386318));
#223306=CARTESIAN_POINT('Ctrl Pts',(6.48440906132903,4.53296624502326,75.5614847608781));
#223307=CARTESIAN_POINT('Ctrl Pts',(6.42257605008965,4.62015822003535,75.5658714605769));
#223308=CARTESIAN_POINT('Ctrl Pts',(6.34925266620873,4.71923507611359,75.5708484396384));
#223309=CARTESIAN_POINT('Ctrl Pts',(6.33947099281746,4.73236691927049,75.5715079454101));
#223310=CARTESIAN_POINT('Ctrl Pts',(6.32458222021835,4.75222601247567,75.572505097304));
#223311=CARTESIAN_POINT('Ctrl Pts',(6.31950503337093,4.75897556914844,75.5728439649213));
#223312=CARTESIAN_POINT('Ctrl Pts',(6.31069985741217,4.77064213540199,75.5734296357372));
#223313=CARTESIAN_POINT('Ctrl Pts',(6.30697691176529,4.77556293112161,75.5736766451168));
#223314=CARTESIAN_POINT('Ctrl Pts',(6.29924643047442,4.7857558717302,75.574188264207));
#223315=CARTESIAN_POINT('Ctrl Pts',(6.29523802341134,4.79102735167879,75.5744528378765));
#223316=CARTESIAN_POINT('Ctrl Pts',(6.28430418546764,4.80536909460649,75.5751725928584));
#223317=CARTESIAN_POINT('Ctrl Pts',(6.27736572742716,4.81442943207951,75.575627238457));
#223318=CARTESIAN_POINT('Ctrl Pts',(6.25113068697281,4.84853438906449,75.5773384269291));
#223319=CARTESIAN_POINT('Ctrl Pts',(6.23170350806327,4.87347842981928,75.5785895844747));
#223320=CARTESIAN_POINT('Ctrl Pts',(5.91404250680955,5.27634234293237,75.5987927249157));
#223321=CARTESIAN_POINT('Ctrl Pts',(5.58205684864035,5.62640150080307,75.6162025471674));
#223322=CARTESIAN_POINT('Ctrl Pts',(4.81354129420974,6.30133103701195,75.6517718893306));
#223323=CARTESIAN_POINT('Ctrl Pts',(4.37124324603791,6.61582356277707,75.6696674322865));
#223324=CARTESIAN_POINT('Ctrl Pts',(3.83207786166765,6.92136225548355,75.692128373699));
#223325=CARTESIAN_POINT('Ctrl Pts',(3.76325045477522,6.9590244822036,75.6950086347324));
#223326=CARTESIAN_POINT('Ctrl Pts',(3.56871966367596,7.06174144766385,75.7032150282966));
#223327=CARTESIAN_POINT('Ctrl Pts',(3.44182090656361,7.12445230916788,75.7086516062201));
#223328=CARTESIAN_POINT('Ctrl Pts',(3.28839927274547,7.19521391395797,75.7153664478632));
#223329=CARTESIAN_POINT('Ctrl Pts',(3.26343759394008,7.20656978650558,75.7164627628123));
#223330=CARTESIAN_POINT('Ctrl Pts',(3.23007575052749,7.22153828769013,75.7179326562098));
#223331=CARTESIAN_POINT('Ctrl Pts',(3.22172743809201,7.22526656313712,75.7183008617681));
#223332=CARTESIAN_POINT('Ctrl Pts',(3.20796120529136,7.2313858267981,75.7189086434657));
#223333=CARTESIAN_POINT('Ctrl Pts',(3.20254701560521,7.23378522512571,75.719147837824));
#223334=CARTESIAN_POINT('Ctrl Pts',(3.1920159849293,7.23843810585262,75.719613388622));
#223335=CARTESIAN_POINT('Ctrl Pts',(3.18689943780378,7.2406922482185,75.7198397153873));
#223336=CARTESIAN_POINT('Ctrl Pts',(3.17503066156771,7.24590613041933,75.7203650331848));
#223337=CARTESIAN_POINT('Ctrl Pts',(3.16827668247244,7.24886185656421,75.7206642007303));
#223338=CARTESIAN_POINT('Ctrl Pts',(3.15003583670891,7.2568141868062,75.7214727916144));
#223339=CARTESIAN_POINT('Ctrl Pts',(3.13854124572396,7.26179294395677,75.7219829853023));
#223340=CARTESIAN_POINT('Ctrl Pts',(3.05436751965186,7.29801469167306,75.725723649837));
#223341=CARTESIAN_POINT('Ctrl Pts',(2.98123666457522,7.32819260095663,75.7289984183885));
#223342=CARTESIAN_POINT('Ctrl Pts',(2.5603640999454,7.49452572160723,75.7479446882151));
#223343=CARTESIAN_POINT('Ctrl Pts',(2.20379043847942,7.60701429817823,75.7643609285011));
#223344=CARTESIAN_POINT('Ctrl Pts',(1.45210967108439,7.78684024587518,75.7984382403976));
#223345=CARTESIAN_POINT('Ctrl Pts',(1.05709777199716,7.85022740945161,75.8160481073981));
#223346=CARTESIAN_POINT('Ctrl Pts',(0.311821299954308,7.91252487273128,
75.8480919422494));
#223347=CARTESIAN_POINT('Ctrl Pts',(-0.036888965241275,7.91858232233994,
75.8626157436356));
#223348=CARTESIAN_POINT('Ctrl Pts',(-0.418191306487795,7.90000944545624,
75.8780611293533));
#223349=CARTESIAN_POINT('Ctrl Pts',(-0.451491186756857,7.89817630458115,
75.8794065728138));
#223350=CARTESIAN_POINT('Ctrl Pts',(-0.500338698918058,7.89517733904263,
75.8813751336046));
#223351=CARTESIAN_POINT('Ctrl Pts',(-0.515895951624096,7.89417604299847,
75.8820013382166));
#223352=CARTESIAN_POINT('Ctrl Pts',(-0.543326737103672,7.89232910799169,
75.8831041402679));
#223353=CARTESIAN_POINT('Ctrl Pts',(-0.55520149641962,7.89150264470963,
75.8835811019236));
#223354=CARTESIAN_POINT('Ctrl Pts',(-0.578360075786323,7.88983831569531,
75.8845104315158));
#223355=CARTESIAN_POINT('Ctrl Pts',(-0.589644051186677,7.88900303706528,
75.8849628481302));
#223356=CARTESIAN_POINT('Ctrl Pts',(-0.616761448128302,7.8869372081937,
75.8860491317093));
#223357=CARTESIAN_POINT('Ctrl Pts',(-0.632593049729356,7.88568318192396,
75.8866825406924));
#223358=CARTESIAN_POINT('Ctrl Pts',(-0.681072129444093,7.88169620540049,
75.8886197617215));
#223359=CARTESIAN_POINT('Ctrl Pts',(-0.713706611554314,7.87880810866663,
75.8899205161509));
#223360=CARTESIAN_POINT('Ctrl Pts',(-1.29653564927582,7.82357779374865,
75.9130926152636));
#223361=CARTESIAN_POINT('Ctrl Pts',(-1.83977467643434,7.71392621406561,
75.9335912899948));
#223362=CARTESIAN_POINT('Ctrl Pts',(-2.82901299981564,7.40370678258994,
75.9712776094163));
#223363=CARTESIAN_POINT('Ctrl Pts',(-3.27655092009862,7.21680961232943,
75.9885280548554));
#223364=CARTESIAN_POINT('Ctrl Pts',(-3.79013207565515,6.94465867842439,
76.010989865121));
#223365=CARTESIAN_POINT('Ctrl Pts',(-3.87524358373726,6.89752647135095,
76.0148089468064));
#223366=CARTESIAN_POINT('Ctrl Pts',(-3.97045560350569,6.84248233912221,
76.0192143673533));
#223367=CARTESIAN_POINT('Ctrl Pts',(-3.98143408405275,6.83610012303953,
76.0197243660112));
#223368=CARTESIAN_POINT('Ctrl Pts',(-3.99789160910994,6.82647963357907,
76.0204920091297));
#223369=CARTESIAN_POINT('Ctrl Pts',(-4.00338222494194,6.82326111668929,
76.0207486354436));
#223370=CARTESIAN_POINT('Ctrl Pts',(-4.01281331276942,6.81771745165045,
76.0211903446315));
#223371=CARTESIAN_POINT('Ctrl Pts',(-4.01675566873945,6.81539550071784,
76.0213752600788));
#223372=CARTESIAN_POINT('Ctrl Pts',(-4.02486561051468,6.81060946302465,
76.0217562228724));
#223373=CARTESIAN_POINT('Ctrl Pts',(-4.02903295301425,6.80814496789887,
76.0219522918301));
#223374=CARTESIAN_POINT('Ctrl Pts',(-4.03904981571421,6.80220874834244,
76.022424323896));
#223375=CARTESIAN_POINT('Ctrl Pts',(-4.04489711795348,6.79873330662017,
76.022700486178));
#223376=CARTESIAN_POINT('Ctrl Pts',(-4.06277954751779,6.78807335037843,
76.023546962586));
#223377=CARTESIAN_POINT('Ctrl Pts',(-4.0748000218748,6.78086441683733,76.0241186072022));
#223378=CARTESIAN_POINT('Ctrl Pts',(-4.24886322457027,6.67584504340291,
76.0324357076554));
#223379=CARTESIAN_POINT('Ctrl Pts',(-4.40734466036384,6.57229355039865,
76.040523721009));
#223380=CARTESIAN_POINT('Ctrl Pts',(-5.08269097375305,6.09560933702818,
76.0768429640418));
#223381=CARTESIAN_POINT('Ctrl Pts',(-5.55710617108765,5.66646282998117,
76.1070903356604));
#223382=CARTESIAN_POINT('Ctrl Pts',(-6.29080110260823,4.82100271446624,
76.1577224931605));
#223383=CARTESIAN_POINT('Ctrl Pts',(-6.57281247981719,4.42882411785305,
76.1786422200377));
#223384=CARTESIAN_POINT('Ctrl Pts',(-6.82876344676009,3.99404722670944,
76.1990994496335));
#223385=CARTESIAN_POINT('Ctrl Pts',(-6.84005312966079,3.97468195643466,
76.2000054819511));
#223386=CARTESIAN_POINT('Ctrl Pts',(-6.85631832285003,3.94650762036242,
76.2013162531928));
#223387=CARTESIAN_POINT('Ctrl Pts',(-6.86135943564066,3.93773666434462,
76.2017232728102));
#223388=CARTESIAN_POINT('Ctrl Pts',(-6.8701398821569,3.92239164282142,76.2024335602847));
#223389=CARTESIAN_POINT('Ctrl Pts',(-6.87388663310417,3.91582184933087,
76.202737085282));
#223390=CARTESIAN_POINT('Ctrl Pts',(-6.88111604814793,3.90310297989199,
76.2033235868195));
#223391=CARTESIAN_POINT('Ctrl Pts',(-6.88459990434437,3.89695459264327,
76.2036066044646));
#223392=CARTESIAN_POINT('Ctrl Pts',(-6.89285420439953,3.88234160309588,
76.2042780714797));
#223393=CARTESIAN_POINT('Ctrl Pts',(-6.89761730684863,3.87387285482698,
76.2046662668753));
#223394=CARTESIAN_POINT('Ctrl Pts',(-6.91436963448022,3.84395853386793,
76.2060341819681));
#223395=CARTESIAN_POINT('Ctrl Pts',(-6.9262745983675,3.82246580805148,76.2070109952575));
#223396=CARTESIAN_POINT('Ctrl Pts',(-7.08132887761979,3.53943446423079,
76.2197964999699));
#223397=CARTESIAN_POINT('Ctrl Pts',(-7.20968786287085,3.27005139364672,
76.2310826461926));
#223398=CARTESIAN_POINT('Ctrl Pts',(-7.60372995609988,2.30634264731731,
76.26910644646));
#223399=CARTESIAN_POINT('Ctrl Pts',(-7.78661998319807,1.58251926277892,
76.2933044448404));
#223400=CARTESIAN_POINT('Ctrl Pts',(-7.87693674838221,0.740650574163553,
76.3237888080469));
#223401=CARTESIAN_POINT('Ctrl Pts',(-7.88597654076273,0.637235325388901,
76.3275787382517));
#223402=CARTESIAN_POINT('Ctrl Pts',(-7.89901085438058,0.44445949053502,
76.3347678943308));
#223403=CARTESIAN_POINT('Ctrl Pts',(-7.90352983378602,0.355150785214006,
76.3381480019443));
#223404=CARTESIAN_POINT('Ctrl Pts',(-7.9095138143717,0.17714151986588,76.3450117027852));
#223405=CARTESIAN_POINT('Ctrl Pts',(-7.91100253418007,0.0884597651576268,
76.3484973308441));
#223406=CARTESIAN_POINT('Ctrl Pts',(-7.91099963220847,-0.0129679707314106,
76.3525525794503));
#223407=CARTESIAN_POINT('Ctrl Pts',(-7.91096848474549,-0.0257095316003968,
76.35306321325));
#223408=CARTESIAN_POINT('Ctrl Pts',(-7.91086865393941,-0.0462487621033094,
76.3538882358912));
#223409=CARTESIAN_POINT('Ctrl Pts',(-7.91081922303907,-0.0540465330244665,
76.354201896431));
#223410=CARTESIAN_POINT('Ctrl Pts',(-7.91071069604874,-0.067928688127151,
76.3547610646232));
#223411=CARTESIAN_POINT('Ctrl Pts',(-7.91065610950113,-0.0740131083675887,
76.3550064052051));
#223412=CARTESIAN_POINT('Ctrl Pts',(-7.91052752954996,-0.0867119379314251,
76.3555189968786));
#223413=CARTESIAN_POINT('Ctrl Pts',(-7.91045225964427,-0.0933263281004106,
76.3557862942395));
#223414=CARTESIAN_POINT('Ctrl Pts',(-7.91023509872252,-0.110514766928626,
76.3564816870029));
#223415=CARTESIAN_POINT('Ctrl Pts',(-7.91008030144159,-0.121088621421877,
76.3569102429269));
#223416=CARTESIAN_POINT('Ctrl Pts',(-7.9093267462546,-0.16636018607024,
76.3587483026548));
#223417=CARTESIAN_POINT('Ctrl Pts',(-7.90852088699473,-0.201053793574192,
76.3601649702217));
#223418=CARTESIAN_POINT('Ctrl Pts',(-7.90072335247937,-0.462607747035005,
76.3709011970511));
#223419=CARTESIAN_POINT('Ctrl Pts',(-7.88419992786868,-0.689071620868773,
76.3805108104684));
#223420=CARTESIAN_POINT('Ctrl Pts',(-7.80478393924574,-1.37146263479148,
76.4099505587532));
#223421=CARTESIAN_POINT('Ctrl Pts',(-7.71184492116253,-1.82291744877112,
76.4300212318081));
#223422=CARTESIAN_POINT('Ctrl Pts',(-7.41133833433478,-2.82917047643946,
76.4748148886292));
#223423=CARTESIAN_POINT('Ctrl Pts',(-7.17974367895566,-3.37393875914322,
76.4990761601005));
#223424=CARTESIAN_POINT('Ctrl Pts',(-6.8485465187623,-3.96085219546914,
76.5264408298348));
#223425=CARTESIAN_POINT('Ctrl Pts',(-6.80621757084358,-4.03315534669668,
76.529833181467));
#223426=CARTESIAN_POINT('Ctrl Pts',(-6.74648707499715,-4.13156329880377,
76.5344796399074));
#223427=CARTESIAN_POINT('Ctrl Pts',(-6.73006705451193,-4.15825691785126,
76.5357430339251));
#223428=CARTESIAN_POINT('Ctrl Pts',(-6.70159787450962,-4.20392818823517,
76.5379098688576));
#223429=CARTESIAN_POINT('Ctrl Pts',(-6.68962566393961,-4.22295332236366,
76.5388140760126));
#223430=CARTESIAN_POINT('Ctrl Pts',(-6.66476013538056,-4.26209623127658,
76.5406777035256));
#223431=CARTESIAN_POINT('Ctrl Pts',(-6.65185642691635,-4.28220714424607,
76.541637004512));
#223432=CARTESIAN_POINT('Ctrl Pts',(-6.6215138713567,-4.32902906210366,
76.5438747000131));
#223433=CARTESIAN_POINT('Ctrl Pts',(-6.6040041678896,-4.35569369086335,
76.545152310807));
#223434=CARTESIAN_POINT('Ctrl Pts',(-6.54664141738235,-4.44190740810062,
76.5492939862479));
#223435=CARTESIAN_POINT('Ctrl Pts',(-6.50614035091938,-4.501021340535,76.5521506659481));
#223436=CARTESIAN_POINT('Ctrl Pts',(-6.24385835757158,-4.87290045838385,
76.5702356921297));
#223437=CARTESIAN_POINT('Ctrl Pts',(-6.00038657459935,-5.16974834149366,
76.5851655206213));
#223438=CARTESIAN_POINT('Ctrl Pts',(-5.56470955310888,-5.62850340715576,
76.6096376376599));
#223439=CARTESIAN_POINT('Ctrl Pts',(-5.38462826504667,-5.80101893090419,
76.6192298097057));
#223440=CARTESIAN_POINT('Ctrl Pts',(-5.11156478423377,-6.03892189137479,
76.6332779150652));
#223441=CARTESIAN_POINT('Ctrl Pts',(-5.02484666258029,-6.11126728103273,
76.6376726542771));
#223442=CARTESIAN_POINT('Ctrl Pts',(-4.82428005240047,-6.27143588530811,
76.6477284519601));
#223443=CARTESIAN_POINT('Ctrl Pts',(-4.70952728040981,-6.35806082496251,
76.6534056223974));
#223444=CARTESIAN_POINT('Ctrl Pts',(-4.57446218967838,-6.45435561097018,
76.6600476664002));
#223445=CARTESIAN_POINT('Ctrl Pts',(-4.55639023085987,-6.46712600271583,
76.6609355847764));
#223446=CARTESIAN_POINT('Ctrl Pts',(-4.52747385972399,-6.48737813126574,
76.6623552867094));
#223447=CARTESIAN_POINT('Ctrl Pts',(-4.51666388741157,-6.49490892123612,
76.6628857942449));
#223448=CARTESIAN_POINT('Ctrl Pts',(-4.49752977992603,-6.50816786666971,
76.6638244705906));
#223449=CARTESIAN_POINT('Ctrl Pts',(-4.48921337778987,-6.51390714932612,
76.6642323401517));
#223450=CARTESIAN_POINT('Ctrl Pts',(-4.47196583027777,-6.52576124056592,
76.6650780224806));
#223451=CARTESIAN_POINT('Ctrl Pts',(-4.46303308764215,-6.53187368323698,
76.6655158989007));
#223452=CARTESIAN_POINT('Ctrl Pts',(-4.43985636860782,-6.54766316802918,
76.6666517563069));
#223453=CARTESIAN_POINT('Ctrl Pts',(-4.42559338797976,-6.55731200233249,
76.6673505396136));
#223454=CARTESIAN_POINT('Ctrl Pts',(-4.35580663761875,-6.60419097971223,
76.6707684977405));
#223455=CARTESIAN_POINT('Ctrl Pts',(-4.29984457614301,-6.64076248568217,
76.6735057609012));
#223456=CARTESIAN_POINT('Ctrl Pts',(-3.66030169212112,-7.04723359945113,
76.704711173181));
#223457=CARTESIAN_POINT('Ctrl Pts',(-3.031125569441,-7.33986746085772,76.7344053909393));
#223458=CARTESIAN_POINT('Ctrl Pts',(-2.21346180294125,-7.59684814624296,
76.7697558642873));
#223459=CARTESIAN_POINT('Ctrl Pts',(-2.05345843746716,-7.64165067482622,
76.7765459870432));
#223460=CARTESIAN_POINT('Ctrl Pts',(-1.85284797860512,-7.6910671982888,
76.7849136872439));
#223461=CARTESIAN_POINT('Ctrl Pts',(-1.81346121059945,-7.70044925587654,
76.786549713573));
#223462=CARTESIAN_POINT('Ctrl Pts',(-1.75128868264871,-7.71475548911146,
76.7891218282532));
#223463=CARTESIAN_POINT('Ctrl Pts',(-1.72855031927075,-7.71988200072024,
76.790060350592));
#223464=CARTESIAN_POINT('Ctrl Pts',(-1.68827165425998,-7.72877620730823,
76.7917190915845));
#223465=CARTESIAN_POINT('Ctrl Pts',(-1.67074059005184,-7.7325848669138,
76.7924397939047));
#223466=CARTESIAN_POINT('Ctrl Pts',(-1.63038909534158,-7.74120767958216,
76.7940958197187));
#223467=CARTESIAN_POINT('Ctrl Pts',(-1.60756000967662,-7.74598061967059,
76.7950306513656));
#223468=CARTESIAN_POINT('Ctrl Pts',(-1.54384023063618,-7.75900886176455,
76.7976343165433));
#223469=CARTESIAN_POINT('Ctrl Pts',(-1.50290476220918,-7.76704180976044,
76.799300560192));
#223470=CARTESIAN_POINT('Ctrl Pts',(-1.23695142590228,-7.81704973977265,
76.8100868897481));
#223471=CARTESIAN_POINT('Ctrl Pts',(-1.01026306651008,-7.84956602602521,
76.8190963092071));
#223472=CARTESIAN_POINT('Ctrl Pts',(-0.217984704384075,-7.9283168522101,
76.8502609313704));
#223473=CARTESIAN_POINT('Ctrl Pts',(0.350925627523741,-7.92354827175539,
76.8719460904962));
#223474=CARTESIAN_POINT('Ctrl Pts',(1.32316897105209,-7.81040775349422,
76.908659661111));
#223475=CARTESIAN_POINT('Ctrl Pts',(1.72755639665303,-7.73102700946478,
76.9238734703231));
#223476=CARTESIAN_POINT('Ctrl Pts',(2.31262192602222,-7.56796371712911,
76.9470680183079));
#223477=CARTESIAN_POINT('Ctrl Pts',(2.4992981248048,-7.50838188305888,76.9546619254942));
#223478=CARTESIAN_POINT('Ctrl Pts',(2.70071059881239,-7.43575251977539,
76.9632107171017));
#223479=CARTESIAN_POINT('Ctrl Pts',(2.71783667040661,-7.42950988295323,
76.9639404862569));
#223480=CARTESIAN_POINT('Ctrl Pts',(2.74333440375094,-7.42011572433422,
76.965031432397));
#223481=CARTESIAN_POINT('Ctrl Pts',(2.75172260100697,-7.41700908316175,
76.9653910491678));
#223482=CARTESIAN_POINT('Ctrl Pts',(2.76612681189296,-7.41164656077807,
76.9660098429142));
#223483=CARTESIAN_POINT('Ctrl Pts',(2.77214538907784,-7.40939756140302,
76.9662687748677));
#223484=CARTESIAN_POINT('Ctrl Pts',(2.7845311029556,-7.40475211064766,76.9668024245606));
#223485=CARTESIAN_POINT('Ctrl Pts',(2.79089789977172,-7.4023547737306,76.967077174175));
#223486=CARTESIAN_POINT('Ctrl Pts',(2.80566359717387,-7.39677317893505,
76.967715378823));
#223487=CARTESIAN_POINT('Ctrl Pts',(2.81406017409229,-7.3935828268122,76.968079058053));
#223488=CARTESIAN_POINT('Ctrl Pts',(2.84061845668676,-7.3834399820539,76.9692318267219));
#223489=CARTESIAN_POINT('Ctrl Pts',(2.85875989176211,-7.37643484741358,
76.9700228984838));
#223490=CARTESIAN_POINT('Ctrl Pts',(3.37363761505448,-7.17543525300957,
76.992582118535));
#223491=CARTESIAN_POINT('Ctrl Pts',(3.84939343422768,-6.93182428975471,
77.016835596477));
#223492=CARTESIAN_POINT('Ctrl Pts',(4.52373506539515,-6.49559190686231,
77.0536595166864));
#223493=CARTESIAN_POINT('Ctrl Pts',(4.74288873478383,-6.33734220443818,
77.0660526505566));
#223494=CARTESIAN_POINT('Ctrl Pts',(5.30683188770887,-5.88445331552284,
77.0986151183145));
#223495=CARTESIAN_POINT('Ctrl Pts',(5.63514153606628,-5.57086347889153,
77.1182589329069));
#223496=CARTESIAN_POINT('Ctrl Pts',(5.95345962559196,-5.20970573402456,
77.1378135105385));
#223497=CARTESIAN_POINT('Ctrl Pts',(5.97198235264814,-5.18846240706497,
77.138953677477));
#223498=CARTESIAN_POINT('Ctrl Pts',(5.9969939914618,-5.1594656948837,77.1404964730489));
#223499=CARTESIAN_POINT('Ctrl Pts',(6.00358203583363,-5.15179832003059,
77.1409031494016));
#223500=CARTESIAN_POINT('Ctrl Pts',(6.01472623034433,-5.13877794677304,
77.1415915973854));
#223501=CARTESIAN_POINT('Ctrl Pts',(6.01928996749723,-5.13343147414771,
77.1418736780397));
#223502=CARTESIAN_POINT('Ctrl Pts',(6.02806906903521,-5.12311884799037,
77.1424165969397));
#223503=CARTESIAN_POINT('Ctrl Pts',(6.03228543660801,-5.11815355799759,
77.1426774759119));
#223504=CARTESIAN_POINT('Ctrl Pts',(6.04210756670188,-5.10655779756107,
77.1432855042037));
#223505=CARTESIAN_POINT('Ctrl Pts',(6.04770856069563,-5.09992328892645,
77.1436324598246));
#223506=CARTESIAN_POINT('Ctrl Pts',(6.06309286162972,-5.08163924095278,
77.1445860913525));
#223507=CARTESIAN_POINT('Ctrl Pts',(6.07285352891187,-5.06997065510325,
77.1451918501512));
#223508=CARTESIAN_POINT('Ctrl Pts',(6.09501950047367,-5.04331604759972,
77.1465691713219));
#223509=CARTESIAN_POINT('Ctrl Pts',(6.10740332598903,-5.02831225041406,
77.1473398673863));
#223510=CARTESIAN_POINT('Ctrl Pts',(6.36084238851596,-4.7189370752753,77.1631378338541));
#223511=CARTESIAN_POINT('Ctrl Pts',(6.58041656511223,-4.40758901291123,
77.1772655475297));
#223512=CARTESIAN_POINT('Ctrl Pts',(6.96091227020838,-3.77584873618555,
77.2034777585124));
#223513=CARTESIAN_POINT('Ctrl Pts',(7.12417490566864,-3.45795816443406,
77.2156104395252));
#223514=CARTESIAN_POINT('Ctrl Pts',(7.4881183575066,-2.61320015636736,77.2468958250767));
#223515=CARTESIAN_POINT('Ctrl Pts',(7.65499465531323,-2.07403935846896,
77.2659453806929));
#223516=CARTESIAN_POINT('Ctrl Pts',(7.77013436597465,-1.48667933675384,
77.2895670635791));
#223517=CARTESIAN_POINT('Ctrl Pts',(7.77678467420677,-1.45149012100044,
77.2909931643193));
#223518=CARTESIAN_POINT('Ctrl Pts',(7.78456823384693,-1.40871472963587,
77.2927411385468));
#223519=CARTESIAN_POINT('Ctrl Pts',(7.78592977005468,-1.40117000822365,
77.2930499902626));
#223520=CARTESIAN_POINT('Ctrl Pts',(7.78814731183403,-1.38877884130431,
77.2935581458677));
#223521=CARTESIAN_POINT('Ctrl Pts',(7.78900976833996,-1.38393354224265,
77.2937570772932));
#223522=CARTESIAN_POINT('Ctrl Pts',(7.79054991706618,-1.37523390916273,
77.2941146685741));
#223523=CARTESIAN_POINT('Ctrl Pts',(7.7912292723661,-1.37137986733455,77.2942732316256));
#223524=CARTESIAN_POINT('Ctrl Pts',(7.79266569668858,-1.36319538788206,
77.2946102699534));
#223525=CARTESIAN_POINT('Ctrl Pts',(7.79342201613189,-1.35886482190437,
77.2947887890336));
#223526=CARTESIAN_POINT('Ctrl Pts',(7.79543329961403,-1.34729161732688,
77.2952663724309));
#223527=CARTESIAN_POINT('Ctrl Pts',(7.79668177696388,-1.34004787186593,
77.2955658189194));
#223528=CARTESIAN_POINT('Ctrl Pts',(7.80273772619129,-1.30461590702181,
77.2970331308405));
#223529=CARTESIAN_POINT('Ctrl Pts',(7.80740234816075,-1.27640401212969,
77.2982095401699));
#223530=CARTESIAN_POINT('Ctrl Pts',(7.8458088210817,-1.03602926515093,77.3082977145133));
#223531=CARTESIAN_POINT('Ctrl Pts',(7.87104619629272,-0.822612316093222,
77.3176817122153));
#223532=CARTESIAN_POINT('Ctrl Pts',(7.91681991744016,-0.22923071993547,
77.344410605188));
#223533=CARTESIAN_POINT('Ctrl Pts',(7.91868628182647,0.151596047997172,
77.3622605995352));
#223534=CARTESIAN_POINT('Ctrl Pts',(7.85157213574104,1.14909495846763,77.4086400764158));
#223535=CARTESIAN_POINT('Ctrl Pts',(7.7375437605627,1.76018885134718,77.4364886989475));
#223536=CARTESIAN_POINT('Ctrl Pts',(7.54213941461043,2.3877760018051,77.4632386514524));
#223537=CARTESIAN_POINT('Ctrl Pts',(7.53067919231729,2.42367740055003,77.4647632341558));
#223538=CARTESIAN_POINT('Ctrl Pts',(7.51521943076385,2.47093967551408,77.4667629491241));
#223539=CARTESIAN_POINT('Ctrl Pts',(7.51144997249829,2.48237492837154,77.4672462193244));
#223540=CARTESIAN_POINT('Ctrl Pts',(7.50556779411171,2.50008337923575,77.4679937324917));
#223541=CARTESIAN_POINT('Ctrl Pts',(7.50347329091114,2.5063625811159,77.4682586215396));
#223542=CARTESIAN_POINT('Ctrl Pts',(7.49927100900739,2.51890830425175,77.4687875264812));
#223543=CARTESIAN_POINT('Ctrl Pts',(7.49716325066102,2.52517482662088,77.4690515428222));
#223544=CARTESIAN_POINT('Ctrl Pts',(7.49250290862249,2.53897310087461,77.4696325111202));
#223545=CARTESIAN_POINT('Ctrl Pts',(7.48994681721243,2.54650366552312,77.4699493379941));
#223546=CARTESIAN_POINT('Ctrl Pts',(7.48255654950627,2.56816892777995,77.4708601463924));
#223547=CARTESIAN_POINT('Ctrl Pts',(7.47769367388293,2.58229384097178,77.4714531054398));
#223548=CARTESIAN_POINT('Ctrl Pts',(7.46666087460653,2.61404767080262,77.4727842274293));
#223549=CARTESIAN_POINT('Ctrl Pts',(7.46046846049478,2.63166870979522,77.4735215858361));
#223550=CARTESIAN_POINT('Ctrl Pts',(7.32781121035121,3.00492486421935,77.4891132311119));
#223551=CARTESIAN_POINT('Ctrl Pts',(7.17611332320944,3.35109367064447,77.5030086465629));
#223552=CARTESIAN_POINT('Ctrl Pts',(6.80702504483415,4.0522108850848,77.5308860611456));
#223553=CARTESIAN_POINT('Ctrl Pts',(6.58521176629109,4.40352053079047,77.5446939448114));
#223554=CARTESIAN_POINT('Ctrl Pts',(6.06102167519495,5.10492715990078,77.5743821133893));
#223555=CARTESIAN_POINT('Ctrl Pts',(5.75347103359281,5.44919604848762,77.5902789473847));
#223556=CARTESIAN_POINT('Ctrl Pts',(5.3959102833323,5.78523745015897,77.6096762217839));
#223557=CARTESIAN_POINT('Ctrl Pts',(5.37394360351371,5.80564813251346,77.6108713604107));
#223558=CARTESIAN_POINT('Ctrl Pts',(5.34630499731195,5.83103771289881,77.6123802364051));
#223559=CARTESIAN_POINT('Ctrl Pts',(5.34074100112988,5.83613429348374,77.6126842509345));
#223560=CARTESIAN_POINT('Ctrl Pts',(5.33197677989886,5.84413922820667,77.6131635478668));
#223561=CARTESIAN_POINT('Ctrl Pts',(5.32878144157685,5.84705293696424,77.6133383828464));
#223562=CARTESIAN_POINT('Ctrl Pts',(5.32286762132675,5.85243665296755,77.6136621224598));
#223563=CARTESIAN_POINT('Ctrl Pts',(5.32014979922594,5.85490739507209,77.6138109666877));
#223564=CARTESIAN_POINT('Ctrl Pts',(5.31411984324568,5.86038149629061,77.6141413402678));
#223565=CARTESIAN_POINT('Ctrl Pts',(5.31080688418205,5.86338394011517,77.614322944589));
#223566=CARTESIAN_POINT('Ctrl Pts',(5.30133256211888,5.87195564058169,77.6148425488391));
#223567=CARTESIAN_POINT('Ctrl Pts',(5.29516498843464,5.87751799004787,77.6151811091879));
#223568=CARTESIAN_POINT('Ctrl Pts',(5.25596525936006,5.912759267607,77.6173348161676));
#223569=CARTESIAN_POINT('Ctrl Pts',(5.22269308500364,5.94216877479076,77.6191713637252));
#223570=CARTESIAN_POINT('Ctrl Pts',(5.12168865239798,6.02994364819143,77.6247670525515));
#223571=CARTESIAN_POINT('Ctrl Pts',(5.05321450940839,6.08744092695492,77.6285878689974));
#223572=CARTESIAN_POINT('Ctrl Pts',(4.86721434929003,6.23832311867019,77.6390032106648));
#223573=CARTESIAN_POINT('Ctrl Pts',(4.7479829477844,6.32954222217595,77.6457174580962));
#223574=CARTESIAN_POINT('Ctrl Pts',(4.3472056316177,6.61846233565767,77.6682123913164));
#223575=CARTESIAN_POINT('Ctrl Pts',(4.05536120710385,6.80119657325046,77.6844623802304));
#223576=CARTESIAN_POINT('Ctrl Pts',(3.40855002260958,7.14971394998826,77.7189691097025));
#223577=CARTESIAN_POINT('Ctrl Pts',(3.05125595790959,7.30934343525296,77.7371381856648));
#223578=CARTESIAN_POINT('Ctrl Pts',(2.55815853211328,7.4871576261782,77.7604470378504));
#223579=CARTESIAN_POINT('Ctrl Pts',(2.43158393973321,7.52921683996112,77.7662852437559));
#223580=CARTESIAN_POINT('Ctrl Pts',(2.10535539986208,7.62853311717715,77.7809507864971));
#223581=CARTESIAN_POINT('Ctrl Pts',(1.90439583992086,7.68116686815188,77.7896239977303));
#223582=CARTESIAN_POINT('Ctrl Pts',(1.68250868153269,7.73003668454191,77.7988224927611));
#223583=CARTESIAN_POINT('Ctrl Pts',(1.66341554021376,7.73416778689073,77.7996110128789));
#223584=CARTESIAN_POINT('Ctrl Pts',(1.63511744170344,7.74018089043761,77.8007752859817));
#223585=CARTESIAN_POINT('Ctrl Pts',(1.62592419234598,7.74211726767259,77.801152838846));
#223586=CARTESIAN_POINT('Ctrl Pts',(1.61021523413533,7.74539683668304,77.8017968155789));
#223587=CARTESIAN_POINT('Ctrl Pts',(1.60370125063025,7.74674819243386,77.8020635090713));
#223588=CARTESIAN_POINT('Ctrl Pts',(1.59105397123338,7.74935529283511,77.8025806482088));
#223589=CARTESIAN_POINT('Ctrl Pts',(1.58492087482318,7.75061197679073,77.8028311247043));
#223590=CARTESIAN_POINT('Ctrl Pts',(1.57224824469199,7.75319295362273,77.8033480553484));
#223591=CARTESIAN_POINT('Ctrl Pts',(1.56570851334359,7.75451625638698,77.8036144767077));
#223592=CARTESIAN_POINT('Ctrl Pts',(1.54544374066389,7.75859011588527,77.8044389871983));
#223593=CARTESIAN_POINT('Ctrl Pts',(1.53171303218555,7.76131252634275,77.8049961502282));
#223594=CARTESIAN_POINT('Ctrl Pts',(1.45853933869499,7.77561905236369,77.8079574829352));
#223595=CARTESIAN_POINT('Ctrl Pts',(1.39897127190299,7.78655689251933,77.8103404258614));
#223596=CARTESIAN_POINT('Ctrl Pts',(1.23199578992739,7.81523879740535,77.8169458940189));
#223597=CARTESIAN_POINT('Ctrl Pts',(1.12433774749176,7.83145177101568,77.8211191443115));
#223598=CARTESIAN_POINT('Ctrl Pts',(0.696440555039915,7.8868858611171,77.8374042917127));
#223599=CARTESIAN_POINT('Ctrl Pts',(0.374257070161404,7.90872607166841,
77.8489839292691));
#223600=CARTESIAN_POINT('Ctrl Pts',(-0.682728726760493,7.91562390989119,
77.8860047764095));
#223601=CARTESIAN_POINT('Ctrl Pts',(-1.41414352335224,7.81814241127103,
77.9099116164651));
#223602=CARTESIAN_POINT('Ctrl Pts',(-2.16279527107709,7.60973514527557,
77.9405670438782));
#223603=CARTESIAN_POINT('Ctrl Pts',(-2.20392776828705,7.59792436512276,
77.9422705187981));
#223604=CARTESIAN_POINT('Ctrl Pts',(-2.25609009328976,7.58248726837354,
77.9444537725741));
#223605=CARTESIAN_POINT('Ctrl Pts',(-2.26721104809879,7.57916946278228,
77.9449205732845));
#223606=CARTESIAN_POINT('Ctrl Pts',(-2.28482754738544,7.57387154573944,
77.94566210214));
#223607=CARTESIAN_POINT('Ctrl Pts',(-2.2913279383155,7.57190751339285,77.945936171431));
#223608=CARTESIAN_POINT('Ctrl Pts',(-2.30336772200221,7.5682528816291,77.9464446167069));
#223609=CARTESIAN_POINT('Ctrl Pts',(-2.30890780638163,7.56656456289447,
77.9466789005935));
#223610=CARTESIAN_POINT('Ctrl Pts',(-2.32121642131671,7.56279878446657,
77.9472001314188));
#223611=CARTESIAN_POINT('Ctrl Pts',(-2.32798402266772,7.56071832028621,
77.9474871977965));
#223612=CARTESIAN_POINT('Ctrl Pts',(-2.34740579030132,7.55471922307376,
77.9483123890394));
#223613=CARTESIAN_POINT('Ctrl Pts',(-2.36005288541576,7.55077789762234,
77.9488514017277));
#223614=CARTESIAN_POINT('Ctrl Pts',(-2.44287481713292,7.52473896178988,
77.9523919217114));
#223615=CARTESIAN_POINT('Ctrl Pts',(-2.51274714208484,7.50169548879922,
77.9554292015039));
#223616=CARTESIAN_POINT('Ctrl Pts',(-2.73317966984023,7.42557296862749,
77.965153872295));
#223617=CARTESIAN_POINT('Ctrl Pts',(-2.88245692108499,7.3689106512389,77.9719518520097));
#223618=CARTESIAN_POINT('Ctrl Pts',(-3.50435477055147,7.11106242071615,
78.0009621446071));
#223619=CARTESIAN_POINT('Ctrl Pts',(-3.95851597577381,6.86861581018722,
78.0237736388431));
#223620=CARTESIAN_POINT('Ctrl Pts',(-4.74260182460372,6.34628021883938,
78.0644147080596));
#223621=CARTESIAN_POINT('Ctrl Pts',(-5.07935214457477,6.08011252520854,
78.0823942268664));
#223622=CARTESIAN_POINT('Ctrl Pts',(-5.42239712183903,5.76048223196537,
78.1013904397017));
#223623=CARTESIAN_POINT('Ctrl Pts',(-5.45168082966606,5.73277613880576,
78.1030184423208));
#223624=CARTESIAN_POINT('Ctrl Pts',(-5.4935892406331,5.69251395897022,78.105357772358));
#223625=CARTESIAN_POINT('Ctrl Pts',(-5.50638526724705,5.68013725270134,
78.1060733281485));
#223626=CARTESIAN_POINT('Ctrl Pts',(-5.52835001356206,5.65874830747929,
78.1073038057979));
#223627=CARTESIAN_POINT('Ctrl Pts',(-5.53753872758249,5.64975673118095,
78.1078192329772));
#223628=CARTESIAN_POINT('Ctrl Pts',(-5.55621206840689,5.63139469514049,
78.1088680527892));
#223629=CARTESIAN_POINT('Ctrl Pts',(-5.56569500815437,5.62202257546752,
78.1094014014431));
#223630=CARTESIAN_POINT('Ctrl Pts',(-5.58898003424249,5.59889301012379,
78.1107128046191));
#223631=CARTESIAN_POINT('Ctrl Pts',(-5.60275508531585,5.58510843404367,
78.1114901620989));
#223632=CARTESIAN_POINT('Ctrl Pts',(-5.65302017104975,5.53443549084582,
78.1143324484749));
#223633=CARTESIAN_POINT('Ctrl Pts',(-5.68919819416887,5.4972390563282,78.1163892565158));
#223634=CARTESIAN_POINT('Ctrl Pts',(-5.89483760099557,5.28160640599078,
78.1281455254455));
#223635=CARTESIAN_POINT('Ctrl Pts',(-6.05626983074201,5.09569231729241,
78.1376258254963));
#223636=CARTESIAN_POINT('Ctrl Pts',(-6.43217919107187,4.61962604532561,
78.1605158125718));
#223637=CARTESIAN_POINT('Ctrl Pts',(-6.63598390843638,4.32175900319384,
78.173661290718));
#223638=CARTESIAN_POINT('Ctrl Pts',(-6.97677875995999,3.74240636299991,
78.1981058565199));
#223639=CARTESIAN_POINT('Ctrl Pts',(-7.11877559423572,3.46468899349478,
78.2093999677342));
#223640=CARTESIAN_POINT('Ctrl Pts',(-7.2670819533056,3.12677705606071,78.2232824043481));
#223641=CARTESIAN_POINT('Ctrl Pts',(-7.28957436711832,3.07397467105855,
78.225456029218));
#223642=CARTESIAN_POINT('Ctrl Pts',(-7.32579239824619,2.98631705419967,
78.2290779919308));
#223643=CARTESIAN_POINT('Ctrl Pts',(-7.33984868002205,2.95160043331317,
78.2305159326895));
#223644=CARTESIAN_POINT('Ctrl Pts',(-7.36063596688101,2.89919253829818,
78.2326935039014));
#223645=CARTESIAN_POINT('Ctrl Pts',(-7.367550964607,2.88157456754953,78.2334267007099));
#223646=CARTESIAN_POINT('Ctrl Pts',(-7.40364044764668,2.78864695062231,
78.2373008909252));
#223647=CARTESIAN_POINT('Ctrl Pts',(-7.43172300949163,2.71292023447926,
78.2404816706145));
#223648=CARTESIAN_POINT('Ctrl Pts',(-7.46302583095415,2.62437412547728,
78.2442417199794));
#223649=CARTESIAN_POINT('Ctrl Pts',(-7.46738012459949,2.61195868568348,
78.2447698603604));
#223650=CARTESIAN_POINT('Ctrl Pts',(-7.4738753886561,2.5932896801331,78.2455654896149));
#223651=CARTESIAN_POINT('Ctrl Pts',(-7.47603954031818,2.58704415916208,
78.245831905564));
#223652=CARTESIAN_POINT('Ctrl Pts',(-7.47987568709139,2.5759284190981,78.246306520887));
#223653=CARTESIAN_POINT('Ctrl Pts',(-7.48155076122501,2.57105926063264,
78.2465145756145));
#223654=CARTESIAN_POINT('Ctrl Pts',(-7.48506217617925,2.56081967978592,
78.2469524324354));
#223655=CARTESIAN_POINT('Ctrl Pts',(-7.48689749321258,2.55544891154598,
78.2471822829267));
#223656=CARTESIAN_POINT('Ctrl Pts',(-7.49170691897792,2.5413252249918,78.2477872383819));
#223657=CARTESIAN_POINT('Ctrl Pts',(-7.49467146180025,2.53256907854438,
78.2481628021888));
#223658=CARTESIAN_POINT('Ctrl Pts',(-7.50778462225264,2.49361306015807,
78.2498360480472));
#223659=CARTESIAN_POINT('Ctrl Pts',(-7.51776604064202,2.46335741637706,
78.2511419129291));
#223660=CARTESIAN_POINT('Ctrl Pts',(-7.59191090184999,2.23396141522681,
78.261096088382));
#223661=CARTESIAN_POINT('Ctrl Pts',(-7.64833039736845,2.03241860934034,
78.2701407907994));
#223662=CARTESIAN_POINT('Ctrl Pts',(-7.83905738313568,1.22976457236923,
78.306758924624));
#223663=CARTESIAN_POINT('Ctrl Pts',(-7.91097894886285,0.616079605845327,
78.3358990774571));
#223664=CARTESIAN_POINT('Ctrl Pts',(-7.91099999537971,0.000270374307908966,
78.3636650122822));
#223665=CARTESIAN_POINT('',(-7.911,-4.5324854980322E-12,80.3576684917632));
#223666=CARTESIAN_POINT('Ctrl Pts',(-7.911,-4.92828000631107E-12,78.3576684917632));
#223667=CARTESIAN_POINT('Ctrl Pts',(-7.91099999999863,-2.2016758966715,
78.4462559274959));
#223668=CARTESIAN_POINT('Ctrl Pts',(-6.94214576672116,-4.38610418339077,
78.5348433632287));
#223669=CARTESIAN_POINT('Ctrl Pts',(-3.67820201487898,-7.34180684107821,
78.7120182346941));
#223670=CARTESIAN_POINT('Ctrl Pts',(-1.4086817587134,-8.08992666571401,
78.8006056704268));
#223671=CARTESIAN_POINT('Ctrl Pts',(2.97309270521618,-7.65454228025118,
78.9777805418922));
#223672=CARTESIAN_POINT('Ctrl Pts',(5.05102072675873,-6.47444880834007,
79.066367977625));
#223673=CARTESIAN_POINT('Ctrl Pts',(7.66951518847977,-2.93425195367416,
79.2435428490904));
#223674=CARTESIAN_POINT('Ctrl Pts',(8.18956872247087,-0.601881960096307,
79.3321302848231));
#223675=CARTESIAN_POINT('Ctrl Pts',(7.32306689761226,3.71537198232669,79.5093051562885));
#223676=CARTESIAN_POINT('Ctrl Pts',(5.94329958850042,5.6664351893667,79.5978925920213));
#223677=CARTESIAN_POINT('Ctrl Pts',(2.16154501637666,7.92205913233042,79.7750674634867));
#223678=CARTESIAN_POINT('Ctrl Pts',(-0.210816529302004,8.20894963712993,
79.8636548992194));
#223679=CARTESIAN_POINT('Ctrl Pts',(-4.42123908576541,6.91982244717759,
80.0408297706849));
#223680=CARTESIAN_POINT('Ctrl Pts',(-6.22631625634251,5.3539035880344,80.1294172064176));
#223681=CARTESIAN_POINT('Ctrl Pts',(-7.65317280859565,2.31334857514328,
80.2645592586879));
#223682=CARTESIAN_POINT('Ctrl Pts',(-7.91100000000066,1.1570283783619,80.3111138752256));
#223683=CARTESIAN_POINT('Ctrl Pts',(-7.911,-4.5324854980322E-12,80.3576684917632));
#223684=CARTESIAN_POINT('',(-7.91099794240846,0.00570571723741386,84.3576684917632));
#223685=CARTESIAN_POINT('Ctrl Pts',(-7.91099987852728,-0.00138634102841706,
80.3603921088743));
#223686=CARTESIAN_POINT('Ctrl Pts',(-7.91095793537386,-0.24073025048579,
80.3695915106551));
#223687=CARTESIAN_POINT('Ctrl Pts',(-7.9000542515115,-0.479956577419262,
80.3785790578079));
#223688=CARTESIAN_POINT('Ctrl Pts',(-7.81569063911966,-1.40521807938145,
80.4129340180817));
#223689=CARTESIAN_POINT('Ctrl Pts',(-7.6635114518347,-2.08087428066251,
80.4368573329913));
#223690=CARTESIAN_POINT('Ctrl Pts',(-7.40946242548989,-2.772364669455,80.4658737675769));
#223691=CARTESIAN_POINT('Ctrl Pts',(-7.39282587712584,-2.8164276518804,
80.4677448525175));
#223692=CARTESIAN_POINT('Ctrl Pts',(-7.37197854201269,-2.87018551934564,
80.4700576007669));
#223693=CARTESIAN_POINT('Ctrl Pts',(-7.36814027622444,-2.88002454983967,
80.4704821272609));
#223694=CARTESIAN_POINT('Ctrl Pts',(-7.36210183251155,-2.89541244701035,
80.4711480489127));
#223695=CARTESIAN_POINT('Ctrl Pts',(-7.35991504801162,-2.90096658311365,
80.4713888117564));
#223696=CARTESIAN_POINT('Ctrl Pts',(-7.35603196292923,-2.91079644077777,
80.471815644071));
#223697=CARTESIAN_POINT('Ctrl Pts',(-7.35433821370686,-2.91507317190321,
80.4720015912719));
#223698=CARTESIAN_POINT('Ctrl Pts',(-7.35072802056362,-2.924165767027,80.4723974479248));
#223699=CARTESIAN_POINT('Ctrl Pts',(-7.34881057253635,-2.92898122802785,
80.4726074059676));
#223700=CARTESIAN_POINT('Ctrl Pts',(-7.34331976918453,-2.94273144652949,
80.4732078255246));
#223701=CARTESIAN_POINT('Ctrl Pts',(-7.33973485098251,-2.95166155155004,
80.4735988540301));
#223702=CARTESIAN_POINT('Ctrl Pts',(-7.32429967848262,-2.98990888649565,
80.475278355521));
#223703=CARTESIAN_POINT('Ctrl Pts',(-7.31229005405701,-3.01916131986956,
80.4765748322347));
#223704=CARTESIAN_POINT('Ctrl Pts',(-7.12013556792224,-3.47932902306754,
80.4971696743844));
#223705=CARTESIAN_POINT('Ctrl Pts',(-6.90236700072341,-3.89349611162777,
80.5184320397395));
#223706=CARTESIAN_POINT('Ctrl Pts',(-6.56805011579318,-4.41216161926071,
80.5468415634856));
#223707=CARTESIAN_POINT('Ctrl Pts',(-6.48315239239182,-4.53598805123894,
80.553774624271));
#223708=CARTESIAN_POINT('Ctrl Pts',(-6.31777510742065,-4.76306090839403,
80.5667063731205));
#223709=CARTESIAN_POINT('Ctrl Pts',(-6.23815543313102,-4.86687262062322,
80.57270874959));
#223710=CARTESIAN_POINT('Ctrl Pts',(-6.13038887501367,-5.00039155576887,
80.5805240127588));
#223711=CARTESIAN_POINT('Ctrl Pts',(-6.10453527998605,-5.03192135473416,
80.5823767754192));
#223712=CARTESIAN_POINT('Ctrl Pts',(-5.93869806269754,-5.23100917251759,
80.594118759109));
#223713=CARTESIAN_POINT('Ctrl Pts',(-5.79206716241005,-5.39291732373115,
80.6038604241587));
#223714=CARTESIAN_POINT('Ctrl Pts',(-5.44063571003916,-5.75007203217559,
80.6256919331491));
#223715=CARTESIAN_POINT('Ctrl Pts',(-5.23168180123048,-5.94082246340584,
80.6376075846975));
#223716=CARTESIAN_POINT('Ctrl Pts',(-4.9964776490394,-6.13348069283378,
80.6499306919887));
#223717=CARTESIAN_POINT('Ctrl Pts',(-4.97995234760287,-6.14690563870763,
80.6507910754564));
#223718=CARTESIAN_POINT('Ctrl Pts',(-4.95563367044605,-6.16649938814303,
80.6520493183198));
#223719=CARTESIAN_POINT('Ctrl Pts',(-4.94788261014304,-6.17272042593602,
80.6524491867495));
#223720=CARTESIAN_POINT('Ctrl Pts',(-4.9342073266964,-6.18365396512743,
80.6531526270698));
#223721=CARTESIAN_POINT('Ctrl Pts',(-4.92828803243892,-6.18837259487222,
80.6534564338072));
#223722=CARTESIAN_POINT('Ctrl Pts',(-4.91674365329109,-6.19754825347419,
80.6540476369052));
#223723=CARTESIAN_POINT('Ctrl Pts',(-4.91111925984339,-6.20200613690654,
80.654335065817));
#223724=CARTESIAN_POINT('Ctrl Pts',(-4.89761714119421,-6.2126780063063,
80.6550236345171));
#223725=CARTESIAN_POINT('Ctrl Pts',(-4.88973363603806,-6.21888467824472,
80.6554244951526));
#223726=CARTESIAN_POINT('Ctrl Pts',(-4.86567588721527,-6.23775128062091,
80.6566442196407));
#223727=CARTESIAN_POINT('Ctrl Pts',(-4.84946407340832,-6.25036327638874,
80.6574612613718));
#223728=CARTESIAN_POINT('Ctrl Pts',(-4.67293970306116,-6.38659034673561,
80.6663051093463));
#223729=CARTESIAN_POINT('Ctrl Pts',(-4.50798252653677,-6.50407580453327,
80.6740974921286));
#223730=CARTESIAN_POINT('Ctrl Pts',(-3.99548681892427,-6.84020952683684,
80.6970687377426));
#223731=CARTESIAN_POINT('Ctrl Pts',(-3.63527099537886,-7.03826782921289,
80.7115469612408));
#223732=CARTESIAN_POINT('Ctrl Pts',(-3.08120565376169,-7.28897576366361,
80.7326249854692));
#223733=CARTESIAN_POINT('Ctrl Pts',(-2.89811986318283,-7.3636877419717,
80.7394176322963));
#223734=CARTESIAN_POINT('Ctrl Pts',(-2.528347432509,-7.49865189982054,80.7530436453756));
#223735=CARTESIAN_POINT('Ctrl Pts',(-2.34183706319534,-7.55897593552349,
80.7598717422723));
#223736=CARTESIAN_POINT('Ctrl Pts',(-1.85368237466897,-7.697059561135,80.7779800655483));
#223737=CARTESIAN_POINT('Ctrl Pts',(-1.54934176187841,-7.76404596926381,
80.789526415985));
#223738=CARTESIAN_POINT('Ctrl Pts',(-1.22322088076005,-7.8158817133152,
80.8026935060415));
#223739=CARTESIAN_POINT('Ctrl Pts',(-1.20459528325662,-7.81877397520732,
80.8034477538113));
#223740=CARTESIAN_POINT('Ctrl Pts',(-1.17770093522285,-7.8228518636963,
80.8045399195286));
#223741=CARTESIAN_POINT('Ctrl Pts',(-1.16944027996602,-7.82409101462229,
80.8048757985141));
#223742=CARTESIAN_POINT('Ctrl Pts',(-1.15505942069356,-7.82622495154673,
80.8054612363056));
#223743=CARTESIAN_POINT('Ctrl Pts',(-1.14894009189633,-7.82712564882711,
80.8057105750701));
#223744=CARTESIAN_POINT('Ctrl Pts',(-1.13714052641633,-7.828848278252,80.8061917854172));
#223745=CARTESIAN_POINT('Ctrl Pts',(-1.1314604379527,-7.82967120751795,
80.8064236203898));
#223746=CARTESIAN_POINT('Ctrl Pts',(-1.11802851524996,-7.83160229826112,
80.8069722899079));
#223747=CARTESIAN_POINT('Ctrl Pts',(-1.11027592802888,-7.83270513182781,
80.8072893156823));
#223748=CARTESIAN_POINT('Ctrl Pts',(-1.08321920133923,-7.83651307212582,
80.8083969264799));
#223749=CARTESIAN_POINT('Ctrl Pts',(-1.06390679203152,-7.83915832841082,
80.8091896110198));
#223750=CARTESIAN_POINT('Ctrl Pts',(-0.715263154346291,-7.88560060326201,
80.8235355695218));
#223751=CARTESIAN_POINT('Ctrl Pts',(-0.383516257476511,-7.90867854893081,
80.8377420696769));
#223752=CARTESIAN_POINT('Ctrl Pts',(0.453292814945432,-7.91410700853291,
80.8738137113066));
#223753=CARTESIAN_POINT('Ctrl Pts',(0.957086507945457,-7.86909071114896,
80.895670344785));
#223754=CARTESIAN_POINT('Ctrl Pts',(1.74797015052176,-7.7212997216921,80.9295163748176));
#223755=CARTESIAN_POINT('Ctrl Pts',(2.03941333682996,-7.64948822650898,
80.9419125583887));
#223756=CARTESIAN_POINT('Ctrl Pts',(2.53512223128145,-7.49699336929173,
80.9631413083895));
#223757=CARTESIAN_POINT('Ctrl Pts',(2.74141063437854,-7.4240436779781,80.9720455145676));
#223758=CARTESIAN_POINT('Ctrl Pts',(2.98873004121259,-7.32486817192277,
80.9828200691888));
#223759=CARTESIAN_POINT('Ctrl Pts',(3.03288714042946,-7.3066953279378,80.9847474855872));
#223760=CARTESIAN_POINT('Ctrl Pts',(3.09826238214475,-7.27909541437862,
80.9876066245835));
#223761=CARTESIAN_POINT('Ctrl Pts',(3.11960782437201,-7.26997296181839,
80.9885410423733));
#223762=CARTESIAN_POINT('Ctrl Pts',(3.16262980782737,-7.25136218802389,
80.9904261946402));
#223763=CARTESIAN_POINT('Ctrl Pts',(3.18430455384401,-7.24187029676157,
80.9913768857457));
#223764=CARTESIAN_POINT('Ctrl Pts',(3.23081898312706,-7.22125131127351,
80.993419145273));
#223765=CARTESIAN_POINT('Ctrl Pts',(3.25564450102866,-7.21009297378671,
80.9945104014346));
#223766=CARTESIAN_POINT('Ctrl Pts',(3.32272462936286,-7.17952534425862,
80.9974625730817));
#223767=CARTESIAN_POINT('Ctrl Pts',(3.3648665870068,-7.15987122863654,80.9993210321844));
#223768=CARTESIAN_POINT('Ctrl Pts',(3.57145093136669,-7.06129791398134,
81.0084512408306));
#223769=CARTESIAN_POINT('Ctrl Pts',(3.73330489017435,-6.97707862897671,
81.0156655775695));
#223770=CARTESIAN_POINT('Ctrl Pts',(4.12353642253008,-6.75655485303899,
81.033267744533));
#223771=CARTESIAN_POINT('Ctrl Pts',(4.34823076894736,-6.61418764680973,
81.0435835300217));
#223772=CARTESIAN_POINT('Ctrl Pts',(4.85180298629871,-6.25835201303758,
81.0674370532624));
#223773=CARTESIAN_POINT('Ctrl Pts',(5.12448782893615,-6.03710023523412,
81.0809193590969));
#223774=CARTESIAN_POINT('Ctrl Pts',(5.47602470542838,-5.71083847505918,
81.0997582262461));
#223775=CARTESIAN_POINT('Ctrl Pts',(5.56830852423742,-5.62089510610995,
81.1048580446437));
#223776=CARTESIAN_POINT('Ctrl Pts',(5.67382646128203,-5.5129034549772,81.1109078950903));
#223777=CARTESIAN_POINT('Ctrl Pts',(5.68923336570411,-5.49700235768921,
81.1117969001049));
#223778=CARTESIAN_POINT('Ctrl Pts',(5.71156847651353,-5.47375634066113,
81.1130941623482));
#223779=CARTESIAN_POINT('Ctrl Pts',(5.71854973736505,-5.46646246117536,
81.1135008637168));
#223780=CARTESIAN_POINT('Ctrl Pts',(5.73258908392174,-5.45173811028733,
81.1143212295277));
#223781=CARTESIAN_POINT('Ctrl Pts',(5.73964673187823,-5.44430724893198,
81.1147349058878));
#223782=CARTESIAN_POINT('Ctrl Pts',(5.75332612615036,-5.42984831530666,
81.115539218677));
#223783=CARTESIAN_POINT('Ctrl Pts',(5.75994948478011,-5.4228217906585,81.1159298045814));
#223784=CARTESIAN_POINT('Ctrl Pts',(5.77575378420161,-5.40599385695902,
81.1168645840447));
#223785=CARTESIAN_POINT('Ctrl Pts',(5.78492265960937,-5.39618116623948,
81.1174091558369));
#223786=CARTESIAN_POINT('Ctrl Pts',(5.82068340246384,-5.35771350116169,
81.1195420863586));
#223787=CARTESIAN_POINT('Ctrl Pts',(5.84708753669568,-5.32888511135394,
81.121136379339));
#223788=CARTESIAN_POINT('Ctrl Pts',(6.2209255082974,-4.91460004225055,81.1439792650136));
#223789=CARTESIAN_POINT('Ctrl Pts',(6.52982118227819,-4.4960693730446,81.1661315478555));
#223790=CARTESIAN_POINT('Ctrl Pts',(6.96113102891696,-3.77243007450554,
81.2014735723344));
#223791=CARTESIAN_POINT('Ctrl Pts',(7.10956169887988,-3.4846402505623,81.214884497823));
#223792=CARTESIAN_POINT('Ctrl Pts',(7.26826772330108,-3.12428214550926,
81.2309134748122));
#223793=CARTESIAN_POINT('Ctrl Pts',(7.29572097510323,-3.05962582736397,
81.2337613819408));
#223794=CARTESIAN_POINT('Ctrl Pts',(7.33318442751359,-2.96802164113235,
81.2377585138106));
#223795=CARTESIAN_POINT('Ctrl Pts',(7.34391424519294,-2.94137210804497,
81.2389169096192));
#223796=CARTESIAN_POINT('Ctrl Pts',(7.36194061613685,-2.89588662776988,
81.2408866585347));
#223797=CARTESIAN_POINT('Ctrl Pts',(7.36931061064185,-2.87708013847965,
81.241698929542));
#223798=CARTESIAN_POINT('Ctrl Pts',(7.3840187892947,-2.83912102258128,81.2433341799274));
#223799=CARTESIAN_POINT('Ctrl Pts',(7.39135467976364,-2.8199676704655,81.244157125335));
#223800=CARTESIAN_POINT('Ctrl Pts',(7.4091091386683,-2.77306711280438,81.2461670707101));
#223801=CARTESIAN_POINT('Ctrl Pts',(7.41944643263451,-2.74528943518467,
81.2473530695204));
#223802=CARTESIAN_POINT('Ctrl Pts',(7.45515230772397,-2.64766816042951,
81.251506095322));
#223803=CARTESIAN_POINT('Ctrl Pts',(7.47969283879862,-2.57752551596964,
81.2544632161534));
#223804=CARTESIAN_POINT('Ctrl Pts',(7.73162887285294,-1.82351618160533,
81.285991052157));
#223805=CARTESIAN_POINT('Ctrl Pts',(7.86556005425078,-1.1119223363754,81.3137087882593));
#223806=CARTESIAN_POINT('Ctrl Pts',(7.91457622043815,-0.12407446912366,
81.3508654404041));
#223807=CARTESIAN_POINT('Ctrl Pts',(7.91423131011837,0.144407793103972,
81.3608545458554));
#223808=CARTESIAN_POINT('Ctrl Pts',(7.88798191323639,0.647319257892521,
81.3797418201335));
#223809=CARTESIAN_POINT('Ctrl Pts',(7.86524170847977,0.881616976885259,
81.3886154158048));
#223810=CARTESIAN_POINT('Ctrl Pts',(7.81289836057658,1.24944215341381,81.4029721490455));
#223811=CARTESIAN_POINT('Ctrl Pts',(7.79022055809496,1.38381651902715,81.4083089711112));
#223812=CARTESIAN_POINT('Ctrl Pts',(7.76081282121446,1.53427385930797,81.4144389491362));
#223813=CARTESIAN_POINT('Ctrl Pts',(7.75748684524419,1.55100282472295,81.415122692386));
#223814=CARTESIAN_POINT('Ctrl Pts',(7.75241838394963,1.5760719501794,81.4161507033002));
#223815=CARTESIAN_POINT('Ctrl Pts',(7.75071647337759,1.5844203169084,81.4164936097246));
#223816=CARTESIAN_POINT('Ctrl Pts',(7.74776985141665,1.59875599346317,81.4170834329636));
#223817=CARTESIAN_POINT('Ctrl Pts',(7.74653167617132,1.60474464853645,81.4173301256056));
#223818=CARTESIAN_POINT('Ctrl Pts',(7.74397055468193,1.61705993231343,81.4178380531386));
#223819=CARTESIAN_POINT('Ctrl Pts',(7.74264679672763,1.62338638570648,81.418099316106));
#223820=CARTESIAN_POINT('Ctrl Pts',(7.73944697959424,1.63858588443645,81.4187278303027));
#223821=CARTESIAN_POINT('Ctrl Pts',(7.73756341483344,1.64745732911463,81.4190953467729));
#223822=CARTESIAN_POINT('Ctrl Pts',(7.73064700683451,1.67975956243382,81.4204360341884));
#223823=CARTESIAN_POINT('Ctrl Pts',(7.72552298428528,1.70317055389527,81.4214125007712));
#223824=CARTESIAN_POINT('Ctrl Pts',(7.64656598108964,2.05622632553145,81.4362149782184));
#223825=CARTESIAN_POINT('Ctrl Pts',(7.55181638850403,2.38076000285328,81.4510147315965));
#223826=CARTESIAN_POINT('Ctrl Pts',(7.30787984703686,3.05308762090558,81.4833146319153));
#223827=CARTESIAN_POINT('Ctrl Pts',(7.15387658658543,3.39830899248751,81.5008054031428));
#223828=CARTESIAN_POINT('Ctrl Pts',(6.818780190892,4.02479919207307,81.5331039380034));
#223829=CARTESIAN_POINT('Ctrl Pts',(6.64336259496362,4.30819370359075,81.5479546116735));
#223830=CARTESIAN_POINT('Ctrl Pts',(6.32950281334622,4.75027057655303,81.5711917709364));
#223831=CARTESIAN_POINT('Ctrl Pts',(6.20168673598109,4.91597056960559,81.5799241509856));
#223832=CARTESIAN_POINT('Ctrl Pts',(6.05283955405643,5.09387597567603,81.5893233840186));
#223833=CARTESIAN_POINT('Ctrl Pts',(6.03815782714681,5.11127079974586,81.5902426988214));
#223834=CARTESIAN_POINT('Ctrl Pts',(6.01692753983949,5.13620518424576,81.5915609456116));
#223835=CARTESIAN_POINT('Ctrl Pts',(6.0104395261145,5.14379601249999,81.5919623250743));
#223836=CARTESIAN_POINT('Ctrl Pts',(5.99914929265777,5.15695480172843,81.592658234461));
#223837=CARTESIAN_POINT('Ctrl Pts',(5.99435365794574,5.16252838118148,81.5929530315727));
#223838=CARTESIAN_POINT('Ctrl Pts',(5.98511436853565,5.17323623102756,81.5935194602497));
#223839=CARTESIAN_POINT('Ctrl Pts',(5.98067186198861,5.17837148010471,81.5937911381978));
#223840=CARTESIAN_POINT('Ctrl Pts',(5.97018627942039,5.19046064086167,81.5944307853124));
#223841=CARTESIAN_POINT('Ctrl Pts',(5.96413765049933,5.19740973581731,81.5947985266634));
#223842=CARTESIAN_POINT('Ctrl Pts',(5.94316376480033,5.22142120030768,81.5960694101149));
#223843=CARTESIAN_POINT('Ctrl Pts',(5.92817725401173,5.23843004555065,81.5969700307434));
#223844=CARTESIAN_POINT('Ctrl Pts',(5.75659028637497,5.43149221051784,81.6071974000554));
#223845=CARTESIAN_POINT('Ctrl Pts',(5.59226673986383,5.6005359629502,81.6161920728563));
#223846=CARTESIAN_POINT('Ctrl Pts',(5.28906469099099,5.88577485801962,81.6315777226181));
#223847=CARTESIAN_POINT('Ctrl Pts',(5.15329268966539,6.00500867541816,81.6380830008919));
#223848=CARTESIAN_POINT('Ctrl Pts',(4.56284328516325,6.48874966564526,81.6650464799613));
#223849=CARTESIAN_POINT('Ctrl Pts',(4.07274610511969,6.80706311478944,81.6841219929992));
#223850=CARTESIAN_POINT('Ctrl Pts',(3.38322563201565,7.15356210590033,81.7112001400796));
#223851=CARTESIAN_POINT('Ctrl Pts',(3.2113093555447,7.23236840931404,81.7179830039537));
#223852=CARTESIAN_POINT('Ctrl Pts',(2.94502523962398,7.34306566051393,81.7287516512723));
#223853=CARTESIAN_POINT('Ctrl Pts',(2.85260022555226,7.37946187871021,81.7325363168097));
#223854=CARTESIAN_POINT('Ctrl Pts',(2.70744972211006,7.43348664039645,81.738585643333));
#223855=CARTESIAN_POINT('Ctrl Pts',(2.65518030475908,7.45231674756735,81.740785086895));
#223856=CARTESIAN_POINT('Ctrl Pts',(2.59406797067548,7.47360798207317,81.7433853837973));
#223857=CARTESIAN_POINT('Ctrl Pts',(2.58541268416741,7.47660659373052,81.7437543301238));
#223858=CARTESIAN_POINT('Ctrl Pts',(2.57222145259777,7.48115103197362,81.7443176718346));
#223859=CARTESIAN_POINT('Ctrl Pts',(2.567689253967,7.48270778924813,81.7445114101748));
#223860=CARTESIAN_POINT('Ctrl Pts',(2.55981769004762,7.48540358581523,81.7448482259304));
#223861=CARTESIAN_POINT('Ctrl Pts',(2.55647896775854,7.48654451240003,81.7449911890297));
#223862=CARTESIAN_POINT('Ctrl Pts',(2.54953076460418,7.48891370075458,81.7452889247662));
#223863=CARTESIAN_POINT('Ctrl Pts',(2.54592115754027,7.49014158721355,81.7454437202009));
#223864=CARTESIAN_POINT('Ctrl Pts',(2.53711168708902,7.49313121662858,81.7458218062986));
#223865=CARTESIAN_POINT('Ctrl Pts',(2.53191088156307,7.49489015462524,81.7460452685698));
#223866=CARTESIAN_POINT('Ctrl Pts',(2.5118890539416,7.50163841684503,81.7469065320414));
#223867=CARTESIAN_POINT('Ctrl Pts',(2.4970553860401,7.50658910167934,81.7475467264879));
#223868=CARTESIAN_POINT('Ctrl Pts',(2.23647118891562,7.59270031099475,81.7588290508521));
#223869=CARTESIAN_POINT('Ctrl Pts',(1.98691753267487,7.66179073754788,81.7701887889786));
#223870=CARTESIAN_POINT('Ctrl Pts',(1.69341242801769,7.72774511815841,81.7837912253489));
#223871=CARTESIAN_POINT('Ctrl Pts',(1.65230067566767,7.73663962438062,81.7857020905813));
#223872=CARTESIAN_POINT('Ctrl Pts',(1.61095367510114,7.74524042787896,81.7876281357673));
#223873=CARTESIAN_POINT('Ctrl Pts',(1.61078702816548,7.74527508735915,81.7876358986615));
#223874=CARTESIAN_POINT('Ctrl Pts',(1.61027838362078,7.74538085889022,81.7876595930001));
#223875=CARTESIAN_POINT('Ctrl Pts',(1.60993638246581,7.74545195365849,81.7876755248316));
#223876=CARTESIAN_POINT('Ctrl Pts',(1.60891396167713,7.74566442255782,81.7877231542983));
#223877=CARTESIAN_POINT('Ctrl Pts',(1.60823352819894,7.74580572966649,81.7877548534371));
#223878=CARTESIAN_POINT('Ctrl Pts',(1.60627654705985,7.74621187123596,81.7878460259853));
#223879=CARTESIAN_POINT('Ctrl Pts',(1.60499995277116,7.74647647974964,81.7879055044472));
#223880=CARTESIAN_POINT('Ctrl Pts',(1.60154968021547,7.74719075206476,81.7880662686424));
#223881=CARTESIAN_POINT('Ctrl Pts',(1.59937587860581,7.74763981648615,81.7881675676888));
#223882=CARTESIAN_POINT('Ctrl Pts',(1.59394343081634,7.74875966901115,81.788420747875));
#223883=CARTESIAN_POINT('Ctrl Pts',(1.59068455102749,7.74942931626785,81.7885726540629));
#223884=CARTESIAN_POINT('Ctrl Pts',(1.58311676995922,7.75097939840382,81.7889254688787));
#223885=CARTESIAN_POINT('Ctrl Pts',(1.57880755640599,7.7518582960204,81.789126410662));
#223886=CARTESIAN_POINT('Ctrl Pts',(1.56931133234322,7.7537868779784,81.7895693191143));
#223887=CARTESIAN_POINT('Ctrl Pts',(1.56412399828654,7.75483495148737,81.7898113196925));
#223888=CARTESIAN_POINT('Ctrl Pts',(1.5530331485394,7.7570642182638,81.7903288568955));
#223889=CARTESIAN_POINT('Ctrl Pts',(1.54712932940918,7.75824387891118,81.7906044248241));
#223890=CARTESIAN_POINT('Ctrl Pts',(1.53461513075224,7.7607295277699,81.7911886921897));
#223891=CARTESIAN_POINT('Ctrl Pts',(1.52800441885909,7.76203381196496,81.791497425244));
#223892=CARTESIAN_POINT('Ctrl Pts',(1.09765160112955,7.8463707388102,81.811601242663));
#223893=CARTESIAN_POINT('Ctrl Pts',(0.667820828851879,7.89458090532381,
81.8319728907238));
#223894=CARTESIAN_POINT('Ctrl Pts',(-0.0271539508753081,7.91533926038405,
81.8637145230358));
#223895=CARTESIAN_POINT('Ctrl Pts',(-0.290739402635426,7.91004548402641,
81.8754903903777));
#223896=CARTESIAN_POINT('Ctrl Pts',(-0.778609303229863,7.87582208437207,
81.8966102169183));
#223897=CARTESIAN_POINT('Ctrl Pts',(-1.0028658017784,7.85041897234444,81.9060521923009));
#223898=CARTESIAN_POINT('Ctrl Pts',(-1.24674586899656,7.81216984187532,
81.9160272586093));
#223899=CARTESIAN_POINT('Ctrl Pts',(-1.26773384431033,7.8087914436263,81.9168833484167));
#223900=CARTESIAN_POINT('Ctrl Pts',(-1.29781473948881,7.80382490156138,
81.9181069985101));
#223901=CARTESIAN_POINT('Ctrl Pts',(-1.30691879835144,7.80230539312487,
81.9184769006093));
#223902=CARTESIAN_POINT('Ctrl Pts',(-1.32268504658034,7.7996455657929,81.9191167345214));
#223903=CARTESIAN_POINT('Ctrl Pts',(-1.32934846189865,7.79851263713773,
81.9193869185405));
#223904=CARTESIAN_POINT('Ctrl Pts',(-1.34213685063274,7.79632146009281,
81.9199050066194));
#223905=CARTESIAN_POINT('Ctrl Pts',(-1.34826204245178,7.79526453047266,
81.9201529555133));
#223906=CARTESIAN_POINT('Ctrl Pts',(-1.36265548076988,7.79276340524096,
81.9207351428442));
#223907=CARTESIAN_POINT('Ctrl Pts',(-1.37092269549307,7.79131326625609,
81.9210691777513));
#223908=CARTESIAN_POINT('Ctrl Pts',(-1.39932843396219,7.78628404970597,
81.9222156805535));
#223909=CARTESIAN_POINT('Ctrl Pts',(-1.41945546002415,7.78264001316065,
81.9230259241));
#223910=CARTESIAN_POINT('Ctrl Pts',(-1.63773325234848,7.74224547781596,
81.9317903944476));
#223911=CARTESIAN_POINT('Ctrl Pts',(-1.8344318129604,7.69801290440657,81.9394828332048));
#223912=CARTESIAN_POINT('Ctrl Pts',(-2.68966166940109,7.47104552090079,
81.9722470607308));
#223913=CARTESIAN_POINT('Ctrl Pts',(-3.32453706002264,7.21097903172215,
81.9944509037068));
#223914=CARTESIAN_POINT('Ctrl Pts',(-4.09183705892401,6.77353533795482,
82.0247386285417));
#223915=CARTESIAN_POINT('Ctrl Pts',(-4.26173987697471,6.66794411905766,
82.0317167529024));
#223916=CARTESIAN_POINT('Ctrl Pts',(-4.54824429813732,6.47446057082404,
82.044274005449));
#223917=CARTESIAN_POINT('Ctrl Pts',(-4.66675292640679,6.38956798004194,
82.0497176262539));
#223918=CARTESIAN_POINT('Ctrl Pts',(-4.83103586247086,6.26487621872617,
82.0577285895207));
#223919=CARTESIAN_POINT('Ctrl Pts',(-4.87880620038059,6.22774688153805,
82.0601158307149));
#223920=CARTESIAN_POINT('Ctrl Pts',(-4.93309294665807,6.1845447555156,82.0629017841679));
#223921=CARTESIAN_POINT('Ctrl Pts',(-4.94003183833697,6.17900358377093,
82.0632592678746));
#223922=CARTESIAN_POINT('Ctrl Pts',(-4.95051747999784,6.17060114142821,
82.0638016008171));
#223923=CARTESIAN_POINT('Ctrl Pts',(-4.95407111546102,6.16774846673863,
82.0639857710088));
#223924=CARTESIAN_POINT('Ctrl Pts',(-4.96051487157396,6.16256659086966,
82.0643203957692));
#223925=CARTESIAN_POINT('Ctrl Pts',(-4.96340582233012,6.16023842239672,
82.0644707686589));
#223926=CARTESIAN_POINT('Ctrl Pts',(-4.96961807384124,6.15522829991797,
82.0647944253526));
#223927=CARTESIAN_POINT('Ctrl Pts',(-4.9729388428885,6.15254569172029,82.0649677604811));
#223928=CARTESIAN_POINT('Ctrl Pts',(-4.98185196334507,6.14533349843203,
82.0654338677595));
#223929=CARTESIAN_POINT('Ctrl Pts',(-4.98744029594451,6.14079897776614,
82.0657270244584));
#223930=CARTESIAN_POINT('Ctrl Pts',(-5.01285540452236,6.120118910123,82.0670644182324));
#223931=CARTESIAN_POINT('Ctrl Pts',(-5.03260980985598,6.10388509493277,
82.068115453591));
#223932=CARTESIAN_POINT('Ctrl Pts',(-5.36505351018126,5.82797793232107,
82.0859932118389));
#223933=CARTESIAN_POINT('Ctrl Pts',(-5.6573215476664,5.54470645178441,82.1045432310019));
#223934=CARTESIAN_POINT('Ctrl Pts',(-6.29108301346846,4.82795255213831,
82.149180758206));
#223935=CARTESIAN_POINT('Ctrl Pts',(-6.61167625526668,4.37866205571579,
82.1754013955193));
#223936=CARTESIAN_POINT('Ctrl Pts',(-7.052285985175,3.60098211660418,82.2154878805488));
#223937=CARTESIAN_POINT('Ctrl Pts',(-7.20192362117619,3.29152650347996,
82.2302808829215));
#223938=CARTESIAN_POINT('Ctrl Pts',(-7.34983305079788,2.92683930140138,
82.2463896059893));
#223939=CARTESIAN_POINT('Ctrl Pts',(-7.36823286280451,2.88020464142071,
82.2484260781635));
#223940=CARTESIAN_POINT('Ctrl Pts',(-7.39090328854906,2.82110667597188,
82.2509778313498));
#223941=CARTESIAN_POINT('Ctrl Pts',(-7.39558752059712,2.80880393145235,
82.251507467849));
#223942=CARTESIAN_POINT('Ctrl Pts',(-7.40300090621415,2.78918617846562,
82.2523495235542));
#223943=CARTESIAN_POINT('Ctrl Pts',(-7.40574996725616,2.78187874978493,
82.2526626312999));
#223944=CARTESIAN_POINT('Ctrl Pts',(-7.410911812419,2.76809589083751,82.2532521647126));
#223945=CARTESIAN_POINT('Ctrl Pts',(-7.41332693729977,2.76162134865589,
82.2535286709953));
#223946=CARTESIAN_POINT('Ctrl Pts',(-7.41874206089802,2.74704602367712,
82.2541501734305));
#223947=CARTESIAN_POINT('Ctrl Pts',(-7.42173728296416,2.73894346886283,
82.254495004814));
#223948=CARTESIAN_POINT('Ctrl Pts',(-7.42932948898273,2.71830143913055,
82.2553718045485));
#223949=CARTESIAN_POINT('Ctrl Pts',(-7.43390800975065,2.70575517641983,
82.2559031383485));
#223950=CARTESIAN_POINT('Ctrl Pts',(-7.45920301797278,2.63589183168084,
82.2588530913417));
#223951=CARTESIAN_POINT('Ctrl Pts',(-7.47928865541226,2.57834769465273,
82.261250098861));
#223952=CARTESIAN_POINT('Ctrl Pts',(-7.77234805148472,1.70649680452938,
82.2970931324115));
#223953=CARTESIAN_POINT('Ctrl Pts',(-7.91157906642316,0.853414248781925,
82.3251486570467));
#223954=CARTESIAN_POINT('Ctrl Pts',(-7.91077331315912,-0.3378085693112,
82.3672811834467));
#223955=CARTESIAN_POINT('Ctrl Pts',(-7.88959213361958,-0.669922515704042,
82.3794870143087));
#223956=CARTESIAN_POINT('Ctrl Pts',(-7.84479873300275,-1.02153659819372,
82.3936223337489));
#223957=CARTESIAN_POINT('Ctrl Pts',(-7.84193003947626,-1.04332996965621,
82.3945027533589));
#223958=CARTESIAN_POINT('Ctrl Pts',(-7.83788396125921,-1.07310817072276,
82.3957114153547));
#223959=CARTESIAN_POINT('Ctrl Pts',(-7.83678511378554,-1.08110370269847,
82.3960365037062));
#223960=CARTESIAN_POINT('Ctrl Pts',(-7.83489317745713,-1.09471551989898,
82.3965908824659));
#223961=CARTESIAN_POINT('Ctrl Pts',(-7.83410627899595,-1.10033266825351,
82.3968199288134));
#223962=CARTESIAN_POINT('Ctrl Pts',(-7.83257208771091,-1.11119917435111,
82.3972635465748));
#223963=CARTESIAN_POINT('Ctrl Pts',(-7.83182555668265,-1.11644863911374,
82.3974780883156));
#223964=CARTESIAN_POINT('Ctrl Pts',(-7.83004073379113,-1.1289092906493,
82.3979879008959));
#223965=CARTESIAN_POINT('Ctrl Pts',(-7.82899775775516,-1.13611979472033,
82.3982833514167));
#223966=CARTESIAN_POINT('Ctrl Pts',(-7.82588979960558,-1.15739882156305,
82.3991565465952));
#223967=CARTESIAN_POINT('Ctrl Pts',(-7.82379685209385,-1.17146318834051,
82.3997353455173));
#223968=CARTESIAN_POINT('Ctrl Pts',(-7.80717755231707,-1.28111162705549,
82.4042604073615));
#223969=CARTESIAN_POINT('Ctrl Pts',(-7.79093831936637,-1.37642564016029,
82.4082687695339));
#223970=CARTESIAN_POINT('Ctrl Pts',(-7.72630650776583,-1.71785212681102,
82.4228522917019));
#223971=CARTESIAN_POINT('Ctrl Pts',(-7.66796435740848,-1.96192317875596,
82.4336964550047));
#223972=CARTESIAN_POINT('Ctrl Pts',(-7.4223711763198,-2.80904870025764,
82.4721764003748));
#223973=CARTESIAN_POINT('Ctrl Pts',(-7.17466700541084,-3.39213933116439,
82.4999977809956));
#223974=CARTESIAN_POINT('Ctrl Pts',(-6.75825811163003,-4.11726198080747,
82.5349523138276));
#223975=CARTESIAN_POINT('Ctrl Pts',(-6.64936149261017,-4.29090844788996,
82.5433753329582));
#223976=CARTESIAN_POINT('Ctrl Pts',(-6.51427612181203,-4.48880074467213,
82.5530676090506));
#223977=CARTESIAN_POINT('Ctrl Pts',(-6.49452061189002,-4.51733633497682,
82.5544676689171));
#223978=CARTESIAN_POINT('Ctrl Pts',(-6.46504753216663,-4.55931535381337,
82.5565309620976));
#223979=CARTESIAN_POINT('Ctrl Pts',(-6.45547447802529,-4.57285964738681,
82.557197235464));
#223980=CARTESIAN_POINT('Ctrl Pts',(-6.43843094884148,-4.59681325202846,
82.558376561052));
#223981=CARTESIAN_POINT('Ctrl Pts',(-6.4309776560482,-4.60723469616784,
82.5588899836728));
#223982=CARTESIAN_POINT('Ctrl Pts',(-6.4153071872829,-4.62903355553002,
82.5599646293773));
#223983=CARTESIAN_POINT('Ctrl Pts',(-6.40708498356156,-4.64040730759268,
82.5605257390872));
#223984=CARTESIAN_POINT('Ctrl Pts',(-6.38547731826575,-4.67013022050076,
82.5619931399957));
#223985=CARTESIAN_POINT('Ctrl Pts',(-6.37204300111364,-4.68844375640407,
82.562898327873));
#223986=CARTESIAN_POINT('Ctrl Pts',(-6.31221779763707,-4.76926480087159,
82.5668978200427));
#223987=CARTESIAN_POINT('Ctrl Pts',(-6.2649842569111,-4.83114404586901,
82.5699724868492));
#223988=CARTESIAN_POINT('Ctrl Pts',(-5.7541423162739,-5.4802894499713,82.6023693136571));
#223989=CARTESIAN_POINT('Ctrl Pts',(-5.21040549354036,-5.99961446857308,
82.6289908979123));
#223990=CARTESIAN_POINT('Ctrl Pts',(-4.33742871092313,-6.62391840200282,
82.6683845693374));
#223991=CARTESIAN_POINT('Ctrl Pts',(-4.06163996236525,-6.79651639335913,
82.6805235458911));
#223992=CARTESIAN_POINT('Ctrl Pts',(-3.7599676482456,-6.96038065463423,
82.6942251026017));
#223993=CARTESIAN_POINT('Ctrl Pts',(-3.74386431908072,-6.96905556913394,
82.6949577583295));
#223994=CARTESIAN_POINT('Ctrl Pts',(-3.72163497689141,-6.98093130382919,
82.6959710565294));
#223995=CARTESIAN_POINT('Ctrl Pts',(-3.71553455623929,-6.98418010442027,
82.6962493362241));
#223996=CARTESIAN_POINT('Ctrl Pts',(-3.70508418523015,-6.98972791945096,
82.6967263988581));
#223997=CARTESIAN_POINT('Ctrl Pts',(-3.70073632720209,-6.9920308812205,
82.6969249844896));
#223998=CARTESIAN_POINT('Ctrl Pts',(-3.69227288228109,-6.99650367033614,
82.6973117555037));
#223999=CARTESIAN_POINT('Ctrl Pts',(-3.68815752419057,-6.99867392602734,
82.6974999190925));
#224000=CARTESIAN_POINT('Ctrl Pts',(-3.67830953709404,-7.00385621531218,
82.6979504261005));
#224001=CARTESIAN_POINT('Ctrl Pts',(-3.67257512548434,-7.00686483976604,
82.6982129429197));
#224002=CARTESIAN_POINT('Ctrl Pts',(-3.65536729800244,-7.01586619520672,
82.6990012909677));
#224003=CARTESIAN_POINT('Ctrl Pts',(-3.6438829015453,-7.02183778999953,
82.6995282115491));
#224004=CARTESIAN_POINT('Ctrl Pts',(-3.53080063714065,-7.0802855695115,
82.7047247516858));
#224005=CARTESIAN_POINT('Ctrl Pts',(-3.42810174862639,-7.1305757784351,
82.7095163738962));
#224006=CARTESIAN_POINT('Ctrl Pts',(-3.21542307986974,-7.22906539100864,
82.7195496061427));
#224007=CARTESIAN_POINT('Ctrl Pts',(-3.10536024016603,-7.27702328033204,
82.7247983650968));
#224008=CARTESIAN_POINT('Ctrl Pts',(-2.50267359694306,-7.5234701060025,
82.7536976899882));
#224009=CARTESIAN_POINT('Ctrl Pts',(-1.99210882143967,-7.67446935100861,
82.778659208289));
#224010=CARTESIAN_POINT('Ctrl Pts',(-0.946833949408674,-7.87217987137696,
82.8271596900419));
#224011=CARTESIAN_POINT('Ctrl Pts',(-0.414682023245925,-7.91807321898009,
82.8505449018719));
#224012=CARTESIAN_POINT('Ctrl Pts',(0.151558302360977,-7.90961886281755,
82.8736131146609));
#224013=CARTESIAN_POINT('Ctrl Pts',(0.185009860855236,-7.90890712171439,
82.8749696798301));
#224014=CARTESIAN_POINT('Ctrl Pts',(0.230794097781978,-7.90764234303347,
82.8768179816804));
#224015=CARTESIAN_POINT('Ctrl Pts',(0.243131256760908,-7.90727263565717,
82.8773151965656));
#224016=CARTESIAN_POINT('Ctrl Pts',(0.262700212086144,-7.90664037153556,
82.8781025546574));
#224017=CARTESIAN_POINT('Ctrl Pts',(0.269932576694688,-7.9063967627866,
82.8783932644828));
#224018=CARTESIAN_POINT('Ctrl Pts',(0.283950964554022,-7.90590532203296,
82.8789561934256));
#224019=CARTESIAN_POINT('Ctrl Pts',(0.290737021961011,-7.90565867563084,
82.8792284477929));
#224020=CARTESIAN_POINT('Ctrl Pts',(0.306885877416345,-7.90505090750927,
82.8798757426573));
#224021=CARTESIAN_POINT('Ctrl Pts',(0.316248377168858,-7.90468188839704,
82.8802505463851));
#224022=CARTESIAN_POINT('Ctrl Pts',(0.344024687195734,-7.90353766883258,
82.8813611034298));
#224023=CARTESIAN_POINT('Ctrl Pts',(0.362436523467322,-7.90271475128366,
82.882095427242));
#224024=CARTESIAN_POINT('Ctrl Pts',(0.510761194825826,-7.89556592808002,
82.8879966098208));
#224025=CARTESIAN_POINT('Ctrl Pts',(0.640506041467702,-7.88610120546517,
82.8930685798915));
#224026=CARTESIAN_POINT('Ctrl Pts',(1.08603635849855,-7.84253174683352,
82.9102141535868));
#224027=CARTESIAN_POINT('Ctrl Pts',(1.39997485186861,-7.79261632392008,
82.9218126748684));
#224028=CARTESIAN_POINT('Ctrl Pts',(1.97567957711024,-7.66515578786913,
82.9427285896526));
#224029=CARTESIAN_POINT('Ctrl Pts',(2.23807488375363,-7.59269042865542,
82.9521242474289));
#224030=CARTESIAN_POINT('Ctrl Pts',(2.7822979240428,-7.41172251067891,82.9719142542052));
#224031=CARTESIAN_POINT('Ctrl Pts',(3.06269904234073,-7.30032038348587,
82.9822910784481));
#224032=CARTESIAN_POINT('Ctrl Pts',(3.60758530853732,-7.04690912909354,
83.0037826169518));
#224033=CARTESIAN_POINT('Ctrl Pts',(3.8717289957021,-6.90531092995292,83.0149021430282));
#224034=CARTESIAN_POINT('Ctrl Pts',(4.1453031290591,-6.73801398379112,83.0276694023004));
#224035=CARTESIAN_POINT('Ctrl Pts',(4.1633454950578,-6.72688075969151,83.028516896351));
#224036=CARTESIAN_POINT('Ctrl Pts',(4.18823199666722,-6.71138581832311,
83.0296932621845));
#224037=CARTESIAN_POINT('Ctrl Pts',(4.19511459772902,-6.70708583302821,
83.0300193821187));
#224038=CARTESIAN_POINT('Ctrl Pts',(4.20691627733504,-6.69968732357613,
83.03057991696));
#224039=CARTESIAN_POINT('Ctrl Pts',(4.21183858729832,-6.69659394860776,
83.0308141068948));
#224040=CARTESIAN_POINT('Ctrl Pts',(4.22143209266467,-6.6905502472934,83.0312713118254));
#224041=CARTESIAN_POINT('Ctrl Pts',(4.22610361662003,-6.68760044753913,
83.0314943040955));
#224042=CARTESIAN_POINT('Ctrl Pts',(4.23730904450276,-6.68050843209629,
83.0320300413071));
#224043=CARTESIAN_POINT('Ctrl Pts',(4.24383996404174,-6.67636152474065,
83.0323429852616));
#224044=CARTESIAN_POINT('Ctrl Pts',(4.26354620584603,-6.66380814615335,
83.0332893405968));
#224045=CARTESIAN_POINT('Ctrl Pts',(4.27670266951694,-6.65537223081037,
83.0339239760548));
#224046=CARTESIAN_POINT('Ctrl Pts',(4.40033962514064,-6.57557830868276,
83.0399139586767));
#224047=CARTESIAN_POINT('Ctrl Pts',(4.50904673191947,-6.50151632875985,
83.0453764135102));
#224048=CARTESIAN_POINT('Ctrl Pts',(4.81775263480765,-6.27972803232172,
83.061368059381));
#224049=CARTESIAN_POINT('Ctrl Pts',(5.01269815945171,-6.12524096805037,
83.0720649522018));
#224050=CARTESIAN_POINT('Ctrl Pts',(5.49539747835406,-5.7042202377735,83.0997192224108));
#224051=CARTESIAN_POINT('Ctrl Pts',(5.77121007323627,-5.42500431346597,
83.1166648191338));
#224052=CARTESIAN_POINT('Ctrl Pts',(6.2832098679501,-4.82324834506387,83.1501402722954));
#224053=CARTESIAN_POINT('Ctrl Pts',(6.51796769969943,-4.50095162963353,
83.1666099030009));
#224054=CARTESIAN_POINT('Ctrl Pts',(6.82855019362817,-3.99896638413514,
83.1907340465467));
#224055=CARTESIAN_POINT('Ctrl Pts',(6.92364858310609,-3.83196057614499,
83.1985522584594));
#224056=CARTESIAN_POINT('Ctrl Pts',(7.03452778330465,-3.61961182303977,
83.2082383304687));
#224057=CARTESIAN_POINT('Ctrl Pts',(7.05610389450611,-3.57736896889967,
83.2101529161304));
#224058=CARTESIAN_POINT('Ctrl Pts',(7.08959355692613,-3.51031925443538,
83.2131725775974));
#224059=CARTESIAN_POINT('Ctrl Pts',(7.10175978056362,-3.48563998356122,
83.2142799568727));
#224060=CARTESIAN_POINT('Ctrl Pts',(7.12332588765428,-3.44131133771696,
83.2162617613255));
#224061=CARTESIAN_POINT('Ctrl Pts',(7.13277383303186,-3.42168567731919,
83.2171366351646));
#224062=CARTESIAN_POINT('Ctrl Pts',(7.15465770366415,-3.37574308283499,
83.2191787923347));
#224063=CARTESIAN_POINT('Ctrl Pts',(7.16702968930932,-3.34939601377875,
83.2203454429381));
#224064=CARTESIAN_POINT('Ctrl Pts',(7.20091579904378,-3.27618553159718,
83.2235749298959));
#224065=CARTESIAN_POINT('Ctrl Pts',(7.22211761118548,-3.2291790334804,83.2256346217858));
#224066=CARTESIAN_POINT('Ctrl Pts',(7.36620075273548,-2.90121418707225,
83.2399112293772));
#224067=CARTESIAN_POINT('Ctrl Pts',(7.47311635429268,-2.61352176066586,
83.2519484734084));
#224068=CARTESIAN_POINT('Ctrl Pts',(7.67367808667517,-1.95979955702333,
83.2785494734345));
#224069=CARTESIAN_POINT('Ctrl Pts',(7.75836933962422,-1.5918080378604,83.2930178503985));
#224070=CARTESIAN_POINT('Ctrl Pts',(7.85153372898945,-0.994508137693976,
83.3165228182334));
#224071=CARTESIAN_POINT('Ctrl Pts',(7.87687360764529,-0.76843067980944,
83.3254296696135));
#224072=CARTESIAN_POINT('Ctrl Pts',(7.89425818301156,-0.515086468564058,
83.3355914905457));
#224073=CARTESIAN_POINT('Ctrl Pts',(7.8959428886597,-0.488581843384374,
83.3366568372539));
#224074=CARTESIAN_POINT('Ctrl Pts',(7.89825431245943,-0.449075964246679,
83.3382484730032));
#224075=CARTESIAN_POINT('Ctrl Pts',(7.89898246499564,-0.436080751931087,
83.3387726290335));
#224076=CARTESIAN_POINT('Ctrl Pts',(7.90019066843466,-0.413521584896281,
83.3396836335847));
#224077=CARTESIAN_POINT('Ctrl Pts',(7.90068543116149,-0.403958433553598,
83.3400701614623));
#224078=CARTESIAN_POINT('Ctrl Pts',(7.90163211961558,-0.384992801212348,
83.3408374222254));
#224079=CARTESIAN_POINT('Ctrl Pts',(7.90208462927214,-0.375590364586619,
83.3412181414479));
#224080=CARTESIAN_POINT('Ctrl Pts',(7.90324148151608,-0.350624856639488,
83.3422299693235));
#224081=CARTESIAN_POINT('Ctrl Pts',(7.90391663223043,-0.335060554196697,
83.3428617450956));
#224082=CARTESIAN_POINT('Ctrl Pts',(7.9064881195928,-0.271439889146017,
83.3454483171678));
#224083=CARTESIAN_POINT('Ctrl Pts',(7.90799216933934,-0.223369143930525,
83.3474121728015));
#224084=CARTESIAN_POINT('Ctrl Pts',(7.91658069307538,0.164147980571805,
83.3633103526081));
#224085=CARTESIAN_POINT('Ctrl Pts',(7.90224410556563,0.503710038774721,
83.3776387815922));
#224086=CARTESIAN_POINT('Ctrl Pts',(7.81439987833045,1.32506035679555,83.4124861127088));
#224087=CARTESIAN_POINT('Ctrl Pts',(7.7181407126294,1.80304461020453,83.4328809339111));
#224088=CARTESIAN_POINT('Ctrl Pts',(7.55765683534286,2.33903039394703,83.4556716194591));
#224089=CARTESIAN_POINT('Ctrl Pts',(7.53577208895681,2.40860523768575,83.4586301650926));
#224090=CARTESIAN_POINT('Ctrl Pts',(7.50445571268423,2.50355690193685,83.4626696701596));
#224091=CARTESIAN_POINT('Ctrl Pts',(7.49585142908382,2.5292022586484,83.4637608858997));
#224092=CARTESIAN_POINT('Ctrl Pts',(7.48091545657614,2.57297367792859,83.4656238310926));
#224093=CARTESIAN_POINT('Ctrl Pts',(7.47464901457149,2.59112171216366,83.4663963617202));
#224094=CARTESIAN_POINT('Ctrl Pts',(7.46166049499911,2.62829810204554,83.4679792393806));
#224095=CARTESIAN_POINT('Ctrl Pts',(7.45493154605436,2.64732391338453,83.4687894955948));
#224096=CARTESIAN_POINT('Ctrl Pts',(7.43920460010276,2.69125568777074,83.4706609431245));
#224097=CARTESIAN_POINT('Ctrl Pts',(7.43015419298055,2.71614265716186,83.471721486329));
#224098=CARTESIAN_POINT('Ctrl Pts',(7.40220261246189,2.79181916922449,83.4749478519308));
#224099=CARTESIAN_POINT('Ctrl Pts',(7.38290431375928,2.84246050722346,83.4771088742181));
#224100=CARTESIAN_POINT('Ctrl Pts',(7.1747808307712,3.37218205102407,83.4997442403497));
#224101=CARTESIAN_POINT('Ctrl Pts',(6.9401150812684,3.83196190948123,83.5197918389516));
#224102=CARTESIAN_POINT('Ctrl Pts',(6.25104012678044,4.90820965896344,83.5686855664903));
#224103=CARTESIAN_POINT('Ctrl Pts',(5.74889553623901,5.48781111356882,83.5961851812145));
#224104=CARTESIAN_POINT('Ctrl Pts',(5.14831676399449,6.00663829463994,83.6270070190922));
#224105=CARTESIAN_POINT('Ctrl Pts',(5.1248987834675,6.0266310276842,83.6282068501316));
#224106=CARTESIAN_POINT('Ctrl Pts',(5.06348481828428,6.07844542350151,83.6313495925962));
#224107=CARTESIAN_POINT('Ctrl Pts',(5.02530570382728,6.11004744310652,83.6332995480799));
#224108=CARTESIAN_POINT('Ctrl Pts',(4.95557042497136,6.16667369841242,83.6368583374995));
#224109=CARTESIAN_POINT('Ctrl Pts',(4.92411519212769,6.19181978533826,83.6384625545024));
#224110=CARTESIAN_POINT('Ctrl Pts',(4.88267009232263,6.22443646260455,83.6405764886028));
#224111=CARTESIAN_POINT('Ctrl Pts',(4.8728523575697,6.23212535230677,83.6410772657497));
#224112=CARTESIAN_POINT('Ctrl Pts',(4.85766769709547,6.24395960364342,83.6418518785545));
#224113=CARTESIAN_POINT('Ctrl Pts',(4.85231353058334,6.2481213486893,83.6421250256679));
#224114=CARTESIAN_POINT('Ctrl Pts',(4.84163945601494,6.2563962148506,83.6426696153642));
#224115=CARTESIAN_POINT('Ctrl Pts',(4.83631964183338,6.26050944739533,83.6429410527959));
#224116=CARTESIAN_POINT('Ctrl Pts',(4.8246388371033,6.26951716719819,83.6435371118081));
#224117=CARTESIAN_POINT('Ctrl Pts',(4.81827563348594,6.27440876397808,83.6438618577877));
#224118=CARTESIAN_POINT('Ctrl Pts',(4.80010063547729,6.28833650976067,83.6447895561835));
#224119=CARTESIAN_POINT('Ctrl Pts',(4.78827082394726,6.29734902031241,83.6453935455298));
#224120=CARTESIAN_POINT('Ctrl Pts',(4.76180404865713,6.31739496778729,83.6467453569093));
#224121=CARTESIAN_POINT('Ctrl Pts',(4.74715403669076,6.32841097920356,83.6474939635037));
#224122=CARTESIAN_POINT('Ctrl Pts',(4.70181287381567,6.36225902863544,83.6498123002648));
#224123=CARTESIAN_POINT('Ctrl Pts',(4.67099458592989,6.38491924435384,83.6513900814732));
#224124=CARTESIAN_POINT('Ctrl Pts',(4.55854858534755,6.46634925450629,83.6571581378105));
#224125=CARTESIAN_POINT('Ctrl Pts',(4.4759739579674,6.52377901991802,83.6614207117391));
#224126=CARTESIAN_POINT('Ctrl Pts',(4.14493139596264,6.74477173448362,83.6785862126986));
#224127=CARTESIAN_POINT('Ctrl Pts',(3.88842867827139,6.89583250529151,83.6920230123419));
#224128=CARTESIAN_POINT('Ctrl Pts',(3.04749100116697,7.32921712540238,83.7352395680662));
#224129=CARTESIAN_POINT('Ctrl Pts',(2.43649411675311,7.55435760765001,83.7652022853264));
#224130=CARTESIAN_POINT('Ctrl Pts',(1.63809467658986,7.74144014381819,83.8000002643202));
#224131=CARTESIAN_POINT('Ctrl Pts',(1.47012438352523,7.77508769754772,83.8071066567348));
#224132=CARTESIAN_POINT('Ctrl Pts',(1.28053940133635,7.80670084080667,83.8148896763576));
#224133=CARTESIAN_POINT('Ctrl Pts',(1.25987814557453,7.8100618591148,83.8157347551638));
#224134=CARTESIAN_POINT('Ctrl Pts',(1.2304892191868,7.81472297229582,83.816932396698));
#224135=CARTESIAN_POINT('Ctrl Pts',(1.22177242510334,7.81609051854859,83.8172870675629));
#224136=CARTESIAN_POINT('Ctrl Pts',(1.20577640991618,7.81857266245478,83.8179369091646));
#224137=CARTESIAN_POINT('Ctrl Pts',(1.19849789029871,7.81969168421257,83.8182322180597));
#224138=CARTESIAN_POINT('Ctrl Pts',(1.18374433515528,7.82193885795055,83.8188300360461));
#224139=CARTESIAN_POINT('Ctrl Pts',(1.17626922318441,7.82306646165835,83.8191325277064));
#224140=CARTESIAN_POINT('Ctrl Pts',(1.15786330295216,7.82581597562434,83.8198763648368));
#224141=CARTESIAN_POINT('Ctrl Pts',(1.14693067603073,7.82742570314811,83.8203173285272));
#224142=CARTESIAN_POINT('Ctrl Pts',(1.10706399198377,7.83321038429453,83.8219222331473));
#224143=CARTESIAN_POINT('Ctrl Pts',(1.07811006236087,7.83724787942993,83.8230818668319));
#224144=CARTESIAN_POINT('Ctrl Pts',(0.662326208235594,7.89287931993071,
83.8396501980792));
#224145=CARTESIAN_POINT('Ctrl Pts',(0.272203034349274,7.91594391967045,
83.8541129800971));
#224146=CARTESIAN_POINT('Ctrl Pts',(-0.616048464188318,7.90268624582155,
83.8856154149718));
#224147=CARTESIAN_POINT('Ctrl Pts',(-1.11220543198012,7.84824572459026,
83.9021693582787));
#224148=CARTESIAN_POINT('Ctrl Pts',(-1.73247216290351,7.7201536336102,83.9239588351184));
#224149=CARTESIAN_POINT('Ctrl Pts',(-1.864267496859,7.68939122006654,83.9286588253206));
#224150=CARTESIAN_POINT('Ctrl Pts',(-2.24164075069757,7.59103569760671,
83.9424610574042));
#224151=CARTESIAN_POINT('Ctrl Pts',(-2.48481384750551,7.5149490078564,83.9517803870244));
#224152=CARTESIAN_POINT('Ctrl Pts',(-2.7754075646578,7.40837677864145,83.9638670844904));
#224153=CARTESIAN_POINT('Ctrl Pts',(-2.82673977489904,7.38894279485918,
83.9660391564227));
#224154=CARTESIAN_POINT('Ctrl Pts',(-2.88612109598342,7.36575214005795,
83.9685991231355));
#224155=CARTESIAN_POINT('Ctrl Pts',(-2.89437226758516,7.36251375176632,
83.9689559029708));
#224156=CARTESIAN_POINT('Ctrl Pts',(-2.90748101629529,7.35734343825061,
83.9695244445711));
#224157=CARTESIAN_POINT('Ctrl Pts',(-2.91234216869083,7.35542054682404,
83.9697356550837));
#224158=CARTESIAN_POINT('Ctrl Pts',(-2.92089020079191,7.35202946020039,
83.9701077239152));
#224159=CARTESIAN_POINT('Ctrl Pts',(-2.92457789302919,7.35056330468839,
83.9702684565481));
#224160=CARTESIAN_POINT('Ctrl Pts',(-2.93217207143489,7.34753738588908,
83.9705999123453));
#224161=CARTESIAN_POINT('Ctrl Pts',(-2.93607841908332,7.34597728082528,
83.9707706566976));
#224162=CARTESIAN_POINT('Ctrl Pts',(-2.94394586398515,7.34282792703042,
83.971115041016));
#224163=CARTESIAN_POINT('Ctrl Pts',(-2.9479069227592,7.3412385869593,83.9712886866683));
#224164=CARTESIAN_POINT('Ctrl Pts',(-2.95751917116754,7.33737272262775,
83.971710698124));
#224165=CARTESIAN_POINT('Ctrl Pts',(-2.96316902220273,7.33509287360441,
83.9719592737827));
#224166=CARTESIAN_POINT('Ctrl Pts',(-3.01179712076684,7.31540492893928,
83.9741033386373));
#224167=CARTESIAN_POINT('Ctrl Pts',(-3.054623313679,7.29762614879642,83.9760223703351));
#224168=CARTESIAN_POINT('Ctrl Pts',(-3.18473579924077,7.24226553128536,
83.9819405886828));
#224169=CARTESIAN_POINT('Ctrl Pts',(-3.2715011616058,7.20348741774783,83.9860086356401));
#224170=CARTESIAN_POINT('Ctrl Pts',(-3.52134392085782,7.08638012351287,
83.9980281507908));
#224171=CARTESIAN_POINT('Ctrl Pts',(-3.68245547971792,7.00401041396173,
84.0061625001843));
#224172=CARTESIAN_POINT('Ctrl Pts',(-3.9726999178255,6.84283639324876,84.0213320101033));
#224173=CARTESIAN_POINT('Ctrl Pts',(-4.10267489034448,6.76570852137468,
84.0283248803467));
#224174=CARTESIAN_POINT('Ctrl Pts',(-4.86806100040528,6.2813550632928,84.070392995994));
#224175=CARTESIAN_POINT('Ctrl Pts',(-5.44488931594817,5.78852936302091,
84.1053048693084));
#224176=CARTESIAN_POINT('Ctrl Pts',(-5.97525459222509,5.18484483300554,
84.1381433884286));
#224177=CARTESIAN_POINT('Ctrl Pts',(-6.00699727577083,5.1480352788246,84.140114567468));
#224178=CARTESIAN_POINT('Ctrl Pts',(-6.04688416521127,5.10091025063367,
84.1425992260308));
#224179=CARTESIAN_POINT('Ctrl Pts',(-6.0553442597492,5.09086430684931,84.1431266775751));
#224180=CARTESIAN_POINT('Ctrl Pts',(-6.0687093849896,5.07491343039701,84.1439606630954));
#224181=CARTESIAN_POINT('Ctrl Pts',(-6.07363088646257,5.06902236934853,
84.1442679223739));
#224182=CARTESIAN_POINT('Ctrl Pts',(-6.08277139370409,5.05804871509945,
84.1448388778819));
#224183=CARTESIAN_POINT('Ctrl Pts',(-6.08699262068158,5.05296798608959,
84.1451026716101));
#224184=CARTESIAN_POINT('Ctrl Pts',(-6.09632412366518,5.04170779395371,
84.1456860807374));
#224185=CARTESIAN_POINT('Ctrl Pts',(-6.1014313809285,5.03552583200022,84.1460055637652));
#224186=CARTESIAN_POINT('Ctrl Pts',(-6.11610244324625,5.01771249258475,
84.1469238186304));
#224187=CARTESIAN_POINT('Ctrl Pts',(-6.12564247458783,5.00606152893751,
84.1475215516014));
#224188=CARTESIAN_POINT('Ctrl Pts',(-6.1885796777465,4.92874885477668,84.1514691463573));
#224189=CARTESIAN_POINT('Ctrl Pts',(-6.24095446927867,4.86225992822554,
84.1547744897285));
#224190=CARTESIAN_POINT('Ctrl Pts',(-6.38804443069569,4.66923833814942,
84.1641249129226));
#224191=CARTESIAN_POINT('Ctrl Pts',(-6.48004983869782,4.54068891678361,
84.1700568376414));
#224192=CARTESIAN_POINT('Ctrl Pts',(-6.7520430594211,4.13553968877194,84.1879523586286));
#224193=CARTESIAN_POINT('Ctrl Pts',(-6.91863003999255,3.85037005191991,
84.1994267418065));
#224194=CARTESIAN_POINT('Ctrl Pts',(-7.12439989321341,3.44139470085532,
84.2150183840971));
#224195=CARTESIAN_POINT('Ctrl Pts',(-7.17909309925279,3.32579222176747,
84.2193376615019));
#224196=CARTESIAN_POINT('Ctrl Pts',(-7.25663207896628,3.15106606429279,
84.2257896634228));
#224197=CARTESIAN_POINT('Ctrl Pts',(-7.28160858365655,3.09291171788683,
84.2279247968904));
#224198=CARTESIAN_POINT('Ctrl Pts',(-7.33224290043826,2.97100271693194,
84.2323851086089));
#224199=CARTESIAN_POINT('Ctrl Pts',(-7.35777316287724,2.90720090731082,
84.2347106803973));
#224200=CARTESIAN_POINT('Ctrl Pts',(-7.48318454524311,2.5815515024007,84.2465690620951));
#224201=CARTESIAN_POINT('Ctrl Pts',(-7.56992767889091,2.31487327588627,
84.2562367340625));
#224202=CARTESIAN_POINT('Ctrl Pts',(-7.65001962945739,2.0154416681411,84.2675843648592));
#224203=CARTESIAN_POINT('Ctrl Pts',(-7.65754211608016,1.98666911158072,
84.268679769749));
#224204=CARTESIAN_POINT('Ctrl Pts',(-7.70236406505108,1.81119348197654,
84.2753945642773));
#224205=CARTESIAN_POINT('Ctrl Pts',(-7.73560683611332,1.66349502048231,
84.2811916657058));
#224206=CARTESIAN_POINT('Ctrl Pts',(-7.76693080147547,1.50294918398679,
84.2877395926663));
#224207=CARTESIAN_POINT('Ctrl Pts',(-7.76924307459088,1.490950156478,84.2882304575188));
#224208=CARTESIAN_POINT('Ctrl Pts',(-7.77242525392877,1.47422852080638,
84.2889166405472));
#224209=CARTESIAN_POINT('Ctrl Pts',(-7.77331868524816,1.46951035281488,
84.2891104890733));
#224210=CARTESIAN_POINT('Ctrl Pts',(-7.77485735096298,1.46134406554483,
84.289446415832));
#224211=CARTESIAN_POINT('Ctrl Pts',(-7.77550458508005,1.4578963450964,84.2895883667165));
#224212=CARTESIAN_POINT('Ctrl Pts',(-7.77684481387798,1.45073086507197,
84.2898836470429));
#224213=CARTESIAN_POINT('Ctrl Pts',(-7.77753743613674,1.44701303774437,
84.2900369996036));
#224214=CARTESIAN_POINT('Ctrl Pts',(-7.77915872442144,1.43827556454946,
84.2903977417281));
#224215=CARTESIAN_POINT('Ctrl Pts',(-7.7800851972655,1.43325551886765,84.2906052666353));
#224216=CARTESIAN_POINT('Ctrl Pts',(-7.78202190883545,1.42270433491175,
84.2910419927238));
#224217=CARTESIAN_POINT('Ctrl Pts',(-7.78303111062175,1.41717301164568,
84.2912712571515));
#224218=CARTESIAN_POINT('Ctrl Pts',(-7.78573793332209,1.40224711579425,
84.2918907557057));
#224219=CARTESIAN_POINT('Ctrl Pts',(-7.78742444213325,1.39285056506307,
84.2922816610334));
#224220=CARTESIAN_POINT('Ctrl Pts',(-7.8698932032324,0.928535663717718,
84.3116413221783));
#224221=CARTESIAN_POINT('Ctrl Pts',(-7.91067346782161,0.467472541057296,
84.3329021201673));
#224222=CARTESIAN_POINT('Ctrl Pts',(-7.91099804691657,0.00555892815145176,
84.354531530966));
#224223=CARTESIAN_POINT('',(-7.91099985457727,0.00151686464269769,86.3576684917632));
#224224=CARTESIAN_POINT('Ctrl Pts',(-7.91099794240846,0.00570571723741387,
84.3576684917632));
#224225=CARTESIAN_POINT('Ctrl Pts',(-7.91113604848863,-0.185778871053852,
84.3653996801986));
#224226=CARTESIAN_POINT('Ctrl Pts',(-7.90431775442304,-0.377536863908371,
84.3731308686339));
#224227=CARTESIAN_POINT('Ctrl Pts',(-7.89051010449761,-0.56900904282895,
84.3808620570693));
#224228=CARTESIAN_POINT('Ctrl Pts',(-7.87671499291532,-0.76030735118546,
84.3885862250273));
#224229=CARTESIAN_POINT('Ctrl Pts',(-7.85594318587293,-0.951320004677742,
84.3963103929853));
#224230=CARTESIAN_POINT('Ctrl Pts',(-7.82821373839945,-1.14148616545889,
84.4040345609433));
#224231=CARTESIAN_POINT('Ctrl Pts',(-7.80050379262063,-1.33151858529892,
84.4117532966126));
#224232=CARTESIAN_POINT('Ctrl Pts',(-7.76584600076575,-1.52070534188531,
84.4194720322819));
#224233=CARTESIAN_POINT('Ctrl Pts',(-7.72431137276304,-1.70848904491763,
84.4271907679511));
#224234=CARTESIAN_POINT('Ctrl Pts',(-7.68197768574935,-1.89988540243222,
84.4350579996004));
#224235=CARTESIAN_POINT('Ctrl Pts',(-7.63249989493742,-2.0898237926873,
84.4429252312498));
#224236=CARTESIAN_POINT('Ctrl Pts',(-7.57600833561745,-2.27772226108779,
84.4507924628991));
#224237=CARTESIAN_POINT('Ctrl Pts',(-7.52062078331188,-2.4619486547641,
84.4585059462888));
#224238=CARTESIAN_POINT('Ctrl Pts',(-7.45849118039364,-2.64421376180912,
84.4662194296786));
#224239=CARTESIAN_POINT('Ctrl Pts',(-7.38979331569571,-2.82398225052831,
84.4739329130683));
#224240=CARTESIAN_POINT('Ctrl Pts',(-7.32109843615863,-3.00374292768225,
84.4816460612804));
#224241=CARTESIAN_POINT('Ctrl Pts',(-7.24583599174336,-3.18100686477606,
84.4893592094926));
#224242=CARTESIAN_POINT('Ctrl Pts',(-7.16422858305065,-3.35525704079435,
84.4970723577047));
#224243=CARTESIAN_POINT('Ctrl Pts',(-7.08260961283277,-3.52953190326976,
84.5047865986577));
#224244=CARTESIAN_POINT('Ctrl Pts',(-6.9946440423981,-3.70079182754728,
84.5125008396108));
#224245=CARTESIAN_POINT('Ctrl Pts',(-6.90060125580291,-3.86854278875279,
84.5202150805638));
#224246=CARTESIAN_POINT('Ctrl Pts',(-6.80328894119551,-4.04212584497161,
84.5281975178114));
#224247=CARTESIAN_POINT('Ctrl Pts',(-6.69946944564072,-4.21195119241786,
84.536179955059));
#224248=CARTESIAN_POINT('Ctrl Pts',(-6.58949077703927,-4.37750297536329,
84.5441623923065));
#224249=CARTESIAN_POINT('Ctrl Pts',(-6.48306975367048,-4.53769940604956,
84.5518866096631));
#224250=CARTESIAN_POINT('Ctrl Pts',(-6.37088206819916,-4.69389417900211,
84.5596108270196));
#224251=CARTESIAN_POINT('Ctrl Pts',(-6.25328460762502,-4.84565296075153,
84.5673350443762));
#224252=CARTESIAN_POINT('Ctrl Pts',(-6.12979023826714,-5.00502166612291,
84.5754465915692));
#224253=CARTESIAN_POINT('Ctrl Pts',(-6.00032990717017,-5.15949770095725,
84.5835581387623));
#224254=CARTESIAN_POINT('Ctrl Pts',(-5.8653609453887,-5.3086214764578,84.5916696859554));
#224255=CARTESIAN_POINT('Ctrl Pts',(-5.73039198360722,-5.45774525195836,
84.5997812331484));
#224256=CARTESIAN_POINT('Ctrl Pts',(-5.58991475892938,-5.6015164931973,
84.6078927803415));
#224257=CARTESIAN_POINT('Ctrl Pts',(-5.4444264966568,-5.739524468325,84.6160043275345));
#224258=CARTESIAN_POINT('Ctrl Pts',(-5.29028986392483,-5.88573615746103,
84.6245980556542));
#224259=CARTESIAN_POINT('Ctrl Pts',(-5.13016600954508,-6.02582518548657,
84.633191783774));
#224260=CARTESIAN_POINT('Ctrl Pts',(-4.96454415718908,-6.15931995526453,
84.6417855118937));
#224261=CARTESIAN_POINT('Ctrl Pts',(-4.7991614341823,-6.29262198165163,
84.6503668321543));
#224262=CARTESIAN_POINT('Ctrl Pts',(-4.62829674783593,-6.41934859482711,
84.658948152415));
#224263=CARTESIAN_POINT('Ctrl Pts',(-4.45247390254535,-6.53906699362781,
84.6675294726756));
#224264=CARTESIAN_POINT('Ctrl Pts',(-4.26904727864673,-6.66396283224461,
84.6764819077325));
#224265=CARTESIAN_POINT('Ctrl Pts',(-4.08022430269794,-6.78123065431066,
84.6854343427895));
#224266=CARTESIAN_POINT('Ctrl Pts',(-3.88663929913602,-6.89042494759296,
84.6943867778465));
#224267=CARTESIAN_POINT('Ctrl Pts',(-3.70181026101123,-6.99468031771324,
84.702934288914));
#224268=CARTESIAN_POINT('Ctrl Pts',(-3.5126406794845,-7.09157613834774,
84.7114817999816));
#224269=CARTESIAN_POINT('Ctrl Pts',(-3.31971423384642,-7.18076725744523,
84.7200293110491));
#224270=CARTESIAN_POINT('Ctrl Pts',(-3.12708439685608,-7.26982125248418,
84.7285636810167));
#224271=CARTESIAN_POINT('Ctrl Pts',(-2.930709442653,-7.35119407246323,84.7370980509843));
#224272=CARTESIAN_POINT('Ctrl Pts',(-2.73119816444677,-7.42458602122183,
84.745632420952));
#224273=CARTESIAN_POINT('Ctrl Pts',(-2.53212126793053,-7.49781817891989,
84.754148209644));
#224274=CARTESIAN_POINT('Ctrl Pts',(-2.32992190578842,-7.56310405227874,
84.762663998336));
#224275=CARTESIAN_POINT('Ctrl Pts',(-2.12522945593439,-7.62019164848423,
84.771179787028));
#224276=CARTESIAN_POINT('Ctrl Pts',(-2.09495182995846,-7.62863591150911,
84.7724394224717));
#224277=CARTESIAN_POINT('Ctrl Pts',(-2.06461969657883,-7.63690088298914,
84.7736990579155));
#224278=CARTESIAN_POINT('Ctrl Pts',(-2.03423513389271,-7.64498583517566,
84.7749586933592));
#224279=CARTESIAN_POINT('Ctrl Pts',(-1.8438052755895,-7.69565683923694,
84.782853235122));
#224280=CARTESIAN_POINT('Ctrl Pts',(-1.65149082274922,-7.73920588467801,
84.7907477768848));
#224281=CARTESIAN_POINT('Ctrl Pts',(-1.45786565126126,-7.77550954876094,
84.7986423186475));
#224282=CARTESIAN_POINT('Ctrl Pts',(-1.26419684484369,-7.8118213941553,
84.8065386395063));
#224283=CARTESIAN_POINT('Ctrl Pts',(-1.06921706769643,-7.84088454089397,
84.8144349603651));
#224284=CARTESIAN_POINT('Ctrl Pts',(-0.873508646527078,-7.8626270192883,
84.8223312812239));
#224285=CARTESIAN_POINT('Ctrl Pts',(-0.67772385586492,-7.88437798204952,
84.8302306833912));
#224286=CARTESIAN_POINT('Ctrl Pts',(-0.481210194663697,-7.89880254565144,
84.8381300855585));
#224287=CARTESIAN_POINT('Ctrl Pts',(-0.284553626403908,-7.90588073738153,
84.8460294877258));
#224288=CARTESIAN_POINT('Ctrl Pts',(-0.0876806601074991,-7.91296671785119,
84.8539375822807));
#224289=CARTESIAN_POINT('Ctrl Pts',(0.109335184935045,-7.91269016399037,
84.8618456768356));
#224290=CARTESIAN_POINT('Ctrl Pts',(0.305908196360126,-7.90508324911254,
84.8697537713905));
#224291=CARTESIAN_POINT('Ctrl Pts',(0.502598322842411,-7.89747180215646,
84.8776665774617));
#224292=CARTESIAN_POINT('Ctrl Pts',(0.698844748872493,-7.88252131195011,
84.8855793835329));
#224293=CARTESIAN_POINT('Ctrl Pts',(0.89406802737253,-7.86031572918227,
84.8934921896041));
#224294=CARTESIAN_POINT('Ctrl Pts',(1.08956487888816,-7.83807902897655,
84.9014160841594));
#224295=CARTESIAN_POINT('Ctrl Pts',(1.28403537992718,-7.80856697254367,
84.9093399787147));
#224296=CARTESIAN_POINT('Ctrl Pts',(1.47691003068571,-7.77191467794519,
84.91726387327));
#224297=CARTESIAN_POINT('Ctrl Pts',(1.61199536850572,-7.74624418377584,
84.922813601908));
#224298=CARTESIAN_POINT('Ctrl Pts',(1.74629814737207,-7.71707224984252,
84.928363330546));
#224299=CARTESIAN_POINT('Ctrl Pts',(1.87962762946362,-7.68445970609235,
84.9339130591839));
#224300=CARTESIAN_POINT('Ctrl Pts',(2.07481455226748,-7.63671676162467,
84.9420375522686));
#224301=CARTESIAN_POINT('Ctrl Pts',(2.26834439119837,-7.58149306887894,
84.9501620453533));
#224302=CARTESIAN_POINT('Ctrl Pts',(2.45962225138909,-7.51892142401234,
84.958286538438));
#224303=CARTESIAN_POINT('Ctrl Pts',(2.65073111809408,-7.45640506102918,
84.9664038535545));
#224304=CARTESIAN_POINT('Ctrl Pts',(2.83959166948251,-7.38655378831354,
84.974521168671));
#224305=CARTESIAN_POINT('Ctrl Pts',(3.02562192866049,-7.3095508032169,84.9826384837875));
#224306=CARTESIAN_POINT('Ctrl Pts',(3.21151431841751,-7.23260488602423,
84.9907497830571));
#224307=CARTESIAN_POINT('Ctrl Pts',(3.39458030307072,-7.14851794693131,
84.9988610823268));
#224308=CARTESIAN_POINT('Ctrl Pts',(3.57425518234388,-7.05752229124981,
85.0069723815965));
#224309=CARTESIAN_POINT('Ctrl Pts',(3.75382245118213,-6.96658113446165,
85.0150788228669));
#224310=CARTESIAN_POINT('Ctrl Pts',(3.93000237929859,-6.86873965682307,
85.0231852641373));
#224311=CARTESIAN_POINT('Ctrl Pts',(4.10225177013506,-6.76427759738051,
85.0312917054076));
#224312=CARTESIAN_POINT('Ctrl Pts',(4.27442246418287,-6.65986326425253,
85.0393944430313));
#224313=CARTESIAN_POINT('Ctrl Pts',(4.44266592860689,-6.54883454786702,
85.0474971806549));
#224314=CARTESIAN_POINT('Ctrl Pts',(4.60646453285016,-6.43151657912763,
85.0555999182785));
#224315=CARTESIAN_POINT('Ctrl Pts',(4.77174236002558,-6.31313914208254,
85.063775829635));
#224316=CARTESIAN_POINT('Ctrl Pts',(4.93249436129339,-6.18835846000633,
85.0719517409914));
#224317=CARTESIAN_POINT('Ctrl Pts',(5.08821866783614,-6.05755328398222,
85.0801276523479));
#224318=CARTESIAN_POINT('Ctrl Pts',(5.2424904198382,-5.92796822353672,85.0882273009973));
#224319=CARTESIAN_POINT('Ctrl Pts',(5.39182763156347,-5.79247080162955,
85.0963269496468));
#224320=CARTESIAN_POINT('Ctrl Pts',(5.53577535425382,-5.65146991739635,
85.1044265982962));
#224321=CARTESIAN_POINT('Ctrl Pts',(5.67972209868514,-5.51046999139567,
85.112526191901));
#224322=CARTESIAN_POINT('Ctrl Pts',(5.81827919810207,-5.36396690215908,
85.1206257855058));
#224323=CARTESIAN_POINT('Ctrl Pts',(5.95102817406918,-5.21240680218216,
85.1287253791106));
#224324=CARTESIAN_POINT('Ctrl Pts',(6.08379338683677,-5.06082816457747,
85.1368259633933));
#224325=CARTESIAN_POINT('Ctrl Pts',(6.21074884848166,-4.90419152427333,
85.144926547676));
#224326=CARTESIAN_POINT('Ctrl Pts',(6.33151567088062,-4.74297694590572,
85.1530271319588));
#224327=CARTESIAN_POINT('Ctrl Pts',(6.45425493476013,-4.57912930727102,
85.1612600201983));
#224328=CARTESIAN_POINT('Ctrl Pts',(6.57060144306575,-4.4105531653976,85.1694929084379));
#224329=CARTESIAN_POINT('Ctrl Pts',(6.68020258790092,-4.23778413614967,
85.1777257966775));
#224330=CARTESIAN_POINT('Ctrl Pts',(6.78814540013673,-4.06762920836751,
85.1858341162643));
#224331=CARTESIAN_POINT('Ctrl Pts',(6.88954538753533,-3.89340767100451,
85.193942435851));
#224332=CARTESIAN_POINT('Ctrl Pts',(6.98411140464275,-3.71565726185005,
85.2020507554378));
#224333=CARTESIAN_POINT('Ctrl Pts',(7.08085665776017,-3.53381066566912,
85.2103459280038));
#224334=CARTESIAN_POINT('Ctrl Pts',(7.17044901172711,-3.34827091383366,
85.2186411005697));
#224335=CARTESIAN_POINT('Ctrl Pts',(7.25262812550995,-3.15963704767841,
85.2269362731357));
#224336=CARTESIAN_POINT('Ctrl Pts',(7.3348072392928,-2.97100318152317,85.2352314457016));
#224337=CARTESIAN_POINT('Ctrl Pts',(7.40957300812188,-2.7792755437729,85.2435266182676));
#224338=CARTESIAN_POINT('Ctrl Pts',(7.47671889352995,-2.58507167930259,
85.2518217908336));
#224339=CARTESIAN_POINT('Ctrl Pts',(7.54008315516352,-2.40180528250461,
85.2596497832946));
#224340=CARTESIAN_POINT('Ctrl Pts',(7.59678305044347,-2.21598231132712,
85.2674777757557));
#224341=CARTESIAN_POINT('Ctrl Pts',(7.64660662407232,-2.02813415155245,
85.2753057682167));
#224342=CARTESIAN_POINT('Ctrl Pts',(7.69638811586044,-1.84044465153988,
85.2831271490217));
#224343=CARTESIAN_POINT('Ctrl Pts',(7.73930476051446,-1.65073370680453,
85.2909485298267));
#224344=CARTESIAN_POINT('Ctrl Pts',(7.77519342645454,-1.45955067785194,
85.2987699106317));
#224345=CARTESIAN_POINT('Ctrl Pts',(7.81105811794983,-1.26849536350931,
85.3065860665765));
#224346=CARTESIAN_POINT('Ctrl Pts',(7.83990411592811,-1.07597026803862,
85.3144022225213));
#224347=CARTESIAN_POINT('Ctrl Pts',(7.86161864288046,-0.88253799573413,
85.3222183784661));
#224348=CARTESIAN_POINT('Ctrl Pts',(7.88332273809248,-0.689198649019919,
85.3300307795002));
#224349=CARTESIAN_POINT('Ctrl Pts',(7.89790214722644,-0.494953342733305,
85.3378431805343));
#224350=CARTESIAN_POINT('Ctrl Pts',(7.90529550428984,-0.30037308443819,
85.3456555815685));
#224351=CARTESIAN_POINT('Ctrl Pts',(7.91268670035618,-0.105849699815022,
85.3534656991236));
#224352=CARTESIAN_POINT('Ctrl Pts',(7.91289601589372,0.0890080901747599,
85.3612758166787));
#224353=CARTESIAN_POINT('Ctrl Pts',(7.90591407798284,0.283625794935357,
85.3690859342338));
#224354=CARTESIAN_POINT('Ctrl Pts',(7.89893174226187,0.478254588434868,
85.3768964967862));
#224355=CARTESIAN_POINT('Ctrl Pts',(7.8847573406027,0.672642917142711,85.3847070593387));
#224356=CARTESIAN_POINT('Ctrl Pts',(7.86343361833381,0.866217484271463,
85.3925176218911));
#224357=CARTESIAN_POINT('Ctrl Pts',(7.846817660913,1.01705544420197,85.3986038001468));
#224358=CARTESIAN_POINT('Ctrl Pts',(7.82586175405752,1.16739927011033,85.4046899784025));
#224359=CARTESIAN_POINT('Ctrl Pts',(7.80060791314723,1.31698032838185,85.4107761566583));
#224360=CARTESIAN_POINT('Ctrl Pts',(7.76475578734917,1.52933610179506,85.4194165226615));
#224361=CARTESIAN_POINT('Ctrl Pts',(7.72025736249287,1.74005315430232,85.4280568886648));
#224362=CARTESIAN_POINT('Ctrl Pts',(7.66729613795211,1.94845860437031,85.4366972546681));
#224363=CARTESIAN_POINT('Ctrl Pts',(7.61424681291079,2.15721073495082,85.4453519938392));
#224364=CARTESIAN_POINT('Ctrl Pts',(7.55270660496586,2.36364335393564,85.4540067330103));
#224365=CARTESIAN_POINT('Ctrl Pts',(7.48290875299718,2.56709906203835,85.4626614721814));
#224366=CARTESIAN_POINT('Ctrl Pts',(7.41095212923674,2.77684743432968,85.4715838930399));
#224367=CARTESIAN_POINT('Ctrl Pts',(7.33021903219875,2.98343155973446,85.4805063138983));
#224368=CARTESIAN_POINT('Ctrl Pts',(7.24101746202913,3.18615553835483,85.4894287347568));
#224369=CARTESIAN_POINT('Ctrl Pts',(7.15420168632371,3.3834574403791,85.4981125156199));
#224370=CARTESIAN_POINT('Ctrl Pts',(7.05936472485675,3.57710283796482,85.506796296483));
#224371=CARTESIAN_POINT('Ctrl Pts',(6.95683702361201,3.76647575684501,85.5154800773461));
#224372=CARTESIAN_POINT('Ctrl Pts',(6.8500829587818,3.96365494465266,85.5245218182023));
#224373=CARTESIAN_POINT('Ctrl Pts',(6.734990861555,4.15620173043621,85.5335635590584));
#224374=CARTESIAN_POINT('Ctrl Pts',(6.61198423995321,4.34345316661874,85.5426052999146));
#224375=CARTESIAN_POINT('Ctrl Pts',(6.48897761835143,4.53070460280126,85.5516470407707));
#224376=CARTESIAN_POINT('Ctrl Pts',(6.35805665142987,4.71266047486259,85.5606887816269));
#224377=CARTESIAN_POINT('Ctrl Pts',(6.21969377629556,4.88869413331519,85.569730522483));
#224378=CARTESIAN_POINT('Ctrl Pts',(6.09234496111341,5.05071503534079,85.5780525162555));
#224379=CARTESIAN_POINT('Ctrl Pts',(5.9585836531275,5.20785666569505,85.5863745100281));
#224380=CARTESIAN_POINT('Ctrl Pts',(5.81880209117596,5.35961409279869,85.5946965038006));
#224381=CARTESIAN_POINT('Ctrl Pts',(5.67914485336173,5.51123654422353,85.603011095848));
#224382=CARTESIAN_POINT('Ctrl Pts',(5.53347824063766,5.65748413123612,85.6113256878954));
#224383=CARTESIAN_POINT('Ctrl Pts',(5.38223448981308,5.79788520899358,85.6196402799428));
#224384=CARTESIAN_POINT('Ctrl Pts',(5.23111603421675,5.93816997394481,85.6279479839125));
#224385=CARTESIAN_POINT('Ctrl Pts',(5.07442987155089,6.07261769380693,85.6362556878822));
#224386=CARTESIAN_POINT('Ctrl Pts',(4.91264539316631,6.20079319450358,85.6445633918519));
#224387=CARTESIAN_POINT('Ctrl Pts',(4.75102414802908,6.32883937189666,85.6528627137227));
#224388=CARTESIAN_POINT('Ctrl Pts',(4.5843150835293,6.4506257809609,85.6611620355935));
#224389=CARTESIAN_POINT('Ctrl Pts',(4.41302127921891,6.56575693954331,85.6694613574643));
#224390=CARTESIAN_POINT('Ctrl Pts',(4.24183691465861,6.68081454073539,85.6777553768917));
#224391=CARTESIAN_POINT('Ctrl Pts',(4.06607389509714,6.78922521017799,85.686049396319));
#224392=CARTESIAN_POINT('Ctrl Pts',(3.88626610731897,6.8906354382672,85.6943434157464));
#224393=CARTESIAN_POINT('Ctrl Pts',(3.70659165595874,6.99197046562834,85.7026312847458));
#224394=CARTESIAN_POINT('Ctrl Pts',(3.52287867679531,7.0863152689388,85.7109191537452));
#224395=CARTESIAN_POINT('Ctrl Pts',(3.33568806308976,7.17336086822352,85.7192070227446));
#224396=CARTESIAN_POINT('Ctrl Pts',(3.26433206588753,7.2065421555545,85.7223663112657));
#224397=CARTESIAN_POINT('Ctrl Pts',(3.19247100940407,7.23866326756346,85.7255255997868));
#224398=CARTESIAN_POINT('Ctrl Pts',(3.12013692538982,7.26970883645411,85.7286848883079));
#224399=CARTESIAN_POINT('Ctrl Pts',(2.93462896820803,7.34932828754603,85.7367871981343));
#224400=CARTESIAN_POINT('Ctrl Pts',(2.74608624849957,7.42183683932858,85.7448895079607));
#224401=CARTESIAN_POINT('Ctrl Pts',(2.5550838464558,7.48701993703641,85.7529918177871));
#224402=CARTESIAN_POINT('Ctrl Pts',(2.36403928567685,7.55221742219133,85.7610959159844));
#224403=CARTESIAN_POINT('Ctrl Pts',(2.170534261616,7.61008612551288,85.7692000141818));
#224404=CARTESIAN_POINT('Ctrl Pts',(1.97515980724869,7.66046113075638,85.7773041123791));
#224405=CARTESIAN_POINT('Ctrl Pts',(1.77971772182673,7.7108535738719,85.7854110159007));
#224406=CARTESIAN_POINT('Ctrl Pts',(1.58240522414939,7.7537470657263,85.7935179194223));
#224407=CARTESIAN_POINT('Ctrl Pts',(1.38382490644727,7.78902751492741,85.8016248229439));
#224408=CARTESIAN_POINT('Ctrl Pts',(1.18506549931651,7.8243397817606,85.809739037667));
#224409=CARTESIAN_POINT('Ctrl Pts',(0.985036301616426,7.852025230093,85.8178532523902));
#224410=CARTESIAN_POINT('Ctrl Pts',(0.784347771465897,7.8720213143383,85.8259674671133));
#224411=CARTESIAN_POINT('Ctrl Pts',(0.583561158362665,7.89202717131443,
85.8340856475147));
#224412=CARTESIAN_POINT('Ctrl Pts',(0.382114887803085,7.90433614324904,
85.8422038279161));
#224413=CARTESIAN_POINT('Ctrl Pts',(0.180621766553604,7.90893777807406,
85.8503220083174));
#224414=CARTESIAN_POINT('Ctrl Pts',(-0.0210880415602115,7.9135443615237,
85.8584489190568));
#224415=CARTESIAN_POINT('Ctrl Pts',(-0.222844482137192,7.91042704530252,
85.8665758297962));
#224416=CARTESIAN_POINT('Ctrl Pts',(-0.424036111522702,7.89962748337697,
85.8747027405356));
#224417=CARTESIAN_POINT('Ctrl Pts',(-0.530789191201968,7.89389719281637,
85.8790149117346));
#224418=CARTESIAN_POINT('Ctrl Pts',(-0.637383339135011,7.88600491528602,
85.8833270829335));
#224419=CARTESIAN_POINT('Ctrl Pts',(-0.743728062832032,7.87596277089704,
85.8876392541325));
#224420=CARTESIAN_POINT('Ctrl Pts',(-0.940965729908816,7.85733759549695,
85.895637042436));
#224421=CARTESIAN_POINT('Ctrl Pts',(-1.13768722476516,7.83128161932807,
85.9036348307394));
#224422=CARTESIAN_POINT('Ctrl Pts',(-1.33329998644681,7.79783509354622,
85.9116326190429));
#224423=CARTESIAN_POINT('Ctrl Pts',(-1.52875303054633,7.764415876812,85.9196238771619));
#224424=CARTESIAN_POINT('Ctrl Pts',(-1.72309881744133,7.72361819231812,
85.927615135281));
#224425=CARTESIAN_POINT('Ctrl Pts',(-1.91574988369583,7.67553407803779,
85.9356063934));
#224426=CARTESIAN_POINT('Ctrl Pts',(-2.10827631892025,7.62748107063275,
85.9435924817645));
#224427=CARTESIAN_POINT('Ctrl Pts',(-2.29910989511405,7.57215110917399,
85.9515785701289));
#224428=CARTESIAN_POINT('Ctrl Pts',(-2.48767291357099,7.50968737532297,
85.9595646584934));
#224429=CARTESIAN_POINT('Ctrl Pts',(-2.67614590701011,7.44725346332567,
85.9675469340861));
#224430=CARTESIAN_POINT('Ctrl Pts',(-2.86235018657887,7.37769267290381,
85.9755292096789));
#224431=CARTESIAN_POINT('Ctrl Pts',(-3.04572240669765,7.30119825928182,
85.9835114852716));
#224432=CARTESIAN_POINT('Ctrl Pts',(-3.22903815125117,7.224727404655,85.9914913024575));
#224433=CARTESIAN_POINT('Ctrl Pts',(-3.40952326682269,7.14132731276972,
85.9994711196433));
#224434=CARTESIAN_POINT('Ctrl Pts',(-3.58663323146954,7.05123982452153,
86.0074509368292));
#224435=CARTESIAN_POINT('Ctrl Pts',(-3.76982958233562,6.95805647857785,
86.0157049805356));
#224436=CARTESIAN_POINT('Ctrl Pts',(-3.94941433989758,6.85771808629206,
86.0239590242419));
#224437=CARTESIAN_POINT('Ctrl Pts',(-4.12481074975638,6.75054496160822,
86.0322130679483));
#224438=CARTESIAN_POINT('Ctrl Pts',(-4.29440284545406,6.64691846872714,
86.0401939643148));
#224439=CARTESIAN_POINT('Ctrl Pts',(-4.46007907286651,6.53690255942615,
86.0481748606813));
#224440=CARTESIAN_POINT('Ctrl Pts',(-4.6213459701,6.42083191063592,86.0561557570479));
#224441=CARTESIAN_POINT('Ctrl Pts',(-4.78264867064435,6.30473549267923,
86.0641384252753));
#224442=CARTESIAN_POINT('Ctrl Pts',(-4.93953981750619,6.18258185067508,
86.0721210935028));
#224443=CARTESIAN_POINT('Ctrl Pts',(-5.09155724222624,6.0547473811162,86.0801037617302));
#224444=CARTESIAN_POINT('Ctrl Pts',(-5.24363178438832,5.92686488036671,
86.0880894292822));
#224445=CARTESIAN_POINT('Ctrl Pts',(-5.39082869761023,5.7932975121146,86.0960750968341));
#224446=CARTESIAN_POINT('Ctrl Pts',(-5.53272075889855,5.65446036364683,
86.1040607643861));
#224447=CARTESIAN_POINT('Ctrl Pts',(-5.67468794819326,5.51554970466632,
86.1120506601329));
#224448=CARTESIAN_POINT('Ctrl Pts',(-5.81134444700214,5.37136393659938,
86.1200405558797));
#224449=CARTESIAN_POINT('Ctrl Pts',(-5.94230133112456,5.22235348191936,
86.1280304516265));
#224450=CARTESIAN_POINT('Ctrl Pts',(-6.07341334448758,5.07316651205398,
86.1360298120645));
#224451=CARTESIAN_POINT('Ctrl Pts',(-6.19881203488972,4.91914368996471,
86.1440291725025));
#224452=CARTESIAN_POINT('Ctrl Pts',(-6.31814929029164,4.76076785251993,
86.1520285329404));
#224453=CARTESIAN_POINT('Ctrl Pts',(-6.43756996916001,4.60228130143995,
86.1600334853821));
#224454=CARTESIAN_POINT('Ctrl Pts',(-6.55092057149521,4.43943593975026,
86.1680384378238));
#224455=CARTESIAN_POINT('Ctrl Pts',(-6.65789719176911,4.27274220891374,
86.1760433902654));
#224456=CARTESIAN_POINT('Ctrl Pts',(-6.7650134252622,4.10583092915557,86.1840587898233));
#224457=CARTESIAN_POINT('Ctrl Pts',(-6.86573889120565,3.9350615352411,86.1920741893811));
#224458=CARTESIAN_POINT('Ctrl Pts',(-6.95981580439282,3.76096862110334,
86.200089588939));
#224459=CARTESIAN_POINT('Ctrl Pts',(-6.98117091057466,3.72145018304063,
86.2019090545533));
#224460=CARTESIAN_POINT('Ctrl Pts',(-7.00218363185694,3.68176057224964,
86.2037285201677));
#224461=CARTESIAN_POINT('Ctrl Pts',(-7.02285130238581,3.64190617459841,
86.205547985782));
#224462=CARTESIAN_POINT('Ctrl Pts',(-7.11591107381369,3.46245483630463,
86.2137404453026));
#224463=CARTESIAN_POINT('Ctrl Pts',(-7.20222462229796,3.27917296624159,
86.2219329048231));
#224464=CARTESIAN_POINT('Ctrl Pts',(-7.28147094893788,3.09258820727457,
86.2301253643437));
#224465=CARTESIAN_POINT('Ctrl Pts',(-7.36057633600453,2.90633528925743,
86.2383032535769));
#224466=CARTESIAN_POINT('Ctrl Pts',(-7.43263943396914,2.71679147092681,
86.2464811428101));
#224467=CARTESIAN_POINT('Ctrl Pts',(-7.49738407016285,2.52451046828258,
86.2546590320433));
#224468=CARTESIAN_POINT('Ctrl Pts',(-7.56534486261059,2.32267800646674,
86.2632431536867));
#224469=CARTESIAN_POINT('Ctrl Pts',(-7.62524141955897,2.11782974578302,
86.27182727533));
#224470=CARTESIAN_POINT('Ctrl Pts',(-7.67680871449751,1.91063574786381,
86.2804113969733));
#224471=CARTESIAN_POINT('Ctrl Pts',(-7.72574556083931,1.71401071932198,
86.2885576424248));
#224472=CARTESIAN_POINT('Ctrl Pts',(-7.76718150490366,1.51527364761672,
86.2967038878763));
#224473=CARTESIAN_POINT('Ctrl Pts',(-7.80093890573647,1.31501832267354,
86.3048501333278));
#224474=CARTESIAN_POINT('Ctrl Pts',(-7.83465351447246,1.11501684859099,
86.3129860523052));
#224475=CARTESIAN_POINT('Ctrl Pts',(-7.86070892734315,0.913501258557734,
86.3211219712826));
#224476=CARTESIAN_POINT('Ctrl Pts',(-7.87897754926956,0.711079305075185,
86.3292578902601));
#224477=CARTESIAN_POINT('Ctrl Pts',(-7.89721819453409,0.508967341616738,
86.3373813498492));
#224478=CARTESIAN_POINT('Ctrl Pts',(-7.90769580288915,0.305952088394149,
86.3455048094383));
#224479=CARTESIAN_POINT('Ctrl Pts',(-7.91033399567166,0.102650265081471,
86.3536282690274));
#224480=CARTESIAN_POINT('Ctrl Pts',(-7.91077136624201,0.0689460433861521,
86.3549750099394));
#224481=CARTESIAN_POINT('Ctrl Pts',(-7.91099338961968,0.0352339657993602,
86.3563217508513));
#224482=CARTESIAN_POINT('Ctrl Pts',(-7.91099985457727,0.00151686464269769,
86.3576684917632));
#224483=CARTESIAN_POINT('',(-7.91729508967814,0.000522195832882638,90.3577115106449));
#224484=CARTESIAN_POINT('Ctrl Pts',(-7.91099999344164,0.00032212781326103,
86.3656351409683));
#224485=CARTESIAN_POINT('Ctrl Pts',(-7.91100080997057,-0.0197306589497159,
86.3664459662309));
#224486=CARTESIAN_POINT('Ctrl Pts',(-7.91092538186667,-0.0397834962520868,
86.3672542192267));
#224487=CARTESIAN_POINT('Ctrl Pts',(-7.910713182016,-0.0678379502749371,
86.3683814149145));
#224488=CARTESIAN_POINT('Ctrl Pts',(-7.91064051456589,-0.0758398671859283,
86.3687025162124));
#224489=CARTESIAN_POINT('Ctrl Pts',(-7.91048823017332,-0.0902080694887452,
86.3692783568725));
#224490=CARTESIAN_POINT('Ctrl Pts',(-7.91041306906146,-0.0965743889316467,
86.3695332462364));
#224491=CARTESIAN_POINT('Ctrl Pts',(-7.91024521821163,-0.10947265626111,
86.3700491384557));
#224492=CARTESIAN_POINT('Ctrl Pts',(-7.91015212300533,-0.11600459432782,
86.3703101274322));
#224493=CARTESIAN_POINT('Ctrl Pts',(-7.90994949763443,-0.12908459942319,
86.3708322128475));
#224494=CARTESIAN_POINT('Ctrl Pts',(-7.90983992698668,-0.13563266078522,
86.3710933077157));
#224495=CARTESIAN_POINT('Ctrl Pts',(-7.90951205263652,-0.153872809060541,
86.3718198602508));
#224496=CARTESIAN_POINT('Ctrl Pts',(-7.90927595439742,-0.165564582518292,
86.3722847176708));
#224497=CARTESIAN_POINT('Ctrl Pts',(-7.90822827504168,-0.212311202249965,
86.3741399323737));
#224498=CARTESIAN_POINT('Ctrl Pts',(-7.90720955481084,-0.247361266830406,
86.3755233005311));
#224499=CARTESIAN_POINT('Ctrl Pts',(-7.89911209452814,-0.474051554622186,
86.3844220510694));
#224500=CARTESIAN_POINT('Ctrl Pts',(-7.88529988808621,-0.665393730805927,
86.3917072471893));
#224501=CARTESIAN_POINT('Ctrl Pts',(-7.78440005472862,-1.59235766819493,
86.4261284881292));
#224502=CARTESIAN_POINT('Ctrl Pts',(-7.60127252092226,-2.31366250068811,
86.4497912572859));
#224503=CARTESIAN_POINT('Ctrl Pts',(-7.22302588665172,-3.23696937748152,
86.4845111112983));
#224504=CARTESIAN_POINT('Ctrl Pts',(-7.1139809506084,-3.4700620689676,86.4937436339693));
#224505=CARTESIAN_POINT('Ctrl Pts',(-6.955967207387,-3.76895068721524,86.5067314190248));
#224506=CARTESIAN_POINT('Ctrl Pts',(-6.91705291563581,-3.83990197187149,
86.5099035065655));
#224507=CARTESIAN_POINT('Ctrl Pts',(-6.8723717250825,-3.91848411764104,
86.5135314146414));
#224508=CARTESIAN_POINT('Ctrl Pts',(-6.86767018701722,-3.92671836381037,
86.5139129874863));
#224509=CARTESIAN_POINT('Ctrl Pts',(-6.86062750466591,-3.93900153808379,
86.5144843429472));
#224510=CARTESIAN_POINT('Ctrl Pts',(-6.85829755248642,-3.94305687963214,
86.5146733307154));
#224511=CARTESIAN_POINT('Ctrl Pts',(-6.85428205350724,-3.95003163214844,
86.5149989748387));
#224512=CARTESIAN_POINT('Ctrl Pts',(-6.85259823684805,-3.95295203212586,
86.5151355080476));
#224513=CARTESIAN_POINT('Ctrl Pts',(-6.84912343505769,-3.95896981205482,
86.5154172237893));
#224514=CARTESIAN_POINT('Ctrl Pts',(-6.8473322148897,-3.96206705398455,
86.5155624228958));
#224515=CARTESIAN_POINT('Ctrl Pts',(-6.84300977062074,-3.96952941046667,
86.5159127516772));
#224516=CARTESIAN_POINT('Ctrl Pts',(-6.84047647320407,-3.97389331520969,
86.5161180267254));
#224517=CARTESIAN_POINT('Ctrl Pts',(-6.83116963763305,-3.98989017249295,
86.5168719909511));
#224518=CARTESIAN_POINT('Ctrl Pts',(-6.82437062156164,-4.00150819339113,
86.5174224513293));
#224519=CARTESIAN_POINT('Ctrl Pts',(-6.71307412918163,-4.19058069675694,
86.5264269311842));
#224520=CARTESIAN_POINT('Ctrl Pts',(-6.6017239104728,-4.36389265796386,
86.5353450064085));
#224521=CARTESIAN_POINT('Ctrl Pts',(-6.4662798921334,-4.55763919649667,
86.5459111944932));
#224522=CARTESIAN_POINT('Ctrl Pts',(-6.44866584843267,-4.582527624766,86.5472802400863));
#224523=CARTESIAN_POINT('Ctrl Pts',(-6.38906597817513,-4.66571738887227,
86.551894151413));
#224524=CARTESIAN_POINT('Ctrl Pts',(-6.34643046391109,-4.72354769588965,
86.5551644431527));
#224525=CARTESIAN_POINT('Ctrl Pts',(-5.86818333086136,-5.35407099606345,
86.5914512676185));
#224526=CARTESIAN_POINT('Ctrl Pts',(-5.35707603827227,-5.86546037841427,
86.6262947345837));
#224527=CARTESIAN_POINT('Ctrl Pts',(-4.61599112944313,-6.42813970254441,
86.6675129438308));
#224528=CARTESIAN_POINT('Ctrl Pts',(-4.44307230151566,-6.54885272425989,
86.6766128403462));
#224529=CARTESIAN_POINT('Ctrl Pts',(-4.19836059940411,-6.70552384023978,
86.6887830503198));
#224530=CARTESIAN_POINT('Ctrl Pts',(-4.13054533756924,-6.74750897920067,
86.6920845387099));
#224531=CARTESIAN_POINT('Ctrl Pts',(-4.03496585602683,-6.80470218490236,
86.6966406039261));
#224532=CARTESIAN_POINT('Ctrl Pts',(-4.00772900570744,-6.82077924676423,
86.69792810286));
#224533=CARTESIAN_POINT('Ctrl Pts',(-3.9604061292534,-6.84833113615353,
86.7001465755725));
#224534=CARTESIAN_POINT('Ctrl Pts',(-3.94036494183646,-6.85988193750319,
86.7010804007526));
#224535=CARTESIAN_POINT('Ctrl Pts',(-3.91179639207971,-6.87618100647102,
86.7024035470075));
#224536=CARTESIAN_POINT('Ctrl Pts',(-3.9033105573464,-6.8810015942932,86.7027955659575));
#224537=CARTESIAN_POINT('Ctrl Pts',(-3.8891691281601,-6.88900040489715,
86.7034471977288));
#224538=CARTESIAN_POINT('Ctrl Pts',(-3.88351851744834,-6.89218738942948,
86.7037071361753));
#224539=CARTESIAN_POINT('Ctrl Pts',(-3.87170709452342,-6.8988299783935,
86.7042495680634));
#224540=CARTESIAN_POINT('Ctrl Pts',(-3.86554556041542,-6.90228428980156,
86.7045320134045));
#224541=CARTESIAN_POINT('Ctrl Pts',(-3.85195975473014,-6.90987693763166,
86.7051536485966));
#224542=CARTESIAN_POINT('Ctrl Pts',(-3.84453341844849,-6.91401157363263,
86.7054927014495));
#224543=CARTESIAN_POINT('Ctrl Pts',(-3.81860505733569,-6.92839257894107,
86.7066738746354));
#224544=CARTESIAN_POINT('Ctrl Pts',(-3.80006854091723,-6.93857675646127,
86.707513702498));
#224545=CARTESIAN_POINT('Ctrl Pts',(-3.61453636789031,-7.03954379494797,
86.7158740809038));
#224546=CARTESIAN_POINT('Ctrl Pts',(-3.44435556272662,-7.12435756566815,
86.723173608394));
#224547=CARTESIAN_POINT('Ctrl Pts',(-2.95562501459095,-7.34631803580239,
86.7432488431515));
#224548=CARTESIAN_POINT('Ctrl Pts',(-2.63088044060601,-7.46877469895862,
86.7555445586615));
#224549=CARTESIAN_POINT('Ctrl Pts',(-2.09279555569682,-7.63221021107031,
86.7750967370254));
#224550=CARTESIAN_POINT('Ctrl Pts',(-1.88397665847125,-7.68642037077053,
86.7824985683819));
#224551=CARTESIAN_POINT('Ctrl Pts',(-1.61016904236078,-7.74567209629457,
86.7921876548449));
#224552=CARTESIAN_POINT('Ctrl Pts',(-1.54696916739977,-7.75854154443141,
86.7944231853528));
#224553=CARTESIAN_POINT('Ctrl Pts',(-1.2828972574553,-7.8089598292688,86.8037816813999));
#224554=CARTESIAN_POINT('Ctrl Pts',(-1.08077156150081,-7.83949020440895,
86.8109859434624));
#224555=CARTESIAN_POINT('Ctrl Pts',(-0.721487165227515,-7.87959917684714,
86.8241745858946));
#224556=CARTESIAN_POINT('Ctrl Pts',(-0.564798054676068,-7.89237769646901,
86.8300543409894));
#224557=CARTESIAN_POINT('Ctrl Pts',(-0.332450052560969,-7.90437200046374,
86.8390880587341));
#224558=CARTESIAN_POINT('Ctrl Pts',(-0.257010673168978,-7.90718436597017,
86.8420704654145));
#224559=CARTESIAN_POINT('Ctrl Pts',(-0.168197491439732,-7.90922302448745,
86.8456320271209));
#224560=CARTESIAN_POINT('Ctrl Pts',(-0.154849381716239,-7.9094956168707,
86.846168649934));
#224561=CARTESIAN_POINT('Ctrl Pts',(-0.134398957736245,-7.90986146345503,
86.8469928014412));
#224562=CARTESIAN_POINT('Ctrl Pts',(-0.127297062045217,-7.90997894488089,
86.8472793771911));
#224563=CARTESIAN_POINT('Ctrl Pts',(-0.114347507489207,-7.91017571543004,
86.8478025820219));
#224564=CARTESIAN_POINT('Ctrl Pts',(-0.108499895419027,-7.91025808516443,
86.8480390918719));
#224565=CARTESIAN_POINT('Ctrl Pts',(-0.0967427837715226,-7.91041065691015,
86.8485151053803));
#224566=CARTESIAN_POINT('Ctrl Pts',(-0.0908332862093388,-7.91048072123581,
86.8487546141378));
#224567=CARTESIAN_POINT('Ctrl Pts',(-0.0740218888743161,-7.91066120016003,
86.8494366716147));
#224568=CARTESIAN_POINT('Ctrl Pts',(-0.0631198552882879,-7.91075570006669,
86.8498798175897));
#224569=CARTESIAN_POINT('Ctrl Pts',(-0.0167954266850209,-7.91106147779371,
86.8517662953784));
#224570=CARTESIAN_POINT('Ctrl Pts',(0.0186276770786875,-7.91105737263887,
86.8532174860652));
#224571=CARTESIAN_POINT('Ctrl Pts',(0.696898345013335,-7.90642321145098,
86.8811580069799));
#224572=CARTESIAN_POINT('Ctrl Pts',(1.33680656792559,-7.82369079059429,
86.9099536411519));
#224573=CARTESIAN_POINT('Ctrl Pts',(2.22372433341331,-7.59692541375302,
86.9497204339889));
#224574=CARTESIAN_POINT('Ctrl Pts',(2.48415866729134,-7.51579608691643,
86.9614109236797));
#224575=CARTESIAN_POINT('Ctrl Pts',(2.94325129735218,-7.34630410881085,
86.9819742569405));
#224576=CARTESIAN_POINT('Ctrl Pts',(3.14344288454988,-7.26289781113607,
86.9909270730247));
#224577=CARTESIAN_POINT('Ctrl Pts',(3.38502426818469,-7.1503847983006,87.0017451099702));
#224578=CARTESIAN_POINT('Ctrl Pts',(3.42988799727005,-7.12897330921446,
87.0037549603082));
#224579=CARTESIAN_POINT('Ctrl Pts',(3.49190134627194,-7.09865615014279,
87.0065347915504));
#224580=CARTESIAN_POINT('Ctrl Pts',(3.50922448338432,-7.09010843916444,
87.0073114931489));
#224581=CARTESIAN_POINT('Ctrl Pts',(3.53841919874099,-7.07556975741225,
87.0086207456193));
#224582=CARTESIAN_POINT('Ctrl Pts',(3.55030727074349,-7.06961216069184,
87.0091539501184));
#224583=CARTESIAN_POINT('Ctrl Pts',(3.5736843235827,-7.0578231314884,87.0102026100713));
#224584=CARTESIAN_POINT('Ctrl Pts',(3.58517419047641,-7.05199354970652,
87.0107181005766));
#224585=CARTESIAN_POINT('Ctrl Pts',(3.61073973870512,-7.03894379808993,
87.0118652538032));
#224586=CARTESIAN_POINT('Ctrl Pts',(3.62480811816114,-7.03170941962386,
87.0124966253805));
#224587=CARTESIAN_POINT('Ctrl Pts',(3.67180122785184,-7.00736566081812,
87.0146059844207));
#224588=CARTESIAN_POINT('Ctrl Pts',(3.70462740351025,-6.99006678014924,
87.0160800384539));
#224589=CARTESIAN_POINT('Ctrl Pts',(4.09144692105395,-6.78272870435253,
87.0334577051192));
#224590=CARTESIAN_POINT('Ctrl Pts',(4.43059814643726,-6.56621476713183,
87.048721533589));
#224591=CARTESIAN_POINT('Ctrl Pts',(5.30401681726587,-5.91001761965357,
87.0891137448454));
#224592=CARTESIAN_POINT('Ctrl Pts',(5.79941080327842,-5.42471405632217,
87.1130656522426));
#224593=CARTESIAN_POINT('Ctrl Pts',(6.25371368432081,-4.84531553019176,
87.142081680206));
#224594=CARTESIAN_POINT('Ctrl Pts',(6.28165192373258,-4.80904007306202,
87.1439012558184));
#224595=CARTESIAN_POINT('Ctrl Pts',(6.31558736616769,-4.76417744881517,
87.1461577316284));
#224596=CARTESIAN_POINT('Ctrl Pts',(6.32188485329516,-4.75581774710273,
87.1465784641479));
#224597=CARTESIAN_POINT('Ctrl Pts',(6.33173525827635,-4.74268752924207,
87.1472397389886));
#224598=CARTESIAN_POINT('Ctrl Pts',(6.33529943177351,-4.73792544162726,
87.1474796634325));
#224599=CARTESIAN_POINT('Ctrl Pts',(6.34160993788723,-4.72947413022372,
87.1479056309369));
#224600=CARTESIAN_POINT('Ctrl Pts',(6.3443584331467,-4.72578651912962,87.1480915537724));
#224601=CARTESIAN_POINT('Ctrl Pts',(6.3506770856694,-4.71729343926865,87.1485198980597));
#224602=CARTESIAN_POINT('Ctrl Pts',(6.35424500404566,-4.71248631476798,
87.14876244468));
#224603=CARTESIAN_POINT('Ctrl Pts',(6.36397032094023,-4.69935208391768,
87.149425431448));
#224604=CARTESIAN_POINT('Ctrl Pts',(6.37011681459522,-4.6910169495814,87.149846488723));
#224605=CARTESIAN_POINT('Ctrl Pts',(6.39995661033749,-4.65038502095655,
87.1519007185575));
#224606=CARTESIAN_POINT('Ctrl Pts',(6.42342028146211,-4.61792132121841,
87.1535472717164));
#224607=CARTESIAN_POINT('Ctrl Pts',(6.81921875183373,-4.06145174842563,
87.181876278338));
#224608=CARTESIAN_POINT('Ctrl Pts',(7.12654388958106,-3.49419710615459,
87.2120952085419));
#224609=CARTESIAN_POINT('Ctrl Pts',(7.58501847296354,-2.32874997926644,
87.2696355149641));
#224610=CARTESIAN_POINT('Ctrl Pts',(7.74189920187815,-1.73746297631295,
87.2967842337955));
#224611=CARTESIAN_POINT('Ctrl Pts',(7.83332894162752,-1.10619420938644,
87.3228425372274));
#224612=CARTESIAN_POINT('Ctrl Pts',(7.83720227789363,-1.07841013179822,
87.3239840992476));
#224613=CARTESIAN_POINT('Ctrl Pts',(7.84375594292394,-1.02949853113753,
87.3259844229303));
#224614=CARTESIAN_POINT('Ctrl Pts',(7.84649888591375,-1.00837976972269,
87.3268450656254));
#224615=CARTESIAN_POINT('Ctrl Pts',(7.85039201066779,-0.977427383861025,
87.3281020344587));
#224616=CARTESIAN_POINT('Ctrl Pts',(7.85160905203771,-0.967602349482378,
87.3285003751994));
#224617=CARTESIAN_POINT('Ctrl Pts',(7.85367190939861,-0.950688960129488,
87.3291849864326));
#224618=CARTESIAN_POINT('Ctrl Pts',(7.85452657869798,-0.9436017084756,87.3294715234497));
#224619=CARTESIAN_POINT('Ctrl Pts',(7.85620581465859,-0.929516459933167,
87.3300403217283));
#224620=CARTESIAN_POINT('Ctrl Pts',(7.8570306267173,-0.922518499915964,
87.3303225901182));
#224621=CARTESIAN_POINT('Ctrl Pts',(7.85894950610844,-0.906048878052633,
87.3309861389019));
#224622=CARTESIAN_POINT('Ctrl Pts',(7.86003580313419,-0.896576312002753,
87.3313671850038));
#224623=CARTESIAN_POINT('Ctrl Pts',(7.86318682501633,-0.868653345077344,
87.3324886735253));
#224624=CARTESIAN_POINT('Ctrl Pts',(7.86520373523742,-0.850197558213323,
87.3332276762771));
#224625=CARTESIAN_POINT('Ctrl Pts',(7.88199617357621,-0.691362395781781,
87.3395685891973));
#224626=CARTESIAN_POINT('Ctrl Pts',(7.89307747108192,-0.550614269424851,
87.345058332559));
#224627=CARTESIAN_POINT('Ctrl Pts',(7.94586149357713,0.467386207393339,
87.3839429104912));
#224628=CARTESIAN_POINT('Ctrl Pts',(7.84499507891126,1.34575759054625,87.4123719819369));
#224629=CARTESIAN_POINT('Ctrl Pts',(7.58595076924457,2.24513139283784,87.4458430470043));
#224630=CARTESIAN_POINT('Ctrl Pts',(7.56933939906867,2.30051406641358,87.4479254870153));
#224631=CARTESIAN_POINT('Ctrl Pts',(7.48609315914763,2.56739159145599,87.4580815321679));
#224632=CARTESIAN_POINT('Ctrl Pts',(7.41119382945113,2.77620183849515,87.4664037871057));
#224633=CARTESIAN_POINT('Ctrl Pts',(7.31359220570024,3.0160695519762,87.4766333534637));
#224634=CARTESIAN_POINT('Ctrl Pts',(7.299320449289,3.05044708360466,87.4781147265758));
#224635=CARTESIAN_POINT('Ctrl Pts',(7.28055621858089,3.09476024554365,87.4800429369869));
#224636=CARTESIAN_POINT('Ctrl Pts',(7.27628492544599,3.10478944721812,87.4804805846549));
#224637=CARTESIAN_POINT('Ctrl Pts',(7.26934788545216,3.12098501283162,87.4811892946056));
#224638=CARTESIAN_POINT('Ctrl Pts',(7.26669498077498,3.12715688542911,87.4814598380453));
#224639=CARTESIAN_POINT('Ctrl Pts',(7.2616132901407,3.13893784349771,87.4819771350045));
#224640=CARTESIAN_POINT('Ctrl Pts',(7.25918585768141,3.14454751025898,87.4822238347049));
#224641=CARTESIAN_POINT('Ctrl Pts',(7.25361728092996,3.15737538331515,87.4827888387962));
#224642=CARTESIAN_POINT('Ctrl Pts',(7.2504718615776,3.16459171984505,87.4831073099816));
#224643=CARTESIAN_POINT('Ctrl Pts',(7.24099655912272,3.18624202437329,87.4840646419385));
#224644=CARTESIAN_POINT('Ctrl Pts',(7.23463432629258,3.20066173904904,87.4847047388569));
#224645=CARTESIAN_POINT('Ctrl Pts',(7.18730907245739,3.30706023008099,87.4894457491503));
#224646=CARTESIAN_POINT('Ctrl Pts',(7.14463728426783,3.39826665236209,87.4936088898356));
#224647=CARTESIAN_POINT('Ctrl Pts',(7.0880642319882,3.51340695765493,87.4989725116867));
#224648=CARTESIAN_POINT('Ctrl Pts',(7.07576154331384,3.53811836628076,87.5001300942847));
#224649=CARTESIAN_POINT('Ctrl Pts',(7.05560999291647,3.57806965610495,87.5020115782177));
#224650=CARTESIAN_POINT('Ctrl Pts',(7.04784045032624,3.59334938736389,87.5027335549588));
#224651=CARTESIAN_POINT('Ctrl Pts',(6.85448901178064,3.97055851397311,87.5206143732838));
#224652=CARTESIAN_POINT('Ctrl Pts',(6.64132061157659,4.31766283054549,87.5383296955375));
#224653=CARTESIAN_POINT('Ctrl Pts',(6.13473853989593,5.01563210302715,87.5754876507643));
#224654=CARTESIAN_POINT('Ctrl Pts',(5.83569201552565,5.36062626807766,87.5947917088525));
#224655=CARTESIAN_POINT('Ctrl Pts',(5.26806793090443,5.91131880782493,87.6275119117655));
#224656=CARTESIAN_POINT('Ctrl Pts',(5.01294702321836,6.12915974701263,87.6411730088532));
#224657=CARTESIAN_POINT('Ctrl Pts',(4.69796491102103,6.36525488511783,87.6571107062464));
#224658=CARTESIAN_POINT('Ctrl Pts',(4.65076130454223,6.39982526275107,87.6594746651094));
#224659=CARTESIAN_POINT('Ctrl Pts',(4.57892975210359,6.45121789339013,87.6630353829554));
#224660=CARTESIAN_POINT('Ctrl Pts',(4.55458317547364,6.46842964614736,87.664236006972));
#224661=CARTESIAN_POINT('Ctrl Pts',(4.51223793280284,6.49800790079411,87.6663134752363));
#224662=CARTESIAN_POINT('Ctrl Pts',(4.49428431089011,6.51043826302279,87.6671909725844));
#224663=CARTESIAN_POINT('Ctrl Pts',(4.45681171833629,6.53615389827236,87.6690156268913));
#224664=CARTESIAN_POINT('Ctrl Pts',(4.43728426761626,6.54942644866664,87.6699626419246));
#224665=CARTESIAN_POINT('Ctrl Pts',(4.38327252502149,6.58578507701514,87.6725715362533));
#224666=CARTESIAN_POINT('Ctrl Pts',(4.34866548634216,6.60868758655402,87.6742314177128));
#224667=CARTESIAN_POINT('Ctrl Pts',(4.20982525625314,6.69900751472013,87.680844730775));
#224668=CARTESIAN_POINT('Ctrl Pts',(4.10419112116401,6.76424024817593,87.6857735524406));
#224669=CARTESIAN_POINT('Ctrl Pts',(3.84990988423524,6.91311741879084,87.697412078626));
#224670=CARTESIAN_POINT('Ctrl Pts',(3.70000640861012,6.99449442756818,87.7040955139439));
#224671=CARTESIAN_POINT('Ctrl Pts',(3.13407717418437,7.27842802094015,87.7287771377114));
#224672=CARTESIAN_POINT('Ctrl Pts',(2.70316879030007,7.4492164167693,87.7464552979666));
#224673=CARTESIAN_POINT('Ctrl Pts',(2.08805530787275,7.63256634686153,87.7715214270525));
#224674=CARTESIAN_POINT('Ctrl Pts',(1.91460739493355,7.67791117145885,87.7785780233219));
#224675=CARTESIAN_POINT('Ctrl Pts',(1.71590530383868,7.72270604270233,87.7867352930723));
#224676=CARTESIAN_POINT('Ctrl Pts',(1.69201256055684,7.72797600407672,87.7877173608471));
#224677=CARTESIAN_POINT('Ctrl Pts',(1.65582098115427,7.73578280211078,87.7892070809978));
#224678=CARTESIAN_POINT('Ctrl Pts',(1.64353985416293,7.73840134844053,87.7897129681732));
#224679=CARTESIAN_POINT('Ctrl Pts',(1.62134434564484,7.74307858963739,87.7906279705967));
#224680=CARTESIAN_POINT('Ctrl Pts',(1.61143213845709,7.74514751279154,87.7910368569473));
#224681=CARTESIAN_POINT('Ctrl Pts',(1.59166984882534,7.7492328124804,87.7918526121139));
#224682=CARTESIAN_POINT('Ctrl Pts',(1.58181983998259,7.75124945301157,87.7922594740462));
#224683=CARTESIAN_POINT('Ctrl Pts',(1.55397890853426,7.7568941844088,87.7934102667248));
#224684=CARTESIAN_POINT('Ctrl Pts',(1.53597930340683,7.76047842669492,87.7941552384448));
#224685=CARTESIAN_POINT('Ctrl Pts',(1.45107130388154,7.77707909280664,87.797674012409));
#224686=CARTESIAN_POINT('Ctrl Pts',(1.38400970133299,7.78929291346083,87.8004663097038));
#224687=CARTESIAN_POINT('Ctrl Pts',(0.633794979466337,7.91593412443728,
87.8318123023659));
#224688=CARTESIAN_POINT('Ctrl Pts',(-0.0614089438128411,7.94103310830199,
87.8615694260812));
#224689=CARTESIAN_POINT('Ctrl Pts',(-0.913482989596982,7.85977807747364,
87.8968468073517));
#224690=CARTESIAN_POINT('Ctrl Pts',(-1.07545210965178,7.83925806134967,
87.9035147448832));
#224691=CARTESIAN_POINT('Ctrl Pts',(-1.27503551001025,7.80767020368677,
87.9116951463416));
#224692=CARTESIAN_POINT('Ctrl Pts',(-1.31335310697317,7.80131611967476,
87.9132640815826));
#224693=CARTESIAN_POINT('Ctrl Pts',(-1.37400597830323,7.79079871753301,
87.9157453503438));
#224694=CARTESIAN_POINT('Ctrl Pts',(-1.39637268782135,7.78682094351948,
87.916659883563));
#224695=CARTESIAN_POINT('Ctrl Pts',(-1.4384019705062,7.77915939819513,87.9183775842211));
#224696=CARTESIAN_POINT('Ctrl Pts',(-1.45806829883422,7.77549728377791,
87.9191810006594));
#224697=CARTESIAN_POINT('Ctrl Pts',(-1.50225831000621,7.76709500643872,
87.9209856092262));
#224698=CARTESIAN_POINT('Ctrl Pts',(-1.52677387854837,7.76231321180602,
87.9219863059004));
#224699=CARTESIAN_POINT('Ctrl Pts',(-1.58939574296139,7.74979058770908,
87.924541483828));
#224700=CARTESIAN_POINT('Ctrl Pts',(-1.62746842884367,7.74188475202751,
87.9260940497014));
#224701=CARTESIAN_POINT('Ctrl Pts',(-1.88635747285399,7.68613201134486,
87.9366471649885));
#224702=CARTESIAN_POINT('Ctrl Pts',(-2.10509674706303,7.62912447065724,
87.9455400162122));
#224703=CARTESIAN_POINT('Ctrl Pts',(-2.33231028974806,7.55939066701257,
87.9548432703343));
#224704=CARTESIAN_POINT('Ctrl Pts',(-2.34351439834022,7.55592474877756,
87.9553022018588));
#224705=CARTESIAN_POINT('Ctrl Pts',(-2.35960716713393,7.55090731780756,
87.9559616574063));
#224706=CARTESIAN_POINT('Ctrl Pts',(-2.36450208738591,7.54937594666487,
87.9561622807256));
#224707=CARTESIAN_POINT('Ctrl Pts',(-2.59507035312394,7.47699663971959,
87.9656141087257));
#224708=CARTESIAN_POINT('Ctrl Pts',(-2.81745712368215,7.39606701524068,
87.9748041215321));
#224709=CARTESIAN_POINT('Ctrl Pts',(-3.08829899464355,7.28351233109193,
87.9860806855725));
#224710=CARTESIAN_POINT('Ctrl Pts',(-3.14047627668738,7.26116735524773,
87.9882573733916));
#224711=CARTESIAN_POINT('Ctrl Pts',(-3.71980475264395,7.0056566927738,88.0124784115644));
#224712=CARTESIAN_POINT('Ctrl Pts',(-4.22018742908342,6.71611328896293,
88.0337119031437));
#224713=CARTESIAN_POINT('Ctrl Pts',(-4.86823051933445,6.23988377540042,
88.0640485545537));
#224714=CARTESIAN_POINT('Ctrl Pts',(-5.04588398340681,6.09711950886217,
88.0727313860423));
#224715=CARTESIAN_POINT('Ctrl Pts',(-5.27193993800442,5.89880393378416,
88.0845309448591));
#224716=CARTESIAN_POINT('Ctrl Pts',(-5.32608852104222,5.84995891340575,
88.0874181618653));
#224717=CARTESIAN_POINT('Ctrl Pts',(-5.39023750492656,5.79046396985332,
88.09092091153));
#224718=CARTESIAN_POINT('Ctrl Pts',(-5.40089437221624,5.78052535006996,
88.091505587918));
#224719=CARTESIAN_POINT('Ctrl Pts',(-5.41735723667327,5.7650867754221,88.0924132032141));
#224720=CARTESIAN_POINT('Ctrl Pts',(-5.42318248280896,5.75960734039428,
88.0927352131094));
#224721=CARTESIAN_POINT('Ctrl Pts',(-5.43340428760738,5.74996308882354,
88.0933017839848));
#224722=CARTESIAN_POINT('Ctrl Pts',(-5.43780439620327,5.74580203486148,
88.0935461706383));
#224723=CARTESIAN_POINT('Ctrl Pts',(-5.44779585102022,5.73633165165722,
88.0941022513311));
#224724=CARTESIAN_POINT('Ctrl Pts',(-5.45338421737433,5.73101919639127,
88.0944140926257));
#224725=CARTESIAN_POINT('Ctrl Pts',(-5.46832350686898,5.71677585924211,
88.0952499470565));
#224726=CARTESIAN_POINT('Ctrl Pts',(-5.47766029383313,5.70783022729303,
88.09577467035));
#224727=CARTESIAN_POINT('Ctrl Pts',(-5.51967617407549,5.66737651975696,
88.0981466618111));
#224728=CARTESIAN_POINT('Ctrl Pts',(-5.55210523739451,5.63561079263626,
88.1000067834171));
#224729=CARTESIAN_POINT('Ctrl Pts',(-6.14830562214165,5.04146487184841,
88.1347870544739));
#224730=CARTESIAN_POINT('Ctrl Pts',(-6.62416848020391,4.39751159722814,
88.1728936578792));
#224731=CARTESIAN_POINT('Ctrl Pts',(-7.1465903781655,3.40799045111042,88.2230720140554));
#224732=CARTESIAN_POINT('Ctrl Pts',(-7.27971319486202,3.11351210739892,
88.2371603675924));
#224733=CARTESIAN_POINT('Ctrl Pts',(-7.43710405713788,2.699590703408,88.2556745106913));
#224734=CARTESIAN_POINT('Ctrl Pts',(-7.47717890441449,2.58652353326187,
88.260607488423));
#224735=CARTESIAN_POINT('Ctrl Pts',(-7.5201561265799,2.45590738905284,88.2661664041054));
#224736=CARTESIAN_POINT('Ctrl Pts',(-7.52558826565268,2.43921104718805,
88.2668744028457));
#224737=CARTESIAN_POINT('Ctrl Pts',(-7.53371455678899,2.41394834497199,
88.2679417703779));
#224738=CARTESIAN_POINT('Ctrl Pts',(-7.536449764568,2.40539530684519,88.2683024712615));
#224739=CARTESIAN_POINT('Ctrl Pts',(-7.54114865056292,2.39061512229162,
88.2689246294653));
#224740=CARTESIAN_POINT('Ctrl Pts',(-7.54311919026548,2.38439017665291,
88.2691863092788));
#224741=CARTESIAN_POINT('Ctrl Pts',(-7.54717983482096,2.37150716612742,
88.269727146537));
#224742=CARTESIAN_POINT('Ctrl Pts',(-7.54926884166676,2.36484875936864,
88.2700062681858));
#224743=CARTESIAN_POINT('Ctrl Pts',(-7.55491208255456,2.34677806732403,
88.2707627056684));
#224744=CARTESIAN_POINT('Ctrl Pts',(-7.5584492730617,2.33536045623653,88.2712394682537));
#224745=CARTESIAN_POINT('Ctrl Pts',(-7.57156320299398,2.29268842450722,
88.2730169388504));
#224746=CARTESIAN_POINT('Ctrl Pts',(-7.58097213383292,2.26138256101762,
88.2743122024809));
#224747=CARTESIAN_POINT('Ctrl Pts',(-7.72840851147747,1.75956188909231,
88.2949368270008));
#224748=CARTESIAN_POINT('Ctrl Pts',(-7.82259783315802,1.27725907156672,
88.3127298887389));
#224749=CARTESIAN_POINT('Ctrl Pts',(-7.89781751367036,0.52710037195774,
88.3389136277887));
#224750=CARTESIAN_POINT('Ctrl Pts',(-7.91099178079852,0.263756986168273,
88.3478486968288));
#224751=CARTESIAN_POINT('Ctrl Pts',(-7.91101694035408,-0.543244617673399,
88.3753081746271));
#224752=CARTESIAN_POINT('Ctrl Pts',(-7.85502632930673,-1.08523180736228,
88.3938192804968));
#224753=CARTESIAN_POINT('Ctrl Pts',(-7.737144850556,-1.64973341490619,88.4166116165124));
#224754=CARTESIAN_POINT('Ctrl Pts',(-7.73012929889818,-1.68229953938953,
88.4179393682475));
#224755=CARTESIAN_POINT('Ctrl Pts',(-7.72128933436136,-1.72211143726707,
88.4195792816945));
#224756=CARTESIAN_POINT('Ctrl Pts',(-7.71965998436012,-1.72940062231682,
88.4198802230356));
#224757=CARTESIAN_POINT('Ctrl Pts',(-7.71695331049812,-1.74142936339991,
88.4203779935989));
#224758=CARTESIAN_POINT('Ctrl Pts',(-7.71588193456887,-1.74617026537544,
88.4205744760918));
#224759=CARTESIAN_POINT('Ctrl Pts',(-7.71394117352235,-1.75472158663843,
88.4209294159117));
#224760=CARTESIAN_POINT('Ctrl Pts',(-7.7130733316943,-1.75853235824049,
88.4210877824789));
#224761=CARTESIAN_POINT('Ctrl Pts',(-7.71121423376137,-1.76666797331657,
88.4214262937414));
#224762=CARTESIAN_POINT('Ctrl Pts',(-7.71022216290022,-1.77099262716503,
88.4216064866274));
#224763=CARTESIAN_POINT('Ctrl Pts',(-7.70753633687523,-1.78265569783465,
88.4220931253795));
#224764=CARTESIAN_POINT('Ctrl Pts',(-7.70583574354406,-1.78999251786735,
88.4223999791152));
#224765=CARTESIAN_POINT('Ctrl Pts',(-7.69712481441774,-1.82733134870511,
88.4239653789702));
#224766=CARTESIAN_POINT('Ctrl Pts',(-7.68994985400923,-1.85729411770513,
88.4252339070756));
#224767=CARTESIAN_POINT('Ctrl Pts',(-7.6201803035531,-2.14131683950218,
88.4373703258417));
#224768=CARTESIAN_POINT('Ctrl Pts',(-7.54519667171131,-2.39214768773682,
88.4489348301647));
#224769=CARTESIAN_POINT('Ctrl Pts',(-7.26573593112366,-3.18198222994523,
88.4869884300581));
#224770=CARTESIAN_POINT('Ctrl Pts',(-7.01476776392652,-3.70257268025828,
88.5144423311623));
#224771=CARTESIAN_POINT('Ctrl Pts',(-6.63172581499798,-4.31574525202144,
88.5469255406739));
#224772=CARTESIAN_POINT('Ctrl Pts',(-6.5505499425266,-4.43798858169724,
88.5534206457648));
#224773=CARTESIAN_POINT('Ctrl Pts',(-6.32269495318178,-4.76123218775531,
88.5706071862891));
#224774=CARTESIAN_POINT('Ctrl Pts',(-6.1698536050818,-4.95769360216837,
88.5810609127793));
#224775=CARTESIAN_POINT('Ctrl Pts',(-5.99395479275036,-5.16303135740085,
88.5919900401683));
#224776=CARTESIAN_POINT('Ctrl Pts',(-5.97984605447867,-5.17936560112691,
88.5928595083835));
#224777=CARTESIAN_POINT('Ctrl Pts',(-5.96002931770756,-5.20211930960653,
88.5940708278627));
#224778=CARTESIAN_POINT('Ctrl Pts',(-5.95437751293358,-5.20858744895521,
88.5944151830864));
#224779=CARTESIAN_POINT('Ctrl Pts',(-5.9445845715237,-5.21975809152442,
88.5950099252724));
#224780=CARTESIAN_POINT('Ctrl Pts',(-5.9404483671787,-5.22446489692322,
88.5952605326552));
#224781=CARTESIAN_POINT('Ctrl Pts',(-5.93186242116831,-5.23421191967796,
88.5957795215033));
#224782=CARTESIAN_POINT('Ctrl Pts',(-5.92741183635443,-5.23925138987717,
88.5960478647947));
#224783=CARTESIAN_POINT('Ctrl Pts',(-5.91697335439893,-5.25104072909789,
88.5966756583168));
#224784=CARTESIAN_POINT('Ctrl Pts',(-5.9109803169816,-5.25778604626653,
88.597034876796));
#224785=CARTESIAN_POINT('Ctrl Pts',(-5.89159126730898,-5.27953386824249,
88.5981931318671));
#224786=CARTESIAN_POINT('Ctrl Pts',(-5.87814952568701,-5.2944956028725,
88.5989901023857));
#224787=CARTESIAN_POINT('Ctrl Pts',(-5.55240493376366,-5.65430577486697,
88.6181601508027));
#224788=CARTESIAN_POINT('Ctrl Pts',(-5.21033552532158,-5.97100033731662,
88.6350366501181));
#224789=CARTESIAN_POINT('Ctrl Pts',(-4.74483721245125,-6.33132327105307,
88.6554057210577));
#224790=CARTESIAN_POINT('Ctrl Pts',(-4.64554717602665,-6.40453172455108,
88.6596217873688));
#224791=CARTESIAN_POINT('Ctrl Pts',(-4.43858457962816,-6.54978308298424,
88.6682094156754));
#224792=CARTESIAN_POINT('Ctrl Pts',(-4.33077309649846,-6.62156296491187,
88.6725768947865));
#224793=CARTESIAN_POINT('Ctrl Pts',(-3.8225551286767,-6.94220588656738,
88.6928583743673));
#224794=CARTESIAN_POINT('Ctrl Pts',(-3.40221254233858,-7.15758450384787,
88.7087245874296));
#224795=CARTESIAN_POINT('Ctrl Pts',(-2.9479910767082,-7.34122716143946,
88.7273557736604));
#224796=CARTESIAN_POINT('Ctrl Pts',(-2.93070609902059,-7.34814462133207,
88.7280669810845));
#224797=CARTESIAN_POINT('Ctrl Pts',(-2.83806114565047,-7.38484230895787,
88.7318916224475));
#224798=CARTESIAN_POINT('Ctrl Pts',(-2.76227377166025,-7.41352343515758,
88.7350651184924));
#224799=CARTESIAN_POINT('Ctrl Pts',(-2.67713023843656,-7.44425851611172,
88.7386946002181));
#224800=CARTESIAN_POINT('Ctrl Pts',(-2.66819289052675,-7.44746654007975,
88.739076364801));
#224801=CARTESIAN_POINT('Ctrl Pts',(-2.6547673029491,-7.4522583301866,88.7396510566824));
#224802=CARTESIAN_POINT('Ctrl Pts',(-2.65028335142292,-7.45385415807101,
88.7398431979907));
#224803=CARTESIAN_POINT('Ctrl Pts',(-2.64250196837033,-7.45661562498681,
88.7401769911241));
#224804=CARTESIAN_POINT('Ctrl Pts',(-2.63920521856608,-7.45778311871919,
88.7403185195026));
#224805=CARTESIAN_POINT('Ctrl Pts',(-2.63233486637463,-7.46021102319318,
88.7406136883837));
#224806=CARTESIAN_POINT('Ctrl Pts',(-2.62876113138943,-7.46147105290219,
88.7407673535259));
#224807=CARTESIAN_POINT('Ctrl Pts',(-2.62032959490861,-7.4644370398999,
88.741130195725));
#224808=CARTESIAN_POINT('Ctrl Pts',(-2.61547103579838,-7.46614082168484,
88.7413395126198));
#224809=CARTESIAN_POINT('Ctrl Pts',(-2.59952826134319,-7.47171410397762,
88.7420271194424));
#224810=CARTESIAN_POINT('Ctrl Pts',(-2.58843714338575,-7.47556365666566,
88.7425066781246));
#224811=CARTESIAN_POINT('Ctrl Pts',(-2.18074201189771,-7.61605214399134,
88.7601776328176));
#224812=CARTESIAN_POINT('Ctrl Pts',(-1.77394553591557,-7.72094065130411,
88.7792801012561));
#224813=CARTESIAN_POINT('Ctrl Pts',(-0.9476121671058,-7.86523295458176,
88.8183932288109));
#224814=CARTESIAN_POINT('Ctrl Pts',(-0.52931208548964,-7.90441073791194,
88.8383280646829));
#224815=CARTESIAN_POINT('Ctrl Pts',(0.387914087462226,-7.91715149784917,
88.8805185944954));
#224816=CARTESIAN_POINT('Ctrl Pts',(0.885295356752189,-7.87706426171078,
88.902380205155));
#224817=CARTESIAN_POINT('Ctrl Pts',(1.40954616123498,-7.78448995176033,
88.9240515020288));
#224818=CARTESIAN_POINT('Ctrl Pts',(1.44338053315756,-7.77828752792368,
88.9254444374308));
#224819=CARTESIAN_POINT('Ctrl Pts',(1.48886297999582,-7.76964282338008,
88.9273094256373));
#224820=CARTESIAN_POINT('Ctrl Pts',(1.50054729508004,-7.76739469790199,
88.9277878695766));
#224821=CARTESIAN_POINT('Ctrl Pts',(1.51887333532028,-7.76382577386114,
88.9285372401026));
#224822=CARTESIAN_POINT('Ctrl Pts',(1.52551848842739,-7.76252279850979,
88.9288087533365));
#224823=CARTESIAN_POINT('Ctrl Pts',(1.53827146157543,-7.76000519916228,
88.9293294167995));
#224824=CARTESIAN_POINT('Ctrl Pts',(1.54437953471024,-7.75879189265492,
88.9295786101808));
#224825=CARTESIAN_POINT('Ctrl Pts',(1.55872321325263,-7.75592505788742,
88.9301633744871));
#224826=CARTESIAN_POINT('Ctrl Pts',(1.56695763790714,-7.75426562097835,
88.9304987506442));
#224827=CARTESIAN_POINT('Ctrl Pts',(1.59074247285435,-7.7494329643363,88.9314665389876));
#224828=CARTESIAN_POINT('Ctrl Pts',(1.60628603898638,-7.74622605198929,
88.9320978421508));
#224829=CARTESIAN_POINT('Ctrl Pts',(1.71157474274845,-7.72417259399143,
88.9363664528819));
#224830=CARTESIAN_POINT('Ctrl Pts',(1.80099765769058,-7.70381324515539,
88.9399537732689));
#224831=CARTESIAN_POINT('Ctrl Pts',(1.99299572387748,-7.65657421826673,
88.9475832749825));
#224832=CARTESIAN_POINT('Ctrl Pts',(2.09542555195124,-7.62917777172763,
88.9516082288176));
#224833=CARTESIAN_POINT('Ctrl Pts',(2.51514707477109,-7.50782555350359,
88.9679516055825));
#224834=CARTESIAN_POINT('Ctrl Pts',(2.82694961431663,-7.39606536926273,
88.9797205709783));
#224835=CARTESIAN_POINT('Ctrl Pts',(3.45223152302835,-7.12660417506277,
89.0034388245891));
#224836=CARTESIAN_POINT('Ctrl Pts',(3.76406426169689,-6.96693645160515,
89.0153346777934));
#224837=CARTESIAN_POINT('Ctrl Pts',(4.37591260307645,-6.60054808698712,
89.0403683026975));
#224838=CARTESIAN_POINT('Ctrl Pts',(4.67431209451183,-6.39270406833882,
89.0535483406642));
#224839=CARTESIAN_POINT('Ctrl Pts',(4.97790416914924,-6.1485839516202,89.0690402716622));
#224840=CARTESIAN_POINT('Ctrl Pts',(4.99834441144837,-6.13197909724792,
89.0700931055343));
#224841=CARTESIAN_POINT('Ctrl Pts',(5.02659289353847,-6.10879604404624,
89.0715613961585));
#224842=CARTESIAN_POINT('Ctrl Pts',(5.03447202655267,-6.10230420724019,
89.0719723784135));
#224843=CARTESIAN_POINT('Ctrl Pts',(5.04678262352544,-6.09212109319449,
89.0726167473329));
#224844=CARTESIAN_POINT('Ctrl Pts',(5.05122267136329,-6.08844017687189,
89.0728496081757));
#224845=CARTESIAN_POINT('Ctrl Pts',(5.05971908841751,-6.08138073260774,
89.0732960785586));
#224846=CARTESIAN_POINT('Ctrl Pts',(5.06377611006337,-6.07800299239878,
89.0735096485714));
#224847=CARTESIAN_POINT('Ctrl Pts',(5.07315829300004,-6.07017578734881,
89.0740044244693));
#224848=CARTESIAN_POINT('Ctrl Pts',(5.07848098242425,-6.06572337532063,
89.0742857764904));
#224849=CARTESIAN_POINT('Ctrl Pts',(5.09358928316965,-6.05305150583187,
89.0750862394353));
#224850=CARTESIAN_POINT('Ctrl Pts',(5.10336082103688,-6.04481535249912,
89.0756061662113));
#224851=CARTESIAN_POINT('Ctrl Pts',(5.12531085871779,-6.02622312610047,
89.0767790173081));
#224852=CARTESIAN_POINT('Ctrl Pts',(5.13747799334752,-6.01585375714953,
89.0774325733103));
#224853=CARTESIAN_POINT('Ctrl Pts',(5.40418037700571,-5.78715902915146,
89.0918328070513));
#224854=CARTESIAN_POINT('Ctrl Pts',(5.64459837793763,-5.55291473319003,
89.1062933403793));
#224855=CARTESIAN_POINT('Ctrl Pts',(6.28301977483555,-4.84645509327848,
89.1478396790811));
#224856=CARTESIAN_POINT('Ctrl Pts',(6.64170755335334,-4.34192158305693,
89.1750306117343));
#224857=CARTESIAN_POINT('Ctrl Pts',(7.0422408391639,-3.61077902904357,89.2099485105464));
#224858=CARTESIAN_POINT('Ctrl Pts',(7.13850520234323,-3.41652311684236,
89.2188671420879));
#224859=CARTESIAN_POINT('Ctrl Pts',(7.24103665745436,-3.18630745760502,
89.2290630511905));
#224860=CARTESIAN_POINT('Ctrl Pts',(7.25518240576039,-3.15396502425295,
89.2304872088299));
#224861=CARTESIAN_POINT('Ctrl Pts',(7.27563181797133,-3.10634443278226,
89.2325720701079));
#224862=CARTESIAN_POINT('Ctrl Pts',(7.28210480690269,-3.09113954221639,
89.2332359531901));
#224863=CARTESIAN_POINT('Ctrl Pts',(7.29352356704223,-3.06408223010943,
89.234414147183));
#224864=CARTESIAN_POINT('Ctrl Pts',(7.29848820236185,-3.05223785066061,
89.2349288190136));
#224865=CARTESIAN_POINT('Ctrl Pts',(7.30877781075989,-3.02752076338877,
89.236000586599));
#224866=CARTESIAN_POINT('Ctrl Pts',(7.31409767069249,-3.01464597006946,
89.2365575815631));
#224867=CARTESIAN_POINT('Ctrl Pts',(7.32782419289511,-2.98117568096985,
89.238002282422));
#224868=CARTESIAN_POINT('Ctrl Pts',(7.33617805761328,-2.96055862226515,
89.2388889480326));
#224869=CARTESIAN_POINT('Ctrl Pts',(7.37175341906241,-2.87168461292541,
89.2426971869306));
#224870=CARTESIAN_POINT('Ctrl Pts',(7.39811033756079,-2.80308484427902,
89.2456014074783));
#224871=CARTESIAN_POINT('Ctrl Pts',(7.57479916722589,-2.32335186561229,
89.2656712060856));
#224872=CARTESIAN_POINT('Ctrl Pts',(7.69173832209123,-1.90072096707954,
89.2820686020286));
#224873=CARTESIAN_POINT('Ctrl Pts',(7.8890732413498,-0.857646648316181,
89.3209611424736));
#224874=CARTESIAN_POINT('Ctrl Pts',(7.93211630525977,-0.233237506243383,
89.3428624459517));
#224875=CARTESIAN_POINT('Ctrl Pts',(7.89986951178722,0.420648519860349,
89.368822955207));
#224876=CARTESIAN_POINT('Ctrl Pts',(7.89815916154212,0.451625178697357,
89.3700604266088));
#224877=CARTESIAN_POINT('Ctrl Pts',(7.89568457378939,0.492114989354451,
89.3716887936087));
#224878=CARTESIAN_POINT('Ctrl Pts',(7.89508525268277,0.501638219478262,
89.3720725726294));
#224879=CARTESIAN_POINT('Ctrl Pts',(7.89413469811329,0.516318786670662,
89.3726654304444));
#224880=CARTESIAN_POINT('Ctrl Pts',(7.89379563574389,0.521476924081097,
89.372873972338));
#224881=CARTESIAN_POINT('Ctrl Pts',(7.89311113535584,0.531736541343692,
89.3732892420114));
#224882=CARTESIAN_POINT('Ctrl Pts',(7.8927658066103,0.536838026128945,89.3734959648196));
#224883=CARTESIAN_POINT('Ctrl Pts',(7.89199886739546,0.54800718196608,89.3739490821931));
#224884=CARTESIAN_POINT('Ctrl Pts',(7.89157520495236,0.554074705003744,
89.3741955692982));
#224885=CARTESIAN_POINT('Ctrl Pts',(7.8903751126361,0.570981322721977,89.3748833343878));
#224886=CARTESIAN_POINT('Ctrl Pts',(7.8895833480246,0.581819286158091,89.3753253141265));
#224887=CARTESIAN_POINT('Ctrl Pts',(7.8877555387337,0.606149043888864,89.3763200090322));
#224888=CARTESIAN_POINT('Ctrl Pts',(7.88670720562293,0.619639856172831,
89.3768732997237));
#224889=CARTESIAN_POINT('Ctrl Pts',(7.84827506856253,1.09831315307018,89.3965683888143));
#224890=CARTESIAN_POINT('Ctrl Pts',(7.76984113715447,1.55921713442513,89.4177377404537));
#224891=CARTESIAN_POINT('Ctrl Pts',(7.52972908385702,2.47302449974956,89.4612007333255));
#224892=CARTESIAN_POINT('Ctrl Pts',(7.3664753035758,2.92365598710213,89.4833901677259));
#224893=CARTESIAN_POINT('Ctrl Pts',(7.09483577063776,3.50334412523636,89.5117360187883));
#224894=CARTESIAN_POINT('Ctrl Pts',(7.02167876149942,3.64775898533374,89.518787531536));
#224895=CARTESIAN_POINT('Ctrl Pts',(6.84997276692335,3.96237720463552,89.5341012455857));
#224896=CARTESIAN_POINT('Ctrl Pts',(6.74940332083147,4.13135835279973,89.5422925922031));
#224897=CARTESIAN_POINT('Ctrl Pts',(6.63050175427649,4.31519024927493,89.5511713779665));
#224898=CARTESIAN_POINT('Ctrl Pts',(6.61828553873177,4.33390319907581,89.5520748284619));
#224899=CARTESIAN_POINT('Ctrl Pts',(6.60088703628817,4.36030931954863,89.5533492411625));
#224900=CARTESIAN_POINT('Ctrl Pts',(6.5957703138219,4.36804544344368,89.5537225460679));
#224901=CARTESIAN_POINT('Ctrl Pts',(6.58639175393044,4.38217111174358,89.5544040789044));
#224902=CARTESIAN_POINT('Ctrl Pts',(6.58213419712742,4.38856347798309,89.5547124598697));
#224903=CARTESIAN_POINT('Ctrl Pts',(6.57352140529801,4.40145413807569,89.5553342605217));
#224904=CARTESIAN_POINT('Ctrl Pts',(6.56916582694053,4.40795219280863,89.5556476673492));
#224905=CARTESIAN_POINT('Ctrl Pts',(6.55848210269377,4.42384015578137,89.5564138715508));
#224906=CARTESIAN_POINT('Ctrl Pts',(6.55214341316844,4.43322297091472,89.5568662882951));
#224907=CARTESIAN_POINT('Ctrl Pts',(6.52931285684642,4.46686186864544,89.5584880283742));
#224908=CARTESIAN_POINT('Ctrl Pts',(6.51270617463136,4.49103992875739,89.5596531965669));
#224909=CARTESIAN_POINT('Ctrl Pts',(6.28838421364665,4.81377464802117,89.5752012715354));
#224910=CARTESIAN_POINT('Ctrl Pts',(6.06044690048255,5.09776612378701,89.5888001135856));
#224911=CARTESIAN_POINT('Ctrl Pts',(5.7467590370768,5.43768713906179,89.6054314335121));
#224912=CARTESIAN_POINT('Ctrl Pts',(5.67840542845199,5.50902832692753,89.6089455902053));
#224913=CARTESIAN_POINT('Ctrl Pts',(5.49274258668274,5.69567825184592,89.6182337838134));
#224914=CARTESIAN_POINT('Ctrl Pts',(5.3731429924138,5.80864075880536,89.6239542223849));
#224915=CARTESIAN_POINT('Ctrl Pts',(4.88013385055123,6.24602522249206,89.6467583500699));
#224916=CARTESIAN_POINT('Ctrl Pts',(4.48021536229425,6.53881892026914,89.6635114877978));
#224917=CARTESIAN_POINT('Ctrl Pts',(3.89351107514106,6.88913184997641,89.6888044120073));
#224918=CARTESIAN_POINT('Ctrl Pts',(3.72802304411072,6.98007232576191,89.6960305867875));
#224919=CARTESIAN_POINT('Ctrl Pts',(3.54346877045847,7.07305230436783,89.704275316243));
#224920=CARTESIAN_POINT('Ctrl Pts',(3.52749540246873,7.08103212861304,89.7049900767568));
#224921=CARTESIAN_POINT('Ctrl Pts',(3.50425389099129,7.09254474579114,89.7060316254028));
#224922=CARTESIAN_POINT('Ctrl Pts',(3.4970070664154,7.0961206218905,89.7063566053943));
#224923=CARTESIAN_POINT('Ctrl Pts',(3.4842231848722,7.10240436680213,89.7069302635156));
#224924=CARTESIAN_POINT('Ctrl Pts',(3.4786884111821,7.10511688357183,89.7071787510516));
#224925=CARTESIAN_POINT('Ctrl Pts',(3.46802550696183,7.11032718092058,89.7076576982074));
#224926=CARTESIAN_POINT('Ctrl Pts',(3.46289783233325,7.11282588984812,89.707888120312));
#224927=CARTESIAN_POINT('Ctrl Pts',(3.4494311584266,7.11937016799325,89.70849353045));
#224928=CARTESIAN_POINT('Ctrl Pts',(3.44108775672879,7.12340662571423,89.7088688780094));
#224929=CARTESIAN_POINT('Ctrl Pts',(3.41120294246717,7.13779985576776,89.7102142012905));
#224930=CARTESIAN_POINT('Ctrl Pts',(3.38962182093009,7.148073600117,89.7111873596248));
#224931=CARTESIAN_POINT('Ctrl Pts',(3.33628080932876,7.17317083149837,89.7135961791555));
#224932=CARTESIAN_POINT('Ctrl Pts',(3.30446845674579,7.18788130076766,89.7150358424057));
#224933=CARTESIAN_POINT('Ctrl Pts',(3.18125506181018,7.24386601711875,89.7206210698701));
#224934=CARTESIAN_POINT('Ctrl Pts',(3.08917144639956,7.28361158012059,89.7248145538047));
#224935=CARTESIAN_POINT('Ctrl Pts',(2.61149700329055,7.47909960635989,89.7465940071312));
#224936=CARTESIAN_POINT('Ctrl Pts',(2.21481825961996,7.60601248213001,89.7647165187889));
#224937=CARTESIAN_POINT('Ctrl Pts',(1.10847252472751,7.86603747543558,89.8136564115216));
#224938=CARTESIAN_POINT('Ctrl Pts',(0.38767293313818,7.93429597415291,89.8435105576992));
#224939=CARTESIAN_POINT('Ctrl Pts',(-0.424582505072139,7.90013692017579,
89.8765519541056));
#224940=CARTESIAN_POINT('Ctrl Pts',(-0.516690679117052,7.89464784364581,
89.8802914154652));
#224941=CARTESIAN_POINT('Ctrl Pts',(-0.649111671634326,7.88442891495911,
89.8856564092761));
#224942=CARTESIAN_POINT('Ctrl Pts',(-0.689516670322647,7.88099816363337,
89.8872919249779));
#224943=CARTESIAN_POINT('Ctrl Pts',(-0.753229285302769,7.87509465803832,
89.8898686025099));
#224944=CARTESIAN_POINT('Ctrl Pts',(-0.776555277528733,7.87282872502474,
89.8908114733203));
#224945=CARTESIAN_POINT('Ctrl Pts',(-0.824081979906426,7.86799860965712,
89.8927316113695));
#224946=CARTESIAN_POINT('Ctrl Pts',(-0.848281624364969,7.86542634068607,
89.8937087985975));
#224947=CARTESIAN_POINT('Ctrl Pts',(-0.903830946221119,7.85926245263223,
89.8959507669192));
#224948=CARTESIAN_POINT('Ctrl Pts',(-0.935171803801835,7.85559484600503,
89.8972148573639));
#224949=CARTESIAN_POINT('Ctrl Pts',(-1.00033311460267,7.84757398016518,
89.8998414412593));
#224950=CARTESIAN_POINT('Ctrl Pts',(-1.03414907418209,7.84318936515009,
89.9012036235906));
#224951=CARTESIAN_POINT('Ctrl Pts',(-1.27281181811938,7.81067374841976,
89.9108117095876));
#224952=CARTESIAN_POINT('Ctrl Pts',(-1.47651727089769,7.77473944208692,
89.9189802029492));
#224953=CARTESIAN_POINT('Ctrl Pts',(-1.84497300572026,7.69473757420097,
89.9337589236691));
#224954=CARTESIAN_POINT('Ctrl Pts',(-2.01015406069892,7.65324723826584,
89.9403862599132));
#224955=CARTESIAN_POINT('Ctrl Pts',(-2.29237348608272,7.57259105006406,
89.9517691599466));
#224956=CARTESIAN_POINT('Ctrl Pts',(-2.41007086980918,7.53595846292259,
89.9565349050008));
#224957=CARTESIAN_POINT('Ctrl Pts',(-2.68788025409696,7.44231767676551,
89.9678669340323));
#224958=CARTESIAN_POINT('Ctrl Pts',(-2.84710504134614,7.38287106254389,
89.9744283754043));
#224959=CARTESIAN_POINT('Ctrl Pts',(-3.23603907112414,7.22320774276778,
89.9907501450847));
#224960=CARTESIAN_POINT('Ctrl Pts',(-3.46313186657929,7.11711953451216,
90.0005407255389));
#224961=CARTESIAN_POINT('Ctrl Pts',(-3.70853159368869,6.98794916479542,
90.0116372971271));
#224962=CARTESIAN_POINT('Ctrl Pts',(-3.73219751766202,6.97533811284435,
90.0127129446798));
#224963=CARTESIAN_POINT('Ctrl Pts',(-3.76729752894372,6.95640431714803,
90.0143169086905));
#224964=CARTESIAN_POINT('Ctrl Pts',(-3.77878088581273,6.95017314250423,
90.0148430432491));
#224965=CARTESIAN_POINT('Ctrl Pts',(-3.79899377745614,6.93914018735975,
90.0157716311196));
#224966=CARTESIAN_POINT('Ctrl Pts',(-3.80772978591342,6.93435030394225,
90.0161737896032));
#224967=CARTESIAN_POINT('Ctrl Pts',(-3.82605657570935,6.92425679699983,
90.0170192151313));
#224968=CARTESIAN_POINT('Ctrl Pts',(-3.8356454280898,6.91894972234862,90.0174625693701));
#224969=CARTESIAN_POINT('Ctrl Pts',(-3.86032232133006,6.90522491179611,
90.018606206727));
#224970=CARTESIAN_POINT('Ctrl Pts',(-3.8753937685858,6.89677769995755,90.0193072731166));
#224971=CARTESIAN_POINT('Ctrl Pts',(-3.94789256821951,6.85583104864192,
90.0226922477453));
#224972=CARTESIAN_POINT('Ctrl Pts',(-4.00493883193406,6.82266369295523,
90.0253936829161));
#224973=CARTESIAN_POINT('Ctrl Pts',(-4.16630066885229,6.72612490785261,
90.0331352077428));
#224974=CARTESIAN_POINT('Ctrl Pts',(-4.26957299051384,6.66104820734109,
90.0382108514524));
#224975=CARTESIAN_POINT('Ctrl Pts',(-4.69408723622533,6.37961239821007,
90.0595156877767));
#224976=CARTESIAN_POINT('Ctrl Pts',(-5.00072802467814,6.14220089914491,
90.0759578256208));
#224977=CARTESIAN_POINT('Ctrl Pts',(-5.43208037849606,5.75443914104567,
90.1002563264523));
#224978=CARTESIAN_POINT('Ctrl Pts',(-5.57065846399161,5.62039443164324,
90.1082739126623));
#224979=CARTESIAN_POINT('Ctrl Pts',(-5.81171831454006,5.36953707134801,
90.1226040288587));
#224980=CARTESIAN_POINT('Ctrl Pts',(-5.91591842822285,5.25451316954187,
90.1289416196723));
#224981=CARTESIAN_POINT('Ctrl Pts',(-6.04233342450657,5.10643614507045,
90.1368255868165));
#224982=CARTESIAN_POINT('Ctrl Pts',(-6.06777161433447,5.07618271690519,
90.1384225499012));
#224983=CARTESIAN_POINT('Ctrl Pts',(-6.10771568750982,5.0279482593246,90.1409472982731));
#224984=CARTESIAN_POINT('Ctrl Pts',(-6.12237131244892,5.01009222817514,
90.1418773649009));
#224985=CARTESIAN_POINT('Ctrl Pts',(-6.14954853077716,4.97668288589911,
90.1436091525843));
#224986=CARTESIAN_POINT('Ctrl Pts',(-6.16208984896194,4.96114587321428,
90.1444111647053));
#224987=CARTESIAN_POINT('Ctrl Pts',(-6.18985843475167,4.92647657669666,
90.1461934136246));
#224988=CARTESIAN_POINT('Ctrl Pts',(-6.20505610196316,4.90732082500633,
90.1471732082018));
#224989=CARTESIAN_POINT('Ctrl Pts',(-6.24922105904906,4.85112033877046,
90.1500335996376));
#224990=CARTESIAN_POINT('Ctrl Pts',(-6.27794722334512,4.81388731497672,
90.1519107153334));
#224991=CARTESIAN_POINT('Ctrl Pts',(-6.44874626807695,4.58837924130525,
90.1631762681679));
#224992=CARTESIAN_POINT('Ctrl Pts',(-6.58267429353875,4.3940817554646,90.1724490387872));
#224993=CARTESIAN_POINT('Ctrl Pts',(-6.94704595983688,3.81133201517904,
90.1993306021307));
#224994=CARTESIAN_POINT('Ctrl Pts',(-7.15317481661213,3.40878451382984,
90.2166965377758));
#224995=CARTESIAN_POINT('Ctrl Pts',(-7.46758790260554,2.63886435708357,
90.2480930516166));
#224996=CARTESIAN_POINT('Ctrl Pts',(-7.5857651023487,2.27698040406869,90.2621934591091));
#224997=CARTESIAN_POINT('Ctrl Pts',(-7.6902188556557,1.85667773415046,90.2784756864801));
#224998=CARTESIAN_POINT('Ctrl Pts',(-7.70245975924784,1.80522349713467,
90.2804680417822));
#224999=CARTESIAN_POINT('Ctrl Pts',(-7.7752604537458,1.48497843806964,90.2928753407252));
#225000=CARTESIAN_POINT('Ctrl Pts',(-7.82225683670705,1.21330974372384,
90.3034248837244));
#225001=CARTESIAN_POINT('Ctrl Pts',(-7.85726750318379,0.920672503587411,
90.3151868848032));
#225002=CARTESIAN_POINT('Ctrl Pts',(-7.85948130156511,0.901578692610415,
90.3159561564195));
#225003=CARTESIAN_POINT('Ctrl Pts',(-7.86265110519296,0.873340215743733,
90.3170967605841));
#225004=CARTESIAN_POINT('Ctrl Pts',(-7.86366079920464,0.864201578742495,
90.3174663360601));
#225005=CARTESIAN_POINT('Ctrl Pts',(-7.86535687073511,0.848601506695357,
90.3180980095393));
#225006=CARTESIAN_POINT('Ctrl Pts',(-7.86605122427481,0.842140937139422,
90.3183598405009));
#225007=CARTESIAN_POINT('Ctrl Pts',(-7.86742411739459,0.829217095454429,
90.3188840852809));
#225008=CARTESIAN_POINT('Ctrl Pts',(-7.86810265383972,0.822753828731993,
90.3191464989553));
#225009=CARTESIAN_POINT('Ctrl Pts',(-7.86944749626716,0.809789975935379,
90.3196733265499));
#225010=CARTESIAN_POINT('Ctrl Pts',(-7.87011371352183,0.803289385943585,
90.3199377433063));
#225011=CARTESIAN_POINT('Ctrl Pts',(-7.87161333374309,0.788475948970979,
90.3205408609559));
#225012=CARTESIAN_POINT('Ctrl Pts',(-7.87244162350826,0.780162599648683,
90.3208797407798));
#225013=CARTESIAN_POINT('Ctrl Pts',(-7.87451196677343,0.759044005517582,
90.3217416700244));
#225014=CARTESIAN_POINT('Ctrl Pts',(-7.87573595249364,0.746237041021348,
90.322265364541));
#225015=CARTESIAN_POINT('Ctrl Pts',(-7.89962297498831,0.489693004688716,
90.3327765289753));
#225016=CARTESIAN_POINT('Ctrl Pts',(-7.91098842582327,0.245089548895191,
90.343250676027));
#225017=CARTESIAN_POINT('Ctrl Pts',(-7.91099999116524,0.000373876422793476,
90.3540864678166));
#225018=CARTESIAN_POINT('',(-7.90697312323461,0.00395131442269322,92.3576684917631));
#225019=CARTESIAN_POINT('Ctrl Pts',(-7.91729508967814,0.000522195832882638,
90.3577115106449));
#225020=CARTESIAN_POINT('Ctrl Pts',(-7.90068245752772,-2.46740656103677,
90.4572310833883));
#225021=CARTESIAN_POINT('Ctrl Pts',(-5.36653499073731,-7.5605983309967,
90.6627202333486));
#225022=CARTESIAN_POINT('Ctrl Pts',(3.36342892092229,-8.73984422960058,
90.9741789605246));
#225023=CARTESIAN_POINT('Ctrl Pts',(8.17091791536676,-3.04564661273073,
91.2391029035664));
#225024=CARTESIAN_POINT('Ctrl Pts',(7.877328711738,2.37408643071016,91.4510420579989));
#225025=CARTESIAN_POINT('Ctrl Pts',(5.11028731654382,7.0745385235803,91.6629812124325));
#225026=CARTESIAN_POINT('Ctrl Pts',(-0.58978711048923,8.70507802341428,
91.8749203668651));
#225027=CARTESIAN_POINT('Ctrl Pts',(-5.43791012976105,6.18501921579393,
92.0868595212981));
#225028=CARTESIAN_POINT('Ctrl Pts',(-7.52009634502631,3.17273990218627,
92.230113966728));
#225029=CARTESIAN_POINT('Ctrl Pts',(-7.90704442232692,0.931371954907319,
92.3203836235497));
#225030=CARTESIAN_POINT('Ctrl Pts',(-7.90697312323461,0.00395131442269322,
92.3576684917631));
#225031=CARTESIAN_POINT('',(-7.91099999858106,-0.000149834679674665,96.3535680629415));
#225032=CARTESIAN_POINT('Ctrl Pts',(-7.9109989942205,0.00398916560548777,
92.3599925715499));
#225033=CARTESIAN_POINT('Ctrl Pts',(-7.91100938498044,-0.0166169709954872,
92.3608274381967));
#225034=CARTESIAN_POINT('Ctrl Pts',(-7.91093926512935,-0.0372231259525087,
92.3616613362639));
#225035=CARTESIAN_POINT('Ctrl Pts',(-7.91063655989461,-0.0786321807808416,
92.363335207322));
#225036=CARTESIAN_POINT('Ctrl Pts',(-7.91040242391774,-0.0994348909806759,
92.3641751545412));
#225037=CARTESIAN_POINT('Ctrl Pts',(-7.90978919970167,-0.139777527739423,
92.3658022719579));
#225038=CARTESIAN_POINT('Ctrl Pts',(-7.90941975715157,-0.159317446761974,
92.366589550345));
#225039=CARTESIAN_POINT('Ctrl Pts',(-7.90854413621853,-0.198037272686675,
92.3681480490989));
#225040=CARTESIAN_POINT('Ctrl Pts',(-7.90804058205259,-0.217217105688372,
92.36891929487));
#225041=CARTESIAN_POINT('Ctrl Pts',(-7.90689568000985,-0.255514351188711,
92.3704578308992));
#225042=CARTESIAN_POINT('Ctrl Pts',(-7.90625476052629,-0.27463164842514,
92.3712251209344));
#225043=CARTESIAN_POINT('Ctrl Pts',(-7.90435117265783,-0.325862558156829,
92.3732794806724));
#225044=CARTESIAN_POINT('Ctrl Pts',(-7.90296213596042,-0.357971166897346,
92.3745650976691));
#225045=CARTESIAN_POINT('Ctrl Pts',(-7.89707498725394,-0.477222900635277,
92.3793333297991));
#225046=CARTESIAN_POINT('Ctrl Pts',(-7.8913308281871,-0.564298694092066,
92.382801926403));
#225047=CARTESIAN_POINT('Ctrl Pts',(-7.83017837327691,-1.30460721407445,
92.4122146422615));
#225048=CARTESIAN_POINT('Ctrl Pts',(-7.69520025481478,-1.94876153228048,
92.4375076951123));
#225049=CARTESIAN_POINT('Ctrl Pts',(-7.36253101271792,-2.91772214554893,
92.4761089506171));
#225050=CARTESIAN_POINT('Ctrl Pts',(-7.21851089450144,-3.25776959262321,
92.4897858538874));
#225051=CARTESIAN_POINT('Ctrl Pts',(-6.94877001984275,-3.78809420973568,
92.5121839715152));
#225052=CARTESIAN_POINT('Ctrl Pts',(-6.83765174551799,-3.98516943178604,
92.5207723245413));
#225053=CARTESIAN_POINT('Ctrl Pts',(-6.66814912926701,-4.25778233649769,
92.5332958043001));
#225054=CARTESIAN_POINT('Ctrl Pts',(-6.61660548561992,-4.3374479095469,
92.5370378978809));
#225055=CARTESIAN_POINT('Ctrl Pts',(-6.5548931927439,-4.4291694353639,92.5414612985536));
#225056=CARTESIAN_POINT('Ctrl Pts',(-6.54610522256729,-4.44214734860757,
92.5420899051164));
#225057=CARTESIAN_POINT('Ctrl Pts',(-6.53264214494182,-4.46190266525581,
92.5430510659916));
#225058=CARTESIAN_POINT('Ctrl Pts',(-6.52799490369737,-4.46869906402541,
92.5433825088896));
#225059=CARTESIAN_POINT('Ctrl Pts',(-6.51953146434152,-4.48103511887802,
92.5439855368851));
#225060=CARTESIAN_POINT('Ctrl Pts',(-6.51571879082492,-4.48657719088195,
92.5442569781028));
#225061=CARTESIAN_POINT('Ctrl Pts',(-6.50806621359993,-4.49767058837432,
92.5448013800863));
#225062=CARTESIAN_POINT('Ctrl Pts',(-6.50422626476366,-4.50322187534129,
92.5450743426261));
#225063=CARTESIAN_POINT('Ctrl Pts',(-6.49334867548826,-4.51890430825782,
92.5458469986067));
#225064=CARTESIAN_POINT('Ctrl Pts',(-6.48629445341719,-4.52902389375338,
92.5463473934074));
#225065=CARTESIAN_POINT('Ctrl Pts',(-6.4568179292362,-4.57109911862609,
92.54843565204));
#225066=CARTESIAN_POINT('Ctrl Pts',(-6.43418314635648,-4.60290474521572,
92.5500327995815));
#225067=CARTESIAN_POINT('Ctrl Pts',(-6.07306714245963,-5.10246404580114,
92.575431774828));
#225068=CARTESIAN_POINT('Ctrl Pts',(-5.68468124080384,-5.53185391562479,
92.6020957239176));
#225069=CARTESIAN_POINT('Ctrl Pts',(-5.11885266772687,-6.03436248066652,
92.6367696783688));
#225070=CARTESIAN_POINT('Ctrl Pts',(-4.98052718605918,-6.14902709888229,
92.6449725018298));
#225071=CARTESIAN_POINT('Ctrl Pts',(-4.63168936426824,-6.41869534487419,
92.6648755179029));
#225072=CARTESIAN_POINT('Ctrl Pts',(-4.41716260374373,-6.56817208396009,
92.6764538430598));
#225073=CARTESIAN_POINT('Ctrl Pts',(-4.06681200061117,-6.78734453143579,
92.6942107741201));
#225074=CARTESIAN_POINT('Ctrl Pts',(-3.93570524263836,-6.86419937992903,
92.7006189097873));
#225075=CARTESIAN_POINT('Ctrl Pts',(-3.75716715237918,-6.96206032262379,
92.7090288612561));
#225076=CARTESIAN_POINT('Ctrl Pts',(-3.71163026549438,-6.98644329038017,
92.7111470889938));
#225077=CARTESIAN_POINT('Ctrl Pts',(-3.64541325462485,-7.02106939495927,
92.7141889823475));
#225078=CARTESIAN_POINT('Ctrl Pts',(-3.62492246132342,-7.03167052746739,
92.7151250402943));
#225079=CARTESIAN_POINT('Ctrl Pts',(-3.5882089842486,-7.05046151082425,
92.7167928508726));
#225080=CARTESIAN_POINT('Ctrl Pts',(-3.57200394584062,-7.05868536250372,
92.7175257785663));
#225081=CARTESIAN_POINT('Ctrl Pts',(-3.54763615075159,-7.07094630613488,
92.7186230734468));
#225082=CARTESIAN_POINT('Ctrl Pts',(-3.53949457859831,-7.07502523325229,
92.7189888877827));
#225083=CARTESIAN_POINT('Ctrl Pts',(-3.52548750805267,-7.08201254536804,
92.7196168693265));
#225084=CARTESIAN_POINT('Ctrl Pts',(-3.51962541797617,-7.08492771872567,
92.7198792710638));
#225085=CARTESIAN_POINT('Ctrl Pts',(-3.50755256984423,-7.09091277391166,
92.7204188308959));
#225086=CARTESIAN_POINT('Ctrl Pts',(-3.50134138404111,-7.09398178106876,
92.7206959586091));
#225087=CARTESIAN_POINT('Ctrl Pts',(-3.48639139773006,-7.10134429684321,
92.7213618800303));
#225088=CARTESIAN_POINT('Ctrl Pts',(-3.47764867637372,-7.10562984436176,
92.7217503987316));
#225089=CARTESIAN_POINT('Ctrl Pts',(-3.45083963354855,-7.11870989416034,
92.7229389891278));
#225090=CARTESIAN_POINT('Ctrl Pts',(-3.43274763695967,-7.12745174674585,
92.7237372452002));
#225091=CARTESIAN_POINT('Ctrl Pts',(-3.22890593023575,-7.22498962682392,
92.7326881233595));
#225092=CARTESIAN_POINT('Ctrl Pts',(-3.03978456449599,-7.30657415660692,
92.740588629205));
#225093=CARTESIAN_POINT('Ctrl Pts',(-2.49757698115558,-7.51577367860479,
92.7622555933756));
#225094=CARTESIAN_POINT('Ctrl Pts',(-2.13828685354568,-7.62577860371302,
92.7754524668928));
#225095=CARTESIAN_POINT('Ctrl Pts',(-1.49926631792096,-7.772692036761,92.7979739588008));
#225096=CARTESIAN_POINT('Ctrl Pts',(-1.22285744503376,-7.82094367356461,
92.8074265627922));
#225097=CARTESIAN_POINT('Ctrl Pts',(-0.832815915349954,-7.86784506087785,
92.820879457616));
#225098=CARTESIAN_POINT('Ctrl Pts',(-0.720887854965985,-7.87888877844551,
92.824754039082));
#225099=CARTESIAN_POINT('Ctrl Pts',(-0.452133448357972,-7.89963135618467,
92.8341568930095));
#225100=CARTESIAN_POINT('Ctrl Pts',(-0.295182120274044,-7.90705158855909,
92.8397288157136));
#225101=CARTESIAN_POINT('Ctrl Pts',(0.0501372317934248,-7.91308148057443,
92.8523405174425));
#225102=CARTESIAN_POINT('Ctrl Pts',(0.238439895594762,-7.9096466523416,
92.8594480916385));
#225103=CARTESIAN_POINT('Ctrl Pts',(0.453820756865387,-7.89802001993127,
92.8680060939527));
#225104=CARTESIAN_POINT('Ctrl Pts',(0.481204685471592,-7.89639889639212,
92.8691021304385));
#225105=CARTESIAN_POINT('Ctrl Pts',(0.515931635378348,-7.89416175591615,
92.8705027322171));
#225106=CARTESIAN_POINT('Ctrl Pts',(0.523283267102684,-7.89367784385905,
92.8707998435465));
#225107=CARTESIAN_POINT('Ctrl Pts',(0.535024615419098,-7.89288850952927,
92.8712753449931));
#225108=CARTESIAN_POINT('Ctrl Pts',(0.53941478669654,-7.89258969228144,
92.8714533577446));
#225109=CARTESIAN_POINT('Ctrl Pts',(0.547708930880645,-7.89201819830882,
92.8717900870345));
#225110=CARTESIAN_POINT('Ctrl Pts',(0.551612956943343,-7.89174628716801,
92.8719487594642));
#225111=CARTESIAN_POINT('Ctrl Pts',(0.560421157791934,-7.89112623762177,
92.8723071516092));
#225112=CARTESIAN_POINT('Ctrl Pts',(0.565325209022588,-7.89077642440936,
92.8725069683021));
#225113=CARTESIAN_POINT('Ctrl Pts',(0.577851127287873,-7.88987119515674,
92.8730180574294));
#225114=CARTESIAN_POINT('Ctrl Pts',(0.585472520853694,-7.88930930617988,
92.8733297085931));
#225115=CARTESIAN_POINT('Ctrl Pts',(0.630884317619753,-7.88589514434616,
92.8751907725022));
#225116=CARTESIAN_POINT('Ctrl Pts',(0.668654019531223,-7.88278243742453,
92.8767555422772));
#225117=CARTESIAN_POINT('Ctrl Pts',(1.31915090443823,-7.82446446900298,
92.90397700445));
#225118=CARTESIAN_POINT('Ctrl Pts',(1.92337088229537,-7.69824570717951,
92.9332463235326));
#225119=CARTESIAN_POINT('Ctrl Pts',(2.79779135388342,-7.40610513746522,
92.9759252735163));
#225120=CARTESIAN_POINT('Ctrl Pts',(3.08286788282679,-7.29204886941688,
92.9899285621019));
#225121=CARTESIAN_POINT('Ctrl Pts',(3.55501379689497,-7.07049573562311,
93.0128962197114));
#225122=CARTESIAN_POINT('Ctrl Pts',(3.74562634417476,-6.97139342888992,
93.0221060445501));
#225123=CARTESIAN_POINT('Ctrl Pts',(3.98772276131054,-6.83272380931817,
93.0336953026738));
#225124=CARTESIAN_POINT('Ctrl Pts',(4.04307394327187,-6.80011770785419,
93.0363376968675));
#225125=CARTESIAN_POINT('Ctrl Pts',(4.12076090437963,-6.75307020624562,
93.0400364374367));
#225126=CARTESIAN_POINT('Ctrl Pts',(4.14342960387535,-6.73918532010579,
93.0411145054489));
#225127=CARTESIAN_POINT('Ctrl Pts',(4.17777028518914,-6.71791241639486,
93.0427458869343));
#225128=CARTESIAN_POINT('Ctrl Pts',(4.18949349500327,-6.71060772569821,
93.0433024907732));
#225129=CARTESIAN_POINT('Ctrl Pts',(4.20856312930315,-6.69865605539308,
93.0442073887338));
#225130=CARTESIAN_POINT('Ctrl Pts',(4.21592110589361,-6.69402762104716,
93.0445564186348));
#225131=CARTESIAN_POINT('Ctrl Pts',(4.23016462653967,-6.68503512985991,
93.0452318334574));
#225132=CARTESIAN_POINT('Ctrl Pts',(4.23705108102411,-6.68067254042836,
93.0455582761753));
#225133=CARTESIAN_POINT('Ctrl Pts',(4.24897797505282,-6.67309095809721,
93.0461234716154));
#225134=CARTESIAN_POINT('Ctrl Pts',(4.25402152347942,-6.66987688383469,
93.0463624202564));
#225135=CARTESIAN_POINT('Ctrl Pts',(4.26449053864898,-6.66318864741752,
93.0468582954444));
#225136=CARTESIAN_POINT('Ctrl Pts',(4.26991541733665,-6.6597135699945,93.0471151851519));
#225137=CARTESIAN_POINT('Ctrl Pts',(4.28472824441541,-6.65019920586704,
93.0478164564955));
#225138=CARTESIAN_POINT('Ctrl Pts',(4.29410768227187,-6.64414665857638,
93.0482603066853));
#225139=CARTESIAN_POINT('Ctrl Pts',(4.32972733759817,-6.62105437828654,
93.0499451716143));
#225140=CARTESIAN_POINT('Ctrl Pts',(4.35587936853312,-6.60387877352104,
93.0511807229141));
#225141=CARTESIAN_POINT('Ctrl Pts',(4.76406439674376,-6.33231956949401,
93.0704440758127));
#225142=CARTESIAN_POINT('Ctrl Pts',(5.12337140268718,-6.04530470249025,
93.0870273555765));
#225143=CARTESIAN_POINT('Ctrl Pts',(5.81347914967821,-5.38807634900018,
93.1199413898806));
#225144=CARTESIAN_POINT('Ctrl Pts',(6.13846185931715,-5.01469429243429,
93.1360883442968));
#225145=CARTESIAN_POINT('Ctrl Pts',(6.47235547374767,-4.54958447763153,
93.1560966421463));
#225146=CARTESIAN_POINT('Ctrl Pts',(6.51725684192208,-4.48502699800584,
93.1588736174151));
#225147=CARTESIAN_POINT('Ctrl Pts',(6.62741212455137,-4.32150205945998,
93.1659349775229));
#225148=CARTESIAN_POINT('Ctrl Pts',(6.69141659073724,-4.22171927942477,
93.1702682016949));
#225149=CARTESIAN_POINT('Ctrl Pts',(6.81100185861919,-4.02573097601757,
93.1789020253756));
#225150=CARTESIAN_POINT('Ctrl Pts',(6.86684546382416,-3.92971849728949,
93.1831865549045));
#225151=CARTESIAN_POINT('Ctrl Pts',(6.9300234931657,-3.81563493860856,93.1883802159809));
#225152=CARTESIAN_POINT('Ctrl Pts',(6.93933778128576,-3.79866907542071,
93.1891552148171));
#225153=CARTESIAN_POINT('Ctrl Pts',(6.95155493025224,-3.77622080013829,
93.190184345447));
#225154=CARTESIAN_POINT('Ctrl Pts',(6.95451381331411,-3.77076876778859,
93.1904345784268));
#225155=CARTESIAN_POINT('Ctrl Pts',(6.95936724639826,-3.76180069667185,
93.1908466680273));
#225156=CARTESIAN_POINT('Ctrl Pts',(6.96126554484257,-3.75828670617201,
93.1910082591212));
#225157=CARTESIAN_POINT('Ctrl Pts',(6.96495386352822,-3.75144678024166,
93.1913230257674));
#225158=CARTESIAN_POINT('Ctrl Pts',(6.96674416496649,-3.7481209966951,93.1914761817259));
#225159=CARTESIAN_POINT('Ctrl Pts',(6.97089350013284,-3.74039967058265,
93.1918320023187));
#225160=CARTESIAN_POINT('Ctrl Pts',(6.97325075703691,-3.73600318055833,
93.1920347892064));
#225161=CARTESIAN_POINT('Ctrl Pts',(6.98086898587666,-3.72176218937561,
93.1926922393008));
#225162=CARTESIAN_POINT('Ctrl Pts',(6.98611325987225,-3.7119088229527,93.1931480394696));
#225163=CARTESIAN_POINT('Ctrl Pts',(7.03523950192268,-3.61913357369488,
93.1974479609954));
#225164=CARTESIAN_POINT('Ctrl Pts',(7.07766230447068,-3.53545153765817,
93.2013886367707));
#225165=CARTESIAN_POINT('Ctrl Pts',(7.34323923851818,-2.98763611351291,
93.2274853362286));
#225166=CARTESIAN_POINT('Ctrl Pts',(7.52209281168821,-2.50343451769239,
93.251858772893));
#225167=CARTESIAN_POINT('Ctrl Pts',(7.73667318431216,-1.68456651734583,
93.2916331421163));
#225168=CARTESIAN_POINT('Ctrl Pts',(7.80048132052756,-1.35881894988339,
93.3071163607108));
#225169=CARTESIAN_POINT('Ctrl Pts',(7.88312283668575,-0.729495809077691,
93.3357927506921));
#225170=CARTESIAN_POINT('Ctrl Pts',(7.90528555523668,-0.426939614350551,
93.3490467108417));
#225171=CARTESIAN_POINT('Ctrl Pts',(7.91189723898176,-0.00460770748252659,
93.3667292619499));
#225172=CARTESIAN_POINT('Ctrl Pts',(7.91106799101316,0.114647751889499,
93.3716335736553));
#225173=CARTESIAN_POINT('Ctrl Pts',(7.90704156296035,0.250804025094959,
93.3771360921947));
#225174=CARTESIAN_POINT('Ctrl Pts',(7.9064854089161,0.267763740682974,93.3778197792648));
#225175=CARTESIAN_POINT('Ctrl Pts',(7.90556408676369,0.293346124639158,
93.3788485144518));
#225176=CARTESIAN_POINT('Ctrl Pts',(7.90523937084471,0.301970145961379,
93.3791948714548));
#225177=CARTESIAN_POINT('Ctrl Pts',(7.90465493970392,0.316844468840303,
93.3797915019353));
#225178=CARTESIAN_POINT('Ctrl Pts',(7.90440192196381,0.323095016218909,
93.3800419917666));
#225179=CARTESIAN_POINT('Ctrl Pts',(7.90386391937633,0.336006841605739,
93.3805589612405));
#225180=CARTESIAN_POINT('Ctrl Pts',(7.90357792679258,0.342668074144689,
93.3808254081194));
#225181=CARTESIAN_POINT('Ctrl Pts',(7.90278128627859,0.360691418258543,
93.3815456391873));
#225182=CARTESIAN_POINT('Ctrl Pts',(7.9022545552573,0.372052823275241,93.3819989037226));
#225183=CARTESIAN_POINT('Ctrl Pts',(7.90020875533877,0.414214410003667,
93.3836781907799));
#225184=CARTESIAN_POINT('Ctrl Pts',(7.8985340914399,0.445006954890051,93.3848991939718));
#225185=CARTESIAN_POINT('Ctrl Pts',(7.86824129531418,0.947776927959096,
93.4047485300279));
#225186=CARTESIAN_POINT('Ctrl Pts',(7.79754359296911,1.41628977528384,93.421913978139));
#225187=CARTESIAN_POINT('Ctrl Pts',(7.56526084763376,2.36802920960121,93.456195367089));
#225188=CARTESIAN_POINT('Ctrl Pts',(7.3980855505712,2.84763391166258,93.4731518462819));
#225189=CARTESIAN_POINT('Ctrl Pts',(7.09080731427141,3.51517012172091,93.4997264244385));
#225190=CARTESIAN_POINT('Ctrl Pts',(6.98649305502315,3.71818323144582,93.5082665550157));
#225191=CARTESIAN_POINT('Ctrl Pts',(6.85505131169054,3.9488717828786,93.5187732418155));
#225192=CARTESIAN_POINT('Ctrl Pts',(6.83632591529052,3.98120142137484,93.5202632020728));
#225193=CARTESIAN_POINT('Ctrl Pts',(6.81196052771146,4.0225897837538,93.5221922560521));
#225194=CARTESIAN_POINT('Ctrl Pts',(6.80653004293423,4.03177176593947,93.5226215917408));
#225195=CARTESIAN_POINT('Ctrl Pts',(6.79775449156869,4.04654139772446,93.523314388061));
#225196=CARTESIAN_POINT('Ctrl Pts',(6.79442105717944,4.05213596866749,93.5235773190727));
#225197=CARTESIAN_POINT('Ctrl Pts',(6.78806251204761,4.06277773919609,93.5240784151784));
#225198=CARTESIAN_POINT('Ctrl Pts',(6.78503866942263,4.06782569436965,93.5243165232858));
#225199=CARTESIAN_POINT('Ctrl Pts',(6.77813728577621,4.07931765075101,93.5248595216778));
#225200=CARTESIAN_POINT('Ctrl Pts',(6.77425618525469,4.08575950058308,93.5251645695953));
#225201=CARTESIAN_POINT('Ctrl Pts',(6.76267561736756,4.10491906333621,93.5260738268494));
#225202=CARTESIAN_POINT('Ctrl Pts',(6.75494950345145,4.11762057800221,93.5266791969676));
#225203=CARTESIAN_POINT('Ctrl Pts',(6.70063243420383,4.20635201233481,93.5309260961685));
#225204=CARTESIAN_POINT('Ctrl Pts',(6.65279568702758,4.28160964000401,93.5346199660138));
#225205=CARTESIAN_POINT('Ctrl Pts',(6.49060547752171,4.52748777581894,93.5469626826401));
#225206=CARTESIAN_POINT('Ctrl Pts',(6.37088220214842,4.69446053740996,93.5557882744055));
#225207=CARTESIAN_POINT('Ctrl Pts',(5.73738355623192,5.50904076248536,93.6006092768132));
#225208=CARTESIAN_POINT('Ctrl Pts',(5.13074565646177,6.07806307536993,93.6371338650679));
#225209=CARTESIAN_POINT('Ctrl Pts',(4.40287684945072,6.57278043374012,93.6730914924105));
#225210=CARTESIAN_POINT('Ctrl Pts',(4.35845152702862,6.602322890394,93.675261735693));
#225211=CARTESIAN_POINT('Ctrl Pts',(4.27987143886916,6.6534391867632,93.6790589930235));
#225212=CARTESIAN_POINT('Ctrl Pts',(4.24584397623971,6.67520497888694,93.6806899270685));
#225213=CARTESIAN_POINT('Ctrl Pts',(4.19668176798468,6.70612375777788,93.6830272510761));
#225214=CARTESIAN_POINT('Ctrl Pts',(4.18168077487292,6.71548804007421,93.6837379134559));
#225215=CARTESIAN_POINT('Ctrl Pts',(4.15561175855939,6.73164025207384,93.6849685285133));
#225216=CARTESIAN_POINT('Ctrl Pts',(4.14455820671209,6.73845136834701,93.6854889619464));
#225217=CARTESIAN_POINT('Ctrl Pts',(4.12327685056646,6.75149260785739,93.6864883362116));
#225218=CARTESIAN_POINT('Ctrl Pts',(4.11305157122084,6.75772677708905,93.6869673610576));
#225219=CARTESIAN_POINT('Ctrl Pts',(4.08892038560573,6.7723640676628,93.6880951185734));
#225220=CARTESIAN_POINT('Ctrl Pts',(4.07500265616423,6.78074762392845,93.6887434352382));
#225221=CARTESIAN_POINT('Ctrl Pts',(4.03374708655778,6.80542565176369,93.6906589449656));
#225222=CARTESIAN_POINT('Ctrl Pts',(4.00633655104851,6.8215981498265,93.691923520908));
#225223=CARTESIAN_POINT('Ctrl Pts',(3.73788080786514,6.97781359786196,93.7042300672765));
#225224=CARTESIAN_POINT('Ctrl Pts',(3.48968357178826,7.10519215339375,93.7149812447937));
#225225=CARTESIAN_POINT('Ctrl Pts',(2.8198451895752,7.40537853194782,93.7426375706072));
#225226=CARTESIAN_POINT('Ctrl Pts',(2.38913294412111,7.5553429467244,93.7590342458436));
#225227=CARTESIAN_POINT('Ctrl Pts',(1.74852787663755,7.71808851307111,93.7831396311856));
#225228=CARTESIAN_POINT('Ctrl Pts',(1.54724990728456,7.76094413759684,93.7906870954495));
#225229=CARTESIAN_POINT('Ctrl Pts',(1.17116705281317,7.82580600339481,93.8050369900584));
#225230=CARTESIAN_POINT('Ctrl Pts',(0.996855508088804,7.84991374547872,
93.8117857421288));
#225231=CARTESIAN_POINT('Ctrl Pts',(0.793540975126717,7.87115152685873,
93.8199037060692));
#225232=CARTESIAN_POINT('Ctrl Pts',(0.765172884231253,7.87395987200559,
93.8210419599621));
#225233=CARTESIAN_POINT('Ctrl Pts',(0.727955951045604,7.87744120037873,
93.8225432434986));
#225234=CARTESIAN_POINT('Ctrl Pts',(0.719120049607398,7.87825273048601,
93.8229002614678));
#225235=CARTESIAN_POINT('Ctrl Pts',(0.704712803339993,7.87955151909762,
93.8234833773497));
#225236=CARTESIAN_POINT('Ctrl Pts',(0.699142258559244,7.88004773966276,
93.8237090785524));
#225237=CARTESIAN_POINT('Ctrl Pts',(0.688418471399684,7.88099154704123,
93.8241440429175));
#225238=CARTESIAN_POINT('Ctrl Pts',(0.683265305541657,7.88143998761343,
93.8243532677057));
#225239=CARTESIAN_POINT('Ctrl Pts',(0.671468575278274,7.88245491013709,
93.8248327141972));
#225240=CARTESIAN_POINT('Ctrl Pts',(0.664824733326373,7.88301804713609,
93.8251030873265));
#225241=CARTESIAN_POINT('Ctrl Pts',(0.643952603914165,7.88476061015299,
93.8259536113917));
#225242=CARTESIAN_POINT('Ctrl Pts',(0.629721888180468,7.88590991419918,
93.8265351467812));
#225243=CARTESIAN_POINT('Ctrl Pts',(0.494167361238814,7.89648833371844,
93.8320908375226));
#225244=CARTESIAN_POINT('Ctrl Pts',(0.372657028259306,7.90315449398576,
93.8372034640449));
#225245=CARTESIAN_POINT('Ctrl Pts',(0.044010437756169,7.91358911027385,
93.851326418367));
#225246=CARTESIAN_POINT('Ctrl Pts',(-0.163197428941168,7.91202803036976,
93.8605406246455));
#225247=CARTESIAN_POINT('Ctrl Pts',(-0.942609019082659,7.87552550398702,
93.8958621692219));
#225248=CARTESIAN_POINT('Ctrl Pts',(-1.51052601414932,7.78657729178238,
93.922822854702));
#225249=CARTESIAN_POINT('Ctrl Pts',(-2.45583749880284,7.53111150939652,
93.9665911341828));
#225250=CARTESIAN_POINT('Ctrl Pts',(-2.8390950056219,7.39515911864513,93.98403220925));
#225251=CARTESIAN_POINT('Ctrl Pts',(-3.23336712280999,7.22010370088025,
94.0015458693013));
#225252=CARTESIAN_POINT('Ctrl Pts',(-3.2564287748672,7.20973176001715,94.0025688248642));
#225253=CARTESIAN_POINT('Ctrl Pts',(-3.289144640983,7.19482885433623,94.0040180158385));
#225254=CARTESIAN_POINT('Ctrl Pts',(-3.29883992084115,7.19038871621482,
94.0044472299036));
#225255=CARTESIAN_POINT('Ctrl Pts',(-3.31551391633487,7.18271171976697,
94.0051849690741));
#225256=CARTESIAN_POINT('Ctrl Pts',(-3.32249693096221,7.17948426579795,
94.0054938030563));
#225257=CARTESIAN_POINT('Ctrl Pts',(-3.33582056485977,7.17330266259076,
94.006082816973));
#225258=CARTESIAN_POINT('Ctrl Pts',(-3.34216199265932,7.17035028050864,
94.0063630547244));
#225259=CARTESIAN_POINT('Ctrl Pts',(-3.35695089770015,7.16344112044127,
94.0070163565512));
#225260=CARTESIAN_POINT('Ctrl Pts',(-3.36539531719436,7.15947780046607,
94.0073892043283));
#225261=CARTESIAN_POINT('Ctrl Pts',(-3.39516599821417,7.14544086325066,
94.008703028755));
#225262=CARTESIAN_POINT('Ctrl Pts',(-3.41645429269883,7.13528677512961,
94.0096413426246));
#225263=CARTESIAN_POINT('Ctrl Pts',(-3.64427234825545,7.02536883700728,
94.0196707365327));
#225264=CARTESIAN_POINT('Ctrl Pts',(-3.84642311307951,6.91675987626382,
94.0284595773323));
#225265=CARTESIAN_POINT('Ctrl Pts',(-4.20178737822674,6.70542956646218,
94.0438416196255));
#225266=CARTESIAN_POINT('Ctrl Pts',(-4.35666790088356,6.60584978440244,
94.0505218341207));
#225267=CARTESIAN_POINT('Ctrl Pts',(-5.05429608060325,6.12209553391066,
94.0807859764034));
#225268=CARTESIAN_POINT('Ctrl Pts',(-5.55067548035882,5.67590264991658,
94.1026395842793));
#225269=CARTESIAN_POINT('Ctrl Pts',(-6.06629520315752,5.07930088074213,
94.1313435886781));
#225270=CARTESIAN_POINT('Ctrl Pts',(-6.14500339632481,4.98379035997132,
94.1359314726989));
#225271=CARTESIAN_POINT('Ctrl Pts',(-6.29614708634102,4.79135498140239,
94.1452336258219));
#225272=CARTESIAN_POINT('Ctrl Pts',(-6.3686573440028,4.69454493083037,94.1499490730039));
#225273=CARTESIAN_POINT('Ctrl Pts',(-6.44774678490864,4.58374443732366,
94.1553886517839));
#225274=CARTESIAN_POINT('Ctrl Pts',(-6.4565348812596,4.57135745616198,94.1559972312646));
#225275=CARTESIAN_POINT('Ctrl Pts',(-6.46969394550482,4.5526958745461,94.1569146884381));
#225276=CARTESIAN_POINT('Ctrl Pts',(-6.47409160484178,4.54644007617127,
94.1572223430037));
#225277=CARTESIAN_POINT('Ctrl Pts',(-6.48164502223485,4.53566193803275,
94.1577525641087));
#225278=CARTESIAN_POINT('Ctrl Pts',(-6.48480513953105,4.53114264976563,
94.1579749354299));
#225279=CARTESIAN_POINT('Ctrl Pts',(-6.49130864574305,4.52182123755353,
94.1584336900456));
#225280=CARTESIAN_POINT('Ctrl Pts',(-6.49465143644311,4.51701870237035,
94.1586700993812));
#225281=CARTESIAN_POINT('Ctrl Pts',(-6.50364540311766,4.50406658721538,
94.1593078105225));
#225282=CARTESIAN_POINT('Ctrl Pts',(-6.5092865786265,4.49591009561214,94.1597095435943));
#225283=CARTESIAN_POINT('Ctrl Pts',(-6.52999850518052,4.46584233423246,
94.1611909318397));
#225284=CARTESIAN_POINT('Ctrl Pts',(-6.54497399374246,4.44386584336544,
94.1622745649921));
#225285=CARTESIAN_POINT('Ctrl Pts',(-6.64584547236964,4.29422125743691,
94.1696573567015));
#225286=CARTESIAN_POINT('Ctrl Pts',(-6.72810940619944,4.16414928980825,
94.1760933792891));
#225287=CARTESIAN_POINT('Ctrl Pts',(-6.81040714676181,4.02521223178472,
94.1829337085062));
#225288=CARTESIAN_POINT('Ctrl Pts',(-6.81427950313355,4.01865324064847,
94.18325655262));
#225289=CARTESIAN_POINT('Ctrl Pts',(-6.83221206120797,3.98817865642534,
94.1847561796137));
#225290=CARTESIAN_POINT('Ctrl Pts',(-6.84615582458517,3.96419488157962,
94.1859353105009));
#225291=CARTESIAN_POINT('Ctrl Pts',(-6.8728184469609,3.91777395524983,94.1882149379885));
#225292=CARTESIAN_POINT('Ctrl Pts',(-6.88555432364497,3.89534694443504,
94.1893151187998));
#225293=CARTESIAN_POINT('Ctrl Pts',(-7.2239141726075,3.29267389086386,94.2188435588778));
#225294=CARTESIAN_POINT('Ctrl Pts',(-7.4751656363043,2.67369422110814,94.2479024486583));
#225295=CARTESIAN_POINT('Ctrl Pts',(-7.72152983219981,1.74601342728185,
94.2880591896939));
#225296=CARTESIAN_POINT('Ctrl Pts',(-7.78115169498604,1.45748777314945,
94.300164573372));
#225297=CARTESIAN_POINT('Ctrl Pts',(-7.84209318887623,1.04864093691202,
94.317040744289));
#225298=CARTESIAN_POINT('Ctrl Pts',(-7.85697562913057,0.930595354712951,
94.321885558924));
#225299=CARTESIAN_POINT('Ctrl Pts',(-7.87752105116231,0.73155060892787,
94.3300053577431));
#225300=CARTESIAN_POINT('Ctrl Pts',(-7.88460965892463,0.650718720851011,
94.3332890979757));
#225301=CARTESIAN_POINT('Ctrl Pts',(-7.89289316547287,0.536009048793502,
94.3379295905942));
#225302=CARTESIAN_POINT('Ctrl Pts',(-7.89511572941062,0.502210962620324,
94.339294478028));
#225303=CARTESIAN_POINT('Ctrl Pts',(-7.89858305094691,0.443752629603006,
94.341651150523));
#225304=CARTESIAN_POINT('Ctrl Pts',(-7.89992953729559,0.419098936628841,
94.342643778216));
#225305=CARTESIAN_POINT('Ctrl Pts',(-7.90229472965168,0.371720887862366,
94.3445489748828));
#225306=CARTESIAN_POINT('Ctrl Pts',(-7.90333088359629,0.348997650837556,
94.3454616860851));
#225307=CARTESIAN_POINT('Ctrl Pts',(-7.90554565331897,0.295342323872047,
94.3476143889633));
#225308=CARTESIAN_POINT('Ctrl Pts',(-7.90664075587045,0.264407130490534,
94.3488536244774));
#225309=CARTESIAN_POINT('Ctrl Pts',(-7.90985060311432,0.155688880748797,
94.3532022416483));
#225310=CARTESIAN_POINT('Ctrl Pts',(-7.91099931732731,0.0778814711349728,
94.3563026675399));
#225311=CARTESIAN_POINT('Ctrl Pts',(-7.91100311735682,-0.355436634977919,
94.3735104335096));
#225312=CARTESIAN_POINT('Ctrl Pts',(-7.88704271218661,-0.710543157949429,
94.3873734868895));
#225313=CARTESIAN_POINT('Ctrl Pts',(-7.80633970902302,-1.30579201857021,
94.4106411291279));
#225314=CARTESIAN_POINT('Ctrl Pts',(-7.76212394814162,-1.54708234257868,
94.4200865099885));
#225315=CARTESIAN_POINT('Ctrl Pts',(-7.64608724613857,-2.04781279598876,
94.4400198483939));
#225316=CARTESIAN_POINT('Ctrl Pts',(-7.57209172869083,-2.30642729521904,
94.4505075308377));
#225317=CARTESIAN_POINT('Ctrl Pts',(-7.47618419940208,-2.58676358543974,
94.4623626944828));
#225318=CARTESIAN_POINT('Ctrl Pts',(-7.46715436354632,-2.6127153937246,
94.4634649042376));
#225319=CARTESIAN_POINT('Ctrl Pts',(-7.45359948224675,-2.65102791368683,
94.4650995299478));
#225320=CARTESIAN_POINT('Ctrl Pts',(-7.44917846992508,-2.66342530637054,
94.4656296281301));
#225321=CARTESIAN_POINT('Ctrl Pts',(-7.44127971493652,-2.68540146918219,
94.4665714138426));
#225322=CARTESIAN_POINT('Ctrl Pts',(-7.43781436076781,-2.69498467169194,
94.4669828144461));
#225323=CARTESIAN_POINT('Ctrl Pts',(-7.43050825356696,-2.71506778792675,
94.4678464985998));
#225324=CARTESIAN_POINT('Ctrl Pts',(-7.42666374026287,-2.72556630582662,
94.4682988707544));
#225325=CARTESIAN_POINT('Ctrl Pts',(-7.41644416267689,-2.75329155437023,
94.4694959036888));
#225326=CARTESIAN_POINT('Ctrl Pts',(-7.41003138084584,-2.77050416561249,
94.4702415036757));
#225327=CARTESIAN_POINT('Ctrl Pts',(-7.3751378736,-2.86317434392187,94.4742689563162));
#225328=CARTESIAN_POINT('Ctrl Pts',(-7.34556475986508,-2.93821442608593,
94.477577251185));
#225329=CARTESIAN_POINT('Ctrl Pts',(-7.25214224166292,-3.16503810086119,
94.4877044270859));
#225330=CARTESIAN_POINT('Ctrl Pts',(-7.18469743902851,-3.31529099579833,
94.4945876254037));
#225331=CARTESIAN_POINT('Ctrl Pts',(-6.87751762639847,-3.94614434673074,
94.5240726357052));
#225332=CARTESIAN_POINT('Ctrl Pts',(-6.59385787640216,-4.40379155007968,
94.546841043515));
#225333=CARTESIAN_POINT('Ctrl Pts',(-6.17976896788432,-4.94108714641089,
94.5747346564772));
#225334=CARTESIAN_POINT('Ctrl Pts',(-6.09053017596727,-5.0506761822404,
94.5804999236285));
#225335=CARTESIAN_POINT('Ctrl Pts',(-5.97312099419522,-5.18721989677197,
94.587790126787));
#225336=CARTESIAN_POINT('Ctrl Pts',(-5.94762311156027,-5.21643594927226,
94.5893565008894));
#225337=CARTESIAN_POINT('Ctrl Pts',(-5.90685747058384,-5.2624586724597,
94.5918346563528));
#225338=CARTESIAN_POINT('Ctrl Pts',(-5.89173045790178,-5.27938904351281,
94.5927486278947));
#225339=CARTESIAN_POINT('Ctrl Pts',(-5.86326501852637,-5.31097325880319,
94.5944581533772));
#225340=CARTESIAN_POINT('Ctrl Pts',(-5.84994401770068,-5.32564255519518,
94.5952539716704));
#225341=CARTESIAN_POINT('Ctrl Pts',(-5.8197567849657,-5.35863529000138,
94.5970480695286));
#225342=CARTESIAN_POINT('Ctrl Pts',(-5.80285884728956,-5.37692945938086,
94.5980458452744));
#225343=CARTESIAN_POINT('Ctrl Pts',(-5.75228805457715,-5.43116272858518,
94.6010128568565));
#225344=CARTESIAN_POINT('Ctrl Pts',(-5.71836559191151,-5.46686760802811,
94.6029782021669));
#225345=CARTESIAN_POINT('Ctrl Pts',(-5.39471560465398,-5.80121474382613,
94.6215026173401));
#225346=CARTESIAN_POINT('Ctrl Pts',(-5.08217254270664,-6.07688957964575,
94.6377550941958));
#225347=CARTESIAN_POINT('Ctrl Pts',(-4.23646627352083,-6.71175391712623,
94.6786001540875));
#225348=CARTESIAN_POINT('Ctrl Pts',(-3.67861936862207,-7.03299680558552,
94.7023284389113));
#225349=CARTESIAN_POINT('Ctrl Pts',(-2.77958218484106,-7.41418633553808,
94.7390221070907));
#225350=CARTESIAN_POINT('Ctrl Pts',(-2.46304921729124,-7.52526423277672,
94.7517388038982));
#225351=CARTESIAN_POINT('Ctrl Pts',(-2.12178906712441,-7.62117496172933,
94.7658845745831));
#225352=CARTESIAN_POINT('Ctrl Pts',(-2.10311134444142,-7.62635032689576,
94.7666601978689));
#225353=CARTESIAN_POINT('Ctrl Pts',(-2.07550831575809,-7.63388966884469,
94.7678087275509));
#225354=CARTESIAN_POINT('Ctrl Pts',(-2.06659751991481,-7.63630676012746,
94.7681798436649));
#225355=CARTESIAN_POINT('Ctrl Pts',(-2.05139826970505,-7.64040106909934,
94.7688134796344));
#225356=CARTESIAN_POINT('Ctrl Pts',(-2.04511192876923,-7.64208613901881,
94.7690757288671));
#225357=CARTESIAN_POINT('Ctrl Pts',(-2.03292525048982,-7.64533669570523,
94.7695844836222));
#225358=CARTESIAN_POINT('Ctrl Pts',(-2.02702516587332,-7.64690311442734,
94.7698309563094));
#225359=CARTESIAN_POINT('Ctrl Pts',(-2.01298312185734,-7.65061375579703,
94.7704179528391));
#225360=CARTESIAN_POINT('Ctrl Pts',(-2.0048395495188,-7.65275181025254,
94.7707586950401));
#225361=CARTESIAN_POINT('Ctrl Pts',(-1.98066483169606,-7.65905752633964,
94.7717711876686));
#225362=CARTESIAN_POINT('Ctrl Pts',(-1.96462404742732,-7.66318782978493,
94.7724442869267));
#225363=CARTESIAN_POINT('Ctrl Pts',(-1.8322429071636,-7.69683136388682,
94.7780104482887));
#225364=CARTESIAN_POINT('Ctrl Pts',(-1.71526177069653,-7.72374287066485,
94.783003628501));
#225365=CARTESIAN_POINT('Ctrl Pts',(-1.50449684846218,-7.76720467731892,
94.7921740754335));
#225366=CARTESIAN_POINT('Ctrl Pts',(-1.41094638844822,-7.78474203441101,
94.7962995881021));
#225367=CARTESIAN_POINT('Ctrl Pts',(-1.12152431016233,-7.83361006070977,
94.8091888406299));
#225368=CARTESIAN_POINT('Ctrl Pts',(-0.924777211435029,-7.85926491513839,
94.8181265007611));
#225369=CARTESIAN_POINT('Ctrl Pts',(-0.216809522595592,-7.92462729157328,
94.8504963226563));
#225370=CARTESIAN_POINT('Ctrl Pts',(0.297075373271897,-7.92202815092615,
94.8742940643039));
#225371=CARTESIAN_POINT('Ctrl Pts',(0.958710551606543,-7.85417227414245,
94.9036474528743));
#225372=CARTESIAN_POINT('Ctrl Pts',(1.10984289361545,-7.83424532252421,
94.9102722219331));
#225373=CARTESIAN_POINT('Ctrl Pts',(1.44977810268847,-7.7793892637523,94.9249635234814));
#225374=CARTESIAN_POINT('Ctrl Pts',(1.63807784143411,-7.74192879736747,
94.9329529040568));
#225375=CARTESIAN_POINT('Ctrl Pts',(1.84399165277139,-7.69311401633058,
94.9415246932727));
#225376=CARTESIAN_POINT('Ctrl Pts',(1.86312847499661,-7.68850185514843,
94.9423197590846));
#225377=CARTESIAN_POINT('Ctrl Pts',(1.89160629556575,-7.68152585467548,
94.943500604155));
#225378=CARTESIAN_POINT('Ctrl Pts',(1.90096044233482,-7.67921631619811,
94.9438881067535));
#225379=CARTESIAN_POINT('Ctrl Pts',(1.91700688133529,-7.67522333466126,
94.9445522091324));
#225380=CARTESIAN_POINT('Ctrl Pts',(1.92370122323677,-7.67354821605128,
94.9448290736016));
#225381=CARTESIAN_POINT('Ctrl Pts',(1.9374599780665,-7.67008624018572,94.9453977201063));
#225382=CARTESIAN_POINT('Ctrl Pts',(1.94452413267082,-7.66829837684532,
94.9456894697582));
#225383=CARTESIAN_POINT('Ctrl Pts',(1.9608706308643,-7.66413720930678,94.9463640955198));
#225384=CARTESIAN_POINT('Ctrl Pts',(1.97015116195069,-7.66175679553687,
94.9467467441555));
#225385=CARTESIAN_POINT('Ctrl Pts',(1.99934901109399,-7.65421112262899,
94.9479494778538));
#225386=CARTESIAN_POINT('Ctrl Pts',(2.01925058736795,-7.64898499485241,
94.9487676140312));
#225387=CARTESIAN_POINT('Ctrl Pts',(2.30869676470766,-7.57176842344998,
94.9606426991289));
#225388=CARTESIAN_POINT('Ctrl Pts',(2.57428032063671,-7.4856433525196,94.9712280419606));
#225389=CARTESIAN_POINT('Ctrl Pts',(3.21352206506899,-7.2402885659004,94.9962627482606));
#225390=CARTESIAN_POINT('Ctrl Pts',(3.58053712545472,-7.06599450743142,
95.0102271887046));
#225391=CARTESIAN_POINT('Ctrl Pts',(4.41893686528471,-6.58567451776689,
95.0431336541905));
#225392=CARTESIAN_POINT('Ctrl Pts',(4.87426402384145,-6.25616014019791,
95.0618305689935));
#225393=CARTESIAN_POINT('Ctrl Pts',(5.35104459947213,-5.82724526231747,
95.08633975079));
#225394=CARTESIAN_POINT('Ctrl Pts',(5.41035288108064,-5.77222197901689,
95.0894881776148));
#225395=CARTESIAN_POINT('Ctrl Pts',(5.48611496764926,-5.69974012036319,
95.0936558851752));
#225396=CARTESIAN_POINT('Ctrl Pts',(5.50334933894179,-5.68310134596841,
95.0946139666527));
#225397=CARTESIAN_POINT('Ctrl Pts',(5.52575107594743,-5.66127632564756,
95.095872823852));
#225398=CARTESIAN_POINT('Ctrl Pts',(5.53098734425356,-5.6561606753786,95.096168044941));
#225399=CARTESIAN_POINT('Ctrl Pts',(5.53903902473622,-5.64827259393717,
95.0966235092425));
#225400=CARTESIAN_POINT('Ctrl Pts',(5.54185948439862,-5.64550529784895,
95.096783342029));
#225401=CARTESIAN_POINT('Ctrl Pts',(5.5474592636113,-5.64000283017586,95.0971012478024));
#225402=CARTESIAN_POINT('Ctrl Pts',(5.55023863677766,-5.63726771410929,
95.0972593163278));
#225403=CARTESIAN_POINT('Ctrl Pts',(5.55627699482406,-5.63131671278909,
95.0976033426708));
#225404=CARTESIAN_POINT('Ctrl Pts',(5.55953521057789,-5.6281000528706,95.0977893634665));
#225405=CARTESIAN_POINT('Ctrl Pts',(5.56880115835381,-5.61893638677033,
95.0983194964332));
#225406=CARTESIAN_POINT('Ctrl Pts',(5.57480214986017,-5.61298258054092,
95.0986641664747));
#225407=CARTESIAN_POINT('Ctrl Pts',(5.58820827309988,-5.59963916146452,
95.0994371741608));
#225408=CARTESIAN_POINT('Ctrl Pts',(5.59560828128917,-5.5922444870057,95.0998659320829));
#225409=CARTESIAN_POINT('Ctrl Pts',(5.85206507970058,-5.33495385228391,
95.1147962010079));
#225410=CARTESIAN_POINT('Ctrl Pts',(6.08411935213516,-5.06871205931401,
95.1306248953303));
#225411=CARTESIAN_POINT('Ctrl Pts',(6.50607578164984,-4.51370618108745,
95.1626837849411));
#225412=CARTESIAN_POINT('Ctrl Pts',(6.69641278960825,-4.22618337785823,
95.1788572399632));
#225413=CARTESIAN_POINT('Ctrl Pts',(7.04744980020009,-3.61232779564468,
95.2114213267389));
#225414=CARTESIAN_POINT('Ctrl Pts',(7.20564149441936,-3.28545788860019,
95.2277342273834));
#225415=CARTESIAN_POINT('Ctrl Pts',(7.4130606911038,-2.76911087488665,95.2515525030292));
#225416=CARTESIAN_POINT('Ctrl Pts',(7.47864302004084,-2.58676438374428,
95.2596181596478));
#225417=CARTESIAN_POINT('Ctrl Pts',(7.54310995074024,-2.38448284201722,
95.2681944841267));
#225418=CARTESIAN_POINT('Ctrl Pts',(7.54868892372849,-2.36676185794345,
95.2689427651741));
#225419=CARTESIAN_POINT('Ctrl Pts',(7.55686865789422,-2.34045669315049,
95.2700490237938));
#225420=CARTESIAN_POINT('Ctrl Pts',(7.55951730761193,-2.33188754484616,
95.2704086918688));
#225421=CARTESIAN_POINT('Ctrl Pts',(7.56402122153669,-2.31722776122552,
95.2710227962964));
#225422=CARTESIAN_POINT('Ctrl Pts',(7.56588371364676,-2.31113936600717,
95.2712774875131));
#225423=CARTESIAN_POINT('Ctrl Pts',(7.56948837565898,-2.29930484791211,
95.2717718655606));
#225424=CARTESIAN_POINT('Ctrl Pts',(7.57123135756137,-2.29355897752457,
95.2720115809091));
#225425=CARTESIAN_POINT('Ctrl Pts',(7.57537731951149,-2.27983527626451,
95.2725833802332));
#225426=CARTESIAN_POINT('Ctrl Pts',(7.57777424349534,-2.27185561492547,
95.2729152506915));
#225427=CARTESIAN_POINT('Ctrl Pts',(7.58489601311404,-2.24800968237248,
95.2739051981634));
#225428=CARTESIAN_POINT('Ctrl Pts',(7.5895836808108,-2.23213230305818,95.2745619665853));
#225429=CARTESIAN_POINT('Ctrl Pts',(7.62874939616838,-2.09792613284254,
95.280093557864));
#225430=CARTESIAN_POINT('Ctrl Pts',(7.66050858339328,-1.97881819764149,
95.2848722477829));
#225431=CARTESIAN_POINT('Ctrl Pts',(7.73246221433118,-1.6811949463027,95.2965155270619));
#225432=CARTESIAN_POINT('Ctrl Pts',(7.76927205767993,-1.50193374837558,
95.3032649610828));
#225433=CARTESIAN_POINT('Ctrl Pts',(7.90916911912388,-0.676256499060295,
95.3333998599116));
#225434=CARTESIAN_POINT('Ctrl Pts',(7.93799782165575,-0.0199530447597436,
95.35445016023));
#225435=CARTESIAN_POINT('Ctrl Pts',(7.86609003060477,0.876713959469128,
95.3857692659853));
#225436=CARTESIAN_POINT('Ctrl Pts',(7.83515312778967,1.11998208707394,95.3945629168146));
#225437=CARTESIAN_POINT('Ctrl Pts',(7.77770596322982,1.44882231462876,95.4073232137154));
#225438=CARTESIAN_POINT('Ctrl Pts',(7.76096504677763,1.53597413628007,95.4107900543444));
#225439=CARTESIAN_POINT('Ctrl Pts',(7.74076314876747,1.63236082039198,95.4147377530691));
#225440=CARTESIAN_POINT('Ctrl Pts',(7.73874640772947,1.64189524891376,95.4151294915976));
#225441=CARTESIAN_POINT('Ctrl Pts',(7.73570555030763,1.65614126415098,95.4157166988722));
#225442=CARTESIAN_POINT('Ctrl Pts',(7.73469472965689,1.66085570923426,95.4159113329517));
#225443=CARTESIAN_POINT('Ctrl Pts',(7.732940005443,1.66900335900794,95.4162482430516));
#225444=CARTESIAN_POINT('Ctrl Pts',(7.73219812821894,1.67243697819914,95.4163903899198));
#225445=CARTESIAN_POINT('Ctrl Pts',(7.73065352581933,1.6795628421741,95.416685730574));
#225446=CARTESIAN_POINT('Ctrl Pts',(7.729850442098,1.68325500735021,95.416838946791));
#225447=CARTESIAN_POINT('Ctrl Pts',(7.72796030958165,1.69191498439407,95.4171987581437));
#225448=CARTESIAN_POINT('Ctrl Pts',(7.72687111636236,1.69688232113088,95.4174054866333));
#225449=CARTESIAN_POINT('Ctrl Pts',(7.72337576336947,1.71274995962605,95.4180669434725));
#225450=CARTESIAN_POINT('Ctrl Pts',(7.72095133152585,1.72364617600235,95.418522797581));
#225451=CARTESIAN_POINT('Ctrl Pts',(7.69187126317123,1.85304935276744,95.4239556366843));
#225452=CARTESIAN_POINT('Ctrl Pts',(7.66251399609224,1.97092661600016,95.4290951999472));
#225453=CARTESIAN_POINT('Ctrl Pts',(7.56786631338446,2.31679779787797,95.4446424938688));
#225454=CARTESIAN_POINT('Ctrl Pts',(7.49502762631491,2.54257733094657,95.4553958813207));
#225455=CARTESIAN_POINT('Ctrl Pts',(7.32665523349672,2.99397923415774,95.4776744496272));
#225456=CARTESIAN_POINT('Ctrl Pts',(7.23055683625024,3.21913545343965,95.4892004382441));
#225457=CARTESIAN_POINT('Ctrl Pts',(6.81303711039458,4.08394425872501,95.5343272624876));
#225458=CARTESIAN_POINT('Ctrl Pts',(6.41582353996539,4.68333817199578,95.5671125421243));
#225459=CARTESIAN_POINT('Ctrl Pts',(5.91053559431507,5.25851300232902,95.5984569785344));
#225460=CARTESIAN_POINT('Ctrl Pts',(5.87738989983026,5.2955337875968,95.6004760232698));
#225461=CARTESIAN_POINT('Ctrl Pts',(5.83473235205424,5.34228455448099,95.6030282523511));
#225462=CARTESIAN_POINT('Ctrl Pts',(5.82554160637273,5.35230519272411,95.6035754521454));
#225463=CARTESIAN_POINT('Ctrl Pts',(5.81091323789715,5.36817213642894,95.6044421579996));
#225464=CARTESIAN_POINT('Ctrl Pts',(5.80549254166501,5.37403396843314,95.6047624065745));
#225465=CARTESIAN_POINT('Ctrl Pts',(5.79537552501334,5.38494113565621,95.6053584037892));
#225466=CARTESIAN_POINT('Ctrl Pts',(5.7906814694577,5.38998855564706,95.6056342516189));
#225467=CARTESIAN_POINT('Ctrl Pts',(5.78025521409997,5.40117034985979,95.6062454495056));
#225468=CARTESIAN_POINT('Ctrl Pts',(5.77451982980509,5.40730175079031,95.6065806586117));
#225469=CARTESIAN_POINT('Ctrl Pts',(5.75792796806482,5.42498274373831,95.6075474930593));
#225470=CARTESIAN_POINT('Ctrl Pts',(5.7470464959024,5.43650888282897,95.6081780127852));
#225471=CARTESIAN_POINT('Ctrl Pts',(5.6732680102981,5.51418928621705,95.6124291917285));
#225472=CARTESIAN_POINT('Ctrl Pts',(5.60926353845871,5.57928460152488,95.616000333285));
#225473=CARTESIAN_POINT('Ctrl Pts',(5.44522127844096,5.74044575411594,95.6248750262381));
#225474=CARTESIAN_POINT('Ctrl Pts',(5.34375640511205,5.83501687186271,95.6301135421232));
#225475=CARTESIAN_POINT('Ctrl Pts',(4.90281728975392,6.22484406412965,95.6519330883453));
#225476=CARTESIAN_POINT('Ctrl Pts',(4.54096662598676,6.49353117907175,95.6674937695733));
#225477=CARTESIAN_POINT('Ctrl Pts',(3.70167429740342,7.01210047603634,95.7015242947141));
#225478=CARTESIAN_POINT('Ctrl Pts',(3.21760062047393,7.24699701786401,95.719916291599));
#225479=CARTESIAN_POINT('Ctrl Pts',(2.66829779604019,7.447578384699,95.7429223354167));
#225480=CARTESIAN_POINT('Ctrl Pts',(2.62294424126368,7.46367203787041,95.7448352532185));
#225481=CARTESIAN_POINT('Ctrl Pts',(2.56700911476872,7.48294775483598,95.7472088739514));
#225482=CARTESIAN_POINT('Ctrl Pts',(2.55656335280786,7.48652300593243,95.7476527569251));
#225483=CARTESIAN_POINT('Ctrl Pts',(2.53925312566767,7.49240729112723,95.7483893232753));
#225484=CARTESIAN_POINT('Ctrl Pts',(2.53239289249868,7.49472879362012,95.7486814882004));
#225485=CARTESIAN_POINT('Ctrl Pts',(2.51997925428017,7.49891057814395,95.7492106146666));
#225486=CARTESIAN_POINT('Ctrl Pts',(2.51442694755972,7.50077412179241,95.7494474429402));
#225487=CARTESIAN_POINT('Ctrl Pts',(2.50265970287279,7.50470907683185,95.7499497032018));
#225488=CARTESIAN_POINT('Ctrl Pts',(2.49644425315105,7.50677893685754,95.7502151973066));
#225489=CARTESIAN_POINT('Ctrl Pts',(2.47975030991459,7.51231530329536,95.7509288097155));
#225490=CARTESIAN_POINT('Ctrl Pts',(2.46926714210567,7.51576759852443,95.7513774888817));
#225491=CARTESIAN_POINT('Ctrl Pts',(2.44608346967278,7.52334865661364,95.752370937552));
#225492=CARTESIAN_POINT('Ctrl Pts',(2.43337967885803,7.52746721583356,95.7529160972669));
#225493=CARTESIAN_POINT('Ctrl Pts',(2.39519647830983,7.53973941943001,95.7545569176983));
#225494=CARTESIAN_POINT('Ctrl Pts',(2.36968620922721,7.54779596518536,95.755656168534));
#225495=CARTESIAN_POINT('Ctrl Pts',(2.27801783385412,7.57623574767693,95.7596160423244));
#225496=CARTESIAN_POINT('Ctrl Pts',(2.2116345583565,7.59587951614912,95.7625019661246));
#225497=CARTESIAN_POINT('Ctrl Pts',(2.0031047593703,7.65462116887048,95.7716105123528));
#225498=CARTESIAN_POINT('Ctrl Pts',(1.86012000677474,7.69061800946029,95.7779177269329));
#225499=CARTESIAN_POINT('Ctrl Pts',(0.98918698741493,7.88416816158806,95.8164681990765));
#225500=CARTESIAN_POINT('Ctrl Pts',(0.242874917137029,7.94227882690981,
95.849633988647));
#225501=CARTESIAN_POINT('Ctrl Pts',(-0.689331782249625,7.88318051767555,
95.8885771653028));
#225502=CARTESIAN_POINT('Ctrl Pts',(-0.877655499756,7.86444135706684,95.8963434571706));
#225503=CARTESIAN_POINT('Ctrl Pts',(-1.09866423585044,7.83441147262645,
95.9053637810009));
#225504=CARTESIAN_POINT('Ctrl Pts',(-1.13216793682291,7.82963996693112,
95.9067287465753));
#225505=CARTESIAN_POINT('Ctrl Pts',(-1.18187290458387,7.82223540871206,
95.9087500877257));
#225506=CARTESIAN_POINT('Ctrl Pts',(-1.1980981871931,7.81976669013278,95.9094093326295));
#225507=CARTESIAN_POINT('Ctrl Pts',(-1.22695426435346,7.81528424439515,
95.9105807288982));
#225508=CARTESIAN_POINT('Ctrl Pts',(-1.23958806478099,7.81329034519343,
95.9110932334639));
#225509=CARTESIAN_POINT('Ctrl Pts',(-1.26616243628537,7.80903023160124,
95.9121704992509));
#225510=CARTESIAN_POINT('Ctrl Pts',(-1.28010189121267,7.80675730523104,
95.912735136582));
#225511=CARTESIAN_POINT('Ctrl Pts',(-1.316836423216,7.8006664473461,95.914221967605));
#225512=CARTESIAN_POINT('Ctrl Pts',(-1.33962102861553,7.79678592080007,
95.9151430028793));
#225513=CARTESIAN_POINT('Ctrl Pts',(-1.4429283725739,7.77872506674225,95.9193137546079));
#225514=CARTESIAN_POINT('Ctrl Pts',(-1.52324609814851,7.76339665254577,
95.9225416556768));
#225515=CARTESIAN_POINT('Ctrl Pts',(-2.33714390950144,7.5949492440655,95.9551103551461));
#225516=CARTESIAN_POINT('Ctrl Pts',(-3.04562407628151,7.33959384271519,
95.9817422378083));
#225517=CARTESIAN_POINT('Ctrl Pts',(-3.91841477401823,6.87654728846172,
96.0180338644231));
#225518=CARTESIAN_POINT('Ctrl Pts',(-4.12405948538945,6.75522027622282,
96.0269218884242));
#225519=CARTESIAN_POINT('Ctrl Pts',(-4.39741303990627,6.57680672757507,
96.0395758928123));
#225520=CARTESIAN_POINT('Ctrl Pts',(-4.47012455291757,6.52760399294634,
96.0430277776526));
#225521=CARTESIAN_POINT('Ctrl Pts',(-4.55318250199247,6.46936137748287,
96.04708833144));
#225522=CARTESIAN_POINT('Ctrl Pts',(-4.56434437741481,6.46149115374658,
96.0476365060947));
#225523=CARTESIAN_POINT('Ctrl Pts',(-4.58088542161116,6.44976383799779,
96.0484526478827));
#225524=CARTESIAN_POINT('Ctrl Pts',(-4.58628025824946,6.4459288085019,96.0487194318479));
#225525=CARTESIAN_POINT('Ctrl Pts',(-4.59586426734274,6.43909769780573,
96.0491944579694));
#225526=CARTESIAN_POINT('Ctrl Pts',(-4.60005534367424,6.43610428447769,
96.0494025545518));
#225527=CARTESIAN_POINT('Ctrl Pts',(-4.60813230933346,6.43032351357419,
96.049804310977));
#225528=CARTESIAN_POINT('Ctrl Pts',(-4.61201860126713,6.42753672031224,
96.0499979396032));
#225529=CARTESIAN_POINT('Ctrl Pts',(-4.62256652427517,6.41995849393949,
96.0505243517563));
#225530=CARTESIAN_POINT('Ctrl Pts',(-4.62922321833875,6.41516022631306,
96.0508575177392));
#225531=CARTESIAN_POINT('Ctrl Pts',(-4.65427118332568,6.39704590486054,
96.0521148008158));
#225532=CARTESIAN_POINT('Ctrl Pts',(-4.67261242905173,6.3836611460421,96.0530428430758));
#225533=CARTESIAN_POINT('Ctrl Pts',(-4.71759747003296,6.35053499488541,
96.0553379511365));
#225534=CARTESIAN_POINT('Ctrl Pts',(-4.74417440436931,6.33070531036108,
96.0567105544983));
#225535=CARTESIAN_POINT('Ctrl Pts',(-4.85037850963349,6.25041956142837,
96.0622615662839));
#225536=CARTESIAN_POINT('Ctrl Pts',(-4.92897869434102,6.18862537689729,
96.0665190586318));
#225537=CARTESIAN_POINT('Ctrl Pts',(-5.11825236490796,6.03392808609395,
96.0771026902919));
#225538=CARTESIAN_POINT('Ctrl Pts',(-5.22759112484819,5.93945144247613,
96.0835038000803));
#225539=CARTESIAN_POINT('Ctrl Pts',(-6.0600908488128,5.17930836899359,96.1341780073597));
#225540=CARTESIAN_POINT('Ctrl Pts',(-6.65631139006487,4.38683471995058,
96.1809947286347));
#225541=CARTESIAN_POINT('Ctrl Pts',(-7.11576627382732,3.45726284832877,
96.2235291415259));
#225542=CARTESIAN_POINT('Ctrl Pts',(-7.13903588058207,3.40895334438121,
96.2257123214576));
#225543=CARTESIAN_POINT('Ctrl Pts',(-7.16806676225463,3.34708181172404,
96.228474194963));
#225544=CARTESIAN_POINT('Ctrl Pts',(-7.17428349305476,3.3337357613821,96.2290679352078));
#225545=CARTESIAN_POINT('Ctrl Pts',(-7.18409674531395,3.31251413740988,
96.2300088686513));
#225546=CARTESIAN_POINT('Ctrl Pts',(-7.18771764363688,3.30464991073399,
96.2303568654387));
#225547=CARTESIAN_POINT('Ctrl Pts',(-7.19444385795732,3.28997789705409,
96.2310048281613));
#225548=CARTESIAN_POINT('Ctrl Pts',(-7.19755243751562,3.28317162177041,
96.2313049013309));
#225549=CARTESIAN_POINT('Ctrl Pts',(-7.20443032676624,3.26805567954645,
96.2319701927862));
#225550=CARTESIAN_POINT('Ctrl Pts',(-7.20819492832488,3.25974387549168,
96.2323352560016));
#225551=CARTESIAN_POINT('Ctrl Pts',(-7.21903890337987,3.23569099411405,
96.2333894939135));
#225552=CARTESIAN_POINT('Ctrl Pts',(-7.22608117307899,3.21993319536517,
96.2340774503846));
#225553=CARTESIAN_POINT('Ctrl Pts',(-7.2737145924873,3.11240524405664,96.2387536291785));
#225554=CARTESIAN_POINT('Ctrl Pts',(-7.31260884192761,3.01989125318424,
96.2426861106858));
#225555=CARTESIAN_POINT('Ctrl Pts',(-7.40471796364719,2.78857725201936,
96.2523073539752));
#225556=CARTESIAN_POINT('Ctrl Pts',(-7.45580166083015,2.64896873229796,
96.2579285248489));
#225557=CARTESIAN_POINT('Ctrl Pts',(-7.77324781735989,1.69929785443723,
96.2950870966343));
#225558=CARTESIAN_POINT('Ctrl Pts',(-7.91101614490582,0.852346899750275,
96.3224167912368));
#225559=CARTESIAN_POINT('Ctrl Pts',(-7.91099999858106,-0.000149834679674665,
96.3535680629415));
#225560=CARTESIAN_POINT('',(-7.91099998983997,0.000400938813840742,100.360997295013));
#225561=CARTESIAN_POINT('Ctrl Pts',(-7.91099999844005,-0.00015710359732031,
96.3535683285568));
#225562=CARTESIAN_POINT('Ctrl Pts',(-7.91099547183649,-0.228095618794251,
96.3618974865411));
#225563=CARTESIAN_POINT('Ctrl Pts',(-7.90114013362385,-0.455922551071472,
96.3705375672487));
#225564=CARTESIAN_POINT('Ctrl Pts',(-7.88039505359977,-0.695303428629795,
96.3801233621209));
#225565=CARTESIAN_POINT('Ctrl Pts',(-7.87930168561817,-0.707586039626178,
96.3806164462078));
#225566=CARTESIAN_POINT('Ctrl Pts',(-7.87746571638615,-0.727678800481275,
96.3814250427537));
#225567=CARTESIAN_POINT('Ctrl Pts',(-7.87674020433675,-0.735490518183862,
96.3817398997601));
#225568=CARTESIAN_POINT('Ctrl Pts',(-7.87543924029822,-0.749275505734465,
96.3822963623341));
#225569=CARTESIAN_POINT('Ctrl Pts',(-7.87486860897096,-0.755249231924752,
96.3825377868069));
#225570=CARTESIAN_POINT('Ctrl Pts',(-7.87373569209671,-0.766968433314642,
96.3830119562606));
#225571=CARTESIAN_POINT('Ctrl Pts',(-7.87317391339796,-0.772713954763641,
96.383244682401));
#225572=CARTESIAN_POINT('Ctrl Pts',(-7.87204253423117,-0.784155667159567,
96.3837086425232));
#225573=CARTESIAN_POINT('Ctrl Pts',(-7.87147303891542,-0.78985186490412,
96.3839398725461));
#225574=CARTESIAN_POINT('Ctrl Pts',(-7.87011571281016,-0.803280824711324,
96.3844855864139));
#225575=CARTESIAN_POINT('Ctrl Pts',(-7.86932266800957,-0.811013047129047,
96.3848002565994));
#225576=CARTESIAN_POINT('Ctrl Pts',(-7.86653541309912,-0.837799886668064,
96.3858919238506));
#225577=CARTESIAN_POINT('Ctrl Pts',(-7.86448338847706,-0.856848341698109,
96.386670942257));
#225578=CARTESIAN_POINT('Ctrl Pts',(-7.83475236111732,-1.12372701046691,
96.3976219756003));
#225579=CARTESIAN_POINT('Ctrl Pts',(-7.79544028618084,-1.37011243253586,
96.4081684378632));
#225580=CARTESIAN_POINT('Ctrl Pts',(-7.73511039132125,-1.65955815149987,
96.4208333911937));
#225581=CARTESIAN_POINT('Ctrl Pts',(-7.72526211798902,-1.70481412506614,
96.4228218998646));
#225582=CARTESIAN_POINT('Ctrl Pts',(-7.60948566179,-2.21522962116972,96.4453313650302));
#225583=CARTESIAN_POINT('Ctrl Pts',(-7.4620800375311,-2.67000066021761,
96.466063583998));
#225584=CARTESIAN_POINT('Ctrl Pts',(-7.18922794257249,-3.30849225958182,
96.4954635245194));
#225585=CARTESIAN_POINT('Ctrl Pts',(-7.09566192538619,-3.50466901269359,
96.5045560704901));
#225586=CARTESIAN_POINT('Ctrl Pts',(-6.86170768879972,-3.94730332843422,
96.5252939947216));
#225587=CARTESIAN_POINT('Ctrl Pts',(-6.71590782422891,-4.1905634285916,
96.5368689893605));
#225588=CARTESIAN_POINT('Ctrl Pts',(-6.51808292967413,-4.48368684803633,
96.5512449244125));
#225589=CARTESIAN_POINT('Ctrl Pts',(-6.47802388354467,-4.54137198063387,
96.5540939215078));
#225590=CARTESIAN_POINT('Ctrl Pts',(-6.41445166012157,-4.63036312796215,
96.5585199920225));
#225591=CARTESIAN_POINT('Ctrl Pts',(-6.39146529786671,-4.66204077172549,
96.5601017423418));
#225592=CARTESIAN_POINT('Ctrl Pts',(-6.34766617888135,-4.72146779638247,
96.5630809182373));
#225593=CARTESIAN_POINT('Ctrl Pts',(-6.32690415212631,-4.74925340775851,
96.5644788079145));
#225594=CARTESIAN_POINT('Ctrl Pts',(-6.29096333772848,-4.79669866743941,
96.5668743535523));
#225595=CARTESIAN_POINT('Ctrl Pts',(-6.27587348959498,-4.81642499884057,
96.567872927643));
#225596=CARTESIAN_POINT('Ctrl Pts',(-6.24688921792902,-4.85394744862527,
96.5697773344805));
#225597=CARTESIAN_POINT('Ctrl Pts',(-6.23301101594554,-4.87175578341792,
96.5706833338061));
#225598=CARTESIAN_POINT('Ctrl Pts',(-6.20034979039231,-4.91329823738387,
96.5728019138365));
#225599=CARTESIAN_POINT('Ctrl Pts',(-6.18150639828315,-4.9369844792358,
96.5740137976861));
#225600=CARTESIAN_POINT('Ctrl Pts',(-6.11628491889484,-5.01800940274258,
96.5781731102492));
#225601=CARTESIAN_POINT('Ctrl Pts',(-6.06924108375768,-5.07480761734321,
96.5811126083227));
#225602=CARTESIAN_POINT('Ctrl Pts',(-5.65920630471633,-5.55600353761578,
96.6062314527234));
#225603=CARTESIAN_POINT('Ctrl Pts',(-5.2530112736366,-5.94152149207426,
96.6277014713144));
#225604=CARTESIAN_POINT('Ctrl Pts',(-4.56065890113762,-6.47167888016717,
96.6614498985478));
#225605=CARTESIAN_POINT('Ctrl Pts',(-4.30060140213634,-6.64733434620611,
96.6736265400546));
#225606=CARTESIAN_POINT('Ctrl Pts',(-4.00499732372843,-6.82237625595014,
96.687362812733));
#225607=CARTESIAN_POINT('Ctrl Pts',(-3.97909202315596,-6.83751767790462,
96.6885658181687));
#225608=CARTESIAN_POINT('Ctrl Pts',(-3.9412842054516,-6.85932838761716,
96.6903209848783));
#225609=CARTESIAN_POINT('Ctrl Pts',(-3.92944949403805,-6.86611489777649,
96.6908703108593));
#225610=CARTESIAN_POINT('Ctrl Pts',(-3.90915122132476,-6.87768509334585,
96.6918124080321));
#225611=CARTESIAN_POINT('Ctrl Pts',(-3.90069627544968,-6.88248385980615,
96.692204801681));
#225612=CARTESIAN_POINT('Ctrl Pts',(-3.8830351214881,-6.89246478802746,
96.6930244342126));
#225613=CARTESIAN_POINT('Ctrl Pts',(-3.87382733794453,-6.89764411693488,
96.6934517444074));
#225614=CARTESIAN_POINT('Ctrl Pts',(-3.85081599766598,-6.91052726200476,
96.6945196557035));
#225615=CARTESIAN_POINT('Ctrl Pts',(-3.83699974948331,-6.91820813563104,
96.6951608588306));
#225616=CARTESIAN_POINT('Ctrl Pts',(-3.78089754683806,-6.94917730202297,
96.697764732388));
#225617=CARTESIAN_POINT('Ctrl Pts',(-3.73842224834018,-6.97211950939762,
96.6997364715091));
#225618=CARTESIAN_POINT('Ctrl Pts',(-3.51234379191757,-7.09157146814619,
96.7102265755632));
#225619=CARTESIAN_POINT('Ctrl Pts',(-3.32521091544579,-7.18121951894139,
96.7188915217075));
#225620=CARTESIAN_POINT('Ctrl Pts',(-2.64361144581839,-7.47538744184029,
96.7500979745021));
#225621=CARTESIAN_POINT('Ctrl Pts',(-2.13218791315477,-7.63700932828069,
96.7727691426322));
#225622=CARTESIAN_POINT('Ctrl Pts',(-1.47092733809158,-7.7743166077336,
96.8005288181542));
#225623=CARTESIAN_POINT('Ctrl Pts',(-1.33274788861426,-7.79919290916647,
96.8062541329836));
#225624=CARTESIAN_POINT('Ctrl Pts',(-1.15717629169226,-7.82599833650151,
96.8134417973244));
#225625=CARTESIAN_POINT('Ctrl Pts',(-1.12033529402086,-7.83135721192357,
96.8149452405692));
#225626=CARTESIAN_POINT('Ctrl Pts',(-1.06130560157301,-7.83951857683851,
96.8173468536801));
#225627=CARTESIAN_POINT('Ctrl Pts',(-1.03914055450353,-7.84248736106824,
96.8182469852547));
#225628=CARTESIAN_POINT('Ctrl Pts',(-0.997068678588804,-7.84794097146024,
96.819952503946));
#225629=CARTESIAN_POINT('Ctrl Pts',(-0.97716441225162,-7.85044413747507,
96.8207580997162));
#225630=CARTESIAN_POINT('Ctrl Pts',(-0.931889584993449,-7.85596305682155,
96.8225876899034));
#225631=CARTESIAN_POINT('Ctrl Pts',(-0.906513483038265,-7.85893167418894,
96.8236111310436));
#225632=CARTESIAN_POINT('Ctrl Pts',(-0.840598223579007,-7.86631925011927,
96.8262645106965));
#225633=CARTESIAN_POINT('Ctrl Pts',(-0.800038411933684,-7.87054778780272,
96.8278922743001));
#225634=CARTESIAN_POINT('Ctrl Pts',(-0.482186699644027,-7.90120279613035,
96.8406126490297));
#225635=CARTESIAN_POINT('Ctrl Pts',(-0.203703911787188,-7.91328111759463,
96.8515425985047));
#225636=CARTESIAN_POINT('Ctrl Pts',(0.0802563238618417,-7.91059474928651,
96.8626264199348));
#225637=CARTESIAN_POINT('Ctrl Pts',(0.0856749730396105,-7.91053791875003,
96.8628378950546));
#225638=CARTESIAN_POINT('Ctrl Pts',(0.565725856991825,-7.9050098636676,
96.8815701937917));
#225639=CARTESIAN_POINT('Ctrl Pts',(1.03891298264263,-7.85683847286887,
96.8997059611012));
#225640=CARTESIAN_POINT('Ctrl Pts',(1.75788659866591,-7.71752182985089,
96.9272290993342));
#225641=CARTESIAN_POINT('Ctrl Pts',(2.00829301566487,-7.65617839568246,
96.9368273188885));
#225642=CARTESIAN_POINT('Ctrl Pts',(2.52484080425947,-7.50254643520879,
96.9570210189468));
#225643=CARTESIAN_POINT('Ctrl Pts',(2.78994749304644,-7.40805017928735,
96.9676124107701));
#225644=CARTESIAN_POINT('Ctrl Pts',(3.11674604150809,-7.27152902189387,
96.9813816425818));
#225645=CARTESIAN_POINT('Ctrl Pts',(3.18364980349044,-7.24248671621858,
96.9842399746396));
#225646=CARTESIAN_POINT('Ctrl Pts',(3.27627426072687,-7.20074784790378,
96.9882619893091));
#225647=CARTESIAN_POINT('Ctrl Pts',(3.30234271919194,-7.18882988701723,
96.9894011909934));
#225648=CARTESIAN_POINT('Ctrl Pts',(3.34155051976329,-7.17064662322809,
96.9911261755855));
#225649=CARTESIAN_POINT('Ctrl Pts',(3.35473840699098,-7.16448624041209,
96.9917083763873));
#225650=CARTESIAN_POINT('Ctrl Pts',(3.37889544993873,-7.15312057459422,
96.9927785829963));
#225651=CARTESIAN_POINT('Ctrl Pts',(3.38986978188682,-7.14792636198583,
96.9932661946));
#225652=CARTESIAN_POINT('Ctrl Pts',(3.40751194197308,-7.13952646197214,
96.9940524228808));
#225653=CARTESIAN_POINT('Ctrl Pts',(3.41418732725791,-7.13633663933164,
96.9943504566522));
#225654=CARTESIAN_POINT('Ctrl Pts',(3.42694654637268,-7.13021766577263,
96.994921167605));
#225655=CARTESIAN_POINT('Ctrl Pts',(3.43303112599411,-7.12729007973062,
96.9951937860206));
#225656=CARTESIAN_POINT('Ctrl Pts',(3.44679812100053,-7.1206443919729,96.995811667542));
#225657=CARTESIAN_POINT('Ctrl Pts',(3.45447827593597,-7.11692164382133,
96.9961571076197));
#225658=CARTESIAN_POINT('Ctrl Pts',(3.47705071774455,-7.10593511434129,
96.9971746025724));
#225659=CARTESIAN_POINT('Ctrl Pts',(3.49192617570184,-7.09863699039693,
96.9978479955809));
#225660=CARTESIAN_POINT('Ctrl Pts',(3.5889593463041,-7.05065224678577,97.0022598064176));
#225661=CARTESIAN_POINT('Ctrl Pts',(3.67042600644359,-7.00858749078639,
97.006054171164));
#225662=CARTESIAN_POINT('Ctrl Pts',(4.27538044189192,-6.68278252195722,
97.035025511134));
#225663=CARTESIAN_POINT('Ctrl Pts',(4.7660444399419,-6.34217841030185,97.0628742895321));
#225664=CARTESIAN_POINT('Ctrl Pts',(5.36669744536995,-5.81582268587094,
97.0993099841394));
#225665=CARTESIAN_POINT('Ctrl Pts',(5.51435047035643,-5.67601784211672,
97.1085039253896));
#225666=CARTESIAN_POINT('Ctrl Pts',(5.741198866624,-5.44401034281534,97.122919997594));
#225667=CARTESIAN_POINT('Ctrl Pts',(5.82393759965858,-5.35540523930648,
97.1282458997021));
#225668=CARTESIAN_POINT('Ctrl Pts',(6.02259908069153,-5.13260681267485,
97.1411854386722));
#225669=CARTESIAN_POINT('Ctrl Pts',(6.13611117103182,-4.99634838432643,
97.1487131239244));
#225670=CARTESIAN_POINT('Ctrl Pts',(6.30040453350522,-4.78507920594545,
97.1598064022359));
#225671=CARTESIAN_POINT('Ctrl Pts',(6.35463112082665,-4.71282763422311,
97.1635036637587));
#225672=CARTESIAN_POINT('Ctrl Pts',(6.41717453817223,-4.62645198051672,
97.1678122652857));
#225673=CARTESIAN_POINT('Ctrl Pts',(6.42669860568185,-4.61321276522296,
97.1684696311704));
#225674=CARTESIAN_POINT('Ctrl Pts',(6.44125004171768,-4.59285258617101,
97.1694759431189));
#225675=CARTESIAN_POINT('Ctrl Pts',(6.44630666805044,-4.58575264490919,
97.1698260011463));
#225676=CARTESIAN_POINT('Ctrl Pts',(6.45511288616091,-4.57334460343449,
97.1704362749591));
#225677=CARTESIAN_POINT('Ctrl Pts',(6.45886768614249,-4.56804021961416,
97.1706966883102));
#225678=CARTESIAN_POINT('Ctrl Pts',(6.46730760163202,-4.55608599088633,
97.1712824997253));
#225679=CARTESIAN_POINT('Ctrl Pts',(6.47198900859316,-4.54943352997186,
97.1716077570809));
#225680=CARTESIAN_POINT('Ctrl Pts',(6.48450365325546,-4.53159132537088,
97.1724781267602));
#225681=CARTESIAN_POINT('Ctrl Pts',(6.4923182012014,-4.52038847290719,97.1730225315924));
#225682=CARTESIAN_POINT('Ctrl Pts',(6.52602968935439,-4.47179230265024,
97.1753750842385));
#225683=CARTESIAN_POINT('Ctrl Pts',(6.55163311604825,-4.43419592531209,
97.1771721514604));
#225684=CARTESIAN_POINT('Ctrl Pts',(6.95452331100971,-3.83147897144885,
97.205622702174));
#225685=CARTESIAN_POINT('Ctrl Pts',(7.2577820270356,-3.22029861498986,97.2291479340883));
#225686=CARTESIAN_POINT('Ctrl Pts',(7.56509326849239,-2.32867683549825,
97.2612349974756));
#225687=CARTESIAN_POINT('Ctrl Pts',(7.63846228352745,-2.07539416867657,
97.2701629216353));
#225688=CARTESIAN_POINT('Ctrl Pts',(7.75084400605901,-1.59971138835418,
97.2872114056735));
#225689=CARTESIAN_POINT('Ctrl Pts',(7.79324602661001,-1.37839251122473,
97.2952548950128));
#225690=CARTESIAN_POINT('Ctrl Pts',(7.84038694720149,-1.05913097588485,
97.3073568110061));
#225691=CARTESIAN_POINT('Ctrl Pts',(7.85284342424922,-0.962431717163583,
97.3110873262495));
#225692=CARTESIAN_POINT('Ctrl Pts',(7.86874486523778,-0.817964057433518,
97.3167872120169));
#225693=CARTESIAN_POINT('Ctrl Pts',(7.8735486387958,-0.770352263021179,
97.3186861183502));
#225694=CARTESIAN_POINT('Ctrl Pts',(7.878721260414,-0.713967237865432,97.3209618640779));
#225695=CARTESIAN_POINT('Ctrl Pts',(7.87950792393595,-0.705232437932734,
97.3213151717509));
#225696=CARTESIAN_POINT('Ctrl Pts',(7.88069803326697,-0.691767335910473,
97.3218610119056));
#225697=CARTESIAN_POINT('Ctrl Pts',(7.88111175073392,-0.68703792532019,
97.3220529579735));
#225698=CARTESIAN_POINT('Ctrl Pts',(7.88182509144429,-0.678797938889844,
97.3223877842976));
#225699=CARTESIAN_POINT('Ctrl Pts',(7.88212662747459,-0.675287525680402,
97.3225305544656));
#225700=CARTESIAN_POINT('Ctrl Pts',(7.88275144822702,-0.667956069208977,
97.3228289952043));
#225701=CARTESIAN_POINT('Ctrl Pts',(7.88307429995726,-0.664134990926276,
97.3229846907889));
#225702=CARTESIAN_POINT('Ctrl Pts',(7.88385920386712,-0.654764130988174,
97.323366894811));
#225703=CARTESIAN_POINT('Ctrl Pts',(7.88431817373639,-0.649214100745314,
97.3235935826308));
#225704=CARTESIAN_POINT('Ctrl Pts',(7.88608837269084,-0.627529460222969,
97.3244805512199));
#225705=CARTESIAN_POINT('Ctrl Pts',(7.88735591136494,-0.611391656063683,
97.3251434120767));
#225706=CARTESIAN_POINT('Ctrl Pts',(7.90875491336743,-0.327800647260582,
97.3368395425324));
#225707=CARTESIAN_POINT('Ctrl Pts',(7.91531996182526,-0.059519098985165,
97.3486416614873));
#225708=CARTESIAN_POINT('Ctrl Pts',(7.89123618552217,0.853736761718965,
97.3900427745075));
#225709=CARTESIAN_POINT('Ctrl Pts',(7.79533734154688,1.49443656619456,97.420925222916));
#225710=CARTESIAN_POINT('Ctrl Pts',(7.53143407129858,2.44492242450904,97.4647105745562));
#225711=CARTESIAN_POINT('Ctrl Pts',(7.41908471514528,2.76719491001734,97.4792315600571));
#225712=CARTESIAN_POINT('Ctrl Pts',(7.27865842188863,3.09926367564651,97.4937885888836));
#225713=CARTESIAN_POINT('Ctrl Pts',(7.27097157630804,3.11725457701841,97.4945760512397));
#225714=CARTESIAN_POINT('Ctrl Pts',(7.25968243504384,3.14340763047326,97.4957190339759));
#225715=CARTESIAN_POINT('Ctrl Pts',(7.25613297764106,3.15159242296956,97.4960764904644));
#225716=CARTESIAN_POINT('Ctrl Pts',(7.24989087415495,3.16591981802518,97.4967017826272));
#225717=CARTESIAN_POINT('Ctrl Pts',(7.24720425137891,3.17206502461992,97.4969698392007));
#225718=CARTESIAN_POINT('Ctrl Pts',(7.24198137326416,3.18397022586088,97.4974888807895));
#225719=CARTESIAN_POINT('Ctrl Pts',(7.23944605351197,3.18973062317209,97.4977398999078));
#225720=CARTESIAN_POINT('Ctrl Pts',(7.23339156716608,3.20344237412281,97.4983371240578));
#225721=CARTESIAN_POINT('Ctrl Pts',(7.22986615602592,3.21139097198033,97.4986830988146));
#225722=CARTESIAN_POINT('Ctrl Pts',(7.21729004904704,3.23962012629002,97.4999110002761));
#225723=CARTESIAN_POINT('Ctrl Pts',(7.20816702504041,3.25986845822123,97.5007902570765));
#225724=CARTESIAN_POINT('Ctrl Pts',(7.08379332390719,3.53283790920206,97.5126239006332));
#225725=CARTESIAN_POINT('Ctrl Pts',(6.95539151596179,3.77936751685317,97.5230720243156));
#225726=CARTESIAN_POINT('Ctrl Pts',(6.64366230950462,4.30795538938865,97.5452735363578));
#225727=CARTESIAN_POINT('Ctrl Pts',(6.45479141596844,4.58611066683757,97.5568142626404));
#225728=CARTESIAN_POINT('Ctrl Pts',(6.02319011598133,5.14202819215417,97.5806538326943));
#225729=CARTESIAN_POINT('Ctrl Pts',(5.7775851715395,5.41652704018834,97.5928913284044));
#225730=CARTESIAN_POINT('Ctrl Pts',(5.37064471927252,5.81205121208812,97.6128144815226));
#225731=CARTESIAN_POINT('Ctrl Pts',(5.22230064376214,5.94569857918039,97.6200198514225));
#225732=CARTESIAN_POINT('Ctrl Pts',(4.99686823289023,6.13384654129154,97.6311621041247));
#225733=CARTESIAN_POINT('Ctrl Pts',(4.92359975116294,6.19281274532406,97.6348118178087));
#225734=CARTESIAN_POINT('Ctrl Pts',(4.83989476177235,6.25775370309663,97.6390356430057));
#225735=CARTESIAN_POINT('Ctrl Pts',(4.83047276018806,6.26502957883436,97.6395118463631));
#225736=CARTESIAN_POINT('Ctrl Pts',(4.81371671477996,6.27790869434471,97.6403601463575));
#225737=CARTESIAN_POINT('Ctrl Pts',(4.80638920055243,6.2835204333263,97.6407315934619));
#225738=CARTESIAN_POINT('Ctrl Pts',(4.79533995735754,6.29195180329596,97.6412924546718));
#225739=CARTESIAN_POINT('Ctrl Pts',(4.79162552229719,6.29478098549499,97.6414811282059));
#225740=CARTESIAN_POINT('Ctrl Pts',(4.78522589452983,6.29964645794024,97.6418064146796));
#225741=CARTESIAN_POINT('Ctrl Pts',(4.7825419048714,6.30168432125908,97.6419429052726));
#225742=CARTESIAN_POINT('Ctrl Pts',(4.77700322941131,6.30588407514947,97.6422247018895));
#225743=CARTESIAN_POINT('Ctrl Pts',(4.77414837718096,6.30804574298635,97.6423700248229));
#225744=CARTESIAN_POINT('Ctrl Pts',(4.76725831530157,6.31325547787101,97.642720931286));
#225745=CARTESIAN_POINT('Ctrl Pts',(4.76322165367694,6.31630161181189,97.642926661226));
#225746=CARTESIAN_POINT('Ctrl Pts',(4.74837343154869,6.3274840057802,97.6436839311086));
#225747=CARTESIAN_POINT('Ctrl Pts',(4.73754397975144,6.33559635111259,97.6442372622774));
#225748=CARTESIAN_POINT('Ctrl Pts',(4.55811567422073,6.46928886961355,97.6534212393237));
#225749=CARTESIAN_POINT('Ctrl Pts',(4.38461020285829,6.58811782416493,97.6625353368626));
#225750=CARTESIAN_POINT('Ctrl Pts',(3.76137989566182,6.97941948458593,97.695470354475));
#225751=CARTESIAN_POINT('Ctrl Pts',(3.28942223245733,7.21387325520067,97.7206667935144));
#225752=CARTESIAN_POINT('Ctrl Pts',(2.47187406201008,7.52297169109212,97.7613890603567));
#225753=CARTESIAN_POINT('Ctrl Pts',(2.13823938070407,7.62451518065699,97.7772875098587));
#225754=CARTESIAN_POINT('Ctrl Pts',(1.56321109901522,7.75879544377492,97.8030833485542));
#225755=CARTESIAN_POINT('Ctrl Pts',(1.32503454735889,7.80300157161696,97.8133242429023));
#225756=CARTESIAN_POINT('Ctrl Pts',(1.0445859698114,7.84183915792317,97.8248751974729));
#225757=CARTESIAN_POINT('Ctrl Pts',(1.00393939693293,7.8471464229465,97.826537140895));
#225758=CARTESIAN_POINT('Ctrl Pts',(0.951092865194161,7.85362931742629,
97.8286824030371));
#225759=CARTESIAN_POINT('Ctrl Pts',(0.938929260661309,7.85509280270145,
97.8291751095672));
#225760=CARTESIAN_POINT('Ctrl Pts',(0.919211683745207,7.85741870368982,
97.8299720879975));
#225761=CARTESIAN_POINT('Ctrl Pts',(0.911659804927863,7.85829849300339,
97.8302769254328));
#225762=CARTESIAN_POINT('Ctrl Pts',(0.897200543415067,7.85996186444046,
97.830859808803));
#225763=CARTESIAN_POINT('Ctrl Pts',(0.890293375590038,7.86074723110165,
97.831137912534));
#225764=CARTESIAN_POINT('Ctrl Pts',(0.874589487059018,7.86251184864004,
97.8317694324102));
#225765=CARTESIAN_POINT('Ctrl Pts',(0.865792133049322,7.86348544373966,
97.8321226645511));
#225766=CARTESIAN_POINT('Ctrl Pts',(0.842720663683838,7.86599955540351,
97.833047607024));
#225767=CARTESIAN_POINT('Ctrl Pts',(0.828443926474746,7.86751598575828,
97.833618536016));
#225768=CARTESIAN_POINT('Ctrl Pts',(0.77586990251867,7.87295554159818,97.8357157680262));
#225769=CARTESIAN_POINT('Ctrl Pts',(0.737547965979794,7.87663799585846,
97.8372342906579));
#225770=CARTESIAN_POINT('Ctrl Pts',(0.0385986760178754,7.93865614902397,
97.8647504927799));
#225771=CARTESIAN_POINT('Ctrl Pts',(-0.62672874199101,7.91397707627933,
97.8877110379457));
#225772=CARTESIAN_POINT('Ctrl Pts',(-1.79444034881421,7.72233070518094,
97.9285340081368));
#225773=CARTESIAN_POINT('Ctrl Pts',(-2.29809799756727,7.58769673231528,
97.9464646536779));
#225774=CARTESIAN_POINT('Ctrl Pts',(-2.82687578773917,7.38882313738592,
97.9687370056147));
#225775=CARTESIAN_POINT('Ctrl Pts',(-2.86873541897305,7.37267190750078,
97.9705227743298));
#225776=CARTESIAN_POINT('Ctrl Pts',(-2.92103077785455,7.35198133536311,
97.9727805090986));
#225777=CARTESIAN_POINT('Ctrl Pts',(-2.93159770198906,7.34777417131288,
97.9732380894682));
#225778=CARTESIAN_POINT('Ctrl Pts',(-2.9483473620747,7.34106350102359,97.9739655538734));
#225779=CARTESIAN_POINT('Ctrl Pts',(-2.95453609196583,7.33857492803828,
97.9742348073474));
#225780=CARTESIAN_POINT('Ctrl Pts',(-2.96615434398524,7.33388599100251,
97.9747411530418));
#225781=CARTESIAN_POINT('Ctrl Pts',(-2.97158458674744,7.33168741593191,
97.9749781707658));
#225782=CARTESIAN_POINT('Ctrl Pts',(-2.98374313835775,7.32674898309896,
97.9755096581231));
#225783=CARTESIAN_POINT('Ctrl Pts',(-2.99047012069428,7.32400588706953,
97.975804260529));
#225784=CARTESIAN_POINT('Ctrl Pts',(-3.00749696443932,7.31703539468532,
97.9765513047736));
#225785=CARTESIAN_POINT('Ctrl Pts',(-3.01779167950126,7.31279552125958,
97.9770042499056));
#225786=CARTESIAN_POINT('Ctrl Pts',(-3.06455451726518,7.29342070652667,
97.9790674006498));
#225787=CARTESIAN_POINT('Ctrl Pts',(-3.10091761961902,7.27803475135415,
97.9806874658829));
#225788=CARTESIAN_POINT('Ctrl Pts',(-3.64818762825039,7.04162792893815,
98.0052950396016));
#225789=CARTESIAN_POINT('Ctrl Pts',(-4.13447150310487,6.76756346515747,
98.0300237236067));
#225790=CARTESIAN_POINT('Ctrl Pts',(-4.86211254384341,6.24956373282065,
98.0690354277152));
#225791=CARTESIAN_POINT('Ctrl Pts',(-5.12355794879224,6.0370817331948,98.083569190072));
#225792=CARTESIAN_POINT('Ctrl Pts',(-5.5392910443434,5.6526903314339,98.107415175593));
#225793=CARTESIAN_POINT('Ctrl Pts',(-5.70103531946369,5.489522393476,98.1169127748497));
#225794=CARTESIAN_POINT('Ctrl Pts',(-5.89006814094829,5.28144560593661,
98.1283289027479));
#225795=CARTESIAN_POINT('Ctrl Pts',(-5.92430691229725,5.24301040100238,
98.1304105134284));
#225796=CARTESIAN_POINT('Ctrl Pts',(-5.97106499191914,5.18947860511051,
98.1332731969114));
#225797=CARTESIAN_POINT('Ctrl Pts',(-5.98390680020672,5.17466566466596,
98.1340615149998));
#225798=CARTESIAN_POINT('Ctrl Pts',(-6.0054051119838,5.14968046022803,98.1353847646924));
#225799=CARTESIAN_POINT('Ctrl Pts',(-6.01409113713178,5.1395337528861,98.1359203816579));
#225800=CARTESIAN_POINT('Ctrl Pts',(-6.03117305403424,5.11947666237961,
98.1369756625038));
#225801=CARTESIAN_POINT('Ctrl Pts',(-6.03957031802873,5.10956750411814,
98.1374953575957));
#225802=CARTESIAN_POINT('Ctrl Pts',(-6.05796716193314,5.08774966668146,
98.1386359654884));
#225803=CARTESIAN_POINT('Ctrl Pts',(-6.0679561171447,5.07583208630414,98.1392566254849));
#225804=CARTESIAN_POINT('Ctrl Pts',(-6.10254338786483,5.03431883898408,
98.1414103775079));
#225805=CARTESIAN_POINT('Ctrl Pts',(-6.12696094512677,5.0045730669092,98.1429391438879));
#225806=CARTESIAN_POINT('Ctrl Pts',(-6.45537265462178,4.5984916112999,98.1636147973657));
#225807=CARTESIAN_POINT('Ctrl Pts',(-6.72444605504976,4.19521519982848,
98.1817939801042));
#225808=CARTESIAN_POINT('Ctrl Pts',(-7.15527352312746,3.40038275201998,
98.2149174703692));
#225809=CARTESIAN_POINT('Ctrl Pts',(-7.32577578648008,3.01554823521631,
98.2299455050489));
#225810=CARTESIAN_POINT('Ctrl Pts',(-7.51690779666314,2.47076858777956,
98.2515044409374));
#225811=CARTESIAN_POINT('Ctrl Pts',(-7.56448724807535,2.32101911524334,
98.2574645104757));
#225812=CARTESIAN_POINT('Ctrl Pts',(-7.62755998726831,2.09989473099575,
98.2664312742758));
#225813=CARTESIAN_POINT('Ctrl Pts',(-7.64657532172659,2.02956020802687,
98.2693076857157));
#225814=CARTESIAN_POINT('Ctrl Pts',(-7.66758403521467,1.94736224667472,
98.2727073325733));
#225815=CARTESIAN_POINT('Ctrl Pts',(-7.67052560689406,1.93574315666371,
98.2731887717426));
#225816=CARTESIAN_POINT('Ctrl Pts',(-7.67496740081584,1.91802914337357,
98.2739241573202));
#225817=CARTESIAN_POINT('Ctrl Pts',(-7.67648680141312,1.91193901205368,
98.2741772373399));
#225818=CARTESIAN_POINT('Ctrl Pts',(-7.67923167384485,1.90088087011957,
98.2746372346061));
#225819=CARTESIAN_POINT('Ctrl Pts',(-7.68045957781583,1.89591346224504,
98.2748440403623));
#225820=CARTESIAN_POINT('Ctrl Pts',(-7.68308976052964,1.88522873567911,
98.2752892471517));
#225821=CARTESIAN_POINT('Ctrl Pts',(-7.68449047812275,1.87951103895206,
98.2755277202829));
#225822=CARTESIAN_POINT('Ctrl Pts',(-7.6882364845701,1.86414573843466,98.2761692061615));
#225823=CARTESIAN_POINT('Ctrl Pts',(-7.69056999001595,1.85449529632038,
98.2765727708293));
#225824=CARTESIAN_POINT('Ctrl Pts',(-7.70116444731239,1.81031698171258,
98.278423389243));
#225825=CARTESIAN_POINT('Ctrl Pts',(-7.70921102447997,1.77573838083047,
98.2798807524509));
#225826=CARTESIAN_POINT('Ctrl Pts',(-7.84593585391419,1.16973934828971,
98.3055912540705));
#225827=CARTESIAN_POINT('Ctrl Pts',(-7.91098363973838,0.585864373381105,
98.3328497194227));
#225828=CARTESIAN_POINT('Ctrl Pts',(-7.91101873720173,-0.670743544786332,
98.3907569465403));
#225829=CARTESIAN_POINT('Ctrl Pts',(-7.82567762832376,-1.33908526720668,
98.4209363875106));
#225830=CARTESIAN_POINT('Ctrl Pts',(-7.64628732108988,-2.02978156441373,
98.4500986923818));
#225831=CARTESIAN_POINT('Ctrl Pts',(-7.63528548029237,-2.07078214711567,
98.451823212657));
#225832=CARTESIAN_POINT('Ctrl Pts',(-7.62032294958488,-2.12480215298481,
98.4540868686438));
#225833=CARTESIAN_POINT('Ctrl Pts',(-7.61665803010437,-2.13790235980257,
98.4546351602644));
#225834=CARTESIAN_POINT('Ctrl Pts',(-7.61092312184153,-2.15819978593878,
98.4554836696857));
#225835=CARTESIAN_POINT('Ctrl Pts',(-7.6088766801701,-2.16540359955203,
98.4557846184494));
#225836=CARTESIAN_POINT('Ctrl Pts',(-7.60476382065264,-2.17980372711546,
98.456385809281));
#225837=CARTESIAN_POINT('Ctrl Pts',(-7.60269740971548,-2.18700003505791,
98.4566860511905));
#225838=CARTESIAN_POINT('Ctrl Pts',(-7.59806864169619,-2.20303394994832,
98.4573545772178));
#225839=CARTESIAN_POINT('Ctrl Pts',(-7.59550107370888,-2.21187004784318,
98.4577226986473));
#225840=CARTESIAN_POINT('Ctrl Pts',(-7.58797095520063,-2.23761667286436,
98.4587944777998));
#225841=CARTESIAN_POINT('Ctrl Pts',(-7.58296729188018,-2.25451516891353,
98.4594968532769));
#225842=CARTESIAN_POINT('Ctrl Pts',(-7.54673402656659,-2.37539775219195,
98.4645137099034));
#225843=CARTESIAN_POINT('Ctrl Pts',(-7.51342251781657,-2.47874809691327,
98.4687626613628));
#225844=CARTESIAN_POINT('Ctrl Pts',(-7.40074878849384,-2.80515202141151,
98.4820730093524));
#225845=CARTESIAN_POINT('Ctrl Pts',(-7.31349672209356,-3.02534883182184,
98.4908848770619));
#225846=CARTESIAN_POINT('Ctrl Pts',(-6.94099281301107,-3.85469623306248,
98.5238340332307));
#225847=CARTESIAN_POINT('Ctrl Pts',(-6.58843178329839,-4.43041419571599,
98.545995230871));
#225848=CARTESIAN_POINT('Ctrl Pts',(-5.9747327248717,-5.19432968054969,
98.5809925291853));
#225849=CARTESIAN_POINT('Ctrl Pts',(-5.76831998543478,-5.42263603990238,
98.5924005709364));
#225850=CARTESIAN_POINT('Ctrl Pts',(-5.5352728381868,-5.65199556551644,
98.6054315508172));
#225851=CARTESIAN_POINT('Ctrl Pts',(-5.52136086053785,-5.66558677498388,
98.6062094868047));
#225852=CARTESIAN_POINT('Ctrl Pts',(-5.50178434511155,-5.68457132865936,
98.6073040581866));
#225853=CARTESIAN_POINT('Ctrl Pts',(-5.49616164511361,-5.69000785069846,
98.607618423863));
#225854=CARTESIAN_POINT('Ctrl Pts',(-5.48640119716941,-5.69941714630616,
98.6081640946727));
#225855=CARTESIAN_POINT('Ctrl Pts',(-5.48226716823733,-5.7033937791229,
98.60839520167));
#225856=CARTESIAN_POINT('Ctrl Pts',(-5.47366677684582,-5.71164873469736,
98.6088759642936));
#225857=CARTESIAN_POINT('Ctrl Pts',(-5.46919971486687,-5.71592632310298,
98.6091256566775));
#225858=CARTESIAN_POINT('Ctrl Pts',(-5.45868946179345,-5.72596717552358,
98.6097130929393));
#225859=CARTESIAN_POINT('Ctrl Pts',(-5.45264215796011,-5.73172611279303,
98.6100510497705));
#225860=CARTESIAN_POINT('Ctrl Pts',(-5.43292311905883,-5.75044539750492,
98.6111529066858));
#225861=CARTESIAN_POINT('Ctrl Pts',(-5.4192142594299,-5.7633664373078,98.6119186902154));
#225862=CARTESIAN_POINT('Ctrl Pts',(-5.13288345468371,-6.03131756173488,
98.6279061365615));
#225863=CARTESIAN_POINT('Ctrl Pts',(-4.84260276689632,-6.26677445135892,
98.6439484209776));
#225864=CARTESIAN_POINT('Ctrl Pts',(-4.27390255252831,-6.66488274681919,
98.673918804139));
#225865=CARTESIAN_POINT('Ctrl Pts',(-4.00004598469345,-6.83275521322612,
98.6878049456468));
#225866=CARTESIAN_POINT('Ctrl Pts',(-3.44212601675245,-7.12968928874179,
98.7147638393729));
#225867=CARTESIAN_POINT('Ctrl Pts',(-3.15911564739508,-7.25952475633295,
98.7278259953252));
#225868=CARTESIAN_POINT('Ctrl Pts',(-2.64198312911293,-7.4607832332036,
98.7507802882766));
#225869=CARTESIAN_POINT('Ctrl Pts',(-2.41081092964281,-7.53865732956205,
98.7607449958936));
#225870=CARTESIAN_POINT('Ctrl Pts',(-2.05940076095497,-7.63921473906827,
98.775624463039));
#225871=CARTESIAN_POINT('Ctrl Pts',(-1.94163343364575,-7.66999304525702,
98.7805623636893));
#225872=CARTESIAN_POINT('Ctrl Pts',(-1.78380533569913,-7.70737300924631,
98.7871140685367));
#225873=CARTESIAN_POINT('Ctrl Pts',(-1.74433728215809,-7.71640121053048,
98.7887470345179));
#225874=CARTESIAN_POINT('Ctrl Pts',(-1.68192841604885,-7.73017376671745,
98.7913206761723));
#225875=CARTESIAN_POINT('Ctrl Pts',(-1.65903292598478,-7.73511987070554,
98.7922630539052));
#225876=CARTESIAN_POINT('Ctrl Pts',(-1.6123019019529,-7.74499812895948,
98.7941828683496));
#225877=CARTESIAN_POINT('Ctrl Pts',(-1.58846488851236,-7.74992211202235,
98.7951602237806));
#225878=CARTESIAN_POINT('Ctrl Pts',(-1.53364193106535,-7.76098326228714,
98.7974036824061));
#225879=CARTESIAN_POINT('Ctrl Pts',(-1.50264116615804,-7.76704501754189,
98.7986690917331));
#225880=CARTESIAN_POINT('Ctrl Pts',(-1.40539072386973,-7.78545691502914,
98.802628873742));
#225881=CARTESIAN_POINT('Ctrl Pts',(-1.33901881075219,-7.79714634795118,
98.8053170528809));
#225882=CARTESIAN_POINT('Ctrl Pts',(-0.937927380250833,-7.86251416057637,
98.8214803021833));
#225883=CARTESIAN_POINT('Ctrl Pts',(-0.600185919568113,-7.89548110125634,
98.8347334863076));
#225884=CARTESIAN_POINT('Ctrl Pts',(-0.0246677904935639,-7.91450567373134,
98.8570695051716));
#225885=CARTESIAN_POINT('Ctrl Pts',(0.212262926423433,-7.91169723486317,
98.8661982021483));
#225886=CARTESIAN_POINT('Ctrl Pts',(0.759972172086068,-7.88058120306497,
98.8874337134158));
#225887=CARTESIAN_POINT('Ctrl Pts',(1.06990866691048,-7.84451415959061,
98.8995478124556));
#225888=CARTESIAN_POINT('Ctrl Pts',(1.40376157272442,-7.78550696426278,
98.9131138329763));
#225889=CARTESIAN_POINT('Ctrl Pts',(1.43060116509962,-7.78061986846865,
98.9142081852918));
#225890=CARTESIAN_POINT('Ctrl Pts',(1.47031382070948,-7.77317634548602,
98.915833375055));
#225891=CARTESIAN_POINT('Ctrl Pts',(1.48320675079332,-7.77072654018406,
98.9163619330019));
#225892=CARTESIAN_POINT('Ctrl Pts',(1.50609523145509,-7.76631842631278,
98.9173019794369));
#225893=CARTESIAN_POINT('Ctrl Pts',(1.51609321894849,-7.76437287202534,
98.9177131846985));
#225894=CARTESIAN_POINT('Ctrl Pts',(1.53707686316422,-7.76024749301256,
98.9185774679981));
#225895=CARTESIAN_POINT('Ctrl Pts',(1.54806170063479,-7.75806363766974,
98.9190306369322));
#225896=CARTESIAN_POINT('Ctrl Pts',(1.57714518747676,-7.7522174267336,98.9202324111841));
#225897=CARTESIAN_POINT('Ctrl Pts',(1.59523558129246,-7.74851504541726,
98.9209819700916));
#225898=CARTESIAN_POINT('Ctrl Pts',(1.69370014617598,-7.72800383934418,
98.9250728845901));
#225899=CARTESIAN_POINT('Ctrl Pts',(1.77382085339344,-7.71000796148252,
98.9284416655938));
#225900=CARTESIAN_POINT('Ctrl Pts',(2.01821425200847,-7.65110373003592,
98.9388226137978));
#225901=CARTESIAN_POINT('Ctrl Pts',(2.18146487550481,-7.60616765252071,
98.9459026261555));
#225902=CARTESIAN_POINT('Ctrl Pts',(2.68719672269585,-7.44933883790576,
98.9681609105973));
#225903=CARTESIAN_POINT('Ctrl Pts',(3.02356479363775,-7.31927160074027,
98.9834224472502));
#225904=CARTESIAN_POINT('Ctrl Pts',(3.48770527884947,-7.10232167752844,
99.0048263390568));
#225905=CARTESIAN_POINT('Ctrl Pts',(3.62362831538655,-7.03394485904147,
99.0111423730151));
#225906=CARTESIAN_POINT('Ctrl Pts',(3.76166445949593,-6.95944135133719,
99.0176046637327));
#225907=CARTESIAN_POINT('Ctrl Pts',(3.76583001924336,-6.95718820319961,
99.0177997249003));
#225908=CARTESIAN_POINT('Ctrl Pts',(3.84118415175708,-6.91634170435553,
99.021329187333));
#225909=CARTESIAN_POINT('Ctrl Pts',(3.91177854312674,-6.87666104163887,
99.0246493140159));
#225910=CARTESIAN_POINT('Ctrl Pts',(4.05664281298024,-6.79228103450938,
99.031492475074));
#225911=CARTESIAN_POINT('Ctrl Pts',(4.13081247487797,-6.74743070373213,
99.0350128964895));
#225912=CARTESIAN_POINT('Ctrl Pts',(4.23154456760542,-6.68423452995794,
99.0398199092137));
#225913=CARTESIAN_POINT('Ctrl Pts',(4.25875341140569,-6.66693183346884,
99.0411209768227));
#225914=CARTESIAN_POINT('Ctrl Pts',(4.30194473364927,-6.63909322871091,
99.0431907244313));
#225915=CARTESIAN_POINT('Ctrl Pts',(4.31799601499919,-6.62866485861541,
99.0439608934649));
#225916=CARTESIAN_POINT('Ctrl Pts',(4.3509141434526,-6.60710794845414,99.0455424544446));
#225917=CARTESIAN_POINT('Ctrl Pts',(4.36777652176863,-6.59597283082689,
99.0463537483332));
#225918=CARTESIAN_POINT('Ctrl Pts',(4.40678942579361,-6.56999534903854,
99.0482334934496));
#225919=CARTESIAN_POINT('Ctrl Pts',(4.42890796742315,-6.5551053502039,99.0493012779171));
#225920=CARTESIAN_POINT('Ctrl Pts',(4.49926030241381,-6.50722617329936,
99.052704457633));
#225921=CARTESIAN_POINT('Ctrl Pts',(4.54720419930508,-6.47381415965826,
99.0550340474065));
#225922=CARTESIAN_POINT('Ctrl Pts',(5.24646893870848,-5.97489704992239,
99.0891817507046));
#225923=CARTESIAN_POINT('Ctrl Pts',(5.82386893201732,-5.4136424181868,99.1198409935087));
#225924=CARTESIAN_POINT('Ctrl Pts',(6.64221580538611,-4.33277928054284,
99.1706381247242));
#225925=CARTESIAN_POINT('Ctrl Pts',(6.92973663164825,-3.85625118077057,
99.1910123616771));
#225926=CARTESIAN_POINT('Ctrl Pts',(7.17019824564363,-3.34250331177446,
99.2134958864722));
#225927=CARTESIAN_POINT('Ctrl Pts',(7.17536900682167,-3.33138873225042,
99.2139825987286));
#225928=CARTESIAN_POINT('Ctrl Pts',(7.19278697138116,-3.29372003962416,
99.2156332448697));
#225929=CARTESIAN_POINT('Ctrl Pts',(7.20491269926392,-3.26711020436851,
99.2168011669056));
#225930=CARTESIAN_POINT('Ctrl Pts',(7.22137695041343,-3.23044206040998,
99.2184137642866));
#225931=CARTESIAN_POINT('Ctrl Pts',(7.22584260538315,-3.2204409025077,99.218853923675));
#225932=CARTESIAN_POINT('Ctrl Pts',(7.23291627397618,-3.20451012410709,
99.2195556096784));
#225933=CARTESIAN_POINT('Ctrl Pts',(7.23553780732859,-3.19858650036404,
99.2198166439741));
#225934=CARTESIAN_POINT('Ctrl Pts',(7.24062001124114,-3.18706451917233,
99.2203246276588));
#225935=CARTESIAN_POINT('Ctrl Pts',(7.24308147196374,-3.18146651511298,
99.2205715475689));
#225936=CARTESIAN_POINT('Ctrl Pts',(7.24894743708985,-3.16808368710794,
99.2211621271317));
#225937=CARTESIAN_POINT('Ctrl Pts',(7.25234589179522,-3.16029622967963,
99.2215060128619));
#225938=CARTESIAN_POINT('Ctrl Pts',(7.26248234121273,-3.13696640238405,
99.2225369497129));
#225939=CARTESIAN_POINT('Ctrl Pts',(7.26918294289581,-3.12140790405018,
99.223225425313));
#225940=CARTESIAN_POINT('Ctrl Pts',(7.32870920387433,-2.98195937300613,
99.2294054645787));
#225941=CARTESIAN_POINT('Ctrl Pts',(7.37840681388255,-2.85677652079024,
99.2350260527524));
#225942=CARTESIAN_POINT('Ctrl Pts',(7.44935769551707,-2.66383503064301,
99.2438340069574));
#225943=CARTESIAN_POINT('Ctrl Pts',(7.47293020285764,-2.59697148874598,
99.246908825913));
#225944=CARTESIAN_POINT('Ctrl Pts',(7.55238080543388,-2.3615656903002,99.2577922049086));
#225945=CARTESIAN_POINT('Ctrl Pts',(7.60347931466858,-2.19147127737009,
99.2657584727625));
#225946=CARTESIAN_POINT('Ctrl Pts',(7.7706368263004,-1.55846266697287,99.2954662118341));
#225947=CARTESIAN_POINT('Ctrl Pts',(7.85048012432108,-1.08701359333058,
99.3176475870243));
#225948=CARTESIAN_POINT('Ctrl Pts',(7.90410469806455,-0.395055029340094,
99.3486391877209));
#225949=CARTESIAN_POINT('Ctrl Pts',(7.91196380928407,-0.17825985578506,
99.3581406332996));
#225950=CARTESIAN_POINT('Ctrl Pts',(7.90996582736476,0.231277259141387,
99.375617604322));
#225951=CARTESIAN_POINT('Ctrl Pts',(7.90198648914165,0.423868870817894,
99.3836398312914));
#225952=CARTESIAN_POINT('Ctrl Pts',(7.88544742337866,0.6356321597011,99.3922435974754));
#225953=CARTESIAN_POINT('Ctrl Pts',(7.8838396532414,0.655272186597666,99.3930395153676));
#225954=CARTESIAN_POINT('Ctrl Pts',(7.88133608038385,0.6845111552324,99.3942214184362));
#225955=CARTESIAN_POINT('Ctrl Pts',(7.88049609358636,0.694114726383551,
99.394609131192));
#225956=CARTESIAN_POINT('Ctrl Pts',(7.8790245802502,0.710591516297084,99.3952734997001));
#225957=CARTESIAN_POINT('Ctrl Pts',(7.87840160993954,0.717465477952482,
99.3955504206153));
#225958=CARTESIAN_POINT('Ctrl Pts',(7.87710251092903,0.731594232613963,
99.3961190976005));
#225959=CARTESIAN_POINT('Ctrl Pts',(7.87642535378712,0.738848926012412,
99.3964108214559));
#225960=CARTESIAN_POINT('Ctrl Pts',(7.87483499467366,0.755636497234123,
99.3970852453478));
#225961=CARTESIAN_POINT('Ctrl Pts',(7.87391450286643,0.765168681835595,
99.3974677183516));
#225962=CARTESIAN_POINT('Ctrl Pts',(7.87109962839674,0.793775193009246,
99.3986141246069));
#225963=CARTESIAN_POINT('Ctrl Pts',(7.86915322119475,0.812844391697003,
99.3993764374307));
#225964=CARTESIAN_POINT('Ctrl Pts',(7.85344592962012,0.961384444731322,
99.4052999713715));
#225965=CARTESIAN_POINT('Ctrl Pts',(7.83655965069292,1.09050806284452,99.4103627189021));
#225966=CARTESIAN_POINT('Ctrl Pts',(7.76572813182077,1.54463554969295,99.4278988366886));
#225967=CARTESIAN_POINT('Ctrl Pts',(7.69468161645525,1.86663601457365,99.4398264764234));
#225968=CARTESIAN_POINT('Ctrl Pts',(7.52496664335182,2.45770457073493,99.4613792201013));
#225969=CARTESIAN_POINT('Ctrl Pts',(7.43137347190531,2.72765971308225,99.4710877813163));
#225970=CARTESIAN_POINT('Ctrl Pts',(7.14201751954367,3.43591193272017,99.4971100332526));
#225971=CARTESIAN_POINT('Ctrl Pts',(6.92066575446557,3.86241050028523,99.5133517542529));
#225972=CARTESIAN_POINT('Ctrl Pts',(6.59827504956847,4.36585508380428,99.5359785540405));
#225973=CARTESIAN_POINT('Ctrl Pts',(6.53223462772573,4.46406010133416,99.5405728360392));
#225974=CARTESIAN_POINT('Ctrl Pts',(6.4569133424467,4.57081426256553,99.5458089232293));
#225975=CARTESIAN_POINT('Ctrl Pts',(6.44978372757322,4.58086921872577,99.5463045140328));
#225976=CARTESIAN_POINT('Ctrl Pts',(6.43980445550087,4.59487358835497,99.5469981948218));
#225977=CARTESIAN_POINT('Ctrl Pts',(6.43697457505507,4.59883713975062,99.5471949065805));
#225978=CARTESIAN_POINT('Ctrl Pts',(6.43201802876971,4.60576577694451,99.54753945347));
#225979=CARTESIAN_POINT('Ctrl Pts',(6.42989296565739,4.60873201266815,99.5476871758118));
#225980=CARTESIAN_POINT('Ctrl Pts',(6.42542860009387,4.61495442883033,99.5479975191016));
#225981=CARTESIAN_POINT('Ctrl Pts',(6.42308887373719,4.6182103021671,99.5481601701002));
#225982=CARTESIAN_POINT('Ctrl Pts',(6.41750368342175,4.6259699837609,99.5485484477531));
#225983=CARTESIAN_POINT('Ctrl Pts',(6.41425595588301,4.63047215189779,99.5487742361499));
#225984=CARTESIAN_POINT('Ctrl Pts',(6.40324302910806,4.64570502257368,99.5495399199206));
#225985=CARTESIAN_POINT('Ctrl Pts',(6.39545577811958,4.65641942163472,99.5500814228644));
#225986=CARTESIAN_POINT('Ctrl Pts',(6.19722667876004,4.92772549688855,99.5638675442345));
#225987=CARTESIAN_POINT('Ctrl Pts',(5.99105739798228,5.17641658403769,99.5782333546393));
#225988=CARTESIAN_POINT('Ctrl Pts',(5.41993088809848,5.78537753992614,99.6164302182257));
#225989=CARTESIAN_POINT('Ctrl Pts',(5.03407603840127,6.12408151391154,99.6407002800454));
#225990=CARTESIAN_POINT('Ctrl Pts',(4.28250626289484,6.66445773220789,99.682484282267));
#225991=CARTESIAN_POINT('Ctrl Pts',(3.92839257188176,6.87914681779897,99.7003562911821));
#225992=CARTESIAN_POINT('Ctrl Pts',(3.53554684585869,7.07704200256692,99.7181746442548));
#225993=CARTESIAN_POINT('Ctrl Pts',(3.51196023590244,7.0887763630854,99.7192373389474));
#225994=CARTESIAN_POINT('Ctrl Pts',(3.47992325037195,7.10451564823155,99.7206711980472));
#225995=CARTESIAN_POINT('Ctrl Pts',(3.47152389039472,7.1086236574798,99.7210462357114));
#225996=CARTESIAN_POINT('Ctrl Pts',(3.4572986767142,7.1155497849202,99.7216799062755));
#225997=CARTESIAN_POINT('Ctrl Pts',(3.45147662225779,7.11837565797071,99.721938830037));
#225998=CARTESIAN_POINT('Ctrl Pts',(3.44027402499826,7.12379613091841,99.7224362307485));
#225999=CARTESIAN_POINT('Ctrl Pts',(3.43489399963865,7.12639178641137,99.7226747471569));
#226000=CARTESIAN_POINT('Ctrl Pts',(3.42222039983532,7.13248862524414,99.7232357708466));
#226001=CARTESIAN_POINT('Ctrl Pts',(3.41492437745777,7.13598472189183,99.7235580876067));
#226002=CARTESIAN_POINT('Ctrl Pts',(3.39495045267268,7.14551814788077,99.7244386854815));
#226003=CARTESIAN_POINT('Ctrl Pts',(3.38226178948552,7.15153293832773,99.7249961242341));
#226004=CARTESIAN_POINT('Ctrl Pts',(3.30224808529317,7.18920114969296,99.7284989553831));
#226005=CARTESIAN_POINT('Ctrl Pts',(3.23449426377056,7.21993787035328,99.7314101218146));
#226006=CARTESIAN_POINT('Ctrl Pts',(3.03478114565198,7.30716264832339,99.7398369059276));
#226007=CARTESIAN_POINT('Ctrl Pts',(2.90170398506538,7.36102161355111,99.7452566758439));
#226008=CARTESIAN_POINT('Ctrl Pts',(2.45031442786735,7.52956294805092,99.7630626215027));
#226009=CARTESIAN_POINT('Ctrl Pts',(2.12612378533902,7.62744887504805,99.7748868692137));
#226010=CARTESIAN_POINT('Ctrl Pts',(1.11075455528472,7.86423420933607,99.8104736048209));
#226011=CARTESIAN_POINT('Ctrl Pts',(0.406690666053647,7.93185002458857,
99.8329572724607));
#226012=CARTESIAN_POINT('Ctrl Pts',(-0.338035826160578,7.90388185081331,
99.8622130333718));
#226013=CARTESIAN_POINT('Ctrl Pts',(-0.379170216534957,7.9020153350695,
99.8638474514539));
#226014=CARTESIAN_POINT('Ctrl Pts',(-0.427966331734888,7.89941927939347,
99.8658102803397));
#226015=CARTESIAN_POINT('Ctrl Pts',(-0.435644628270546,7.89899954993055,
99.8661198457778));
#226016=CARTESIAN_POINT('Ctrl Pts',(-0.448083273495483,7.89830140717396,
99.8666224944332));
#226017=CARTESIAN_POINT('Ctrl Pts',(-0.452843992029466,7.89802988453942,
99.8668151523714));
#226018=CARTESIAN_POINT('Ctrl Pts',(-0.461329434976493,7.8975382287393,
99.8671590348939));
#226019=CARTESIAN_POINT('Ctrl Pts',(-0.465054244069399,7.89731976508169,
99.8673101557158));
#226020=CARTESIAN_POINT('Ctrl Pts',(-0.472905817002281,7.89685368863958,
99.86762905851));
#226021=CARTESIAN_POINT('Ctrl Pts',(-0.477032542688414,7.89660547606497,
99.8677968770894));
#226022=CARTESIAN_POINT('Ctrl Pts',(-0.487927225552354,7.89594161583414,
99.8682404630001));
#226023=CARTESIAN_POINT('Ctrl Pts',(-0.494694832863919,7.89552050214902,
99.8685165615946));
#226024=CARTESIAN_POINT('Ctrl Pts',(-0.525201471588934,7.89358285295974,
99.869763595958));
#226025=CARTESIAN_POINT('Ctrl Pts',(-0.548933896884607,7.89196796716087,
99.8707404137593));
#226026=CARTESIAN_POINT('Ctrl Pts',(-0.724856136695996,7.87919987974183,
99.8780290851628));
#226027=CARTESIAN_POINT('Ctrl Pts',(-0.876693656528433,7.86375291250337,
99.8845848860862));
#226028=CARTESIAN_POINT('Ctrl Pts',(-1.22110303201062,7.81861659708257,
99.8999104414949));
#226029=CARTESIAN_POINT('Ctrl Pts',(-1.41321695100678,7.78618448157754,
99.9087853264157));
#226030=CARTESIAN_POINT('Ctrl Pts',(-2.02289269791113,7.65995314096664,
99.9375995350762));
#226031=CARTESIAN_POINT('Ctrl Pts',(-2.43413094089788,7.53936313303955,
99.9579828949913));
#226032=CARTESIAN_POINT('Ctrl Pts',(-2.94204080598174,7.34450850181288,
99.9831749588147));
#226033=CARTESIAN_POINT('Ctrl Pts',(-3.04954667650439,7.30052569107931,
99.9885115869853));
#226034=CARTESIAN_POINT('Ctrl Pts',(-3.52844454229034,7.09217380966174,
100.012254229967));
#226035=CARTESIAN_POINT('Ctrl Pts',(-3.88784257573235,6.90170974331125,
100.029946247056));
#226036=CARTESIAN_POINT('Ctrl Pts',(-4.27621615772971,6.65588101810236,
100.048789482886));
#226037=CARTESIAN_POINT('Ctrl Pts',(-4.32107990253558,6.62684279153073,
100.050962600504));
#226038=CARTESIAN_POINT('Ctrl Pts',(-4.37729986957994,6.58964051483371,
100.053681834073));
#226039=CARTESIAN_POINT('Ctrl Pts',(-4.38893273794415,6.58189833463449,
100.054244274717));
#226040=CARTESIAN_POINT('Ctrl Pts',(-4.40725271524248,6.56963542792334,
100.055129708881));
#226041=CARTESIAN_POINT('Ctrl Pts',(-4.41395349574257,6.5651352377371,100.055453499973));
#226042=CARTESIAN_POINT('Ctrl Pts',(-4.42578884400816,6.5571604025512,100.056025283168));
#226043=CARTESIAN_POINT('Ctrl Pts',(-4.43092623089538,6.55368996620407,
100.056273438725));
#226044=CARTESIAN_POINT('Ctrl Pts',(-4.44269484299823,6.54571980399677,
100.056841820331));
#226045=CARTESIAN_POINT('Ctrl Pts',(-4.44932332641263,6.54121603052424,
100.057161888295));
#226046=CARTESIAN_POINT('Ctrl Pts',(-4.46758875441763,6.52876483729024,
100.058043696273));
#226047=CARTESIAN_POINT('Ctrl Pts',(-4.47921135129115,6.52079636642775,
100.058604614279));
#226048=CARTESIAN_POINT('Ctrl Pts',(-4.53868904410173,6.47978431273023,
100.061474151067));
#226049=CARTESIAN_POINT('Ctrl Pts',(-4.58620060277757,6.44624442569634,
100.063763309444));
#226050=CARTESIAN_POINT('Ctrl Pts',(-4.71402705842803,6.35387912016852,
100.069916615734));
#226051=CARTESIAN_POINT('Ctrl Pts',(-4.79360933159158,6.29405603926756,
100.073741433449));
#226052=CARTESIAN_POINT('Ctrl Pts',(-5.07942099013546,6.07064137567329,
100.087480445971));
#226053=CARTESIAN_POINT('Ctrl Pts',(-5.27858640632783,5.89828291865341,
100.097052707928));
#226054=CARTESIAN_POINT('Ctrl Pts',(-5.60729108466952,5.58381087315769,
100.11318185826));
#226055=CARTESIAN_POINT('Ctrl Pts',(-5.74092604192876,5.44632237629273,
100.119847616671));
#226056=CARTESIAN_POINT('Ctrl Pts',(-6.28239925648062,4.84713788875576,
100.147769130589));
#226057=CARTESIAN_POINT('Ctrl Pts',(-6.64057738476161,4.34350109300738,
100.168481894583));
#226058=CARTESIAN_POINT('Ctrl Pts',(-6.95620979018949,3.76785268141195,
100.194408357079));
#226059=CARTESIAN_POINT('Ctrl Pts',(-6.97544972951901,3.73211326997488,
100.196025014702));
#226060=CARTESIAN_POINT('Ctrl Pts',(-6.99972811589647,3.68617100640897,
100.198110850572));
#226061=CARTESIAN_POINT('Ctrl Pts',(-7.00502098498729,3.67610274381265,
100.198568430119));
#226062=CARTESIAN_POINT('Ctrl Pts',(-7.01341415730664,3.66005303887433,
100.199298562521));
#226063=CARTESIAN_POINT('Ctrl Pts',(-7.0165285778904,3.65407896802547,100.199570490907));
#226064=CARTESIAN_POINT('Ctrl Pts',(-7.02233395673365,3.64290832245376,
100.200079240985));
#226065=CARTESIAN_POINT('Ctrl Pts',(-7.02502678930221,3.63771272299616,
100.200315981043));
#226066=CARTESIAN_POINT('Ctrl Pts',(-7.03100777589281,3.62614149145517,
100.200843477906));
#226067=CARTESIAN_POINT('Ctrl Pts',(-7.03429302564407,3.61976436935683,
100.201134358607));
#226068=CARTESIAN_POINT('Ctrl Pts',(-7.04382014383441,3.6012089710082,100.201981199657));
#226069=CARTESIAN_POINT('Ctrl Pts',(-7.05003907495541,3.58901898995439,
100.202538121082));
#226070=CARTESIAN_POINT('Ctrl Pts',(-7.09374963978311,3.50278813594496,
100.206481627742));
#226071=CARTESIAN_POINT('Ctrl Pts',(-7.13010501193297,3.42817890692869,
100.209913859396));
#226072=CARTESIAN_POINT('Ctrl Pts',(-7.24354722690091,3.18575661924743,
100.221105052021));
#226073=CARTESIAN_POINT('Ctrl Pts',(-7.31593287202391,3.015815599745,100.22900877245));
#226074=CARTESIAN_POINT('Ctrl Pts',(-7.69508737201932,2.03145472543838,
100.274677109224));
#226075=CARTESIAN_POINT('Ctrl Pts',(-7.8717964715237,1.1731838255701,100.313261996288));
#226076=CARTESIAN_POINT('Ctrl Pts',(-7.90778348611013,0.235565568481009,
100.351510221745));
#226077=CARTESIAN_POINT('Ctrl Pts',(-7.90951398097792,0.167688775737525,
100.354262554791));
#226078=CARTESIAN_POINT('Ctrl Pts',(-7.91063518710626,0.0788173711341605,
100.357846248243));
#226079=CARTESIAN_POINT('Ctrl Pts',(-7.91081640755467,0.0578360815328407,
100.358690834597));
#226080=CARTESIAN_POINT('Ctrl Pts',(-7.91095939646905,0.0271429402881354,
100.359924196337));
#226081=CARTESIAN_POINT('Ctrl Pts',(-7.91098675602236,0.0174315323452157,
100.360314118503));
#226082=CARTESIAN_POINT('Ctrl Pts',(-7.9109986139482,0.00528037141865606,
100.36080160118));
#226083=CARTESIAN_POINT('Ctrl Pts',(-7.91099986619226,0.0028406554486198,
100.36089945812));
#226084=CARTESIAN_POINT('Ctrl Pts',(-7.91099998983997,0.000400938813840742,
100.360997295013));
#226085=CARTESIAN_POINT('',(-7.91099966760513,0.0022932840043321,104.357668491763));
#226086=CARTESIAN_POINT('Ctrl Pts',(-7.91099998985159,0.000400709535323949,
100.360997304208));
#226087=CARTESIAN_POINT('Ctrl Pts',(-7.91100005916832,-0.00096777466909486,
100.361052182811));
#226088=CARTESIAN_POINT('Ctrl Pts',(-7.91099977339425,-0.0023362592533744,
100.361107055113));
#226089=CARTESIAN_POINT('Ctrl Pts',(-7.91099481889614,-0.0129159455629224,
100.361531221317));
#226090=CARTESIAN_POINT('Ctrl Pts',(-7.91097441761624,-0.0221271438946392,
100.361900235188));
#226091=CARTESIAN_POINT('Ctrl Pts',(-7.9108839673096,-0.0449601254811435,
100.362814247241));
#226092=CARTESIAN_POINT('Ctrl Pts',(-7.91079482285094,-0.0585818167777481,
100.363358901693));
#226093=CARTESIAN_POINT('Ctrl Pts',(-7.91047650445436,-0.0934571507487213,
100.364751764797));
#226094=CARTESIAN_POINT('Ctrl Pts',(-7.91019685774666,-0.114710259158208,
100.365599052871));
#226095=CARTESIAN_POINT('Ctrl Pts',(-7.90875991398719,-0.198306994295018,
100.368925776633));
#226096=CARTESIAN_POINT('Ctrl Pts',(-7.90695119593621,-0.260637607527513,
100.371393086984));
#226097=CARTESIAN_POINT('Ctrl Pts',(-7.90249133677941,-0.36979856628818,
100.375691679267));
#226098=CARTESIAN_POINT('Ctrl Pts',(-7.90016029240393,-0.416638596432845,
100.377528920584));
#226099=CARTESIAN_POINT('Ctrl Pts',(-7.84862792702768,-1.29476478794368,
100.411841212678));
#226100=CARTESIAN_POINT('Ctrl Pts',(-7.66891076730538,-2.11305738826948,
100.44078653494));
#226101=CARTESIAN_POINT('Ctrl Pts',(-7.30927976399866,-3.03011227916851,
100.477635387858));
#226102=CARTESIAN_POINT('Ctrl Pts',(-7.24954767217067,-3.17036380904551,
100.48342851042));
#226103=CARTESIAN_POINT('Ctrl Pts',(-7.15675422184594,-3.37188582833366,
100.492090936159));
#226104=CARTESIAN_POINT('Ctrl Pts',(-7.12687537517983,-3.43458760615161,
100.494835201216));
#226105=CARTESIAN_POINT('Ctrl Pts',(-7.09094407331893,-3.50750241825568,
100.498092809226));
#226106=CARTESIAN_POINT('Ctrl Pts',(-7.08568891353161,-3.5181065480568,
100.498568226209));
#226107=CARTESIAN_POINT('Ctrl Pts',(-7.07762446072729,-3.53428804595264,
100.499296285653));
#226108=CARTESIAN_POINT('Ctrl Pts',(-7.07483231129418,-3.53987397594719,
100.499548088056));
#226109=CARTESIAN_POINT('Ctrl Pts',(-7.06974115123421,-3.55002918556588,
100.500006734873));
#226110=CARTESIAN_POINT('Ctrl Pts',(-7.06744431572416,-3.55459955659971,
100.500213470987));
#226111=CARTESIAN_POINT('Ctrl Pts',(-7.06248339828401,-3.56444724978386,
100.500659620807));
#226112=CARTESIAN_POINT('Ctrl Pts',(-7.05981783171737,-3.56972381707702,
100.500899109287));
#226113=CARTESIAN_POINT('Ctrl Pts',(-7.05261156336944,-3.58394919545232,
100.501545941749));
#226114=CARTESIAN_POINT('Ctrl Pts',(-7.04805975554051,-3.59289234186743,
100.501953853564));
#226115=CARTESIAN_POINT('Ctrl Pts',(-7.02683902294677,-3.63439018384741,
100.503852622512));
#226116=CARTESIAN_POINT('Ctrl Pts',(-7.00996164324436,-3.66683738680443,
100.50535447422));
#226117=CARTESIAN_POINT('Ctrl Pts',(-6.70604959406883,-4.24134902490025,
100.532268565335));
#226118=CARTESIAN_POINT('Ctrl Pts',(-6.35717693381678,-4.74829909701657,
100.560950994744));
#226119=CARTESIAN_POINT('Ctrl Pts',(-5.89970098056773,-5.27105985696377,
100.592927251231));
#226120=CARTESIAN_POINT('Ctrl Pts',(-5.84516589666356,-5.33147066726718,
100.596665848537));
#226121=CARTESIAN_POINT('Ctrl Pts',(-5.67328505447062,-5.51606247539534,
100.608210721887));
#226122=CARTESIAN_POINT('Ctrl Pts',(-5.55283970542294,-5.63729390171303,
100.615966660102));
#226123=CARTESIAN_POINT('Ctrl Pts',(-5.22584614081406,-5.94576451901958,
100.636082923621));
#226124=CARTESIAN_POINT('Ctrl Pts',(-5.01315853501962,-6.12616058863582,
100.64823983385));
#226125=CARTESIAN_POINT('Ctrl Pts',(-4.67712960497867,-6.38192721901521,
100.666017629867));
#226126=CARTESIAN_POINT('Ctrl Pts',(-4.56052961069703,-6.4657643614975,
100.671948211451));
#226127=CARTESIAN_POINT('Ctrl Pts',(-4.42602670540259,-6.55702430384257,
100.678529492214));
#226128=CARTESIAN_POINT('Ctrl Pts',(-4.41030691548808,-6.56760786249891,
100.679294755282));
#226129=CARTESIAN_POINT('Ctrl Pts',(-4.38666934192807,-6.58339903756214,
100.680439642338));
#226130=CARTESIAN_POINT('Ctrl Pts',(-4.3787800348527,-6.58864904288807,
100.680820792555));
#226131=CARTESIAN_POINT('Ctrl Pts',(-4.36520877535687,-6.59764500891665,
100.681474792782));
#226132=CARTESIAN_POINT('Ctrl Pts',(-4.35953139658114,-6.60139783065872,
100.68174788911));
#226133=CARTESIAN_POINT('Ctrl Pts',(-4.34784198503017,-6.6091030283048,
100.682309159904));
#226134=CARTESIAN_POINT('Ctrl Pts',(-4.34182938763695,-6.61305453890542,
100.682597303221));
#226135=CARTESIAN_POINT('Ctrl Pts',(-4.32566470163404,-6.62364650695907,
100.683370485952));
#226136=CARTESIAN_POINT('Ctrl Pts',(-4.31550269821128,-6.63027183631714,
100.683854983857));
#226137=CARTESIAN_POINT('Ctrl Pts',(-4.27839620460869,-6.6543427373366,
100.685618443905));
#226138=CARTESIAN_POINT('Ctrl Pts',(-4.2513606816658,-6.67164775250914,
100.686892393602));
#226139=CARTESIAN_POINT('Ctrl Pts',(-3.81382648893587,-6.9479670039561,
100.707336783204));
#226140=CARTESIAN_POINT('Ctrl Pts',(-3.38043850933824,-7.16883667239189,
100.725063383063));
#226141=CARTESIAN_POINT('Ctrl Pts',(-2.84720211064242,-7.38140976604101,
100.745227892795));
#226142=CARTESIAN_POINT('Ctrl Pts',(-2.76435998044787,-7.41283239400004,
100.748318652713));
#226143=CARTESIAN_POINT('Ctrl Pts',(-2.43402420655599,-7.53182332837274,
100.760515467844));
#226144=CARTESIAN_POINT('Ctrl Pts',(-2.18276736766272,-7.60844020606949,
100.769506912133));
#226145=CARTESIAN_POINT('Ctrl Pts',(-1.84167196983505,-7.69416138619284,
100.781724609971));
#226146=CARTESIAN_POINT('Ctrl Pts',(-1.75481518895129,-7.71443442395475,
100.784837201403));
#226147=CARTESIAN_POINT('Ctrl Pts',(-1.53823893740258,-7.76113805571743,
100.792633668757));
#226148=CARTESIAN_POINT('Ctrl Pts',(-1.40816548850933,-7.78578907201624,
100.797347232527));
#226149=CARTESIAN_POINT('Ctrl Pts',(-1.05840165874163,-7.84302323090708,
100.810221403693));
#226150=CARTESIAN_POINT('Ctrl Pts',(-0.837855640838945,-7.86963948626871,
100.818554502827));
#226151=CARTESIAN_POINT('Ctrl Pts',(-0.579343375109531,-7.88984599264882,
100.828797216712));
#226152=CARTESIAN_POINT('Ctrl Pts',(-0.54218740047322,-7.89248638226708,
100.830279669501));
#226153=CARTESIAN_POINT('Ctrl Pts',(-0.494133034163816,-7.89556029914677,
100.832209090516));
#226154=CARTESIAN_POINT('Ctrl Pts',(-0.483250077759971,-7.89623386519002,
100.832646854621));
#226155=CARTESIAN_POINT('Ctrl Pts',(-0.465659242591914,-7.89728609134848,
100.83335570745));
#226156=CARTESIAN_POINT('Ctrl Pts',(-0.458952191503839,-7.8976787111398,
100.83362627694));
#226157=CARTESIAN_POINT('Ctrl Pts',(-0.446142465048931,-7.89841219864895,
100.834143593219));
#226158=CARTESIAN_POINT('Ctrl Pts',(-0.440039876332967,-7.89875453890491,
100.834390286114));
#226159=CARTESIAN_POINT('Ctrl Pts',(-0.426077969227882,-7.89952153699445,
100.83495523163));
#226160=CARTESIAN_POINT('Ctrl Pts',(-0.41821840786343,-7.89994153852388,
100.835273650924));
#226161=CARTESIAN_POINT('Ctrl Pts',(-0.397732550399217,-7.90100561047211,
100.836104616503));
#226162=CARTESIAN_POINT('Ctrl Pts',(-0.385105338999635,-7.90163114262455,
100.836617811781));
#226163=CARTESIAN_POINT('Ctrl Pts',(-0.305865402588814,-7.9053661700103,
100.839844348893));
#226164=CARTESIAN_POINT('Ctrl Pts',(-0.239218046762037,-7.90766352166946,
100.842585003055));
#226165=CARTESIAN_POINT('Ctrl Pts',(0.459836101678615,-7.92291456581624,
100.871565607677));
#226166=CARTESIAN_POINT('Ctrl Pts',(1.09160157046669,-7.86081892124048,
100.899484006929));
#226167=CARTESIAN_POINT('Ctrl Pts',(2.25074628292139,-7.60431839871772,
100.950136841868));
#226168=CARTESIAN_POINT('Ctrl Pts',(2.77816658765272,-7.42787622751898,
100.973003691385));
#226169=CARTESIAN_POINT('Ctrl Pts',(3.39813805748106,-7.14511353541758,
101.000747912315));
#226170=CARTESIAN_POINT('Ctrl Pts',(3.51219080823494,-7.08974652916456,
101.005891423149));
#226171=CARTESIAN_POINT('Ctrl Pts',(3.66024580239727,-7.01342328465121,
101.012619174058));
#226172=CARTESIAN_POINT('Ctrl Pts',(3.69548897919018,-6.9949172063736,101.014224541886));
#226173=CARTESIAN_POINT('Ctrl Pts',(3.75065085023848,-6.96541862836639,
101.016743410991));
#226174=CARTESIAN_POINT('Ctrl Pts',(3.77066430089724,-6.95460489185226,
101.017658580189));
#226175=CARTESIAN_POINT('Ctrl Pts',(3.80911675744417,-6.93361335072045,
101.019419435291));
#226176=CARTESIAN_POINT('Ctrl Pts',(3.82756230668795,-6.92344793870984,
101.020265234119));
#226177=CARTESIAN_POINT('Ctrl Pts',(3.87134428700345,-6.899091079969,101.022275505455));
#226178=CARTESIAN_POINT('Ctrl Pts',(3.89664362678815,-6.88483353252962,
101.023439299797));
#226179=CARTESIAN_POINT('Ctrl Pts',(3.96917665107978,-6.84342937539568,
101.026782242814));
#226180=CARTESIAN_POINT('Ctrl Pts',(4.01620929610038,-6.8159336732329,101.028957700803));
#226181=CARTESIAN_POINT('Ctrl Pts',(4.41605306701844,-6.57660575090095,
101.047522276427));
#226182=CARTESIAN_POINT('Ctrl Pts',(4.75212759784963,-6.33802527947089,
101.063562877318));
#226183=CARTESIAN_POINT('Ctrl Pts',(5.27529237619319,-5.90152608548048,
101.089937214565));
#226184=CARTESIAN_POINT('Ctrl Pts',(5.47348532135607,-5.71818824218199,
101.100325569543));
#226185=CARTESIAN_POINT('Ctrl Pts',(5.77156886456959,-5.41272220065917,
101.116923132515));
#226186=CARTESIAN_POINT('Ctrl Pts',(5.87784527551233,-5.29712208291849,
101.123061142573));
#226187=CARTESIAN_POINT('Ctrl Pts',(6.0331678807113,-5.11773905591105,101.132449264833));
#226188=CARTESIAN_POINT('Ctrl Pts',(6.08479795655919,-5.05624379065121,
101.135644736944));
#226189=CARTESIAN_POINT('Ctrl Pts',(6.14795112896188,-4.97865524500463,
101.139657082936));
#226190=CARTESIAN_POINT('Ctrl Pts',(6.16036237328176,-4.96328989257336,
101.140450745238));
#226191=CARTESIAN_POINT('Ctrl Pts',(6.17999134344313,-4.93880180905347,
101.141714323082));
#226192=CARTESIAN_POINT('Ctrl Pts',(6.18724674062582,-4.92970933055073,
101.142183209729));
#226193=CARTESIAN_POINT('Ctrl Pts',(6.20077459498975,-4.91267928632703,
101.143060940007));
#226194=CARTESIAN_POINT('Ctrl Pts',(6.20705193494342,-4.90474562280118,
101.143469645702));
#226195=CARTESIAN_POINT('Ctrl Pts',(6.2210079192751,-4.88703754527129,101.144381480321));
#226196=CARTESIAN_POINT('Ctrl Pts',(6.22867877464739,-4.87725703869315,
101.144884830793));
#226197=CARTESIAN_POINT('Ctrl Pts',(6.25170195895001,-4.84775907900361,
101.146402195357));
#226198=CARTESIAN_POINT('Ctrl Pts',(6.26698382969566,-4.82798706833381,
101.147418318326));
#226199=CARTESIAN_POINT('Ctrl Pts',(6.43621251127311,-4.60687808560089,
101.158769536299));
#226200=CARTESIAN_POINT('Ctrl Pts',(6.58048878899962,-4.3983312933797,101.169359868471));
#226201=CARTESIAN_POINT('Ctrl Pts',(6.90398041715958,-3.8790944094191,101.195095066997));
#226202=CARTESIAN_POINT('Ctrl Pts',(7.07257935107417,-3.56243545856963,
101.21026932914));
#226203=CARTESIAN_POINT('Ctrl Pts',(7.32623582837749,-2.99645991642265,
101.236157494663));
#226204=CARTESIAN_POINT('Ctrl Pts',(7.42140998372079,-2.75230513497619,
101.246962134732));
#226205=CARTESIAN_POINT('Ctrl Pts',(7.5241502452779,-2.44438481050283,101.260160327724));
#226206=CARTESIAN_POINT('Ctrl Pts',(7.54329149933407,-2.38466086942852,
101.26270112367));
#226207=CARTESIAN_POINT('Ctrl Pts',(7.56978994556906,-2.298468014344,101.266341761741));
#226208=CARTESIAN_POINT('Ctrl Pts',(7.57772250846246,-2.27217882773768,
101.267448693727));
#226209=CARTESIAN_POINT('Ctrl Pts',(7.59064366273581,-2.22853668732433,
101.269280671657));
#226210=CARTESIAN_POINT('Ctrl Pts',(7.59570999937156,-2.21120704343135,
101.270006660184));
#226211=CARTESIAN_POINT('Ctrl Pts',(7.60635096546553,-2.1743409877202,101.271548034982));
#226212=CARTESIAN_POINT('Ctrl Pts',(7.61190975628225,-2.15480013130315,
101.272363225454));
#226213=CARTESIAN_POINT('Ctrl Pts',(7.62530685042445,-2.10700642774324,
101.274352712888));
#226214=CARTESIAN_POINT('Ctrl Pts',(7.63306348906893,-2.07873096626329,
101.275526032187));
#226215=CARTESIAN_POINT('Ctrl Pts',(7.65942393061049,-1.9805013668055,101.279589835149));
#226216=CARTESIAN_POINT('Ctrl Pts',(7.67722477270231,-1.9103351857398,101.282470970352));
#226217=CARTESIAN_POINT('Ctrl Pts',(7.89729692987313,-0.990058558941479,
101.320006150638));
#226218=CARTESIAN_POINT('Ctrl Pts',(7.95833190498834,-0.112304059540934,
101.353170914501));
#226219=CARTESIAN_POINT('Ctrl Pts',(7.83927230885938,1.12522379101394,101.39965769443));
#226220=CARTESIAN_POINT('Ctrl Pts',(7.77820526873281,1.48990706853756,101.413416232623));
#226221=CARTESIAN_POINT('Ctrl Pts',(7.6634649773623,1.967236535514,101.432447323821));
#226222=CARTESIAN_POINT('Ctrl Pts',(7.6323142229527,2.08482450204241,101.43722284046));
#226223=CARTESIAN_POINT('Ctrl Pts',(7.59383411895244,2.21762967049555,101.442752665435));
#226224=CARTESIAN_POINT('Ctrl Pts',(7.58915199659253,2.23360022155599,101.44341992122));
#226225=CARTESIAN_POINT('Ctrl Pts',(7.58202083237059,2.25764307521548,101.444427985319));
#226226=CARTESIAN_POINT('Ctrl Pts',(7.57960920373895,2.26572647854178,101.444767509556));
#226227=CARTESIAN_POINT('Ctrl Pts',(7.57543042168483,2.27965176652856,101.445353470827));
#226228=CARTESIAN_POINT('Ctrl Pts',(7.57366942558344,2.28549550036317,101.445599691788));
#226229=CARTESIAN_POINT('Ctrl Pts',(7.57002011958822,2.29755491544697,101.446108481042));
#226230=CARTESIAN_POINT('Ctrl Pts',(7.56813091320335,2.30377031858125,101.446371081109));
#226231=CARTESIAN_POINT('Ctrl Pts',(7.56300261091426,2.32056781410366,101.44708179057));
#226232=CARTESIAN_POINT('Ctrl Pts',(7.55974896854687,2.33114542739003,101.447530426397));
#226233=CARTESIAN_POINT('Ctrl Pts',(7.54761972911092,2.37028521479327,101.449194632818));
#226234=CARTESIAN_POINT('Ctrl Pts',(7.53860443425562,2.3988036034688,101.450415399509));
#226235=CARTESIAN_POINT('Ctrl Pts',(7.42609301827079,2.74781570205716,101.465462074449));
#226236=CARTESIAN_POINT('Ctrl Pts',(7.30241715924047,3.06136647774508,101.480258866279));
#226237=CARTESIAN_POINT('Ctrl Pts',(6.99575079669148,3.71361144334974,101.512842903827));
#226238=CARTESIAN_POINT('Ctrl Pts',(6.80723407151014,4.04882794291579,101.530643011971));
#226239=CARTESIAN_POINT('Ctrl Pts',(6.4126718746228,4.64442568530208,101.56307557485));
#226240=CARTESIAN_POINT('Ctrl Pts',(6.21314911762186,4.90814182622734,101.577774236613));
#226241=CARTESIAN_POINT('Ctrl Pts',(5.90838107768859,5.26248225490896,101.597752204288));
#226242=CARTESIAN_POINT('Ctrl Pts',(5.81636918978122,5.36400394144666,101.603507992191));
#226243=CARTESIAN_POINT('Ctrl Pts',(5.67151050549033,5.5157216461343,101.612156834108));
#226244=CARTESIAN_POINT('Ctrl Pts',(5.6205321273874,5.56765980119811,101.615126656836));
#226245=CARTESIAN_POINT('Ctrl Pts',(5.56100348343034,5.62665825315384,101.618511347816));
#226246=CARTESIAN_POINT('Ctrl Pts',(5.55314723047137,5.63441200823218,101.618956401246));
#226247=CARTESIAN_POINT('Ctrl Pts',(5.53813369423426,5.64916776509272,101.619803798435));
#226248=CARTESIAN_POINT('Ctrl Pts',(5.53097929930793,5.65617266753311,101.62020626783));
#226249=CARTESIAN_POINT('Ctrl Pts',(5.51854470624005,5.6683012849824,101.620903457087));
#226250=CARTESIAN_POINT('Ctrl Pts',(5.51327063162163,5.67343124352167,101.621198446886));
#226251=CARTESIAN_POINT('Ctrl Pts',(5.50311989623314,5.68327708533786,101.621764818774));
#226252=CARTESIAN_POINT('Ctrl Pts',(5.49824431282853,5.68799406625638,101.622036248155));
#226253=CARTESIAN_POINT('Ctrl Pts',(5.48675101410622,5.69908490277653,101.622674662552));
#226254=CARTESIAN_POINT('Ctrl Pts',(5.48012824332055,5.70545351899075,101.623041421925));
#226255=CARTESIAN_POINT('Ctrl Pts',(5.4572292853893,5.7273970542991,101.624305703633));
#226256=CARTESIAN_POINT('Ctrl Pts',(5.44089760660451,5.74291404567405,101.625200739425));
#226257=CARTESIAN_POINT('Ctrl Pts',(5.25713706375049,5.91602042080533,101.635197600733));
#226258=CARTESIAN_POINT('Ctrl Pts',(5.08297426266895,6.06631441966097,101.643983652174));
#226259=CARTESIAN_POINT('Ctrl Pts',(4.78185207503718,6.3040815045025,101.658187464135));
#226260=CARTESIAN_POINT('Ctrl Pts',(4.65844841703589,6.39581219610273,101.663754411411));
#226261=CARTESIAN_POINT('Ctrl Pts',(4.02438910800785,6.83903988745184,101.691282926015));
#226262=CARTESIAN_POINT('Ctrl Pts',(3.47638624463482,7.1332223252011,101.711495174422));
#226263=CARTESIAN_POINT('Ctrl Pts',(2.7248463785409,7.4292964907886,101.739868734176));
#226264=CARTESIAN_POINT('Ctrl Pts',(2.54761520587758,7.49192131832584,101.746619168375));
#226265=CARTESIAN_POINT('Ctrl Pts',(2.27076744670681,7.57878564650835,101.75746834213));
#226266=CARTESIAN_POINT('Ctrl Pts',(2.1726230989006,7.60750183158416,101.761372343206));
#226267=CARTESIAN_POINT('Ctrl Pts',(2.02577142320548,7.64739589355367,101.76733383238));
#226268=CARTESIAN_POINT('Ctrl Pts',(1.97746776458933,7.66002838451151,101.769313861859));
#226269=CARTESIAN_POINT('Ctrl Pts',(1.92041884334143,7.67437239450965,101.771678025428));
#226270=CARTESIAN_POINT('Ctrl Pts',(1.9117853178829,7.67652767080179,101.772036497268));
#226271=CARTESIAN_POINT('Ctrl Pts',(1.89855072150598,7.67980784871366,101.772587089985));
#226272=CARTESIAN_POINT('Ctrl Pts',(1.89395222256896,7.68094319818439,101.772778598846));
#226273=CARTESIAN_POINT('Ctrl Pts',(1.88556538001958,7.68300588371648,101.77312824505));
#226274=CARTESIAN_POINT('Ctrl Pts',(1.88177736226349,7.68393455010604,101.773286303813));
#226275=CARTESIAN_POINT('Ctrl Pts',(1.87416220147529,7.68579550591782,101.773604331513));
#226276=CARTESIAN_POINT('Ctrl Pts',(1.87033504567331,7.68672773896978,101.773764303751));
#226277=CARTESIAN_POINT('Ctrl Pts',(1.85944752238259,7.68937115039387,101.774219798406));
#226278=CARTESIAN_POINT('Ctrl Pts',(1.85238550832352,7.69107545827402,101.774515731048));
#226279=CARTESIAN_POINT('Ctrl Pts',(1.8215613895581,7.69846946576185,101.775809556101));
#226280=CARTESIAN_POINT('Ctrl Pts',(1.79777575019328,7.70405869149959,101.776813538316));
#226281=CARTESIAN_POINT('Ctrl Pts',(1.38538859640253,7.79894899712448,101.794311873737));
#226282=CARTESIAN_POINT('Ctrl Pts',(0.990641383771469,7.85884708564601,
101.812442911936));
#226283=CARTESIAN_POINT('Ctrl Pts',(0.131139386026713,7.92346792267918,
101.852333732414));
#226284=CARTESIAN_POINT('Ctrl Pts',(-0.333022073000432,7.91755571718185,
101.874095304605));
#226285=CARTESIAN_POINT('Ctrl Pts',(-0.97823645412795,7.85246838059121,
101.903130740182));
#226286=CARTESIAN_POINT('Ctrl Pts',(-1.16176184292804,7.82742113503187,
101.911260611669));
#226287=CARTESIAN_POINT('Ctrl Pts',(-1.51976401526566,7.76569122562137,
101.926815803433));
#226288=CARTESIAN_POINT('Ctrl Pts',(-1.69421504182749,7.72950736660577,
101.934251806786));
#226289=CARTESIAN_POINT('Ctrl Pts',(-1.89945574223054,7.67965386974466,
101.942829218535));
#226290=CARTESIAN_POINT('Ctrl Pts',(-1.93155769537997,7.67164262610024,
101.944165870249));
#226291=CARTESIAN_POINT('Ctrl Pts',(-1.97427337694746,7.6606975423293,101.945937963322));
#226292=CARTESIAN_POINT('Ctrl Pts',(-1.98493234237679,7.65794266102388,
101.946379618963));
#226293=CARTESIAN_POINT('Ctrl Pts',(-2.00247953939511,7.65336837288868,
101.947105806372));
#226294=CARTESIAN_POINT('Ctrl Pts',(-2.00937110773991,7.65156189993774,
101.947390787998));
#226295=CARTESIAN_POINT('Ctrl Pts',(-2.02275958873118,7.64803306885342,
101.947943996919));
#226296=CARTESIAN_POINT('Ctrl Pts',(-2.02925676373576,7.64631173594315,
101.948212259644));
#226297=CARTESIAN_POINT('Ctrl Pts',(-2.04430800678826,7.64230359084514,
101.94883325338));
#226298=CARTESIAN_POINT('Ctrl Pts',(-2.05286045293176,7.64001069127248,
101.949185771736));
#226299=CARTESIAN_POINT('Ctrl Pts',(-2.0804534559024,7.63256336544137,101.950322009204));
#226300=CARTESIAN_POINT('Ctrl Pts',(-2.0994786624646,7.62735206105405,101.951103741579));
#226301=CARTESIAN_POINT('Ctrl Pts',(-2.27618076738009,7.57823933329035,
101.958348792452));
#226302=CARTESIAN_POINT('Ctrl Pts',(-2.43248409934646,7.52952425532047,
101.964641152945));
#226303=CARTESIAN_POINT('Ctrl Pts',(-3.2912235966148,7.23234563404386,101.998703255845));
#226304=CARTESIAN_POINT('Ctrl Pts',(-3.95724804379451,6.89050746818473,
102.022733455498));
#226305=CARTESIAN_POINT('Ctrl Pts',(-4.72921261343966,6.34496573219549,
102.055286368333));
#226306=CARTESIAN_POINT('Ctrl Pts',(-4.88833526020827,6.223199657322,102.062321926151));
#226307=CARTESIAN_POINT('Ctrl Pts',(-5.1415302443183,6.01373873494089,102.074364761423));
#226308=CARTESIAN_POINT('Ctrl Pts',(-5.23839306547455,5.92955496332986,
102.079191043471));
#226309=CARTESIAN_POINT('Ctrl Pts',(-5.37451684279496,5.80531005160545,
102.086367726004));
#226310=CARTESIAN_POINT('Ctrl Pts',(-5.41546947915409,5.76712633004835,
102.088580255351));
#226311=CARTESIAN_POINT('Ctrl Pts',(-5.46231953483101,5.72250488563383,
102.091178700688));
#226312=CARTESIAN_POINT('Ctrl Pts',(-5.46861677578066,5.71648733271724,
102.091529388404));
#226313=CARTESIAN_POINT('Ctrl Pts',(-5.4781685914276,5.7073295276684,102.092063511409));
#226314=CARTESIAN_POINT('Ctrl Pts',(-5.48143043629186,5.70419686066637,
102.0922462988));
#226315=CARTESIAN_POINT('Ctrl Pts',(-5.48736314812334,5.69848931245899,
102.092579464802));
#226316=CARTESIAN_POINT('Ctrl Pts',(-5.49003489558143,5.69591534424395,
102.09272976533));
#226317=CARTESIAN_POINT('Ctrl Pts',(-5.49579626490353,5.69035700698463,
102.093054437749));
#226318=CARTESIAN_POINT('Ctrl Pts',(-5.49888526710921,5.68737200043111,
102.093228863761));
#226319=CARTESIAN_POINT('Ctrl Pts',(-5.50722485609883,5.67930002996268,
102.093700716961));
#226320=CARTESIAN_POINT('Ctrl Pts',(-5.5124708136108,5.67420831256058,102.093998544958));
#226321=CARTESIAN_POINT('Ctrl Pts',(-5.53680386870649,5.65052509786252,
102.095384675183));
#226322=CARTESIAN_POINT('Ctrl Pts',(-5.55580380764055,5.63184472254529,
102.09648038816));
#226323=CARTESIAN_POINT('Ctrl Pts',(-5.86027209043677,5.32945720042755,
102.114249690311));
#226324=CARTESIAN_POINT('Ctrl Pts',(-6.12374840860168,5.0244940981396,102.132608310082));
#226325=CARTESIAN_POINT('Ctrl Pts',(-6.68695182748333,4.2621685154702,102.176815405996));
#226326=CARTESIAN_POINT('Ctrl Pts',(-6.96484615878175,3.79109631327008,
102.202805037158));
#226327=CARTESIAN_POINT('Ctrl Pts',(-7.35332848749448,2.94319135485258,
102.244701423262));
#226328=CARTESIAN_POINT('Ctrl Pts',(-7.48854966190747,2.5798251595956,102.261321006705));
#226329=CARTESIAN_POINT('Ctrl Pts',(-7.60270692669792,2.18706257386873,
102.277880734497));
#226330=CARTESIAN_POINT('Ctrl Pts',(-7.60869907336325,2.16612412768465,
102.278759559651));
#226331=CARTESIAN_POINT('Ctrl Pts',(-7.61719646555212,2.13596122620519,
102.280019879222));
#226332=CARTESIAN_POINT('Ctrl Pts',(-7.61977155152352,2.12675665230545,
102.280403722566));
#226333=CARTESIAN_POINT('Ctrl Pts',(-7.62421407805264,2.11076532061459,
102.281069272828));
#226334=CARTESIAN_POINT('Ctrl Pts',(-7.62608915083823,2.1039807058259,102.28135123569));
#226335=CARTESIAN_POINT('Ctrl Pts',(-7.62967866455126,2.09092485353419,
102.281893042218));
#226336=CARTESIAN_POINT('Ctrl Pts',(-7.63139443420316,2.08465398982704,
102.282152930205));
#226337=CARTESIAN_POINT('Ctrl Pts',(-7.63542025553442,2.06986868018247,
102.282764872836));
#226338=CARTESIAN_POINT('Ctrl Pts',(-7.63772380090847,2.06135246223299,
102.283116709702));
#226339=CARTESIAN_POINT('Ctrl Pts',(-7.64564752684936,2.031862782375,102.284332845349));
#226340=CARTESIAN_POINT('Ctrl Pts',(-7.6511956249906,2.01086995830706,102.2851947386));
#226341=CARTESIAN_POINT('Ctrl Pts',(-7.71375122810141,1.77016551230626,
102.295033894612));
#226342=CARTESIAN_POINT('Ctrl Pts',(-7.76136584925352,1.54811303075789,
102.303693074474));
#226343=CARTESIAN_POINT('Ctrl Pts',(-7.8121259399081,1.24916702187163,102.314913841405));
#226344=CARTESIAN_POINT('Ctrl Pts',(-7.82379824227897,1.17384467408581,
102.317704887032));
#226345=CARTESIAN_POINT('Ctrl Pts',(-7.83830899652329,1.07034280412142,
102.32149699441));
#226346=CARTESIAN_POINT('Ctrl Pts',(-7.84208721696192,1.04230021540008,
102.322520101876));
#226347=CARTESIAN_POINT('Ctrl Pts',(-7.88949208347646,0.675596217674615,
102.335845939355));
#226348=CARTESIAN_POINT('Ctrl Pts',(-7.91129923408663,0.33446853751554,
102.34763225072));
#226349=CARTESIAN_POINT('Ctrl Pts',(-7.9105135010674,-0.552979556538924,
102.378243440295));
#226350=CARTESIAN_POINT('Ctrl Pts',(-7.85351089883097,-1.0974420703393,
102.39697895592));
#226351=CARTESIAN_POINT('Ctrl Pts',(-7.73311163939765,-1.668631607545,102.420065163984));
#226352=CARTESIAN_POINT('Ctrl Pts',(-7.72505838799676,-1.7055262832714,
102.421570447011));
#226353=CARTESIAN_POINT('Ctrl Pts',(-7.71427584963855,-1.75328104778071,
102.423536066676));
#226354=CARTESIAN_POINT('Ctrl Pts',(-7.7117871457801,-1.76419537843943,
102.423986479541));
#226355=CARTESIAN_POINT('Ctrl Pts',(-7.70778755054815,-1.78156561397224,
102.424705148206));
#226356=CARTESIAN_POINT('Ctrl Pts',(-7.7062916890954,-1.78802498962012,
102.424972799758));
#226357=CARTESIAN_POINT('Ctrl Pts',(-7.70347037188664,-1.80013859373368,
102.425475491031));
#226358=CARTESIAN_POINT('Ctrl Pts',(-7.70214680622793,-1.80579326122002,
102.425710455827));
#226359=CARTESIAN_POINT('Ctrl Pts',(-7.69914628586926,-1.81854906648088,
102.426241176095));
#226360=CARTESIAN_POINT('Ctrl Pts',(-7.69746573235635,-1.82564934671549,
102.426537071923));
#226361=CARTESIAN_POINT('Ctrl Pts',(-7.69246899130551,-1.84663085199819,
102.427412855211));
#226362=CARTESIAN_POINT('Ctrl Pts',(-7.68912507009595,-1.86050539877712,
102.427993806308));
#226363=CARTESIAN_POINT('Ctrl Pts',(-7.66248115917167,-1.96975713953592,
102.43258236548));
#226364=CARTESIAN_POINT('Ctrl Pts',(-7.63744550460029,-2.06469996177659,
102.43665402664));
#226365=CARTESIAN_POINT('Ctrl Pts',(-7.54015105154648,-2.40764700267757,
102.451620788147));
#226366=CARTESIAN_POINT('Ctrl Pts',(-7.45752590461562,-2.65253475415538,
102.462800669732));
#226367=CARTESIAN_POINT('Ctrl Pts',(-7.15964538621602,-3.41069841602233,
102.498360784226));
#226368=CARTESIAN_POINT('Ctrl Pts',(-6.90215527302022,-3.90559883129204,
102.52287856345));
#226369=CARTESIAN_POINT('Ctrl Pts',(-6.4477167670995,-4.59149807003878,
102.557615149195));
#226370=CARTESIAN_POINT('Ctrl Pts',(-6.28943189325535,-4.80603398931511,
102.568630219762));
#226371=CARTESIAN_POINT('Ctrl Pts',(-6.09693839310463,-5.04109710498091,
102.580928359718));
#226372=CARTESIAN_POINT('Ctrl Pts',(-6.07305472440847,-5.06984458690464,
102.582436691265));
#226373=CARTESIAN_POINT('Ctrl Pts',(-6.03805953313594,-5.11136425810804,
102.584621508952));
#226374=CARTESIAN_POINT('Ctrl Pts',(-6.02710936711312,-5.1242716735365,
102.58530160994));
#226375=CARTESIAN_POINT('Ctrl Pts',(-6.00773710391849,-5.14695856355616,
102.586498576701));
#226376=CARTESIAN_POINT('Ctrl Pts',(-5.9993323533238,-5.15675274570047,
102.587015842585));
#226377=CARTESIAN_POINT('Ctrl Pts',(-5.98191918240937,-5.17694438367749,
102.58808331457));
#226378=CARTESIAN_POINT('Ctrl Pts',(-5.97290753010803,-5.1873389994071,
102.588633441824));
#226379=CARTESIAN_POINT('Ctrl Pts',(-5.94976870746713,-5.21388855685571,
102.590040082865));
#226380=CARTESIAN_POINT('Ctrl Pts',(-5.93560280761871,-5.2300096435207,
102.590895658928));
#226381=CARTESIAN_POINT('Ctrl Pts',(-5.87715900307138,-5.29597660193595,
102.594402651206));
#226382=CARTESIAN_POINT('Ctrl Pts',(-5.83231708253384,-5.34531979689645,
102.597040002323));
#226383=CARTESIAN_POINT('Ctrl Pts',(-5.53355388377572,-5.66583715557513,
102.614267865631));
#226384=CARTESIAN_POINT('Ctrl Pts',(-5.2614189859492,-5.91941065421507,
102.628324531081));
#226385=CARTESIAN_POINT('Ctrl Pts',(-4.42862584826985,-6.59242769396648,
102.667871738866));
#226386=CARTESIAN_POINT('Ctrl Pts',(-3.82900579519542,-6.95782357448853,
102.692098243892));
#226387=CARTESIAN_POINT('Ctrl Pts',(-3.16128979765534,-7.25197236569389,
102.721036984712));
#226388=CARTESIAN_POINT('Ctrl Pts',(-3.13323032448645,-7.26413959635661,
102.722257067898));
#226389=CARTESIAN_POINT('Ctrl Pts',(-3.09637381157708,-7.27986814847662,
102.723865709839));
#226390=CARTESIAN_POINT('Ctrl Pts',(-3.08763967894946,-7.28357688584858,
102.724247363525));
#226391=CARTESIAN_POINT('Ctrl Pts',(-3.07414708221909,-7.2892775586892,
102.724837659927));
#226392=CARTESIAN_POINT('Ctrl Pts',(-3.06939328761387,-7.29128057727119,
102.725045773201));
#226393=CARTESIAN_POINT('Ctrl Pts',(-3.0603934733858,-7.29506230135016,
102.725440034084));
#226394=CARTESIAN_POINT('Ctrl Pts',(-3.05614785268475,-7.29684195353759,
102.725626135838));
#226395=CARTESIAN_POINT('Ctrl Pts',(-3.04635696004198,-7.30093599331547,
102.726055568892));
#226396=CARTESIAN_POINT('Ctrl Pts',(-3.04081060417867,-7.30324776902099,
102.726299027341));
#226397=CARTESIAN_POINT('Ctrl Pts',(-3.02534208974715,-7.30967452233391,
102.72697857166));
#226398=CARTESIAN_POINT('Ctrl Pts',(-3.01541420219895,-7.3137756029198,
102.727415342708));
#226399=CARTESIAN_POINT('Ctrl Pts',(-2.95853363056975,-7.33713672102073,
102.729921536307));
#226400=CARTESIAN_POINT('Ctrl Pts',(-2.91140783761361,-7.3559636180685,
102.732013196208));
#226401=CARTESIAN_POINT('Ctrl Pts',(-2.77177352063081,-7.41019588857052,
102.738257830478));
#226402=CARTESIAN_POINT('Ctrl Pts',(-2.67878220428987,-7.44431703637101,
102.742474355842));
#226403=CARTESIAN_POINT('Ctrl Pts',(-2.48824741424025,-7.51019737599392,
102.751199157523));
#226404=CARTESIAN_POINT('Ctrl Pts',(-2.39067677561764,-7.54182360045362,
102.755711664976));
#226405=CARTESIAN_POINT('Ctrl Pts',(-1.91492511453467,-7.68587230974907,
102.777849352505));
#226406=CARTESIAN_POINT('Ctrl Pts',(-1.52931476610035,-7.77179216328433,
102.796177584676));
#226407=CARTESIAN_POINT('Ctrl Pts',(-0.72251106458374,-7.88916742361963,
102.833709107039));
#226408=CARTESIAN_POINT('Ctrl Pts',(-0.301906919710609,-7.91643153467123,
102.852816447499));
#226409=CARTESIAN_POINT('Ctrl Pts',(0.125923726172375,-7.91000086071323,
102.871329541374));
#226410=CARTESIAN_POINT('Ctrl Pts',(0.132951404656118,-7.90988586046578,
102.871633403476));
#226411=CARTESIAN_POINT('Ctrl Pts',(0.16882141587529,-7.90925106941212,
102.873183120322));
#226412=CARTESIAN_POINT('Ctrl Pts',(0.197661070810024,-7.90858288642949,
102.874425048364));
#226413=CARTESIAN_POINT('Ctrl Pts',(0.439437232381221,-7.90165785306008,
102.884802367676));
#226414=CARTESIAN_POINT('Ctrl Pts',(0.652053434278941,-7.88695994251887,
102.893701513969));
#226415=CARTESIAN_POINT('Ctrl Pts',(0.884524536447429,-7.86142295289256,
102.903187969697));
#226416=CARTESIAN_POINT('Ctrl Pts',(0.905211740432468,-7.85906776997854,
102.904030055333));
#226417=CARTESIAN_POINT('Ctrl Pts',(0.935922963434576,-7.85544850883296,
102.905277094851));
#226418=CARTESIAN_POINT('Ctrl Pts',(0.945954169452295,-7.85424686259701,
102.905683926892));
#226419=CARTESIAN_POINT('Ctrl Pts',(0.963125790518057,-7.85215648635099,
102.906379519066));
#226420=CARTESIAN_POINT('Ctrl Pts',(0.970267334577204,-7.85127722566981,
102.906668564181));
#226421=CARTESIAN_POINT('Ctrl Pts',(0.984160883865129,-7.84954741799592,
102.907230411359));
#226422=CARTESIAN_POINT('Ctrl Pts',(0.990913010292175,-7.84869789959059,
102.907503244188));
#226423=CARTESIAN_POINT('Ctrl Pts',(1.00706316344464,-7.84664479609154,
102.90815530043));
#226424=CARTESIAN_POINT('Ctrl Pts',(1.01646014983422,-7.84543303685376,
102.908534276978));
#226425=CARTESIAN_POINT('Ctrl Pts',(1.04463714455635,-7.84174808574261,
102.9096693829));
#226426=CARTESIAN_POINT('Ctrl Pts',(1.06341052847631,-7.83922431482134,
102.910423985417));
#226427=CARTESIAN_POINT('Ctrl Pts',(1.22748154563073,-7.81656745330419,
102.917004399839));
#226428=CARTESIAN_POINT('Ctrl Pts',(1.37220611662675,-7.79246371547353,
102.922708845393));
#226429=CARTESIAN_POINT('Ctrl Pts',(1.8317545964935,-7.70272548245994,102.940555523329));
#226430=CARTESIAN_POINT('Ctrl Pts',(2.1432894220011,-7.62191804575855,102.95223809563));
#226431=CARTESIAN_POINT('Ctrl Pts',(2.74573158978619,-7.42578107943707,
102.974626528167));
#226432=CARTESIAN_POINT('Ctrl Pts',(3.03643651033686,-7.31172507076696,
102.98533413929));
#226433=CARTESIAN_POINT('Ctrl Pts',(3.79388794695346,-6.96155922536145,
103.014160078732));
#226434=CARTESIAN_POINT('Ctrl Pts',(4.24524168261052,-6.69587950753181,
103.032342864703));
#226435=CARTESIAN_POINT('Ctrl Pts',(4.69483116159098,-6.36739048500372,
103.054361119655));
#226436=CARTESIAN_POINT('Ctrl Pts',(4.72243767803881,-6.34694285089252,
103.055728952403));
#226437=CARTESIAN_POINT('Ctrl Pts',(4.75854707536771,-6.31983127848204,
103.057538089855));
#226438=CARTESIAN_POINT('Ctrl Pts',(4.76717099645756,-6.31332862649009,
103.057971674058));
#226439=CARTESIAN_POINT('Ctrl Pts',(4.78109212463166,-6.30278696051444,
103.058674000708));
#226440=CARTESIAN_POINT('Ctrl Pts',(4.7863976112701,-6.29875886824868,103.058942233816));
#226441=CARTESIAN_POINT('Ctrl Pts',(4.7964444304158,-6.29111098369043,103.059451248374));
#226442=CARTESIAN_POINT('Ctrl Pts',(4.80118677099405,-6.28749251872111,
103.059691968893));
#226443=CARTESIAN_POINT('Ctrl Pts',(4.81195562227484,-6.27925646317358,
103.060239617743));
#226444=CARTESIAN_POINT('Ctrl Pts',(4.81797958298133,-6.27463555742869,
103.060546695806));
#226445=CARTESIAN_POINT('Ctrl Pts',(4.83582418240097,-6.26090633742654,
103.061458490809));
#226446=CARTESIAN_POINT('Ctrl Pts',(4.84762567761959,-6.25177326646535,
103.062064304693));
#226447=CARTESIAN_POINT('Ctrl Pts',(4.94317798467285,-6.17739296274878,
103.06699169395));
#226448=CARTESIAN_POINT('Ctrl Pts',(5.02563166480635,-6.11050061117071,
103.071383094474));
#226449=CARTESIAN_POINT('Ctrl Pts',(5.33688247869962,-5.84742945330845,
103.088435848353));
#226450=CARTESIAN_POINT('Ctrl Pts',(5.55574343514753,-5.639898290658,103.101430035675));
#226451=CARTESIAN_POINT('Ctrl Pts',(5.94368682903356,-5.22748967347134,
103.125889304387));
#226452=CARTESIAN_POINT('Ctrl Pts',(6.11534900139186,-5.02559165327295,
103.137335662844));
#226453=CARTESIAN_POINT('Ctrl Pts',(6.65909162905771,-4.31686756192522,
103.175527248456));
#226454=CARTESIAN_POINT('Ctrl Pts',(6.9808563308753,-3.77445905809207,103.20138271375));
#226455=CARTESIAN_POINT('Ctrl Pts',(7.27020421796336,-3.12019341722742,
103.230430669976));
#226456=CARTESIAN_POINT('Ctrl Pts',(7.30404812498197,-3.04012458097429,
103.233950380115));
#226457=CARTESIAN_POINT('Ctrl Pts',(7.34861079439945,-2.92965476510445,
103.238758389564));
#226458=CARTESIAN_POINT('Ctrl Pts',(7.3604733735777,-2.89972229282019,103.240056375177));
#226459=CARTESIAN_POINT('Ctrl Pts',(7.38051901876886,-2.84822609964404,
103.242281305089));
#226460=CARTESIAN_POINT('Ctrl Pts',(7.38879111212421,-2.82669750869779,
103.243209035795));
#226461=CARTESIAN_POINT('Ctrl Pts',(7.40565626201868,-2.78222511138245,
103.245120509821));
#226462=CARTESIAN_POINT('Ctrl Pts',(7.41423711864489,-2.75927693318314,
103.246104131693));
#226463=CARTESIAN_POINT('Ctrl Pts',(7.43402135517971,-2.70560838323863,
103.24839822615));
#226464=CARTESIAN_POINT('Ctrl Pts',(7.44514115552639,-2.67485764415331,
103.24970789585));
#226465=CARTESIAN_POINT('Ctrl Pts',(7.48064082204575,-2.57475018702315,
103.253956132854));
#226466=CARTESIAN_POINT('Ctrl Pts',(7.50424472473221,-2.50512212377008,
103.256887098778));
#226467=CARTESIAN_POINT('Ctrl Pts',(7.7042404958447,-1.88695577744984,103.282707785775));
#226468=CARTESIAN_POINT('Ctrl Pts',(7.82118269288217,-1.32099886795408,
103.304831832444));
#226469=CARTESIAN_POINT('Ctrl Pts',(7.904203045034,-0.446146461133101,103.338859961155));
#226470=CARTESIAN_POINT('Ctrl Pts',(7.91548219648333,-0.143540911452603,
103.350627064907));
#226471=CARTESIAN_POINT('Ctrl Pts',(7.908864396144,0.185750328063237,103.363805937198));
#226472=CARTESIAN_POINT('Ctrl Pts',(7.9081897613279,0.212541544195681,103.36488092154));
#226473=CARTESIAN_POINT('Ctrl Pts',(7.90698389329729,0.25238321569165,103.366484036457));
#226474=CARTESIAN_POINT('Ctrl Pts',(7.90655645220347,0.265436702617317,
103.367009988176));
#226475=CARTESIAN_POINT('Ctrl Pts',(7.90573637282956,0.288718145752481,
103.367949379758));
#226476=CARTESIAN_POINT('Ctrl Pts',(7.90535620580901,0.298946521843469,
103.368362547875));
#226477=CARTESIAN_POINT('Ctrl Pts',(7.90452502957055,0.320198015622069,
103.369221973725));
#226478=CARTESIAN_POINT('Ctrl Pts',(7.90407081016079,0.331220982650436,
103.369668302186));
#226479=CARTESIAN_POINT('Ctrl Pts',(7.90283056328759,0.35986264610135,103.370829508655));
#226480=CARTESIAN_POINT('Ctrl Pts',(7.90200868009032,0.377479605379283,
103.37154522002));
#226481=CARTESIAN_POINT('Ctrl Pts',(7.89760783332676,0.465488226258899,
103.375128140699));
#226482=CARTESIAN_POINT('Ctrl Pts',(7.89314720800499,0.535831792455592,
103.3780154227));
#226483=CARTESIAN_POINT('Ctrl Pts',(7.83444006368487,1.29983590891204,103.409589995928));
#226484=CARTESIAN_POINT('Ctrl Pts',(7.68984714882252,1.98351866001974,103.4394810665));
#226485=CARTESIAN_POINT('Ctrl Pts',(7.40537194881248,2.78728781814451,103.474607160953));
#226486=CARTESIAN_POINT('Ctrl Pts',(7.34867270343761,2.93351631877009,103.481012144068));
#226487=CARTESIAN_POINT('Ctrl Pts',(7.27223360981663,3.11450032075621,103.48896782148));
#226488=CARTESIAN_POINT('Ctrl Pts',(7.25652831350302,3.15091903765182,103.490570228675));
#226489=CARTESIAN_POINT('Ctrl Pts',(7.2312306852643,3.20838881916228,103.493101647804));
#226490=CARTESIAN_POINT('Ctrl Pts',(7.22181878324293,3.22951846331162,103.494032961595));
#226491=CARTESIAN_POINT('Ctrl Pts',(7.20411082473884,3.26880816513423,103.495765916297));
#226492=CARTESIAN_POINT('Ctrl Pts',(7.19583843590211,3.28697867391424,103.496567851599));
#226493=CARTESIAN_POINT('Ctrl Pts',(7.17729775115692,3.32729830369259,103.498348478842));
#226494=CARTESIAN_POINT('Ctrl Pts',(7.16699552563286,3.34943161612485,103.499326732497));
#226495=CARTESIAN_POINT('Ctrl Pts',(7.13662992162976,3.41388753089522,103.502178076006));
#226496=CARTESIAN_POINT('Ctrl Pts',(7.11629289081814,3.45608018395123,103.504047718402));
#226497=CARTESIAN_POINT('Ctrl Pts',(6.93719760317999,3.81935996949329,103.520177726733));
#226498=CARTESIAN_POINT('Ctrl Pts',(6.75717207857305,4.129510274642,103.534193049738));
#226499=CARTESIAN_POINT('Ctrl Pts',(6.35956145314151,4.7184849148636,103.561776832244));
#226500=CARTESIAN_POINT('Ctrl Pts',(6.14307256667544,4.99707831118731,103.575232829187));
#226501=CARTESIAN_POINT('Ctrl Pts',(5.59679641021371,5.61069116482583,103.606197225456));
#226502=CARTESIAN_POINT('Ctrl Pts',(5.25432973085988,5.93262048307298,103.623481171852));
#226503=CARTESIAN_POINT('Ctrl Pts',(4.71425526879374,6.35665394662141,103.649616406839));
#226504=CARTESIAN_POINT('Ctrl Pts',(4.53767483433895,6.4838840279869,103.65802161916));
#226505=CARTESIAN_POINT('Ctrl Pts',(4.33918359116201,6.61481796087853,103.667514113218));
#226506=CARTESIAN_POINT('Ctrl Pts',(4.32224083443446,6.62590107491069,103.668324733923));
#226507=CARTESIAN_POINT('Ctrl Pts',(4.29754825961059,6.6419187257959,103.669506893814));
#226508=CARTESIAN_POINT('Ctrl Pts',(4.28983202950851,6.64690503629937,103.669876415455));
#226509=CARTESIAN_POINT('Ctrl Pts',(4.27642493363103,6.65553577518509,103.670518675778));
#226510=CARTESIAN_POINT('Ctrl Pts',(4.27073804346122,6.65918637909803,103.670791168682));
#226511=CARTESIAN_POINT('Ctrl Pts',(4.25974931508833,6.6662205432022,103.671317841451));
#226512=CARTESIAN_POINT('Ctrl Pts',(4.25444810441001,6.6696050771112,103.671571981747));
#226513=CARTESIAN_POINT('Ctrl Pts',(4.24075718700752,6.67832301654717,103.672228495657));
#226514=CARTESIAN_POINT('Ctrl Pts',(4.2323614664137,6.68364692731906,103.672631256667));
#226515=CARTESIAN_POINT('Ctrl Pts',(4.20290690172965,6.70224695950866,103.67404489975));
#226516=CARTESIAN_POINT('Ctrl Pts',(4.181795570517,6.71543941375966,103.675059267274));
#226517=CARTESIAN_POINT('Ctrl Pts',(3.89647060903419,6.89187157801256,103.688788146536));
#226518=CARTESIAN_POINT('Ctrl Pts',(3.62298749997597,7.03947928388921,103.702319116291));
#226519=CARTESIAN_POINT('Ctrl Pts',(2.65082037431713,7.49251929629156,103.750547533893));
#226520=CARTESIAN_POINT('Ctrl Pts',(1.91701530476906,7.71297932275493,103.786442346441));
#226521=CARTESIAN_POINT('Ctrl Pts',(0.978372810038053,7.85248706292999,
103.826875259803));
#226522=CARTESIAN_POINT('Ctrl Pts',(0.792811334313815,7.87338699311333,
103.834639802152));
#226523=CARTESIAN_POINT('Ctrl Pts',(0.585031038117041,7.88936822143292,
103.843080299582));
#226524=CARTESIAN_POINT('Ctrl Pts',(0.563379827306682,7.89094388706255,
103.843956782869));
#226525=CARTESIAN_POINT('Ctrl Pts',(0.532928486811197,7.89303401255125,
103.845185274643));
#226526=CARTESIAN_POINT('Ctrl Pts',(0.524133660699422,7.89362290723916,
103.845539585659));
#226527=CARTESIAN_POINT('Ctrl Pts',(0.5079917610494,7.89467665998413,103.846188974694));
#226528=CARTESIAN_POINT('Ctrl Pts',(0.500644992513982,7.89514596361971,
103.84648419015));
#226529=CARTESIAN_POINT('Ctrl Pts',(0.485749697261641,7.896076584249,103.847082030624));
#226530=CARTESIAN_POINT('Ctrl Pts',(0.478201142059657,7.89653733359465,
103.847384637752));
#226531=CARTESIAN_POINT('Ctrl Pts',(0.459607071743803,7.89764552013317,
103.848129147004));
#226532=CARTESIAN_POINT('Ctrl Pts',(0.448560822010508,7.89828061113949,
103.84857066579));
#226533=CARTESIAN_POINT('Ctrl Pts',(0.408231545195871,7.90051441705673,
103.850179814796));
#226534=CARTESIAN_POINT('Ctrl Pts',(0.378940856210546,7.90197348132454,
103.85134310757));
#226535=CARTESIAN_POINT('Ctrl Pts',(-0.0401653747111206,7.92051484063087,
103.867911896506));
#226536=CARTESIAN_POINT('Ctrl Pts',(-0.430730966989419,7.90889891653234,
103.88237186308));
#226537=CARTESIAN_POINT('Ctrl Pts',(-0.923458946856395,7.85762051124463,
103.899938980386));
#226538=CARTESIAN_POINT('Ctrl Pts',(-1.02781323110723,7.84465276764938,
103.903623191188));
#226539=CARTESIAN_POINT('Ctrl Pts',(-1.2132892001396,7.81783962422734,103.910131911088));
#226540=CARTESIAN_POINT('Ctrl Pts',(-1.29451108939239,7.8048016182882,103.912968601785));
#226541=CARTESIAN_POINT('Ctrl Pts',(-1.44239887394455,7.77869007864867,
103.91812294844));
#226542=CARTESIAN_POINT('Ctrl Pts',(-1.50912769967523,7.76602005559466,
103.92044467713));
#226543=CARTESIAN_POINT('Ctrl Pts',(-1.63230384283162,7.74098464326481,
103.924731817012));
#226544=CARTESIAN_POINT('Ctrl Pts',(-1.68879467670604,7.72885707215091,
103.926698537813));
#226545=CARTESIAN_POINT('Ctrl Pts',(-1.79400936284059,7.70506073934629,
103.930368439178));
#226546=CARTESIAN_POINT('Ctrl Pts',(-1.84276499066233,7.69354585219021,
103.932071816118));
#226547=CARTESIAN_POINT('Ctrl Pts',(-1.93416419386295,7.67104092030055,
103.935274266467));
#226548=CARTESIAN_POINT('Ctrl Pts',(-1.97683175220599,7.66015640472539,
103.936773061735));
#226549=CARTESIAN_POINT('Ctrl Pts',(-2.14751771150057,7.61509325243354,
103.942790127807));
#226550=CARTESIAN_POINT('Ctrl Pts',(-2.27475806731773,7.57805731037085,
103.947323645382));
#226551=CARTESIAN_POINT('Ctrl Pts',(-2.68330630466245,7.44792366549738,
103.962177800813));
#226552=CARTESIAN_POINT('Ctrl Pts',(-2.96031438222329,7.34222143500387,
103.972709714878));
#226553=CARTESIAN_POINT('Ctrl Pts',(-3.25409758198842,7.21078537508867,
103.984975951814));
#226554=CARTESIAN_POINT('Ctrl Pts',(-3.27742222932424,7.2002139070118,103.985957574412));
#226555=CARTESIAN_POINT('Ctrl Pts',(-3.34711747620623,7.16821699409926,
103.988915077347));
#226556=CARTESIAN_POINT('Ctrl Pts',(-3.39333162759222,7.14645580274434,
103.990908608273));
#226557=CARTESIAN_POINT('Ctrl Pts',(-3.46864176616134,7.11009877944754,
103.99421532469));
#226558=CARTESIAN_POINT('Ctrl Pts',(-3.49786462754324,7.0957679884593,103.995512912344));
#226559=CARTESIAN_POINT('Ctrl Pts',(-3.53362680915434,7.07795573724664,
103.997119598829));
#226560=CARTESIAN_POINT('Ctrl Pts',(-3.54025112943678,7.07464471084221,
103.997418001981));
#226561=CARTESIAN_POINT('Ctrl Pts',(-3.55119766647502,7.06915409125499,
103.997912432289));
#226562=CARTESIAN_POINT('Ctrl Pts',(-3.55552256001436,7.06697981865559,
103.998108120774));
#226563=CARTESIAN_POINT('Ctrl Pts',(-3.56312740649478,7.06314785284663,
103.998452825005));
#226564=CARTESIAN_POINT('Ctrl Pts',(-3.56640820895334,7.06149183905997,
103.99860173286));
#226565=CARTESIAN_POINT('Ctrl Pts',(-3.57350893888364,7.05790147262813,
103.998924451936));
#226566=CARTESIAN_POINT('Ctrl Pts',(-3.57732845022648,7.05596630467197,
103.99909831588));
#226567=CARTESIAN_POINT('Ctrl Pts',(-3.58739002597015,7.0508583046246,103.99955703995));
#226568=CARTESIAN_POINT('Ctrl Pts',(-3.59362943974904,7.04768029066821,
103.99984223795));
#226569=CARTESIAN_POINT('Ctrl Pts',(-3.62208534656855,7.03313880455226,
104.001146311763));
#226570=CARTESIAN_POINT('Ctrl Pts',(-3.64425179495893,7.02167875301273,
104.002171608329));
#226571=CARTESIAN_POINT('Ctrl Pts',(-3.70334879541277,6.99077040190886,
104.004929604827));
#226572=CARTESIAN_POINT('Ctrl Pts',(-3.74018001223325,6.97113451782528,
104.006674177917));
#226573=CARTESIAN_POINT('Ctrl Pts',(-3.84072335425268,6.9165055318967,104.011503236261));
#226574=CARTESIAN_POINT('Ctrl Pts',(-3.90411022455767,6.88092489660138,
104.014621724334));
#226575=CARTESIAN_POINT('Ctrl Pts',(-4.09343632235216,6.77119322754072,
104.024137582085));
#226576=CARTESIAN_POINT('Ctrl Pts',(-4.21781684708899,6.6944227706998,104.030661433935));
#226577=CARTESIAN_POINT('Ctrl Pts',(-5.12587168843778,6.09859560842986,
104.07991183628));
#226578=CARTESIAN_POINT('Ctrl Pts',(-5.81390203939381,5.44673491787291,
104.125124322255));
#226579=CARTESIAN_POINT('Ctrl Pts',(-6.40335301967687,4.64584796381104,
104.165842123544));
#226580=CARTESIAN_POINT('Ctrl Pts',(-6.43489595765177,4.60205903639653,
104.168033205165));
#226581=CARTESIAN_POINT('Ctrl Pts',(-6.47315525012999,4.54778372633621,
104.170706433047));
#226582=CARTESIAN_POINT('Ctrl Pts',(-6.48029771376349,4.53760038531198,
104.171206170787));
#226583=CARTESIAN_POINT('Ctrl Pts',(-6.49209008166837,4.5207028294275,104.172032395572));
#226584=CARTESIAN_POINT('Ctrl Pts',(-6.49675364533883,4.51399820257221,
104.172359444604));
#226585=CARTESIAN_POINT('Ctrl Pts',(-6.50517531338007,4.50185060736039,
104.172950590257));
#226586=CARTESIAN_POINT('Ctrl Pts',(-6.50893698651854,4.4964101297176,104.173214833315));
#226587=CARTESIAN_POINT('Ctrl Pts',(-6.51698421277751,4.48474023124861,
104.17378054792));
#226588=CARTESIAN_POINT('Ctrl Pts',(-6.52126766888685,4.47850936836607,
104.17408193342));
#226589=CARTESIAN_POINT('Ctrl Pts',(-6.53287199665189,4.46157736505054,
104.174899133248));
#226590=CARTESIAN_POINT('Ctrl Pts',(-6.54017551962917,4.45086432995026,
104.17541423807));
#226591=CARTESIAN_POINT('Ctrl Pts',(-6.57664940707072,4.397079672211,104.177990622748));
#226592=CARTESIAN_POINT('Ctrl Pts',(-6.60542110872749,4.35373852958503,
104.180035654169));
#226593=CARTESIAN_POINT('Ctrl Pts',(-6.9312629576137,3.85223051579598,104.203351103466));
#226594=CARTESIAN_POINT('Ctrl Pts',(-7.1805725468827,3.3647499328151,104.222545757408));
#226595=CARTESIAN_POINT('Ctrl Pts',(-7.54437659947113,2.42478078451246,
104.256786922232));
#226596=CARTESIAN_POINT('Ctrl Pts',(-7.67302194342936,1.98037085670152,
104.27199968181));
#226597=CARTESIAN_POINT('Ctrl Pts',(-7.7669124643957,1.50319515790408,104.28941954837));
#226598=CARTESIAN_POINT('Ctrl Pts',(-7.77154446621564,1.47906102237896,
104.29030360783));
#226599=CARTESIAN_POINT('Ctrl Pts',(-7.81508163153357,1.24636707679826,
104.298859770764));
#226600=CARTESIAN_POINT('Ctrl Pts',(-7.84569187805009,1.03635781168871,
104.306830807747));
#226601=CARTESIAN_POINT('Ctrl Pts',(-7.86921209141696,0.812157052864072,
104.315847017301));
#226602=CARTESIAN_POINT('Ctrl Pts',(-7.8705668494434,0.798921449377772,
104.316381155163));
#226603=CARTESIAN_POINT('Ctrl Pts',(-7.87238258706678,0.780729263276773,
104.317117968936));
#226604=CARTESIAN_POINT('Ctrl Pts',(-7.87287229392831,0.775775497938781,
104.317318874509));
#226605=CARTESIAN_POINT('Ctrl Pts',(-7.87370349478392,0.767285408646501,
104.317663666046));
#226606=CARTESIAN_POINT('Ctrl Pts',(-7.87404728115733,0.763749328058591,
104.317807408258));
#226607=CARTESIAN_POINT('Ctrl Pts',(-7.87473315746019,0.756644929113058,
104.318096479118));
#226608=CARTESIAN_POINT('Ctrl Pts',(-7.87507520427521,0.753076607575596,
104.318241810375));
#226609=CARTESIAN_POINT('Ctrl Pts',(-7.87576040850192,0.745876861759802,
104.318535323293));
#226610=CARTESIAN_POINT('Ctrl Pts',(-7.87610347990846,0.742245430244154,
104.31868351017));
#226611=CARTESIAN_POINT('Ctrl Pts',(-7.87688444354181,0.733917374887801,
104.319023678722));
#226612=CARTESIAN_POINT('Ctrl Pts',(-7.87732064658357,0.72922059816389,
104.319215762732));
#226613=CARTESIAN_POINT('Ctrl Pts',(-7.8784277896093,0.71718261793078,104.319708687229));
#226614=CARTESIAN_POINT('Ctrl Pts',(-7.87909266814807,0.709840876216685,
104.320009891584));
#226615=CARTESIAN_POINT('Ctrl Pts',(-7.88442274332827,0.650054754388907,
104.32246734418));
#226616=CARTESIAN_POINT('Ctrl Pts',(-7.88857442631856,0.59756710309949,
104.324653929315));
#226617=CARTESIAN_POINT('Ctrl Pts',(-7.90468572739658,0.364276148668387,
104.334489649893));
#226618=CARTESIAN_POINT('Ctrl Pts',(-7.91095452025883,0.183146265022534,
104.34243748295));
#226619=CARTESIAN_POINT('Ctrl Pts',(-7.91099975343153,0.00197514715529489,
104.350590048145));
#226620=CARTESIAN_POINT('',(-7.91212843677151,0.00142906907571687,106.355715790758));
#226621=CARTESIAN_POINT('Ctrl Pts',(-7.91099966760513,0.0022932840043321,
104.357668491763));
#226622=CARTESIAN_POINT('Ctrl Pts',(-7.91105540365936,-0.189975927168933,
104.365452204501));
#226623=CARTESIAN_POINT('Ctrl Pts',(-7.90409755832876,-0.382548785251838,
104.373235917239));
#226624=CARTESIAN_POINT('Ctrl Pts',(-7.89008583166137,-0.574862217419591,
104.381019629977));
#226625=CARTESIAN_POINT('Ctrl Pts',(-7.87608942923311,-0.766965321688851,
104.388794829884));
#226626=CARTESIAN_POINT('Ctrl Pts',(-7.85505452960641,-0.958809212370408,
104.39657002979));
#226627=CARTESIAN_POINT('Ctrl Pts',(-7.82699276817718,-1.1498283380149,
104.404345229696));
#226628=CARTESIAN_POINT('Ctrl Pts',(-7.79895606160157,-1.34067691284624,
104.41211348754));
#226629=CARTESIAN_POINT('Ctrl Pts',(-7.76390503675182,-1.53070183793467,
104.419881745383));
#226630=CARTESIAN_POINT('Ctrl Pts',(-7.72190330477566,-1.71934009192329,
104.427650003227));
#226631=CARTESIAN_POINT('Ctrl Pts',(-7.6799306472337,-1.90784776676084,
104.435412883729));
#226632=CARTESIAN_POINT('Ctrl Pts',(-7.63101694138477,-2.09497033484641,
104.44317576423));
#226633=CARTESIAN_POINT('Ctrl Pts',(-7.57527732234824,-2.28015229524619,
104.450938644731));
#226634=CARTESIAN_POINT('Ctrl Pts',(-7.5174414684052,-2.47229851008754,
104.458993468761));
#226635=CARTESIAN_POINT('Ctrl Pts',(-7.45225636839487,-2.66235493024437,
104.467048292791));
#226636=CARTESIAN_POINT('Ctrl Pts',(-7.37990848984268,-2.84971431577762,
104.475103116821));
#226637=CARTESIAN_POINT('Ctrl Pts',(-7.31022957258088,-3.03016188914186,
104.482860793043));
#226638=CARTESIAN_POINT('Ctrl Pts',(-7.23390704747383,-3.2081074994048,
104.490618469265));
#226639=CARTESIAN_POINT('Ctrl Pts',(-7.15115772006215,-3.38302590335864,
104.498376145487));
#226640=CARTESIAN_POINT('Ctrl Pts',(-7.06841177366112,-3.55793716041467,
104.506133504743));
#226641=CARTESIAN_POINT('Ctrl Pts',(-6.97923970021827,-3.72982113424552,
104.513890863998));
#226642=CARTESIAN_POINT('Ctrl Pts',(-6.88390556306171,-3.89817459830215,
104.521648223253));
#226643=CARTESIAN_POINT('Ctrl Pts',(-6.78855801588808,-4.06655174351742,
104.529406673684));
#226644=CARTESIAN_POINT('Ctrl Pts',(-6.68704685527186,-4.23139707923972,
104.537165124115));
#226645=CARTESIAN_POINT('Ctrl Pts',(-6.57968104908572,-4.39223386129453,
104.544923574547));
#226646=CARTESIAN_POINT('Ctrl Pts',(-6.47228064805728,-4.55312246732672,
104.552684524865));
#226647=CARTESIAN_POINT('Ctrl Pts',(-6.35902204361093,-4.70999965104927,
104.560445475183));
#226648=CARTESIAN_POINT('Ctrl Pts',(-6.24025632262631,-4.862419359529,104.568206425501));
#226649=CARTESIAN_POINT('Ctrl Pts',(-6.12137695518243,-5.01498491783851,
104.575974802242));
#226650=CARTESIAN_POINT('Ctrl Pts',(-5.99698016904949,-5.16308420280908,
104.583743178984));
#226651=CARTESIAN_POINT('Ctrl Pts',(-5.86745651897299,-5.3063052115348,
104.591511555725));
#226652=CARTESIAN_POINT('Ctrl Pts',(-5.73785926939866,-5.44960760303745,
104.599284346708));
#226653=CARTESIAN_POINT('Ctrl Pts',(-5.60312960014719,-5.58802594057014,
104.60705713769));
#226654=CARTESIAN_POINT('Ctrl Pts',(-5.46369334513455,-5.721186592861,104.614829928673));
#226655=CARTESIAN_POINT('Ctrl Pts',(-5.32409135039537,-5.85450552543623,
104.622611958718));
#226656=CARTESIAN_POINT('Ctrl Pts',(-5.17977186798612,-5.98255406145579,
104.630393988763));
#226657=CARTESIAN_POINT('Ctrl Pts',(-5.03119268895238,-6.10499968277085,
104.638176018807));
#226658=CARTESIAN_POINT('Ctrl Pts',(-4.99250852085789,-6.13687970141269,
104.640202153023));
#226659=CARTESIAN_POINT('Ctrl Pts',(-4.9535357447777,-6.16838014373279,
104.642228287239));
#226660=CARTESIAN_POINT('Ctrl Pts',(-4.91428273928625,-6.19949563741706,
104.644254421454));
#226661=CARTESIAN_POINT('Ctrl Pts',(-4.74779344431759,-6.33147015863494,
104.652848149574));
#226662=CARTESIAN_POINT('Ctrl Pts',(-4.57588316661556,-6.4568154454824,
104.661441877694));
#226663=CARTESIAN_POINT('Ctrl Pts',(-4.39908100386116,-6.57510511866296,
104.670035605814));
#226664=CARTESIAN_POINT('Ctrl Pts',(-4.2225341128925,-6.69322400198644,
104.678616926074));
#226665=CARTESIAN_POINT('Ctrl Pts',(-4.0411096380926,-6.80430746372126,
104.687198246335));
#226666=CARTESIAN_POINT('Ctrl Pts',(-3.8553676831306,-6.90797083287648,
104.695779566596));
#226667=CARTESIAN_POINT('Ctrl Pts',(-3.6615929796295,-7.01611731290082,
104.704732001653));
#226668=CARTESIAN_POINT('Ctrl Pts',(-3.46311926290425,-7.11618749880798,
104.713684436709));
#226669=CARTESIAN_POINT('Ctrl Pts',(-3.26061784832021,-7.20779385437844,
104.722636871766));
#226670=CARTESIAN_POINT('Ctrl Pts',(-3.06727569377342,-7.29525679972406,
104.731184382834));
#226671=CARTESIAN_POINT('Ctrl Pts',(-2.87026238401813,-7.3750044417643,
104.739731893902));
#226672=CARTESIAN_POINT('Ctrl Pts',(-2.67018989329174,-7.44674472059857,
104.748279404969));
#226673=CARTESIAN_POINT('Ctrl Pts',(-2.47042499767427,-7.51837470461518,
104.756813774937));
#226674=CARTESIAN_POINT('Ctrl Pts',(-2.26761053651013,-7.58202180048187,
104.765348144904));
#226675=CARTESIAN_POINT('Ctrl Pts',(-2.06237947018481,-7.63744145122961,
104.773882514872));
#226676=CARTESIAN_POINT('Ctrl Pts',(-1.85759523883733,-7.69274044072047,
104.782398303564));
#226677=CARTESIAN_POINT('Ctrl Pts',(-1.65040514059566,-7.73984766417033,
104.790914092256));
#226678=CARTESIAN_POINT('Ctrl Pts',(-1.44145841140395,-7.77856790471053,
104.799429880948));
#226679=CARTESIAN_POINT('Ctrl Pts',(-1.41055150242955,-7.7842953116648,
104.800689516392));
#226680=CARTESIAN_POINT('Ctrl Pts',(-1.37960619187283,-7.78983930151628,
104.801949151836));
#226681=CARTESIAN_POINT('Ctrl Pts',(-1.34862461415533,-7.79519933357027,
104.803208787279));
#226682=CARTESIAN_POINT('Ctrl Pts',(-1.1544530700158,-7.82879238393236,
104.811103329042));
#226683=CARTESIAN_POINT('Ctrl Pts',(-0.959035595012537,-7.85512446690431,
104.818997870805));
#226684=CARTESIAN_POINT('Ctrl Pts',(-0.762954745848102,-7.87412351032087,
104.826892412568));
#226685=CARTESIAN_POINT('Ctrl Pts',(-0.5668297083475,-7.89312683531883,
104.834788733427));
#226686=CARTESIAN_POINT('Ctrl Pts',(-0.370041339620588,-7.90479379417677,
104.842685054285));
#226687=CARTESIAN_POINT('Ctrl Pts',(-0.173176053447485,-7.90910431430212,
104.850581375144));
#226688=CARTESIAN_POINT('Ctrl Pts',(0.0237660536522444,-7.91341651648201,
104.858480777312));
#226689=CARTESIAN_POINT('Ctrl Pts',(0.220784795879588,-7.91036655159211,
104.866380179479));
#226690=CARTESIAN_POINT('Ctrl Pts',(0.417294745685731,-7.89998646171138,
104.874279581647));
#226691=CARTESIAN_POINT('Ctrl Pts',(0.614020932190244,-7.88959494973032,
104.882187676201));
#226692=CARTESIAN_POINT('Ctrl Pts',(0.810236865532022,-7.87185721642027,
104.890095770756));
#226693=CARTESIAN_POINT('Ctrl Pts',(1.00536199019258,-7.84685722239649,
104.898003865311));
#226694=CARTESIAN_POINT('Ctrl Pts',(1.200603367283,-7.82184233377595,104.905916671383));
#226695=CARTESIAN_POINT('Ctrl Pts',(1.39475230272953,-7.78955661321012,
104.913829477454));
#226696=CARTESIAN_POINT('Ctrl Pts',(1.5872390708678,-7.75013503959194,104.921742283525));
#226697=CARTESIAN_POINT('Ctrl Pts',(1.77999557725638,-7.71065822318281,
104.92966617808));
#226698=CARTESIAN_POINT('Ctrl Pts',(1.97108492994987,-7.66402565369724,
104.937590072636));
#226699=CARTESIAN_POINT('Ctrl Pts',(2.15995184656808,-7.61042239435546,
104.945513967191));
#226700=CARTESIAN_POINT('Ctrl Pts',(2.29223025190917,-7.57287980196408,
104.951063695829));
#226701=CARTESIAN_POINT('Ctrl Pts',(2.423418832233,-7.53191891169716,104.956613424467));
#226702=CARTESIAN_POINT('Ctrl Pts',(2.55333299200044,-7.48761721991463,
104.962163153104));
#226703=CARTESIAN_POINT('Ctrl Pts',(2.74352007348458,-7.4227620149084,104.970287646189));
#226704=CARTESIAN_POINT('Ctrl Pts',(2.93139354558582,-7.35060237745438,
104.978412139274));
#226705=CARTESIAN_POINT('Ctrl Pts',(3.11637262500933,-7.27132330886837,
104.986536632358));
#226706=CARTESIAN_POINT('Ctrl Pts',(3.3011882759034,-7.19211428313064,104.994653947475));
#226707=CARTESIAN_POINT('Ctrl Pts',(3.48311433912189,-7.10579849261481,
105.002771262591));
#226708=CARTESIAN_POINT('Ctrl Pts',(3.66158736575237,-7.0126099964965,105.010888577708));
#226709=CARTESIAN_POINT('Ctrl Pts',(3.83992812372441,-6.91949056357275,
105.018999876977));
#226710=CARTESIAN_POINT('Ctrl Pts',(4.01482066445471,-6.81950872892337,
105.027111176247));
#226711=CARTESIAN_POINT('Ctrl Pts',(4.18572310027882,-6.71294593511614,
105.035222475517));
#226712=CARTESIAN_POINT('Ctrl Pts',(4.35652317963895,-6.60644696363369,
105.043328916787));
#226713=CARTESIAN_POINT('Ctrl Pts',(4.52333764808086,-6.49337506201214,
105.051435358057));
#226714=CARTESIAN_POINT('Ctrl Pts',(4.68565024125884,-6.37405701391123,
105.059541799328));
#226715=CARTESIAN_POINT('Ctrl Pts',(4.84788867754221,-6.25479347948512,
105.067644536951));
#226716=CARTESIAN_POINT('Ctrl Pts',(5.00562908260075,-6.12928967956017,
105.075747274575));
#226717=CARTESIAN_POINT('Ctrl Pts',(5.1583846807232,-5.99791534499115,105.083850012199));
#226718=CARTESIAN_POINT('Ctrl Pts',(5.31251977523874,-5.86535460270345,
105.092025923555));
#226719=CARTESIAN_POINT('Ctrl Pts',(5.46157931214299,-5.72681695804001,
105.100201834912));
#226720=CARTESIAN_POINT('Ctrl Pts',(5.605096967992,-5.58272415397778,105.108377746268));
#226721=CARTESIAN_POINT('Ctrl Pts',(5.74727592966195,-5.4399754089228,105.116477394917));
#226722=CARTESIAN_POINT('Ctrl Pts',(5.88401573682601,-5.29177493899788,
105.124577043567));
#226723=CARTESIAN_POINT('Ctrl Pts',(6.01489947357244,-5.13857035787368,
105.132676692216));
#226724=CARTESIAN_POINT('Ctrl Pts',(6.14578232084147,-4.98536681791789,
105.140776285821));
#226725=CARTESIAN_POINT('Ctrl Pts',(6.2708089688368,-4.82715947850089,105.148875879426));
#226726=CARTESIAN_POINT('Ctrl Pts',(6.38960213034008,-4.66442982753021,
105.15697547303));
#226727=CARTESIAN_POINT('Ctrl Pts',(6.50840982167866,-4.50168027276208,
105.165076057313));
#226728=CARTESIAN_POINT('Ctrl Pts',(6.62098231733734,-4.33440756265213,
105.173176641596));
#226729=CARTESIAN_POINT('Ctrl Pts',(6.72698477035619,-4.16312345473875,
105.181277225878));
#226730=CARTESIAN_POINT('Ctrl Pts',(6.83471852367279,-3.9890418245173,105.189510114118));
#226731=CARTESIAN_POINT('Ctrl Pts',(6.93566557619923,-3.81081691551062,
105.197743002358));
#226732=CARTESIAN_POINT('Ctrl Pts',(7.02952218148843,-3.62901348853406,
105.205975890597));
#226733=CARTESIAN_POINT('Ctrl Pts',(7.12195867872563,-3.44996085900788,
105.214084210184));
#226734=CARTESIAN_POINT('Ctrl Pts',(7.20751766270693,-3.26743754053747,
105.222192529771));
#226735=CARTESIAN_POINT('Ctrl Pts',(7.28595679560303,-3.08200495986072,
105.230300849357));
#226736=CARTESIAN_POINT('Ctrl Pts',(7.36620352691879,-2.89229915958795,
105.238596021923));
#226737=CARTESIAN_POINT('Ctrl Pts',(7.43899817239824,-2.69954872770601,
105.246891194489));
#226738=CARTESIAN_POINT('Ctrl Pts',(7.50413451096247,-2.50437342291082,
105.255186367055));
#226739=CARTESIAN_POINT('Ctrl Pts',(7.5692708495267,-2.30919811811563,105.263481539621));
#226740=CARTESIAN_POINT('Ctrl Pts',(7.6267488071954,-2.11159829106925,105.271776712187));
#226741=CARTESIAN_POINT('Ctrl Pts',(7.67641739374365,-1.91220736245574,
105.280071884753));
#226742=CARTESIAN_POINT('Ctrl Pts',(7.72328866953158,-1.72404603445868,
105.287899877215));
#226743=CARTESIAN_POINT('Ctrl Pts',(7.76329520909628,-1.53392888232882,
105.295727869676));
#226744=CARTESIAN_POINT('Ctrl Pts',(7.79627299009179,-1.34240398687027,
105.303555862137));
#226745=CARTESIAN_POINT('Ctrl Pts',(7.82922291749054,-1.15104085660777,
105.311377242942));
#226746=CARTESIAN_POINT('Ctrl Pts',(7.85515584751052,-0.958272695125778,
105.319198623747));
#226747=CARTESIAN_POINT('Ctrl Pts',(7.87395798253529,-0.76466115977527,
105.327020004552));
#226748=CARTESIAN_POINT('Ctrl Pts',(7.89274755730638,-0.571178961332209,
105.334836160496));
#226749=CARTESIAN_POINT('Ctrl Pts',(7.90441578986685,-0.376854860062968,
105.342652316441));
#226750=CARTESIAN_POINT('Ctrl Pts',(7.90890021233917,-0.182259241909436,
105.350468472386));
#226751=CARTESIAN_POINT('Ctrl Pts',(7.9133824804781,0.0122428917785477,
105.35828087342));
#226752=CARTESIAN_POINT('Ctrl Pts',(7.91068780466358,0.207015931256116,
105.366093274454));
#226753=CARTESIAN_POINT('Ctrl Pts',(7.90080567100698,0.401485677183981,
105.373905675488));
#226754=CARTESIAN_POINT('Ctrl Pts',(7.89092642578947,0.595898581742127,
105.381715793043));
#226755=CARTESIAN_POINT('Ctrl Pts',(7.87386392630452,0.790008017999797,
105.389525910599));
#226756=CARTESIAN_POINT('Ctrl Pts',(7.84965975582054,0.983240925639028,
105.397336028154));
#226757=CARTESIAN_POINT('Ctrl Pts',(7.82545420625492,1.17648484311458,105.405146590706));
#226758=CARTESIAN_POINT('Ctrl Pts',(7.79410621004036,1.36885178188897,105.412957153259));
#226759=CARTESIAN_POINT('Ctrl Pts',(7.75570915775862,1.55977449019374,105.420767715811));
#226760=CARTESIAN_POINT('Ctrl Pts',(7.72578925082309,1.70854605792873,105.426853894067));
#226761=CARTESIAN_POINT('Ctrl Pts',(7.69159027227738,1.85644077009817,105.432940072323));
#226762=CARTESIAN_POINT('Ctrl Pts',(7.65317788216522,2.00319477433851,105.439026250578));
#226763=CARTESIAN_POINT('Ctrl Pts',(7.59864495597029,2.21153706334161,105.447666616582));
#226764=CARTESIAN_POINT('Ctrl Pts',(7.53564500625163,2.41748072643363,105.456306982585));
#226765=CARTESIAN_POINT('Ctrl Pts',(7.46442045024432,2.62037179460747,105.464947348588));
#226766=CARTESIAN_POINT('Ctrl Pts',(7.39307741285503,2.82360037017338,105.473602087759));
#226767=CARTESIAN_POINT('Ctrl Pts',(7.31348249750433,3.02376598366972,105.482256826931));
#226768=CARTESIAN_POINT('Ctrl Pts',(7.22592629292175,3.22023449600524,105.490911566102));
#226769=CARTESIAN_POINT('Ctrl Pts',(7.13566206998034,3.42277956614581,105.49983398696));
#226770=CARTESIAN_POINT('Ctrl Pts',(7.03693637482808,3.62139495060253,105.508756407819));
#226771=CARTESIAN_POINT('Ctrl Pts',(6.93011767567737,3.81541478757737,105.517678828677));
#226772=CARTESIAN_POINT('Ctrl Pts',(6.82615596055228,4.00424534983444,105.52636260954));
#226773=CARTESIAN_POINT('Ctrl Pts',(6.71452871879979,4.18872285026605,105.535046390404));
#226774=CARTESIAN_POINT('Ctrl Pts',(6.59561969201529,4.36826302760034,105.543730171267));
#226775=CARTESIAN_POINT('Ctrl Pts',(6.47180903596822,4.55520415178306,105.552771912123));
#226776=CARTESIAN_POINT('Ctrl Pts',(6.34010375121489,4.73679207408774,105.561813652979));
#226777=CARTESIAN_POINT('Ctrl Pts',(6.20098443854627,4.91240399325086,105.570855393835));
#226778=CARTESIAN_POINT('Ctrl Pts',(6.06186512587764,5.08801591241399,105.579897134691));
#226779=CARTESIAN_POINT('Ctrl Pts',(5.91533198265794,5.25765163063006,105.588938875547));
#226780=CARTESIAN_POINT('Ctrl Pts',(5.76191112895378,5.42072883863772,105.597980616403));
#226781=CARTESIAN_POINT('Ctrl Pts',(5.62070299111643,5.57082465879838,105.606302610176));
#226782=CARTESIAN_POINT('Ctrl Pts',(5.4735400667773,5.71549204698301,105.614624603948));
#226783=CARTESIAN_POINT('Ctrl Pts',(5.32085780504846,5.85426282451129,105.62294659772));
#226784=CARTESIAN_POINT('Ctrl Pts',(5.16831134156209,5.99291017691159,105.631261189768));
#226785=CARTESIAN_POINT('Ctrl Pts',(5.01025554918787,6.12567118499115,105.639575781815));
#226786=CARTESIAN_POINT('Ctrl Pts',(4.84716276725742,6.25211437097191,105.647890373862));
#226787=CARTESIAN_POINT('Ctrl Pts',(4.6842050966759,6.37845280731739,105.656198077832));
#226788=CARTESIAN_POINT('Ctrl Pts',(4.51621899160593,6.49848368439002,105.664505781802));
#226789=CARTESIAN_POINT('Ctrl Pts',(4.34371056714706,6.61181514478853,105.672813485772));
#226790=CARTESIAN_POINT('Ctrl Pts',(4.17137619591483,6.72503225885048,105.681112807642));
#226791=CARTESIAN_POINT('Ctrl Pts',(3.99452885677393,6.83156328840419,105.689412129513));
#226792=CARTESIAN_POINT('Ctrl Pts',(3.81370470239067,6.93105889766948,105.697711451384));
#226793=CARTESIAN_POINT('Ctrl Pts',(3.63299607670489,7.0304909391101,105.706005470811));
#226794=CARTESIAN_POINT('Ctrl Pts',(3.44831595931696,7.12289638557427,105.714299490238));
#226795=CARTESIAN_POINT('Ctrl Pts',(3.26022746868949,7.20797043920149,105.722593509666));
#226796=CARTESIAN_POINT('Ctrl Pts',(3.07227845503456,7.29298140618581,105.730881378665));
#226797=CARTESIAN_POINT('Ctrl Pts',(2.88092637839446,7.37067171053527,105.739169247664));
#226798=CARTESIAN_POINT('Ctrl Pts',(2.68675731058709,7.4407833024492,105.747457116664));
#226799=CARTESIAN_POINT('Ctrl Pts',(2.61274116637358,7.4675094424917,105.750616405185));
#226800=CARTESIAN_POINT('Ctrl Pts',(2.53831591804569,7.49313481443207,105.753775693706));
#226801=CARTESIAN_POINT('Ctrl Pts',(2.46351483339233,7.51764695005398,105.756934982227));
#226802=CARTESIAN_POINT('Ctrl Pts',(2.271680007557,7.58051076131652,105.765037292054));
#226803=CARTESIAN_POINT('Ctrl Pts',(2.07745262938128,7.63602267718541,105.77313960188));
#226804=CARTESIAN_POINT('Ctrl Pts',(1.88142453251002,7.68401995888021,105.781241911706));
#226805=CARTESIAN_POINT('Ctrl Pts',(1.68535316761434,7.73202783470713,105.789346009904));
#226806=CARTESIAN_POINT('Ctrl Pts',(1.48748060110207,7.77251769248018,105.797450108101));
#226807=CARTESIAN_POINT('Ctrl Pts',(1.28841015696449,7.8053776505324,105.805554206298));
#226808=CARTESIAN_POINT('Ctrl Pts',(1.08927080236307,7.83824898342715,105.81366110982));
#226809=CARTESIAN_POINT('Ctrl Pts',(0.88893305766179,7.86348509705911,105.821768013342));
#226810=CARTESIAN_POINT('Ctrl Pts',(0.688007255811946,7.88102575912236,
105.829874916863));
#226811=CARTESIAN_POINT('Ctrl Pts',(0.486900249261919,7.89858224021124,
105.837989131586));
#226812=CARTESIAN_POINT('Ctrl Pts',(0.285204443780371,7.90842937344495,
105.84610334631));
#226813=CARTESIAN_POINT('Ctrl Pts',(0.0835334385470369,7.91055896663722,
105.854217561033));
#226814=CARTESIAN_POINT('Ctrl Pts',(-0.118236129806538,7.91268960063032,
105.862335741434));
#226815=CARTESIAN_POINT('Ctrl Pts',(-0.319980555027692,7.90709517442139,
105.870453921836));
#226816=CARTESIAN_POINT('Ctrl Pts',(-0.521088515780572,7.89381959248637,
105.878572102237));
#226817=CARTESIAN_POINT('Ctrl Pts',(-0.722412749193519,7.88052973391401,
105.886699012976));
#226818=CARTESIAN_POINT('Ctrl Pts',(-0.923098832767194,7.85954224158228,
105.894825923716));
#226819=CARTESIAN_POINT('Ctrl Pts',(-1.12254142126977,7.83095280010892,
105.902952834455));
#226820=CARTESIAN_POINT('Ctrl Pts',(-1.22836645289374,7.81578312862227,
105.907265005654));
#226821=CARTESIAN_POINT('Ctrl Pts',(-1.33384155310845,7.79847406587492,
105.911577176853));
#226822=CARTESIAN_POINT('Ctrl Pts',(-1.43887765982924,7.77904570497207,
105.915889348052));
#226823=CARTESIAN_POINT('Ctrl Pts',(-1.63368823366864,7.74301190426861,
105.923887136356));
#226824=CARTESIAN_POINT('Ctrl Pts',(-1.82732604650489,7.69962229868353,
105.931884924659));
#226825=CARTESIAN_POINT('Ctrl Pts',(-2.01920443715297,7.64896950189905,
105.939882712963));
#226826=CARTESIAN_POINT('Ctrl Pts',(-2.21092615932943,7.59835806306128,
105.947873971082));
#226827=CARTESIAN_POINT('Ctrl Pts',(-2.40089100033975,7.54049533650564,
105.955865229201));
#226828=CARTESIAN_POINT('Ctrl Pts',(-2.58852196651859,7.47552506710069,
105.96385648732));
#226829=CARTESIAN_POINT('Ctrl Pts',(-2.77603154930131,7.41059682866806,
105.971842575685));
#226830=CARTESIAN_POINT('Ctrl Pts',(-2.96120995140607,7.33857032082342,
105.979828664049));
#226831=CARTESIAN_POINT('Ctrl Pts',(-3.14349443852666,7.25963936535087,
105.987814752414));
#226832=CARTESIAN_POINT('Ctrl Pts',(-3.32569189816689,7.18074609362358,
105.995797028006));
#226833=CARTESIAN_POINT('Ctrl Pts',(-3.50499789047128,7.09495507767446,
106.003779303599));
#226834=CARTESIAN_POINT('Ctrl Pts',(-3.6808684159817,7.00250874360242,106.011761579192));
#226835=CARTESIAN_POINT('Ctrl Pts',(-3.85668477632484,6.91009088144821,
106.019741396378));
#226836=CARTESIAN_POINT('Ctrl Pts',(-4.0290674834548,6.81102194306289,106.027721213564));
#226837=CARTESIAN_POINT('Ctrl Pts',(-4.19749559379963,6.70559108058587,
106.03570103075));
#226838=CARTESIAN_POINT('Ctrl Pts',(-4.37171173832614,6.59653708516166,
106.043955074456));
#226839=CARTESIAN_POINT('Ctrl Pts',(-4.54169632465342,6.48067631299969,
106.052209118162));
#226840=CARTESIAN_POINT('Ctrl Pts',(-4.70690325897771,6.35837893732554,
106.060463161869));
#226841=CARTESIAN_POINT('Ctrl Pts',(-4.86664307485283,6.24012869345955,
106.068444058235));
#226842=CARTESIAN_POINT('Ctrl Pts',(-5.02191611579783,6.1158612585264,106.076424954602));
#226843=CARTESIAN_POINT('Ctrl Pts',(-5.17226052574444,5.98595372967632,
106.084405850968));
#226844=CARTESIAN_POINT('Ctrl Pts',(-5.32263831407062,5.85601735969534,
106.092388519196));
#226845=CARTESIAN_POINT('Ctrl Pts',(-5.46808503643004,5.72043861809531,
106.100371187423));
#226846=CARTESIAN_POINT('Ctrl Pts',(-5.60817370479094,5.57963338373513,
106.108353855651));
#226847=CARTESIAN_POINT('Ctrl Pts',(-5.74831500860744,5.4387752446843,106.116339523203));
#226848=CARTESIAN_POINT('Ctrl Pts',(-5.88309400892707,5.2926869351,106.124325190755));
#226849=CARTESIAN_POINT('Ctrl Pts',(-6.01212195496138,5.14181977500879,
106.132310858307));
#226850=CARTESIAN_POINT('Ctrl Pts',(-6.1412182178009,4.99087273483959,106.140300754053));
#226851=CARTESIAN_POINT('Ctrl Pts',(-6.26455713846359,4.83514205375893,
106.1482906498));
#226852=CARTESIAN_POINT('Ctrl Pts',(-6.38179124611312,4.67511085334176,
106.156280545547));
#226853=CARTESIAN_POINT('Ctrl Pts',(-6.49916422724139,4.51489008275636,
106.164279905985));
#226854=CARTESIAN_POINT('Ctrl Pts',(-6.61041775138325,4.35035888618521,
106.172279266423));
#226855=CARTESIAN_POINT('Ctrl Pts',(-6.7152478722501,4.18202905468631,106.180278626861));
#226856=CARTESIAN_POINT('Ctrl Pts',(-6.82015127527881,4.01358155114949,
106.188283579303));
#226857=CARTESIAN_POINT('Ctrl Pts',(-6.9186221538547,3.84133040617136,106.196288531744));
#226858=CARTESIAN_POINT('Ctrl Pts',(-7.0104030409166,3.6658109885682,106.204293484186));
#226859=CARTESIAN_POINT('Ctrl Pts',(-7.10230370952609,3.49006250380142,
106.212308883744));
#226860=CARTESIAN_POINT('Ctrl Pts',(-7.18749680345879,3.31103752751581,
106.220324283302));
#226861=CARTESIAN_POINT('Ctrl Pts',(-7.26577293518402,3.12929139811993,
106.22833968286));
#226862=CARTESIAN_POINT('Ctrl Pts',(-7.28354132327757,3.08803570892796,
106.230159148474));
#226863=CARTESIAN_POINT('Ctrl Pts',(-7.30095350231,3.04663986757932,106.231978614088));
#226864=CARTESIAN_POINT('Ctrl Pts',(-7.31800738292345,3.00511047109384,
106.233798079702));
#226865=CARTESIAN_POINT('Ctrl Pts',(-7.39877472521689,2.8084268506786,106.242415086315));
#226866=CARTESIAN_POINT('Ctrl Pts',(-7.47170868025304,2.60824228953016,
106.251032092929));
#226867=CARTESIAN_POINT('Ctrl Pts',(-7.53651565036496,2.40517210440419,
106.259649099543));
#226868=CARTESIAN_POINT('Ctrl Pts',(-7.6010415810271,2.20298254574469,106.268228737972));
#226869=CARTESIAN_POINT('Ctrl Pts',(-7.6575107334181,1.99793254499741,106.276808376402));
#226870=CARTESIAN_POINT('Ctrl Pts',(-7.70567814829004,1.79065498490509,
106.285388014831));
#226871=CARTESIAN_POINT('Ctrl Pts',(-7.75372047593898,1.58391570934492,
106.293945372573));
#226872=CARTESIAN_POINT('Ctrl Pts',(-7.79350400063278,1.37496063973674,
106.302502730314));
#226873=CARTESIAN_POINT('Ctrl Pts',(-7.82483228615782,1.1644400772484,106.311060088056));
#226874=CARTESIAN_POINT('Ctrl Pts',(-7.85602840229548,0.954807669771018,
106.319581343575));
#226875=CARTESIAN_POINT('Ctrl Pts',(-7.87884037064651,0.743623174706886,
106.328102599094));
#226876=CARTESIAN_POINT('Ctrl Pts',(-7.8931222040916,0.531547619010923,
106.336623854613));
#226877=CARTESIAN_POINT('Ctrl Pts',(-7.90487931359323,0.356962504255063,
106.343638733663));
#226878=CARTESIAN_POINT('Ctrl Pts',(-7.91085644909219,0.181773925383775,
106.350653612713));
#226879=CARTESIAN_POINT('Ctrl Pts',(-7.91099744449602,0.00635870878843768,
106.357668491763));
#226880=CARTESIAN_POINT('',(-7.90668697097569,-0.00507742928152955,108.357668491763));
#226881=CARTESIAN_POINT('Ctrl Pts',(-7.911,-2.54019028034236E-12,106.357668491763));
#226882=CARTESIAN_POINT('Ctrl Pts',(-7.91099999999929,-2.20167589666934,
106.446255927496));
#226883=CARTESIAN_POINT('Ctrl Pts',(-6.94214576672228,-4.38610418338912,
106.534843363229));
#226884=CARTESIAN_POINT('Ctrl Pts',(-3.6782020148804,-7.34180684107756,
106.712018234694));
#226885=CARTESIAN_POINT('Ctrl Pts',(-1.40868175871469,-8.08992666571385,
106.800605670427));
#226886=CARTESIAN_POINT('Ctrl Pts',(2.9730927052154,-7.65454228025154,106.977780541892));
#226887=CARTESIAN_POINT('Ctrl Pts',(5.0510207267583,-6.47444880834049,107.066367977625));
#226888=CARTESIAN_POINT('Ctrl Pts',(7.66951518847977,-2.93425195367433,
107.24354284909));
#226889=CARTESIAN_POINT('Ctrl Pts',(8.18956872247094,-0.601881960096207,
107.332130284823));
#226890=CARTESIAN_POINT('Ctrl Pts',(7.32306689761207,3.7153719823272,107.509305156289));
#226891=CARTESIAN_POINT('Ctrl Pts',(5.94329958849991,5.66643518936733,107.597892592021));
#226892=CARTESIAN_POINT('Ctrl Pts',(2.16154501637548,7.9220591323308,107.775067463487));
#226893=CARTESIAN_POINT('Ctrl Pts',(-0.210816529303511,8.20894963712995,
107.863654899219));
#226894=CARTESIAN_POINT('Ctrl Pts',(-4.42123908576707,6.9198224471766,108.040829770685));
#226895=CARTESIAN_POINT('Ctrl Pts',(-6.22631625634399,5.35390358803276,
108.129417206418));
#226896=CARTESIAN_POINT('Ctrl Pts',(-7.65317280859563,2.31334857514252,
108.264559258688));
#226897=CARTESIAN_POINT('Ctrl Pts',(-7.91100000000028,1.15702837836286,
108.311113875226));
#226898=CARTESIAN_POINT('Ctrl Pts',(-7.911,-1.9195756095769E-12,108.357668491763));
#226899=CARTESIAN_POINT('',(-7.92015086488778,-0.000676322392208838,110.357668491763));
#226900=CARTESIAN_POINT('Ctrl Pts',(-7.90464730954992,-0.00747858090497255,
108.357668491763));
#226901=CARTESIAN_POINT('Ctrl Pts',(-7.91210078102921,-0.847847773565596,
108.391498728258));
#226902=CARTESIAN_POINT('Ctrl Pts',(-7.40339374633633,-4.31311009557957,
108.531298541969));
#226903=CARTESIAN_POINT('Ctrl Pts',(-2.33386570890254,-9.06921176931051,
108.777067932898));
#226904=CARTESIAN_POINT('Ctrl Pts',(4.88597846667002,-7.2226779862135,109.041991875939));
#226905=CARTESIAN_POINT('Ctrl Pts',(7.79261686719547,-2.6388854416884,109.253931030372));
#226906=CARTESIAN_POINT('Ctrl Pts',(8.26759383351024,2.79482092152063,109.465870184806));
#226907=CARTESIAN_POINT('Ctrl Pts',(4.57231411070881,7.4310279169445,109.677809339238));
#226908=CARTESIAN_POINT('Ctrl Pts',(-0.838290124238692,8.19283827172977,
109.889748493671));
#226909=CARTESIAN_POINT('Ctrl Pts',(-4.65967318531691,6.81204228408581,
110.048702859496));
#226910=CARTESIAN_POINT('Ctrl Pts',(-7.28542678060952,3.80108478578778,
110.204676192194));
#226911=CARTESIAN_POINT('Ctrl Pts',(-7.92152424932248,1.2396389119941,110.307664736282));
#226912=CARTESIAN_POINT('Ctrl Pts',(-7.92015086488778,-0.000676322392208838,
110.357668491763));
#226913=CARTESIAN_POINT('',(-7.90798625669136,0.00451216966572269,112.357668491763));
#226914=CARTESIAN_POINT('Ctrl Pts',(-7.92015086488778,-0.000676322392208838,
110.357668491763));
#226915=CARTESIAN_POINT('Ctrl Pts',(-7.92006898894752,-0.0746191846174104,
110.360649524891));
#226916=CARTESIAN_POINT('Ctrl Pts',(-7.9188845772038,-0.148550187530037,
110.363630558018));
#226917=CARTESIAN_POINT('Ctrl Pts',(-7.83490291760856,-2.8490699327844,
110.472581168362));
#226918=CARTESIAN_POINT('Ctrl Pts',(-4.85753102683806,-7.99819754528262,
110.684520322796));
#226919=CARTESIAN_POINT('Ctrl Pts',(4.12483722040859,-8.40733305923675,
111.002429054444));
#226920=CARTESIAN_POINT('Ctrl Pts',(8.40870675888375,-2.30944008633724,
111.267352997486));
#226921=CARTESIAN_POINT('Ctrl Pts',(7.63590137194488,3.06294045831641,111.479292151919));
#226922=CARTESIAN_POINT('Ctrl Pts',(4.46313123637914,7.49963941440561,111.691231306351));
#226923=CARTESIAN_POINT('Ctrl Pts',(-1.35903023235194,8.61854216541067,
111.903170460786));
#226924=CARTESIAN_POINT('Ctrl Pts',(-5.96470993446413,5.67869392350227,
112.115109615218));
#226925=CARTESIAN_POINT('Ctrl Pts',(-7.65292984181716,2.70307941383637,
112.248947362674));
#226926=CARTESIAN_POINT('Ctrl Pts',(-7.90915144490032,0.696989207157879,
112.329800321523));
#226927=CARTESIAN_POINT('Ctrl Pts',(-7.90798625669136,0.00451216966572269,
112.357668491763));
#226928=CARTESIAN_POINT('',(-7.911,-1.68698388591793E-12,116.357668491763));
#226929=CARTESIAN_POINT('Ctrl Pts',(-7.91099909341042,0.00378735521236961,
112.359438569417));
#226930=CARTESIAN_POINT('Ctrl Pts',(-7.91110391793188,-0.215169317115718,
112.368531704429));
#226931=CARTESIAN_POINT('Ctrl Pts',(-7.90211847162492,-0.434041754412859,
112.377526913421));
#226932=CARTESIAN_POINT('Ctrl Pts',(-7.88108246637407,-0.688308156281573,
112.387881319802));
#226933=CARTESIAN_POINT('Ctrl Pts',(-7.87785345400522,-0.724329990006576,
112.389346070283));
#226934=CARTESIAN_POINT('Ctrl Pts',(-7.8720841184119,-0.784080380183848,
112.391772375696));
#226935=CARTESIAN_POINT('Ctrl Pts',(-7.86968324575642,-0.80782177882518,
112.392735581477));
#226936=CARTESIAN_POINT('Ctrl Pts',(-7.86516700529536,-0.85054917756705,
112.394467590496));
#226937=CARTESIAN_POINT('Ctrl Pts',(-7.86309021752687,-0.86953904925642,
112.395236844623));
#226938=CARTESIAN_POINT('Ctrl Pts',(-7.85871900643568,-0.908212123988966,
112.396802429831));
#226939=CARTESIAN_POINT('Ctrl Pts',(-7.85641936817883,-0.927894605184168,
112.39759869399));
#226940=CARTESIAN_POINT('Ctrl Pts',(-7.85129336098033,-0.970382198386325,
112.399316473813));
#226941=CARTESIAN_POINT('Ctrl Pts',(-7.84844153078315,-0.99318406813759,
112.400237686468));
#226942=CARTESIAN_POINT('Ctrl Pts',(-7.84047545541975,-1.05469923960324,
112.402721294243));
#226943=CARTESIAN_POINT('Ctrl Pts',(-7.83517384599178,-1.09338770616955,
112.404281529201));
#226944=CARTESIAN_POINT('Ctrl Pts',(-7.80724111346652,-1.28658106376407,
112.412065404366));
#226945=CARTESIAN_POINT('Ctrl Pts',(-7.78032515087,-1.44043265128534,112.418240217163));
#226946=CARTESIAN_POINT('Ctrl Pts',(-7.71946914944251,-1.73638400145209,
112.430122324764));
#226947=CARTESIAN_POINT('Ctrl Pts',(-7.68611230144968,-1.87853972945209,
112.435835263813));
#226948=CARTESIAN_POINT('Ctrl Pts',(-7.4358977017971,-2.82613602366019,
112.47405799312));
#226949=CARTESIAN_POINT('Ctrl Pts',(-7.0967628488701,-3.59381851737072,
112.504736754193));
#226950=CARTESIAN_POINT('Ctrl Pts',(-6.53707512693398,-4.45975115321796,
112.543696044146));
#226951=CARTESIAN_POINT('Ctrl Pts',(-6.42399579831044,-4.62114763320364,
112.551215180201));
#226952=CARTESIAN_POINT('Ctrl Pts',(-6.25284548959735,-4.84698923599435,
112.562294026589));
#226953=CARTESIAN_POINT('Ctrl Pts',(-6.19955397931614,-4.91496808548651,
112.565705655712));
#226954=CARTESIAN_POINT('Ctrl Pts',(-6.13553354891786,-4.99393459921745,
112.56977406205));
#226955=CARTESIAN_POINT('Ctrl Pts',(-6.12587160035205,-5.00578184139577,
112.570387282534));
#226956=CARTESIAN_POINT('Ctrl Pts',(-6.11100531676054,-5.02390301103125,
112.571329716701));
#226957=CARTESIAN_POINT('Ctrl Pts',(-6.10582549833209,-5.03019705668593,
112.571657884525));
#226958=CARTESIAN_POINT('Ctrl Pts',(-6.09639627480391,-5.04161857035328,
112.572254926099));
#226959=CARTESIAN_POINT('Ctrl Pts',(-6.09215010180067,-5.04674870438436,
112.572523658712));
#226960=CARTESIAN_POINT('Ctrl Pts',(-6.08356689682495,-5.05709212889711,
112.573066628641));
#226961=CARTESIAN_POINT('Ctrl Pts',(-6.07922962955142,-5.06230521592135,
112.573340876347));
#226962=CARTESIAN_POINT('Ctrl Pts',(-6.06688367817154,-5.07710542411794,
112.574121176705));
#226963=CARTESIAN_POINT('Ctrl Pts',(-6.05885900073047,-5.08667913861518,
112.574627953717));
#226964=CARTESIAN_POINT('Ctrl Pts',(-6.02485094157122,-5.12705726326551,
112.576774087429));
#226965=CARTESIAN_POINT('Ctrl Pts',(-5.99865532668357,-5.15768157646999,
112.578423385601));
#226966=CARTESIAN_POINT('Ctrl Pts',(-5.62110291550108,-5.59229675746159,
112.602158449571));
#226967=CARTESIAN_POINT('Ctrl Pts',(-5.22992590767809,-5.95971630803955,
112.626709873887));
#226968=CARTESIAN_POINT('Ctrl Pts',(-4.66511587914959,-6.39151873578675,
112.659310489173));
#226969=CARTESIAN_POINT('Ctrl Pts',(-4.52195329497706,-6.49359359529973,
112.667362624421));
#226970=CARTESIAN_POINT('Ctrl Pts',(-4.21533781734595,-6.6971493484238,
112.684063874268));
#226971=CARTESIAN_POINT('Ctrl Pts',(-4.0513402853464,-6.79761199024794,
112.692692307174));
#226972=CARTESIAN_POINT('Ctrl Pts',(-3.67881505754575,-7.00754058808218,
112.711526260314));
#226973=CARTESIAN_POINT('Ctrl Pts',(-3.46872724239839,-7.11387716125557,
112.721640843663));
#226974=CARTESIAN_POINT('Ctrl Pts',(-3.1572777764017,-7.25443484992384,
112.73587097101));
#226975=CARTESIAN_POINT('Ctrl Pts',(-3.05948239035484,-7.296217964917,112.740234815822));
#226976=CARTESIAN_POINT('Ctrl Pts',(-2.94507203749039,-7.3423948403118,
112.745221366311));
#226977=CARTESIAN_POINT('Ctrl Pts',(-2.92925166161774,-7.34872070530823,
112.745908294875));
#226978=CARTESIAN_POINT('Ctrl Pts',(-2.90516317970548,-7.35826247138739,
112.746950298369));
#226979=CARTESIAN_POINT('Ctrl Pts',(-2.89690994425414,-7.36151563701957,
112.747306611587));
#226980=CARTESIAN_POINT('Ctrl Pts',(-2.88194300212572,-7.36738606670268,
112.747951508545));
#226981=CARTESIAN_POINT('Ctrl Pts',(-2.87523116439721,-7.37000805121509,
112.748240248919));
#226982=CARTESIAN_POINT('Ctrl Pts',(-2.86180870316945,-7.37523041949227,
112.748816760699));
#226983=CARTESIAN_POINT('Ctrl Pts',(-2.85509809496872,-7.37783082366342,
112.749104532592));
#226984=CARTESIAN_POINT('Ctrl Pts',(-2.83621561657294,-7.38511828603602,
112.749912990048));
#226985=CARTESIAN_POINT('Ctrl Pts',(-2.82403566463424,-7.38978441426982,
112.750432980452));
#226986=CARTESIAN_POINT('Ctrl Pts',(-2.77400499419833,-7.40880936040276,
112.752562796256));
#226987=CARTESIAN_POINT('Ctrl Pts',(-2.7360555648631,-7.4229077762043,112.754163978913));
#226988=CARTESIAN_POINT('Ctrl Pts',(-2.14551303640637,-7.63715336867258,
112.778862374931));
#226989=CARTESIAN_POINT('Ctrl Pts',(-1.57240802252616,-7.77540770426758,
112.799688643695));
#226990=CARTESIAN_POINT('Ctrl Pts',(-0.687423736733492,-7.88694473036076,
112.830220914817));
#226991=CARTESIAN_POINT('Ctrl Pts',(-0.383689152701452,-7.90754244968169,
112.840456887215));
#226992=CARTESIAN_POINT('Ctrl Pts',(-0.037365374191139,-7.91102411903661,
112.852406943225));
#226993=CARTESIAN_POINT('Ctrl Pts',(0.00479878470609816,-7.91111090314451,
112.853866719993));
#226994=CARTESIAN_POINT('Ctrl Pts',(0.185755773332728,-7.91003668417216,
112.860158922853));
#226995=CARTESIAN_POINT('Ctrl Pts',(0.324501274579026,-7.90556023642795,
112.865051896828));
#226996=CARTESIAN_POINT('Ctrl Pts',(0.68185420656507,-7.88460741903093,
112.877971698729));
#226997=CARTESIAN_POINT('Ctrl Pts',(0.900013055256525,-7.86269184129545,
112.886166329226));
#226998=CARTESIAN_POINT('Ctrl Pts',(1.14638554205417,-7.82755417543703,
112.896026935467));
#226999=CARTESIAN_POINT('Ctrl Pts',(1.17578194491904,-7.82319250401897,
112.89721335305));
#227000=CARTESIAN_POINT('Ctrl Pts',(1.21263889942198,-7.81751145020797,
112.898713994789));
#227001=CARTESIAN_POINT('Ctrl Pts',(1.22012340279418,-7.81634679730411,
112.899019408456));
#227002=CARTESIAN_POINT('Ctrl Pts',(1.23199898070919,-7.81448138293267,
112.899505099109));
#227003=CARTESIAN_POINT('Ctrl Pts',(1.23639117288685,-7.81378766285104,
112.899684969854));
#227004=CARTESIAN_POINT('Ctrl Pts',(1.24464160440901,-7.81247742670176,
112.900023294816));
#227005=CARTESIAN_POINT('Ctrl Pts',(1.24849997833709,-7.81186175441789,
112.90018169994));
#227006=CARTESIAN_POINT('Ctrl Pts',(1.2571432261738,-7.8104760032265,112.900536964976));
#227007=CARTESIAN_POINT('Ctrl Pts',(1.26192784804837,-7.80970438583998,
112.900733914889));
#227008=CARTESIAN_POINT('Ctrl Pts',(1.27403280069354,-7.80774080198006,
112.901232924162));
#227009=CARTESIAN_POINT('Ctrl Pts',(1.28135216304042,-7.80654293794121,
112.90153533178));
#227010=CARTESIAN_POINT('Ctrl Pts',(1.32297696445081,-7.79967063501432,
112.903259010896));
#227011=CARTESIAN_POINT('Ctrl Pts',(1.35724587437818,-7.79378044501303,
112.904693159579));
#227012=CARTESIAN_POINT('Ctrl Pts',(1.94123807873922,-7.68943463857647,
112.929375784607));
#227013=CARTESIAN_POINT('Ctrl Pts',(2.47901890126596,-7.53327277421705,
112.955663656277));
#227014=CARTESIAN_POINT('Ctrl Pts',(3.209169117443,-7.23452048933398,112.992314636444));
#227015=CARTESIAN_POINT('Ctrl Pts',(3.41859487278246,-7.13794567891392,
113.002964997158));
#227016=CARTESIAN_POINT('Ctrl Pts',(3.87118663982711,-6.9047422230209,113.026025639755));
#227017=CARTESIAN_POINT('Ctrl Pts',(4.1119618519506,-6.76412161807801,113.038319595422));
#227018=CARTESIAN_POINT('Ctrl Pts',(4.43843949654639,-6.54955898637998,
113.054896555846));
#227019=CARTESIAN_POINT('Ctrl Pts',(4.53073263492991,-6.48605668569394,
113.05957319829));
#227020=CARTESIAN_POINT('Ctrl Pts',(4.65434640757037,-6.39707773841129,
113.065823899636));
#227021=CARTESIAN_POINT('Ctrl Pts',(4.68686394305266,-6.37329196884744,
113.067466970943));
#227022=CARTESIAN_POINT('Ctrl Pts',(4.7342659135548,-6.33805961609715,113.069860505458));
#227023=CARTESIAN_POINT('Ctrl Pts',(4.7492932772553,-6.32680699965637,113.070619061501));
#227024=CARTESIAN_POINT('Ctrl Pts',(4.77636171659958,-6.30638714074617,
113.071985022468));
#227025=CARTESIAN_POINT('Ctrl Pts',(4.78841678632789,-6.2972386568037,113.072593213018));
#227026=CARTESIAN_POINT('Ctrl Pts',(4.80683198267604,-6.2831800743934,113.073522067685));
#227027=CARTESIAN_POINT('Ctrl Pts',(4.81321096880611,-6.27829481047383,
113.073843782161));
#227028=CARTESIAN_POINT('Ctrl Pts',(4.82431462711144,-6.26976434869976,
113.074403713303));
#227029=CARTESIAN_POINT('Ctrl Pts',(4.82904263196144,-6.26612351206904,
113.074642114774));
#227030=CARTESIAN_POINT('Ctrl Pts',(4.83891153452042,-6.25850608396308,
113.075139695514));
#227031=CARTESIAN_POINT('Ctrl Pts',(4.84405166175257,-6.25452849865389,
113.075398832223));
#227032=CARTESIAN_POINT('Ctrl Pts',(4.8582315274726,-6.24352772614433,113.076113639642));
#227033=CARTESIAN_POINT('Ctrl Pts',(4.8672609501161,-6.2364912319877,113.076568742474));
#227034=CARTESIAN_POINT('Ctrl Pts',(4.90247055816215,-6.20892986713702,
113.078343129357));
#227035=CARTESIAN_POINT('Ctrl Pts',(4.92853663255235,-6.18825939721531,
113.079656173752));
#227036=CARTESIAN_POINT('Ctrl Pts',(5.33765698439499,-5.85960112397001,
113.100258677564));
#227037=CARTESIAN_POINT('Ctrl Pts',(5.6913420690343,-5.51672041297941,113.117876688909));
#227038=CARTESIAN_POINT('Ctrl Pts',(6.36690502540627,-4.72717974376021,
113.15354471197));
#227039=CARTESIAN_POINT('Ctrl Pts',(6.67869135551183,-4.27536109999382,
113.171322632807));
#227040=CARTESIAN_POINT('Ctrl Pts',(7.04175631420485,-3.61129191145059,
113.198523797016));
#227041=CARTESIAN_POINT('Ctrl Pts',(7.13485900466652,-3.42367289360687,
113.206330502067));
#227042=CARTESIAN_POINT('Ctrl Pts',(7.23185916858235,-3.20701103946101,
113.215729808808));
#227043=CARTESIAN_POINT('Ctrl Pts',(7.24317775071759,-3.18136493872878,
113.216848376715));
#227044=CARTESIAN_POINT('Ctrl Pts',(7.25718659932713,-3.14916082276682,
113.218261123051));
#227045=CARTESIAN_POINT('Ctrl Pts',(7.26000481357919,-3.14265832239199,
113.218546792701));
#227046=CARTESIAN_POINT('Ctrl Pts',(7.26447234677335,-3.13231224758086,
113.219001992224));
#227047=CARTESIAN_POINT('Ctrl Pts',(7.26612736706759,-3.12847112481371,
113.219171138576));
#227048=CARTESIAN_POINT('Ctrl Pts',(7.26924950071512,-3.12120914888068,
113.219491200025));
#227049=CARTESIAN_POINT('Ctrl Pts',(7.27071724812643,-3.11778856762346,
113.219642072818));
#227050=CARTESIAN_POINT('Ctrl Pts',(7.27402473882655,-3.11006543268988,
113.219982978173));
#227051=CARTESIAN_POINT('Ctrl Pts',(7.27586307839314,-3.10576228339939,
113.220173103432));
#227052=CARTESIAN_POINT('Ctrl Pts',(7.28055411377078,-3.09475457597844,
113.220659912145));
#227053=CARTESIAN_POINT('Ctrl Pts',(7.2834013607103,-3.08804771775673,113.220956951919));
#227054=CARTESIAN_POINT('Ctrl Pts',(7.29947243618667,-3.05004547920541,
113.222642442401));
#227055=CARTESIAN_POINT('Ctrl Pts',(7.3125036295819,-3.01866955275799,113.224043290719));
#227056=CARTESIAN_POINT('Ctrl Pts',(7.52739699507563,-2.49170135578868,
113.247713083894));
#227057=CARTESIAN_POINT('Ctrl Pts',(7.67864615754396,-1.97701063565568,
113.272856248665));
#227058=CARTESIAN_POINT('Ctrl Pts',(7.83376938138709,-1.14564515426838,
113.312610247343));
#227059=CARTESIAN_POINT('Ctrl Pts',(7.87271707739679,-0.837129145396408,
113.327199153451));
#227060=CARTESIAN_POINT('Ctrl Pts',(7.91679991703811,-0.176997222439834,
113.357455722306));
#227061=CARTESIAN_POINT('Ctrl Pts',(7.91686215876792,0.174310392148266,
113.372978577639));
#227062=CARTESIAN_POINT('Ctrl Pts',(7.88456468887725,0.660385353834943,
113.393477711963));
#227063=CARTESIAN_POINT('Ctrl Pts',(7.87202737273524,0.796025595825848,
113.399094915723));
#227064=CARTESIAN_POINT('Ctrl Pts',(7.85393469127237,0.948650008243326,
113.405305041202));
#227065=CARTESIAN_POINT('Ctrl Pts',(7.85181791582858,0.966013661854685,
113.406009940833));
#227066=CARTESIAN_POINT('Ctrl Pts',(7.84855745976568,0.992039890028385,
113.407064125316));
#227067=CARTESIAN_POINT('Ctrl Pts',(7.84745699644182,1.00070776569241,113.407414818286));
#227068=CARTESIAN_POINT('Ctrl Pts',(7.84554206918107,1.015593404926,113.40801639839));
#227069=CARTESIAN_POINT('Ctrl Pts',(7.84473456953753,1.02181204589919,113.408267512124));
#227070=CARTESIAN_POINT('Ctrl Pts',(7.843058684269,1.03459913663296,113.408783449678));
#227071=CARTESIAN_POINT('Ctrl Pts',(7.84218943904832,1.04116747009265,113.4090482453));
#227072=CARTESIAN_POINT('Ctrl Pts',(7.83983375724926,1.05879753958153,113.409758381213));
#227073=CARTESIAN_POINT('Ctrl Pts',(7.83833215862413,1.06985725382443,113.410203227722));
#227074=CARTESIAN_POINT('Ctrl Pts',(7.83277985626358,1.11011238197129,113.411820083304));
#227075=CARTESIAN_POINT('Ctrl Pts',(7.82858937730947,1.13928844608132,113.412987545689));
#227076=CARTESIAN_POINT('Ctrl Pts',(7.75843857498311,1.60903968331242,113.431715436527));
#227077=CARTESIAN_POINT('Ctrl Pts',(7.65553970168657,2.04331686113108,113.44798649548));
#227078=CARTESIAN_POINT('Ctrl Pts',(7.38892898988996,2.85575890663298,113.478043427477));
#227079=CARTESIAN_POINT('Ctrl Pts',(7.23122169912992,3.2343554663412,113.491894666743));
#227080=CARTESIAN_POINT('Ctrl Pts',(6.87209045805419,3.93733525900934,113.519588844311));
#227081=CARTESIAN_POINT('Ctrl Pts',(6.67511837697347,4.2627513887646,113.53339371771));
#227082=CARTESIAN_POINT('Ctrl Pts',(6.44521138912371,4.58731829371914,113.549296253781));
#227083=CARTESIAN_POINT('Ctrl Pts',(6.4348549380833,4.6018345143263,113.55001168697));
#227084=CARTESIAN_POINT('Ctrl Pts',(6.41978588157494,4.62280586973609,113.551051229688));
#227085=CARTESIAN_POINT('Ctrl Pts',(6.41511238820293,4.62928913772402,113.551373432809));
#227086=CARTESIAN_POINT('Ctrl Pts',(6.40694071231118,4.6405890947951,113.551936450492));
#227087=CARTESIAN_POINT('Ctrl Pts',(6.40344689751289,4.64540894521621,113.552177055654));
#227088=CARTESIAN_POINT('Ctrl Pts',(6.39668631094385,4.65471331256008,113.552642404484));
#227089=CARTESIAN_POINT('Ctrl Pts',(6.39342025454864,4.65919834642077,113.552867114248));
#227090=CARTESIAN_POINT('Ctrl Pts',(6.38566505020503,4.66982448624168,113.553400438384));
#227091=CARTESIAN_POINT('Ctrl Pts',(6.38117176254886,4.6759625535309,113.553709246292));
#227092=CARTESIAN_POINT('Ctrl Pts',(6.36771636976929,4.694287814086,113.554633388443));
#227093=CARTESIAN_POINT('Ctrl Pts',(6.35872818070992,4.70645575430839,113.555249922279));
#227094=CARTESIAN_POINT('Ctrl Pts',(6.27141623491458,4.82394936998101,113.561230863727));
#227095=CARTESIAN_POINT('Ctrl Pts',(6.19051976092825,4.92733316274009,113.566709192393));
#227096=CARTESIAN_POINT('Ctrl Pts',(5.70678285797201,5.51481165091869,113.59893609962));
#227097=CARTESIAN_POINT('Ctrl Pts',(5.24985412705107,5.9514358048604,113.627129031921));
#227098=CARTESIAN_POINT('Ctrl Pts',(4.44878940704382,6.55211280762734,113.670227265589));
#227099=CARTESIAN_POINT('Ctrl Pts',(4.13625447685716,6.75376454892645,113.685833570334));
#227100=CARTESIAN_POINT('Ctrl Pts',(3.75026236030472,6.96593195919709,113.703786433901));
#227101=CARTESIAN_POINT('Ctrl Pts',(3.68940199107702,6.99835615881094,113.706581249646));
#227102=CARTESIAN_POINT('Ctrl Pts',(3.60845490327048,7.0401323980446,113.710253229917));
#227103=CARTESIAN_POINT('Ctrl Pts',(3.58874216557697,7.05020146135516,113.711143924879));
#227104=CARTESIAN_POINT('Ctrl Pts',(3.55657778430463,7.06646084079189,113.712591482818));
#227105=CARTESIAN_POINT('Ctrl Pts',(3.54415165922709,7.07270127801969,113.713149330364));
#227106=CARTESIAN_POINT('Ctrl Pts',(3.52020978345086,7.08464602005354,113.714221481858));
#227107=CARTESIAN_POINT('Ctrl Pts',(3.50869646249076,7.09035508872612,113.714735879444));
#227108=CARTESIAN_POINT('Ctrl Pts',(3.48230004910934,7.10336414397074,113.715912518658));
#227109=CARTESIAN_POINT('Ctrl Pts',(3.46740780731474,7.11064546255504,113.716574382687));
#227110=CARTESIAN_POINT('Ctrl Pts',(3.42039172861212,7.13345038095268,113.718657750478));
#227111=CARTESIAN_POINT('Ctrl Pts',(3.38818558328636,7.14880356375863,113.720075773544));
#227112=CARTESIAN_POINT('Ctrl Pts',(3.09338535191011,7.28689983344149,113.732973337495));
#227113=CARTESIAN_POINT('Ctrl Pts',(2.82432757882454,7.39534506147803,113.744137725305));
#227114=CARTESIAN_POINT('Ctrl Pts',(2.15641584556803,7.62276746168111,113.77067123349));
#227115=CARTESIAN_POINT('Ctrl Pts',(1.75297346276947,7.72552936251439,113.785695606884));
#227116=CARTESIAN_POINT('Ctrl Pts',(1.00720051997519,7.85403069464445,113.813253009672));
#227117=CARTESIAN_POINT('Ctrl Pts',(0.667704405565595,7.89014560768651,
113.825735307388));
#227118=CARTESIAN_POINT('Ctrl Pts',(0.236678896904833,7.90797499995271,
113.842453276867));
#227119=CARTESIAN_POINT('Ctrl Pts',(0.146343353599015,7.91016234248309,
113.846006323216));
#227120=CARTESIAN_POINT('Ctrl Pts',(0.043352051265991,7.91089131463553,
113.850131613114));
#227121=CARTESIAN_POINT('Ctrl Pts',(0.0307113248932789,7.91095048677443,
113.850639213784));
#227122=CARTESIAN_POINT('Ctrl Pts',(0.0116570841825131,7.9109940112052,
113.851406352323));
#227123=CARTESIAN_POINT('Ctrl Pts',(0.00524360287973972,7.91100086191436,
113.851664905096));
#227124=CARTESIAN_POINT('Ctrl Pts',(-0.00581179448030742,7.91099922706025,
113.852111189915));
#227125=CARTESIAN_POINT('Ctrl Pts',(-0.0104537146909189,7.91099445501144,
113.85229875693));
#227126=CARTESIAN_POINT('Ctrl Pts',(-0.0200369077773404,7.91097616851029,
113.852686366837));
#227127=CARTESIAN_POINT('Ctrl Pts',(-0.0249781774822837,7.91096211006675,
113.852886434102));
#227128=CARTESIAN_POINT('Ctrl Pts',(-0.0369099305279455,7.9109169838234,
113.853370049368));
#227129=CARTESIAN_POINT('Ctrl Pts',(-0.0439003826038125,7.91088127984601,
113.853653807631));
#227130=CARTESIAN_POINT('Ctrl Pts',(-0.0696841907078328,7.91071541146477,
113.85470201851));
#227131=CARTESIAN_POINT('Ctrl Pts',(-0.0884770020701102,7.91052754359945,
113.855469129858));
#227132=CARTESIAN_POINT('Ctrl Pts',(-0.40090984731379,7.90629073550376,
113.86827668661));
#227133=CARTESIAN_POINT('Ctrl Pts',(-0.694063027933667,7.88596175562164,
113.881130812795));
#227134=CARTESIAN_POINT('Ctrl Pts',(-1.58438845386493,7.77419549238371,
113.921550005572));
#227135=CARTESIAN_POINT('Ctrl Pts',(-2.17284410502626,7.63067624980089,
113.950032454192));
#227136=CARTESIAN_POINT('Ctrl Pts',(-3.12075156759568,7.2808091132448,113.995176417622));
#227137=CARTESIAN_POINT('Ctrl Pts',(-3.49083400230011,7.1107953456663,114.012631633916));
#227138=CARTESIAN_POINT('Ctrl Pts',(-3.86654691882151,6.9017589119921,114.030072457503));
#227139=CARTESIAN_POINT('Ctrl Pts',(-3.88680657111852,6.89036979014518,
114.031012164163));
#227140=CARTESIAN_POINT('Ctrl Pts',(-3.91597410871349,6.8738034535794,114.032363999145));
#227141=CARTESIAN_POINT('Ctrl Pts',(-3.92492244188336,6.86869790897473,
114.032778586829));
#227142=CARTESIAN_POINT('Ctrl Pts',(-3.94047888764842,6.85978172562282,
114.033499093715));
#227143=CARTESIAN_POINT('Ctrl Pts',(-3.94709149943844,6.85597898790885,
114.033805284475));
#227144=CARTESIAN_POINT('Ctrl Pts',(-3.95982634105648,6.84863098720405,
114.034394814258));
#227145=CARTESIAN_POINT('Ctrl Pts',(-3.96594933339578,6.84508706558619,
114.034678199114));
#227146=CARTESIAN_POINT('Ctrl Pts',(-3.98040888461964,6.83669211984154,
114.035347266919));
#227147=CARTESIAN_POINT('Ctrl Pts',(-3.98874135087479,6.83183404854993,
114.035732705804));
#227148=CARTESIAN_POINT('Ctrl Pts',(-4.01774923103656,6.81485044707601,
114.037074135406));
#227149=CARTESIAN_POINT('Ctrl Pts',(-4.0383784969098,6.80264614893191,114.038027394298));
#227150=CARTESIAN_POINT('Ctrl Pts',(-4.2863791308345,6.65440298682244,114.049479294935));
#227151=CARTESIAN_POINT('Ctrl Pts',(-4.50684187677284,6.50711272365055,
114.059570954346));
#227152=CARTESIAN_POINT('Ctrl Pts',(-5.23717595321437,5.96422343360179,
114.093108797631));
#227153=CARTESIAN_POINT('Ctrl Pts',(-5.70581632969501,5.51757399025604,
114.114649427063));
#227154=CARTESIAN_POINT('Ctrl Pts',(-6.24129167229568,4.86516230569001,
114.144210619873));
#227155=CARTESIAN_POINT('Ctrl Pts',(-6.36169656723498,4.70662700340428,
114.151287719837));
#227156=CARTESIAN_POINT('Ctrl Pts',(-6.55790251242576,4.42698251285291,
114.16384876517));
#227157=CARTESIAN_POINT('Ctrl Pts',(-6.63663822890178,4.308049372721,114.169213909542));
#227158=CARTESIAN_POINT('Ctrl Pts',(-6.75063307453688,4.12530857840029,
114.177576742986));
#227159=CARTESIAN_POINT('Ctrl Pts',(-6.78829692042551,4.06303356582502,
114.180448362466));
#227160=CARTESIAN_POINT('Ctrl Pts',(-6.83194371453909,3.98856484667433,
114.183900906737));
#227161=CARTESIAN_POINT('Ctrl Pts',(-6.83876255775517,3.97686197026392,
114.18444401212));
#227162=CARTESIAN_POINT('Ctrl Pts',(-6.84921110549794,3.95882325308944,
114.185281905799));
#227163=CARTESIAN_POINT('Ctrl Pts',(-6.85286216801887,3.9524997688279,114.185575772447));
#227164=CARTESIAN_POINT('Ctrl Pts',(-6.85923494263708,3.94142702139087,
114.186090586076));
#227165=CARTESIAN_POINT('Ctrl Pts',(-6.86196049324754,3.93667996567686,
114.186311370902));
#227166=CARTESIAN_POINT('Ctrl Pts',(-6.86810481870518,3.92595270605843,
114.18681046046));
#227167=CARTESIAN_POINT('Ctrl Pts',(-6.87152071200877,3.9199708614996,114.187088884494));
#227168=CARTESIAN_POINT('Ctrl Pts',(-6.88069932929613,3.90384858534741,
114.187839592956));
#227169=CARTESIAN_POINT('Ctrl Pts',(-6.88644743629607,3.89369987838445,
114.188312470227));
#227170=CARTESIAN_POINT('Ctrl Pts',(-6.91172589162478,3.84883783117163,
114.190404103119));
#227171=CARTESIAN_POINT('Ctrl Pts',(-6.93101618851922,3.81399029666978,
114.192032231833));
#227172=CARTESIAN_POINT('Ctrl Pts',(-6.95945928513589,3.76167995516114,
114.194479858436));
#227173=CARTESIAN_POINT('Ctrl Pts',(-6.96881145293289,3.74432591436242,
114.195292452261));
#227174=CARTESIAN_POINT('Ctrl Pts',(-6.98080365893185,3.72187241110995,
114.19634443735));
#227175=CARTESIAN_POINT('Ctrl Pts',(-6.98350318553716,3.71680470654052,
114.19658190811));
#227176=CARTESIAN_POINT('Ctrl Pts',(-7.25257773447291,3.21035466999441,
114.220317695055));
#227177=CARTESIAN_POINT('Ctrl Pts',(-7.46421101672682,2.68175804945603,
114.245273218623));
#227178=CARTESIAN_POINT('Ctrl Pts',(-7.72799653396587,1.74063006208821,
114.28720414022));
#227179=CARTESIAN_POINT('Ctrl Pts',(-7.80775184094904,1.33819215334711,
114.304447118835));
#227180=CARTESIAN_POINT('Ctrl Pts',(-7.8926253055992,0.622299896547812,
114.334199202781));
#227181=CARTESIAN_POINT('Ctrl Pts',(-7.91099712768033,0.31132281523364,
114.346883831773));
#227182=CARTESIAN_POINT('Ctrl Pts',(-7.91100046921692,-0.0508125362661093,
114.361542464529));
#227183=CARTESIAN_POINT('Ctrl Pts',(-7.91050997602132,-0.101697042451125,
114.363598538078));
#227184=CARTESIAN_POINT('Ctrl Pts',(-7.90892569116772,-0.183827639839791,
114.366911308835));
#227185=CARTESIAN_POINT('Ctrl Pts',(-7.90813755703808,-0.215078070272413,
114.368170440797));
#227186=CARTESIAN_POINT('Ctrl Pts',(-7.90640767271903,-0.27060871720694,
114.370405473599));
#227187=CARTESIAN_POINT('Ctrl Pts',(-7.90553924734589,-0.29489078910114,
114.37138198172));
#227188=CARTESIAN_POINT('Ctrl Pts',(-7.90347359279863,-0.346048993979574,
114.373437641103));
#227189=CARTESIAN_POINT('Ctrl Pts',(-7.90225110803007,-0.372923811469791,
114.374516559514));
#227190=CARTESIAN_POINT('Ctrl Pts',(-7.89864173147062,-0.444254149842892,
114.377377677623));
#227191=CARTESIAN_POINT('Ctrl Pts',(-7.89601662118153,-0.488696730055696,
114.379157707979));
#227192=CARTESIAN_POINT('Ctrl Pts',(-7.88146242786094,-0.70417839197012,
114.38777651036));
#227193=CARTESIAN_POINT('Ctrl Pts',(-7.86435017178404,-0.874822803298755,
114.394565005318));
#227194=CARTESIAN_POINT('Ctrl Pts',(-7.79933150743108,-1.36282810323231,
114.413924157409));
#227195=CARTESIAN_POINT('Ctrl Pts',(-7.73764604538597,-1.67800794404747,
114.426351899085));
#227196=CARTESIAN_POINT('Ctrl Pts',(-7.55364373798267,-2.38650791108691,
114.45465010542));
#227197=CARTESIAN_POINT('Ctrl Pts',(-7.41943633296866,-2.77576993859876,
114.470455242708));
#227198=CARTESIAN_POINT('Ctrl Pts',(-7.23868404502707,-3.19173533043536,
114.488530549082));
#227199=CARTESIAN_POINT('Ctrl Pts',(-7.22146232733047,-3.23051124955968,
114.490227592927));
#227200=CARTESIAN_POINT('Ctrl Pts',(-7.19724409067357,-3.28387884023547,
114.49258145412));
#227201=CARTESIAN_POINT('Ctrl Pts',(-7.1905133918184,-3.29859059257909,
114.493232262768));
#227202=CARTESIAN_POINT('Ctrl Pts',(-7.1796826728208,-3.32207336707161,
114.494274252522));
#227203=CARTESIAN_POINT('Ctrl Pts',(-7.17561158635427,-3.33085771232942,
114.494664748293));
#227204=CARTESIAN_POINT('Ctrl Pts',(-7.16720107313771,-3.34891843119276,
114.495469105643));
#227205=CARTESIAN_POINT('Ctrl Pts',(-7.16285973944643,-3.3581938946182,
114.495883013033));
#227206=CARTESIAN_POINT('Ctrl Pts',(-7.15274585166959,-3.3796938532829,
114.496844347737));
#227207=CARTESIAN_POINT('Ctrl Pts',(-7.14695995511448,-3.39191202107821,
114.497392108035));
#227208=CARTESIAN_POINT('Ctrl Pts',(-7.1274692568734,-3.43279954928797,
114.499230129098));
#227209=CARTESIAN_POINT('Ctrl Pts',(-7.11362312090812,-3.46140099088234,
114.500524080103));
#227210=CARTESIAN_POINT('Ctrl Pts',(-7.07964453918537,-3.53052425123799,
114.503670429529));
#227211=CARTESIAN_POINT('Ctrl Pts',(-7.0593360745306,-3.570958193539,114.505526970269));
#227212=CARTESIAN_POINT('Ctrl Pts',(-6.98030617585935,-3.724996727436,114.512657758108));
#227213=CARTESIAN_POINT('Ctrl Pts',(-6.91918074534351,-3.83734437446094,
114.517980038605));
#227214=CARTESIAN_POINT('Ctrl Pts',(-6.64325322131385,-4.31644928591205,
114.54112408142));
#227215=CARTESIAN_POINT('Ctrl Pts',(-6.40181229919149,-4.66704992478172,
114.55917947104));
#227216=CARTESIAN_POINT('Ctrl Pts',(-6.03798316807709,-5.11365739297227,
114.583231000718));
#227217=CARTESIAN_POINT('Ctrl Pts',(-5.9392548849071,-5.22800011441727,
114.589497903788));
#227218=CARTESIAN_POINT('Ctrl Pts',(-5.73509946839674,-5.45119154951351,
114.601951298568));
#227219=CARTESIAN_POINT('Ctrl Pts',(-5.6296974057503,-5.55997874241855,
114.608134961385));
#227220=CARTESIAN_POINT('Ctrl Pts',(-5.4931507360499,-5.69304434150861,
114.615854916244));
#227221=CARTESIAN_POINT('Ctrl Pts',(-5.46486202839355,-5.72020470927214,
114.617439268702));
#227222=CARTESIAN_POINT('Ctrl Pts',(-5.41964247483699,-5.76297898451397,
114.61994856147));
#227223=CARTESIAN_POINT('Ctrl Pts',(-5.40284345820501,-5.77873116709164,
114.620875735899));
#227224=CARTESIAN_POINT('Ctrl Pts',(-5.37134716496034,-5.80800736276362,
114.622604836508));
#227225=CARTESIAN_POINT('Ctrl Pts',(-5.35666699918144,-5.82154949778256,
114.623407046012));
#227226=CARTESIAN_POINT('Ctrl Pts',(-5.32383260523814,-5.85160916203313,
114.625193148465));
#227227=CARTESIAN_POINT('Ctrl Pts',(-5.30565246171449,-5.86809810367799,
114.626176589886));
#227228=CARTESIAN_POINT('Ctrl Pts',(-5.25208407361887,-5.91623085345773,
114.629058449194));
#227229=CARTESIAN_POINT('Ctrl Pts',(-5.21648729321816,-5.94764112760066,
114.6309533053));
#227230=CARTESIAN_POINT('Ctrl Pts',(-4.89860821440357,-6.22308552634251,
114.647702296468));
#227231=CARTESIAN_POINT('Ctrl Pts',(-4.59966312507277,-6.44719047553382,
114.662295929651));
#227232=CARTESIAN_POINT('Ctrl Pts',(-3.98780530654852,-6.84157948303174,
114.690517662134));
#227233=CARTESIAN_POINT('Ctrl Pts',(-3.67699450072474,-7.01352428025668,
114.704039301233));
#227234=CARTESIAN_POINT('Ctrl Pts',(-2.90838226381092,-7.37354820581,114.735989960386));
#227235=CARTESIAN_POINT('Ctrl Pts',(-2.44245500137967,-7.54070850188199,
114.75415341825));
#227236=CARTESIAN_POINT('Ctrl Pts',(-1.79381878329526,-7.70694497782435,
114.779815810314));
#227237=CARTESIAN_POINT('Ctrl Pts',(-1.62223196417972,-7.74487870719792,
114.786648708209));
#227238=CARTESIAN_POINT('Ctrl Pts',(-1.43006646431055,-7.78069553055407,
114.794455046235));
#227239=CARTESIAN_POINT('Ctrl Pts',(-1.41058842887558,-7.78425033694811,
114.795248061723));
#227240=CARTESIAN_POINT('Ctrl Pts',(-1.38227864882495,-7.78930722130641,
114.796403410766));
#227241=CARTESIAN_POINT('Ctrl Pts',(-1.37345729974141,-7.79086749315856,
114.79676380772));
#227242=CARTESIAN_POINT('Ctrl Pts',(-1.35790419708779,-7.79359120441833,
114.797399940862));
#227243=CARTESIAN_POINT('Ctrl Pts',(-1.35117354281084,-7.79476091531577,
114.797675463623));
#227244=CARTESIAN_POINT('Ctrl Pts',(-1.33727320503375,-7.79715809036756,
114.798244976801));
#227245=CARTESIAN_POINT('Ctrl Pts',(-1.33010332842332,-7.79838438693538,
114.798539007233));
#227246=CARTESIAN_POINT('Ctrl Pts',(-1.31177986011599,-7.80149232787706,
114.799291150671));
#227247=CARTESIAN_POINT('Ctrl Pts',(-1.30062392565899,-7.80335993952415,
114.799749755957));
#227248=CARTESIAN_POINT('Ctrl Pts',(-1.25534861128635,-7.81083967913317,
114.801613813791));
#227249=CARTESIAN_POINT('Ctrl Pts',(-1.22119691350172,-7.81625195857195,
114.803026458787));
#227250=CARTESIAN_POINT('Ctrl Pts',(-1.01052729553345,-7.84822397240568,
114.811785888706));
#227251=CARTESIAN_POINT('Ctrl Pts',(-0.833216060158749,-7.86902304349495,
114.81938451316));
#227252=CARTESIAN_POINT('Ctrl Pts',(-0.3765139858485,-7.9069874257473,114.839444543487));
#227253=CARTESIAN_POINT('Ctrl Pts',(-0.0966461626634426,-7.91535594265123,
114.852157377885));
#227254=CARTESIAN_POINT('Ctrl Pts',(0.937484913179871,-7.89141940733783,
114.899502089259));
#227255=CARTESIAN_POINT('Ctrl Pts',(1.68568462350727,-7.76609480531195,
114.934036512435));
#227256=CARTESIAN_POINT('Ctrl Pts',(2.44924172806315,-7.52245361173462,
114.966812755988));
#227257=CARTESIAN_POINT('Ctrl Pts',(2.49351924675345,-7.50789286319354,
114.968706149439));
#227258=CARTESIAN_POINT('Ctrl Pts',(2.55072611703099,-7.48851837192134,
114.971143230204));
#227259=CARTESIAN_POINT('Ctrl Pts',(2.56377469014718,-7.48406109484297,
114.971698492594));
#227260=CARTESIAN_POINT('Ctrl Pts',(2.5845299208604,-7.47691064086798,114.972580718251));
#227261=CARTESIAN_POINT('Ctrl Pts',(2.5922441501592,-7.47423962084607,114.972908404333));
#227262=CARTESIAN_POINT('Ctrl Pts',(2.60608871014328,-7.46942198723165,
114.973496109205));
#227263=CARTESIAN_POINT('Ctrl Pts',(2.61222055198045,-7.46727975748451,
114.973756271118));
#227264=CARTESIAN_POINT('Ctrl Pts',(2.62653787897491,-7.46225804054248,
114.974363410327));
#227265=CARTESIAN_POINT('Ctrl Pts',(2.63472128604847,-7.45937263037536,
114.974710193086));
#227266=CARTESIAN_POINT('Ctrl Pts',(2.65809872577036,-7.45108664477432,
114.975700156336));
#227267=CARTESIAN_POINT('Ctrl Pts',(2.67328105538915,-7.44565305575614,
114.976342251259));
#227268=CARTESIAN_POINT('Ctrl Pts',(2.77002942598582,-7.4106938098248,114.980428737664));
#227269=CARTESIAN_POINT('Ctrl Pts',(2.851123231997,-7.37987416389321,114.983830204505));
#227270=CARTESIAN_POINT('Ctrl Pts',(3.08821746960157,-7.28527509247047,
114.993712601705));
#227271=CARTESIAN_POINT('Ctrl Pts',(3.24270856101847,-7.21783661557888,
115.000070366208));
#227272=CARTESIAN_POINT('Ctrl Pts',(3.57225493447896,-7.06126449634528,
115.013522514855));
#227273=CARTESIAN_POINT('Ctrl Pts',(3.7463834905061,-6.97044309740656,115.020560176763));
#227274=CARTESIAN_POINT('Ctrl Pts',(4.36351771523466,-6.61874711751563,
115.045523529907));
#227275=CARTESIAN_POINT('Ctrl Pts',(4.78419632755308,-6.32135644391238,
115.062505885464));
#227276=CARTESIAN_POINT('Ctrl Pts',(5.45076177937666,-5.74524609382843,
115.093120893189));
#227277=CARTESIAN_POINT('Ctrl Pts',(5.711406248275,-5.4862048937083,115.106318667656));
#227278=CARTESIAN_POINT('Ctrl Pts',(5.96910558537377,-5.19175211594869,
115.121868938784));
#227279=CARTESIAN_POINT('Ctrl Pts',(5.98502505642458,-5.17339217272492,
115.122840685189));
#227280=CARTESIAN_POINT('Ctrl Pts',(6.00565662369404,-5.14937508001318,
115.124115037774));
#227281=CARTESIAN_POINT('Ctrl Pts',(6.01044591369807,-5.14378412398889,
115.124411918834));
#227282=CARTESIAN_POINT('Ctrl Pts',(6.01779918117103,-5.13517572183373,
115.124869383742));
#227283=CARTESIAN_POINT('Ctrl Pts',(6.02036871951092,-5.13216300988515,
115.125029551333));
#227284=CARTESIAN_POINT('Ctrl Pts',(6.02546392776124,-5.12617992830821,
115.125347771049));
#227285=CARTESIAN_POINT('Ctrl Pts',(6.02798966610444,-5.12320961774751,
115.125505817956));
#227286=CARTESIAN_POINT('Ctrl Pts',(6.03355916207464,-5.116649976845,115.125854997987));
#227287=CARTESIAN_POINT('Ctrl Pts',(6.03660191276698,-5.11305979765488,
115.126046207096));
#227288=CARTESIAN_POINT('Ctrl Pts',(6.04529845321364,-5.10278005867984,
115.126593982228));
#227289=CARTESIAN_POINT('Ctrl Pts',(6.05094433659836,-5.09608382495479,
115.12695115145));
#227290=CARTESIAN_POINT('Ctrl Pts',(6.09004190623342,-5.04955603463053,
115.129435390882));
#227291=CARTESIAN_POINT('Ctrl Pts',(6.12311041011407,-5.00940567598472,
115.131591718052));
#227292=CARTESIAN_POINT('Ctrl Pts',(6.16041664094631,-4.96318872376782,
115.134084807249));
#227293=CARTESIAN_POINT('Ctrl Pts',(6.1650454140451,-4.95743790076046,115.134395216588));
#227294=CARTESIAN_POINT('Ctrl Pts',(6.25646955912382,-4.84352577820048,
115.140547420832));
#227295=CARTESIAN_POINT('Ctrl Pts',(6.34041004262891,-4.73311209194905,
115.146574958172));
#227296=CARTESIAN_POINT('Ctrl Pts',(6.70929675339811,-4.2204530329368,115.174608850229));
#227297=CARTESIAN_POINT('Ctrl Pts',(6.9591632550898,-3.79432834520779,115.197960311305));
#227298=CARTESIAN_POINT('Ctrl Pts',(7.32433485857248,-3.01246723627982,
115.237768744965));
#227299=CARTESIAN_POINT('Ctrl Pts',(7.45721630304886,-2.66661001770044,
115.254462095115));
#227300=CARTESIAN_POINT('Ctrl Pts',(7.6245880294134,-2.11909436696631,115.279029475194));
#227301=CARTESIAN_POINT('Ctrl Pts',(7.67631916182465,-1.92328788684706,
115.287471164522));
#227302=CARTESIAN_POINT('Ctrl Pts',(7.72494900949725,-1.7057264475141,115.296477684661));
#227303=CARTESIAN_POINT('Ctrl Pts',(7.7293362380623,-1.68573462943908,115.297301898305));
#227304=CARTESIAN_POINT('Ctrl Pts',(7.73541365628183,-1.65751834239886,
115.298460429486));
#227305=CARTESIAN_POINT('Ctrl Pts',(7.73716839406809,-1.64930795535596,
115.298796972283));
#227306=CARTESIAN_POINT('Ctrl Pts',(7.74019960232129,-1.63501368762621,
115.29938190912));
#227307=CARTESIAN_POINT('Ctrl Pts',(7.74148197679239,-1.6289310745878,115.299630506517));
#227308=CARTESIAN_POINT('Ctrl Pts',(7.74414362495616,-1.61623209796531,
115.300148871166));
#227309=CARTESIAN_POINT('Ctrl Pts',(7.74552159236152,-1.60961546371343,
115.30041859325));
#227310=CARTESIAN_POINT('Ctrl Pts',(7.74876083397874,-1.59396100456534,
115.301055874813));
#227311=CARTESIAN_POINT('Ctrl Pts',(7.75061477999538,-1.58492166342505,
115.30142318172));
#227312=CARTESIAN_POINT('Ctrl Pts',(7.75668470957422,-1.55506096923214,
115.302634319699));
#227313=CARTESIAN_POINT('Ctrl Pts',(7.76083265746889,-1.5342257898421,115.303475809457));
#227314=CARTESIAN_POINT('Ctrl Pts',(7.80436195135305,-1.31088347060548,
115.312458259013));
#227315=CARTESIAN_POINT('Ctrl Pts',(7.8358929832383,-1.10691920188111,115.320324773723));
#227316=CARTESIAN_POINT('Ctrl Pts',(7.87146680556487,-0.796933974362133,
115.331859772975));
#227317=CARTESIAN_POINT('Ctrl Pts',(7.88141221054073,-0.691690605637102,
115.335704055763));
#227318=CARTESIAN_POINT('Ctrl Pts',(7.92519909013768,-0.102472081404216,
115.356889971864));
#227319=CARTESIAN_POINT('Ctrl Pts',(7.91657251543921,0.383626567769483,
115.373017014852));
#227320=CARTESIAN_POINT('Ctrl Pts',(7.81257706791243,1.32808098499041,115.405217440915));
#227321=CARTESIAN_POINT('Ctrl Pts',(7.72103087389865,1.78486438183143,115.421237306732));
#227322=CARTESIAN_POINT('Ctrl Pts',(7.5814368592811,2.25978818781267,115.440804056808));
#227323=CARTESIAN_POINT('Ctrl Pts',(7.5727816181309,2.2886253560514,115.44200402192));
#227324=CARTESIAN_POINT('Ctrl Pts',(7.56174866143145,2.32463658987252,115.443518233396));
#227325=CARTESIAN_POINT('Ctrl Pts',(7.55952489017749,2.3318579561401,115.443822672566));
#227326=CARTESIAN_POINT('Ctrl Pts',(7.55601148934728,2.34320935754085,115.444302490332));
#227327=CARTESIAN_POINT('Ctrl Pts',(7.5547288092541,2.34734154710282,115.444477419813));
#227328=CARTESIAN_POINT('Ctrl Pts',(7.55235105870395,2.35497940012985,115.444801241424));
#227329=CARTESIAN_POINT('Ctrl Pts',(7.55125693327885,2.35848536490217,115.444950072884));
#227330=CARTESIAN_POINT('Ctrl Pts',(7.54882640371201,2.36625461187455,115.445280302166));
#227331=CARTESIAN_POINT('Ctrl Pts',(7.54748882951831,2.3705175236068,115.445461774653));
#227332=CARTESIAN_POINT('Ctrl Pts',(7.5436587975669,2.38268791211798,115.445980660677));
#227333=CARTESIAN_POINT('Ctrl Pts',(7.54115752588845,2.39059258539437,115.446318632273));
#227334=CARTESIAN_POINT('Ctrl Pts',(7.52525967482702,2.44056072077617,115.448461039643));
#227335=CARTESIAN_POINT('Ctrl Pts',(7.51152388379876,2.48251457098658,115.450286620838));
#227336=CARTESIAN_POINT('Ctrl Pts',(7.46912290988269,2.60844743199752,115.455842432686));
#227337=CARTESIAN_POINT('Ctrl Pts',(7.43939589865643,2.69205917474495,115.459633388966));
#227338=CARTESIAN_POINT('Ctrl Pts',(7.34878770878699,2.93393795262027,115.470861755087));
#227339=CARTESIAN_POINT('Ctrl Pts',(7.28421851391765,3.09076490238342,115.478471561948));
#227340=CARTESIAN_POINT('Ctrl Pts',(7.06360205280373,3.58120665738194,115.503058170901));
#227341=CARTESIAN_POINT('Ctrl Pts',(6.88928045816948,3.90606218817292,115.520512853899));
#227342=CARTESIAN_POINT('Ctrl Pts',(6.44984367420417,4.60341273534195,115.559146806795));
#227343=CARTESIAN_POINT('Ctrl Pts',(6.17378840619966,4.96752538413764,115.580117856845));
#227344=CARTESIAN_POINT('Ctrl Pts',(5.71213461696114,5.47807950511128,115.609922011658));
#227345=CARTESIAN_POINT('Ctrl Pts',(5.54888647996662,5.64337740120692,115.619659140253));
#227346=CARTESIAN_POINT('Ctrl Pts',(5.36252565471285,5.81616021112204,115.629950841878));
#227347=CARTESIAN_POINT('Ctrl Pts',(5.34639762526163,5.83098906206626,115.630835126201));
#227348=CARTESIAN_POINT('Ctrl Pts',(5.32366395247655,5.85171782919558,115.632072721508));
#227349=CARTESIAN_POINT('Ctrl Pts',(5.3171097627054,5.85767387308551,115.632428496));
#227350=CARTESIAN_POINT('Ctrl Pts',(5.30572040596201,5.86798895305928,115.633044956603));
#227351=CARTESIAN_POINT('Ctrl Pts',(5.30088984063395,5.87235304432713,115.633305863545));
#227352=CARTESIAN_POINT('Ctrl Pts',(5.29082975811026,5.88141912526233,115.633848080099));
#227353=CARTESIAN_POINT('Ctrl Pts',(5.28559934546498,5.88612011565128,115.634129346137));
#227354=CARTESIAN_POINT('Ctrl Pts',(5.27327303863231,5.89716907575898,115.634790689271));
#227355=CARTESIAN_POINT('Ctrl Pts',(5.26617193218292,5.90351122888612,115.635170513975));
#227356=CARTESIAN_POINT('Ctrl Pts',(5.24294311845491,5.92418212675156,115.636409174016));
#227357=CARTESIAN_POINT('Ctrl Pts',(5.2267681802668,5.93845778074769,115.637265718514));
#227358=CARTESIAN_POINT('Ctrl Pts',(4.90890585901931,6.21669150221918,115.653982543674));
#227359=CARTESIAN_POINT('Ctrl Pts',(4.58763028114866,6.45742226445213,115.668805236461));
#227360=CARTESIAN_POINT('Ctrl Pts',(3.84874103221612,6.92797366636466,115.699914436927));
#227361=CARTESIAN_POINT('Ctrl Pts',(3.42585608702336,7.14654630848013,115.715891152156));
#227362=CARTESIAN_POINT('Ctrl Pts',(2.65945964723125,7.45891946632256,115.744974653488));
#227363=CARTESIAN_POINT('Ctrl Pts',(2.32446287689067,7.57001238927081,115.757778891481));
#227364=CARTESIAN_POINT('Ctrl Pts',(1.95338339815199,7.6661046700647,115.772993485803));
#227365=CARTESIAN_POINT('Ctrl Pts',(1.92355587959227,7.67364321910505,115.774222301238));
#227366=CARTESIAN_POINT('Ctrl Pts',(1.88366756217731,7.68347733601705,115.775872834761));
#227367=CARTESIAN_POINT('Ctrl Pts',(1.87364489326573,7.68592754783054,115.776288170449));
#227368=CARTESIAN_POINT('Ctrl Pts',(1.85799114219552,7.68972193458691,115.776937781258));
#227369=CARTESIAN_POINT('Ctrl Pts',(1.85236330768408,7.6910795530839,115.777171515743));
#227370=CARTESIAN_POINT('Ctrl Pts',(1.84108768430507,7.6937865097095,115.777640181255));
#227371=CARTESIAN_POINT('Ctrl Pts',(1.83543989002038,7.69513580959907,115.777875113618));
#227372=CARTESIAN_POINT('Ctrl Pts',(1.82270017870578,7.69816459778535,115.77840545977));
#227373=CARTESIAN_POINT('Ctrl Pts',(1.81560742108134,7.69984050536865,115.778701013114));
#227374=CARTESIAN_POINT('Ctrl Pts',(1.79601233838172,7.70444193614334,115.779518310111));
#227375=CARTESIAN_POINT('Ctrl Pts',(1.78350522149186,7.70734681907788,115.780040843859));
#227376=CARTESIAN_POINT('Ctrl Pts',(1.69848191329918,7.72687615818212,115.783598731874));
#227377=CARTESIAN_POINT('Ctrl Pts',(1.62574269991136,7.74250710207346,115.786670737522));
#227378=CARTESIAN_POINT('Ctrl Pts',(1.39330975624231,7.78903484342039,115.796558288458));
#227379=CARTESIAN_POINT('Ctrl Pts',(1.23288190322035,7.81603320176458,115.803488669266));
#227380=CARTESIAN_POINT('Ctrl Pts',(0.644976039080087,7.89642074702735,
115.829072779577));
#227381=CARTESIAN_POINT('Ctrl Pts',(0.214158742873291,7.91982289611658,
115.848137723667));
#227382=CARTESIAN_POINT('Ctrl Pts',(-0.4142838620456,7.90262418194324,115.875459685748));
#227383=CARTESIAN_POINT('Ctrl Pts',(-0.611877672184438,7.88978511101164,
115.883987302897));
#227384=CARTESIAN_POINT('Ctrl Pts',(-1.11963246733086,7.83760105803829,
115.90568466056));
#227385=CARTESIAN_POINT('Ctrl Pts',(-1.42832365770927,7.78726365027231,
115.918657643377));
#227386=CARTESIAN_POINT('Ctrl Pts',(-1.76737409262188,7.71113050203308,
115.932728466672));
#227387=CARTESIAN_POINT('Ctrl Pts',(-1.80145605158341,7.70323963795825,
115.934141072386));
#227388=CARTESIAN_POINT('Ctrl Pts',(-1.85209442092933,7.69116108510853,
115.936237282013));
#227389=CARTESIAN_POINT('Ctrl Pts',(-1.86869136720885,7.68714544924807,
115.936923897418));
#227390=CARTESIAN_POINT('Ctrl Pts',(-1.89711651343863,7.68017047944249,
115.938099106876));
#227391=CARTESIAN_POINT('Ctrl Pts',(-1.9089510932208,7.67723748385643,115.938588176066));
#227392=CARTESIAN_POINT('Ctrl Pts',(-1.93325217684861,7.67115521617233,
115.939591975422));
#227393=CARTESIAN_POINT('Ctrl Pts',(-1.94571788080572,7.66800288597811,
115.940106647775));
#227394=CARTESIAN_POINT('Ctrl Pts',(-1.97030940848329,7.66172034641187,
115.941121473797));
#227395=CARTESIAN_POINT('Ctrl Pts',(-1.98243559403818,7.65859170790232,
115.941621655067));
#227396=CARTESIAN_POINT('Ctrl Pts',(-2.01033869523115,7.65132180668212,
115.942772065033));
#227397=CARTESIAN_POINT('Ctrl Pts',(-2.0261103484449,7.64716051337231,115.943421913879));
#227398=CARTESIAN_POINT('Ctrl Pts',(-2.11003254448707,7.62474009655097,
115.946877705694));
#227399=CARTESIAN_POINT('Ctrl Pts',(-2.17795000157489,7.60561850654065,
115.949667001964));
#227400=CARTESIAN_POINT('Ctrl Pts',(-2.35064869761054,7.55449358164935,
115.956741737866));
#227401=CARTESIAN_POINT('Ctrl Pts',(-2.45503826509474,7.52121734984968,
115.961001091233));
#227402=CARTESIAN_POINT('Ctrl Pts',(-2.82084914964607,7.39618006234371,
115.975882508051));
#227403=CARTESIAN_POINT('Ctrl Pts',(-3.07811094143381,7.29286715493864,
115.986257694316));
#227404=CARTESIAN_POINT('Ctrl Pts',(-3.53236907042016,7.08211398175384,
116.004707874759));
#227405=CARTESIAN_POINT('Ctrl Pts',(-3.73122345337743,6.97939414065008,
116.012835405181));
#227406=CARTESIAN_POINT('Ctrl Pts',(-4.2607608151437,6.676749982985,116.035016948536));
#227407=CARTESIAN_POINT('Ctrl Pts',(-4.58156305601182,6.46082964463733,
116.049039398213));
#227408=CARTESIAN_POINT('Ctrl Pts',(-4.95707818367383,6.16600567789951,
116.067524435051));
#227409=CARTESIAN_POINT('Ctrl Pts',(-5.02787918340899,6.10841061142607,
116.071110021645));
#227410=CARTESIAN_POINT('Ctrl Pts',(-5.10822900128518,6.04070428617413,
116.075315419447));
#227411=CARTESIAN_POINT('Ctrl Pts',(-5.11876863511714,6.03177581308082,
116.075869800701));
#227412=CARTESIAN_POINT('Ctrl Pts',(-5.13434742505062,6.01850826523902,
116.076693412202));
#227413=CARTESIAN_POINT('Ctrl Pts',(-5.13940461769222,6.01419033579106,
116.07696142748));
#227414=CARTESIAN_POINT('Ctrl Pts',(-5.14837196697733,6.00651426836845,
116.077437842975));
#227415=CARTESIAN_POINT('Ctrl Pts',(-5.15228430176099,6.00315867190863,
116.077646094546));
#227416=CARTESIAN_POINT('Ctrl Pts',(-5.16048215338354,5.99611348486725,
116.078083303486));
#227417=CARTESIAN_POINT('Ctrl Pts',(-5.16476699766767,5.99242311910205,
116.078312306806));
#227418=CARTESIAN_POINT('Ctrl Pts',(-5.17343162351136,5.98494442504219,
116.07877637497));
#227419=CARTESIAN_POINT('Ctrl Pts',(-5.17781120930317,5.98115587612727,
116.079011453085));
#227420=CARTESIAN_POINT('Ctrl Pts',(-5.18857665790152,5.97182256842947,
116.079590570088));
#227421=CARTESIAN_POINT('Ctrl Pts',(-5.19495778629881,5.96627238076075,
116.079934940573));
#227422=CARTESIAN_POINT('Ctrl Pts',(-5.25904919593762,5.91034608013402,
116.083405018026));
#227423=CARTESIAN_POINT('Ctrl Pts',(-5.31602874442575,5.85914895132501,
116.086584565166));
#227424=CARTESIAN_POINT('Ctrl Pts',(-5.54270233925726,5.64945023392989,
116.099607814317));
#227425=CARTESIAN_POINT('Ctrl Pts',(-5.70611451665905,5.48434872308587,
116.109848377242));
#227426=CARTESIAN_POINT('Ctrl Pts',(-5.9717239372144,5.19125459972362,116.127680049546));
#227427=CARTESIAN_POINT('Ctrl Pts',(-6.07765080057738,5.06683034454545,
116.135153206328));
#227428=CARTESIAN_POINT('Ctrl Pts',(-6.55156443883811,4.47389869719932,
116.170057294602));
#227429=CARTESIAN_POINT('Ctrl Pts',(-6.86977708828372,3.9680049032834,116.197694417281));
#227430=CARTESIAN_POINT('Ctrl Pts',(-7.14033791464335,3.40591840761649,
116.22467221222));
#227431=CARTESIAN_POINT('Ctrl Pts',(-7.15235368251749,3.38061274829772,
116.225879766427));
#227432=CARTESIAN_POINT('Ctrl Pts',(-7.25694358293501,3.15728869501609,
116.236474574776));
#227433=CARTESIAN_POINT('Ctrl Pts',(-7.34141195291808,2.95556800409414,
116.245613599181));
#227434=CARTESIAN_POINT('Ctrl Pts',(-7.42471026007466,2.73094086926193,
116.255332104383));
#227435=CARTESIAN_POINT('Ctrl Pts',(-7.43192106652402,2.71125611974983,
116.25618001467));
#227436=CARTESIAN_POINT('Ctrl Pts',(-7.442502820251,2.68200961042053,116.2574342728));
#227437=CARTESIAN_POINT('Ctrl Pts',(-7.44593374286168,2.67246973372288,
116.257842528636));
#227438=CARTESIAN_POINT('Ctrl Pts',(-7.45177158504158,2.65613876814522,
116.258539927045));
#227439=CARTESIAN_POINT('Ctrl Pts',(-7.45418757906757,2.64935094838669,
116.258829357858));
#227440=CARTESIAN_POINT('Ctrl Pts',(-7.45886631476097,2.63614881250399,
116.259391447375));
#227441=CARTESIAN_POINT('Ctrl Pts',(-7.46113006359658,2.62973486069258,
116.2596641379));
#227442=CARTESIAN_POINT('Ctrl Pts',(-7.46651907194479,2.61440303771855,
116.260315050352));
#227443=CARTESIAN_POINT('Ctrl Pts',(-7.46963663348633,2.60548246199862,
116.260693027836));
#227444=CARTESIAN_POINT('Ctrl Pts',(-7.47891497420166,2.57877993637777,
116.261822231897));
#227445=CARTESIAN_POINT('Ctrl Pts',(-7.48502831331312,2.56098151233283,
116.262571955318));
#227446=CARTESIAN_POINT('Ctrl Pts',(-7.53686705025708,2.40828651131292,
116.268978972365));
#227447=CARTESIAN_POINT('Ctrl Pts',(-7.57900629934637,2.27219603766529,
116.274521986621));
#227448=CARTESIAN_POINT('Ctrl Pts',(-7.71591282562359,1.78373693304042,
116.293881111327));
#227449=CARTESIAN_POINT('Ctrl Pts',(-7.78996080841559,1.42603134276949,
116.307056744525));
#227450=CARTESIAN_POINT('Ctrl Pts',(-7.88696644315222,0.711657536121887,
116.332372618769));
#227451=CARTESIAN_POINT('Ctrl Pts',(-7.91100122708638,0.356016607322614,
116.344506208184));
#227452=CARTESIAN_POINT('Ctrl Pts',(-7.91099999995301,-2.72658871074832E-5,
116.356884209101));
#227453=CARTESIAN_POINT('',(-7.91099986567554,0.00144650702262969,118.357610289563));
#227454=CARTESIAN_POINT('Ctrl Pts',(-7.911,-1.68698388591793E-12,116.357668491763));
#227455=CARTESIAN_POINT('Ctrl Pts',(-7.91099999999953,-2.20167589666848,
116.446255927496));
#227456=CARTESIAN_POINT('Ctrl Pts',(-6.94214576672275,-4.38610418338837,
116.534843363229));
#227457=CARTESIAN_POINT('Ctrl Pts',(-3.67820201488119,-7.34180684107717,
116.712018234694));
#227458=CARTESIAN_POINT('Ctrl Pts',(-1.40868175871556,-8.0899266657137,
116.800605670427));
#227459=CARTESIAN_POINT('Ctrl Pts',(2.97309270521457,-7.65454228025186,
116.977780541892));
#227460=CARTESIAN_POINT('Ctrl Pts',(5.0510207267576,-6.47444880834103,117.066367977625));
#227461=CARTESIAN_POINT('Ctrl Pts',(7.66951518847946,-2.93425195367516,
117.24354284909));
#227462=CARTESIAN_POINT('Ctrl Pts',(8.18956872247087,-0.60188196009709,
117.332130284823));
#227463=CARTESIAN_POINT('Ctrl Pts',(7.32306689761247,3.71537198232641,117.509305156289));
#227464=CARTESIAN_POINT('Ctrl Pts',(5.94329958850052,5.66643518936668,117.597892592021));
#227465=CARTESIAN_POINT('Ctrl Pts',(2.16154501637633,7.92205913233057,117.775067463487));
#227466=CARTESIAN_POINT('Ctrl Pts',(-0.210816529302626,8.20894963712997,
117.863654899219));
#227467=CARTESIAN_POINT('Ctrl Pts',(-4.42123908576632,6.91982244717707,
118.040829770685));
#227468=CARTESIAN_POINT('Ctrl Pts',(-6.22631625634341,5.35390358803343,
118.129417206418));
#227469=CARTESIAN_POINT('Ctrl Pts',(-7.6529679718098,2.31378507137994,118.264539857955));
#227470=CARTESIAN_POINT('Ctrl Pts',(-7.91078507045206,1.15799210747852,
118.311075073758));
#227471=CARTESIAN_POINT('Ctrl Pts',(-7.91099986567554,0.00144650702262969,
118.357610289563));
#227472=CARTESIAN_POINT('',(-7.90626572818492,0.00396378192042368,120.357668491763));
#227473=CARTESIAN_POINT('Ctrl Pts',(-7.91099986706751,0.00145026131998307,
118.357704282581));
#227474=CARTESIAN_POINT('Ctrl Pts',(-7.91103615013821,-0.196469495286411,
118.36570021141));
#227475=CARTESIAN_POINT('Ctrl Pts',(-7.90364072243202,-0.394584910582694,
118.37369614024));
#227476=CARTESIAN_POINT('Ctrl Pts',(-7.888795715768,-0.592303262594768,
118.381692069069));
#227477=CARTESIAN_POINT('Ctrl Pts',(-7.87396372149712,-0.789848304551604,
118.389680989066));
#227478=CARTESIAN_POINT('Ctrl Pts',(-7.85169518682542,-0.986996644197289,
118.397669909062));
#227479=CARTESIAN_POINT('Ctrl Pts',(-7.82202428542851,-1.18315555958067,
118.405658829059));
#227480=CARTESIAN_POINT('Ctrl Pts',(-7.79237432198154,-1.37917605094059,
118.413642111492));
#227481=CARTESIAN_POINT('Ctrl Pts',(-7.75533245337266,-1.57420817929061,
118.421625393924));
#227482=CARTESIAN_POINT('Ctrl Pts',(-7.71098470962028,-1.76766394091248,
118.429608676357));
#227483=CARTESIAN_POINT('Ctrl Pts',(-7.66666068619764,-1.96101622862415,
118.437587688762));
#227484=CARTESIAN_POINT('Ctrl Pts',(-7.61503865223227,-2.15279350427088,
118.445566701167));
#227485=CARTESIAN_POINT('Ctrl Pts',(-7.5562558740262,-2.34241716315532,
118.453545713572));
#227486=CARTESIAN_POINT('Ctrl Pts',(-7.49749132357651,-2.53198202226942,
118.461522251791));
#227487=CARTESIAN_POINT('Ctrl Pts',(-7.43157055276323,-2.71939427544401,
118.469498790011));
#227488=CARTESIAN_POINT('Ctrl Pts',(-7.35868104682497,-2.90408922919027,
118.477475328231));
#227489=CARTESIAN_POINT('Ctrl Pts',(-7.28580243285818,-3.08875658373496,
118.485450674506));
#227490=CARTESIAN_POINT('Ctrl Pts',(-7.20595728206472,-3.27070713624327,
118.493426020781));
#227491=CARTESIAN_POINT('Ctrl Pts',(-7.11938184059797,-3.44939461467716,
118.501401367056));
#227492=CARTESIAN_POINT('Ctrl Pts',(-7.03280593132814,-3.62808305863376,
118.509376756426));
#227493=CARTESIAN_POINT('Ctrl Pts',(-6.93949980539527,-3.80350809174866,
118.517352145795));
#227494=CARTESIAN_POINT('Ctrl Pts',(-6.83974659367512,-3.97514622804113,
118.525327535165));
#227495=CARTESIAN_POINT('Ctrl Pts',(-6.73997739799885,-4.14681186677078,
118.533304202471));
#227496=CARTESIAN_POINT('Ctrl Pts',(-6.63375922651977,-4.31468910969268,
118.541280869777));
#227497=CARTESIAN_POINT('Ctrl Pts',(-6.52141981929608,-4.47828142712049,
118.549257537083));
#227498=CARTESIAN_POINT('Ctrl Pts',(-6.40900368710289,-4.64198547395719,
118.55723965225));
#227499=CARTESIAN_POINT('Ctrl Pts',(-6.29045815669429,-4.80139847184263,
118.565221767418));
#227500=CARTESIAN_POINT('Ctrl Pts',(-6.1661533379606,-4.95605427863309,
118.573203882585));
#227501=CARTESIAN_POINT('Ctrl Pts',(-6.04180093508365,-5.1107692879882,
118.581189053323));
#227502=CARTESIAN_POINT('Ctrl Pts',(-5.91168506425132,-5.26072321916806,
118.589174224061));
#227503=CARTESIAN_POINT('Ctrl Pts',(-5.77621472687111,-5.40548466181131,
118.597159394799));
#227504=CARTESIAN_POINT('Ctrl Pts',(-5.64061596056753,-5.55038334155446,
118.605152135659));
#227505=CARTESIAN_POINT('Ctrl Pts',(-5.49965282233508,-5.69007946015305,
118.613144876518));
#227506=CARTESIAN_POINT('Ctrl Pts',(-5.35377039212665,-5.82417922014665,
118.621137617377));
#227507=CARTESIAN_POINT('Ctrl Pts',(-5.28623242659609,-5.88626226164222,
118.624837949596));
#227508=CARTESIAN_POINT('Ctrl Pts',(-5.21764055852171,-5.94714638170074,
118.628538281814));
#227509=CARTESIAN_POINT('Ctrl Pts',(-5.14804124519898,-6.00679551322751,
118.632238614033));
#227510=CARTESIAN_POINT('Ctrl Pts',(-5.00080503293966,-6.1329822781721,
118.640066606494));
#227511=CARTESIAN_POINT('Ctrl Pts',(-4.84874534686315,-6.2539074889938,
118.647894598955));
#227512=CARTESIAN_POINT('Ctrl Pts',(-4.69227874488835,-6.36917900362904,
118.655722591416));
#227513=CARTESIAN_POINT('Ctrl Pts',(-4.53594429727526,-6.48435315797622,
118.663543972221));
#227514=CARTESIAN_POINT('Ctrl Pts',(-4.37521062660918,-6.59388291674253,
118.671365353027));
#227515=CARTESIAN_POINT('Ctrl Pts',(-4.21052892568385,-6.69741496145935,
118.679186733832));
#227516=CARTESIAN_POINT('Ctrl Pts',(-4.04595723588101,-6.8008778444151,
118.687002889776));
#227517=CARTESIAN_POINT('Ctrl Pts',(-3.87744306508657,-6.89835080592899,
118.694819045721));
#227518=CARTESIAN_POINT('Ctrl Pts',(-3.70546840147755,-6.98952251056189,
118.702635201666));
#227519=CARTESIAN_POINT('Ctrl Pts',(-3.53357635514205,-7.08065041596588,
118.7104476027));
#227520=CARTESIAN_POINT('Ctrl Pts',(-3.35822743780163,-7.16548292961773,
118.718260003734));
#227521=CARTESIAN_POINT('Ctrl Pts',(-3.17993031807008,-7.24375345882359,
118.726072404768));
#227522=CARTESIAN_POINT('Ctrl Pts',(-3.0016853126272,-7.32200111041393,
118.733882522323));
#227523=CARTESIAN_POINT('Ctrl Pts',(-2.82049414387768,-7.39369045760067,
118.741692639879));
#227524=CARTESIAN_POINT('Ctrl Pts',(-2.63688779715974,-7.45860199670086,
118.749502757434));
#227525=CARTESIAN_POINT('Ctrl Pts',(-2.45327098909801,-7.52351723426757,
118.757313319986));
#227526=CARTESIAN_POINT('Ctrl Pts',(-2.26723905805088,-7.58165376865885,
118.765123882539));
#227527=CARTESIAN_POINT('Ctrl Pts',(-2.07934100134186,-7.6328410176119,
118.772934445091));
#227528=CARTESIAN_POINT('Ctrl Pts',(-1.93292631490113,-7.67272735351387,
118.779020623347));
#227529=CARTESIAN_POINT('Ctrl Pts',(-1.78537894391127,-7.70839511676152,
118.785106801602));
#227530=CARTESIAN_POINT('Ctrl Pts',(-1.63696420259712,-7.73978482901273,
118.791192979858));
#227531=CARTESIAN_POINT('Ctrl Pts',(-1.42626421463101,-7.78434786860722,
118.799833345861));
#227532=CARTESIAN_POINT('Ctrl Pts',(-1.21391627437396,-7.82026636386086,
118.808473711865));
#227533=CARTESIAN_POINT('Ctrl Pts',(-1.00061366223356,-7.84746413174036,
118.817114077868));
#227534=CARTESIAN_POINT('Ctrl Pts',(-0.786956223196841,-7.87470714285185,
118.825768817039));
#227535=CARTESIAN_POINT('Ctrl Pts',(-0.572341165909358,-7.89320040003454,
118.83442355621));
#227536=CARTESIAN_POINT('Ctrl Pts',(-0.357465618056908,-7.9029196713561,
118.843078295381));
#227537=CARTESIAN_POINT('Ctrl Pts',(-0.135944202772329,-7.91293954918866,
118.85200071624));
#227538=CARTESIAN_POINT('Ctrl Pts',(0.0858537942406949,-7.91363406139319,
118.860923137098));
#227539=CARTESIAN_POINT('Ctrl Pts',(0.30716799939464,-7.90503439715147,
118.869845557957));
#227540=CARTESIAN_POINT('Ctrl Pts',(0.522562911823992,-7.89666474042302,
118.87852933882));
#227541=CARTESIAN_POINT('Ctrl Pts',(0.73749935952798,-7.87949171753001,
118.887213119683));
#227542=CARTESIAN_POINT('Ctrl Pts',(0.951283084827622,-7.85359672331861,
118.895896900546));
#227543=CARTESIAN_POINT('Ctrl Pts',(1.17387933338185,-7.8266342940705,118.904938641402));
#227544=CARTESIAN_POINT('Ctrl Pts',(1.39522553407994,-7.79021568625419,
118.913980382258));
#227545=CARTESIAN_POINT('Ctrl Pts',(1.61454958687192,-7.74449163157478,
118.923022123114));
#227546=CARTESIAN_POINT('Ctrl Pts',(1.8338736396639,-7.69876757689536,118.93206386397));
#227547=CARTESIAN_POINT('Ctrl Pts',(2.05117527929417,-7.64373816321146,
118.941105604826));
#227548=CARTESIAN_POINT('Ctrl Pts',(2.26569821988195,-7.57961295690115,
118.950147345682));
#227549=CARTESIAN_POINT('Ctrl Pts',(2.46314455284439,-7.52059229085145,
118.958469339455));
#227550=CARTESIAN_POINT('Ctrl Pts',(2.65840469216121,-7.45381611622113,
118.966791333227));
#227551=CARTESIAN_POINT('Ctrl Pts',(2.85086500626089,-7.37946405344433,
118.975113327));
#227552=CARTESIAN_POINT('Ctrl Pts',(3.04315414282958,-7.30517812067772,
118.983427919047));
#227553=CARTESIAN_POINT('Ctrl Pts',(3.23264815010936,-7.22332984657303,
118.991742511094));
#227554=CARTESIAN_POINT('Ctrl Pts',(3.41874968624922,-7.13414827311368,
119.000057103142));
#227555=CARTESIAN_POINT('Ctrl Pts',(3.60469704984099,-7.04504058056206,
119.008364807111));
#227556=CARTESIAN_POINT('Ctrl Pts',(3.78725728609806,-6.94861183441135,
119.016672511081));
#227557=CARTESIAN_POINT('Ctrl Pts',(3.96585334813195,-6.84513902131364,
119.024980215051));
#227558=CARTESIAN_POINT('Ctrl Pts',(4.14426921478889,-6.74177060762063,
119.033279536921));
#227559=CARTESIAN_POINT('Ctrl Pts',(4.31872863852634,-6.63137245959264,
119.041578858792));
#227560=CARTESIAN_POINT('Ctrl Pts',(4.48867913574803,-6.51426746582456,
119.049878180663));
#227561=CARTESIAN_POINT('Ctrl Pts',(4.65852105146005,-6.39723729053139,
119.05817220009));
#227562=CARTESIAN_POINT('Ctrl Pts',(4.82385954666406,-6.27350898213789,
119.066466219518));
#227563=CARTESIAN_POINT('Ctrl Pts',(4.98416987967236,-6.1434494879153,119.074760238945));
#227564=CARTESIAN_POINT('Ctrl Pts',(5.14436133459422,-6.0134864392774,119.083048107945));
#227565=CARTESIAN_POINT('Ctrl Pts',(5.29953184239586,-5.87720175880035,
119.091335976944));
#227566=CARTESIAN_POINT('Ctrl Pts',(5.44918817656425,-5.73500385495881,
119.099623845943));
#227567=CARTESIAN_POINT('Ctrl Pts',(5.50623631990744,-5.68079882283283,
119.102783134465));
#227568=CARTESIAN_POINT('Ctrl Pts',(5.5624835365847,-5.62573496996465,119.105942422986));
#227569=CARTESIAN_POINT('Ctrl Pts',(5.61790377792052,-5.56983645559062,
119.109101711507));
#227570=CARTESIAN_POINT('Ctrl Pts',(5.76003450226718,-5.42647915243961,
119.117204021334));
#227571=CARTESIAN_POINT('Ctrl Pts',(5.89666373218884,-5.27768970130891,
119.12530633116));
#227572=CARTESIAN_POINT('Ctrl Pts',(6.02738087567515,-5.12392435341755,
119.133408640987));
#227573=CARTESIAN_POINT('Ctrl Pts',(6.15812687151884,-4.97012506588636,
119.141512739184));
#227574=CARTESIAN_POINT('Ctrl Pts',(6.28295797178841,-4.81134793413588,
119.149616837381));
#227575=CARTESIAN_POINT('Ctrl Pts',(6.40150390790828,-4.64808226229216,
119.157720935579));
#227576=CARTESIAN_POINT('Ctrl Pts',(6.5200908800299,-4.48476007420997,119.1658278391));
#227577=CARTESIAN_POINT('Ctrl Pts',(6.63238816147137,-4.31694650514095,
119.173934742622));
#227578=CARTESIAN_POINT('Ctrl Pts',(6.73806852270149,-4.14516026027696,
119.182041646144));
#227579=CARTESIAN_POINT('Ctrl Pts',(6.84384419164315,-3.97321909018674,
119.190155860867));
#227580=CARTESIAN_POINT('Ctrl Pts',(6.94299084829057,-3.79729835673636,
119.19827007559));
#227581=CARTESIAN_POINT('Ctrl Pts',(7.03522632795049,-3.61794299492299,
119.206384290313));
#227582=CARTESIAN_POINT('Ctrl Pts',(7.12750688606164,-3.43849997636449,
119.214502470715));
#227583=CARTESIAN_POINT('Ctrl Pts',(7.21286939000608,-3.25561926761517,
119.222620651116));
#227584=CARTESIAN_POINT('Ctrl Pts',(7.2910792737547,-3.0698671019809,119.230738831517));
#227585=CARTESIAN_POINT('Ctrl Pts',(7.36937326486342,-2.88391517739631,
119.238865742257));
#227586=CARTESIAN_POINT('Ctrl Pts',(7.44049914825659,-2.6950859220191,119.246992652996));
#227587=CARTESIAN_POINT('Ctrl Pts',(7.50427133008208,-2.50396341916333,
119.255119563735));
#227588=CARTESIAN_POINT('Ctrl Pts',(7.53810910369348,-2.40255305811633,
119.259431734934));
#227589=CARTESIAN_POINT('Ctrl Pts',(7.56987735906151,-2.30049729704032,
119.263743906133));
#227590=CARTESIAN_POINT('Ctrl Pts',(7.59955416871206,-2.19788476422472,
119.268056077332));
#227591=CARTESIAN_POINT('Ctrl Pts',(7.65459577772019,-2.00756919536555,
119.276053865636));
#227592=CARTESIAN_POINT('Ctrl Pts',(7.7025354397237,-1.81500738908132,119.284051653939));
#227593=CARTESIAN_POINT('Ctrl Pts',(7.74319318408437,-1.62076534820726,
119.292049442243));
#227594=CARTESIAN_POINT('Ctrl Pts',(7.78381773144638,-1.4266819057225,119.300040700362));
#227595=CARTESIAN_POINT('Ctrl Pts',(7.81717214194644,-1.23092128852819,
119.308031958481));
#227596=CARTESIAN_POINT('Ctrl Pts',(7.84312649034786,-1.03406375838421,
119.3160232166));
#227597=CARTESIAN_POINT('Ctrl Pts',(7.86906404820023,-0.83733358054227,
119.324009304964));
#227598=CARTESIAN_POINT('Ctrl Pts',(7.88761104186485,-0.639508234683549,
119.331995393329));
#227599=CARTESIAN_POINT('Ctrl Pts',(7.89868870566191,-0.441177663814656,
119.339981481693));
#227600=CARTESIAN_POINT('Ctrl Pts',(7.90976108068653,-0.242941781255309,
119.347963757286));
#227601=CARTESIAN_POINT('Ctrl Pts',(7.9133712155375,-0.0442014878576724,
119.355946032879));
#227602=CARTESIAN_POINT('Ctrl Pts',(7.9094921921131,0.154448253152782,119.363928308471));
#227603=CARTESIAN_POINT('Ctrl Pts',(7.90561436336275,0.353036813379822,
119.371908125657));
#227604=CARTESIAN_POINT('Ctrl Pts',(7.8942519812414,0.551534542692189,119.379887942843));
#227605=CARTESIAN_POINT('Ctrl Pts',(7.87543023136269,0.749346162289925,
119.387867760029));
#227606=CARTESIAN_POINT('Ctrl Pts',(7.85596167180673,0.953955580745488,
119.396121803735));
#227607=CARTESIAN_POINT('Ctrl Pts',(7.82851195718458,1.15783052104527,119.404375847442));
#227608=CARTESIAN_POINT('Ctrl Pts',(7.79316744696654,1.36031692760952,119.412629891148));
#227609=CARTESIAN_POINT('Ctrl Pts',(7.75899257665929,1.55610254298873,119.420610787514));
#227610=CARTESIAN_POINT('Ctrl Pts',(7.71743714391871,1.75058971130236,119.428591683881));
#227611=CARTESIAN_POINT('Ctrl Pts',(7.66863143007339,1.94319659059258,119.436572580247));
#227612=CARTESIAN_POINT('Ctrl Pts',(7.61981488073649,2.135846231069,119.444555248475));
#227613=CARTESIAN_POINT('Ctrl Pts',(7.56374492319702,2.32661442569172,119.452537916702));
#227614=CARTESIAN_POINT('Ctrl Pts',(7.50060213050016,2.5149331362755,119.46052058493));
#227615=CARTESIAN_POINT('Ctrl Pts',(7.43743561318835,2.70332260376921,119.468506252482));
#227616=CARTESIAN_POINT('Ctrl Pts',(7.36719106909571,2.8892604351785,119.476491920034));
#227617=CARTESIAN_POINT('Ctrl Pts',(7.29009788540409,3.07219690469652,119.484477587586));
#227618=CARTESIAN_POINT('Ctrl Pts',(7.21296388295768,3.25523023412526,119.492467483332));
#227619=CARTESIAN_POINT('Ctrl Pts',(7.12897414148497,3.43525872550265,119.500457379079));
#227620=CARTESIAN_POINT('Ctrl Pts',(7.03840497108245,3.61175531605365,119.508447274826));
#227621=CARTESIAN_POINT('Ctrl Pts',(6.94772851402123,3.78846098138571,119.516446635264));
#227622=CARTESIAN_POINT('Ctrl Pts',(6.85045721147659,3.96162609040045,119.524445995702));
#227623=CARTESIAN_POINT('Ctrl Pts',(6.74691250154266,4.13074965309293,119.53244535614));
#227624=CARTESIAN_POINT('Ctrl Pts',(6.64329540802179,4.29999144268578,119.540450308582));
#227625=CARTESIAN_POINT('Ctrl Pts',(6.53339634539518,4.46518577342108,119.548455261023));
#227626=CARTESIAN_POINT('Ctrl Pts',(6.41757865081015,4.62586265043244,119.556460213465));
#227627=CARTESIAN_POINT('Ctrl Pts',(6.30160980468221,4.78674922388056,119.564475613023));
#227628=CARTESIAN_POINT('Ctrl Pts',(6.17970710251706,4.94310630428356,119.572491012581));
#227629=CARTESIAN_POINT('Ctrl Pts',(6.05227327133962,5.09449793885796,119.580506412138));
#227630=CARTESIAN_POINT('Ctrl Pts',(6.02334626997655,5.12886327166815,119.582325877753));
#227631=CARTESIAN_POINT('Ctrl Pts',(5.99413441054198,5.16297290269607,119.584145343367));
#227632=CARTESIAN_POINT('Ctrl Pts',(5.96464265541942,5.19682200899272,119.585964808982));
#227633=CARTESIAN_POINT('Ctrl Pts',(5.83884770394008,5.3412029272023,119.593725608152));
#227634=CARTESIAN_POINT('Ctrl Pts',(5.70758380519134,5.48126989469719,119.601486407322));
#227635=CARTESIAN_POINT('Ctrl Pts',(5.5711817486657,5.61656967581941,119.609247206492));
#227636=CARTESIAN_POINT('Ctrl Pts',(5.434945282889,5.75170520434416,119.616998584128));
#227637=CARTESIAN_POINT('Ctrl Pts',(5.29358332630605,5.88208481622866,119.624749961765));
#227638=CARTESIAN_POINT('Ctrl Pts',(5.14746799382607,6.00728676296847,119.632501339401));
#227639=CARTESIAN_POINT('Ctrl Pts',(5.00150038414922,6.13236213036705,119.640244880384));
#227640=CARTESIAN_POINT('Ctrl Pts',(4.85078923511304,6.25227002160903,119.647988421367));
#227641=CARTESIAN_POINT('Ctrl Pts',(4.69574478683363,6.36662405808014,119.65573196235));
#227642=CARTESIAN_POINT('Ctrl Pts',(4.54082566327652,6.48088566049105,119.663469244115));
#227643=CARTESIAN_POINT('Ctrl Pts',(4.38158050125974,6.58960213416366,119.671206525879));
#227644=CARTESIAN_POINT('Ctrl Pts',(4.21845409622307,6.69242602036502,119.678943807643));
#227645=CARTESIAN_POINT('Ctrl Pts',(4.05542652010801,6.79518761147819,119.686676401833));
#227646=CARTESIAN_POINT('Ctrl Pts',(3.88852268591381,6.89206353305957,119.694408996022));
#227647=CARTESIAN_POINT('Ctrl Pts',(3.71821803993601,6.98274842791106,119.702141590212));
#227648=CARTESIAN_POINT('Ctrl Pts',(3.54798211470679,7.07339672990378,119.709871064171));
#227649=CARTESIAN_POINT('Ctrl Pts',(3.37434842720722,7.15785881222829,119.717600538131));
#227650=CARTESIAN_POINT('Ctrl Pts',(3.19781887402807,7.23587420073828,119.72533001209));
#227651=CARTESIAN_POINT('Ctrl Pts',(3.02129216768496,7.31388833111888,119.733059361399));
#227652=CARTESIAN_POINT('Ctrl Pts',(2.84187001253841,7.38545581951772,119.740788710708));
#227653=CARTESIAN_POINT('Ctrl Pts',(2.66007659322118,7.45036331451003,119.748518060017));
#227654=CARTESIAN_POINT('Ctrl Pts',(2.4782758242127,7.51527343363498,119.756247721814));
#227655=CARTESIAN_POINT('Ctrl Pts',(2.29410393821104,7.57352290139463,119.763977383611));
#227656=CARTESIAN_POINT('Ctrl Pts',(2.10810252566066,7.62494752383931,119.771707045408));
#227657=CARTESIAN_POINT('Ctrl Pts',(1.92205951152549,7.67638364805572,119.779438436043));
#227658=CARTESIAN_POINT('Ctrl Pts',(1.73418650220548,7.72099179136673,119.787169826677));
#227659=CARTESIAN_POINT('Ctrl Pts',(1.54503763079652,7.75865837109888,119.794901217311));
#227660=CARTESIAN_POINT('Ctrl Pts',(1.35581178450632,7.79634027939461,119.802635754266));
#227661=CARTESIAN_POINT('Ctrl Pts',(1.1653093941541,7.82707492893557,119.81037029122));
#227662=CARTESIAN_POINT('Ctrl Pts',(0.974092152111527,7.85080030819755,
119.818104828175));
#227663=CARTESIAN_POINT('Ctrl Pts',(0.78264972245639,7.87455362773027,119.825848473732));
#227664=CARTESIAN_POINT('Ctrl Pts',(0.590491116317506,7.89128114754464,
119.833592119289));
#227665=CARTESIAN_POINT('Ctrl Pts',(0.398181526491632,7.9009728813584,119.841335764847));
#227666=CARTESIAN_POINT('Ctrl Pts',(0.205748721035988,7.91067082481093,
119.849084371873));
#227667=CARTESIAN_POINT('Ctrl Pts',(0.0131650968569829,7.91332399779083,
119.8568329789));
#227668=CARTESIAN_POINT('Ctrl Pts',(-0.179006949978784,7.9089744917947,
119.864581585927));
#227669=CARTESIAN_POINT('Ctrl Pts',(-0.371470174448657,7.90461839545994,
119.872341933585));
#227670=CARTESIAN_POINT('Ctrl Pts',(-0.5635202191567,7.8932384500904,119.880102281242));
#227671=CARTESIAN_POINT('Ctrl Pts',(-0.754601381223256,7.8749284285926,
119.8878626289));
#227672=CARTESIAN_POINT('Ctrl Pts',(-0.886012315991531,7.8623362033066,
119.893199599477));
#227673=CARTESIAN_POINT('Ctrl Pts',(-1.01696519846024,7.84646738331229,
119.898536570054));
#227674=CARTESIAN_POINT('Ctrl Pts',(-1.14728311387771,7.82736625287274,
119.903873540631));
#227675=CARTESIAN_POINT('Ctrl Pts',(-1.34052922190157,7.79904152787639,
119.91178763893));
#227676=CARTESIAN_POINT('Ctrl Pts',(-1.53299881074559,7.76351608916653,
119.919701737229));
#227677=CARTESIAN_POINT('Ctrl Pts',(-1.72411413628818,7.72083877859467,
119.927615835527));
#227678=CARTESIAN_POINT('Ctrl Pts',(-1.91501000734958,7.67821047365344,
119.935520846201));
#227679=CARTESIAN_POINT('Ctrl Pts',(-2.10455437925534,7.62844672859773,
119.943425856875));
#227680=CARTESIAN_POINT('Ctrl Pts',(-2.29217510595005,7.57164805598246,
119.95133086755));
#227681=CARTESIAN_POINT('Ctrl Pts',(-2.47961523885351,7.51490405476626,
119.959228269278));
#227682=CARTESIAN_POINT('Ctrl Pts',(-2.66513508722515,7.45113871413749,
119.967125671007));
#227683=CARTESIAN_POINT('Ctrl Pts',(-2.84817289568144,7.38050351644829,
119.975023072736));
#227684=CARTESIAN_POINT('Ctrl Pts',(-3.03106850639844,7.30992319357163,
119.98291433916));
#227685=CARTESIAN_POINT('Ctrl Pts',(-3.21148559854803,7.2324837700926,119.990805605584));
#227686=CARTESIAN_POINT('Ctrl Pts',(-3.38887751257084,7.14838654556339,
119.998696872009));
#227687=CARTESIAN_POINT('Ctrl Pts',(-3.56616454321308,7.06433904371322,
120.006583472703));
#227688=CARTESIAN_POINT('Ctrl Pts',(-3.74042964897547,6.97364173176869,
120.014470073398));
#227689=CARTESIAN_POINT('Ctrl Pts',(-3.91114584112585,6.8765441327344,120.022356674093));
#227690=CARTESIAN_POINT('Ctrl Pts',(-4.0817927801578,6.77948592253278,120.030240075491));
#227691=CARTESIAN_POINT('Ctrl Pts',(-4.24889337540426,6.67603276987812,
120.03812347689));
#227692=CARTESIAN_POINT('Ctrl Pts',(-4.41194471236759,6.56648040087014,
120.046006878288));
#227693=CARTESIAN_POINT('Ctrl Pts',(-4.57498299938688,6.45693679997354,
120.053889648732));
#227694=CARTESIAN_POINT('Ctrl Pts',(-4.73397238391049,6.34129514199491,
120.061772419176));
#227695=CARTESIAN_POINT('Ctrl Pts',(-4.88843802027627,6.2198950732241,120.06965518962));
#227696=CARTESIAN_POINT('Ctrl Pts',(-5.04290404734862,6.09849469738302,
120.077537980003));
#227697=CARTESIAN_POINT('Ctrl Pts',(-5.19284603183183,5.97133609448737,
120.085420770386));
#227698=CARTESIAN_POINT('Ctrl Pts',(-5.33782130693576,5.8387999362217,120.093303560769));
#227699=CARTESIAN_POINT('Ctrl Pts',(-5.48282132859799,5.70624115469311,
120.101187696705));
#227700=CARTESIAN_POINT('Ctrl Pts',(-5.62285269699034,5.56830322160043,
120.10907183264));
#227701=CARTESIAN_POINT('Ctrl Pts',(-5.75750861486855,5.42540464386892,
120.116955968576));
#227702=CARTESIAN_POINT('Ctrl Pts',(-5.89221016245567,5.28245764330826,
120.124842776143));
#227703=CARTESIAN_POINT('Ctrl Pts',(-6.02153239375114,5.13454689976469,
120.132729583709));
#227704=CARTESIAN_POINT('Ctrl Pts',(-6.1451077480048,4.98212522578582,120.140616391275));
#227705=CARTESIAN_POINT('Ctrl Pts',(-6.26880385358569,4.82955461337547,
120.148510905414));
#227706=CARTESIAN_POINT('Ctrl Pts',(-6.38674164824982,4.67246453436258,
120.156405419553));
#227707=CARTESIAN_POINT('Ctrl Pts',(-6.49859537110552,4.51133895896174,
120.164299933692));
#227708=CARTESIAN_POINT('Ctrl Pts',(-6.61051164662823,4.3501232762832,120.172198862731));
#227709=CARTESIAN_POINT('Ctrl Pts',(-6.71633688107715,4.18486788757923,
120.180097791769));
#227710=CARTESIAN_POINT('Ctrl Pts',(-6.81579037075905,4.01608299489293,
120.187996720808));
#227711=CARTESIAN_POINT('Ctrl Pts',(-6.91536530335083,3.84709199854374,
120.195905295248));
#227712=CARTESIAN_POINT('Ctrl Pts',(-7.00855278642122,3.67456319215405,
120.203813869689));
#227713=CARTESIAN_POINT('Ctrl Pts',(-7.09511902650703,3.49902943681501,
120.21172244413));
#227714=CARTESIAN_POINT('Ctrl Pts',(-7.1318235554734,3.4246022259181,120.21507572018));
#227715=CARTESIAN_POINT('Ctrl Pts',(-7.16733831531233,3.34963501146115,
120.21842899623));
#227716=CARTESIAN_POINT('Ctrl Pts',(-7.20164816280539,3.27416932047837,
120.221782272281));
#227717=CARTESIAN_POINT('Ctrl Pts',(-7.29218645218861,3.07502723539373,
120.230631040189));
#227718=CARTESIAN_POINT('Ctrl Pts',(-7.37450316996348,2.87203455178348,
120.239479808097));
#227719=CARTESIAN_POINT('Ctrl Pts',(-7.44829984725901,2.6658489051935,120.248328576005));
#227720=CARTESIAN_POINT('Ctrl Pts',(-7.52428895885341,2.45353766460545,
120.257440233015));
#227721=CARTESIAN_POINT('Ctrl Pts',(-7.59124388804176,2.237840989881,120.266551890026));
#227722=CARTESIAN_POINT('Ctrl Pts',(-7.64889092479903,2.01950207242455,
120.275663547036));
#227723=CARTESIAN_POINT('Ctrl Pts',(-7.70459438214935,1.80852448778893,
120.284468003019));
#227724=CARTESIAN_POINT('Ctrl Pts',(-7.75160717027716,1.59508012271073,
120.293272459002));
#227725=CARTESIAN_POINT('Ctrl Pts',(-7.78973097277438,1.37985954785242,
120.302076914985));
#227726=CARTESIAN_POINT('Ctrl Pts',(-7.82776957822532,1.16511993648874,
120.310861695238));
#227727=CARTESIAN_POINT('Ctrl Pts',(-7.85695879704077,0.948612230775094,
120.319646475491));
#227728=CARTESIAN_POINT('Ctrl Pts',(-7.87715066373012,0.731039274523672,
120.328431255744));
#227729=CARTESIAN_POINT('Ctrl Pts',(-7.89727337150146,0.514211524769316,
120.337185947352));
#227730=CARTESIAN_POINT('Ctrl Pts',(-7.90846018411719,0.296326002315819,
120.345940638961));
#227731=CARTESIAN_POINT('Ctrl Pts',(-7.91061455199777,0.0780923153782337,
120.354695330569));
#227732=CARTESIAN_POINT('Ctrl Pts',(-7.91085842941872,0.053387960465725,
120.355686373756));
#227733=CARTESIAN_POINT('Ctrl Pts',(-7.91098661353903,0.0286791569209888,
120.356677416943));
#227734=CARTESIAN_POINT('Ctrl Pts',(-7.91099900539481,0.00396694370733382,
120.357668460131));
#227735=CARTESIAN_POINT('',(-7.90255836853663,-0.00601847252836551,122.357668497961));
#227736=CARTESIAN_POINT('Ctrl Pts',(-7.90626572818492,0.00396378192042368,
120.357668491763));
#227737=CARTESIAN_POINT('Ctrl Pts',(-7.90584785985939,-0.187660776584018,
120.365357873877));
#227738=CARTESIAN_POINT('Ctrl Pts',(-7.84915752905825,-1.70037946986372,
120.426032044598));
#227739=CARTESIAN_POINT('Ctrl Pts',(-6.53602975274865,-5.78311739899863,
120.592675792542));
#227740=CARTESIAN_POINT('Ctrl Pts',(-1.33164505529345,-8.62281587858876,
120.80461494697));
#227741=CARTESIAN_POINT('Ctrl Pts',(3.95079584577209,-7.22610140145887,
121.016554101405));
#227742=CARTESIAN_POINT('Ctrl Pts',(6.93730582468089,-4.47104709983874,
121.175508467229));
#227743=CARTESIAN_POINT('Ctrl Pts',(8.21337391138441,-0.604780945227029,
121.334462833054));
#227744=CARTESIAN_POINT('Ctrl Pts',(7.30159313550923,4.7675339096173,121.546401987488));
#227745=CARTESIAN_POINT('Ctrl Pts',(1.37451247778806,9.25621343198184,121.811325930528));
#227746=CARTESIAN_POINT('Ctrl Pts',(-6.27159982437673,6.44040648793863,
122.099409694823));
#227747=CARTESIAN_POINT('Ctrl Pts',(-7.88681031979375,1.88844581118687,
122.281523881901));
#227748=CARTESIAN_POINT('Ctrl Pts',(-7.90138446041817,-0.00601742412920814,
122.357668491763));
#227749=CARTESIAN_POINT('',(-7.92239988164926,-0.00247633632947917,124.357668806763));
#227750=CARTESIAN_POINT('Ctrl Pts',(-7.91099770491742,-0.00602600956896626,
122.357668542519));
#227751=CARTESIAN_POINT('Ctrl Pts',(-7.91082343745109,-0.234805853083792,
122.366852830167));
#227752=CARTESIAN_POINT('Ctrl Pts',(-7.90072110925209,-0.463199658241609,
122.376037117815));
#227753=CARTESIAN_POINT('Ctrl Pts',(-7.88081444583491,-0.690423544152256,
122.385221405463));
#227754=CARTESIAN_POINT('Ctrl Pts',(-7.86080562440018,-0.918813509040518,
122.394452825501));
#227755=CARTESIAN_POINT('Ctrl Pts',(-7.83089166989144,-1.14602143151767,
122.403684245539));
#227756=CARTESIAN_POINT('Ctrl Pts',(-7.79124766526346,-1.37126978327632,
122.412915665577));
#227757=CARTESIAN_POINT('Ctrl Pts',(-7.75137148169927,-1.59783732372909,
122.422201150317));
#227758=CARTESIAN_POINT('Ctrl Pts',(-7.7016510085194,-1.82242219111774,
122.431486635057));
#227759=CARTESIAN_POINT('Ctrl Pts',(-7.64231316787249,-2.04425302840983,
122.440772119796));
#227760=CARTESIAN_POINT('Ctrl Pts',(-7.62874153236439,-2.09498974608209,
122.442895877807));
#227761=CARTESIAN_POINT('Ctrl Pts',(-7.6146669917704,-2.14558247979062,
122.445019635817));
#227762=CARTESIAN_POINT('Ctrl Pts',(-7.60009261164581,-2.19602215253099,
122.447143393828));
#227763=CARTESIAN_POINT('Ctrl Pts',(-7.54111778509625,-2.4001248948534,
122.455737121948));
#227764=CARTESIAN_POINT('Ctrl Pts',(-7.47388082252246,-2.60197576896231,
122.464330850067));
#227765=CARTESIAN_POINT('Ctrl Pts',(-7.39856509941839,-2.80092046828683,
122.472924578187));
#227766=CARTESIAN_POINT('Ctrl Pts',(-7.32335811921021,-2.99957792582657,
122.481505898448));
#227767=CARTESIAN_POINT('Ctrl Pts',(-7.24009574407455,-3.19533735066757,
122.490087218708));
#227768=CARTESIAN_POINT('Ctrl Pts',(-7.14901080652297,-3.38756040362646,
122.498668538969));
#227769=CARTESIAN_POINT('Ctrl Pts',(-7.05398673524564,-3.58809649199087,
122.507620974026));
#227770=CARTESIAN_POINT('Ctrl Pts',(-6.95044854065877,-3.78478330039433,
122.516573409083));
#227771=CARTESIAN_POINT('Ctrl Pts',(-6.83871795396429,-3.97691560711646,
122.52552584414));
#227772=CARTESIAN_POINT('Ctrl Pts',(-6.73204100849876,-4.16035765474848,
122.534073355207));
#227773=CARTESIAN_POINT('Ctrl Pts',(-6.61789646909609,-4.33964779601734,
122.542620866275));
#227774=CARTESIAN_POINT('Ctrl Pts',(-6.49661316061465,-4.51419300000881,
122.551168377342));
#227775=CARTESIAN_POINT('Ctrl Pts',(-6.37551631531136,-4.68846985500919,
122.55970274731));
#227776=CARTESIAN_POINT('Ctrl Pts',(-6.24730273672162,-4.85801612224831,
122.568237117277));
#227777=CARTESIAN_POINT('Ctrl Pts',(-6.11234591069035,-5.02226527257043,
122.576771487245));
#227778=CARTESIAN_POINT('Ctrl Pts',(-5.97768291654091,-5.18615681492009,
122.585287275937));
#227779=CARTESIAN_POINT('Ctrl Pts',(-5.8363061281154,-5.34477406179062,
122.593803064629));
#227780=CARTESIAN_POINT('Ctrl Pts',(-5.68863092265281,-5.49758121593836,
122.602318853321));
#227781=CARTESIAN_POINT('Ctrl Pts',(-5.66678715342625,-5.52018409094987,
122.603578488765));
#227782=CARTESIAN_POINT('Ctrl Pts',(-5.64480565440291,-5.5426598950434,
122.604838124208));
#227783=CARTESIAN_POINT('Ctrl Pts',(-5.62268784985215,-5.5650069490635,
122.606097759652));
#227784=CARTESIAN_POINT('Ctrl Pts',(-5.48406843215521,-5.70506314715491,
122.613992301415));
#227785=CARTESIAN_POINT('Ctrl Pts',(-5.34022003012878,-5.83992976780298,
122.621886843178));
#227786=CARTESIAN_POINT('Ctrl Pts',(-5.19157519835085,-5.96920999461975,
122.629781384941));
#227787=CARTESIAN_POINT('Ctrl Pts',(-5.04289686831056,-6.0985193557354,
122.6376777058));
#227788=CARTESIAN_POINT('Ctrl Pts',(-4.88942021267008,-6.22223958920075,
122.645574026658));
#227789=CARTESIAN_POINT('Ctrl Pts',(-4.73161110841174,-6.34001398411349,
122.653470347517));
#227790=CARTESIAN_POINT('Ctrl Pts',(-4.57374042376016,-6.45783433704359,
122.661369749685));
#227791=CARTESIAN_POINT('Ctrl Pts',(-4.41153419555483,-6.56970402286812,
122.669269151852));
#227792=CARTESIAN_POINT('Ctrl Pts',(-4.24548774599272,-6.67530934104373,
122.67716855402));
#227793=CARTESIAN_POINT('Ctrl Pts',(-4.0792585813268,-6.78103086577915,
122.685076648575));
#227794=CARTESIAN_POINT('Ctrl Pts',(-3.90918104219986,-6.88047406748113,
122.69298474313));
#227795=CARTESIAN_POINT('Ctrl Pts',(-3.73577661790565,-6.9733703516384,
122.700892837685));
#227796=CARTESIAN_POINT('Ctrl Pts',(-3.56226888202774,-7.0663219819166,
122.708805643756));
#227797=CARTESIAN_POINT('Ctrl Pts',(-3.38543061583238,-7.1527187671374,
122.716718449827));
#227798=CARTESIAN_POINT('Ctrl Pts',(-3.20580410161825,-7.23233994375594,
122.724631255898));
#227799=CARTESIAN_POINT('Ctrl Pts',(-3.02592587066444,-7.3120726962355,
122.732555150454));
#227800=CARTESIAN_POINT('Ctrl Pts',(-2.84325190185535,-7.38501074096721,
122.740479045009));
#227801=CARTESIAN_POINT('Ctrl Pts',(-2.6583417859301,-7.4509824821414,122.748402939565));
#227802=CARTESIAN_POINT('Ctrl Pts',(-2.52883464035107,-7.49718769836549,
122.753952668202));
#227803=CARTESIAN_POINT('Ctrl Pts',(-2.39823091583697,-7.53997677735986,
122.75950239684));
#227804=CARTESIAN_POINT('Ctrl Pts',(-2.26672591224101,-7.57930568315958,
122.765052125477));
#227805=CARTESIAN_POINT('Ctrl Pts',(-2.07420992414844,-7.63688100693887,
122.773176618562));
#227806=CARTESIAN_POINT('Ctrl Pts',(-1.87933832265149,-7.68716533577582,
122.781301111647));
#227807=CARTESIAN_POINT('Ctrl Pts',(-1.68269142842093,-7.72997222224755,
122.789425604731));
#227808=CARTESIAN_POINT('Ctrl Pts',(-1.48621827120316,-7.7727412889479,
122.797542919848));
#227809=CARTESIAN_POINT('Ctrl Pts',(-1.28797326023693,-7.80804601663937,
122.805660234964));
#227810=CARTESIAN_POINT('Ctrl Pts',(-1.08855107457847,-7.83574996780998,
122.813777550081));
#227811=CARTESIAN_POINT('Ctrl Pts',(-0.889276683270306,-7.86343338722555,
122.82188884935));
#227812=CARTESIAN_POINT('Ctrl Pts',(-0.688827173348975,-7.88352721799388,
122.83000014862));
#227813=CARTESIAN_POINT('Ctrl Pts',(-0.48780716835004,-7.89594612231532,
122.83811144789));
#227814=CARTESIAN_POINT('Ctrl Pts',(-0.286907557755394,-7.90835758873729,
122.84621788916));
#227815=CARTESIAN_POINT('Ctrl Pts',(-0.0854384527376454,-7.91310327528335,
122.85432433043));
#227816=CARTESIAN_POINT('Ctrl Pts',(0.115990071895807,-7.91014963848483,
122.862430771701));
#227817=CARTESIAN_POINT('Ctrl Pts',(0.317326568464416,-7.90719735113509,
122.870533509324));
#227818=CARTESIAN_POINT('Ctrl Pts',(0.518622201490153,-7.89655276058245,
122.878636246948));
#227819=CARTESIAN_POINT('Ctrl Pts',(0.71926598195335,-7.87823441179587,
122.886738984571));
#227820=CARTESIAN_POINT('Ctrl Pts',(0.921721724629747,-7.85975063472773,
122.894914895928));
#227821=CARTESIAN_POINT('Ctrl Pts',(1.12351345260795,-7.83345380885929,
122.903090807284));
#227822=CARTESIAN_POINT('Ctrl Pts',(1.32401664272496,-7.79941670445857,
122.911266718641));
#227823=CARTESIAN_POINT('Ctrl Pts',(1.52264959289113,-7.76569708903358,
122.91936636729));
#227824=CARTESIAN_POINT('Ctrl Pts',(1.72001762199083,-7.72438104810107,
122.92746601594));
#227825=CARTESIAN_POINT('Ctrl Pts',(1.91552142449002,-7.67559109595604,
122.935565664589));
#227826=CARTESIAN_POINT('Ctrl Pts',(2.11102389835759,-7.62680147538449,
122.943665258194));
#227827=CARTESIAN_POINT('Ctrl Pts',(2.30466185975625,-7.57053812266403,
122.951764851798));
#227828=CARTESIAN_POINT('Ctrl Pts',(2.4958486122885,-7.50697413772937,122.959864445403));
#227829=CARTESIAN_POINT('Ctrl Pts',(2.68705874926596,-7.44340237815287,
122.967965029686));
#227830=CARTESIAN_POINT('Ctrl Pts',(2.87581677530425,-7.37252830720564,
122.976065613968));
#227831=CARTESIAN_POINT('Ctrl Pts',(3.06155298483146,-7.2945743070497,122.984166198251));
#227832=CARTESIAN_POINT('Ctrl Pts',(3.25032275769383,-7.21534711198306,
122.99239908649));
#227833=CARTESIAN_POINT('Ctrl Pts',(3.4359708315083,-7.12880684220308,123.00063197473));
#227834=CARTESIAN_POINT('Ctrl Pts',(3.6179220623365,-7.03523709272536,123.00886486297));
#227835=CARTESIAN_POINT('Ctrl Pts',(3.79712025935002,-6.9430831109958,123.016973182556));
#227836=CARTESIAN_POINT('Ctrl Pts',(3.97273242345603,-6.84411104754788,
123.025081502143));
#227837=CARTESIAN_POINT('Ctrl Pts',(4.14423535203928,-6.73863742509625,
123.03318982173));
#227838=CARTESIAN_POINT('Ctrl Pts',(4.3196904969638,-6.63073320523344,123.041484994296));
#227839=CARTESIAN_POINT('Ctrl Pts',(4.49084443242895,-6.51602435737667,
123.049780166862));
#227840=CARTESIAN_POINT('Ctrl Pts',(4.65716950940198,-6.39489586785403,
123.058075339428));
#227841=CARTESIAN_POINT('Ctrl Pts',(4.82349458637514,-6.27376737833129,
123.066370511994));
#227842=CARTESIAN_POINT('Ctrl Pts',(4.98499054108189,-6.14621948975367,
123.07466568456));
#227843=CARTESIAN_POINT('Ctrl Pts',(5.14116677031493,-6.01268037066744,
123.082960857126));
#227844=CARTESIAN_POINT('Ctrl Pts',(5.28854722988903,-5.88666211015046,
123.090788849587));
#227845=CARTESIAN_POINT('Ctrl Pts',(5.4314728055252,-5.75506676611666,123.098616842048));
#227846=CARTESIAN_POINT('Ctrl Pts',(5.56949181456856,-5.61824544919976,
123.10644483451));
#227847=CARTESIAN_POINT('Ctrl Pts',(5.70739425040121,-5.48153969390236,
123.114266215315));
#227848=CARTESIAN_POINT('Ctrl Pts',(5.84039812283548,-5.33961700065488,
123.12208759612));
#227849=CARTESIAN_POINT('Ctrl Pts',(5.96808476805478,-5.19286868708545,
123.129908976925));
#227850=CARTESIAN_POINT('Ctrl Pts',(6.09568611569148,-5.04621840472653,
123.13772513287));
#227851=CARTESIAN_POINT('Ctrl Pts',(6.21797707986872,-4.89474918651374,
123.145541288814));
#227852=CARTESIAN_POINT('Ctrl Pts',(6.33457572928104,-4.73888925065817,
123.153357444759));
#227853=CARTESIAN_POINT('Ctrl Pts',(6.45111836426451,-4.58310419050083,
123.161169845793));
#227854=CARTESIAN_POINT('Ctrl Pts',(6.56197392101166,-4.4229328955581,123.168982246827));
#227855=CARTESIAN_POINT('Ctrl Pts',(6.66680056193569,-4.25883684441819,
123.176794647862));
#227856=CARTESIAN_POINT('Ctrl Pts',(6.77159656318468,-4.09478875675054,
123.184604765417));
#227857=CARTESIAN_POINT('Ctrl Pts',(6.87036697022981,-3.92681849502103,
123.192414882972));
#227858=CARTESIAN_POINT('Ctrl Pts',(6.96281303026298,-3.75541684844707,
123.200225000527));
#227859=CARTESIAN_POINT('Ctrl Pts',(7.05526435759767,-3.58400543591711,
123.20803556308));
#227860=CARTESIAN_POINT('Ctrl Pts',(7.14139044505814,-3.40916255485171,
123.215846125632));
#227861=CARTESIAN_POINT('Ctrl Pts',(7.22093809887062,-3.23140433438446,
123.223656688185));
#227862=CARTESIAN_POINT('Ctrl Pts',(7.28292354456225,-3.09289085230257,
123.22974286644));
#227863=CARTESIAN_POINT('Ctrl Pts',(7.34091552061425,-2.95260775733558,
123.235829044696));
#227864=CARTESIAN_POINT('Ctrl Pts',(7.39481435040327,-2.81080801960395,
123.241915222951));
#227865=CARTESIAN_POINT('Ctrl Pts',(7.47133291377299,-2.6094991552019,123.250555588955));
#227866=CARTESIAN_POINT('Ctrl Pts',(7.53956441781505,-2.40522911851261,
123.259195954958));
#227867=CARTESIAN_POINT('Ctrl Pts',(7.59932669159849,-2.19867115193672,
123.267836320962));
#227868=CARTESIAN_POINT('Ctrl Pts',(7.65918837936401,-1.99176957812021,
123.276491060133));
#227869=CARTESIAN_POINT('Ctrl Pts',(7.71055261176152,-1.78257268759434,
123.285145799304));
#227870=CARTESIAN_POINT('Ctrl Pts',(7.75328795444121,-1.5717655345238,123.293800538475));
#227871=CARTESIAN_POINT('Ctrl Pts',(7.79734505487777,-1.35443834505475,
123.302722959334));
#227872=CARTESIAN_POINT('Ctrl Pts',(7.83223096106478,-1.13539997541228,
123.311645380192));
#227873=CARTESIAN_POINT('Ctrl Pts',(7.85785924489575,-0.915406514837176,
123.32056780105));
#227874=CARTESIAN_POINT('Ctrl Pts',(7.88280207198479,-0.701297022214343,
123.329251581914));
#227875=CARTESIAN_POINT('Ctrl Pts',(7.89897612254177,-0.486283093931356,
123.337935362777));
#227876=CARTESIAN_POINT('Ctrl Pts',(7.90635476831299,-0.271063235379707,
123.34661914364));
#227877=CARTESIAN_POINT('Ctrl Pts',(7.91403757422244,-0.0469716537561526,
123.355660884496));
#227878=CARTESIAN_POINT('Ctrl Pts',(7.91218454176299,0.177342906246704,
123.364702625352));
#227879=CARTESIAN_POINT('Ctrl Pts',(7.90082554757362,0.401094336544378,
123.373744366208));
#227880=CARTESIAN_POINT('Ctrl Pts',(7.88946655338425,0.624845766842052,
123.382786107064));
#227881=CARTESIAN_POINT('Ctrl Pts',(7.86860164337229,0.848033791804023,
123.39182784792));
#227882=CARTESIAN_POINT('Ctrl Pts',(7.83832126366524,1.06987885649423,123.400869588776));
#227883=CARTESIAN_POINT('Ctrl Pts',(7.81045128427076,1.27406445262936,123.409191582549));
#227884=CARTESIAN_POINT('Ctrl Pts',(7.77458145061864,1.47728584554186,123.417513576321));
#227885=CARTESIAN_POINT('Ctrl Pts',(7.73079461732031,1.67890904602105,123.425835570094));
#227886=CARTESIAN_POINT('Ctrl Pts',(7.6870467287885,1.8803529193401,123.434150162141));
#227887=CARTESIAN_POINT('Ctrl Pts',(7.63539594948841,2.08020115117116,123.442464754188));
#227888=CARTESIAN_POINT('Ctrl Pts',(7.57597647629685,2.2778282267539,123.450779346235));
#227889=CARTESIAN_POINT('Ctrl Pts',(7.5166062281239,2.47529158165804,123.459087050205));
#227890=CARTESIAN_POINT('Ctrl Pts',(7.44948020934234,2.67053717200129,123.467394754175));
#227891=CARTESIAN_POINT('Ctrl Pts',(7.37478311745651,2.8629521425407,123.475702458144));
#227892=CARTESIAN_POINT('Ctrl Pts',(7.30016139156988,3.05517297504677,123.484001780015));
#227893=CARTESIAN_POINT('Ctrl Pts',(7.21798394589666,3.24456861660356,123.492301101886));
#227894=CARTESIAN_POINT('Ctrl Pts',(7.12848461841886,3.43054340374315,123.500600423756));
#227895=CARTESIAN_POINT('Ctrl Pts',(7.03904247213368,3.61639937144105,123.508894443184));
#227896=CARTESIAN_POINT('Ctrl Pts',(6.94228790147491,3.79883858145367,123.517188462611));
#227897=CARTESIAN_POINT('Ctrl Pts',(6.83850255380036,3.97728598690941,123.525482482038));
#227898=CARTESIAN_POINT('Ctrl Pts',(6.73479416812338,4.15560106473805,123.533770351037));
#227899=CARTESIAN_POINT('Ctrl Pts',(6.62406555767608,4.32992999363992,123.542058220037));
#227900=CARTESIAN_POINT('Ctrl Pts',(6.5066441945941,4.49972247199256,123.550346089036));
#227901=CARTESIAN_POINT('Ctrl Pts',(6.46188383887172,4.5644463989729,123.553505377558));
#227902=CARTESIAN_POINT('Ctrl Pts',(6.41615143597175,4.62851140192374,123.556664666079));
#227903=CARTESIAN_POINT('Ctrl Pts',(6.36946683968058,4.691888018507,123.559823954601));
#227904=CARTESIAN_POINT('Ctrl Pts',(6.24973954643923,4.85442365897783,123.567926264428));
#227905=CARTESIAN_POINT('Ctrl Pts',(6.12379677769075,5.01236119801416,123.576028574254));
#227906=CARTESIAN_POINT('Ctrl Pts',(5.99202601781401,5.16522460323266,123.58413088408));
#227907=CARTESIAN_POINT('Ctrl Pts',(5.86022617302179,5.3181217490111,123.592234982278));
#227908=CARTESIAN_POINT('Ctrl Pts',(5.72259597978328,5.46594228571265,123.600339080475));
#227909=CARTESIAN_POINT('Ctrl Pts',(5.57956179768789,5.60824492562351,123.608443178672));
#227910=CARTESIAN_POINT('Ctrl Pts',(5.43647810270944,5.75059682518593,123.616550082194));
#227911=CARTESIAN_POINT('Ctrl Pts',(5.28798691399609,5.88742679360696,123.624656985716));
#227912=CARTESIAN_POINT('Ctrl Pts',(5.13455027690787,6.01833153406368,123.632763889237));
#227913=CARTESIAN_POINT('Ctrl Pts',(4.98097526316701,6.14935433080829,123.64087810396));
#227914=CARTESIAN_POINT('Ctrl Pts',(4.8224461313417,6.27444101413242,123.648992318683));
#227915=CARTESIAN_POINT('Ctrl Pts',(4.65945779159124,6.3932287686567,123.657106533407));
#227916=CARTESIAN_POINT('Ctrl Pts',(4.49638979418653,6.51207457858479,123.665224713808));
#227917=CARTESIAN_POINT('Ctrl Pts',(4.32885850323306,6.62461513689218,123.673342894209));
#227918=CARTESIAN_POINT('Ctrl Pts',(4.15738721186806,6.73053137356895,123.681461074611));
#227919=CARTESIAN_POINT('Ctrl Pts',(3.98573151928705,6.83656151317771,123.68958798535));
#227920=CARTESIAN_POINT('Ctrl Pts',(3.81012763456716,6.93595293457076,123.69771489609));
#227921=CARTESIAN_POINT('Ctrl Pts',(3.6311240385482,7.02843220189805,123.705841806829));
#227922=CARTESIAN_POINT('Ctrl Pts',(3.53614401773036,7.07750206938291,123.710153978028));
#227923=CARTESIAN_POINT('Ctrl Pts',(3.44020721014769,7.12462668468802,123.714466149226));
#227924=CARTESIAN_POINT('Ctrl Pts',(3.34339780309826,7.16977071671317,123.718778320425));
#227925=CARTESIAN_POINT('Ctrl Pts',(3.16384529748392,7.25349939877722,123.726776108728));
#227926=CARTESIAN_POINT('Ctrl Pts',(2.98097834721167,7.33055742192057,123.734773897032));
#227927=CARTESIAN_POINT('Ctrl Pts',(2.79532843593177,7.40067969414102,123.742771685335));
#227928=CARTESIAN_POINT('Ctrl Pts',(2.60983010757826,7.47074471161163,123.750762943454));
#227929=CARTESIAN_POINT('Ctrl Pts',(2.42155365801753,7.53388514623878,123.758754201573));
#227930=CARTESIAN_POINT('Ctrl Pts',(2.23105237594926,7.58988315428974,123.766745459692));
#227931=CARTESIAN_POINT('Ctrl Pts',(2.04067433415934,7.64584493575984,123.774731548057));
#227932=CARTESIAN_POINT('Ctrl Pts',(1.84807464843812,7.69467340592027,123.782717636421));
#227933=CARTESIAN_POINT('Ctrl Pts',(1.65382406139739,7.73619977598453,123.790703724786));
#227934=CARTESIAN_POINT('Ctrl Pts',(1.45966621477226,7.7777063202512,123.798686000379));
#227935=CARTESIAN_POINT('Ctrl Pts',(1.26385936444381,7.81191764378851,123.806668275971));
#227936=CARTESIAN_POINT('Ctrl Pts',(1.06698720773853,7.83871541124707,123.814650551564));
#227937=CARTESIAN_POINT('Ctrl Pts',(0.870175684351306,7.86550492544329,
123.82263036875));
#227938=CARTESIAN_POINT('Ctrl Pts',(0.672299839827818,7.88488539044696,
123.830610185936));
#227939=CARTESIAN_POINT('Ctrl Pts',(0.473951717323491,7.89678990284319,
123.838590003122));
#227940=CARTESIAN_POINT('Ctrl Pts',(0.268787359032186,7.90910351396139,
123.846844046828));
#227941=CARTESIAN_POINT('Ctrl Pts',(0.0631180567972388,7.91341816727462,
123.855098090534));
#227942=CARTESIAN_POINT('Ctrl Pts',(-0.142396639791706,7.90971833866264,
123.863352134241));
#227943=CARTESIAN_POINT('Ctrl Pts',(-0.341110331361759,7.90614094680762,
123.871333030607));
#227944=CARTESIAN_POINT('Ctrl Pts',(-0.539679135429459,7.89507104707969,
123.879313926974));
#227945=CARTESIAN_POINT('Ctrl Pts',(-0.737508079962727,7.87654764677963,
123.88729482334));
#227946=CARTESIAN_POINT('Ctrl Pts',(-0.935380945047946,7.85802013404816,
123.895277491568));
#227947=CARTESIAN_POINT('Ctrl Pts',(-1.13251328977988,7.83203585266932,
123.903260159795));
#227948=CARTESIAN_POINT('Ctrl Pts',(-1.32831602618527,7.79868562865432,
123.911242828023));
#227949=CARTESIAN_POINT('Ctrl Pts',(-1.52419233146929,7.76532287397387,
123.919228495575));
#227950=CARTESIAN_POINT('Ctrl Pts',(-1.71873770263018,7.72458871529149,
123.927214163127));
#227951=CARTESIAN_POINT('Ctrl Pts',(-1.91137361827227,7.6766250326151,123.935199830679));
#227952=CARTESIAN_POINT('Ctrl Pts',(-2.1041115294198,7.62863595446642,123.943189726425));
#227953=CARTESIAN_POINT('Ctrl Pts',(-2.29493764514277,7.57340980180064,
123.951179622172));
#227954=CARTESIAN_POINT('Ctrl Pts',(-2.4832886008591,7.5111383108583,123.959169517919));
#227955=CARTESIAN_POINT('Ctrl Pts',(-2.67186267383087,7.44879305419442,
123.967168878357));
#227956=CARTESIAN_POINT('Ctrl Pts',(-2.85795541194302,7.37938589245465,
123.975168238795));
#227957=CARTESIAN_POINT('Ctrl Pts',(-3.04102225315112,7.30315717041881,
123.983167599233));
#227958=CARTESIAN_POINT('Ctrl Pts',(-3.2242170683971,7.22687516021075,123.991172551675));
#227959=CARTESIAN_POINT('Ctrl Pts',(-3.40438146507005,7.1437622187103,123.999177504116));
#227960=CARTESIAN_POINT('Ctrl Pts',(-3.58099504504441,7.05410486790262,
124.007182456558));
#227961=CARTESIAN_POINT('Ctrl Pts',(-3.75783912015371,6.96433050693538,
124.015197856116));
#227962=CARTESIAN_POINT('Ctrl Pts',(-3.93112283067098,6.8679948382716,124.023213255674));
#227963=CARTESIAN_POINT('Ctrl Pts',(-4.10035333979208,6.76542855175161,
124.031228655232));
#227964=CARTESIAN_POINT('Ctrl Pts',(-4.13876803016639,6.74214638968775,
124.033048120846));
#227965=CARTESIAN_POINT('Ctrl Pts',(-4.17697399988309,6.71854334881586,
124.03486758646));
#227966=CARTESIAN_POINT('Ctrl Pts',(-4.21496571850726,6.69462358850806,
124.036687052075));
#227967=CARTESIAN_POINT('Ctrl Pts',(-4.37701665040925,6.5925955784805,124.044447851245));
#227968=CARTESIAN_POINT('Ctrl Pts',(-4.53564849664404,6.48449884468234,
124.052208650415));
#227969=CARTESIAN_POINT('Ctrl Pts',(-4.69036243648762,6.37059033484229,
124.059969449585));
#227970=CARTESIAN_POINT('Ctrl Pts',(-4.84488855513684,6.25682010880774,
124.067720827221));
#227971=CARTESIAN_POINT('Ctrl Pts',(-4.99550594919141,6.13725235992835,
124.075472204858));
#227972=CARTESIAN_POINT('Ctrl Pts',(-5.14174053642776,6.0121897222273,124.083223582494));
#227973=CARTESIAN_POINT('Ctrl Pts',(-5.2878272802938,5.88725352302624,124.090967123477));
#227974=CARTESIAN_POINT('Ctrl Pts',(-5.42953976775175,5.75683372497429,
124.09871066446));
#227975=CARTESIAN_POINT('Ctrl Pts',(-5.5664329848305,5.62127608514215,124.106454205443));
#227976=CARTESIAN_POINT('Ctrl Pts',(-5.70321554909599,5.48582801855642,
124.114191487207));
#227977=CARTESIAN_POINT('Ctrl Pts',(-5.83518634509595,5.34525062963367,
124.121928768972));
#227978=CARTESIAN_POINT('Ctrl Pts',(-5.96193348509867,5.19992981868594,
124.129666050736));
#227979=CARTESIAN_POINT('Ctrl Pts',(-6.08860383628698,5.05469704927337,
124.137398644925));
#227980=CARTESIAN_POINT('Ctrl Pts',(-6.21005659804115,4.90472684985828,
124.145131239115));
#227981=CARTESIAN_POINT('Ctrl Pts',(-6.32591675451383,4.75044189680931,
124.152863833304));
#227982=CARTESIAN_POINT('Ctrl Pts',(-6.44173015949393,4.59621920029491,
124.160593307264));
#227983=CARTESIAN_POINT('Ctrl Pts',(-6.55195523855155,4.43768550440512,
124.168322781223));
#227984=CARTESIAN_POINT('Ctrl Pts',(-6.6562572436728,4.27529654013067,124.176052255183));
#227985=CARTESIAN_POINT('Ctrl Pts',(-6.76055756674769,4.11291019465313,
124.183781604492));
#227986=CARTESIAN_POINT('Ctrl Pts',(-6.8589348028198,3.94666900067388,124.1915109538));
#227987=CARTESIAN_POINT('Ctrl Pts',(-6.95109732638403,3.77705797667137,
124.199240303109));
#227988=CARTESIAN_POINT('Ctrl Pts',(-7.0432635759693,3.6074400954972,124.206969964906));
#227989=CARTESIAN_POINT('Ctrl Pts',(-7.12921444026285,3.43445242826447,
124.214699626703));
#227990=CARTESIAN_POINT('Ctrl Pts',(-7.20870417949355,3.25860477084169,
124.222429288501));
#227991=CARTESIAN_POINT('Ctrl Pts',(-7.28821169761661,3.08271778285119,
124.230160679135));
#227992=CARTESIAN_POINT('Ctrl Pts',(-7.36125506484614,2.90396985815291,
124.237892069769));
#227993=CARTESIAN_POINT('Ctrl Pts',(-7.42763661342504,2.72289098917086,
124.245623460404));
#227994=CARTESIAN_POINT('Ctrl Pts',(-7.49404517623827,2.54173842942528,
124.253357997358));
#227995=CARTESIAN_POINT('Ctrl Pts',(-7.55378639849034,2.3582533734224,124.261092534313));
#227996=CARTESIAN_POINT('Ctrl Pts',(-7.60671240123349,2.17298123436918,
124.268827071267));
#227997=CARTESIAN_POINT('Ctrl Pts',(-7.65970073245708,1.98749090897474,
124.276570716824));
#227998=CARTESIAN_POINT('Ctrl Pts',(-7.70585771668609,1.80020964285619,
124.284314362382));
#227999=CARTESIAN_POINT('Ctrl Pts',(-7.7450863382906,1.61169432971156,124.292058007939));
#228000=CARTESIAN_POINT('Ctrl Pts',(-7.78434009425966,1.42305823198637,
124.299806614966));
#228001=CARTESIAN_POINT('Ctrl Pts',(-7.81665658514349,1.23318686488313,
124.307555221992));
#228002=CARTESIAN_POINT('Ctrl Pts',(-7.84199068151589,1.04264238884574,
124.315303829019));
#228003=CARTESIAN_POINT('Ctrl Pts',(-7.86736316391969,0.851809201257965,
124.323064176677));
#228004=CARTESIAN_POINT('Ctrl Pts',(-7.88573208784973,0.660301223715922,
124.330824524334));
#228005=CARTESIAN_POINT('Ctrl Pts',(-7.89710441926124,0.468681972434038,
124.338584871992));
#228006=CARTESIAN_POINT('Ctrl Pts',(-7.90492543460987,0.336900981259918,
124.343921842569));
#228007=CARTESIAN_POINT('Ctrl Pts',(-7.90943841241537,0.20506733643512,
124.349258813147));
#228008=CARTESIAN_POINT('Ctrl Pts',(-7.91065982831679,0.0733626652666543,
124.354595783724));
#228009=CARTESIAN_POINT('Ctrl Pts',(-7.91089423435946,0.0480867778846261,
124.355620019737));
#228010=CARTESIAN_POINT('Ctrl Pts',(-7.91100749162828,0.0228106579640831,
124.35664425575));
#228011=CARTESIAN_POINT('Ctrl Pts',(-7.91099961596495,-0.00246499540847172,
124.357668491763));
#228012=CARTESIAN_POINT('',(-7.90670614352357,0.00719251646262357,126.357668491763));
#228013=CARTESIAN_POINT('Ctrl Pts',(-7.9265347197683,-0.002480449643483,
124.357668921013));
#228014=CARTESIAN_POINT('Ctrl Pts',(-7.92370808336077,-2.59735768496362,
124.462614119133));
#228015=CARTESIAN_POINT('Ctrl Pts',(-5.80631166365505,-6.49188276010665,
124.620544105861));
#228016=CARTESIAN_POINT('Ctrl Pts',(-0.681732440644431,-8.19901426347268,
124.8314588812));
#228017=CARTESIAN_POINT('Ctrl Pts',(4.7061455593866,-7.34957997120415,125.04339803563));
#228018=CARTESIAN_POINT('Ctrl Pts',(8.31436308495323,-2.64529747305826,
125.255337190066));
#228019=CARTESIAN_POINT('Ctrl Pts',(7.74886771041429,2.78933298220472,125.467276344498));
#228020=CARTESIAN_POINT('Ctrl Pts',(5.48726075163886,6.16493663533192,125.626230710322));
#228021=CARTESIAN_POINT('Ctrl Pts',(1.86399302745116,8.02189509988344,125.785185076148));
#228022=CARTESIAN_POINT('Ctrl Pts',(-3.58466317121117,7.94939191666906,
125.99712423058));
#228023=CARTESIAN_POINT('Ctrl Pts',(-7.43754732069607,4.2296490490804,126.187952035785));
#228024=CARTESIAN_POINT('Ctrl Pts',(-7.91164687381234,0.804141605855872,
126.325795052383));
#228025=CARTESIAN_POINT('Ctrl Pts',(-7.90514438368602,0.00980857580332107,
126.357668491763));
#228026=CARTESIAN_POINT('',(-7.911,-2.14273043752655E-13,128.357668491763));
#228027=CARTESIAN_POINT('Ctrl Pts',(-7.911,-3.84692278032617E-13,126.357668491763));
#228028=CARTESIAN_POINT('Ctrl Pts',(-7.91099999999989,-2.20167589666733,
126.446255927496));
#228029=CARTESIAN_POINT('Ctrl Pts',(-6.94214576672333,-4.38610418338752,
126.534843363228));
#228030=CARTESIAN_POINT('Ctrl Pts',(-3.67820201488187,-7.34180684107687,
126.712018234694));
#228031=CARTESIAN_POINT('Ctrl Pts',(-1.40868175871612,-8.08992666571364,
126.800605670427));
#228032=CARTESIAN_POINT('Ctrl Pts',(2.97309270521433,-7.654542280252,126.977780541892));
#228033=CARTESIAN_POINT('Ctrl Pts',(5.05102072675755,-6.47444880834112,
127.066367977625));
#228034=CARTESIAN_POINT('Ctrl Pts',(7.66951518847956,-2.93425195367499,
127.24354284909));
#228035=CARTESIAN_POINT('Ctrl Pts',(8.18956872247094,-0.601881960096723,
127.332130284823));
#228036=CARTESIAN_POINT('Ctrl Pts',(7.3230668976122,3.71537198232701,127.509305156289));
#228037=CARTESIAN_POINT('Ctrl Pts',(5.94329958849997,5.66643518936732,127.597892592021));
#228038=CARTESIAN_POINT('Ctrl Pts',(2.16154501637526,7.92205913233091,127.775067463487));
#228039=CARTESIAN_POINT('Ctrl Pts',(-0.210816529303931,8.20894963712998,
127.863654899219));
#228040=CARTESIAN_POINT('Ctrl Pts',(-4.42123908576769,6.91982244717625,
128.040829770685));
#228041=CARTESIAN_POINT('Ctrl Pts',(-6.2263162563446,5.35390358803212,128.129417206418));
#228042=CARTESIAN_POINT('Ctrl Pts',(-7.65317280859554,2.31334857514237,
128.264559258688));
#228043=CARTESIAN_POINT('Ctrl Pts',(-7.91100000000003,1.15702837836367,
128.311113875225));
#228044=CARTESIAN_POINT('Ctrl Pts',(-7.911,-2.14273043752655E-13,128.357668491763));
#228045=CARTESIAN_POINT('',(-7.90996818647143,0.00413822696500661,132.357668491763));
#228046=CARTESIAN_POINT('Ctrl Pts',(-7.91099890900509,-0.0041547226431693,
128.364649935517));
#228047=CARTESIAN_POINT('Ctrl Pts',(-7.91056187092003,-0.836318048842218,
128.394870332571));
#228048=CARTESIAN_POINT('Ctrl Pts',(-7.77883880110308,-1.6631115170934,
128.42100714115));
#228049=CARTESIAN_POINT('Ctrl Pts',(-7.46272976525518,-2.63182852547884,
128.45823722325));
#228050=CARTESIAN_POINT('Ctrl Pts',(-7.3984705521292,-2.80739774204712,
128.465296010569));
#228051=CARTESIAN_POINT('Ctrl Pts',(-7.31776670017044,-3.00582065284319,
128.473795593309));
#228052=CARTESIAN_POINT('Ctrl Pts',(-7.30734358154125,-3.03107192632827,
128.474887121511));
#228053=CARTESIAN_POINT('Ctrl Pts',(-7.29394783665126,-3.06305404438618,
128.476282719078));
#228054=CARTESIAN_POINT('Ctrl Pts',(-7.29109621518518,-3.0698356801046,
128.476579399161));
#228055=CARTESIAN_POINT('Ctrl Pts',(-7.28652477886291,-3.08066502378771,
128.477054371261));
#228056=CARTESIAN_POINT('Ctrl Pts',(-7.28481103539682,-3.08471530618037,
128.477232287388));
#228057=CARTESIAN_POINT('Ctrl Pts',(-7.28156578967879,-3.09236737289993,
128.477568935933));
#228058=CARTESIAN_POINT('Ctrl Pts',(-7.28003498956775,-3.09596945543065,
128.477727624505));
#228059=CARTESIAN_POINT('Ctrl Pts',(-7.27657369197578,-3.10409737529657,
128.47808619001));
#228060=CARTESIAN_POINT('Ctrl Pts',(-7.27464164554164,-3.10862254685501,
128.478286164305));
#228061=CARTESIAN_POINT('Ctrl Pts',(-7.26969315929526,-3.12018284106618,
128.478797920278));
#228062=CARTESIAN_POINT('Ctrl Pts',(-7.26667072849489,-3.12721539319168,
128.479110082397));
#228063=CARTESIAN_POINT('Ctrl Pts',(-7.2485528224437,-3.16920380625505,
128.480978960651));
#228064=CARTESIAN_POINT('Ctrl Pts',(-7.23321559758548,-3.20405412042349,
128.482551181611));
#228065=CARTESIAN_POINT('Ctrl Pts',(-6.9583412619347,-3.81660989797856,
128.510538015696));
#228066=CARTESIAN_POINT('Ctrl Pts',(-6.63062074787241,-4.36117418717565,
128.540764195017));
#228067=CARTESIAN_POINT('Ctrl Pts',(-6.03500992369722,-5.12596545496245,
128.58556986693));
#228068=CARTESIAN_POINT('Ctrl Pts',(-5.81181518423438,-5.37770409948623,
128.600831636801));
#228069=CARTESIAN_POINT('Ctrl Pts',(-5.45068436703809,-5.73618295584506,
128.622980773011));
#228070=CARTESIAN_POINT('Ctrl Pts',(-5.32414308190378,-5.85382444858474,
128.630331092741));
#228071=CARTESIAN_POINT('Ctrl Pts',(-5.14801074177935,-6.0071290000049,
128.640014410502));
#228072=CARTESIAN_POINT('Ctrl Pts',(-5.10171692454457,-6.04649469325223,
128.642511030369));
#228073=CARTESIAN_POINT('Ctrl Pts',(-5.03535662851792,-6.10161904559869,
128.646022062702));
#228074=CARTESIAN_POINT('Ctrl Pts',(-5.01566106563755,-6.11781950091623,
128.647055805111));
#228075=CARTESIAN_POINT('Ctrl Pts',(-4.98549722024487,-6.14238699818202,
128.648626397462));
#228076=CARTESIAN_POINT('Ctrl Pts',(-4.97508554255796,-6.15082306811171,
128.649166250643));
#228077=CARTESIAN_POINT('Ctrl Pts',(-4.95578341122672,-6.16638156031196,
128.650162902403));
#228078=CARTESIAN_POINT('Ctrl Pts',(-4.9468989219567,-6.17351130425842,
128.650620018083));
#228079=CARTESIAN_POINT('Ctrl Pts',(-4.93241474997797,-6.18508341285493,
128.651362604191));
#228080=CARTESIAN_POINT('Ctrl Pts',(-4.92682440817282,-6.18953740930448,
128.651648577074));
#228081=CARTESIAN_POINT('Ctrl Pts',(-4.91623889908605,-6.19794778062934,
128.652188874966));
#228082=CARTESIAN_POINT('Ctrl Pts',(-4.91124497525431,-6.20190570692576,
128.652443266777));
#228083=CARTESIAN_POINT('Ctrl Pts',(-4.89961116298036,-6.21110320253402,
128.653034725391));
#228084=CARTESIAN_POINT('Ctrl Pts',(-4.89296763677944,-6.21633817025545,
128.653371594195));
#228085=CARTESIAN_POINT('Ctrl Pts',(-4.87280680605442,-6.23217216440233,
128.654391201656));
#228086=CARTESIAN_POINT('Ctrl Pts',(-4.85926332163606,-6.24273786347078,
128.655072511054));
#228087=CARTESIAN_POINT('Ctrl Pts',(-4.76484084223335,-6.31590636751635,
128.65979738694));
#228088=CARTESIAN_POINT('Ctrl Pts',(-4.68278712545681,-6.37698104705263,
128.663775614509));
#228089=CARTESIAN_POINT('Ctrl Pts',(-4.32708719123494,-6.6311688338786,
128.680506519401));
#228090=CARTESIAN_POINT('Ctrl Pts',(-4.04250279138282,-6.80839779726759,
128.692599434196));
#228091=CARTESIAN_POINT('Ctrl Pts',(-3.57710466557525,-7.05873135385175,
128.711006125476));
#228092=CARTESIAN_POINT('Ctrl Pts',(-3.40337814026,-7.14411545477539,128.717602712292));
#228093=CARTESIAN_POINT('Ctrl Pts',(-2.89711559888655,-7.37027408506629,
128.736371798973));
#228094=CARTESIAN_POINT('Ctrl Pts',(-2.55785952689693,-7.4947686166418,
128.748392646314));
#228095=CARTESIAN_POINT('Ctrl Pts',(-2.0758577420648,-7.63509238835664,
128.766027324354));
#228096=CARTESIAN_POINT('Ctrl Pts',(-1.93938679515738,-7.67089286401137,
128.771082890438));
#228097=CARTESIAN_POINT('Ctrl Pts',(-1.66137032994446,-7.73593171881953,
128.781639553966));
#228098=CARTESIAN_POINT('Ctrl Pts',(-1.51983615823292,-7.76497807917405,
128.787146527096));
#228099=CARTESIAN_POINT('Ctrl Pts',(-1.35516060573402,-7.79409903275928,
128.793790967958));
#228100=CARTESIAN_POINT('Ctrl Pts',(-1.3327103061836,-7.79796917268563,
128.794701879188));
#228101=CARTESIAN_POINT('Ctrl Pts',(-1.30374611714872,-7.80283349003321,
128.7958839942));
#228102=CARTESIAN_POINT('Ctrl Pts',(-1.29724704627652,-7.80391661359336,
128.796149688475));
#228103=CARTESIAN_POINT('Ctrl Pts',(-1.28672527082612,-7.80565664701212,
128.796580574145));
#228104=CARTESIAN_POINT('Ctrl Pts',(-1.28270340212337,-7.80631856867759,
128.796745450504));
#228105=CARTESIAN_POINT('Ctrl Pts',(-1.27498419211388,-7.80758287455877,
128.797062229841));
#228106=CARTESIAN_POINT('Ctrl Pts',(-1.27128692971231,-7.80818574161039,
128.797214102828));
#228107=CARTESIAN_POINT('Ctrl Pts',(-1.26285561166517,-7.80955438561218,
128.797560766761));
#228108=CARTESIAN_POINT('Ctrl Pts',(-1.25812128919059,-7.81031848385381,
128.797755660965));
#228109=CARTESIAN_POINT('Ctrl Pts',(-1.24337808743088,-7.81268421701364,
128.798363313542));
#228110=CARTESIAN_POINT('Ctrl Pts',(-1.23336685890424,-7.81427091496779,
128.798776982208));
#228111=CARTESIAN_POINT('Ctrl Pts',(-1.15686969770765,-7.82624442324337,
128.80194573346));
#228112=CARTESIAN_POINT('Ctrl Pts',(-1.0902585973341,-7.8358014861306,128.80475026061));
#228113=CARTESIAN_POINT('Ctrl Pts',(-0.19853192973562,-7.95215220450645,
128.842822023939));
#228114=CARTESIAN_POINT('Ctrl Pts',(0.638291672826344,-7.9289895672604,
128.884004691237));
#228115=CARTESIAN_POINT('Ctrl Pts',(1.71543711493337,-7.7272748975085,128.933930010972));
#228116=CARTESIAN_POINT('Ctrl Pts',(1.97213451803535,-7.66578139660503,
128.945645356666));
#228117=CARTESIAN_POINT('Ctrl Pts',(2.35427287560337,-7.55376624151274,
128.962712732675));
#228118=CARTESIAN_POINT('Ctrl Pts',(2.48226864710161,-7.51267795379807,
128.968365977846));
#228119=CARTESIAN_POINT('Ctrl Pts',(2.65338786730291,-7.45289532165581,
128.975840211399));
#228120=CARTESIAN_POINT('Ctrl Pts',(2.69747805664161,-7.43705103435778,
128.977758464128));
#228121=CARTESIAN_POINT('Ctrl Pts',(2.76135742078552,-7.41345248165311,
128.980527097822));
#228122=CARTESIAN_POINT('Ctrl Pts',(2.78125976513068,-7.40600881929687,
128.981388194214));
#228123=CARTESIAN_POINT('Ctrl Pts',(2.81682577116757,-7.39254321427327,
128.98292436005));
#228124=CARTESIAN_POINT('Ctrl Pts',(2.83250067671713,-7.38655146337526,
128.983600470272));
#228125=CARTESIAN_POINT('Ctrl Pts',(2.85611137178011,-7.37744003949338,
128.984617515344));
#228126=CARTESIAN_POINT('Ctrl Pts',(2.86406132761681,-7.37435735617696,
128.984959731137));
#228127=CARTESIAN_POINT('Ctrl Pts',(2.87784440894416,-7.36898716347637,
128.985552640318));
#228128=CARTESIAN_POINT('Ctrl Pts',(2.88367982105365,-7.36670556948244,
128.985803538423));
#228129=CARTESIAN_POINT('Ctrl Pts',(2.89569304677875,-7.3619920441611,128.986319801379));
#228130=CARTESIAN_POINT('Ctrl Pts',(2.90187052221981,-7.35955926343366,
128.986585136479));
#228131=CARTESIAN_POINT('Ctrl Pts',(2.9167361504912,-7.35368333336157,128.987223313316));
#228132=CARTESIAN_POINT('Ctrl Pts',(2.92542128910286,-7.35023255557451,
128.987595890229));
#228133=CARTESIAN_POINT('Ctrl Pts',(2.95205758337775,-7.33959473816933,
128.988737711222));
#228134=CARTESIAN_POINT('Ctrl Pts',(2.96998858247982,-7.3323572419146,128.989505204854));
#228135=CARTESIAN_POINT('Ctrl Pts',(3.17456864909349,-7.24890893759965,
128.998248929923));
#228136=CARTESIAN_POINT('Ctrl Pts',(3.35827186305671,-7.16565307873128,
129.005975281876));
#228137=CARTESIAN_POINT('Ctrl Pts',(3.93435451042694,-6.877540937294,129.029983956261));
#228138=CARTESIAN_POINT('Ctrl Pts',(4.31281672067203,-6.64675511712714,
129.045372360403));
#228139=CARTESIAN_POINT('Ctrl Pts',(4.95140949284133,-6.17972572264137,
129.072672902979));
#228140=CARTESIAN_POINT('Ctrl Pts',(5.21889344529578,-5.95555199761565,
129.08461894903));
#228141=CARTESIAN_POINT('Ctrl Pts',(5.63568574651383,-5.55653933214197,
129.105482985821));
#228142=CARTESIAN_POINT('Ctrl Pts',(5.79374395211244,-5.39153193491925,
129.114031790362));
#228143=CARTESIAN_POINT('Ctrl Pts',(5.96911166185044,-5.19182283514702,
129.124549050813));
#228144=CARTESIAN_POINT('Ctrl Pts',(5.99357745023262,-5.16355959249529,
129.126039824246));
#228145=CARTESIAN_POINT('Ctrl Pts',(6.02476760592542,-5.12700791292681,
129.12796978757));
#228146=CARTESIAN_POINT('Ctrl Pts',(6.03167705028848,-5.11887749454685,
129.128399207953));
#228147=CARTESIAN_POINT('Ctrl Pts',(6.04277749584214,-5.10576179948299,
129.129092108232));
#228148=CARTESIAN_POINT('Ctrl Pts',(6.04697884011277,-5.10078526544848,
129.129355058217));
#228149=CARTESIAN_POINT('Ctrl Pts',(6.05496431272556,-5.09130266198775,
129.129856168986));
#228150=CARTESIAN_POINT('Ctrl Pts',(6.05874957008869,-5.08679754571132,
129.130094272729));
#228151=CARTESIAN_POINT('Ctrl Pts',(6.06736076284103,-5.07652547723436,
129.130637231328));
#228152=CARTESIAN_POINT('Ctrl Pts',(6.07218350506904,-5.07075586355209,
129.130942243732));
#228153=CARTESIAN_POINT('Ctrl Pts',(6.08651380507773,-5.05356226852524,
129.13185129953));
#228154=CARTESIAN_POINT('Ctrl Pts',(6.09599737370257,-5.04211839581,129.132456502953));
#228155=CARTESIAN_POINT('Ctrl Pts',(6.16210077008492,-4.96189197258841,
129.136699924102));
#228156=CARTESIAN_POINT('Ctrl Pts',(6.21758625226706,-4.89218543582551,
129.140390386949));
#228157=CARTESIAN_POINT('Ctrl Pts',(6.39621230611836,-4.65982872987308,
129.15267116211));
#228158=CARTESIAN_POINT('Ctrl Pts',(6.51423746133555,-4.49335518141653,
129.16143543403));
#228159=CARTESIAN_POINT('Ctrl Pts',(6.8393047016571,-3.99508117137071,129.187272154833));
#228160=CARTESIAN_POINT('Ctrl Pts',(7.02835188804369,-3.65226481004147,
129.204537393867));
#228161=CARTESIAN_POINT('Ctrl Pts',(7.29706880874307,-3.06612835281899,
129.232514751419));
#228162=CARTESIAN_POINT('Ctrl Pts',(7.39169148306106,-2.83041709841477,
129.243393096487));
#228163=CARTESIAN_POINT('Ctrl Pts',(7.54724344703225,-2.38158595348237,
129.263368775281));
#228164=CARTESIAN_POINT('Ctrl Pts',(7.61087378349197,-2.16966389593463,
129.272507438292));
#228165=CARTESIAN_POINT('Ctrl Pts',(7.67797864688371,-1.90659292153293,
129.283529821171));
#228166=CARTESIAN_POINT('Ctrl Pts',(7.68994976157265,-1.85772048329132,
129.285564339855));
#228167=CARTESIAN_POINT('Ctrl Pts',(7.70589318839512,-1.78983467758121,
129.288372684894));
#228168=CARTESIAN_POINT('Ctrl Pts',(7.71026292040913,-1.77091606410035,
129.289153410071));
#228169=CARTESIAN_POINT('Ctrl Pts',(7.71751234138909,-1.73899442882002,
129.290467506746));
#228170=CARTESIAN_POINT('Ctrl Pts',(7.72042891959213,-1.72599990201667,
129.291001542816));
#228171=CARTESIAN_POINT('Ctrl Pts',(7.72611362560204,-1.7003695389147,129.292053096799));
#228172=CARTESIAN_POINT('Ctrl Pts',(7.72888360267606,-1.68773415621328,
129.292570647105));
#228173=CARTESIAN_POINT('Ctrl Pts',(7.7349371507878,-1.65979315423455,129.293713243481));
#228174=CARTESIAN_POINT('Ctrl Pts',(7.73820631103835,-1.64448445763401,
129.294338020872));
#228175=CARTESIAN_POINT('Ctrl Pts',(7.74898220148479,-1.59327985640897,
129.296423626402));
#228176=CARTESIAN_POINT('Ctrl Pts',(7.7562847979623,-1.55734133066358,129.297880615199));
#228177=CARTESIAN_POINT('Ctrl Pts',(7.83496790036148,-1.15582806876709,
129.314082903022));
#228178=CARTESIAN_POINT('Ctrl Pts',(7.88069636440455,-0.785690813013254,
129.328286311182));
#228179=CARTESIAN_POINT('Ctrl Pts',(7.92257113302998,0.0139858436980569,
129.358012417013));
#228180=CARTESIAN_POINT('Ctrl Pts',(7.91020120737385,0.442764543545203,
129.373355070737));
#228181=CARTESIAN_POINT('Ctrl Pts',(7.82792519090264,1.18773038202908,129.400866729264));
#228182=CARTESIAN_POINT('Ctrl Pts',(7.77324715621524,1.50456557210768,129.412862219009));
#228183=CARTESIAN_POINT('Ctrl Pts',(7.69459519072899,1.83781820207173,129.426509384832));
#228184=CARTESIAN_POINT('Ctrl Pts',(7.68964007831451,1.85844191375176,129.427358275959));
#228185=CARTESIAN_POINT('Ctrl Pts',(7.68272195800677,1.88673447370437,129.428529055246));
#228186=CARTESIAN_POINT('Ctrl Pts',(7.6808302617933,1.89442079463921,129.428847756864));
#228187=CARTESIAN_POINT('Ctrl Pts',(7.67763257676687,1.90733007135076,129.429384102417));
#228188=CARTESIAN_POINT('Ctrl Pts',(7.67633278405058,1.91255456738065,129.429601464126));
#228189=CARTESIAN_POINT('Ctrl Pts',(7.67376218915766,1.92284219700226,129.43003006821));
#228190=CARTESIAN_POINT('Ctrl Pts',(7.67249170635665,1.92790540899385,129.4302412958));
#228191=CARTESIAN_POINT('Ctrl Pts',(7.66969557617082,1.93900219198646,129.430704861462));
#228192=CARTESIAN_POINT('Ctrl Pts',(7.66816781978634,1.94503522304873,129.430957297891));
#228193=CARTESIAN_POINT('Ctrl Pts',(7.66288293442325,1.96580195635749,129.431827651203));
#228194=CARTESIAN_POINT('Ctrl Pts',(7.65909046459879,1.98052655834565,129.43244724182));
#228195=CARTESIAN_POINT('Ctrl Pts',(7.61456441630623,2.15136228279456,129.439665379117));
#228196=CARTESIAN_POINT('Ctrl Pts',(7.56911161931509,2.30618498420136,129.446509692779));
#228197=CARTESIAN_POINT('Ctrl Pts',(7.38674054891172,2.86371458039327,129.472047860212));
#228198=CARTESIAN_POINT('Ctrl Pts',(7.22214316172528,3.25659528591906,129.491720937577));
#228199=CARTESIAN_POINT('Ctrl Pts',(6.83393336215497,4.00717968178939,129.530684589541));
#228200=CARTESIAN_POINT('Ctrl Pts',(6.61170364121456,4.364121204987,129.549905582059));
#228201=CARTESIAN_POINT('Ctrl Pts',(6.19941041373206,4.92201592749204,129.580282507631));
#228202=CARTESIAN_POINT('Ctrl Pts',(6.02529962231773,5.13368419490476,129.591909539464));
#228203=CARTESIAN_POINT('Ctrl Pts',(5.82034681200733,5.35802024933356,129.604335771708));
#228204=CARTESIAN_POINT('Ctrl Pts',(5.8000202062194,5.38001706656734,129.605555472827));
#228205=CARTESIAN_POINT('Ctrl Pts',(5.76424083456069,5.41829793479299,129.607680452746));
#228206=CARTESIAN_POINT('Ctrl Pts',(5.74884282671335,5.43463256100433,129.608587948841));
#228207=CARTESIAN_POINT('Ctrl Pts',(5.72639942560201,5.45823901289664,129.609900591646));
#228208=CARTESIAN_POINT('Ctrl Pts',(5.7194093351351,5.46556313306869,129.610308012999));
#228209=CARTESIAN_POINT('Ctrl Pts',(5.70712460314805,5.47838553111681,129.611021578854));
#228210=CARTESIAN_POINT('Ctrl Pts',(5.70183603547348,5.48388959483867,129.611327973871));
#228211=CARTESIAN_POINT('Ctrl Pts',(5.6916354340797,5.49447513732278,129.611917424181));
#228212=CARTESIAN_POINT('Ctrl Pts',(5.68672454250177,5.49955770286471,129.612200526311));
#228213=CARTESIAN_POINT('Ctrl Pts',(5.67511487104764,5.51154104533416,129.612868203183));
#228214=CARTESIAN_POINT('Ctrl Pts',(5.66841029815454,5.51843620843801,129.613252536329));
#228215=CARTESIAN_POINT('Ctrl Pts',(5.64506487534329,5.54235783487604,129.614586466451));
#228216=CARTESIAN_POINT('Ctrl Pts',(5.62835967856365,5.55932146556517,129.615533372154));
#228217=CARTESIAN_POINT('Ctrl Pts',(5.42982145560681,5.75911896850382,129.626698178582));
#228218=CARTESIAN_POINT('Ctrl Pts',(5.23922370564749,5.93303975847275,129.636531279462));
#228219=CARTESIAN_POINT('Ctrl Pts',(4.69071232634645,6.38647440461411,129.662807833496));
#228220=CARTESIAN_POINT('Ctrl Pts',(4.31672502951896,6.6449790715276,129.678512860951));
#228221=CARTESIAN_POINT('Ctrl Pts',(3.59903318321788,7.05476708264577,129.707030019479));
#228222=CARTESIAN_POINT('Ctrl Pts',(3.26279447726962,7.21643458756564,129.719841866464));
#228223=CARTESIAN_POINT('Ctrl Pts',(2.7640030883237,7.41424960547021,129.739418952232));
#228224=CARTESIAN_POINT('Ctrl Pts',(2.60973700464503,7.4699450087469,129.745550763118));
#228225=CARTESIAN_POINT('Ctrl Pts',(2.38187893319387,7.54428965627332,129.754844284878));
#228226=CARTESIAN_POINT('Ctrl Pts',(2.30956975471727,7.56673906792916,129.757829598441));
#228227=CARTESIAN_POINT('Ctrl Pts',(2.22382234453675,7.59201702819807,129.761404961232));
#228228=CARTESIAN_POINT('Ctrl Pts',(2.21068245770068,7.59585356920209,129.761953806811));
#228229=CARTESIAN_POINT('Ctrl Pts',(2.19048857530311,7.60169287531331,129.762798700322));
#228230=CARTESIAN_POINT('Ctrl Pts',(2.18344160423823,7.60371997969149,129.763093801772));
#228231=CARTESIAN_POINT('Ctrl Pts',(2.17056123802547,7.60740571361684,129.763633652466));
#228232=CARTESIAN_POINT('Ctrl Pts',(2.16472872954231,7.6090674400245,129.763878283658));
#228233=CARTESIAN_POINT('Ctrl Pts',(2.15297506109052,7.6124015424406,129.764371609715));
#228234=CARTESIAN_POINT('Ctrl Pts',(2.14705384957303,7.61407372067037,129.764620311764));
#228235=CARTESIAN_POINT('Ctrl Pts',(2.13013549411853,7.61883024008114,129.765331407609));
#228236=CARTESIAN_POINT('Ctrl Pts',(2.11913363642794,7.6218976692058,129.765794421546));
#228237=CARTESIAN_POINT('Ctrl Pts',(2.07175039714012,7.63499807193604,129.767791003711));
#228238=CARTESIAN_POINT('Ctrl Pts',(2.03530442199564,7.64479438065512,129.76933294534));
#228239=CARTESIAN_POINT('Ctrl Pts',(1.86715990434793,7.6887022893419,129.776471483367));
#228240=CARTESIAN_POINT('Ctrl Pts',(1.73466802360506,7.71967317729758,129.78216561357));
#228241=CARTESIAN_POINT('Ctrl Pts',(1.18074385469772,7.83417635993924,129.8061114203));
#228242=CARTESIAN_POINT('Ctrl Pts',(0.753657426327338,7.88672796529521,
129.824851198811));
#228243=CARTESIAN_POINT('Ctrl Pts',(-0.10329475129395,7.92189989176989,
129.86171757323));
#228244=CARTESIAN_POINT('Ctrl Pts',(-0.531739692208522,7.90471047675374,
129.879782875525));
#228245=CARTESIAN_POINT('Ctrl Pts',(-1.27556625247278,7.81409206508833,
129.910739577785));
#228246=CARTESIAN_POINT('Ctrl Pts',(-1.59177649401483,7.75585960544128,
129.923832175341));
#228247=CARTESIAN_POINT('Ctrl Pts',(-1.95921065679009,7.66477010664329,
129.939157039336));
#228248=CARTESIAN_POINT('Ctrl Pts',(-2.01470023209559,7.65037189980341,
129.941473024668));
#228249=CARTESIAN_POINT('Ctrl Pts',(-2.0985775730029,7.62763188156648,129.94497638038));
#228250=CARTESIAN_POINT('Ctrl Pts',(-2.12708297004477,7.61973188476867,
129.94616743269));
#228251=CARTESIAN_POINT('Ctrl Pts',(-2.17652852498675,7.60572943706828,
129.948234254787));
#228252=CARTESIAN_POINT('Ctrl Pts',(-2.19748897189781,7.59969992243665,
129.949110657456));
#228253=CARTESIAN_POINT('Ctrl Pts',(-2.24450538002941,7.58596433426751,
129.951077122105));
#228254=CARTESIAN_POINT('Ctrl Pts',(-2.27054713296442,7.578210541027,129.952166738374));
#228255=CARTESIAN_POINT('Ctrl Pts',(-2.34032906498078,7.5570413524738,129.95508769805));
#228256=CARTESIAN_POINT('Ctrl Pts',(-2.38399375773189,7.54338040434978,
129.956916703571));
#228257=CARTESIAN_POINT('Ctrl Pts',(-2.58419937770159,7.47883203969176,
129.96530957834));
#228258=CARTESIAN_POINT('Ctrl Pts',(-2.73924811821045,7.42344502553817,
129.971827676718));
#228259=CARTESIAN_POINT('Ctrl Pts',(-2.91680045747469,7.35369839627158,
129.979331609379));
#228260=CARTESIAN_POINT('Ctrl Pts',(-2.94109573515341,7.34401531133811,
129.9803593054));
#228261=CARTESIAN_POINT('Ctrl Pts',(-3.08790237325577,7.28465897130143,
129.986575254708));
#228262=CARTESIAN_POINT('Ctrl Pts',(-3.20920157800645,7.23204142069894,
129.991736183988));
#228263=CARTESIAN_POINT('Ctrl Pts',(-3.67902000432681,7.01409330374899,
130.011879698824));
#228264=CARTESIAN_POINT('Ctrl Pts',(-4.0165722542617,6.82640736964534,130.026670153766));
#228265=CARTESIAN_POINT('Ctrl Pts',(-4.5213793949347,6.49527367366471,130.050165149765));
#228266=CARTESIAN_POINT('Ctrl Pts',(-4.69864996365079,6.36821292940971,
130.058715309478));
#228267=CARTESIAN_POINT('Ctrl Pts',(-4.89042197340382,6.2183869931454,130.068458733938));
#228268=CARTESIAN_POINT('Ctrl Pts',(-4.91032686411225,6.20268119058127,
130.069476245164));
#228269=CARTESIAN_POINT('Ctrl Pts',(-4.94011874340805,6.1789408551341,130.071008853701));
#228270=CARTESIAN_POINT('Ctrl Pts',(-4.95006244745346,6.1709776417661,130.071522030045));
#228271=CARTESIAN_POINT('Ctrl Pts',(-4.96713987380967,6.1572336954251,130.072406232153));
#228272=CARTESIAN_POINT('Ctrl Pts',(-4.97428285649951,6.15146448978461,
130.072776935103));
#228273=CARTESIAN_POINT('Ctrl Pts',(-4.98898736199602,6.13954567505202,
130.073541875344));
#228274=CARTESIAN_POINT('Ctrl Pts',(-4.99654759509067,6.13339450252123,
130.073936157213));
#228275=CARTESIAN_POINT('Ctrl Pts',(-5.01476880137936,6.11851327846581,
130.07488886193));
#228276=CARTESIAN_POINT('Ctrl Pts',(-5.02541832663489,6.10976935012077,
130.075447696393));
#228277=CARTESIAN_POINT('Ctrl Pts',(-5.06847217445395,6.0742307171994,130.077715260372));
#228278=CARTESIAN_POINT('Ctrl Pts',(-5.10068521770798,6.04720590428966,
130.07943091401));
#228279=CARTESIAN_POINT('Ctrl Pts',(-5.4145561294069,5.77959475056108,130.096327834523));
#228280=CARTESIAN_POINT('Ctrl Pts',(-5.67919828794121,5.51976723743063,
130.111988896187));
#228281=CARTESIAN_POINT('Ctrl Pts',(-6.24671695867545,4.87838608170758,
130.14811202078));
#228282=CARTESIAN_POINT('Ctrl Pts',(-6.53456480729434,4.48549027533,130.168433166312));
#228283=CARTESIAN_POINT('Ctrl Pts',(-6.81429437817311,4.01903724463986,
130.190529702024));
#228284=CARTESIAN_POINT('Ctrl Pts',(-6.84350456336735,3.96909480972181,
130.192872426639));
#228285=CARTESIAN_POINT('Ctrl Pts',(-6.88533379836675,3.89574206738144,
130.196280723487));
#228286=CARTESIAN_POINT('Ctrl Pts',(-6.89838670088746,3.87258165857005,
130.19735218012));
#228287=CARTESIAN_POINT('Ctrl Pts',(-6.92114982179581,3.83171163264294,
130.199234849875));
#228288=CARTESIAN_POINT('Ctrl Pts',(-6.93090941794958,3.81402982874741,
130.20004671747));
#228289=CARTESIAN_POINT('Ctrl Pts',(-6.94980348913918,3.77948676315984,
130.201627710446));
#228290=CARTESIAN_POINT('Ctrl Pts',(-6.95894457708538,3.76262928097667,
130.202396918238));
#228291=CARTESIAN_POINT('Ctrl Pts',(-6.98079279379227,3.72198605489603,
130.204245936735));
#228292=CARTESIAN_POINT('Ctrl Pts',(-6.99343978463542,3.69816822332976,
130.205324963003));
#228293=CARTESIAN_POINT('Ctrl Pts',(-7.0398361039095,3.6097017930393,130.20931638759));
#228294=CARTESIAN_POINT('Ctrl Pts',(-7.07281294742987,3.54465182177587,
130.212218993939));
#228295=CARTESIAN_POINT('Ctrl Pts',(-7.48334848831802,2.70628494892475,
130.249246710995));
#228296=CARTESIAN_POINT('Ctrl Pts',(-7.73319894900463,1.87676860163868,
130.281950644593));
#228297=CARTESIAN_POINT('Ctrl Pts',(-7.88891258386936,0.683148131472218,
130.326963227141));
#228298=CARTESIAN_POINT('Ctrl Pts',(-7.91111459673225,0.340420927446174,
130.339740904145));
#228299=CARTESIAN_POINT('Ctrl Pts',(-7.91094715504957,-0.158919179004584,
130.358948104736));
#228300=CARTESIAN_POINT('Ctrl Pts',(-7.90626464627182,-0.31514545146595,
130.365044852001));
#228301=CARTESIAN_POINT('Ctrl Pts',(-7.8959248475961,-0.488460202016362,
130.371980140228));
#228302=CARTESIAN_POINT('Ctrl Pts',(-7.894833592724,-0.505791563732877,
130.372675583515));
#228303=CARTESIAN_POINT('Ctrl Pts',(-7.89310764544519,-0.531835507013181,
130.373723662075));
#228304=CARTESIAN_POINT('Ctrl Pts',(-7.89251556967546,-0.540550914221878,
130.374074904111));
#228305=CARTESIAN_POINT('Ctrl Pts',(-7.89146638534851,-0.555625719132479,
130.374683342913));
#228306=CARTESIAN_POINT('Ctrl Pts',(-7.89101602141004,-0.561985587401749,
130.374940314203));
#228307=CARTESIAN_POINT('Ctrl Pts',(-7.89006612743187,-0.57517334290341,
130.375473755316));
#228308=CARTESIAN_POINT('Ctrl Pts',(-7.88956542179449,-0.582001137892017,
130.375750264801));
#228309=CARTESIAN_POINT('Ctrl Pts',(-7.8883708615974,-0.598005723140507,
130.376399193497));
#228310=CARTESIAN_POINT('Ctrl Pts',(-7.88766985631753,-0.607181959476842,
130.37677185914));
#228311=CARTESIAN_POINT('Ctrl Pts',(-7.88534843961067,-0.636886994390217,
130.377980238666));
#228312=CARTESIAN_POINT('Ctrl Pts',(-7.88366389126807,-0.657410600373982,
130.378818213768));
#228313=CARTESIAN_POINT('Ctrl Pts',(-7.85574887837748,-0.981963582256113,
130.392121191229));
#228314=CARTESIAN_POINT('Ctrl Pts',(-7.81203550088187,-1.28416447278493,
130.405368504632));
#228315=CARTESIAN_POINT('Ctrl Pts',(-7.60526204055151,-2.29657986755635,
130.451737270648));
#228316=CARTESIAN_POINT('Ctrl Pts',(-7.36166477587235,-2.98670651743664,
130.486064968325));
#228317=CARTESIAN_POINT('Ctrl Pts',(-6.92138990662583,-3.8381279818609,
130.527355029864));
#228318=CARTESIAN_POINT('Ctrl Pts',(-6.80682966955358,-4.03781449679715,
130.536989878815));
#228319=CARTESIAN_POINT('Ctrl Pts',(-6.67169625797304,-4.25122278565904,
130.54722595989));
#228320=CARTESIAN_POINT('Ctrl Pts',(-6.65959155835353,-4.27015999918037,
130.548133780671));
#228321=CARTESIAN_POINT('Ctrl Pts',(-6.64242977747168,-4.29675830184028,
130.549408192292));
#228322=CARTESIAN_POINT('Ctrl Pts',(-6.63743986873736,-4.30446248011,130.549777245159));
#228323=CARTESIAN_POINT('Ctrl Pts',(-6.62873999585265,-4.31784356570039,
130.550418103538));
#228324=CARTESIAN_POINT('Ctrl Pts',(-6.62503612423523,-4.32352441225514,
130.550690133039));
#228325=CARTESIAN_POINT('Ctrl Pts',(-6.61729763272182,-4.33536010037516,
130.551256802566));
#228326=CARTESIAN_POINT('Ctrl Pts',(-6.61326171877062,-4.34151409065737,
130.551551394426));
#228327=CARTESIAN_POINT('Ctrl Pts',(-6.6037086360126,-4.35603646900358,
130.552246467948));
#228328=CARTESIAN_POINT('Ctrl Pts',(-6.59818413273516,-4.36440002979814,
130.552646677419));
#228329=CARTESIAN_POINT('Ctrl Pts',(-6.57994574852593,-4.39189739061122,
130.553962184657));
#228330=CARTESIAN_POINT('Ctrl Pts',(-6.56716436534541,-4.41098639229762,
130.554874970822));
#228331=CARTESIAN_POINT('Ctrl Pts',(-6.33239244413116,-4.75833600826952,
130.571476716409));
#228332=CARTESIAN_POINT('Ctrl Pts',(-6.08612144810702,-5.06952919780342,
130.586185620073));
#228333=CARTESIAN_POINT('Ctrl Pts',(-5.40931165844547,-5.80397849971194,
130.621624330112));
#228334=CARTESIAN_POINT('Ctrl Pts',(-4.95184523238778,-6.19887101719241,
130.641308498791));
#228335=CARTESIAN_POINT('Ctrl Pts',(-4.36253865693198,-6.60033556069919,
130.666325569196));
#228336=CARTESIAN_POINT('Ctrl Pts',(-4.26976414064126,-6.66072715354705,
130.670260277475));
#228337=CARTESIAN_POINT('Ctrl Pts',(-4.13358030302506,-6.74536141243194,
130.676071222838));
#228338=CARTESIAN_POINT('Ctrl Pts',(-4.09116010634702,-6.77117386944939,
130.677886126856));
#228339=CARTESIAN_POINT('Ctrl Pts',(-3.9610349422242,-6.84868511425587,
130.683475983347));
#228340=CARTESIAN_POINT('Ctrl Pts',(-3.87257475343541,-6.89909045433856,
130.687306948206));
#228341=CARTESIAN_POINT('Ctrl Pts',(-3.73249063600178,-6.97536841249642,
130.69345706889));
#228342=CARTESIAN_POINT('Ctrl Pts',(-3.68151258041225,-7.00240784800352,
130.695712104521));
#228343=CARTESIAN_POINT('Ctrl Pts',(-3.60600701792215,-7.04140458558351,
130.699083059605));
#228344=CARTESIAN_POINT('Ctrl Pts',(-3.58170532336805,-7.05379699835596,
130.700172679809));
#228345=CARTESIAN_POINT('Ctrl Pts',(-3.55054418252642,-7.06948476915608,
130.701576374706));
#228346=CARTESIAN_POINT('Ctrl Pts',(-3.54374315800858,-7.07289638851776,
130.701883131242));
#228347=CARTESIAN_POINT('Ctrl Pts',(-3.53291341633145,-7.07830940471843,
130.702372244711));
#228348=CARTESIAN_POINT('Ctrl Pts',(-3.52888788124158,-7.08031719329628,
130.70255419494));
#228349=CARTESIAN_POINT('Ctrl Pts',(-3.5213671453463,-7.0840602520952,130.702894392296));
#228350=CARTESIAN_POINT('Ctrl Pts',(-3.51787236697227,-7.08579637283116,
130.70305258488));
#228351=CARTESIAN_POINT('Ctrl Pts',(-3.51009740587929,-7.08965161428452,
130.703404764067));
#228352=CARTESIAN_POINT('Ctrl Pts',(-3.50581658887822,-7.09176944461953,
130.703598833655));
#228353=CARTESIAN_POINT('Ctrl Pts',(-3.49338332400954,-7.09790649193071,
130.704162972476));
#228354=CARTESIAN_POINT('Ctrl Pts',(-3.48522587417126,-7.10191553193301,
130.704533703228));
#228355=CARTESIAN_POINT('Ctrl Pts',(-3.42282419987054,-7.13244989618076,
130.707374348834));
#228356=CARTESIAN_POINT('Ctrl Pts',(-3.36828620527822,-7.15836676088272,
130.709883861813));
#228357=CARTESIAN_POINT('Ctrl Pts',(-3.18242524124949,-7.24409505234318,
130.718511162981));
#228358=CARTESIAN_POINT('Ctrl Pts',(-3.04976919386851,-7.30093468406857,
130.724794313426));
#228359=CARTESIAN_POINT('Ctrl Pts',(-2.74491364720468,-7.42179891708394,
130.739381180108));
#228360=CARTESIAN_POINT('Ctrl Pts',(-2.57188746323626,-7.48351789944077,
130.747763540692));
#228361=CARTESIAN_POINT('Ctrl Pts',(-1.87024865897849,-7.70658555893855,
130.781729527731));
#228362=CARTESIAN_POINT('Ctrl Pts',(-1.32746337206994,-7.81839083765405,
130.807805887729));
#228363=CARTESIAN_POINT('Ctrl Pts',(-0.605502295850416,-7.88968564964103,
130.839885127073));
#228364=CARTESIAN_POINT('Ctrl Pts',(-0.43304584130309,-7.90102835415054,
130.847370768208));
#228365=CARTESIAN_POINT('Ctrl Pts',(-0.108900807741692,-7.91170164029605,
130.861081545278));
#228366=CARTESIAN_POINT('Ctrl Pts',(0.0426639127485166,-7.91233629472284,
130.867345853968));
#228367=CARTESIAN_POINT('Ctrl Pts',(0.213453486238489,-7.90814333950836,
130.874242794877));
#228368=CARTESIAN_POINT('Ctrl Pts',(0.23274542477781,-7.90759906948013,
130.875019539904));
#228369=CARTESIAN_POINT('Ctrl Pts',(0.260806475700599,-7.90670462293567,
130.876146013363));
#228370=CARTESIAN_POINT('Ctrl Pts',(0.269577224197976,-7.90641044551862,
130.876497628714));
#228371=CARTESIAN_POINT('Ctrl Pts',(0.285051348138922,-7.9058656531978,
130.877117145507));
#228372=CARTESIAN_POINT('Ctrl Pts',(0.29175491991475,-7.90562110554905,
130.877385251292));
#228373=CARTESIAN_POINT('Ctrl Pts',(0.305608344632387,-7.90509808524587,
130.877938742926));
#228374=CARTESIAN_POINT('Ctrl Pts',(0.31275814860346,-7.90481843804919,
130.878224088902));
#228375=CARTESIAN_POINT('Ctrl Pts',(0.331047414985672,-7.90407824532979,
130.878953208763));
#228376=CARTESIAN_POINT('Ctrl Pts',(0.342186319213008,-7.90360385037199,
130.879396515041));
#228377=CARTESIAN_POINT('Ctrl Pts',(0.3874866545255,-7.90157860794142,130.881196318539));
#228378=CARTESIAN_POINT('Ctrl Pts',(0.4216391151913,-7.89982980206562,130.882546130952));
#228379=CARTESIAN_POINT('Ctrl Pts',(0.642704926114706,-7.88707226245944,
130.891238545469));
#228380=CARTESIAN_POINT('Ctrl Pts',(0.829194890535647,-7.86965185391553,
130.898361753168));
#228381=CARTESIAN_POINT('Ctrl Pts',(1.16429993988588,-7.82630311803096,
130.910859990856));
#228382=CARTESIAN_POINT('Ctrl Pts',(1.31312090800703,-7.80271304095509,
130.916302435787));
#228383=CARTESIAN_POINT('Ctrl Pts',(1.94282853979077,-7.68436825528129,
130.939018531948));
#228384=CARTESIAN_POINT('Ctrl Pts',(2.4150306847506,-7.54928621885128,130.955190881259));
#228385=CARTESIAN_POINT('Ctrl Pts',(3.06268251901901,-7.29697992622877,
130.978878383457));
#228386=CARTESIAN_POINT('Ctrl Pts',(3.2507162750062,-7.21517695087289,130.985960865659));
#228387=CARTESIAN_POINT('Ctrl Pts',(3.49069392962469,-7.09948949748859,
130.995517325331));
#228388=CARTESIAN_POINT('Ctrl Pts',(3.54572043577076,-7.07216809678589,
130.997745173024));
#228389=CARTESIAN_POINT('Ctrl Pts',(3.6842575373213,-7.0013592862187,131.003460988402));
#228390=CARTESIAN_POINT('Ctrl Pts',(3.76731868403214,-6.95701762966985,
131.006987661926));
#228391=CARTESIAN_POINT('Ctrl Pts',(3.92066106283459,-6.8716053810305,131.013723306125));
#228392=CARTESIAN_POINT('Ctrl Pts',(3.99113846528694,-6.8309118381627,131.016910111055));
#228393=CARTESIAN_POINT('Ctrl Pts',(4.06913227931461,-6.78425927305019,
131.020554014006));
#228394=CARTESIAN_POINT('Ctrl Pts',(4.07728258699863,-6.77936413645787,
131.020936245805));
#228395=CARTESIAN_POINT('Ctrl Pts',(4.08950222005293,-6.77199492562322,
131.021511524471));
#228396=CARTESIAN_POINT('Ctrl Pts',(4.09357818913035,-6.76953183683631,
131.021703783102));
#228397=CARTESIAN_POINT('Ctrl Pts',(4.10064421631865,-6.76525315475101,
131.022037722703));
#228398=CARTESIAN_POINT('Ctrl Pts',(4.1036352811846,-6.7634392667957,131.022179279961));
#228399=CARTESIAN_POINT('Ctrl Pts',(4.10986349334535,-6.75965660527918,
131.02247445561));
#228400=CARTESIAN_POINT('Ctrl Pts',(4.11310043046326,-6.75768748937437,
131.022628098535));
#228401=CARTESIAN_POINT('Ctrl Pts',(4.12073008184018,-6.75303865452489,
131.022990792916));
#228402=CARTESIAN_POINT('Ctrl Pts',(4.12512159400354,-6.7503569765844,131.023199983893));
#228403=CARTESIAN_POINT('Ctrl Pts',(4.13950967279792,-6.74155160923391,
131.023886764865));
#228404=CARTESIAN_POINT('Ctrl Pts',(4.14949520089733,-6.73541001023058,
131.024365619414));
#228405=CARTESIAN_POINT('Ctrl Pts',(4.50425717106616,-6.51612531719592,
131.04145614003));
#228406=CARTESIAN_POINT('Ctrl Pts',(4.83212219284879,-6.27684185932895,
131.059854790864));
#228407=CARTESIAN_POINT('Ctrl Pts',(5.46436521001771,-5.73642090136131,
131.098573312149));
#228408=CARTESIAN_POINT('Ctrl Pts',(5.76563343454988,-5.43353517267719,
131.118861876848));
#228409=CARTESIAN_POINT('Ctrl Pts',(6.36707653687011,-4.72221163336846,
131.161751988428));
#228410=CARTESIAN_POINT('Ctrl Pts',(6.65549635243849,-4.30620995182937,
131.183953658628));
#228411=CARTESIAN_POINT('Ctrl Pts',(6.91910937631706,-3.8354958025182,131.205915473879));
#228412=CARTESIAN_POINT('Ctrl Pts',(6.93571003823924,-3.80539471262152,
131.207307472985));
#228413=CARTESIAN_POINT('Ctrl Pts',(6.9577906603516,-3.76473261010134,131.209171402791));
#228414=CARTESIAN_POINT('Ctrl Pts',(6.96344362836989,-3.75426628451074,
131.209649715423));
#228415=CARTESIAN_POINT('Ctrl Pts',(6.97227729335187,-3.73782238628518,
131.210398928716));
#228416=CARTESIAN_POINT('Ctrl Pts',(6.97547394770028,-3.73185343389311,
131.210670415605));
#228417=CARTESIAN_POINT('Ctrl Pts',(6.98159595285452,-3.72038677200616,
131.211191058068));
#228418=CARTESIAN_POINT('Ctrl Pts',(6.9845224821248,-3.71488969946119,131.211440256731));
#228419=CARTESIAN_POINT('Ctrl Pts',(6.99138177683038,-3.70196872371084,
131.212025077482));
#228420=CARTESIAN_POINT('Ctrl Pts',(6.99530921698123,-3.69454199328287,
131.212360504682));
#228421=CARTESIAN_POINT('Ctrl Pts',(7.0066246321403,-3.67306198425774,131.213328584568));
#228422=CARTESIAN_POINT('Ctrl Pts',(7.01398216103787,-3.65899266526142,
131.21396012719));
#228423=CARTESIAN_POINT('Ctrl Pts',(7.06360765230317,-3.56339739235665,
131.218234084477));
#228424=CARTESIAN_POINT('Ctrl Pts',(7.10449645715328,-3.48116142289665,
131.221826367483));
#228425=CARTESIAN_POINT('Ctrl Pts',(7.18096130069846,-3.32041285917845,
131.228694820407));
#228426=CARTESIAN_POINT('Ctrl Pts',(7.21670418007605,-3.2419944602089,131.231976363417));
#228427=CARTESIAN_POINT('Ctrl Pts',(7.37733024898325,-2.87376084165445,
131.247088627686));
#228428=CARTESIAN_POINT('Ctrl Pts',(7.48608588906328,-2.57721515750595,
131.258395927004));
#228429=CARTESIAN_POINT('Ctrl Pts',(7.69998956580586,-1.86479861383034,
131.284430489986));
#228430=CARTESIAN_POINT('Ctrl Pts',(7.78962790029915,-1.44533534284104,
131.298880235897));
#228431=CARTESIAN_POINT('Ctrl Pts',(7.88680415239507,-0.698452646272621,
131.325551606683));
#228432=CARTESIAN_POINT('Ctrl Pts',(7.90883663642662,-0.373937185808327,
131.337495310781));
#228433=CARTESIAN_POINT('Ctrl Pts',(7.91099372363021,-0.0255011837131471,
131.351379417631));
#228434=CARTESIAN_POINT('Ctrl Pts',(7.91103456431694,-0.00202776225569635,
131.352319127705));
#228435=CARTESIAN_POINT('Ctrl Pts',(7.91094843688656,0.0297438130795243,
131.353596689119));
#228436=CARTESIAN_POINT('Ctrl Pts',(7.91091288363323,0.0380422450148598,
131.353930897875));
#228437=CARTESIAN_POINT('Ctrl Pts',(7.91083067877513,0.0520755478662569,
131.354496939756));
#228438=CARTESIAN_POINT('Ctrl Pts',(7.91079084802368,0.057810461949476,
131.354728506332));
#228439=CARTESIAN_POINT('Ctrl Pts',(7.91070232387717,0.0688308166460872,
131.35517395658));
#228440=CARTESIAN_POINT('Ctrl Pts',(7.91065456947036,0.0741162644690045,
131.355387804022));
#228441=CARTESIAN_POINT('Ctrl Pts',(7.91052977514755,0.0865492319514098,
131.355891317345));
#228442=CARTESIAN_POINT('Ctrl Pts',(7.91044834517563,0.0936966964467147,
131.356181149983));
#228443=CARTESIAN_POINT('Ctrl Pts',(7.91018433197714,0.114406289302989,
131.35702199774));
#228444=CARTESIAN_POINT('Ctrl Pts',(7.90997655776122,0.127968034002399,
131.357573953337));
#228445=CARTESIAN_POINT('Ctrl Pts',(7.90832600963994,0.220213333147443,
131.361337047475));
#228446=CARTESIAN_POINT('Ctrl Pts',(7.90574411678412,0.298870625549505,
131.364589157162));
#228447=CARTESIAN_POINT('Ctrl Pts',(7.89362925044877,0.552481152398151,
131.375192762896));
#228448=CARTESIAN_POINT('Ctrl Pts',(7.87945794921925,0.727156734810832,
131.382676654555));
#228449=CARTESIAN_POINT('Ctrl Pts',(7.7716684952341,1.6671923623803,131.423568638727));
#228450=CARTESIAN_POINT('Ctrl Pts',(7.57230951313802,2.41634109516279,131.457891496573));
#228451=CARTESIAN_POINT('Ctrl Pts',(7.20290668976725,3.27551191870523,131.496712989455));
#228452=CARTESIAN_POINT('Ctrl Pts',(7.13342156389494,3.4241995096306,131.503432513099));
#228453=CARTESIAN_POINT('Ctrl Pts',(7.04622159119718,3.5965997524717,131.511242978615));
#228454=CARTESIAN_POINT('Ctrl Pts',(7.03293867726194,3.62250494389511,131.512417171674));
#228455=CARTESIAN_POINT('Ctrl Pts',(7.01164104571621,3.66348225247664,131.514275431587));
#228456=CARTESIAN_POINT('Ctrl Pts',(7.00372003802315,3.67860272383894,131.514961316352));
#228457=CARTESIAN_POINT('Ctrl Pts',(6.98971296462401,3.70513169279424,131.516165040947));
#228458=CARTESIAN_POINT('Ctrl Pts',(6.98364775887051,3.71655111225107,131.516683294972));
#228459=CARTESIAN_POINT('Ctrl Pts',(6.97196187460413,3.73842339381317,131.51767614622));
#228460=CARTESIAN_POINT('Ctrl Pts',(6.96634561878001,3.74887857538239,131.518150831547));
#228461=CARTESIAN_POINT('Ctrl Pts',(6.95155944863181,3.77625643920008,131.519394080109));
#228462=CARTESIAN_POINT('Ctrl Pts',(6.94235125094906,3.79315839042393,131.520161851769));
#228463=CARTESIAN_POINT('Ctrl Pts',(6.90869572393306,3.85440114100887,131.522944692225));
#228464=CARTESIAN_POINT('Ctrl Pts',(6.88388438649135,3.89854082803961,131.524952060594));
#228465=CARTESIAN_POINT('Ctrl Pts',(6.82282275927925,4.00476956525558,131.529787516396));
#228466=CARTESIAN_POINT('Ctrl Pts',(6.78614636501044,4.06660883263131,131.532606076452));
#228467=CARTESIAN_POINT('Ctrl Pts',(6.62755730968866,4.32588078857785,131.544442900794));
#228468=CARTESIAN_POINT('Ctrl Pts',(6.49783043401172,4.51840307414474,131.553275960361));
#228469=CARTESIAN_POINT('Ctrl Pts',(6.11657028029414,5.0337639721956,131.577246613157));
#228470=CARTESIAN_POINT('Ctrl Pts',(5.84818566009107,5.34321433293493,131.591986630454));
#228471=CARTESIAN_POINT('Ctrl Pts',(5.32500385328593,5.85957107808733,131.618797505408));
#228472=CARTESIAN_POINT('Ctrl Pts',(5.07900515266533,6.0740368180053,131.630791900848));
#228473=CARTESIAN_POINT('Ctrl Pts',(4.76057620459584,6.31874555688031,131.646428534573));
#228474=CARTESIAN_POINT('Ctrl Pts',(4.70000391809516,6.3639291230061,131.649408269933));
#228475=CARTESIAN_POINT('Ctrl Pts',(4.62835075171268,6.41579742219139,131.652950318863));
#228476=CARTESIAN_POINT('Ctrl Pts',(4.6178880243812,6.42333226876395,131.653467949892));
#228477=CARTESIAN_POINT('Ctrl Pts',(4.60207960846132,6.43465828356091,131.654250763827));
#228478=CARTESIAN_POINT('Ctrl Pts',(4.59674751986884,6.43846846594865,131.654514924134));
#228479=CARTESIAN_POINT('Ctrl Pts',(4.58722308571632,6.44525653527459,131.654987008186));
#228480=CARTESIAN_POINT('Ctrl Pts',(4.58303255505015,6.44823697166854,131.655194792889));
#228481=CARTESIAN_POINT('Ctrl Pts',(4.57418602009187,6.45451592392825,131.655633614745));
#228482=CARTESIAN_POINT('Ctrl Pts',(4.56952934885523,6.45781349129409,131.655864703849));
#228483=CARTESIAN_POINT('Ctrl Pts',(4.55720824186382,6.46651853974445,131.656476420007));
#228484=CARTESIAN_POINT('Ctrl Pts',(4.54953776548107,6.47191742097055,131.656857524846));
#228485=CARTESIAN_POINT('Ctrl Pts',(4.51532689407749,6.49590594206585,131.658558618974));
#228486=CARTESIAN_POINT('Ctrl Pts',(4.4886821612934,6.51434596906616,131.659887086957));
#228487=CARTESIAN_POINT('Ctrl Pts',(4.41854378725765,6.56225202832388,131.663395425983));
#228488=CARTESIAN_POINT('Ctrl Pts',(4.37486935980116,6.59144891154052,131.665591119698));
#228489=CARTESIAN_POINT('Ctrl Pts',(4.18222597206528,6.71747528828708,131.675314119173));
#228490=CARTESIAN_POINT('Ctrl Pts',(4.030316427061,6.80970126991515,131.683079322232));
#228491=CARTESIAN_POINT('Ctrl Pts',(3.57064907029234,7.06799947699284,131.706603090643));
#228492=CARTESIAN_POINT('Ctrl Pts',(3.25484851122357,7.21887109479932,131.722785671932));
#228493=CARTESIAN_POINT('Ctrl Pts',(2.30051042776497,7.59940805275421,131.770143569925));
#228494=CARTESIAN_POINT('Ctrl Pts',(1.6411541164364,7.76854150435772,131.800685987257));
#228495=CARTESIAN_POINT('Ctrl Pts',(0.923734459519948,7.8570125549352,131.830250308261));
#228496=CARTESIAN_POINT('Ctrl Pts',(0.879185110662258,7.86212218579703,
131.832072835756));
#228497=CARTESIAN_POINT('Ctrl Pts',(0.820769300509547,7.86831951791108,
131.834445501075));
#228498=CARTESIAN_POINT('Ctrl Pts',(0.806940458294124,7.86974976602352,
131.835005928705));
#228499=CARTESIAN_POINT('Ctrl Pts',(0.785596700086403,7.87190039414498,
131.835868980404));
#228500=CARTESIAN_POINT('Ctrl Pts',(0.778084434378132,7.87264648030756,
131.836172376977));
#228501=CARTESIAN_POINT('Ctrl Pts',(0.763125459445799,7.8741105213042,131.836775793019));
#228502=CARTESIAN_POINT('Ctrl Pts',(0.755678777170742,7.8748286682747,131.837075817971));
#228503=CARTESIAN_POINT('Ctrl Pts',(0.739173761606479,7.87639676029255,
131.83774000679));
#228504=CARTESIAN_POINT('Ctrl Pts',(0.730114952277006,7.87724164492489,
131.838104018211));
#228505=CARTESIAN_POINT('Ctrl Pts',(0.703990730607179,7.87963271155895,
131.839152251478));
#228506=CARTESIAN_POINT('Ctrl Pts',(0.686921680075027,7.88113908187342,
131.839835276647));
#228507=CARTESIAN_POINT('Ctrl Pts',(0.572489277602448,7.89086333412594,
131.844401935068));
#228508=CARTESIAN_POINT('Ctrl Pts',(0.474983928235118,7.89733241114043,
131.848232796594));
#228509=CARTESIAN_POINT('Ctrl Pts',(0.209217416272467,7.91002482681946,
131.85852275347));
#228510=CARTESIAN_POINT('Ctrl Pts',(0.040835140910128,7.91268606893869,
131.864876189681));
#228511=CARTESIAN_POINT('Ctrl Pts',(-0.297661556367035,7.90722946366799,
131.877385067391));
#228512=CARTESIAN_POINT('Ctrl Pts',(-0.467684352132172,7.89899704895067,
131.883534334743));
#228513=CARTESIAN_POINT('Ctrl Pts',(-0.850894902728228,7.86802477374352,
131.897206312108));
#228514=CARTESIAN_POINT('Ctrl Pts',(-1.06368980779961,7.84209173778786,
131.904665435726));
#228515=CARTESIAN_POINT('Ctrl Pts',(-1.46461698824881,7.77661010817831,
131.918716868003));
#228516=CARTESIAN_POINT('Ctrl Pts',(-1.6528722614479,7.73878418070761,131.925314438363));
#228517=CARTESIAN_POINT('Ctrl Pts',(-2.29167004799866,7.58605647036536,
131.948093758971));
#228518=CARTESIAN_POINT('Ctrl Pts',(-2.73336750502716,7.43832651494931,
131.964526792273));
#228519=CARTESIAN_POINT('Ctrl Pts',(-3.18963915183753,7.23955812774204,
131.984222122834));
#228520=CARTESIAN_POINT('Ctrl Pts',(-3.21966877286616,7.22625302312937,
131.985530418814));
#228521=CARTESIAN_POINT('Ctrl Pts',(-3.25948427929215,7.20831467279348,
131.987280321433));
#228522=CARTESIAN_POINT('Ctrl Pts',(-3.26934502896877,7.20384767114533,
131.987714955105));
#228523=CARTESIAN_POINT('Ctrl Pts',(-3.28468332133363,7.19686131788961,
131.988392940262));
#228524=CARTESIAN_POINT('Ctrl Pts',(-3.29016722678858,7.19435591070613,
131.988635722847));
#228525=CARTESIAN_POINT('Ctrl Pts',(-3.30117281597283,7.1893126214522,131.989123721389));
#228526=CARTESIAN_POINT('Ctrl Pts',(-3.30669445001531,7.18677464123304,
131.98936894119));
#228527=CARTESIAN_POINT('Ctrl Pts',(-3.31906022764567,7.18107353068025,
131.989918969774));
#228528=CARTESIAN_POINT('Ctrl Pts',(-3.32590278035102,7.17790697508421,
131.990223913795));
#228529=CARTESIAN_POINT('Ctrl Pts',(-3.34604527187692,7.16855056768209,
131.991123293318));
#228530=CARTESIAN_POINT('Ctrl Pts',(-3.35933249525944,7.16233351539971,
131.991718781771));
#228531=CARTESIAN_POINT('Ctrl Pts',(-3.46030491137074,7.11474603410072,
131.99626042358));
#228532=CARTESIAN_POINT('Ctrl Pts',(-3.54723846981561,7.07180455258907,
132.000264749638));
#228533=CARTESIAN_POINT('Ctrl Pts',(-3.84895828295636,6.91580439792312,
132.014447614189));
#228534=CARTESIAN_POINT('Ctrl Pts',(-4.05930867461679,6.79447110254698,
132.024845285061));
#228535=CARTESIAN_POINT('Ctrl Pts',(-4.48271654169488,6.52355379602759,
132.04651220676));
#228536=CARTESIAN_POINT('Ctrl Pts',(-4.694653459865,6.37273349570443,132.057776401105));
#228537=CARTESIAN_POINT('Ctrl Pts',(-5.20093430068734,5.97346481957138,
132.0854879719));
#228538=CARTESIAN_POINT('Ctrl Pts',(-5.48530798932626,5.71344167026328,
132.101766426826));
#228539=CARTESIAN_POINT('Ctrl Pts',(-5.98411674809319,5.18563482811866,
132.131884562175));
#228540=CARTESIAN_POINT('Ctrl Pts',(-6.20229657354122,4.92259953994062,
132.145810219661));
#228541=CARTESIAN_POINT('Ctrl Pts',(-6.44389387263535,4.58966749226703,
132.162486407668));
#228542=CARTESIAN_POINT('Ctrl Pts',(-6.48423221442287,4.53249915616988,
132.165316053974));
#228543=CARTESIAN_POINT('Ctrl Pts',(-6.54197736644485,4.44831260587567,
132.169434076157));
#228544=CARTESIAN_POINT('Ctrl Pts',(-6.55998617648189,4.4217116906728,132.170728270737));
#228545=CARTESIAN_POINT('Ctrl Pts',(-6.59144070679422,4.37463488785543,
132.173006415794));
#228546=CARTESIAN_POINT('Ctrl Pts',(-6.60495426721267,4.35420487863197,
132.173991043116));
#228547=CARTESIAN_POINT('Ctrl Pts',(-6.63069672704732,4.31489142663367,
132.175878096419));
#228548=CARTESIAN_POINT('Ctrl Pts',(-6.64294038764321,4.29601793745975,
132.176780667927));
#228549=CARTESIAN_POINT('Ctrl Pts',(-6.66894044328155,4.2555621697856,132.178708224298));
#228550=CARTESIAN_POINT('Ctrl Pts',(-6.68267295521114,4.23396483159602,
132.179732948371));
#228551=CARTESIAN_POINT('Ctrl Pts',(-6.73280024654331,4.15427741431908,
132.183498189338));
#228552=CARTESIAN_POINT('Ctrl Pts',(-6.7685445050632,4.09578141101457,132.18623164309));
#228553=CARTESIAN_POINT('Ctrl Pts',(-6.93598247194728,3.81358750531054,
132.199277272731));
#228554=CARTESIAN_POINT('Ctrl Pts',(-7.05737464637724,3.58396006838076,
132.209468635308));
#228555=CARTESIAN_POINT('Ctrl Pts',(-7.25448840815833,3.16208503612219,
132.227604503703));
#228556=CARTESIAN_POINT('Ctrl Pts',(-7.33438974739932,2.97205513817852,
132.235573410499));
#228557=CARTESIAN_POINT('Ctrl Pts',(-7.54507205021783,2.41055488400625,
132.258754609685));
#228558=CARTESIAN_POINT('Ctrl Pts',(-7.65565638841629,2.03218969031106,
132.273909238018));
#228559=CARTESIAN_POINT('Ctrl Pts',(-7.74662623168385,1.60485990944624,
132.291318220727));
#228560=CARTESIAN_POINT('Ctrl Pts',(-7.75528824480562,1.56246519802373,
132.293048720586));
#228561=CARTESIAN_POINT('Ctrl Pts',(-7.76673552693982,1.50399675412808,
132.295441524756));
#228562=CARTESIAN_POINT('Ctrl Pts',(-7.76981958350817,1.48798206266565,
132.296097559713));
#228563=CARTESIAN_POINT('Ctrl Pts',(-7.77466025913748,1.46242028333684,
132.297145802009));
#228564=CARTESIAN_POINT('Ctrl Pts',(-7.77644887100753,1.4528792744493,132.297537308999));
#228565=CARTESIAN_POINT('Ctrl Pts',(-7.77998983362453,1.4337968121707,132.298320861744));
#228566=CARTESIAN_POINT('Ctrl Pts',(-7.78174220361343,1.42425537940682,
132.298712906321));
#228567=CARTESIAN_POINT('Ctrl Pts',(-7.78523658949436,1.40502991446249,
132.299503404207));
#228568=CARTESIAN_POINT('Ctrl Pts',(-7.78697809747688,1.39534580791992,
132.299901868415));
#228569=CARTESIAN_POINT('Ctrl Pts',(-7.79091587444081,1.37321180477954,
132.300813270469));
#228570=CARTESIAN_POINT('Ctrl Pts',(-7.79310036643597,1.36075989811202,
132.301326489492));
#228571=CARTESIAN_POINT('Ctrl Pts',(-7.79871935068607,1.32827356421151,
132.302666729167));
#228572=CARTESIAN_POINT('Ctrl Pts',(-7.80210647919657,1.30823111629935,
132.303494843883));
#228573=CARTESIAN_POINT('Ctrl Pts',(-7.81212380183295,1.24753337073086,
132.30600627133));
#228574=CARTESIAN_POINT('Ctrl Pts',(-7.81851370903775,1.20683932001855,
132.307694791727));
#228575=CARTESIAN_POINT('Ctrl Pts',(-7.88191327525664,0.781424354597747,
132.32538857553));
#228576=CARTESIAN_POINT('Ctrl Pts',(-7.91079421575543,0.393060249264107,
132.341872565054));
#228577=CARTESIAN_POINT('Ctrl Pts',(-7.91099890422817,0.00416380844229285,
132.358262606746));
#228578=CARTESIAN_POINT('',(-7.90831251326435,6.9057182936028E-7,134.357573016214));
#228579=CARTESIAN_POINT('Ctrl Pts',(-7.90996818647143,0.00413822696500661,
132.357668491763));
#228580=CARTESIAN_POINT('Ctrl Pts',(-7.90766063577685,-0.852908314836981,
132.392201808104));
#228581=CARTESIAN_POINT('Ctrl Pts',(-7.55022317271499,-3.02898935298784,
132.479719913055));
#228582=CARTESIAN_POINT('Ctrl Pts',(-4.88042203922493,-7.22662596088967,
132.67320759522));
#228583=CARTESIAN_POINT('Ctrl Pts',(2.32377147178489,-9.06459362976759,
132.938131538262));
#228584=CARTESIAN_POINT('Ctrl Pts',(8.89536617229082,-2.9274547798747,133.256040269912));
#228585=CARTESIAN_POINT('Ctrl Pts',(7.52945874066786,4.39853555416276,133.520964212952));
#228586=CARTESIAN_POINT('Ctrl Pts',(3.14753813267379,7.60142069634967,133.732903367385));
#228587=CARTESIAN_POINT('Ctrl Pts',(-2.24296169861593,8.43405333923822,
133.944842521819));
#228588=CARTESIAN_POINT('Ctrl Pts',(-7.0276043223463,5.11216238889513,134.153065738094));
#228589=CARTESIAN_POINT('Ctrl Pts',(-7.91025855294315,1.22824022493078,
134.308304165763));
#228590=CARTESIAN_POINT('Ctrl Pts',(-7.90831251326434,6.90571829360795E-7,
134.357573016214));
#228591=CARTESIAN_POINT('',(-3.42280818030014,7.13531452195942,137.99828572006));
#228592=CARTESIAN_POINT('Ctrl Pts',(-7.91099999973896,6.42667422549036E-5,
134.359122557131));
#228593=CARTESIAN_POINT('Ctrl Pts',(-7.91100135031142,-0.166186245076805,
134.365941313037));
#228594=CARTESIAN_POINT('Ctrl Pts',(-7.90576200601237,-0.33239889165738,
134.372723415823));
#228595=CARTESIAN_POINT('Ctrl Pts',(-7.88937324703694,-0.592057096643569,
134.383300304956));
#228596=CARTESIAN_POINT('Ctrl Pts',(-7.88178839485409,-0.685677559252165,
134.3871077824));
#228597=CARTESIAN_POINT('Ctrl Pts',(-7.86946744438583,-0.810169954690298,
134.392162194791));
#228598=CARTESIAN_POINT('Ctrl Pts',(-7.86621312090279,-0.841180336018112,
134.393420517128));
#228599=CARTESIAN_POINT('Ctrl Pts',(-7.86014286011769,-0.89590482591113,
134.395639873494));
#228600=CARTESIAN_POINT('Ctrl Pts',(-7.85740272414143,-0.919626920377347,
134.396601518469));
#228601=CARTESIAN_POINT('Ctrl Pts',(-7.85176327288654,-0.966583008271905,
134.398504236969));
#228602=CARTESIAN_POINT('Ctrl Pts',(-7.8488681346898,-0.989817262399845,
134.399445336393));
#228603=CARTESIAN_POINT('Ctrl Pts',(-7.84290721123858,-1.03598395442221,
134.401314580324));
#228604=CARTESIAN_POINT('Ctrl Pts',(-7.83984388676748,-1.05891648034513,
134.402242737066));
#228605=CARTESIAN_POINT('Ctrl Pts',(-7.83134082075238,-1.12051163170326,
134.404734784321));
#228606=CARTESIAN_POINT('Ctrl Pts',(-7.82571538047249,-1.15914803525641,
134.406296981637));
#228607=CARTESIAN_POINT('Ctrl Pts',(-7.8036641938834,-1.30311565030008,
134.41211485197));
#228608=CARTESIAN_POINT('Ctrl Pts',(-7.78539586097027,-1.40815370973349,
134.416352972435));
#228609=CARTESIAN_POINT('Ctrl Pts',(-7.73609108725339,-1.66123031908117,
134.426556913989));
#228610=CARTESIAN_POINT('Ctrl Pts',(-7.70292122824836,-1.80881090519743,
134.432500884393));
#228611=CARTESIAN_POINT('Ctrl Pts',(-7.53848515129802,-2.4534477816681,
134.458509361132));
#228612=CARTESIAN_POINT('Ctrl Pts',(-7.36318540038592,-2.93796781686119,
134.478107978626));
#228613=CARTESIAN_POINT('Ctrl Pts',(-7.07122565761197,-3.5508975194716,
134.504645549634));
#228614=CARTESIAN_POINT('Ctrl Pts',(-6.9956869956998,-3.69749468422313,
134.51114146088));
#228615=CARTESIAN_POINT('Ctrl Pts',(-6.90622925658279,-3.85853505902265,
134.518512217244));
#228616=CARTESIAN_POINT('Ctrl Pts',(-6.89677176691106,-3.87541411167201,
134.519287716281));
#228617=CARTESIAN_POINT('Ctrl Pts',(-6.88109707876542,-3.90315007570101,
134.520567065991));
#228618=CARTESIAN_POINT('Ctrl Pts',(-6.87491586138241,-3.91402726338345,
134.52107006877));
#228619=CARTESIAN_POINT('Ctrl Pts',(-6.86382403384081,-3.93343839076604,
134.521970055588));
#228620=CARTESIAN_POINT('Ctrl Pts',(-6.85892324040459,-3.94197792016819,
134.522366799251));
#228621=CARTESIAN_POINT('Ctrl Pts',(-6.84942366647437,-3.95845937960376,
134.523134120481));
#228622=CARTESIAN_POINT('Ctrl Pts',(-6.84482698210708,-3.96640250193163,
134.523504644923));
#228623=CARTESIAN_POINT('Ctrl Pts',(-6.83531418929179,-3.9827749314889,
134.524269881455));
#228624=CARTESIAN_POINT('Ctrl Pts',(-6.83039628642708,-3.99120317585423,
134.524664639442));
#228625=CARTESIAN_POINT('Ctrl Pts',(-6.81847338446442,-4.01154992815681,
134.525619664446));
#228626=CARTESIAN_POINT('Ctrl Pts',(-6.81145274279046,-4.0234591650426,
134.526180347718));
#228627=CARTESIAN_POINT('Ctrl Pts',(-6.78278890587306,-4.07179208252226,
134.528462856215));
#228628=CARTESIAN_POINT('Ctrl Pts',(-6.7608846584911,-4.10805972308446,
134.530191716958));
#228629=CARTESIAN_POINT('Ctrl Pts',(-6.53522830863079,-4.47499346788989,
134.547839724681));
#228630=CARTESIAN_POINT('Ctrl Pts',(-6.30768135718817,-4.79039886381559,
134.564282588085));
#228631=CARTESIAN_POINT('Ctrl Pts',(-5.87855850299361,-5.3013422968962,
134.592418756284));
#228632=CARTESIAN_POINT('Ctrl Pts',(-5.68805156497539,-5.50524793590822,
134.604130439029));
#228633=CARTESIAN_POINT('Ctrl Pts',(-5.38595783210295,-5.79612992460482,
134.621512368895));
#228634=CARTESIAN_POINT('Ctrl Pts',(-5.28216258152839,-5.89087627759218,
134.627295686004));
#228635=CARTESIAN_POINT('Ctrl Pts',(-5.12911411459645,-6.02328284519411,
134.635561606678));
#228636=CARTESIAN_POINT('Ctrl Pts',(-5.08185713907819,-6.06320673731213,
134.638079570315));
#228637=CARTESIAN_POINT('Ctrl Pts',(-4.99669224683271,-6.13346099381015,
134.642557827776));
#228638=CARTESIAN_POINT('Ctrl Pts',(-4.9589643454751,-6.16400436683672,
134.644521355583));
#228639=CARTESIAN_POINT('Ctrl Pts',(-4.90164342481219,-6.2095427538191,
134.647474763863));
#228640=CARTESIAN_POINT('Ctrl Pts',(-4.88225758519829,-6.2247964105413,
134.648468533251));
#228641=CARTESIAN_POINT('Ctrl Pts',(-4.84740815567947,-6.25195457368229,
134.650246073611));
#228642=CARTESIAN_POINT('Ctrl Pts',(-4.83197127673987,-6.26389299098627,
134.651030341599));
#228643=CARTESIAN_POINT('Ctrl Pts',(-4.79870436322047,-6.28942446540238,
134.652713869104));
#228644=CARTESIAN_POINT('Ctrl Pts',(-4.78086038859333,-6.30299909727791,
134.653612855211));
#228645=CARTESIAN_POINT('Ctrl Pts',(-4.73299708855017,-6.33909044755376,
134.656013610461));
#228646=CARTESIAN_POINT('Ctrl Pts',(-4.70287480087382,-6.36146978044476,
134.657513413464));
#228647=CARTESIAN_POINT('Ctrl Pts',(-4.56562549428634,-6.46193141879186,
134.664298402505));
#228648=CARTESIAN_POINT('Ctrl Pts',(-4.45670463711384,-6.5375284517388,
134.669549160093));
#228649=CARTESIAN_POINT('Ctrl Pts',(-3.73793401218352,-7.01007960313806,
134.703446782646));
#228650=CARTESIAN_POINT('Ctrl Pts',(-3.07765217161356,-7.3240368551536,
134.731236723278));
#228651=CARTESIAN_POINT('Ctrl Pts',(-2.24389990383895,-7.58751308993906,
134.763969942717));
#228652=CARTESIAN_POINT('Ctrl Pts',(-2.10281662481511,-7.62781776620551,
134.769447627685));
#228653=CARTESIAN_POINT('Ctrl Pts',(-1.6643911332303,-7.73997834690071,
134.786388741539));
#228654=CARTESIAN_POINT('Ctrl Pts',(-1.36395009197624,-7.79853131933149,
134.797875582633));
#228655=CARTESIAN_POINT('Ctrl Pts',(-0.953415629191189,-7.85408690543955,
134.813984170946));
#228656=CARTESIAN_POINT('Ctrl Pts',(-0.845659419824983,-7.86641859941681,
134.818251591967));
#228657=CARTESIAN_POINT('Ctrl Pts',(-0.721552434783314,-7.87804199477941,
134.823237870058));
#228658=CARTESIAN_POINT('Ctrl Pts',(-0.705413942137415,-7.87950345857654,
134.823887656261));
#228659=CARTESIAN_POINT('Ctrl Pts',(-0.680958359230041,-7.88164236335777,
134.824874533965));
#228660=CARTESIAN_POINT('Ctrl Pts',(-0.672644452873165,-7.88235625116694,
134.825210420756));
#228661=CARTESIAN_POINT('Ctrl Pts',(-0.657619025430322,-7.88362249013696,
134.825818178533));
#228662=CARTESIAN_POINT('Ctrl Pts',(-0.650907892432978,-7.88417942875896,
134.826089894606));
#228663=CARTESIAN_POINT('Ctrl Pts',(-0.637529901924567,-7.88527243401025,
134.826632063879));
#228664=CARTESIAN_POINT('Ctrl Pts',(-0.630863059777419,-7.88580861636203,
134.826902512852));
#228665=CARTESIAN_POINT('Ctrl Pts',(-0.612202229786365,-7.88728560221123,
134.827660262755));
#228666=CARTESIAN_POINT('Ctrl Pts',(-0.600206791140009,-7.88820749898139,
134.828148221189));
#228667=CARTESIAN_POINT('Ctrl Pts',(-0.551640206178058,-7.89182861055798,
134.830127486014));
#228668=CARTESIAN_POINT('Ctrl Pts',(-0.515052943072718,-7.89430086481496,
134.831626903635));
#228669=CARTESIAN_POINT('Ctrl Pts',(0.0260200785681229,-7.92708448936865,
134.853938646844));
#228670=CARTESIAN_POINT('Ctrl Pts',(0.532149369880393,-7.90923143889126,
134.87696000699));
#228671=CARTESIAN_POINT('Ctrl Pts',(1.38991095178326,-7.79625953824765,
134.916625184714));
#228672=CARTESIAN_POINT('Ctrl Pts',(1.74321151562132,-7.72494337933138,
134.933135060912));
#228673=CARTESIAN_POINT('Ctrl Pts',(2.44472697546279,-7.53274022151604,
134.965431384782));
#228674=CARTESIAN_POINT('Ctrl Pts',(2.79184994556288,-7.4111054916239,134.981153613398));
#228675=CARTESIAN_POINT('Ctrl Pts',(3.15554056877153,-7.2544676878701,134.997237081378));
#228676=CARTESIAN_POINT('Ctrl Pts',(3.18172666356277,-7.24302099789654,
134.998393043265));
#228677=CARTESIAN_POINT('Ctrl Pts',(3.2178601992871,-7.22699222719772,134.999985329666));
#228678=CARTESIAN_POINT('Ctrl Pts',(3.2278608576596,-7.22253107981955,135.000425728474));
#228679=CARTESIAN_POINT('Ctrl Pts',(3.2447306417561,-7.21496367939714,135.001168125615));
#228680=CARTESIAN_POINT('Ctrl Pts',(3.25160463477087,-7.2118683523835,135.001470493216));
#228681=CARTESIAN_POINT('Ctrl Pts',(3.26519969990462,-7.2057231693844,135.002068227434));
#228682=CARTESIAN_POINT('Ctrl Pts',(3.27192094805435,-7.20267372467324,
135.00236360755));
#228683=CARTESIAN_POINT('Ctrl Pts',(3.28672622808175,-7.19593153727496,
135.00301396745));
#228684=CARTESIAN_POINT('Ctrl Pts',(3.29480833022685,-7.19223456620105,
135.003368803039));
#228685=CARTESIAN_POINT('Ctrl Pts',(3.32301348611423,-7.17927524880641,
135.004606456555));
#228686=CARTESIAN_POINT('Ctrl Pts',(3.34310393581234,-7.1699419670949,135.005486854537));
#228687=CARTESIAN_POINT('Ctrl Pts',(3.54418053598472,-7.07550031135375,
135.014286883686));
#228688=CARTESIAN_POINT('Ctrl Pts',(3.7219230775093,-6.9836391533939,135.021969477154));
#228689=CARTESIAN_POINT('Ctrl Pts',(4.23037865769221,-6.6959260598306,135.043788102178));
#228690=CARTESIAN_POINT('Ctrl Pts',(4.55054102467892,-6.48260231058685,
135.057298321681));
#228691=CARTESIAN_POINT('Ctrl Pts',(5.13046800663816,-6.03198547380571,
135.082515338386));
#228692=CARTESIAN_POINT('Ctrl Pts',(5.39241210110661,-5.79900305097784,
135.094256470895));
#228693=CARTESIAN_POINT('Ctrl Pts',(5.85705839497631,-5.32693689978065,
135.117179368428));
#228694=CARTESIAN_POINT('Ctrl Pts',(6.06268411110129,-5.09168185821444,
135.128270681824));
#228695=CARTESIAN_POINT('Ctrl Pts',(6.31233972803033,-4.76942417912666,
135.143879284295));
#228696=CARTESIAN_POINT('Ctrl Pts',(6.36944829871924,-4.69288470917488,
135.147615314876));
#228697=CARTESIAN_POINT('Ctrl Pts',(6.43120643581712,-4.60690919794417,
135.151864360133));
#228698=CARTESIAN_POINT('Ctrl Pts',(6.43724092891516,-4.59847342053661,
135.152281820214));
#228699=CARTESIAN_POINT('Ctrl Pts',(6.4461833313349,-4.5859205036222,135.152903877567));
#228700=CARTESIAN_POINT('Ctrl Pts',(6.44910394347002,-4.58181238515924,
135.153107589957));
#228701=CARTESIAN_POINT('Ctrl Pts',(6.45408247280646,-4.57479541954229,
135.153455781213));
#228702=CARTESIAN_POINT('Ctrl Pts',(6.45614235861604,-4.57188796250278,
135.15360012208));
#228703=CARTESIAN_POINT('Ctrl Pts',(6.46034618754733,-4.56594589788487,
135.153895258978));
#228704=CARTESIAN_POINT('Ctrl Pts',(6.4624899583663,-4.56291116977931,135.154046067096));
#228705=CARTESIAN_POINT('Ctrl Pts',(6.46759000682828,-4.55568072270925,
135.154405561177));
#228706=CARTESIAN_POINT('Ctrl Pts',(6.4705443373088,-4.55148363968955,135.154614384883));
#228707=CARTESIAN_POINT('Ctrl Pts',(6.48109655754965,-4.53646154186808,
135.15536233719));
#228708=CARTESIAN_POINT('Ctrl Pts',(6.48867123166355,-4.52562057065816,
135.155903118517));
#228709=CARTESIAN_POINT('Ctrl Pts',(6.60836805040142,-4.35339068464051,
135.164510149394));
#228710=CARTESIAN_POINT('Ctrl Pts',(6.71445809463561,-4.18790880472618,
135.172994701151));
#228711=CARTESIAN_POINT('Ctrl Pts',(6.97020831420628,-3.75424437952543,
135.195378908409));
#228712=CARTESIAN_POINT('Ctrl Pts',(7.11061834884796,-3.48098363525993,
135.209614305358));
#228713=CARTESIAN_POINT('Ctrl Pts',(7.34807697728012,-2.9441652071837,135.236909989157));
#228714=CARTESIAN_POINT('Ctrl Pts',(7.44768783174739,-2.68221898989426,
135.249945455162));
#228715=CARTESIAN_POINT('Ctrl Pts',(7.62617617529547,-2.12557732816804,
135.276562343962));
#228716=CARTESIAN_POINT('Ctrl Pts',(7.70233927235807,-1.83047479559133,
135.290066990104));
#228717=CARTESIAN_POINT('Ctrl Pts',(7.79133006981822,-1.37954597757157,
135.30960242964));
#228718=CARTESIAN_POINT('Ctrl Pts',(7.81687702637453,-1.2265434328895,135.316047255831));
#228719=CARTESIAN_POINT('Ctrl Pts',(7.84066047342695,-1.05279410472832,
135.323161311835));
#228720=CARTESIAN_POINT('Ctrl Pts',(7.84333296366554,-1.03269555833407,
135.323981172133));
#228721=CARTESIAN_POINT('Ctrl Pts',(7.84799005513257,-0.996610549900073,
135.32544769685));
#228722=CARTESIAN_POINT('Ctrl Pts',(7.85000314512618,-0.980627920997422,
135.326095326149));
#228723=CARTESIAN_POINT('Ctrl Pts',(7.8529721526951,-0.956460801343032,
135.327071717635));
#228724=CARTESIAN_POINT('Ctrl Pts',(7.85396411744352,-0.948280832873142,
135.327401703516));
#228725=CARTESIAN_POINT('Ctrl Pts',(7.85565532261476,-0.934150069707103,
135.327970891243));
#228726=CARTESIAN_POINT('Ctrl Pts',(7.85636058485882,-0.928200011500118,
135.328210297356));
#228727=CARTESIAN_POINT('Ctrl Pts',(7.85780563427802,-0.915888979619091,
135.32870510166));
#228728=CARTESIAN_POINT('Ctrl Pts',(7.8585444591157,-0.909527895918776,
135.328960467034));
#228729=CARTESIAN_POINT('Ctrl Pts',(7.86052777928438,-0.892269206758298,
135.32965250777));
#228730=CARTESIAN_POINT('Ctrl Pts',(7.86175733811396,-0.881369879325183,
135.330088675999));
#228731=CARTESIAN_POINT('Ctrl Pts',(7.86626409963879,-0.840660163769034,
135.331714547681));
#228732=CARTESIAN_POINT('Ctrl Pts',(7.86939446933841,-0.81083358897632,
135.332899268815));
#228733=CARTESIAN_POINT('Ctrl Pts',(7.91639991495052,-0.337019964131563,
135.351617935601));
#228734=CARTESIAN_POINT('Ctrl Pts',(7.9228120426035,0.1099035309372,135.367791207442));
#228735=CARTESIAN_POINT('Ctrl Pts',(7.85818389820049,1.02881400171604,135.399695337205));
#228736=CARTESIAN_POINT('Ctrl Pts',(7.78226300692866,1.49862351932244,135.4152691391));
#228737=CARTESIAN_POINT('Ctrl Pts',(7.61696664535482,2.14542625895294,135.438402298407));
#228738=CARTESIAN_POINT('Ctrl Pts',(7.56246620561757,2.33026464255066,135.445225558587));
#228739=CARTESIAN_POINT('Ctrl Pts',(7.45528153936251,2.65021975220097,135.457699449453));
#228740=CARTESIAN_POINT('Ctrl Pts',(7.40552796349576,2.78622301804474,135.463218513244));
#228741=CARTESIAN_POINT('Ctrl Pts',(7.34365033451669,2.9419791381574,135.469877372092));
#228742=CARTESIAN_POINT('Ctrl Pts',(7.33513566111852,2.96314466343925,135.470789573347));
#228743=CARTESIAN_POINT('Ctrl Pts',(7.32404282390114,2.99037809851655,135.471973138509));
#228744=CARTESIAN_POINT('Ctrl Pts',(7.32154837806681,2.99648023619336,135.472238976491));
#228745=CARTESIAN_POINT('Ctrl Pts',(7.31749875947206,3.00635153137009,135.47267006261));
#228746=CARTESIAN_POINT('Ctrl Pts',(7.31594829686062,3.01012261254933,135.472834995253));
#228747=CARTESIAN_POINT('Ctrl Pts',(7.31296759263189,3.01735646311849,135.473151847765));
#228748=CARTESIAN_POINT('Ctrl Pts',(7.31153780473852,3.02081941965885,135.473303737552));
#228749=CARTESIAN_POINT('Ctrl Pts',(7.30827250898547,3.0287120902976,135.473650391464));
#228750=CARTESIAN_POINT('Ctrl Pts',(7.30643543424889,3.03314115010401,135.473845258723));
#228751=CARTESIAN_POINT('Ctrl Pts',(7.30070459878669,3.04692237936565,135.474452645163));
#228752=CARTESIAN_POINT('Ctrl Pts',(7.29679691425301,3.05626870789418,135.474866073205));
#228753=CARTESIAN_POINT('Ctrl Pts',(7.26685467473443,3.12749925590691,135.478028227449));
#228754=CARTESIAN_POINT('Ctrl Pts',(7.24005197045764,3.18905556512344,135.480826159479));
#228755=CARTESIAN_POINT('Ctrl Pts',(7.05303728994141,3.60404918025981,135.500095106783));
#228756=CARTESIAN_POINT('Ctrl Pts',(6.86780251044484,3.94559768628711,135.517947337373));
#228757=CARTESIAN_POINT('Ctrl Pts',(6.47681462644036,4.55496560805641,135.551815270665));
#228758=CARTESIAN_POINT('Ctrl Pts',(6.27750725066601,4.8259455938197,135.567722543651));
#228759=CARTESIAN_POINT('Ctrl Pts',(5.86965037000293,5.31228119662681,135.597122305045));
#228760=CARTESIAN_POINT('Ctrl Pts',(5.66491302108104,5.53009131863548,135.610665465629));
#228761=CARTESIAN_POINT('Ctrl Pts',(5.31621938830087,5.86130833265701,135.6316712657));
#228762=CARTESIAN_POINT('Ctrl Pts',(5.17980287188342,5.98220463318566,135.63944227536));
#228763=CARTESIAN_POINT('Ctrl Pts',(4.9672225430096,6.1578705913434,135.65089461044));
#228764=CARTESIAN_POINT('Ctrl Pts',(4.89406648975625,6.21617117126574,135.654724984464));
#228765=CARTESIAN_POINT('Ctrl Pts',(4.80723660688551,6.28288563550633,135.659146050707));
#228766=CARTESIAN_POINT('Ctrl Pts',(4.79455186031634,6.29257087097112,135.659788844367));
#228767=CARTESIAN_POINT('Ctrl Pts',(4.77513040741212,6.30730699132631,135.66076836519));
#228768=CARTESIAN_POINT('Ctrl Pts',(4.76841483901869,6.3123855882095,135.661106219152));
#228769=CARTESIAN_POINT('Ctrl Pts',(4.75671558517504,6.32120373525802,135.661693332175));
#228770=CARTESIAN_POINT('Ctrl Pts',(4.75173557236388,6.32494813191816,135.661942787487));
#228771=CARTESIAN_POINT('Ctrl Pts',(4.74133999860546,6.33274520013675,135.662462557511));
#228772=CARTESIAN_POINT('Ctrl Pts',(4.73592365241508,6.33679681787336,135.662732829565));
#228773=CARTESIAN_POINT('Ctrl Pts',(4.72264983563816,6.34669957578501,135.663393864796));
#228774=CARTESIAN_POINT('Ctrl Pts',(4.71478666975881,6.35254308406698,135.663784320629));
#228775=CARTESIAN_POINT('Ctrl Pts',(4.6846008558908,6.37488873944882,135.665278929766));
#228776=CARTESIAN_POINT('Ctrl Pts',(4.66220213360857,6.39128804743691,135.66637896227));
#228777=CARTESIAN_POINT('Ctrl Pts',(4.29282268592522,6.65875550520183,135.684373993808));
#228778=CARTESIAN_POINT('Ctrl Pts',(3.92608512076348,6.88137029383959,135.70008173474));
#228779=CARTESIAN_POINT('Ctrl Pts',(3.05739626052743,7.31651233308555,135.734348940853));
#228780=CARTESIAN_POINT('Ctrl Pts',(2.54795303195255,7.50912174039579,135.75242965059));
#228781=CARTESIAN_POINT('Ctrl Pts',(1.92611649079876,7.67359124157175,135.775607093459));
#228782=CARTESIAN_POINT('Ctrl Pts',(1.82893614968746,7.69733193613248,135.77926324371));
#228783=CARTESIAN_POINT('Ctrl Pts',(1.58470292792323,7.7521106762175,135.788590460571));
#228784=CARTESIAN_POINT('Ctrl Pts',(1.43718633442356,7.78080959042918,135.794358266909));
#228785=CARTESIAN_POINT('Ctrl Pts',(1.26010355083917,7.81005206466047,135.801490118031));
#228786=CARTESIAN_POINT('Ctrl Pts',(1.23125819146574,7.81465146032297,135.802657684146));
#228787=CARTESIAN_POINT('Ctrl Pts',(1.19276967484345,7.82057006926553,135.804222868699));
#228788=CARTESIAN_POINT('Ctrl Pts',(1.18314836728234,7.8220314270274,135.804614738344));
#228789=CARTESIAN_POINT('Ctrl Pts',(1.16729194444085,7.82440989686345,135.805261537706));
#228790=CARTESIAN_POINT('Ctrl Pts',(1.16105836948133,7.82533732052821,135.805516060217));
#228791=CARTESIAN_POINT('Ctrl Pts',(1.1489379974558,7.82712577347588,135.806011422399));
#228792=CARTESIAN_POINT('Ctrl Pts',(1.14305132265721,7.82798761300329,135.806252230412));
#228793=CARTESIAN_POINT('Ctrl Pts',(1.12940061227412,7.82997042101067,135.806811143335));
#228794=CARTESIAN_POINT('Ctrl Pts',(1.12163587761646,7.83108648237224,135.807129435833));
#228795=CARTESIAN_POINT('Ctrl Pts',(1.10067208771137,7.83406788648908,135.807989775922));
#228796=CARTESIAN_POINT('Ctrl Pts',(1.08746998853076,7.83591141579306,135.80853264134));
#228797=CARTESIAN_POINT('Ctrl Pts',(0.99057835584056,7.84919169481745,135.8125243142));
#228798=CARTESIAN_POINT('Ctrl Pts',(0.906716750533531,7.85932057302182,
135.816020312002));
#228799=CARTESIAN_POINT('Ctrl Pts',(0.12530905933518,7.94102673852782,135.848899516));
#228800=CARTESIAN_POINT('Ctrl Pts',(-0.578699863589856,7.92090747917323,
135.880462514738));
#228801=CARTESIAN_POINT('Ctrl Pts',(-1.6190286759695,7.75158783938078,135.925720603467));
#228802=CARTESIAN_POINT('Ctrl Pts',(-1.96305030272363,7.67168982855214,
135.94051103658));
#228803=CARTESIAN_POINT('Ctrl Pts',(-2.364542964997,7.54965715686852,135.957607531542));
#228804=CARTESIAN_POINT('Ctrl Pts',(-2.42823179576967,7.52941412714909,
135.960315343433));
#228805=CARTESIAN_POINT('Ctrl Pts',(-2.51240645063944,7.5014807060306,135.963890150371));
#228806=CARTESIAN_POINT('Ctrl Pts',(-2.53312739965129,7.49450895915408,
135.964769801805));
#228807=CARTESIAN_POINT('Ctrl Pts',(-2.56692476538192,7.48298135670251,
135.966203997449));
#228808=CARTESIAN_POINT('Ctrl Pts',(-2.58001855323884,7.47847691727818,
135.966759491648));
#228809=CARTESIAN_POINT('Ctrl Pts',(-2.6052647283038,7.46971769724389,135.967830264257));
#228810=CARTESIAN_POINT('Ctrl Pts',(-2.61741868436853,7.46546758166851,
135.968345628704));
#228811=CARTESIAN_POINT('Ctrl Pts',(-2.64533082442786,7.45563044698993,
135.969528900518));
#228812=CARTESIAN_POINT('Ctrl Pts',(-2.6610817957033,7.45002310143388,135.970196416241));
#228813=CARTESIAN_POINT('Ctrl Pts',(-2.71109014358489,7.43204130233371,
135.972315067849));
#228814=CARTESIAN_POINT('Ctrl Pts',(-2.74528002055947,7.41948012477288,
135.973762552049));
#228815=CARTESIAN_POINT('Ctrl Pts',(-3.07908234330066,7.29421971115853,
135.987885133593));
#228816=CARTESIAN_POINT('Ctrl Pts',(-3.3716886044844,7.16366679148435,136.000170418465));
#228817=CARTESIAN_POINT('Ctrl Pts',(-4.05049948940648,6.80996819382163,
136.02881242978));
#228818=CARTESIAN_POINT('Ctrl Pts',(-4.42732071333323,6.57122850769228,
136.0448014499));
#228819=CARTESIAN_POINT('Ctrl Pts',(-5.07278384057463,6.08144523990192,
136.074429077218));
#228820=CARTESIAN_POINT('Ctrl Pts',(-5.34787889823811,5.84099854693965,
136.087956554177));
#228821=CARTESIAN_POINT('Ctrl Pts',(-5.61693445560959,5.57083806738167,
136.103193525049));
#228822=CARTESIAN_POINT('Ctrl Pts',(-5.62846012187602,5.55919293624044,
136.103850414269));
#228823=CARTESIAN_POINT('Ctrl Pts',(-5.64495206860732,5.542426186801,136.104796502856));
#228824=CARTESIAN_POINT('Ctrl Pts',(-5.64994777681369,5.5373334748598,136.105083905422));
#228825=CARTESIAN_POINT('Ctrl Pts',(-5.65859556898588,5.5284938784054,136.10558284125));
#228826=CARTESIAN_POINT('Ctrl Pts',(-5.6622508426639,5.52475010941454,136.105794177035));
#228827=CARTESIAN_POINT('Ctrl Pts',(-5.66926371262448,5.51755318547138,
136.106200497935));
#228828=CARTESIAN_POINT('Ctrl Pts',(-5.67262187624312,5.51410058366853,
136.106395447493));
#228829=CARTESIAN_POINT('Ctrl Pts',(-5.68051234425018,5.50597338356774,
136.106854408435));
#228830=CARTESIAN_POINT('Ctrl Pts',(-5.68504202946672,5.50129625783993,
136.107118584469));
#228831=CARTESIAN_POINT('Ctrl Pts',(-5.70061727081034,5.48517426535884,
136.10802938381));
#228832=CARTESIAN_POINT('Ctrl Pts',(-5.71163402892843,5.47370173679395,
136.108677840654));
#228833=CARTESIAN_POINT('Ctrl Pts',(-5.87354533996715,5.30407101586759,
136.118271932449));
#228834=CARTESIAN_POINT('Ctrl Pts',(-6.01783649188541,5.13977862894329,
136.127670612993));
#228835=CARTESIAN_POINT('Ctrl Pts',(-6.3498201743387,4.72861047932357,136.151061288945));
#228836=CARTESIAN_POINT('Ctrl Pts',(-6.5301708020188,4.47625162722608,136.16530028286));
#228837=CARTESIAN_POINT('Ctrl Pts',(-6.83991037814008,3.98413143818814,
136.192105527461));
#228838=CARTESIAN_POINT('Ctrl Pts',(-6.97264574394831,3.74698473587029,
136.204643819333));
#228839=CARTESIAN_POINT('Ctrl Pts',(-7.31175402719853,3.0604472068842,136.239381899073));
#228840=CARTESIAN_POINT('Ctrl Pts',(-7.48861622076895,2.59784885706755,
136.260936847229));
#228841=CARTESIAN_POINT('Ctrl Pts',(-7.62973372409618,2.0909576440689,136.282357759272));
#228842=CARTESIAN_POINT('Ctrl Pts',(-7.6381112372613,2.06014497719628,136.283651903632));
#228843=CARTESIAN_POINT('Ctrl Pts',(-7.64940708068612,2.01758242461873,
136.285428677968));
#228844=CARTESIAN_POINT('Ctrl Pts',(-7.65248528253231,2.00587550172729,
136.285916252954));
#228845=CARTESIAN_POINT('Ctrl Pts',(-7.65734903800562,1.98720366517646,
136.286692113057));
#228846=CARTESIAN_POINT('Ctrl Pts',(-7.65915198134217,1.98024332438444,
136.28698093557));
#228847=CARTESIAN_POINT('Ctrl Pts',(-7.66264362922107,1.96668756099512,
136.287542668744));
#228848=CARTESIAN_POINT('Ctrl Pts',(-7.66433331369956,1.96009239778099,
136.28781560951));
#228849=CARTESIAN_POINT('Ctrl Pts',(-7.66835822379588,1.94429762057987,
136.288468431015));
#228850=CARTESIAN_POINT('Ctrl Pts',(-7.6706854134382,1.93509596006992,136.288848063341));
#228851=CARTESIAN_POINT('Ctrl Pts',(-7.67762677053578,1.90744069295049,
136.289986984329));
#228852=CARTESIAN_POINT('Ctrl Pts',(-7.6821909615888,1.88897455267583,136.290744730917));
#228853=CARTESIAN_POINT('Ctrl Pts',(-7.72203369099223,1.72524295548827,
136.29743932926));
#228854=CARTESIAN_POINT('Ctrl Pts',(-7.75325577563833,1.5790171933201,136.303250033498));
#228855=CARTESIAN_POINT('Ctrl Pts',(-7.82274384609175,1.20147310293162,
136.317869998403));
#228856=CARTESIAN_POINT('Ctrl Pts',(-7.85490690069484,0.969177476494734,
136.326498305678));
#228857=CARTESIAN_POINT('Ctrl Pts',(-7.91489028185631,0.327046568713605,
136.34966155197));
#228858=CARTESIAN_POINT('Ctrl Pts',(-7.92119887124829,-0.0840536765173626,
136.363705962504));
#228859=CARTESIAN_POINT('Ctrl Pts',(-7.86376164364314,-1.00247119054195,
136.395516433555));
#228860=CARTESIAN_POINT('Ctrl Pts',(-7.78286352958253,-1.50689096754052,
136.413322594698));
#228861=CARTESIAN_POINT('Ctrl Pts',(-7.64576571696238,-2.03156382264371,
136.434783901456));
#228862=CARTESIAN_POINT('Ctrl Pts',(-7.63732431421645,-2.06307107042614,
136.436083210584));
#228863=CARTESIAN_POINT('Ctrl Pts',(-7.62584104193559,-2.10489549858869,
136.437821233071));
#228864=CARTESIAN_POINT('Ctrl Pts',(-7.62297256340687,-2.11526025655475,
136.438253027805));
#228865=CARTESIAN_POINT('Ctrl Pts',(-7.61847339832232,-2.13138920986506,
136.438926616887));
#228866=CARTESIAN_POINT('Ctrl Pts',(-7.61685727801344,-2.13715747922644,
136.439167846251));
#228867=CARTESIAN_POINT('Ctrl Pts',(-7.61359892450181,-2.1487365775127,
136.439652742026));
#228868=CARTESIAN_POINT('Ctrl Pts',(-7.61195658692626,-2.15454737270082,
136.439896412298));
#228869=CARTESIAN_POINT('Ctrl Pts',(-7.60826150100246,-2.16756408705518,
136.440442993725));
#228870=CARTESIAN_POINT('Ctrl Pts',(-7.60620516644946,-2.17476897728105,
136.440746039376));
#228871=CARTESIAN_POINT('Ctrl Pts',(-7.60011720058397,-2.19598545446804,
136.441639902043));
#228872=CARTESIAN_POINT('Ctrl Pts',(-7.59605707725077,-2.20998879062601,
136.442231766446));
#228873=CARTESIAN_POINT('Ctrl Pts',(-7.5643613783558,-2.31818775854298,
136.44681918667));
#228874=CARTESIAN_POINT('Ctrl Pts',(-7.53501394362846,-2.41187096711469,
136.45087485795));
#228875=CARTESIAN_POINT('Ctrl Pts',(-7.42301395737386,-2.74737852250292,
136.465651543895));
#228876=CARTESIAN_POINT('Ctrl Pts',(-7.33040058904106,-2.98570689433657,
136.476619057148));
#228877=CARTESIAN_POINT('Ctrl Pts',(-6.99494608645096,-3.73874777956843,
136.512195213584));
#228878=CARTESIAN_POINT('Ctrl Pts',(-6.7080859060453,-4.2319208089412,136.536776651183));
#228879=CARTESIAN_POINT('Ctrl Pts',(-6.14303244215255,-4.99946877119786,
136.576556068512));
#228880=CARTESIAN_POINT('Ctrl Pts',(-5.89301322822294,-5.29187498704281,
136.592243489285));
#228881=CARTESIAN_POINT('Ctrl Pts',(-5.57018057078227,-5.61805937193414,
136.610856059387));
#228882=CARTESIAN_POINT('Ctrl Pts',(-5.51687581407221,-5.67041304011356,
136.6138786558));
#228883=CARTESIAN_POINT('Ctrl Pts',(-5.44086927406208,-5.74297701562394,
136.618118235123));
#228884=CARTESIAN_POINT('Ctrl Pts',(-5.41878064099899,-5.76382336918695,
136.619342177075));
#228885=CARTESIAN_POINT('Ctrl Pts',(-5.37838622168782,-5.80150853241021,
136.621565751023));
#228886=CARTESIAN_POINT('Ctrl Pts',(-5.3601200379922,-5.81838919148437,
136.622565851215));
#228887=CARTESIAN_POINT('Ctrl Pts',(-5.32315907846042,-5.8522248220921,
136.624578735194));
#228888=CARTESIAN_POINT('Ctrl Pts',(-5.30446216271045,-5.86917703869629,
136.625591477542));
#228889=CARTESIAN_POINT('Ctrl Pts',(-5.25841682209093,-5.91052591825176,
136.62807223936));
#228890=CARTESIAN_POINT('Ctrl Pts',(-5.23097933893577,-5.93482259837594,
136.629539049168));
#228891=CARTESIAN_POINT('Ctrl Pts',(-5.12931303552639,-6.02359826606543,
136.634932639878));
#228892=CARTESIAN_POINT('Ctrl Pts',(-5.05405244671255,-6.08688281599496,
136.638844652628));
#228893=CARTESIAN_POINT('Ctrl Pts',(-4.91460939214823,-6.19976694474039,
136.645952696338));
#228894=CARTESIAN_POINT('Ctrl Pts',(-4.85080651237334,-6.2498137546493,
136.649153601768));
#228895=CARTESIAN_POINT('Ctrl Pts',(-4.54906517694144,-6.47909420673662,
136.664064289952));
#228896=CARTESIAN_POINT('Ctrl Pts',(-4.30189310048057,-6.6457787902255,
136.675621276554));
#228897=CARTESIAN_POINT('Ctrl Pts',(-3.65918256189946,-7.02828810808652,
136.704537217785));
#228898=CARTESIAN_POINT('Ctrl Pts',(-3.25353448819647,-7.22502177655864,
136.721773360009));
#228899=CARTESIAN_POINT('Ctrl Pts',(-2.79295025801972,-7.4017042008739,
136.741427820764));
#228900=CARTESIAN_POINT('Ctrl Pts',(-2.75239274391208,-7.41688144414838,
136.743159540706));
#228901=CARTESIAN_POINT('Ctrl Pts',(-2.69674102015199,-7.43718783363369,
136.745538670695));
#228902=CARTESIAN_POINT('Ctrl Pts',(-2.68175267251557,-7.44260556548389,
136.746179716044));
#228903=CARTESIAN_POINT('Ctrl Pts',(-2.65679301006792,-7.45154237124322,
136.747247804158));
#228904=CARTESIAN_POINT('Ctrl Pts',(-2.64683080675357,-7.45508681964258,
136.747674264132));
#228905=CARTESIAN_POINT('Ctrl Pts',(-2.62742337876813,-7.46194797631548,
136.748505380958));
#228906=CARTESIAN_POINT('Ctrl Pts',(-2.61797890400205,-7.46526675143261,
136.748909988256));
#228907=CARTESIAN_POINT('Ctrl Pts',(-2.59570038724173,-7.47304791400891,
136.749864802684));
#228908=CARTESIAN_POINT('Ctrl Pts',(-2.58286111204484,-7.47749517549158,
136.750415372867));
#228909=CARTESIAN_POINT('Ctrl Pts',(-2.53997095268429,-7.49222779974579,
136.752255708096));
#228910=CARTESIAN_POINT('Ctrl Pts',(-2.50986988989184,-7.50236515654474,
136.753549234786));
#228911=CARTESIAN_POINT('Ctrl Pts',(-2.43660169230001,-7.52654993232625,
136.756701780051));
#228912=CARTESIAN_POINT('Ctrl Pts',(-2.39337318469666,-7.54040757721394,
136.758565111757));
#228913=CARTESIAN_POINT('Ctrl Pts',(-1.7182118370628,-7.75045136583826,
136.787703291497));
#228914=CARTESIAN_POINT('Ctrl Pts',(-1.06422114946391,-7.86697108315226,
136.816167969104));
#228915=CARTESIAN_POINT('Ctrl Pts',(-0.208718193763188,-7.91064730273531,
136.85163425675));
#228916=CARTESIAN_POINT('Ctrl Pts',(-0.0137754869546448,-7.91338846755851,
136.859619190027));
#228917=CARTESIAN_POINT('Ctrl Pts',(0.21895698198812,-7.90806011575726,
136.869051175369));
#228918=CARTESIAN_POINT('Ctrl Pts',(0.256834453835736,-7.90692057872124,
136.870583124002));
#228919=CARTESIAN_POINT('Ctrl Pts',(0.318967926994052,-7.90460436044039,
136.873091311122));
#228920=CARTESIAN_POINT('Ctrl Pts',(0.343229203732085,-7.90358806824807,
136.874069484961));
#228921=CARTESIAN_POINT('Ctrl Pts',(0.386817111690746,-7.90156111427252,
136.875824828444));
#228922=CARTESIAN_POINT('Ctrl Pts',(0.406145422111844,-7.90059120694265,
136.876602481624));
#228923=CARTESIAN_POINT('Ctrl Pts',(0.447305124695851,-7.89837434416711,
136.878257024626));
#228924=CARTESIAN_POINT('Ctrl Pts',(0.469135308630685,-7.89710777570572,
136.879133674533));
#228925=CARTESIAN_POINT('Ctrl Pts',(0.528008561126827,-7.89344702028305,
136.881495644447));
#228926=CARTESIAN_POINT('Ctrl Pts',(0.565040561878516,-7.89088259219176,
136.882978952819));
#228927=CARTESIAN_POINT('Ctrl Pts',(0.75705964232581,-7.8762268025133,136.890659197131));
#228928=CARTESIAN_POINT('Ctrl Pts',(0.911685126250312,-7.85982946680961,
136.896805744961));
#228929=CARTESIAN_POINT('Ctrl Pts',(1.38630023125547,-7.79530360363674,
136.915634452173));
#228930=CARTESIAN_POINT('Ctrl Pts',(1.70390788228406,-7.73209504900646,
136.92822794354));
#228931=CARTESIAN_POINT('Ctrl Pts',(2.69532085798193,-7.47071785265343,
136.967639385243));
#228932=CARTESIAN_POINT('Ctrl Pts',(3.34704192321646,-7.20233557902392,
136.993278448167));
#228933=CARTESIAN_POINT('Ctrl Pts',(3.99569409638519,-6.82792655369442,
137.021745442572));
#228934=CARTESIAN_POINT('Ctrl Pts',(4.0363924810619,-6.80394650378785,137.023546675736));
#228935=CARTESIAN_POINT('Ctrl Pts',(4.16755765722972,-6.72507112128776,
137.029406375802));
#228936=CARTESIAN_POINT('Ctrl Pts',(4.25713721417319,-6.66872554701499,
137.033493142118));
#228937=CARTESIAN_POINT('Ctrl Pts',(4.41535617473172,-6.56471841439059,
137.040900350845));
#228938=CARTESIAN_POINT('Ctrl Pts',(4.48442213792002,-6.51773393193075,
137.044200475582));
#228939=CARTESIAN_POINT('Ctrl Pts',(4.56469019830904,-6.46124897223342,
137.048127319956));
#228940=CARTESIAN_POINT('Ctrl Pts',(4.57662712976933,-6.4527993150065,137.048713708165));
#228941=CARTESIAN_POINT('Ctrl Pts',(4.59573949504721,-6.43919075610921,
137.049656554245));
#228942=CARTESIAN_POINT('Ctrl Pts',(4.60292986082819,-6.43405282815602,
137.050012173495));
#228943=CARTESIAN_POINT('Ctrl Pts',(4.61567243837084,-6.42491523415001,
137.050644024843));
#228944=CARTESIAN_POINT('Ctrl Pts',(4.62122810470296,-6.42092038794469,
137.050920059408));
#228945=CARTESIAN_POINT('Ctrl Pts',(4.63229182212711,-6.41294313656981,
137.051470876406));
#228946=CARTESIAN_POINT('Ctrl Pts',(4.63779993799344,-6.40896083098058,
137.051745654589));
#228947=CARTESIAN_POINT('Ctrl Pts',(4.65224295404536,-6.39849032396414,
137.052467624567));
#228948=CARTESIAN_POINT('Ctrl Pts',(4.66116939749716,-6.39199051749304,
137.052915309406));
#228949=CARTESIAN_POINT('Ctrl Pts',(4.68029442962054,-6.37800322402905,
137.053877703446));
#228950=CARTESIAN_POINT('Ctrl Pts',(4.6904887150439,-6.37050992350434,137.054392666714));
#228951=CARTESIAN_POINT('Ctrl Pts',(4.71932449286379,-6.34920747252993,
137.055855017416));
#228952=CARTESIAN_POINT('Ctrl Pts',(4.73792319015151,-6.33534079808741,
137.056805006622));
#228953=CARTESIAN_POINT('Ctrl Pts',(4.90231168372407,-6.21164853215248,
137.06526422718));
#228954=CARTESIAN_POINT('Ctrl Pts',(5.04429738329768,-6.09690809464115,
137.073040935022));
#228955=CARTESIAN_POINT('Ctrl Pts',(5.43300599863429,-5.75991014362268,
137.095588621291));
#228956=CARTESIAN_POINT('Ctrl Pts',(5.66988261999473,-5.52689183402546,
137.110777865977));
#228957=CARTESIAN_POINT('Ctrl Pts',(6.05955294442313,-5.09207349950693,
137.137543211365));
#228958=CARTESIAN_POINT('Ctrl Pts',(6.21863871113789,-4.89652245716874,
137.149095208133));
#228959=CARTESIAN_POINT('Ctrl Pts',(6.64018019627438,-4.32460211367056,
137.181124636086));
#228960=CARTESIAN_POINT('Ctrl Pts',(6.87965411248884,-3.93250857936813,
137.201040943593));
#228961=CARTESIAN_POINT('Ctrl Pts',(7.09732896970311,-3.49467625493419,
137.220914748124));
#228962=CARTESIAN_POINT('Ctrl Pts',(7.11067312990908,-3.46744405826491,
137.222141913801));
#228963=CARTESIAN_POINT('Ctrl Pts',(7.12887059784851,-3.42976059533592,
137.223827814578));
#228964=CARTESIAN_POINT('Ctrl Pts',(7.13385806678806,-3.41937462506903,
137.224291191499));
#228965=CARTESIAN_POINT('Ctrl Pts',(7.14177492682433,-3.40279573687417,
137.225028843222));
#228966=CARTESIAN_POINT('Ctrl Pts',(7.14471898415316,-3.39660986427426,
137.225303625158));
#228967=CARTESIAN_POINT('Ctrl Pts',(7.15043705443133,-3.38455507706051,
137.22583823751));
#228968=CARTESIAN_POINT('Ctrl Pts',(7.15321188610707,-3.37868655719622,
137.22609809612));
#228969=CARTESIAN_POINT('Ctrl Pts',(7.15984091569622,-3.36462198348927,
137.226719916768));
#228970=CARTESIAN_POINT('Ctrl Pts',(7.16368827171385,-3.35642270524064,
137.227081642171));
#228971=CARTESIAN_POINT('Ctrl Pts',(7.17521486090875,-3.33174775709674,
137.228167883753));
#228972=CARTESIAN_POINT('Ctrl Pts',(7.18285142225183,-3.31525215762523,
137.228890926097));
#228973=CARTESIAN_POINT('Ctrl Pts',(7.25041497574915,-3.16798001657772,
137.235318552345));
#228974=CARTESIAN_POINT('Ctrl Pts',(7.30682307210091,-3.03561426708979,
137.240900778931));
#228975=CARTESIAN_POINT('Ctrl Pts',(7.44197216408833,-2.69284450122335,
137.254899267162));
#228976=CARTESIAN_POINT('Ctrl Pts',(7.51542027370736,-2.48048937822177,
137.263139143102));
#228977=CARTESIAN_POINT('Ctrl Pts',(7.66831896238124,-1.96888464999519,
137.282204346993));
#228978=CARTESIAN_POINT('Ctrl Pts',(7.73944191938007,-1.66753438224366,
137.292809423382));
#228979=CARTESIAN_POINT('Ctrl Pts',(7.84521605560998,-1.06269310231812,
137.313660076921));
#228980=CARTESIAN_POINT('Ctrl Pts',(7.88031673336665,-0.759824242257206,
137.32389377151));
#228981=CARTESIAN_POINT('Ctrl Pts',(7.91830544702248,-0.101421171746311,
137.346809635786));
#228982=CARTESIAN_POINT('Ctrl Pts',(7.91488398956741,0.253793123182802,
137.359594946649));
#228983=CARTESIAN_POINT('Ctrl Pts',(7.88583301257502,0.630959979855571,
137.37463518708));
#228984=CARTESIAN_POINT('Ctrl Pts',(7.88392473719205,0.654372611468432,
137.37557488224));
#228985=CARTESIAN_POINT('Ctrl Pts',(7.88129577818577,0.6849449822814,137.376810248428));
#228986=CARTESIAN_POINT('Ctrl Pts',(7.88066954363933,0.692112935365577,
137.377100487385));
#228987=CARTESIAN_POINT('Ctrl Pts',(7.87968992919449,0.703151996484756,
137.377548404027));
#228988=CARTESIAN_POINT('Ctrl Pts',(7.8793434722941,0.707023730801474,137.377705678623));
#228989=CARTESIAN_POINT('Ctrl Pts',(7.87864924257936,0.714718018030574,
137.378018583591));
#228990=CARTESIAN_POINT('Ctrl Pts',(7.87830154109193,0.718540576742255,
137.378174209754));
#228991=CARTESIAN_POINT('Ctrl Pts',(7.87752662362451,0.72699167812077,137.378518662073));
#228992=CARTESIAN_POINT('Ctrl Pts',(7.87709811029137,0.731620097203008,
137.378707564711));
#228993=CARTESIAN_POINT('Ctrl Pts',(7.87587255549259,0.744731553629492,
137.379243423262));
#228994=CARTESIAN_POINT('Ctrl Pts',(7.87506589031872,0.753213661141762,
137.379590951245));
#228995=CARTESIAN_POINT('Ctrl Pts',(7.8695838669992,0.809885728993842,137.381918808303));
#228996=CARTESIAN_POINT('Ctrl Pts',(7.86448006579414,0.858031531406276,
137.383925185326));
#228997=CARTESIAN_POINT('Ctrl Pts',(7.84787564778091,1.0020435773276,137.390005790461));
#228998=CARTESIAN_POINT('Ctrl Pts',(7.83506177681284,1.09774726148733,137.394151876249));
#228999=CARTESIAN_POINT('Ctrl Pts',(7.79131402430223,1.38448256494346,137.406835761854));
#229000=CARTESIAN_POINT('Ctrl Pts',(7.75512035563487,1.57463233182598,137.415597058033));
#229001=CARTESIAN_POINT('Ctrl Pts',(7.67063808499086,1.94413500329999,137.43304803864));
#229002=CARTESIAN_POINT('Ctrl Pts',(7.62293138154975,2.12350287717563,137.441720603128));
#229003=CARTESIAN_POINT('Ctrl Pts',(7.45696342516364,2.66943605686101,137.468434527694));
#229004=CARTESIAN_POINT('Ctrl Pts',(7.3182078153177,3.02920128498578,137.486457865711));
#229005=CARTESIAN_POINT('Ctrl Pts',(6.99222649849499,3.71966514697358,137.520767924053));
#229006=CARTESIAN_POINT('Ctrl Pts',(6.80629825478973,4.04987672366209,137.537034440507));
#229007=CARTESIAN_POINT('Ctrl Pts',(6.58441351938915,4.38519954921796,137.553302836553));
#229008=CARTESIAN_POINT('Ctrl Pts',(6.57131973557064,4.40479663860583,137.554252796586));
#229009=CARTESIAN_POINT('Ctrl Pts',(6.55320411359318,4.43164920662849,137.55555340553));
#229010=CARTESIAN_POINT('Ctrl Pts',(6.54825749620984,4.43895512582095,137.55590716099));
#229011=CARTESIAN_POINT('Ctrl Pts',(6.5397838802022,4.45142526710199,137.556510789117));
#229012=CARTESIAN_POINT('Ctrl Pts',(6.53626296687371,4.45659360234842,137.556760913652));
#229013=CARTESIAN_POINT('Ctrl Pts',(6.52941406527846,4.46662150342126,137.557246117771));
#229014=CARTESIAN_POINT('Ctrl Pts',(6.52608677144406,4.47148153775562,137.557481225956));
#229015=CARTESIAN_POINT('Ctrl Pts',(6.51813646202759,4.48306643473186,137.558041545496));
#229016=CARTESIAN_POINT('Ctrl Pts',(6.51350845792592,4.48978787526941,137.558366549107));
#229017=CARTESIAN_POINT('Ctrl Pts',(6.49967936195226,4.5098060550648,137.559334236502));
#229018=CARTESIAN_POINT('Ctrl Pts',(6.49044786692956,4.52308179823314,137.559975652733));
#229019=CARTESIAN_POINT('Ctrl Pts',(6.41326131149601,4.63336030866507,137.565301062576));
#229020=CARTESIAN_POINT('Ctrl Pts',(6.34317475645783,4.72885652544241,137.569894923436));
#229021=CARTESIAN_POINT('Ctrl Pts',(6.09084953000408,5.05695248063119,137.585647244255));
#229022=CARTESIAN_POINT('Ctrl Pts',(5.89774461613417,5.28089416286222,137.596331835361));
#229023=CARTESIAN_POINT('Ctrl Pts',(5.5234011833854,5.66880018543502,137.615183317774));
#229024=CARTESIAN_POINT('Ctrl Pts',(5.34624178723412,5.83617675071304,137.623455919542));
#229025=CARTESIAN_POINT('Ctrl Pts',(4.98453158520127,6.14759992167587,137.639572086774));
#229026=CARTESIAN_POINT('Ctrl Pts',(4.80075605714054,6.29216008422309,137.647412408225));
#229027=CARTESIAN_POINT('Ctrl Pts',(4.30277394768891,6.64934587014393,137.66843927089));
#229028=CARTESIAN_POINT('Ctrl Pts',(3.97923706212365,6.84786652533176,137.681882561439));
#229029=CARTESIAN_POINT('Ctrl Pts',(3.62159537579133,7.03338726050776,137.697879336629));
#229030=CARTESIAN_POINT('Ctrl Pts',(3.60038307126351,7.04426938324619,137.698832313249));
#229031=CARTESIAN_POINT('Ctrl Pts',(3.57260357140288,7.05836228434764,137.700085882373));
#229032=CARTESIAN_POINT('Ctrl Pts',(3.56608118831309,7.06165981715079,137.700380600865));
#229033=CARTESIAN_POINT('Ctrl Pts',(3.55600394518907,7.06673706503045,137.700836541252));
#229034=CARTESIAN_POINT('Ctrl Pts',(3.55245228240092,7.06852315449443,137.700997348227));
#229035=CARTESIAN_POINT('Ctrl Pts',(3.54537413565968,7.07207598910778,137.701318046062));
#229036=CARTESIAN_POINT('Ctrl Pts',(3.54184767332189,7.07384277577609,137.701477934189));
#229037=CARTESIAN_POINT('Ctrl Pts',(3.53402518050049,7.07775459313704,137.70183284497));
#229038=CARTESIAN_POINT('Ctrl Pts',(3.52972851852906,7.07989834972029,137.702027949012));
#229039=CARTESIAN_POINT('Ctrl Pts',(3.52085560428013,7.08431527554123,137.702431183201));
#229040=CARTESIAN_POINT('Ctrl Pts',(3.51627909715017,7.08658792509975,137.702639346111));
#229041=CARTESIAN_POINT('Ctrl Pts',(3.4920512833741,7.09858997758302,137.703742296214));
#229042=CARTESIAN_POINT('Ctrl Pts',(3.47236196283464,7.1082419919824,137.704641924229));
#229043=CARTESIAN_POINT('Ctrl Pts',(3.27506504298794,7.20394469581716,137.713687572718));
#229044=CARTESIAN_POINT('Ctrl Pts',(3.09434773587105,7.28339698755708,137.722222219025));
#229045=CARTESIAN_POINT('Ctrl Pts',(2.78805009204316,7.40460278664932,137.736873241804));
#229046=CARTESIAN_POINT('Ctrl Pts',(2.66404305751848,7.4501166653912,137.742854046942));
#229047=CARTESIAN_POINT('Ctrl Pts',(2.42521066295268,7.53104897139772,137.754396289446));
#229048=CARTESIAN_POINT('Ctrl Pts',(2.31060110278897,7.56699855355914,137.75994519524));
#229049=CARTESIAN_POINT('Ctrl Pts',(1.68119686727785,7.74879083909839,137.790338903395));
#229050=CARTESIAN_POINT('Ctrl Pts',(1.15338828676953,7.84474141608955,137.815420862829));
#229051=CARTESIAN_POINT('Ctrl Pts',(0.587116279381268,7.8892520506006,137.84051973687));
#229052=CARTESIAN_POINT('Ctrl Pts',(0.554300954743872,7.89162555658072,
137.841968314981));
#229053=CARTESIAN_POINT('Ctrl Pts',(0.224501951515393,7.913412391737,137.856466433581));
#229054=CARTESIAN_POINT('Ctrl Pts',(-0.0733546393494361,7.91625801729728,
137.869056190157));
#229055=CARTESIAN_POINT('Ctrl Pts',(-0.39500889416899,7.90116965032467,
137.882114690229));
#229056=CARTESIAN_POINT('Ctrl Pts',(-0.41932580395055,7.89991643964552,
137.883098666567));
#229057=CARTESIAN_POINT('Ctrl Pts',(-0.453222669692455,7.89801255967257,
137.884465844585));
#229058=CARTESIAN_POINT('Ctrl Pts',(-0.462807690714998,7.8974566933462,
137.884851945608));
#229059=CARTESIAN_POINT('Ctrl Pts',(-0.479352537662126,7.8964669803212,
137.885517549711));
#229060=CARTESIAN_POINT('Ctrl Pts',(-0.486312836084989,7.89604137859354,
137.88579730464));
#229061=CARTESIAN_POINT('Ctrl Pts',(-0.500711914334743,7.89514180611295,
137.886375511041));
#229062=CARTESIAN_POINT('Ctrl Pts',(-0.50815060715982,7.89466652371237,
137.886673922148));
#229063=CARTESIAN_POINT('Ctrl Pts',(-0.525521806858425,7.89353196733937,
137.887370100198));
#229064=CARTESIAN_POINT('Ctrl Pts',(-0.535453772929936,7.89286445765136,
137.887767615255));
#229065=CARTESIAN_POINT('Ctrl Pts',(-0.56732404589184,7.89066208060671,
137.889041516466));
#229066=CARTESIAN_POINT('Ctrl Pts',(-0.58925730682568,7.88905447309326,
137.889915682906));
#229067=CARTESIAN_POINT('Ctrl Pts',(-1.06335697122926,7.85231693977553,
137.908757453707));
#229068=CARTESIAN_POINT('Ctrl Pts',(-1.51170353755009,7.77845852054929,
137.925450237707));
#229069=CARTESIAN_POINT('Ctrl Pts',(-2.4575557918196,7.53772252052056,137.960068866455));
#229070=CARTESIAN_POINT('Ctrl Pts',(-2.94978943986607,7.3590436259296,137.977712341762));
#229071=CARTESIAN_POINT('Ctrl Pts',(-3.42078955582569,7.13317039013887,
137.996634350838));
#229072=CARTESIAN_POINT('',(3.42067962509738,7.13322310757512,138.));
#229073=CARTESIAN_POINT('Origin',(0.,0.,138.));
#229074=CARTESIAN_POINT('',(-7.91099871838666,-0.0025630630418797,136.642331508237));
#229075=CARTESIAN_POINT('Ctrl Pts',(3.42067962509738,7.13322310757512,138.));
#229076=CARTESIAN_POINT('Ctrl Pts',(3.61450323792865,7.04027655686782,137.991350898295));
#229077=CARTESIAN_POINT('Ctrl Pts',(3.80449053363425,6.9394483670193,137.982701796591));
#229078=CARTESIAN_POINT('Ctrl Pts',(3.99003223922227,6.83107339515299,137.974052694886));
#229079=CARTESIAN_POINT('Ctrl Pts',(4.17562869260824,6.72266644507969,137.96540104109));
#229080=CARTESIAN_POINT('Ctrl Pts',(4.35677673418512,6.60670838442162,137.956749387295));
#229081=CARTESIAN_POINT('Ctrl Pts',(4.53289396587659,6.48357874126008,137.948097733499));
#229082=CARTESIAN_POINT('Ctrl Pts',(4.71449430712678,6.35661566671367,137.939176725222));
#229083=CARTESIAN_POINT('Ctrl Pts',(4.89074533052145,6.22202742493026,137.930255716945));
#229084=CARTESIAN_POINT('Ctrl Pts',(5.06104230700313,6.08027727712515,137.921334708668));
#229085=CARTESIAN_POINT('Ctrl Pts',(5.22620278543872,5.94280259781207,137.912682775876));
#229086=CARTESIAN_POINT('Ctrl Pts',(5.38576295710407,5.79859189864489,137.904030843084));
#229087=CARTESIAN_POINT('Ctrl Pts',(5.53920484348363,5.64810859508982,137.895378910293));
#229088=CARTESIAN_POINT('Ctrl Pts',(5.69980480385011,5.49060523562916,137.886323364273));
#229089=CARTESIAN_POINT('Ctrl Pts',(5.85370181180418,5.32623024217355,137.877267818253));
#229090=CARTESIAN_POINT('Ctrl Pts',(6.00034404570054,5.1555593618177,137.868212272234));
#229091=CARTESIAN_POINT('Ctrl Pts',(6.1469862795968,4.98488848146197,137.859156726214));
#229092=CARTESIAN_POINT('Ctrl Pts',(6.28637353306249,4.80792192525416,137.850101180194));
#229093=CARTESIAN_POINT('Ctrl Pts',(6.41800015970126,4.62527782409605,137.841045634175));
#229094=CARTESIAN_POINT('Ctrl Pts',(6.53225023542455,4.46674529218672,137.833185546555));
#229095=CARTESIAN_POINT('Ctrl Pts',(6.64068733369427,4.30388758917187,137.825325458936));
#229096=CARTESIAN_POINT('Ctrl Pts',(6.74297429743848,4.13717519862092,137.817465371316));
#229097=CARTESIAN_POINT('Ctrl Pts',(6.84522917872496,3.97051509765826,137.809607749024));
#229098=CARTESIAN_POINT('Ctrl Pts',(6.94133758611483,3.80000301422222,137.801750126733));
#229099=CARTESIAN_POINT('Ctrl Pts',(7.03100584644683,3.62613813681035,137.793892504441));
#229100=CARTESIAN_POINT('Ctrl Pts',(7.12066144242633,3.45229781531256,137.786035991926));
#229101=CARTESIAN_POINT('Ctrl Pts',(7.203878544636,3.27510595323246,137.778179479411));
#229102=CARTESIAN_POINT('Ctrl Pts',(7.28040948782943,3.09508621681581,137.770322966896));
#229103=CARTESIAN_POINT('Ctrl Pts',(7.35696442839242,2.9150100326414,137.762463990859));
#229104=CARTESIAN_POINT('Ctrl Pts',(7.42682888092052,2.73210452182045,137.754605014822));
#229105=CARTESIAN_POINT('Ctrl Pts',(7.48980312788921,2.54691383942628,137.746746038785));
#229106=CARTESIAN_POINT('Ctrl Pts',(7.55278699150612,2.36169487700123,137.738885862622));
#229107=CARTESIAN_POINT('Ctrl Pts',(7.60887844677386,2.17419037968845,137.73102568646));
#229108=CARTESIAN_POINT('Ctrl Pts',(7.6579276241108,1.98495982424852,137.723165510297));
#229109=CARTESIAN_POINT('Ctrl Pts',(7.7070131150093,1.79558917195487,137.715299514853));
#229110=CARTESIAN_POINT('Ctrl Pts',(7.74904583020806,1.60449024757822,137.707433519408));
#229111=CARTESIAN_POINT('Ctrl Pts',(7.78392682092784,1.41223377896162,137.699567523964));
#229112=CARTESIAN_POINT('Ctrl Pts',(7.8097590720885,1.26985200361403,137.693742105426));
#229113=CARTESIAN_POINT('Ctrl Pts',(7.83166993231325,1.1268355922756,137.687916686889));
#229114=CARTESIAN_POINT('Ctrl Pts',(7.84963754731252,0.983418210031437,
137.682091268351));
#229115=CARTESIAN_POINT('Ctrl Pts',(7.87718026824534,0.763572396537256,
137.673161431135));
#229116=CARTESIAN_POINT('Ctrl Pts',(7.89547509537865,0.542630538372062,
137.664231593919));
#229117=CARTESIAN_POINT('Ctrl Pts',(7.90447130504336,0.321332207763367,
137.655301756703));
#229118=CARTESIAN_POINT('Ctrl Pts',(7.91346938005995,0.0999879912458073,
137.646370067898));
#229119=CARTESIAN_POINT('Ctrl Pts',(7.9131649801128,-0.121712667043669,
137.637438379092));
#229120=CARTESIAN_POINT('Ctrl Pts',(7.90355947844026,-0.343028527614233,
137.628506690287));
#229121=CARTESIAN_POINT('Ctrl Pts',(7.89396064943931,-0.564190646287026,
137.619581206074));
#229122=CARTESIAN_POINT('Ctrl Pts',(7.87507364340439,-0.784968323718609,
137.610655721861));
#229123=CARTESIAN_POINT('Ctrl Pts',(7.84695182636227,-1.00462332978574,
137.601730237649));
#229124=CARTESIAN_POINT('Ctrl Pts',(7.81885546307165,-1.22407952067923,
137.592812832112));
#229125=CARTESIAN_POINT('Ctrl Pts',(7.78154100710172,-1.44241489332641,
137.583895426576));
#229126=CARTESIAN_POINT('Ctrl Pts',(7.73511348190396,-1.65889735127513,
137.574978021039));
#229127=CARTESIAN_POINT('Ctrl Pts',(7.68879188541431,-1.87488588440226,
137.566080961391));
#229128=CARTESIAN_POINT('Ctrl Pts',(7.63339877760798,-2.08902977067117,
137.557183901744));
#229129=CARTESIAN_POINT('Ctrl Pts',(7.56908981737375,-2.30060868826689,
137.548286842096));
#229130=CARTESIAN_POINT('Ctrl Pts',(7.5084942750378,-2.49997032017428,137.539903528906));
#229131=CARTESIAN_POINT('Ctrl Pts',(7.43998324254046,-2.69705457975007,
137.531520215716));
#229132=CARTESIAN_POINT('Ctrl Pts',(7.3637285946372,-2.89126653640277,137.523136902526));
#229133=CARTESIAN_POINT('Ctrl Pts',(7.29141407464606,-3.07544343326152,
137.515186760653));
#229134=CARTESIAN_POINT('Ctrl Pts',(7.21216691845961,-3.25695364429777,
137.507236618781));
#229135=CARTESIAN_POINT('Ctrl Pts',(7.1262167607559,-3.4352519090631,137.499286476908));
#229136=CARTESIAN_POINT('Ctrl Pts',(7.04027424968884,-3.61353431135555,
137.491337042328));
#229137=CARTESIAN_POINT('Ctrl Pts',(6.94763007264582,-3.78860503235103,
137.483387607747));
#229138=CARTESIAN_POINT('Ctrl Pts',(6.84856099919256,-3.95994106526078,
137.475438173166));
#229139=CARTESIAN_POINT('Ctrl Pts',(6.74948496992316,-4.13128912797861,
137.467488180442));
#229140=CARTESIAN_POINT('Ctrl Pts',(6.64398331521634,-4.29890168764394,
137.459538187717));
#229141=CARTESIAN_POINT('Ctrl Pts',(6.53237769691227,-4.46228222156366,
137.451588194993));
#229142=CARTESIAN_POINT('Ctrl Pts',(6.4207063793305,-4.62575893328549,137.443633522317));
#229143=CARTESIAN_POINT('Ctrl Pts',(6.30292410901325,-4.78499836153753,
137.435678849642));
#229144=CARTESIAN_POINT('Ctrl Pts',(6.17939520875281,-4.93953397134212,
137.427724176967));
#229145=CARTESIAN_POINT('Ctrl Pts',(6.05582777813717,-5.09411778291913,
137.419767023121));
#229146=CARTESIAN_POINT('Ctrl Pts',(5.92651036112141,-5.2439945915914,137.411809869274));
#229147=CARTESIAN_POINT('Ctrl Pts',(5.79184650745455,-5.38873222883514,
137.403852715428));
#229148=CARTESIAN_POINT('Ctrl Pts',(5.65705792690499,-5.5336039233913,137.395888191593));
#229149=CARTESIAN_POINT('Ctrl Pts',(5.51691325199007,-5.67332669388599,
137.387923667759));
#229150=CARTESIAN_POINT('Ctrl Pts',(5.37185250905003,-5.80750562815163,
137.379959143924));
#229151=CARTESIAN_POINT('Ctrl Pts',(5.27607083134976,-5.89610219242892,
137.37470027485));
#229152=CARTESIAN_POINT('Ctrl Pts',(5.17814657378654,-5.98228256059462,
137.369441405775));
#229153=CARTESIAN_POINT('Ctrl Pts',(5.07821400434164,-6.06594292143509,
137.364182536701));
#229154=CARTESIAN_POINT('Ctrl Pts',(4.92603880247249,-6.19333914841155,
137.356174442168));
#229155=CARTESIAN_POINT('Ctrl Pts',(4.76893302042205,-6.31511772874101,
137.348166347636));
#229156=CARTESIAN_POINT('Ctrl Pts',(4.60734473284941,-6.43088605968764,
137.340158253103));
#229157=CARTESIAN_POINT('Ctrl Pts',(4.44588202042821,-6.54656442355863,
137.332156381903));
#229158=CARTESIAN_POINT('Ctrl Pts',(4.27994401469346,-6.65624165372637,
137.324154510703));
#229159=CARTESIAN_POINT('Ctrl Pts',(4.11001185674365,-6.75956533642708,
137.316152639504));
#229160=CARTESIAN_POINT('Ctrl Pts',(3.94018336624525,-6.86282598630938,
137.308155649861));
#229161=CARTESIAN_POINT('Ctrl Pts',(3.76636586409051,-6.95974064185519,
137.300158660219));
#229162=CARTESIAN_POINT('Ctrl Pts',(3.58906981975408,-7.04999991694542,
137.292161670577));
#229163=CARTESIAN_POINT('Ctrl Pts',(3.4118523266209,-7.14021920256668,137.284168224009));
#229164=CARTESIAN_POINT('Ctrl Pts',(3.23115965990965,-7.22378883490069,
137.276174777441));
#229165=CARTESIAN_POINT('Ctrl Pts',(3.0475276347068,-7.30044493957035,137.268181330874));
#229166=CARTESIAN_POINT('Ctrl Pts',(2.86394631192219,-7.3770798788149,137.260190091367));
#229167=CARTESIAN_POINT('Ctrl Pts',(2.67742755588218,-7.44680496804883,
137.252198851861));
#229168=CARTESIAN_POINT('Ctrl Pts',(2.48852833353138,-7.50940395325831,
137.244207612354));
#229169=CARTESIAN_POINT('Ctrl Pts',(2.29357765115322,-7.57400832129591,
137.235960370383));
#229170=CARTESIAN_POINT('Ctrl Pts',(2.09609179479209,-7.63102228981386,
137.227713128412));
#229171=CARTESIAN_POINT('Ctrl Pts',(1.89670189544186,-7.68026320641599,
137.219465886441));
#229172=CARTESIAN_POINT('Ctrl Pts',(1.70346233245657,-7.72798524868694,
137.211473037057));
#229173=CARTESIAN_POINT('Ctrl Pts',(1.50843478373704,-7.76840656863684,
137.203480187672));
#229174=CARTESIAN_POINT('Ctrl Pts',(1.31220603019056,-7.80141245764711,
137.195487338288));
#229175=CARTESIAN_POINT('Ctrl Pts',(1.11592948169991,-7.83442638581879,
137.187492542105));
#229176=CARTESIAN_POINT('Ctrl Pts',(0.918451473767237,-7.86002122647965,
137.179497745922));
#229177=CARTESIAN_POINT('Ctrl Pts',(0.720366334600081,-7.87813387446385,
137.17150294974));
#229178=CARTESIAN_POINT('Ctrl Pts',(0.522202939233237,-7.89625367809337,
137.163504995105));
#229179=CARTESIAN_POINT('Ctrl Pts',(0.323432266201273,-7.90688536532492,
137.15550704047));
#229180=CARTESIAN_POINT('Ctrl Pts',(0.124651486185002,-7.91001788917016,
137.147509085836));
#229181=CARTESIAN_POINT('Ctrl Pts',(-0.074237946007496,-7.91315212523089,
137.139506759576));
#229182=CARTESIAN_POINT('Ctrl Pts',(-0.273137163426149,-7.90877902027729,
137.131504433315));
#229183=CARTESIAN_POINT('Ctrl Pts',(-0.471450878998735,-7.89693960143367,
137.123502107055));
#229184=CARTESIAN_POINT('Ctrl Pts',(-0.670002770870968,-7.88508596335683,
137.115490169939));
#229185=CARTESIAN_POINT('Ctrl Pts',(-0.867967423520542,-7.86574811784401,
137.107478232823));
#229186=CARTESIAN_POINT('Ctrl Pts',(-1.06475525431146,-7.83901889578129,
137.099466295708));
#229187=CARTESIAN_POINT('Ctrl Pts',(-1.26168279717544,-7.81227069696066,
137.091448670413));
#229188=CARTESIAN_POINT('Ctrl Pts',(-1.45743152451879,-7.77812071217562,
137.083431045119));
#229189=CARTESIAN_POINT('Ctrl Pts',(-1.6514233551077,-7.73671260305078,
137.075413419824));
#229190=CARTESIAN_POINT('Ctrl Pts',(-1.84566907495877,-7.69525030053934,
137.067385301361));
#229191=CARTESIAN_POINT('Ctrl Pts',(-2.03815298324123,-7.6465109805656,
137.059357182898));
#229192=CARTESIAN_POINT('Ctrl Pts',(-2.22831228863559,-7.59068806791029,
137.051329064435));
#229193=CARTESIAN_POINT('Ctrl Pts',(-2.26822635722923,-7.57897094704576,
137.049643977974));
#229194=CARTESIAN_POINT('Ctrl Pts',(-2.3080380813465,-7.56694191164845,
137.047958891513));
#229195=CARTESIAN_POINT('Ctrl Pts',(-2.34774237437529,-7.55460301694025,
137.046273805051));
#229196=CARTESIAN_POINT('Ctrl Pts',(-2.53019976867307,-7.4979007712828,
137.038530146584));
#229197=CARTESIAN_POINT('Ctrl Pts',(-2.71093239789151,-7.43448165792094,
137.030786488117));
#229198=CARTESIAN_POINT('Ctrl Pts',(-2.88939377760752,-7.36446363273816,
137.02304282965));
#229199=CARTESIAN_POINT('Ctrl Pts',(-3.0676382729918,-7.29453070054651,
137.01530858206));
#229200=CARTESIAN_POINT('Ctrl Pts',(-3.2436166815152,-7.2180149475349,137.007574334471));
#229201=CARTESIAN_POINT('Ctrl Pts',(-3.41679451805204,-7.13508487836056,
136.999840086881));
#229202=CARTESIAN_POINT('Ctrl Pts',(-3.58979732104159,-7.05223862790388,
136.992113656417));
#229203=CARTESIAN_POINT('Ctrl Pts',(-3.76000486430489,-6.96299112005469,
136.984387225952));
#229204=CARTESIAN_POINT('Ctrl Pts',(-3.92689952899846,-6.86756005355262,
136.976660795487));
#229205=CARTESIAN_POINT('Ctrl Pts',(-4.09365959479012,-6.77220595126497,
136.968940596313));
#229206=CARTESIAN_POINT('Ctrl Pts',(-4.25711178994332,-6.67067839616624,
136.961220397138));
#229207=CARTESIAN_POINT('Ctrl Pts',(-4.41676007373928,-6.56324244950791,
136.953500197963));
#229208=CARTESIAN_POINT('Ctrl Pts',(-4.5763121659837,-6.45587123533624,
136.945784650376));
#229209=CARTESIAN_POINT('Ctrl Pts',(-4.73206461227333,-6.34259891835515,
136.938069102789));
#229210=CARTESIAN_POINT('Ctrl Pts',(-4.88354745926241,-6.2237356316871,
136.930353555202));
#229211=CARTESIAN_POINT('Ctrl Pts',(-5.03496990566085,-6.10491973924792,
136.922641084026));
#229212=CARTESIAN_POINT('Ctrl Pts',(-5.18212585994934,-5.98051753896768,
136.914928612851));
#229213=CARTESIAN_POINT('Ctrl Pts',(-5.32457571748206,-5.85088150869596,
136.907216141675));
#229214=CARTESIAN_POINT('Ctrl Pts',(-5.46702519221316,-5.72124582679163,
136.899503691226));
#229215=CARTESIAN_POINT('Ctrl Pts',(-5.60476832086258,-5.58637657686959,
136.891791240776));
#229216=CARTESIAN_POINT('Ctrl Pts',(-5.73739958768388,-5.4466656746348,
136.884078790326));
#229217=CARTESIAN_POINT('Ctrl Pts',(-5.87003721824548,-5.30694806897387,
136.876365969827));
#229218=CARTESIAN_POINT('Ctrl Pts',(-5.99756224937468,-5.16238860943103,
136.868653149329));
#229219=CARTESIAN_POINT('Ctrl Pts',(-6.11960711221558,-5.01341498303507,
136.86094032883));
#229220=CARTESIAN_POINT('Ctrl Pts',(-6.24168035510818,-4.86440671463026,
136.853225714809));
#229221=CARTESIAN_POINT('Ctrl Pts',(-6.35827066347908,-4.71098251444336,
136.845511100787));
#229222=CARTESIAN_POINT('Ctrl Pts',(-6.46905172182266,-4.5536019611274,
136.837796486766));
#229223=CARTESIAN_POINT('Ctrl Pts',(-6.57987899456815,-4.39615575355382,
136.830078654448));
#229224=CARTESIAN_POINT('Ctrl Pts',(-6.68489198454414,-4.23475020122318,
136.82236082213));
#229225=CARTESIAN_POINT('Ctrl Pts',(-6.78380852903311,-4.06987258294625,
136.814642989813));
#229226=CARTESIAN_POINT('Ctrl Pts',(-6.8828441955438,-3.90479640784218,
136.806915863157));
#229227=CARTESIAN_POINT('Ctrl Pts',(-6.97576856889581,-3.73624012568704,
136.799188736502));
#229228=CARTESIAN_POINT('Ctrl Pts',(-7.06234569075244,-3.56471518417818,
136.791461609846));
#229229=CARTESIAN_POINT('Ctrl Pts',(-7.14897920919224,-3.39307851083505,
136.783729449718));
#229230=CARTESIAN_POINT('Ctrl Pts',(-7.22925709111192,-3.21846965281537,
136.77599728959));
#229231=CARTESIAN_POINT('Ctrl Pts',(-7.30299218554266,-3.04141844176411,
136.768265129462));
#229232=CARTESIAN_POINT('Ctrl Pts',(-7.37684175556544,-2.86409235424645,
136.760520964961));
#229233=CARTESIAN_POINT('Ctrl Pts',(-7.44412812516747,-2.68431667691066,
136.75277680046));
#229234=CARTESIAN_POINT('Ctrl Pts',(-7.50471415038671,-2.50263591458795,
136.745032635958));
#229235=CARTESIAN_POINT('Ctrl Pts',(-7.54818005581054,-2.37229366480557,
136.739476781773));
#229236=CARTESIAN_POINT('Ctrl Pts',(-7.58819837098074,-2.24097114054649,
136.733920927587));
#229237=CARTESIAN_POINT('Ctrl Pts',(-7.6247348206606,-2.10887171601445,
136.728365073402));
#229238=CARTESIAN_POINT('Ctrl Pts',(-7.69817641599759,-1.84333982756507,
136.717197299893));
#229239=CARTESIAN_POINT('Ctrl Pts',(-7.75774424075977,-1.57396649721242,
136.706029526384));
#229240=CARTESIAN_POINT('Ctrl Pts',(-7.80312831751188,-1.30196369398084,
136.694861752875));
#229241=CARTESIAN_POINT('Ctrl Pts',(-7.84692604597825,-1.03946843637983,
136.684084336065));
#229242=CARTESIAN_POINT('Ctrl Pts',(-7.87751447532542,-0.77452376069535,
136.673306919254));
#229243=CARTESIAN_POINT('Ctrl Pts',(-7.89465718412611,-0.508241030541709,
136.662529502443));
#229244=CARTESIAN_POINT('Ctrl Pts',(-7.90536625412329,-0.341893901309606,
136.655796837708));
#229245=CARTESIAN_POINT('Ctrl Pts',(-7.91082891972596,-0.175025061706264,
136.649064172972));
#229246=CARTESIAN_POINT('Ctrl Pts',(-7.91099604399589,-0.00791150310789744,
136.642331508237));
#229247=CARTESIAN_POINT('',(-7.911,6.23723295234413E-12,134.642331508237));
#229248=CARTESIAN_POINT('Ctrl Pts',(-7.911,6.85784762310959E-12,136.642331508237));
#229249=CARTESIAN_POINT('Ctrl Pts',(-7.91099999999809,2.20167589667335,
136.553744072504));
#229250=CARTESIAN_POINT('Ctrl Pts',(-6.94214576672016,4.38610418339232,
136.465156636771));
#229251=CARTESIAN_POINT('Ctrl Pts',(-3.67820201487745,7.34180684107895,
136.287981765306));
#229252=CARTESIAN_POINT('Ctrl Pts',(-1.40868175871181,8.08992666571427,
136.199394329573));
#229253=CARTESIAN_POINT('Ctrl Pts',(2.97309270521754,7.65454228025063,136.022219458108));
#229254=CARTESIAN_POINT('Ctrl Pts',(5.05102072675981,6.47444880833921,135.933632022375));
#229255=CARTESIAN_POINT('Ctrl Pts',(7.66951518848019,2.934251953673,135.75645715091));
#229256=CARTESIAN_POINT('Ctrl Pts',(8.18956872247094,0.601881960095167,
135.667869715177));
#229257=CARTESIAN_POINT('Ctrl Pts',(7.32306689761179,-3.71537198232757,
135.490694843711));
#229258=CARTESIAN_POINT('Ctrl Pts',(5.94329958849978,-5.66643518936734,
135.402107407979));
#229259=CARTESIAN_POINT('Ctrl Pts',(2.16154501637591,-7.9220591323306,135.224932536513));
#229260=CARTESIAN_POINT('Ctrl Pts',(-0.210816529302679,-8.20894963712989,
135.136345100781));
#229261=CARTESIAN_POINT('Ctrl Pts',(-4.42123908576584,-6.91982244717729,
134.959170229315));
#229262=CARTESIAN_POINT('Ctrl Pts',(-6.22631625634278,-5.35390358803405,
134.870582793582));
#229263=CARTESIAN_POINT('Ctrl Pts',(-7.65317280859594,-2.31334857514253,
134.735440741312));
#229264=CARTESIAN_POINT('Ctrl Pts',(-7.91100000000091,-1.15702837836065,
134.688886124774));
#229265=CARTESIAN_POINT('Ctrl Pts',(-7.911,6.23723295234413E-12,134.642331508237));
#229266=CARTESIAN_POINT('',(-7.91099763196637,-0.00612103116663704,130.642331508237));
#229267=CARTESIAN_POINT('Ctrl Pts',(-7.91099965031895,0.00235215931849442,
134.634842937691));
#229268=CARTESIAN_POINT('Ctrl Pts',(-7.91070729992585,0.985612025887326,
134.597355279287));
#229269=CARTESIAN_POINT('Ctrl Pts',(-7.72714776753475,1.95996465666296,
134.567471101788));
#229270=CARTESIAN_POINT('Ctrl Pts',(-7.31415261496248,3.01836535369072,
134.525553036253));
#229271=CARTESIAN_POINT('Ctrl Pts',(-7.25437688176638,3.15933044397698,
134.519727960306));
#229272=CARTESIAN_POINT('Ctrl Pts',(-7.18066625036259,3.32001739034016,
134.512704803826));
#229273=CARTESIAN_POINT('Ctrl Pts',(-7.17068269178165,3.34152554982886,
134.511756670364));
#229274=CARTESIAN_POINT('Ctrl Pts',(-7.15767334640095,3.36922554119806,
134.510524739347));
#229275=CARTESIAN_POINT('Ctrl Pts',(-7.15473596741449,3.37545874174651,
134.510246816222));
#229276=CARTESIAN_POINT('Ctrl Pts',(-7.14995802542409,3.38556341111709,
134.509795135232));
#229277=CARTESIAN_POINT('Ctrl Pts',(-7.14812244722044,3.38943724760068,
134.509621702051));
#229278=CARTESIAN_POINT('Ctrl Pts',(-7.14459970572387,3.39685611393449,
134.509289038257));
#229279=CARTESIAN_POINT('Ctrl Pts',(-7.14291304972564,3.40040138480072,
134.509129840455));
#229280=CARTESIAN_POINT('Ctrl Pts',(-7.139069267868,3.40846535268475,134.508767219703));
#229281=CARTESIAN_POINT('Ctrl Pts',(-7.13691049146306,3.41298325640359,
134.508563690786));
#229282=CARTESIAN_POINT('Ctrl Pts',(-7.13020554840639,3.42698123384001,
134.507931956892));
#229283=CARTESIAN_POINT('Ctrl Pts',(-7.12564478750139,3.43645426274363,
134.507502823043));
#229284=CARTESIAN_POINT('Ctrl Pts',(-7.09139987360813,3.50722212627631,
134.504285084167));
#229285=CARTESIAN_POINT('Ctrl Pts',(-7.06094499922386,3.56813878738974,
134.501448365001));
#229286=CARTESIAN_POINT('Ctrl Pts',(-6.94142129914273,3.79968938528309,
134.490429767277));
#229287=CARTESIAN_POINT('Ctrl Pts',(-6.84692660120395,3.96743699089044,
134.481952306651));
#229288=CARTESIAN_POINT('Ctrl Pts',(-6.35550715057569,4.7698745756642,134.439527352387));
#229289=CARTESIAN_POINT('Ctrl Pts',(-5.87597847899331,5.34951237034305,
134.403378010267));
#229290=CARTESIAN_POINT('Ctrl Pts',(-5.19235134669754,5.97110921833049,
134.362495107838));
#229291=CARTESIAN_POINT('Ctrl Pts',(-5.05874729136224,6.08471352498639,
134.354890940838));
#229292=CARTESIAN_POINT('Ctrl Pts',(-4.83613591494947,6.26159648918448,
134.342843428782));
#229293=CARTESIAN_POINT('Ctrl Pts',(-4.74940477550864,6.32763437006564,
134.338293640868));
#229294=CARTESIAN_POINT('Ctrl Pts',(-4.62873102055958,6.41563702386578,
134.332155401607));
#229295=CARTESIAN_POINT('Ctrl Pts',(-4.59594603103169,6.43916372101804,
134.3305066431));
#229296=CARTESIAN_POINT('Ctrl Pts',(-4.53985110592844,6.4787710813844,134.327717306397));
#229297=CARTESIAN_POINT('Ctrl Pts',(-4.51663239555363,6.4949791850433,134.326571864853));
#229298=CARTESIAN_POINT('Ctrl Pts',(-4.48437192529442,6.51724234787714,
134.324992834236));
#229299=CARTESIAN_POINT('Ctrl Pts',(-4.47540408339446,6.52340384131562,
134.324555216067));
#229300=CARTESIAN_POINT('Ctrl Pts',(-4.46087077750231,6.53334509775676,
134.323848143605));
#229301=CARTESIAN_POINT('Ctrl Pts',(-4.45531316819409,6.53713628690428,
134.323578258616));
#229302=CARTESIAN_POINT('Ctrl Pts',(-4.44370971825894,6.54503004751404,
134.3230158255));
#229303=CARTESIAN_POINT('Ctrl Pts',(-4.43766301505954,6.54913134302183,
134.322723325478));
#229304=CARTESIAN_POINT('Ctrl Pts',(-4.42363768719583,6.55861595541005,
134.32204623608));
#229305=CARTESIAN_POINT('Ctrl Pts',(-4.4156548952219,6.56399310521258,134.321661878074));
#229306=CARTESIAN_POINT('Ctrl Pts',(-4.38985596927511,6.58130271037187,
134.320422981844));
#229307=CARTESIAN_POINT('Ctrl Pts',(-4.37200105934812,6.59317734804389,
134.319570602593));
#229308=CARTESIAN_POINT('Ctrl Pts',(-4.20428424590407,6.70373870007293,
134.311610559462));
#229309=CARTESIAN_POINT('Ctrl Pts',(-4.05114905908561,6.79737558017027,
134.304691823014));
#229310=CARTESIAN_POINT('Ctrl Pts',(-3.65788389168276,7.01982852255921,
134.287689075509));
#229311=CARTESIAN_POINT('Ctrl Pts',(-3.41403731740536,7.14160119837584,
134.277837359741));
#229312=CARTESIAN_POINT('Ctrl Pts',(-3.00391008688681,7.32059442494948,
134.262012632256));
#229313=CARTESIAN_POINT('Ctrl Pts',(-2.84115202323861,7.38528503494512,
134.25591347262));
#229314=CARTESIAN_POINT('Ctrl Pts',(-2.36201510346746,7.55753953663914,
134.238248325779));
#229315=CARTESIAN_POINT('Ctrl Pts',(-2.04081550068744,7.65052808493037,
134.226772596442));
#229316=CARTESIAN_POINT('Ctrl Pts',(-1.42065228693337,7.78822194147042,
134.204015471019));
#229317=CARTESIAN_POINT('Ctrl Pts',(-1.12316738090208,7.83665441464296,
134.192789956154));
#229318=CARTESIAN_POINT('Ctrl Pts',(-0.801294635919355,7.87034624121721,
134.179894009537));
#229319=CARTESIAN_POINT('Ctrl Pts',(-0.779000233120226,7.87258418023723,
134.178997701949));
#229320=CARTESIAN_POINT('Ctrl Pts',(-0.747228429024424,7.87563719021797,
134.177716225397));
#229321=CARTESIAN_POINT('Ctrl Pts',(-0.737758487662745,7.87652993964204,
134.177333742565));
#229322=CARTESIAN_POINT('Ctrl Pts',(-0.721428555241354,7.87803968508456,
134.176673307624));
#229323=CARTESIAN_POINT('Ctrl Pts',(-0.714569314518207,7.87866480658477,
134.17639562941));
#229324=CARTESIAN_POINT('Ctrl Pts',(-0.701450640028202,7.87984311304252,
134.175864050023));
#229325=CARTESIAN_POINT('Ctrl Pts',(-0.695191344606962,7.88039779964692,
134.175610198683));
#229326=CARTESIAN_POINT('Ctrl Pts',(-0.680550704538279,7.88167764574459,
134.175015929004));
#229327=CARTESIAN_POINT('Ctrl Pts',(-0.672168857583668,7.88239689429476,
134.174675319079));
#229328=CARTESIAN_POINT('Ctrl Pts',(-0.642411189064694,7.88490259810949,
134.173464722853));
#229329=CARTESIAN_POINT('Ctrl Pts',(-0.621029356463556,7.88661547475162,
134.172592407784));
#229330=CARTESIAN_POINT('Ctrl Pts',(-0.253090550480812,7.9145851017779,
134.157541563156));
#229331=CARTESIAN_POINT('Ctrl Pts',(0.0948079532204345,7.91806201106853,
134.142720512965));
#229332=CARTESIAN_POINT('Ctrl Pts',(0.559162513855125,7.89208955629123,
134.122747046785));
#229333=CARTESIAN_POINT('Ctrl Pts',(0.67637341337458,7.88290931110074,134.117686834216));
#229334=CARTESIAN_POINT('Ctrl Pts',(1.69832656368766,7.77990591646846,134.073493473426));
#229335=CARTESIAN_POINT('Ctrl Pts',(2.58087950293275,7.53328953772175,134.035568794168));
#229336=CARTESIAN_POINT('Ctrl Pts',(3.45796295061826,7.11549290833311,133.996144003404));
#229337=CARTESIAN_POINT('Ctrl Pts',(3.51349273445849,7.08823786101105,133.993640896697));
#229338=CARTESIAN_POINT('Ctrl Pts',(3.59300282443886,7.04804890630641,133.990046534826));
#229339=CARTESIAN_POINT('Ctrl Pts',(3.61724467631051,7.03563811180938,133.988949251469));
#229340=CARTESIAN_POINT('Ctrl Pts',(3.65940401583432,7.0137788338023,133.987038472488));
#229341=CARTESIAN_POINT('Ctrl Pts',(3.67735017555703,7.00438626645202,133.986224313934));
#229342=CARTESIAN_POINT('Ctrl Pts',(3.71379968247048,6.98513081896998,133.984569087552));
#229343=CARTESIAN_POINT('Ctrl Pts',(3.73230029191427,6.97526308992605,133.983728086593));
#229344=CARTESIAN_POINT('Ctrl Pts',(3.77872308343237,6.95026484566663,133.981615589364));
#229345=CARTESIAN_POINT('Ctrl Pts',(3.80659383434492,6.93503950653828,133.980345294921));
#229346=CARTESIAN_POINT('Ctrl Pts',(3.91146992995167,6.8769246916588,133.975557335384));
#229347=CARTESIAN_POINT('Ctrl Pts',(3.98784878023691,6.83291684146512,133.972054252011));
#229348=CARTESIAN_POINT('Ctrl Pts',(4.57845825960972,6.47934367071942,133.944822035303));
#229349=CARTESIAN_POINT('Ctrl Pts',(5.05667537576387,6.11344492418261,133.922074582275));
#229350=CARTESIAN_POINT('Ctrl Pts',(5.60901817140684,5.58127707323018,133.892429913593));
#229351=CARTESIAN_POINT('Ctrl Pts',(5.72543544308371,5.46178778410835,133.885944362167));
#229352=CARTESIAN_POINT('Ctrl Pts',(5.89284034526309,5.27872717451378,133.87615645709));
#229353=CARTESIAN_POINT('Ctrl Pts',(5.94676546202799,5.21790265562518,133.872927112294));
#229354=CARTESIAN_POINT('Ctrl Pts',(6.01172370144999,5.14231825285087,133.868931546136));
#229355=CARTESIAN_POINT('Ctrl Pts',(6.02365567218836,5.12833610587973,133.868193113736));
#229356=CARTESIAN_POINT('Ctrl Pts',(6.04275714719806,5.10579393722438,133.867003683716));
#229357=CARTESIAN_POINT('Ctrl Pts',(6.0499574054631,5.09726015232854,133.866553655817));
#229358=CARTESIAN_POINT('Ctrl Pts',(6.06367642953856,5.08093027219427,133.865693012521));
#229359=CARTESIAN_POINT('Ctrl Pts',(6.07019829018416,5.07313679986769,133.865282489572));
#229360=CARTESIAN_POINT('Ctrl Pts',(6.08509601278354,5.0552645086772,133.864341590493));
#229361=CARTESIAN_POINT('Ctrl Pts',(6.09346187737195,5.04517740867602,133.863810931039));
#229362=CARTESIAN_POINT('Ctrl Pts',(6.11916652746654,5.01402695513974,133.862173418814));
#229363=CARTESIAN_POINT('Ctrl Pts',(6.13642139375905,4.99289472784215,133.861064287228));
#229364=CARTESIAN_POINT('Ctrl Pts',(6.34265325608749,4.73763632870868,133.847690102012));
#229365=CARTESIAN_POINT('Ctrl Pts',(6.51823038483631,4.49300710983339,133.835113530052));
#229366=CARTESIAN_POINT('Ctrl Pts',(6.87405300120233,3.9323305228053,133.807240717542));
#229367=CARTESIAN_POINT('Ctrl Pts',(7.04731747628843,3.61263778420711,133.791961776323));
#229368=CARTESIAN_POINT('Ctrl Pts',(7.26674204946458,3.1314262023491,133.770028037084));
#229369=CARTESIAN_POINT('Ctrl Pts',(7.3307278590558,2.97855678215018,133.763203941213));
#229370=CARTESIAN_POINT('Ctrl Pts',(7.41585392593125,2.75578154225637,133.753457413638));
#229371=CARTESIAN_POINT('Ctrl Pts',(7.44090088381112,2.68741800260095,133.75049258707));
#229372=CARTESIAN_POINT('Ctrl Pts',(7.48416387073204,2.5640911608469,133.745188889147));
#229373=CARTESIAN_POINT('Ctrl Pts',(7.50272685477848,2.50925529376175,133.742846356551));
#229374=CARTESIAN_POINT('Ctrl Pts',(7.5298989167658,2.42598952085995,133.739311936622));
#229375=CARTESIAN_POINT('Ctrl Pts',(7.53895246049939,2.39770695842284,133.738115329271));
#229376=CARTESIAN_POINT('Ctrl Pts',(7.55499794020347,2.34659269046629,133.735959587966));
#229377=CARTESIAN_POINT('Ctrl Pts',(7.56204615435491,2.32377905467626,133.734999875491));
#229378=CARTESIAN_POINT('Ctrl Pts',(7.57704736052552,2.27443213586511,133.732929127839));
#229379=CARTESIAN_POINT('Ctrl Pts',(7.58496450688547,2.24788827120917,133.731818472487));
#229380=CARTESIAN_POINT('Ctrl Pts',(7.60577576594224,2.17675232082948,133.728850270435));
#229381=CARTESIAN_POINT('Ctrl Pts',(7.61841711327296,2.13208733031883,133.726995276738));
#229382=CARTESIAN_POINT('Ctrl Pts',(7.6813222812751,1.90212271964092,133.717486283887));
#229383=CARTESIAN_POINT('Ctrl Pts',(7.72522185659126,1.71514757806987,133.709892612196));
#229384=CARTESIAN_POINT('Ctrl Pts',(7.84100751703233,1.12647591692705,133.686280670193));
#229385=CARTESIAN_POINT('Ctrl Pts',(7.88866097942817,0.720691615053063,
133.670522200799));
#229386=CARTESIAN_POINT('Ctrl Pts',(7.91876629570847,-0.0395408363007919,
133.641787822611));
#229387=CARTESIAN_POINT('Ctrl Pts',(7.90912452918413,-0.392651176533162,
133.628744523392));
#229388=CARTESIAN_POINT('Ctrl Pts',(7.84733411201154,-1.04681399129394,
133.604330554539));
#229389=CARTESIAN_POINT('Ctrl Pts',(7.80127938114409,-1.34777551333776,
133.592990423676));
#229390=CARTESIAN_POINT('Ctrl Pts',(7.71584317862537,-1.74958475678387,
133.577072051011));
#229391=CARTESIAN_POINT('Ctrl Pts',(7.69156990597228,-1.85338448485048,
133.572886854609));
#229392=CARTESIAN_POINT('Ctrl Pts',(7.66151993466688,-1.97110516497737,
133.568029101787));
#229393=CARTESIAN_POINT('Ctrl Pts',(7.65779159723041,-1.98554051342504,
133.567431503542));
#229394=CARTESIAN_POINT('Ctrl Pts',(7.65210661151424,-2.0072973965174,133.566527800184));
#229395=CARTESIAN_POINT('Ctrl Pts',(7.65018020112903,-2.0146268443092,133.56622284566));
#229396=CARTESIAN_POINT('Ctrl Pts',(7.64683971670512,-2.02726256394383,
133.565696209394));
#229397=CARTESIAN_POINT('Ctrl Pts',(7.64543064191786,-2.03257016006475,
133.565474721768));
#229398=CARTESIAN_POINT('Ctrl Pts',(7.6425084731209,-2.04353113224334,133.565016740222));
#229399=CARTESIAN_POINT('Ctrl Pts',(7.64099463032019,-2.04918430341032,
133.564780216944));
#229400=CARTESIAN_POINT('Ctrl Pts',(7.63688040825467,-2.06448017033174,
133.564139382174));
#229401=CARTESIAN_POINT('Ctrl Pts',(7.63426804489553,-2.07411961110434,
133.563734591974));
#229402=CARTESIAN_POINT('Ctrl Pts',(7.62450382469438,-2.1098805438719,133.562229321277));
#229403=CARTESIAN_POINT('Ctrl Pts',(7.61723614995478,-2.13597001216449,
133.561124096314));
#229404=CARTESIAN_POINT('Ctrl Pts',(7.50475422953521,-2.53188136403538,
133.544238339615));
#229405=CARTESIAN_POINT('Ctrl Pts',(7.37287032290911,-2.89351464806571,
133.527128447268));
#229406=CARTESIAN_POINT('Ctrl Pts',(7.00605023781762,-3.70937581191444,
133.486318696312));
#229407=CARTESIAN_POINT('Ctrl Pts',(6.75230222157421,-4.15339250603831,
133.462483465425));
#229408=CARTESIAN_POINT('Ctrl Pts',(6.22613584299422,-4.89690262860306,
133.421778811307));
#229409=CARTESIAN_POINT('Ctrl Pts',(5.97018612154915,-5.20589648393161,
133.404554765575));
#229410=CARTESIAN_POINT('Ctrl Pts',(5.67758223457798,-5.50902949833257,
133.387415659092));
#229411=CARTESIAN_POINT('Ctrl Pts',(5.66320599660458,-5.52380701074462,
133.386579379995));
#229412=CARTESIAN_POINT('Ctrl Pts',(5.63718616773183,-5.55034476175778,
133.385076157805));
#229413=CARTESIAN_POINT('Ctrl Pts',(5.62556315584081,-5.56212495794752,
133.384408364525));
#229414=CARTESIAN_POINT('Ctrl Pts',(5.60762225853358,-5.58019471661327,
133.383383225783));
#229415=CARTESIAN_POINT('Ctrl Pts',(5.60133059520238,-5.58651018379219,
133.383024782751));
#229416=CARTESIAN_POINT('Ctrl Pts',(5.58975131153417,-5.59809404972464,
133.382367040442));
#229417=CARTESIAN_POINT('Ctrl Pts',(5.58446688802854,-5.60336562177147,
133.382067607274));
#229418=CARTESIAN_POINT('Ctrl Pts',(5.57304962634139,-5.61472292368488,
133.381422258032));
#229419=CARTESIAN_POINT('Ctrl Pts',(5.56691426036116,-5.62080610462478,
133.381076449332));
#229420=CARTESIAN_POINT('Ctrl Pts',(5.55031288731839,-5.63721242783764,
133.380143398481));
#229421=CARTESIAN_POINT('Ctrl Pts',(5.53982802947232,-5.64751649049666,
133.379556956423));
#229422=CARTESIAN_POINT('Ctrl Pts',(5.49096890530847,-5.69526612424974,
133.376837266112));
#229423=CARTESIAN_POINT('Ctrl Pts',(5.45224291384226,-5.73235057283614,
133.374719067983));
#229424=CARTESIAN_POINT('Ctrl Pts',(4.79460626787116,-6.34941710530771,
133.339360709573));
#229425=CARTESIAN_POINT('Ctrl Pts',(4.08682396485852,-6.82650753453245,
133.311041472194));
#229426=CARTESIAN_POINT('Ctrl Pts',(3.13105028480155,-7.26789524810983,
133.274251508648));
#229427=CARTESIAN_POINT('Ctrl Pts',(2.9420600289252,-7.34643143552284,133.267002245191));
#229428=CARTESIAN_POINT('Ctrl Pts',(2.56533779673298,-7.48611074256786,
133.252282692327));
#229429=CARTESIAN_POINT('Ctrl Pts',(2.37794176554221,-7.54772788883545,
133.244834406396));
#229430=CARTESIAN_POINT('Ctrl Pts',(2.1587941132795,-7.61081345082955,133.235804191481));
#229431=CARTESIAN_POINT('Ctrl Pts',(2.129088041258,-7.61917695493053,133.234573398669));
#229432=CARTESIAN_POINT('Ctrl Pts',(2.09053706622166,-7.62978761346753,
133.232968143788));
#229433=CARTESIAN_POINT('Ctrl Pts',(2.08173579709158,-7.63219367691513,
133.232601121995));
#229434=CARTESIAN_POINT('Ctrl Pts',(2.0674874736476,-7.63606235935512,133.232006103539));
#229435=CARTESIAN_POINT('Ctrl Pts',(2.06204296605477,-7.63753439373948,
133.231778537279));
#229436=CARTESIAN_POINT('Ctrl Pts',(2.05163158021397,-7.640337381323,133.231342991638));
#229437=CARTESIAN_POINT('Ctrl Pts',(2.04666496741692,-7.64166931712836,
133.231135056612));
#229438=CARTESIAN_POINT('Ctrl Pts',(2.03528565281477,-7.64470910833343,
133.230658274311));
#229439=CARTESIAN_POINT('Ctrl Pts',(2.02887209892744,-7.64641373752436,
133.230389284008));
#229440=CARTESIAN_POINT('Ctrl Pts',(2.00912226465456,-7.65163635822852,
133.229560147507));
#229441=CARTESIAN_POINT('Ctrl Pts',(1.99577896739489,-7.65512753276163,
133.228998833104));
#229442=CARTESIAN_POINT('Ctrl Pts',(1.8940200609301,-7.68146785568417,133.224709823971));
#229443=CARTESIAN_POINT('Ctrl Pts',(1.80522598327546,-7.70281888062695,
133.220919620551));
#229444=CARTESIAN_POINT('Ctrl Pts',(1.68105091908591,-7.73041245831064,
133.215571143747));
#229445=CARTESIAN_POINT('Ctrl Pts',(1.64596491820787,-7.7379589306676,133.214054601859));
#229446=CARTESIAN_POINT('Ctrl Pts',(1.58843284128214,-7.74992421876095,
133.211560385568));
#229447=CARTESIAN_POINT('Ctrl Pts',(1.56601660242534,-7.75448491381215,
133.210586710666));
#229448=CARTESIAN_POINT('Ctrl Pts',(1.53012554898418,-7.76162515323484,
133.209025078937));
#229449=CARTESIAN_POINT('Ctrl Pts',(1.51666318428827,-7.76426699684858,
133.208438728657));
#229450=CARTESIAN_POINT('Ctrl Pts',(1.49458726240653,-7.76853955171889,
133.207476301363));
#229451=CARTESIAN_POINT('Ctrl Pts',(1.48597772331084,-7.77019099230378,
133.207100729824));
#229452=CARTESIAN_POINT('Ctrl Pts',(0.968007310495516,-7.86865323204229,
133.18449235496));
#229453=CARTESIAN_POINT('Ctrl Pts',(0.450363337993549,-7.91517129740445,
133.161258006488));
#229454=CARTESIAN_POINT('Ctrl Pts',(-0.506622248122634,-7.90693083020566,
133.119693833949));
#229455=CARTESIAN_POINT('Ctrl Pts',(-0.944074815662322,-7.86670157855124,
133.10121159228));
#229456=CARTESIAN_POINT('Ctrl Pts',(-1.41494310503345,-7.78353541275905,
133.081836339441));
#229457=CARTESIAN_POINT('Ctrl Pts',(-1.45386701724515,-7.77635893222157,
133.080238064113));
#229458=CARTESIAN_POINT('Ctrl Pts',(-1.50987809959367,-7.7655968113854,
133.07794248971));
#229459=CARTESIAN_POINT('Ctrl Pts',(-1.5270096387014,-7.76224627790212,
133.077240949834));
#229460=CARTESIAN_POINT('Ctrl Pts',(-1.55680197414965,-7.75631713847533,
133.076021904543));
#229461=CARTESIAN_POINT('Ctrl Pts',(-1.56946778405745,-7.75376417072802,
133.075503945207));
#229462=CARTESIAN_POINT('Ctrl Pts',(-1.59388259695865,-7.7487807564321,
133.074506071615));
#229463=CARTESIAN_POINT('Ctrl Pts',(-1.60563243399604,-7.74635458986578,
133.074026083752));
#229464=CARTESIAN_POINT('Ctrl Pts',(-1.63343359860102,-7.74054809098502,
133.072890946134));
#229465=CARTESIAN_POINT('Ctrl Pts',(-1.64948003606043,-7.73714454322557,
133.072236200578));
#229466=CARTESIAN_POINT('Ctrl Pts',(-1.70531399080936,-7.72512022872451,
133.069959415842));
#229467=CARTESIAN_POINT('Ctrl Pts',(-1.74504570474384,-7.71624221216602,
133.068341700819));
#229468=CARTESIAN_POINT('Ctrl Pts',(-2.31842962929609,-7.5834648993405,
133.045026853933));
#229469=CARTESIAN_POINT('Ctrl Pts',(-2.83788091781876,-7.404764578742,133.024437070825));
#229470=CARTESIAN_POINT('Ctrl Pts',(-3.70050535140613,-7.00377711255711,
132.98935913984));
#229471=CARTESIAN_POINT('Ctrl Pts',(-4.05274236678752,-6.80601913273081,
132.974707058697));
#229472=CARTESIAN_POINT('Ctrl Pts',(-4.51532203922729,-6.49762074068063,
132.95371295952));
#229473=CARTESIAN_POINT('Ctrl Pts',(-4.63981385001518,-6.4093161283117,
132.947868090166));
#229474=CARTESIAN_POINT('Ctrl Pts',(-4.81855291739327,-6.27459501774054,
132.939093320269));
#229475=CARTESIAN_POINT('Ctrl Pts',(-4.8748530202892,-6.23095518493975,
132.936271198236));
#229476=CARTESIAN_POINT('Ctrl Pts',(-4.94080434151334,-6.17839341817899,
132.93288776733));
#229477=CARTESIAN_POINT('Ctrl Pts',(-4.95103325520092,-6.1701995489811,
132.932360763013));
#229478=CARTESIAN_POINT('Ctrl Pts',(-4.96672536427735,-6.15756524278659,
132.93154877244));
#229479=CARTESIAN_POINT('Ctrl Pts',(-4.9722030998187,-6.1531428471209,132.931264664718));
#229480=CARTESIAN_POINT('Ctrl Pts',(-4.98216508254784,-6.14507814963483,
132.930746759957));
#229481=CARTESIAN_POINT('Ctrl Pts',(-4.98665126082799,-6.14143823363323,
132.930513081179));
#229482=CARTESIAN_POINT('Ctrl Pts',(-4.99640521975191,-6.13350650519537,
132.930004021262));
#229483=CARTESIAN_POINT('Ctrl Pts',(-5.00167146319756,-6.12921281594096,
132.92972854583));
#229484=CARTESIAN_POINT('Ctrl Pts',(-5.01596277626851,-6.11753009611935,
132.928979243361));
#229485=CARTESIAN_POINT('Ctrl Pts',(-5.0249770248426,-6.11012789945369,
132.92850474358));
#229486=CARTESIAN_POINT('Ctrl Pts',(-5.06756018200102,-6.07500208019946,
132.926254173087));
#229487=CARTESIAN_POINT('Ctrl Pts',(-5.10091578014011,-6.04702195858714,
132.924464624876));
#229488=CARTESIAN_POINT('Ctrl Pts',(-5.74071032088883,-5.50127414999527,
132.889590353419));
#229489=CARTESIAN_POINT('Ctrl Pts',(-6.26558824262071,-4.89509781934732,
132.851114189951));
#229490=CARTESIAN_POINT('Ctrl Pts',(-6.79381420856736,-4.05772977819765,
132.806695808827));
#229491=CARTESIAN_POINT('Ctrl Pts',(-6.89067463871677,-3.89097563987157,
132.798192330299));
#229492=CARTESIAN_POINT('Ctrl Pts',(-7.06894195865911,-3.55649584051316,
132.781862440196));
#229493=CARTESIAN_POINT('Ctrl Pts',(-7.15070641823623,-3.38910122292492,
132.774027862526));
#229494=CARTESIAN_POINT('Ctrl Pts',(-7.24726399696753,-3.17233227011671,
132.764313071881));
#229495=CARTESIAN_POINT('Ctrl Pts',(-7.26758592360581,-3.12549555249587,
132.762238864005));
#229496=CARTESIAN_POINT('Ctrl Pts',(-7.2926000190712,-3.06628128004778,
132.759647391238));
#229497=CARTESIAN_POINT('Ctrl Pts',(-7.29771619536364,-3.05408484832029,
132.75911526137));
#229498=CARTESIAN_POINT('Ctrl Pts',(-7.30580459412044,-3.03466657468794,
132.758270638272));
#229499=CARTESIAN_POINT('Ctrl Pts',(-7.3087967393643,-3.02745308966572,
132.757957446682));
#229500=CARTESIAN_POINT('Ctrl Pts',(-7.31440893042893,-3.01386636745109,
132.757368611941));
#229501=CARTESIAN_POINT('Ctrl Pts',(-7.31703133887523,-3.00749411780485,
132.757092886149));
#229502=CARTESIAN_POINT('Ctrl Pts',(-7.32290257600748,-2.99317433174094,
132.756474260389));
#229503=CARTESIAN_POINT('Ctrl Pts',(-7.32614680117663,-2.98522491047493,
132.756131521948));
#229504=CARTESIAN_POINT('Ctrl Pts',(-7.33435331598121,-2.96502229344952,
132.755262216481));
#229505=CARTESIAN_POINT('Ctrl Pts',(-7.33929785405295,-2.95276188949425,
132.754736271418));
#229506=CARTESIAN_POINT('Ctrl Pts',(-7.36632075766717,-2.88526906219566,
132.751849792611));
#229507=CARTESIAN_POINT('Ctrl Pts',(-7.38780667218553,-2.82980067198163,
132.749510017625));
#229508=CARTESIAN_POINT('Ctrl Pts',(-7.74144172349002,-1.88536139352956,
132.710205925155));
#229509=CARTESIAN_POINT('Ctrl Pts',(-7.91156124447503,-0.944180572107552,
132.6802555473));
#229510=CARTESIAN_POINT('Ctrl Pts',(-7.91079403691426,0.349697463186542,
132.635479842313));
#229511=CARTESIAN_POINT('Ctrl Pts',(-7.88802041595599,0.69428979537607,
132.623065240056));
#229512=CARTESIAN_POINT('Ctrl Pts',(-7.8399067843408,1.05843422534096,132.608464906672));
#229513=CARTESIAN_POINT('Ctrl Pts',(-7.83688259007172,1.08059828160568,
132.607570325048));
#229514=CARTESIAN_POINT('Ctrl Pts',(-7.83280230077181,1.10958404852886,
132.606392331632));
#229515=CARTESIAN_POINT('Ctrl Pts',(-7.8318311968387,1.11641781934443,132.606114016469));
#229516=CARTESIAN_POINT('Ctrl Pts',(-7.83032011123745,1.12695250296761,
132.605684058254));
#229517=CARTESIAN_POINT('Ctrl Pts',(-7.8297864445307,1.13065433326774,132.605532798433));
#229518=CARTESIAN_POINT('Ctrl Pts',(-7.82871960159197,1.13801761417929,
132.605231578536));
#229519=CARTESIAN_POINT('Ctrl Pts',(-7.82818648131557,1.14167907232754,
132.605081621898));
#229520=CARTESIAN_POINT('Ctrl Pts',(-7.82700032130464,1.14978570017987,
132.604749227264));
#229521=CARTESIAN_POINT('Ctrl Pts',(-7.82634606344601,1.15423068804853,
132.60456671424));
#229522=CARTESIAN_POINT('Ctrl Pts',(-7.82442888579746,1.16717929963073,
132.604034288818));
#229523=CARTESIAN_POINT('Ctrl Pts',(-7.82315589737849,1.17568138137508,
132.603683756536));
#229524=CARTESIAN_POINT('Ctrl Pts',(-7.81384825565771,1.23716111636876,
132.601142298232));
#229525=CARTESIAN_POINT('Ctrl Pts',(-7.80528957724058,1.29005679416012,
132.598919640146));
#229526=CARTESIAN_POINT('Ctrl Pts',(-7.77629181563464,1.45840804539193,
132.591740579816));
#229527=CARTESIAN_POINT('Ctrl Pts',(-7.75382367888209,1.57349431919397,
132.586675066249));
#229528=CARTESIAN_POINT('Ctrl Pts',(-7.68718367562894,1.87861135635095,
132.572908619207));
#229529=CARTESIAN_POINT('Ctrl Pts',(-7.63852693029445,2.06757660174795,
132.564032356975));
#229530=CARTESIAN_POINT('Ctrl Pts',(-7.4032556108462,2.85888983844256,132.525931213477));
#229531=CARTESIAN_POINT('Ctrl Pts',(-7.15193399510597,3.43968874569621,
132.495888226658));
#229532=CARTESIAN_POINT('Ctrl Pts',(-6.68726901109647,4.23669451729892,
132.455320214001));
#229533=CARTESIAN_POINT('Ctrl Pts',(-6.52637555043864,4.48057979793452,
132.442964007059));
#229534=CARTESIAN_POINT('Ctrl Pts',(-6.33897517602841,4.733055937788,132.430249526307));
#229535=CARTESIAN_POINT('Ctrl Pts',(-6.32552082676708,4.75102210838096,
132.429345124625));
#229536=CARTESIAN_POINT('Ctrl Pts',(-6.3067318518487,4.7758905384318,132.428093721272));
#229537=CARTESIAN_POINT('Ctrl Pts',(-6.30146206687178,4.78284150967167,
132.427743990978));
#229538=CARTESIAN_POINT('Ctrl Pts',(-6.29237171337033,4.79479079837239,
132.427142856981));
#229539=CARTESIAN_POINT('Ctrl Pts',(-6.28855666442385,4.79979329325549,
132.426891220509));
#229540=CARTESIAN_POINT('Ctrl Pts',(-6.28067634582337,4.81010086266624,
132.426372775902));
#229541=CARTESIAN_POINT('Ctrl Pts',(-6.27661031155478,4.8154053481719,132.426106000436));
#229542=CARTESIAN_POINT('Ctrl Pts',(-6.2671414787767,4.82772587246902,132.42548643089));
#229543=CARTESIAN_POINT('Ctrl Pts',(-6.26173360756573,4.83473801185716,
132.425133852276));
#229544=CARTESIAN_POINT('Ctrl Pts',(-6.24451420314792,4.85698827238664,
132.424015217613));
#229545=CARTESIAN_POINT('Ctrl Pts',(-6.2326586894807,4.87219235858723,132.423251031534));
#229546=CARTESIAN_POINT('Ctrl Pts',(-6.03266174936424,5.12675356772148,
132.41045918577));
#229547=CARTESIAN_POINT('Ctrl Pts',(-5.83090562105139,5.35510718071116,
132.39904283836));
#229548=CARTESIAN_POINT('Ctrl Pts',(-5.37409704208839,5.81562124434117,
132.375682576322));
#229549=CARTESIAN_POINT('Ctrl Pts',(-5.1160291526152,6.04389177312378,132.363892858781));
#229550=CARTESIAN_POINT('Ctrl Pts',(-4.72459843231501,6.34703584617935,
132.347059890264));
#229551=CARTESIAN_POINT('Ctrl Pts',(-4.60266736571015,6.43600397450812,
132.341945763408));
#229552=CARTESIAN_POINT('Ctrl Pts',(-4.32907020419059,6.62388319103574,
132.330604430325));
#229553=CARTESIAN_POINT('Ctrl Pts',(-4.17640482476983,6.72118419779869,
132.324362193736));
#229554=CARTESIAN_POINT('Ctrl Pts',(-3.78522390914374,6.95202548985871,
132.308258022734));
#229555=CARTESIAN_POINT('Ctrl Pts',(-3.54288907325115,7.07859378672325,
132.298185098513));
#229556=CARTESIAN_POINT('Ctrl Pts',(-3.27938054635856,7.19929589736811,
132.286617318392));
#229557=CARTESIAN_POINT('Ctrl Pts',(-3.26422227536739,7.20618145228941,
132.285949766988));
#229558=CARTESIAN_POINT('Ctrl Pts',(-3.24391566411867,7.21532839023156,
132.285052540998));
#229559=CARTESIAN_POINT('Ctrl Pts',(-3.23878659945979,7.21763215865377,
132.284825670729));
#229560=CARTESIAN_POINT('Ctrl Pts',(-3.23014665842847,7.22150180664221,
132.284443094412));
#229561=CARTESIAN_POINT('Ctrl Pts',(-3.22663708181063,7.22307060193075,
132.284287576152));
#229562=CARTESIAN_POINT('Ctrl Pts',(-3.21991977061475,7.22606739517272,
132.28398969833));
#229563=CARTESIAN_POINT('Ctrl Pts',(-3.21671222507537,7.22749581734567,
132.283847365915));
#229564=CARTESIAN_POINT('Ctrl Pts',(-3.20920875403746,7.23083136749603,
132.283514186062));
#229565=CARTESIAN_POINT('Ctrl Pts',(-3.20491208181411,7.23273680150267,
132.283323231333));
#229566=CARTESIAN_POINT('Ctrl Pts',(-3.19260203803161,7.23818278136748,
132.282775667751));
#229567=CARTESIAN_POINT('Ctrl Pts',(-3.18458450179376,7.24171383717131,
132.282418463611));
#229568=CARTESIAN_POINT('Ctrl Pts',(-3.13303703051839,7.26431403887533,
132.280118258212));
#229569=CARTESIAN_POINT('Ctrl Pts',(-3.08934271334617,7.28300356365285,
132.278151924914));
#229570=CARTESIAN_POINT('Ctrl Pts',(-2.95642056211746,7.33844743554331,
132.272126017307));
#229571=CARTESIAN_POINT('Ctrl Pts',(-2.86668841021329,7.37396294596851,
132.267998293921));
#229572=CARTESIAN_POINT('Ctrl Pts',(-2.60328017229208,7.47268404788839,
132.255754521818));
#229573=CARTESIAN_POINT('Ctrl Pts',(-2.42801615920669,7.53145441302817,
132.247450145728));
#229574=CARTESIAN_POINT('Ctrl Pts',(-1.74424682103745,7.73439030001617,
132.21485060008));
#229575=CARTESIAN_POINT('Ctrl Pts',(-1.22383344923151,7.83361095620723,
132.189715163654));
#229576=CARTESIAN_POINT('Ctrl Pts',(-0.226539098790644,7.921871171148,132.144098731499));
#229577=CARTESIAN_POINT('Ctrl Pts',(0.247145662952985,7.92126144670701,
132.123490759275));
#229578=CARTESIAN_POINT('Ctrl Pts',(0.750324467869314,7.8754039834075,132.102930204537));
#229579=CARTESIAN_POINT('Ctrl Pts',(0.782633188062952,7.8722588902326,132.101615536776));
#229580=CARTESIAN_POINT('Ctrl Pts',(0.826759997879149,7.867689022179,132.099827361748));
#229581=CARTESIAN_POINT('Ctrl Pts',(0.838595356555082,7.86643632615018,
132.099348477133));
#229582=CARTESIAN_POINT('Ctrl Pts',(0.857344604591703,7.86440904514893,
132.098590982286));
#229583=CARTESIAN_POINT('Ctrl Pts',(0.864260353740726,7.86365204225786,
132.098311822802));
#229584=CARTESIAN_POINT('Ctrl Pts',(0.877650463942954,7.86216847365358,
132.097771794848));
#229585=CARTESIAN_POINT('Ctrl Pts',(0.884124942638113,7.86144303108823,
132.097510891505));
#229586=CARTESIAN_POINT('Ctrl Pts',(0.899510131258267,7.8596999281053,132.096891419214));
#229587=CARTESIAN_POINT('Ctrl Pts',(0.908420029922871,7.85867511009371,
132.096533074161));
#229588=CARTESIAN_POINT('Ctrl Pts',(0.934776141358874,7.85559820419946,
132.095474253243));
#229589=CARTESIAN_POINT('Ctrl Pts',(0.952217334701166,7.85350315036705,
132.09477511933));
#229590=CARTESIAN_POINT('Ctrl Pts',(1.08984254290069,7.83650626623499,132.089270371984));
#229591=CARTESIAN_POINT('Ctrl Pts',(1.2096797759489,7.8189042478654,132.08454966325));
#229592=CARTESIAN_POINT('Ctrl Pts',(1.64560612518417,7.74461150401348,132.067605100019));
#229593=CARTESIAN_POINT('Ctrl Pts',(1.95857765065799,7.67144187293376,132.055893933596));
#229594=CARTESIAN_POINT('Ctrl Pts',(2.85140327374869,7.40448746549866,132.022850996708));
#229595=CARTESIAN_POINT('Ctrl Pts',(3.4142831269127,7.1623684162658,132.002577571574));
#229596=CARTESIAN_POINT('Ctrl Pts',(4.13398663289207,6.74850145176339,131.972108594253));
#229597=CARTESIAN_POINT('Ctrl Pts',(4.31962790377202,6.63120862147032,131.963739602068));
#229598=CARTESIAN_POINT('Ctrl Pts',(4.51651536554941,6.49502922704184,131.954188071791));
#229599=CARTESIAN_POINT('Ctrl Pts',(4.53281228473271,6.48366628462464,131.953392696322));
#229600=CARTESIAN_POINT('Ctrl Pts',(4.55639436143299,6.46709143708528,131.9522349934));
#229601=CARTESIAN_POINT('Ctrl Pts',(4.56371381295691,6.46192830857818,131.951874711739));
#229602=CARTESIAN_POINT('Ctrl Pts',(4.57658980688718,6.45281281580426,131.951239263243));
#229603=CARTESIAN_POINT('Ctrl Pts',(4.58215004508853,6.448865672371,131.95096431078));
#229604=CARTESIAN_POINT('Ctrl Pts',(4.59360954550264,6.4407084136673,131.950396521291));
#229605=CARTESIAN_POINT('Ctrl Pts',(4.59950813854067,6.43649737120558,131.950103646945));
#229606=CARTESIAN_POINT('Ctrl Pts',(4.61435866019226,6.42586465233883,131.94936476027));
#229607=CARTESIAN_POINT('Ctrl Pts',(4.62330296340256,6.41943238007525,131.948918328128));
#229608=CARTESIAN_POINT('Ctrl Pts',(4.65814253861303,6.39426700917826,131.94717396696));
#229609=CARTESIAN_POINT('Ctrl Pts',(4.68393746444788,6.37539585388859,131.945870720368));
#229610=CARTESIAN_POINT('Ctrl Pts',(4.85909023635991,6.24562011416577,131.936944023274));
#229611=CARTESIAN_POINT('Ctrl Pts',(5.00460634244275,6.12963618916547,131.929143226832));
#229612=CARTESIAN_POINT('Ctrl Pts',(5.45341490891541,5.74526914859836,131.90406991572));
#229613=CARTESIAN_POINT('Ctrl Pts',(5.74026290325166,5.45868436433307,131.886523642141));
#229614=CARTESIAN_POINT('Ctrl Pts',(6.49147055438085,4.58315901219154,131.837112421992));
#229615=CARTESIAN_POINT('Ctrl Pts',(6.89590685858335,3.94855326766262,131.80610909589));
#229616=CARTESIAN_POINT('Ctrl Pts',(7.23579345135852,3.19886572087348,131.772648042261));
#229617=CARTESIAN_POINT('Ctrl Pts',(7.26553740029913,3.13072119171093,131.769635568221));
#229618=CARTESIAN_POINT('Ctrl Pts',(7.30481613030589,3.03715625033907,131.765538700701));
#229619=CARTESIAN_POINT('Ctrl Pts',(7.31518706292799,3.01209147061176,131.764445017148));
#229620=CARTESIAN_POINT('Ctrl Pts',(7.33267435491359,2.96920461489199,131.762580144618));
#229621=CARTESIAN_POINT('Ctrl Pts',(7.33985514392959,2.95140910562158,131.7618082234));
#229622=CARTESIAN_POINT('Ctrl Pts',(7.35443249590867,2.91490111676169,131.760228454238));
#229623=CARTESIAN_POINT('Ctrl Pts',(7.36182256156905,2.89618618739312,131.759420686857));
#229624=CARTESIAN_POINT('Ctrl Pts',(7.37853063235474,2.85339676567689,131.757578496812));
#229625=CARTESIAN_POINT('Ctrl Pts',(7.38780236925084,2.82930442929286,131.756544626275));
#229626=CARTESIAN_POINT('Ctrl Pts',(7.41591676594756,2.75516946705602,131.753373492314));
#229627=CARTESIAN_POINT('Ctrl Pts',(7.43437017387719,2.70498067291312,131.751240901248));
#229628=CARTESIAN_POINT('Ctrl Pts',(7.47592236043535,2.58833073156207,131.746316203503));
#229629=CARTESIAN_POINT('Ctrl Pts',(7.49864622569285,2.52174067108512,131.74352871091));
#229630=CARTESIAN_POINT('Ctrl Pts',(7.57285617297698,2.29439766118438,131.734088138855));
#229631=CARTESIAN_POINT('Ctrl Pts',(7.62008521338192,2.13230250028844,131.727486273193));
#229632=CARTESIAN_POINT('Ctrl Pts',(7.74578638703014,1.64310860448985,131.707863231883));
#229633=CARTESIAN_POINT('Ctrl Pts',(7.80862585530429,1.31239342305064,131.695005132221));
#229634=CARTESIAN_POINT('Ctrl Pts',(7.88874083073698,0.669774016502942,
131.67008307852));
#229635=CARTESIAN_POINT('Ctrl Pts',(7.90898404229305,0.358870257901192,
131.658048801793));
#229636=CARTESIAN_POINT('Ctrl Pts',(7.91100561999111,0.022863898115329,
131.644609063699));
#229637=CARTESIAN_POINT('Ctrl Pts',(7.9110384389916,-0.00186825295649431,
131.643617217254));
#229638=CARTESIAN_POINT('Ctrl Pts',(7.910913695667,-0.0389672512191592,
131.642125210408));
#229639=CARTESIAN_POINT('Ctrl Pts',(7.91084311209925,-0.0513342124840412,
131.641627160103));
#229640=CARTESIAN_POINT('Ctrl Pts',(7.91066228089055,-0.0737908597183481,
131.640721552485));
#229641=CARTESIAN_POINT('Ctrl Pts',(7.91056172824003,-0.0838806072956481,
131.640314217099));
#229642=CARTESIAN_POINT('Ctrl Pts',(7.91031217804911,-0.104887841697685,
131.639465219423));
#229643=CARTESIAN_POINT('Ctrl Pts',(7.91015988163277,-0.115805266141546,
131.63902348495));
#229644=CARTESIAN_POINT('Ctrl Pts',(7.90968103930422,-0.145694520238988,
131.63781275561));
#229645=CARTESIAN_POINT('Ctrl Pts',(7.90930883850215,-0.164665508150562,
131.637042785688));
#229646=CARTESIAN_POINT('Ctrl Pts',(7.9083313712687,-0.206763492154223,
131.635330959316));
#229647=CARTESIAN_POINT('Ctrl Pts',(7.90769290117543,-0.229889522892169,
131.634388438799));
#229648=CARTESIAN_POINT('Ctrl Pts',(7.90544734029276,-0.300066117807757,
131.631522152174));
#229649=CARTESIAN_POINT('Ctrl Pts',(7.90352169791984,-0.347105228659188,
131.629592458698));
#229650=CARTESIAN_POINT('Ctrl Pts',(7.89473012600363,-0.523353701474114,
131.622333982576));
#229651=CARTESIAN_POINT('Ctrl Pts',(7.88511450197023,-0.652404277715379,
131.616962635147));
#229652=CARTESIAN_POINT('Ctrl Pts',(7.82961522751308,-1.21171291406717,
131.593509734169));
#229653=CARTESIAN_POINT('Ctrl Pts',(7.75164243637642,-1.63803824784402,
131.575222896025));
#229654=CARTESIAN_POINT('Ctrl Pts',(7.60537040176252,-2.18156141667359,
131.551801021626));
#229655=CARTESIAN_POINT('Ctrl Pts',(7.56844065687543,-2.30642056003329,
131.546409455486));
#229656=CARTESIAN_POINT('Ctrl Pts',(7.4751336948425,-2.59546011176246,131.533902623202));
#229657=CARTESIAN_POINT('Ctrl Pts',(7.41640084691425,-2.75881081020412,
131.526815085619));
#229658=CARTESIAN_POINT('Ctrl Pts',(7.33517263694406,-2.96333040274327,
131.51790203419));
#229659=CARTESIAN_POINT('Ctrl Pts',(7.317621882762,-3.00640893796247,131.516022327462));
#229660=CARTESIAN_POINT('Ctrl Pts',(7.28917046476299,-3.07451785698646,
131.51304612913));
#229661=CARTESIAN_POINT('Ctrl Pts',(7.27851846164613,-3.09965080727473,
131.511946939756));
#229662=CARTESIAN_POINT('Ctrl Pts',(7.25828736265001,-3.14670587568004,
131.509887057419));
#229663=CARTESIAN_POINT('Ctrl Pts',(7.24873849711079,-3.16864064094754,
131.508926049696));
#229664=CARTESIAN_POINT('Ctrl Pts',(7.22712193644164,-3.21768708336256,
131.506775303689));
#229665=CARTESIAN_POINT('Ctrl Pts',(7.21500087931375,-3.24477487196806,
131.505586150802));
#229666=CARTESIAN_POINT('Ctrl Pts',(7.17910225894761,-3.32380429619657,
131.502112507688));
#229667=CARTESIAN_POINT('Ctrl Pts',(7.15491410946176,-3.37555749187765,
131.499832363477));
#229668=CARTESIAN_POINT('Ctrl Pts',(7.09718637547597,-3.49566343932966,
131.494525656358));
#229669=CARTESIAN_POINT('Ctrl Pts',(7.06321631101485,-3.56380313401105,
131.491503479813));
#229670=CARTESIAN_POINT('Ctrl Pts',(6.94248366995176,-3.79746824550364,
131.481089900985));
#229671=CARTESIAN_POINT('Ctrl Pts',(6.85084169358579,-3.96040583485297,
131.47373081443));
#229672=CARTESIAN_POINT('Ctrl Pts',(6.2677679034555,-4.91619466639724,131.429982353456));
#229673=CARTESIAN_POINT('Ctrl Pts',(5.64508723852377,-5.62019479616323,
131.396777274658));
#229674=CARTESIAN_POINT('Ctrl Pts',(4.89693951136714,-6.21324342706174,
131.360168149402));
#229675=CARTESIAN_POINT('Ctrl Pts',(4.87954456824737,-6.22691378302315,
131.359317751109));
#229676=CARTESIAN_POINT('Ctrl Pts',(4.84028492855138,-6.25750166349224,
131.357399750589));
#229677=CARTESIAN_POINT('Ctrl Pts',(4.81838847758797,-6.27437787527741,
131.356330923647));
#229678=CARTESIAN_POINT('Ctrl Pts',(4.71688998157077,-6.35176097156591,
131.351378805897));
#229679=CARTESIAN_POINT('Ctrl Pts',(4.63623539545467,-6.41086881593325,
131.347450287076));
#229680=CARTESIAN_POINT('Ctrl Pts',(4.54164443685752,-6.47747121965408,
131.342827264503));
#229681=CARTESIAN_POINT('Ctrl Pts',(4.52877783052257,-6.48647353727907,
131.342198091247));
#229682=CARTESIAN_POINT('Ctrl Pts',(4.50944011063742,-6.49991788362271,
131.341251862765));
#229683=CARTESIAN_POINT('Ctrl Pts',(4.50298900946952,-6.50438871726726,
131.340936096072));
#229684=CARTESIAN_POINT('Ctrl Pts',(4.49151488482207,-6.51231542642754,
131.34037426288));
#229685=CARTESIAN_POINT('Ctrl Pts',(4.48649449395881,-6.51577511346732,
131.340128370093));
#229686=CARTESIAN_POINT('Ctrl Pts',(4.47594576456272,-6.52302655618528,
131.339611552756));
#229687=CARTESIAN_POINT('Ctrl Pts',(4.47041659772165,-6.52681709430147,
131.339340572405));
#229688=CARTESIAN_POINT('Ctrl Pts',(4.45921723363772,-6.53447394690843,
131.338791508869));
#229689=CARTESIAN_POINT('Ctrl Pts',(4.45354681055171,-6.53833991969169,
131.33851341008));
#229690=CARTESIAN_POINT('Ctrl Pts',(4.43005013245647,-6.55431470277271,
131.337360607571));
#229691=CARTESIAN_POINT('Ctrl Pts',(4.41217957483781,-6.56635795444614,
131.336482795221));
#229692=CARTESIAN_POINT('Ctrl Pts',(4.36951433603597,-6.59485792588513,
131.334384070834));
#229693=CARTESIAN_POINT('Ctrl Pts',(4.34467568579787,-6.61124797185816,
131.333159863127));
#229694=CARTESIAN_POINT('Ctrl Pts',(4.25661271117346,-6.66864665671793,
131.32880914566));
#229695=CARTESIAN_POINT('Ctrl Pts',(4.19289993568851,-6.7088888044265,131.325640303226));
#229696=CARTESIAN_POINT('Ctrl Pts',(4.03027579555711,-6.80838386128025,
131.317508945766));
#229697=CARTESIAN_POINT('Ctrl Pts',(3.93062737874045,-6.86639500934533,
131.312488969125));
#229698=CARTESIAN_POINT('Ctrl Pts',(3.53662037802923,-7.0843816600019,131.29258696103));
#229699=CARTESIAN_POINT('Ctrl Pts',(3.23349542915775,-7.22776855108928,
131.277172752162));
#229700=CARTESIAN_POINT('Ctrl Pts',(2.67834396708993,-7.44844018590403,
131.24964654932));
#229701=CARTESIAN_POINT('Ctrl Pts',(2.42980142330698,-7.53318382762938,
131.237557371073));
#229702=CARTESIAN_POINT('Ctrl Pts',(1.71404280037865,-7.73811223118917,
131.203853927677));
#229703=CARTESIAN_POINT('Ctrl Pts',(1.23938359919552,-7.82817675642457,
131.182867223469));
#229704=CARTESIAN_POINT('Ctrl Pts',(0.727460526266421,-7.87754742711526,
131.161929216356));
#229705=CARTESIAN_POINT('Ctrl Pts',(0.695476526050218,-7.8804355663749,
131.16062764941));
#229706=CARTESIAN_POINT('Ctrl Pts',(0.651402085719223,-7.88414504716499,
131.158843038747));
#229707=CARTESIAN_POINT('Ctrl Pts',(0.639326232371146,-7.88513346572133,
131.158355003629));
#229708=CARTESIAN_POINT('Ctrl Pts',(0.620090460192549,-7.88666345024435,
131.157579072929));
#229709=CARTESIAN_POINT('Ctrl Pts',(0.612932014899007,-7.88722301584542,
131.157290639534));
#229710=CARTESIAN_POINT('Ctrl Pts',(0.599004739605401,-7.88829261620159,
131.156730097936));
#229711=CARTESIAN_POINT('Ctrl Pts',(0.592235995971775,-7.88880368638161,
131.156457958983));
#229712=CARTESIAN_POINT('Ctrl Pts',(0.576046652408271,-7.89000510001128,
131.155807748297));
#229713=CARTESIAN_POINT('Ctrl Pts',(0.566625448200215,-7.89068728477801,
131.155429920772));
#229714=CARTESIAN_POINT('Ctrl Pts',(0.538383010215264,-7.89268146406173,
131.154298942482));
#229715=CARTESIAN_POINT('Ctrl Pts',(0.519558223772725,-7.89394300821675,
131.153547300121));
#229716=CARTESIAN_POINT('Ctrl Pts',(0.355731484426099,-7.904333303052,131.147024913684));
#229717=CARTESIAN_POINT('Ctrl Pts',(0.210504213934108,-7.90953351565325,
131.141372785188));
#229718=CARTESIAN_POINT('Ctrl Pts',(-0.31897172246396,-7.91389819751642,
131.121178961891));
#229719=CARTESIAN_POINT('Ctrl Pts',(-0.702890991865361,-7.88907481284543,
131.10735565344));
#229720=CARTESIAN_POINT('Ctrl Pts',(-1.38764628191403,-7.7943973045146,
131.083146187415));
#229721=CARTESIAN_POINT('Ctrl Pts',(-1.68908339619839,-7.73467446966547,
131.072638801583));
#229722=CARTESIAN_POINT('Ctrl Pts',(-2.11774384123277,-7.62348519771749,
131.057266002313));
#229723=CARTESIAN_POINT('Ctrl Pts',(-2.24830252227199,-7.58600687782166,
131.052522953512));
#229724=CARTESIAN_POINT('Ctrl Pts',(-2.59016459989613,-7.47827066918614,
131.039821436862));
#229725=CARTESIAN_POINT('Ctrl Pts',(-2.79957066622585,-7.40242391479314,
131.03175211285));
#229726=CARTESIAN_POINT('Ctrl Pts',(-3.11860071292908,-7.27139622176705,
131.018671875407));
#229727=CARTESIAN_POINT('Ctrl Pts',(-3.23061831025314,-7.22232502982957,
131.013921305264));
#229728=CARTESIAN_POINT('Ctrl Pts',(-3.35308793643955,-7.16525554224267,
131.00851748926));
#229729=CARTESIAN_POINT('Ctrl Pts',(-3.36470707218285,-7.15980670204315,
131.008002786386));
#229730=CARTESIAN_POINT('Ctrl Pts',(-3.38223554820827,-7.15153456170686,
131.007223311176));
#229731=CARTESIAN_POINT('Ctrl Pts',(-3.388154764195,-7.14873213824349,131.006959570978));
#229732=CARTESIAN_POINT('Ctrl Pts',(-3.39842135530475,-7.14385585607813,
131.006501235615));
#229733=CARTESIAN_POINT('Ctrl Pts',(-3.40277033442436,-7.14178536863234,
131.006306804637));
#229734=CARTESIAN_POINT('Ctrl Pts',(-3.41181567168698,-7.13746887368505,
131.005901838137));
#229735=CARTESIAN_POINT('Ctrl Pts',(-3.41651170892208,-7.13522219997365,
131.005691270577));
#229736=CARTESIAN_POINT('Ctrl Pts',(-3.42756238649814,-7.12992193453942,
131.005195011086));
#229737=CARTESIAN_POINT('Ctrl Pts',(-3.43391516303344,-7.12686448296829,
131.004909135728));
#229738=CARTESIAN_POINT('Ctrl Pts',(-3.44727899788268,-7.12041074661861,
131.0043065383));
#229739=CARTESIAN_POINT('Ctrl Pts',(-3.45428914101289,-7.11701259093155,
131.003989728918));
#229740=CARTESIAN_POINT('Ctrl Pts',(-3.50648886076114,-7.09161356862683,
131.001625432121));
#229741=CARTESIAN_POINT('Ctrl Pts',(-3.5514722307191,-7.06919316327819,
130.999558731628));
#229742=CARTESIAN_POINT('Ctrl Pts',(-3.68354154049401,-7.00178905092022,
130.993410785228));
#229743=CARTESIAN_POINT('Ctrl Pts',(-3.77000729171713,-6.95561444443585,
130.989281923224));
#229744=CARTESIAN_POINT('Ctrl Pts',(-4.08237750706112,-6.78126609055553,
130.974039262031));
#229745=CARTESIAN_POINT('Ctrl Pts',(-4.30278790584083,-6.64359731019736,
130.962655395159));
#229746=CARTESIAN_POINT('Ctrl Pts',(-4.71324885921859,-6.35821583549561,
130.940654172516));
#229747=CARTESIAN_POINT('Ctrl Pts',(-4.90413092883447,-6.2121756077295,
130.930054152948));
#229748=CARTESIAN_POINT('Ctrl Pts',(-5.46153231658274,-5.74399289965348,
130.898286643073));
#229749=CARTESIAN_POINT('Ctrl Pts',(-5.80520533106435,-5.39642930886564,
130.877632599852));
#229750=CARTESIAN_POINT('Ctrl Pts',(-6.13907950793423,-4.9896994243265,
130.856316269144));
#229751=CARTESIAN_POINT('Ctrl Pts',(-6.16324351830985,-4.95982125840603,
130.854764859031));
#229752=CARTESIAN_POINT('Ctrl Pts',(-6.19685941828311,-4.91763105303388,
130.8525938834));
#229753=CARTESIAN_POINT('Ctrl Pts',(-6.20649411136275,-4.90546559170052,
130.851970165368));
#229754=CARTESIAN_POINT('Ctrl Pts',(-6.22410847384288,-4.88308945597198,
130.85082707706));
#229755=CARTESIAN_POINT('Ctrl Pts',(-6.23209896415351,-4.8728873813514,
130.850307466962));
#229756=CARTESIAN_POINT('Ctrl Pts',(-6.24825321342879,-4.8521572795058,
130.849254781945));
#229757=CARTESIAN_POINT('Ctrl Pts',(-6.25641551858542,-4.84162817079275,
130.848721739929));
#229758=CARTESIAN_POINT('Ctrl Pts',(-6.27274840236682,-4.82044901023082,
130.847652768087));
#229759=CARTESIAN_POINT('Ctrl Pts',(-6.28091854977015,-4.80979868102738,
130.847116848675));
#229760=CARTESIAN_POINT('Ctrl Pts',(-6.30041873004687,-4.78424448769462,
130.845834833276));
#229761=CARTESIAN_POINT('Ctrl Pts',(-6.31172305385114,-4.769321082365,130.845089277373));
#229762=CARTESIAN_POINT('Ctrl Pts',(-6.3842234420301,-4.67290046656368,
130.840291995193));
#229763=CARTESIAN_POINT('Ctrl Pts',(-6.44389362357367,-4.59026614137918,
130.836271200349));
#229764=CARTESIAN_POINT('Ctrl Pts',(-6.67740422913668,-4.25335851368372,
130.820228282927));
#229765=CARTESIAN_POINT('Ctrl Pts',(-6.83792819962555,-3.99017991628767,
130.808492775632));
#229766=CARTESIAN_POINT('Ctrl Pts',(-7.0294306256028,-3.63055226294356,
130.793249472181));
#229767=CARTESIAN_POINT('Ctrl Pts',(-7.07450010450672,-3.54192789263511,
130.78955221141));
#229768=CARTESIAN_POINT('Ctrl Pts',(-7.16640534116194,-3.35244911203576,
130.781752297394));
#229769=CARTESIAN_POINT('Ctrl Pts',(-7.21280939127133,-3.25140914994615,
130.777654321761));
#229770=CARTESIAN_POINT('Ctrl Pts',(-7.45709445231892,-2.68851471465759,
130.755075806522));
#229771=CARTESIAN_POINT('Ctrl Pts',(-7.61274357434249,-2.20962509032041,
130.736853953726));
#229772=CARTESIAN_POINT('Ctrl Pts',(-7.73822630616955,-1.64602622079661,
130.71425593118));
#229773=CARTESIAN_POINT('Ctrl Pts',(-7.7534868193402,-1.5725744502583,130.711287581794));
#229774=CARTESIAN_POINT('Ctrl Pts',(-7.77012955626127,-1.48632839059519,
130.707765944901));
#229775=CARTESIAN_POINT('Ctrl Pts',(-7.77252836955353,-1.4737327260642,
130.707250730951));
#229776=CARTESIAN_POINT('Ctrl Pts',(-7.77631643710953,-1.45357585672041,
130.70642472723));
#229777=CARTESIAN_POINT('Ctrl Pts',(-7.77772531533506,-1.44601833320615,
130.706114690963));
#229778=CARTESIAN_POINT('Ctrl Pts',(-7.78019852367665,-1.43264332898656,
130.705565387729));
#229779=CARTESIAN_POINT('Ctrl Pts',(-7.78126735200993,-1.42682667910636,
130.705326296364));
#229780=CARTESIAN_POINT('Ctrl Pts',(-7.78346957776464,-1.41476591900512,
130.704830109819));
#229781=CARTESIAN_POINT('Ctrl Pts',(-7.78460198593676,-1.40852163412866,
130.704572975809));
#229782=CARTESIAN_POINT('Ctrl Pts',(-7.78687076068286,-1.39592492673905,
130.704053759958));
#229783=CARTESIAN_POINT('Ctrl Pts',(-7.78800687040367,-1.38957246334485,
130.703791668081));
#229784=CARTESIAN_POINT('Ctrl Pts',(-7.79075785756785,-1.37408119500227,
130.703151893961));
#229785=CARTESIAN_POINT('Ctrl Pts',(-7.79236442671566,-1.36494093863996,
130.702773875558));
#229786=CARTESIAN_POINT('Ctrl Pts',(-7.79669698786827,-1.34003472941215,
130.701742318702));
#229787=CARTESIAN_POINT('Ctrl Pts',(-7.79939123011584,-1.32426335409457,
130.701087471629));
#229788=CARTESIAN_POINT('Ctrl Pts',(-7.87423464476727,-0.877997953164491,
130.682509602445));
#229789=CARTESIAN_POINT('Ctrl Pts',(-7.91066124806279,-0.442382604334897,
130.662818762618));
#229790=CARTESIAN_POINT('Ctrl Pts',(-7.91099764832253,-0.00609985535713557,
130.642792890452));
#229791=CARTESIAN_POINT('',(-7.91099997694602,-0.000603953663847722,128.642331508237));
#229792=CARTESIAN_POINT('Ctrl Pts',(-7.91099763196637,-0.00612103116663704,
130.642331508237));
#229793=CARTESIAN_POINT('Ctrl Pts',(-7.91114782317046,0.18799042285764,
130.634504138835));
#229794=CARTESIAN_POINT('Ctrl Pts',(-7.90414951540968,0.382321771707403,
130.626676769434));
#229795=CARTESIAN_POINT('Ctrl Pts',(-7.88998090783303,0.576300506706553,
130.618849400032));
#229796=CARTESIAN_POINT('Ctrl Pts',(-7.87582335202878,0.770127934753637,
130.611028136121));
#229797=CARTESIAN_POINT('Ctrl Pts',(-7.85450666116262,0.963602947557249,
130.60320687221));
#229798=CARTESIAN_POINT('Ctrl Pts',(-7.82606108445803,1.15615262934077,
130.5953856083));
#229799=CARTESIAN_POINT('Ctrl Pts',(-7.79763215742691,1.34858960856388,
130.587568922306));
#229800=CARTESIAN_POINT('Ctrl Pts',(-7.7620827075776,1.54010198851846,130.579752236312));
#229801=CARTESIAN_POINT('Ctrl Pts',(-7.71949486697746,1.73012138265169,
130.571935550318));
#229802=CARTESIAN_POINT('Ctrl Pts',(-7.67692366416245,1.92006654193748,
130.564121918068));
#229803=CARTESIAN_POINT('Ctrl Pts',(-7.62731962579182,2.10851953455246,
130.556308285818));
#229804=CARTESIAN_POINT('Ctrl Pts',(-7.57081612274288,2.29492140074916,
130.548494653568));
#229805=CARTESIAN_POINT('Ctrl Pts',(-7.51431398949648,2.48131874804463,
130.540681210742));
#229806=CARTESIAN_POINT('Ctrl Pts',(-7.45091281772856,2.66566472846678,
130.532867767916));
#229807=CARTESIAN_POINT('Ctrl Pts',(-7.38079620123127,2.84741434215151,
130.52505432509));
#229808=CARTESIAN_POINT('Ctrl Pts',(-7.31067703841428,3.02917055616359,
130.517240598515));
#229809=CARTESIAN_POINT('Ctrl Pts',(-7.23384207105125,3.20832988672088,
130.50942687194));
#229810=CARTESIAN_POINT('Ctrl Pts',(-7.15052350236325,3.38436620981696,
130.501613145365));
#229811=CARTESIAN_POINT('Ctrl Pts',(-7.0671872167759,3.56043996535899,130.493797757275));
#229812=CARTESIAN_POINT('Ctrl Pts',(-6.97736473405849,3.73338907226283,
130.485982369186));
#229813=CARTESIAN_POINT('Ctrl Pts',(-6.88133484139416,3.90271082718343,
130.478166981096));
#229814=CARTESIAN_POINT('Ctrl Pts',(-6.78526759506394,4.07209844480666,
130.47034855298));
#229815=CARTESIAN_POINT('Ctrl Pts',(-6.6829883026622,4.23785559386953,130.462530124865));
#229816=CARTESIAN_POINT('Ctrl Pts',(-6.57481987435693,4.39950731557082,
130.454711696749));
#229817=CARTESIAN_POINT('Ctrl Pts',(-6.46653145304692,4.56133836016801,
130.446884595523));
#229818=CARTESIAN_POINT('Ctrl Pts',(-6.35234104332711,4.71905458844504,
130.439057494297));
#229819=CARTESIAN_POINT('Ctrl Pts',(-6.23261341089965,4.87221213313561,
130.431230393072));
#229820=CARTESIAN_POINT('Ctrl Pts',(-6.11281218343387,5.02546382180232,
130.423398480627));
#229821=CARTESIAN_POINT('Ctrl Pts',(-5.98746717643063,5.17415097421666,
130.415566568183));
#229822=CARTESIAN_POINT('Ctrl Pts',(-5.85698107581138,5.31786551894531,
130.407734655738));
#229823=CARTESIAN_POINT('Ctrl Pts',(-5.72631141641576,5.46178223130598,
130.399891725904));
#229824=CARTESIAN_POINT('Ctrl Pts',(-5.59048646306852,5.60071211292389,
130.392048796069));
#229825=CARTESIAN_POINT('Ctrl Pts',(-5.44994399259742,5.73428561178734,
130.384205866235));
#229826=CARTESIAN_POINT('Ctrl Pts',(-5.36622686938654,5.81385151826796,
130.379534057627));
#229827=CARTESIAN_POINT('Ctrl Pts',(-5.28083647453102,5.89151763492538,
130.37486224902));
#229828=CARTESIAN_POINT('Ctrl Pts',(-5.19387032345218,5.96721309014206,
130.370190440412));
#229829=CARTESIAN_POINT('Ctrl Pts',(-5.04941193573323,6.09294986568753,
130.362430157465));
#229830=CARTESIAN_POINT('Ctrl Pts',(-4.90013023472339,6.21365931778303,
130.354669874518));
#229831=CARTESIAN_POINT('Ctrl Pts',(-4.74641559371106,6.32893830051901,
130.346909591571));
#229832=CARTESIAN_POINT('Ctrl Pts',(-4.59288595595854,6.44407853923261,
130.339158648512));
#229833=CARTESIAN_POINT('Ctrl Pts',(-4.43493428100679,6.55380110512324,
130.331407705454));
#229834=CARTESIAN_POINT('Ctrl Pts',(-4.27298750711932,6.65773976391405,
130.323656762396));
#229835=CARTESIAN_POINT('Ctrl Pts',(-4.11120277393074,6.76157442376429,
130.315913574776));
#229836=CARTESIAN_POINT('Ctrl Pts',(-3.94543119870691,6.85963650494034,
130.308170387156));
#229837=CARTESIAN_POINT('Ctrl Pts',(-3.77613257696021,6.9516000863988,130.300427199536));
#229838=CARTESIAN_POINT('Ctrl Pts',(-3.60696903974555,7.04349028948455,
130.292690190258));
#229839=CARTESIAN_POINT('Ctrl Pts',(-3.43428437265227,7.1292915105122,130.284953180981));
#229840=CARTESIAN_POINT('Ctrl Pts',(-3.25856720076424,7.20872116246034,
130.277216171703));
#229841=CARTESIAN_POINT('Ctrl Pts',(-3.08295465862199,7.28810351849424,
130.269483769382));
#229842=CARTESIAN_POINT('Ctrl Pts',(-2.90431353333025,7.36112171272404,
130.261751367061));
#229843=CARTESIAN_POINT('Ctrl Pts',(-2.72315697160088,7.42753910174975,
130.25401896474));
#229844=CARTESIAN_POINT('Ctrl Pts',(-2.54207162691524,7.49393038048692,
130.246289602214));
#229845=CARTESIAN_POINT('Ctrl Pts',(-2.35847315188261,7.55372589889675,
130.238560239688));
#229846=CARTESIAN_POINT('Ctrl Pts',(-2.17289466916262,7.60673712946127,
130.230830877161));
#229847=CARTESIAN_POINT('Ctrl Pts',(-1.98731625884801,7.65974833934291,
130.223101517651));
#229848=CARTESIAN_POINT('Ctrl Pts',(-1.79975818442748,7.70597515703875,
130.215372158141));
#229849=CARTESIAN_POINT('Ctrl Pts',(-1.61076912072071,7.74527880968353,
130.20764279863));
#229850=CARTESIAN_POINT('Ctrl Pts',(-1.42177058420322,7.78458443236855,
130.199913051696));
#229851=CARTESIAN_POINT('Ctrl Pts',(-1.23134126718937,7.8169661248216,130.192183304763));
#229852=CARTESIAN_POINT('Ctrl Pts',(-1.04004026967997,7.84233621043143,
130.184453557829));
#229853=CARTESIAN_POINT('Ctrl Pts',(-0.84869463012058,7.86771221641097,
130.17672200708));
#229854=CARTESIAN_POINT('Ctrl Pts',(-0.656477261096092,7.88607330984533,
130.16899045633));
#229855=CARTESIAN_POINT('Ctrl Pts',(-0.463952669895659,7.89738367562933,
130.161258905581));
#229856=CARTESIAN_POINT('Ctrl Pts',(-0.271347862168685,7.90869875394513,
130.153524133434));
#229857=CARTESIAN_POINT('Ctrl Pts',(-0.0784359355669855,7.91295723374037,
130.145789361288));
#229858=CARTESIAN_POINT('Ctrl Pts',(0.11421826373655,7.91017542082532,130.138054589142));
#229859=CARTESIAN_POINT('Ctrl Pts',(0.30710220327139,7.90739029059694,130.130310593275));
#229860=CARTESIAN_POINT('Ctrl Pts',(0.499727442556436,7.89754810592534,
130.122566597409));
#229861=CARTESIAN_POINT('Ctrl Pts',(0.691532870580185,7.8807171811268,130.114822601543));
#229862=CARTESIAN_POINT('Ctrl Pts',(0.883462789948739,7.86387533221373,
130.107073579435));
#229863=CARTESIAN_POINT('Ctrl Pts',(1.07457148325651,7.84003575197567,130.099324557327));
#229864=CARTESIAN_POINT('Ctrl Pts',(1.26430782929928,7.80931794158572,130.091575535219));
#229865=CARTESIAN_POINT('Ctrl Pts',(1.45433413717369,7.7785531871455,130.08381467078));
#229866=CARTESIAN_POINT('Ctrl Pts',(1.6429835585206,7.74088927881033,130.076053806341));
#229867=CARTESIAN_POINT('Ctrl Pts',(1.82971875817401,7.69649597323263,130.068292941902));
#229868=CARTESIAN_POINT('Ctrl Pts',(1.9581349004912,7.66596709031406,130.062955864189));
#229869=CARTESIAN_POINT('Ctrl Pts',(2.08564611180101,7.6322567852051,130.057618786476));
#229870=CARTESIAN_POINT('Ctrl Pts',(2.21208335260762,7.59543338073057,130.052281708762));
#229871=CARTESIAN_POINT('Ctrl Pts',(2.40193308980169,7.54014180984939,130.044267908439));
#229872=CARTESIAN_POINT('Ctrl Pts',(2.58994300467057,7.4776598214353,130.036254108116));
#229873=CARTESIAN_POINT('Ctrl Pts',(2.77553686750707,7.40812500549964,130.028240307793));
#229874=CARTESIAN_POINT('Ctrl Pts',(2.96091917524786,7.3386694510461,130.020235642257));
#229875=CARTESIAN_POINT('Ctrl Pts',(3.14389060797537,7.26217720475818,130.01223097672));
#229876=CARTESIAN_POINT('Ctrl Pts',(3.32388829368905,7.17883609027793,130.004226311184));
#229877=CARTESIAN_POINT('Ctrl Pts',(3.50371136086772,7.09557582630005,129.996229411097));
#229878=CARTESIAN_POINT('Ctrl Pts',(3.680566128368,7.00548007450622,129.98823251101));
#229879=CARTESIAN_POINT('Ctrl Pts',(3.85390758861673,6.90878551544353,129.980235610923));
#229880=CARTESIAN_POINT('Ctrl Pts',(4.02711029629211,6.81216835632244,129.972245112019));
#229881=CARTESIAN_POINT('Ctrl Pts',(4.19680501077975,6.70896307964677,129.964254613116));
#229882=CARTESIAN_POINT('Ctrl Pts',(4.36246894971703,6.59945343666843,129.956264114212));
#229883=CARTESIAN_POINT('Ctrl Pts',(4.52802837277728,6.49001288233095,129.948278656442));
#229884=CARTESIAN_POINT('Ctrl Pts',(4.68956181093357,6.37427607378451,129.940293198671));
#229885=CARTESIAN_POINT('Ctrl Pts',(4.84657288472726,6.25257165277028,129.932307740901));
#229886=CARTESIAN_POINT('Ctrl Pts',(5.00873197596496,6.12687683498176,129.924060459076));
#229887=CARTESIAN_POINT('Ctrl Pts',(5.16606679754621,5.99481661610349,129.915813177252));
#229888=CARTESIAN_POINT('Ctrl Pts',(5.31806385291161,5.85680099169802,129.907565895427));
#229889=CARTESIAN_POINT('Ctrl Pts',(5.46513583305697,5.72325741005749,129.899585845644));
#229890=CARTESIAN_POINT('Ctrl Pts',(5.6072102771621,5.58413855917991,129.891605795861));
#229891=CARTESIAN_POINT('Ctrl Pts',(5.74385632493325,5.43985620384623,129.883625746077));
#229892=CARTESIAN_POINT('Ctrl Pts',(5.88049152130627,5.29558530632861,129.875646330009));
#229893=CARTESIAN_POINT('Ctrl Pts',(6.01169895042716,5.14615196445618,129.867666913941));
#229894=CARTESIAN_POINT('Ctrl Pts',(6.13708532179537,4.99200408182965,129.859687497873));
#229895=CARTESIAN_POINT('Ctrl Pts',(6.26248100585716,4.83784475033526,129.851707489158));
#229896=CARTESIAN_POINT('Ctrl Pts',(6.38205455954969,4.67897043992738,129.843727480443));
#229897=CARTESIAN_POINT('Ctrl Pts',(6.49545339007537,4.51586162956289,129.835747471728));
#229898=CARTESIAN_POINT('Ctrl Pts',(6.60887807083673,4.35271563714662,129.827765643901));
#229899=CARTESIAN_POINT('Ctrl Pts',(6.71612503229753,4.18533349565868,129.819783816075));
#229900=CARTESIAN_POINT('Ctrl Pts',(6.81688516144929,4.01422442018537,129.811801988248));
#229901=CARTESIAN_POINT('Ctrl Pts',(6.91772021028737,3.84298811742116,129.803814225574));
#229902=CARTESIAN_POINT('Ctrl Pts',(7.01205862217755,3.66801963360344,129.7958264629));
#229903=CARTESIAN_POINT('Ctrl Pts',(7.09963689854132,3.48985342226155,129.787838700225));
#229904=CARTESIAN_POINT('Ctrl Pts',(7.18725374749185,3.31160874018547,129.779847419456));
#229905=CARTESIAN_POINT('Ctrl Pts',(7.26810438443607,3.13016382595912,129.771856138687));
#229906=CARTESIAN_POINT('Ctrl Pts',(7.34197335188398,2.94607336979675,129.763864857918));
#229907=CARTESIAN_POINT('Ctrl Pts',(7.41591182020932,2.76180970899007,129.755866058416));
#229908=CARTESIAN_POINT('Ctrl Pts',(7.48285538381998,2.57489584831195,129.747867258915));
#229909=CARTESIAN_POINT('Ctrl Pts',(7.54263804339973,2.38590283671803,129.739868459413));
#229910=CARTESIAN_POINT('Ctrl Pts',(7.55632903738414,2.34262101882939,129.738036631979));
#229911=CARTESIAN_POINT('Ctrl Pts',(7.56964467461467,2.29923020566681,129.736204804546));
#229912=CARTESIAN_POINT('Ctrl Pts',(7.58258333712301,2.25573733745409,129.734372977112));
#229913=CARTESIAN_POINT('Ctrl Pts',(7.63998395193699,2.06278714852815,129.72624632408));
#229914=CARTESIAN_POINT('Ctrl Pts',(7.69006241361648,1.86748726185573,129.718119671047));
#229915=CARTESIAN_POINT('Ctrl Pts',(7.73263321854928,1.67042045826439,129.709993018014));
#229916=CARTESIAN_POINT('Ctrl Pts',(7.77516778530392,1.47352140677331,129.701873282753));
#229917=CARTESIAN_POINT('Ctrl Pts',(7.81020736932014,1.27485874716274,129.693753547492));
#229918=CARTESIAN_POINT('Ctrl Pts',(7.83761650697373,1.07502952964691,129.685633812231));
#229919=CARTESIAN_POINT('Ctrl Pts',(7.8650057643388,0.875345251477647,129.677519966344));
#229920=CARTESIAN_POINT('Ctrl Pts',(7.88477556718692,0.674496417318688,
129.669406120458));
#229921=CARTESIAN_POINT('Ctrl Pts',(7.89684157865705,0.473089929710325,
129.661292274571));
#229922=CARTESIAN_POINT('Ctrl Pts',(7.90889901677679,0.27182654890996,129.653184193874));
#229923=CARTESIAN_POINT('Ctrl Pts',(7.91326356495437,0.0700066226631564,
129.645076113177));
#229924=CARTESIAN_POINT('Ctrl Pts',(7.90990271011032,-0.131757795175419,
129.63696803248));
#229925=CARTESIAN_POINT('Ctrl Pts',(7.90654329877035,-0.333435554179994,
129.628863434245));
#229926=CARTESIAN_POINT('Ctrl Pts',(7.89546510567637,-0.535057534099425,
129.62075883601));
#229927=CARTESIAN_POINT('Ctrl Pts',(7.8766877001253,-0.736010784360424,
129.612654237774));
#229928=CARTESIAN_POINT('Ctrl Pts',(7.85791616384324,-0.936901222499596,
129.604552172799));
#229929=CARTESIAN_POINT('Ctrl Pts',(7.83145024429911,-1.13712303074794,
129.596450107825));
#229930=CARTESIAN_POINT('Ctrl Pts',(7.79736148799388,-1.33606692405356,
129.58834804285));
#229931=CARTESIAN_POINT('Ctrl Pts',(7.77922832305013,-1.44189309147248,
129.584038232329));
#229932=CARTESIAN_POINT('Ctrl Pts',(7.75893907923601,-1.54735774143948,
129.579728421809));
#229933=CARTESIAN_POINT('Ctrl Pts',(7.73651047970317,-1.6523699941124,129.575418611288));
#229934=CARTESIAN_POINT('Ctrl Pts',(7.69337535876219,-1.85433161069477,
129.567129899468));
#229935=CARTESIAN_POINT('Ctrl Pts',(7.64234282627787,-2.05453237315838,
129.558841187648));
#229936=CARTESIAN_POINT('Ctrl Pts',(7.58358851097656,-2.25235572150234,
129.550552475828));
#229937=CARTESIAN_POINT('Ctrl Pts',(7.52480032438705,-2.45029311307207,
129.542258985647));
#229938=CARTESIAN_POINT('Ctrl Pts',(7.45828155278369,-2.64585007437836,
129.533965495466));
#229939=CARTESIAN_POINT('Ctrl Pts',(7.38425724951933,-2.83842665449034,
129.525672005284));
#229940=CARTESIAN_POINT('Ctrl Pts',(7.31018580901054,-3.03112586364343,
129.517373233969));
#229941=CARTESIAN_POINT('Ctrl Pts',(7.22859940157151,-3.2208406303884,129.509074462654));
#229942=CARTESIAN_POINT('Ctrl Pts',(7.13977095373429,-3.40699159497234,
129.500775691338));
#229943=CARTESIAN_POINT('Ctrl Pts',(7.05083910445851,-3.59335925001971,
129.492467259774));
#229944=CARTESIAN_POINT('Ctrl Pts',(6.95464849006075,-3.77615454630648,
129.48415882821));
#229945=CARTESIAN_POINT('Ctrl Pts',(6.8515184930998,-3.95482178343241,129.475850396646));
#229946=CARTESIAN_POINT('Ctrl Pts',(6.74832487856208,-4.13359923462803,
129.467536839878));
#229947=CARTESIAN_POINT('Ctrl Pts',(6.63818348852295,-4.30824329374038,
129.45922328311));
#229948=CARTESIAN_POINT('Ctrl Pts',(6.52145744518215,-4.47822663458186,
129.450909726342));
#229949=CARTESIAN_POINT('Ctrl Pts',(6.40460378620328,-4.64839581683355,
129.44258708043));
#229950=CARTESIAN_POINT('Ctrl Pts',(6.28115125632881,-4.81389385895475,
129.434264434518));
#229951=CARTESIAN_POINT('Ctrl Pts',(6.15150470580301,-4.97422464857423,
129.425941788605));
#229952=CARTESIAN_POINT('Ctrl Pts',(6.10229236040166,-5.03508437962935,
129.422782607558));
#229953=CARTESIAN_POINT('Ctrl Pts',(6.05218793563885,-5.09519993015592,
129.41962342651));
#229954=CARTESIAN_POINT('Ctrl Pts',(6.00121501131736,-5.15454550740793,
129.416464245463));
#229955=CARTESIAN_POINT('Ctrl Pts',(5.86087052655006,-5.3179425377631,129.407766026903));
#229956=CARTESIAN_POINT('Ctrl Pts',(5.71381491466608,-5.47564514668322,
129.399067808342));
#229957=CARTESIAN_POINT('Ctrl Pts',(5.56051322480689,-5.62713192281358,
129.390369589782));
#229958=CARTESIAN_POINT('Ctrl Pts',(5.40734623103258,-5.77848559750407,
129.381679013773));
#229959=CARTESIAN_POINT('Ctrl Pts',(5.24794428011976,-5.9236341839293,129.372988437764));
#229960=CARTESIAN_POINT('Ctrl Pts',(5.08280978380573,-6.06209251840062,
129.364297861755));
#229961=CARTESIAN_POINT('Ctrl Pts',(4.91371493496276,-6.20387144201179,
129.355398863245));
#229962=CARTESIAN_POINT('Ctrl Pts',(4.73860929424641,-6.33863502031817,
129.346499864736));
#229963=CARTESIAN_POINT('Ctrl Pts',(4.55807175947969,-6.46590309511624,
129.337600866226));
#229964=CARTESIAN_POINT('Ctrl Pts',(4.38228206693546,-6.58982422746335,
129.328935896839));
#229965=CARTESIAN_POINT('Ctrl Pts',(4.20134274486011,-6.70663892205821,
129.320270927452));
#229966=CARTESIAN_POINT('Ctrl Pts',(4.01582217827375,-6.81594404558053,
129.311605958064));
#229967=CARTESIAN_POINT('Ctrl Pts',(3.8227856217016,-6.92967744478627,129.302589944993));
#229968=CARTESIAN_POINT('Ctrl Pts',(3.62478906884573,-7.03527998402457,
129.293573931922));
#229969=CARTESIAN_POINT('Ctrl Pts',(3.42250840623855,-7.13234584195316,
129.284557918851));
#229970=CARTESIAN_POINT('Ctrl Pts',(3.22022774363136,-7.22941169988175,
129.27554190578));
#229971=CARTESIAN_POINT('Ctrl Pts',(3.01366319431664,-7.31794069493331,
129.266525892709));
#229972=CARTESIAN_POINT('Ctrl Pts',(2.80352372497274,-7.39757904476289,
129.257509879638));
#229973=CARTESIAN_POINT('Ctrl Pts',(2.6214829541078,-7.46656859079464,129.249699438436));
#229974=CARTESIAN_POINT('Ctrl Pts',(2.43683770602419,-7.52885590885969,
129.241888997233));
#229975=CARTESIAN_POINT('Ctrl Pts',(2.25012971134512,-7.58424928929172,
129.234078556031));
#229976=CARTESIAN_POINT('Ctrl Pts',(2.06343517793614,-7.63963867597266,
129.226268677946));
#229977=CARTESIAN_POINT('Ctrl Pts',(1.87467853179391,-7.68813501490881,
129.218458799861));
#229978=CARTESIAN_POINT('Ctrl Pts',(1.6844167269518,-7.72959645065413,129.210648921776));
#229979=CARTESIAN_POINT('Ctrl Pts',(1.49413505736912,-7.77106221528021,
129.202838228281));
#229980=CARTESIAN_POINT('Ctrl Pts',(1.30234826035644,-7.80549153953602,
129.195027534787));
#229981=CARTESIAN_POINT('Ctrl Pts',(1.10962368973367,-7.83279364385286,
129.187216841293));
#229982=CARTESIAN_POINT('Ctrl Pts',(0.916762351033343,-7.86011512326189,
129.179400604896));
#229983=CARTESIAN_POINT('Ctrl Pts',(0.722962258273764,-7.88029922835287,
129.171584368499));
#229984=CARTESIAN_POINT('Ctrl Pts',(0.528796982780863,-7.89330695912695,
129.163768132102));
#229985=CARTESIAN_POINT('Ctrl Pts',(0.3345599215757,-7.90631949904733,129.15594900593));
#229986=CARTESIAN_POINT('Ctrl Pts',(0.139957760356455,-7.91215036391374,
129.148129879757));
#229987=CARTESIAN_POINT('Ctrl Pts',(-0.0544355691391259,-7.91081271228263,
129.140310753584));
#229988=CARTESIAN_POINT('Ctrl Pts',(-0.249045058317264,-7.90947357322214,
129.132482932773));
#229989=CARTESIAN_POINT('Ctrl Pts',(-0.443444899973684,-7.90095000545172,
129.124655111961));
#229990=CARTESIAN_POINT('Ctrl Pts',(-0.637064811594767,-7.88530718652278,
129.116827291149));
#229991=CARTESIAN_POINT('Ctrl Pts',(-0.787714653910383,-7.87313597858612,
129.110736698704));
#229992=CARTESIAN_POINT('Ctrl Pts',(-0.937892393890127,-7.85665587907517,
129.104646106259));
#229993=CARTESIAN_POINT('Ctrl Pts',(-1.08733377287872,-7.83591898033392,
129.098555513814));
#229994=CARTESIAN_POINT('Ctrl Pts',(-1.28649543838022,-7.80828275723028,
129.090438534812));
#229995=CARTESIAN_POINT('Ctrl Pts',(-1.48474480775886,-7.77302955959852,
129.08232155581));
#229996=CARTESIAN_POINT('Ctrl Pts',(-1.68147669854351,-7.73023654956659,
129.074204576808));
#229997=CARTESIAN_POINT('Ctrl Pts',(-1.8780646867795,-7.68747484113596,
129.066093535094));
#229998=CARTESIAN_POINT('Ctrl Pts',(-2.07313709734138,-7.63718438462703,
129.057982493381));
#229999=CARTESIAN_POINT('Ctrl Pts',(-2.26609703542969,-7.57949373151115,
129.049871451667));
#230000=CARTESIAN_POINT('Ctrl Pts',(-2.45894326550832,-7.52183707451595,
129.041765189653));
#230001=CARTESIAN_POINT('Ctrl Pts',(-2.64967919891987,-7.45678900823411,
129.033658927638));
#230002=CARTESIAN_POINT('Ctrl Pts',(-2.83772068544547,-7.38452857746484,
129.025552665623));
#230003=CARTESIAN_POINT('Ctrl Pts',(-3.02567806992521,-7.31230046536192,
129.017450029155));
#230004=CARTESIAN_POINT('Ctrl Pts',(-3.21094311195377,-7.2328665366034,
129.009347392688));
#230005=CARTESIAN_POINT('Ctrl Pts',(-3.39294876614398,-7.14645504220953,
129.00124475622));
#230006=CARTESIAN_POINT('Ctrl Pts',(-3.57489884682694,-7.06006993265427,
128.993144593807));
#230007=CARTESIAN_POINT('Ctrl Pts',(-3.75359123527485,-6.96671164425574,
128.985044431393));
#230008=CARTESIAN_POINT('Ctrl Pts',(-3.92848022020225,-6.86665596629682,
128.97694426898));
#230009=CARTESIAN_POINT('Ctrl Pts',(-4.10507270924634,-6.76562569717441,
128.968765207029));
#230010=CARTESIAN_POINT('Ctrl Pts',(-4.27778700634479,-6.65776701350228,
128.960586145079));
#230011=CARTESIAN_POINT('Ctrl Pts',(-4.44608732466862,-6.54341107538117,
128.952407083128));
#230012=CARTESIAN_POINT('Ctrl Pts',(-4.6127632151291,-6.43015889614818,
128.944306965152));
#230013=CARTESIAN_POINT('Ctrl Pts',(-4.77510970111102,-6.31053453282727,
128.936206847177));
#230014=CARTESIAN_POINT('Ctrl Pts',(-4.93263578576802,-6.18490300691617,
128.928106729201));
#230015=CARTESIAN_POINT('Ctrl Pts',(-5.09018307066639,-6.05925457321054,
128.920005521092));
#230016=CARTESIAN_POINT('Ctrl Pts',(-5.24290840960802,-5.92759756459862,
128.911904312983));
#230017=CARTESIAN_POINT('Ctrl Pts',(-5.39035375721154,-5.79033741435812,
128.903803104874));
#230018=CARTESIAN_POINT('Ctrl Pts',(-5.53783799082539,-5.65304106426657,
128.895699760219));
#230019=CARTESIAN_POINT('Ctrl Pts',(-5.68003922133437,-5.51013884410502,
128.887596415565));
#230020=CARTESIAN_POINT('Ctrl Pts',(-5.81653576125156,-5.36207354836557,
128.879493070911));
#230021=CARTESIAN_POINT('Ctrl Pts',(-5.95528686725633,-5.21156260092883,
128.871255880182));
#230022=CARTESIAN_POINT('Ctrl Pts',(-6.08814294612623,-5.05571677712489,
128.863018689453));
#230023=CARTESIAN_POINT('Ctrl Pts',(-6.21470335965031,-4.89503658326995,
128.854781498724));
#230024=CARTESIAN_POINT('Ctrl Pts',(-6.33936942420691,-4.73676144128587,
128.84666760179));
#230025=CARTESIAN_POINT('Ctrl Pts',(-6.45792680946358,-4.57379591904472,
128.838553704857));
#230026=CARTESIAN_POINT('Ctrl Pts',(-6.57003591656469,-4.40664827902682,
128.830439807924));
#230027=CARTESIAN_POINT('Ctrl Pts',(-6.68470033539451,-4.23569082965436,
128.822140970297));
#230028=CARTESIAN_POINT('Ctrl Pts',(-6.79261883201481,-4.06035864948025,
128.81384213267));
#230029=CARTESIAN_POINT('Ctrl Pts',(-6.89347722352456,-3.88122310216099,
128.805543295044));
#230030=CARTESIAN_POINT('Ctrl Pts',(-6.99433561503423,-3.70208755484186,
128.797244457417));
#230031=CARTESIAN_POINT('Ctrl Pts',(-7.08813377025222,-3.51914897332756,
128.78894561979));
#230032=CARTESIAN_POINT('Ctrl Pts',(-7.1746094353811,-3.33300171763239,
128.780646782164));
#230033=CARTESIAN_POINT('Ctrl Pts',(-7.2587303778006,-3.15192323093279,
128.772573920959));
#230034=CARTESIAN_POINT('Ctrl Pts',(-7.3360950640958,-2.96743665300502,
128.764501059755));
#230035=CARTESIAN_POINT('Ctrl Pts',(-7.40642284997545,-2.78007582043394,
128.756428198551));
#230036=CARTESIAN_POINT('Ctrl Pts',(-7.47666360158173,-2.59294685658613,
128.74836532793));
#230037=CARTESIAN_POINT('Ctrl Pts',(-7.53988469464196,-2.40295102848861,
128.740302457309));
#230038=CARTESIAN_POINT('Ctrl Pts',(-7.59585206049751,-2.21064526214312,
128.732239586688));
#230039=CARTESIAN_POINT('Ctrl Pts',(-7.65173768266623,-2.01862036987662,
128.724188492372));
#230040=CARTESIAN_POINT('Ctrl Pts',(-7.70039061785201,-1.82429257827295,
128.716137398056));
#230041=CARTESIAN_POINT('Ctrl Pts',(-7.74162547949035,-1.62823706360768,
128.70808630374));
#230042=CARTESIAN_POINT('Ctrl Pts',(-7.78282540607073,-1.43234765137363,
128.700042030483));
#230043=CARTESIAN_POINT('Ctrl Pts',(-7.81661971546128,-1.2347337488063,
128.691997757227));
#230044=CARTESIAN_POINT('Ctrl Pts',(-7.84287291842816,-1.03598522450182,
128.683953483971));
#230045=CARTESIAN_POINT('Ctrl Pts',(-7.86910184996185,-0.837420445835432,
128.675916647751));
#230046=CARTESIAN_POINT('Ctrl Pts',(-7.88780353659961,-0.637723458176799,
128.667879811532));
#230047=CARTESIAN_POINT('Ctrl Pts',(-7.89889359558828,-0.43749396061485,
128.659842975312));
#230048=CARTESIAN_POINT('Ctrl Pts',(-7.9069483075645,-0.29206723802905,
128.654005819621));
#230049=CARTESIAN_POINT('Ctrl Pts',(-7.91098884942515,-0.146359866205317,
128.648168663929));
#230050=CARTESIAN_POINT('Ctrl Pts',(-7.91099997694602,-0.000603953663847722,
128.642331508237));
#230051=CARTESIAN_POINT('',(-7.9109999966855,0.000229002203636593,124.647722132928));
#230052=CARTESIAN_POINT('Ctrl Pts',(-7.91099999894138,-0.000129419717556176,
128.639166935561));
#230053=CARTESIAN_POINT('Ctrl Pts',(-7.91100121127412,0.0739764775597892,
128.636136268948));
#230054=CARTESIAN_POINT('Ctrl Pts',(-7.90996114968628,0.148079691724727,
128.633125555382));
#230055=CARTESIAN_POINT('Ctrl Pts',(-7.90735126112598,0.240980462184097,
128.629373408072));
#230056=CARTESIAN_POINT('Ctrl Pts',(-7.90675528800012,0.259800633819714,
128.628614428807));
#230057=CARTESIAN_POINT('Ctrl Pts',(-7.9056179254174,0.29207448438457,128.627314782394));
#230058=CARTESIAN_POINT('Ctrl Pts',(-7.90510937232408,0.305529213036417,
128.626773533638));
#230059=CARTESIAN_POINT('Ctrl Pts',(-7.90408917295933,0.330810321266307,
128.625757570898));
#230060=CARTESIAN_POINT('Ctrl Pts',(-7.903585327482,0.342636972377066,128.625282721452));
#230061=CARTESIAN_POINT('Ctrl Pts',(-7.90249553643135,0.366934829989268,
128.624307991145));
#230062=CARTESIAN_POINT('Ctrl Pts',(-7.90190660906471,0.379405871607893,
128.623808163293));
#230063=CARTESIAN_POINT('Ctrl Pts',(-7.90046935423753,0.408384883873768,
128.622647746519));
#230064=CARTESIAN_POINT('Ctrl Pts',(-7.89959880433447,0.424891707948672,
128.621987539022));
#230065=CARTESIAN_POINT('Ctrl Pts',(-7.89669893936198,0.476784135723711,
128.619914399464));
#230066=CARTESIAN_POINT('Ctrl Pts',(-7.89448354223286,0.51215902917028,
128.618504568365));
#230067=CARTESIAN_POINT('Ctrl Pts',(-7.88629008874091,0.630261068471869,
128.613808219431));
#230068=CARTESIAN_POINT('Ctrl Pts',(-7.87924873140524,0.712909591018122,
128.610539195005));
#230069=CARTESIAN_POINT('Ctrl Pts',(-7.78697011253223,1.62601811823754,
128.5746030605));
#230070=CARTESIAN_POINT('Ctrl Pts',(-7.57210414134284,2.43803142597582,
128.544969408907));
#230071=CARTESIAN_POINT('Ctrl Pts',(-7.15984653287076,3.36962347645104,
128.506794549435));
#230072=CARTESIAN_POINT('Ctrl Pts',(-7.07955622243845,3.53520073623228,
128.499802380294));
#230073=CARTESIAN_POINT('Ctrl Pts',(-6.95491557586082,3.77092947282715,
128.489386740156));
#230074=CARTESIAN_POINT('Ctrl Pts',(-6.91511762839045,3.8434239131052,128.486117981144));
#230075=CARTESIAN_POINT('Ctrl Pts',(-6.86743686486009,3.92713867459256,
128.482254085106));
#230076=CARTESIAN_POINT('Ctrl Pts',(-6.86065170309211,3.93898025741314,
128.481705425953));
#230077=CARTESIAN_POINT('Ctrl Pts',(-6.85026247888206,3.95700343327686,
128.480867067355));
#230078=CARTESIAN_POINT('Ctrl Pts',(-6.84668059675476,3.96319782576374,
128.480578338063));
#230079=CARTESIAN_POINT('Ctrl Pts',(-6.84016119063358,3.97443706274176,
128.480053370482));
#230080=CARTESIAN_POINT('Ctrl Pts',(-6.83722647476021,3.97948353585577,
128.479817257192));
#230081=CARTESIAN_POINT('Ctrl Pts',(-6.83090079366699,3.9903333851911,128.47930874711));
#230082=CARTESIAN_POINT('Ctrl Pts',(-6.82750801449153,3.99613569459031,
128.479036268582));
#230083=CARTESIAN_POINT('Ctrl Pts',(-6.81836635055561,4.01172408408465,
128.478302774026));
#230084=CARTESIAN_POINT('Ctrl Pts',(-6.81260380694788,4.02150210555337,
128.477841132327));
#230085=CARTESIAN_POINT('Ctrl Pts',(-6.78617524140649,4.06612690119456,
128.475727091229));
#230086=CARTESIAN_POINT('Ctrl Pts',(-6.76526301596299,4.1008265777983,128.474063117669));
#230087=CARTESIAN_POINT('Ctrl Pts',(-6.42824960169078,4.65043901203498,
128.447365444081));
#230088=CARTESIAN_POINT('Ctrl Pts',(-6.0545011462509,5.12754827620941,128.419079539236));
#230089=CARTESIAN_POINT('Ctrl Pts',(-5.49870413874924,5.69062479448512,
128.382759735616));
#230090=CARTESIAN_POINT('Ctrl Pts',(-5.36252161189191,5.81913421414582,
128.37422098809));
#230091=CARTESIAN_POINT('Ctrl Pts',(-5.03073695829835,6.1106767293155,128.354376293751));
#230092=CARTESIAN_POINT('Ctrl Pts',(-4.83156501548559,6.26934431935141,
128.343194039817));
#230093=CARTESIAN_POINT('Ctrl Pts',(-4.5293528194415,6.48712618490164,128.32736051447));
#230094=CARTESIAN_POINT('Ctrl Pts',(-4.43209288467012,6.55396043425648,
128.322424245819));
#230095=CARTESIAN_POINT('Ctrl Pts',(-4.29805063652521,6.64172146817376,
128.315835424086));
#230096=CARTESIAN_POINT('Ctrl Pts',(-4.26254504276058,6.66456398934121,
128.314110017186));
#230097=CARTESIAN_POINT('Ctrl Pts',(-4.21026732610536,6.69760817471524,
128.31159838707));
#230098=CARTESIAN_POINT('Ctrl Pts',(-4.19363768819147,6.70803318171213,
128.310803662887));
#230099=CARTESIAN_POINT('Ctrl Pts',(-4.16354986777803,6.7267394173849,128.309373370625));
#230100=CARTESIAN_POINT('Ctrl Pts',(-4.15010537281631,6.73504239699292,
128.308736976536));
#230101=CARTESIAN_POINT('Ctrl Pts',(-4.12949887517224,6.7476833171155,128.307765710601));
#230102=CARTESIAN_POINT('Ctrl Pts',(-4.12235475136984,6.75205023770998,
128.30742973828));
#230103=CARTESIAN_POINT('Ctrl Pts',(-4.10989864132629,6.75963702740896,
128.306845272573));
#230104=CARTESIAN_POINT('Ctrl Pts',(-4.10458977755371,6.76286199345599,
128.306596585905));
#230105=CARTESIAN_POINT('Ctrl Pts',(-4.09349665681893,6.76958283790018,
128.3060778099));
#230106=CARTESIAN_POINT('Ctrl Pts',(-4.08771170555547,6.7730775642357,128.305807764335));
#230107=CARTESIAN_POINT('Ctrl Pts',(-4.07174047653524,6.78269797171888,
128.30506356717));
#230108=CARTESIAN_POINT('Ctrl Pts',(-4.06154484096062,6.78880812737592,
128.304590003717));
#230109=CARTESIAN_POINT('Ctrl Pts',(-4.02176220371625,6.81252781711409,
128.302748063967));
#230110=CARTESIAN_POINT('Ctrl Pts',(-3.99207393047296,6.8299672221038,128.301386120921));
#230111=CARTESIAN_POINT('Ctrl Pts',(-3.50928213737817,7.10934407385299,
128.279439688606));
#230112=CARTESIAN_POINT('Ctrl Pts',(-3.03138836506622,7.3258858474412,128.260704198303));
#230113=CARTESIAN_POINT('Ctrl Pts',(-2.2931515475015,7.57567577855633,128.234052269651));
#230114=CARTESIAN_POINT('Ctrl Pts',(-2.04690949239423,7.64588586348729,
128.225493231206));
#230115=CARTESIAN_POINT('Ctrl Pts',(-1.76605233908665,7.71142244367132,
128.215790663973));
#230116=CARTESIAN_POINT('Ctrl Pts',(-1.73436162607159,7.71861170900182,
128.214696619827));
#230117=CARTESIAN_POINT('Ctrl Pts',(-1.6659907971715,7.73367979101778,128.212336532435));
#230118=CARTESIAN_POINT('Ctrl Pts',(-1.62929714106727,7.74149334822053,
128.211070060516));
#230119=CARTESIAN_POINT('Ctrl Pts',(-1.48467495034829,7.77121545747075,
128.20607511708));
#230120=CARTESIAN_POINT('Ctrl Pts',(-1.37635048005621,7.7911300987996,128.202326632114));
#230121=CARTESIAN_POINT('Ctrl Pts',(-1.07345989407446,7.84030019825425,
128.191751208123));
#230122=CARTESIAN_POINT('Ctrl Pts',(-0.878171960371177,7.86456807998093,
128.184825899124));
#230123=CARTESIAN_POINT('Ctrl Pts',(-0.51927092236274,7.89563301418451,
128.171605098645));
#230124=CARTESIAN_POINT('Ctrl Pts',(-0.355961363407117,7.90467889214603,
128.165403245937));
#230125=CARTESIAN_POINT('Ctrl Pts',(-0.167723119136127,7.90926065743318,
128.157928234554));
#230126=CARTESIAN_POINT('Ctrl Pts',(-0.142945135043231,7.90974726862364,
128.156937782592));
#230127=CARTESIAN_POINT('Ctrl Pts',(-0.111295951826042,7.91022006096811,
128.155663918323));
#230128=CARTESIAN_POINT('Ctrl Pts',(-0.1044262498859,7.91031373332172,128.155386889707));
#230129=CARTESIAN_POINT('Ctrl Pts',(-0.09340881010094,7.91044960794139,
128.154941742852));
#230130=CARTESIAN_POINT('Ctrl Pts',(-0.089261132376909,7.91049749735751,
128.154773966207));
#230131=CARTESIAN_POINT('Ctrl Pts',(-0.0813962377484495,7.91058211964043,
128.154455453445));
#230132=CARTESIAN_POINT('Ctrl Pts',(-0.0776790273551331,7.91061949455969,
128.154304756198));
#230133=CARTESIAN_POINT('Ctrl Pts',(-0.0692478609497113,7.91069832296132,
128.153962593291));
#230134=CARTESIAN_POINT('Ctrl Pts',(-0.0645339224007235,7.9107381827475,
128.153771031442));
#230135=CARTESIAN_POINT('Ctrl Pts',(-0.0522928525898666,7.91083074762393,
128.153272920988));
#230136=CARTESIAN_POINT('Ctrl Pts',(-0.0447657354246197,7.91087692282478,
128.152965977143));
#230137=CARTESIAN_POINT('Ctrl Pts',(0.00162847907137823,7.91109531169428,
128.151070129017));
#230138=CARTESIAN_POINT('Ctrl Pts',(0.0404956967984957,7.91099182627501,
128.149464708376));
#230139=CARTESIAN_POINT('Ctrl Pts',(0.734275082004543,7.9040317681045,128.120523403488));
#230140=CARTESIAN_POINT('Ctrl Pts',(1.38580846036759,7.81616030339117,128.089042961505));
#230141=CARTESIAN_POINT('Ctrl Pts',(2.21805256030406,7.59648167987469,128.049116846429));
#230142=CARTESIAN_POINT('Ctrl Pts',(2.41495582983533,7.53619833059681,128.03967026914));
#230143=CARTESIAN_POINT('Ctrl Pts',(2.83017952890383,7.39112662353034,128.019900972368));
#230144=CARTESIAN_POINT('Ctrl Pts',(3.04754656824602,7.30418656388955,128.009646008333));
#230145=CARTESIAN_POINT('Ctrl Pts',(3.36033381813377,7.16268269707147,127.995091978784));
#230146=CARTESIAN_POINT('Ctrl Pts',(3.45897267658545,7.11557279319726,127.990532072382));
#230147=CARTESIAN_POINT('Ctrl Pts',(3.59194910385011,7.04864441884482,127.984424766662));
#230148=CARTESIAN_POINT('Ctrl Pts',(3.62715794216121,7.03059114406723,127.982811558872));
#230149=CARTESIAN_POINT('Ctrl Pts',(3.67864334010268,7.00370238118153,127.980458064688));
#230150=CARTESIAN_POINT('Ctrl Pts',(3.69502638163961,6.99507283117162,127.979709984645));
#230151=CARTESIAN_POINT('Ctrl Pts',(3.72448251138582,6.97942484577755,127.978366409201));
#230152=CARTESIAN_POINT('Ctrl Pts',(3.73756640917296,6.97242701617256,127.977770132838));
#230153=CARTESIAN_POINT('Ctrl Pts',(3.75769598649603,6.96158791274822,127.976853542057));
#230154=CARTESIAN_POINT('Ctrl Pts',(3.7647556022566,6.95777267878535,127.976532234144));
#230155=CARTESIAN_POINT('Ctrl Pts',(3.77704306051581,6.95110798134977,127.975973244228));
#230156=CARTESIAN_POINT('Ctrl Pts',(3.78227350725494,6.9482633489173,127.975735377772));
#230157=CARTESIAN_POINT('Ctrl Pts',(3.79318888994037,6.94231092806197,127.975239143143));
#230158=CARTESIAN_POINT('Ctrl Pts',(3.79887323035141,6.93920205474923,127.974980816798));
#230159=CARTESIAN_POINT('Ctrl Pts',(3.81280409051244,6.93156075606482,127.974347955491));
#230160=CARTESIAN_POINT('Ctrl Pts',(3.82104636545572,6.92702058763709,127.973973717626));
#230161=CARTESIAN_POINT('Ctrl Pts',(3.85276248305608,6.9094762736656,127.972534408928));
#230162=CARTESIAN_POINT('Ctrl Pts',(3.87617833351463,6.89636735340833,127.971473363667));
#230163=CARTESIAN_POINT('Ctrl Pts',(4.2633728756836,6.67700878084544,127.95395339055));
#230164=CARTESIAN_POINT('Ctrl Pts',(4.61032093100209,6.44234319828263,127.938676841411));
#230165=CARTESIAN_POINT('Ctrl Pts',(5.31584473587302,5.8788311362351,127.907110024825));
#230166=CARTESIAN_POINT('Ctrl Pts',(5.66595488929413,5.54218307766664,127.891121907487));
#230167=CARTESIAN_POINT('Ctrl Pts',(6.03005812778953,5.12127747317954,127.871733860245));
#230168=CARTESIAN_POINT('Ctrl Pts',(6.07632406315281,5.0662974266392,127.869210259617));
#230169=CARTESIAN_POINT('Ctrl Pts',(6.18421386044982,4.93448270397832,127.863161202208));
#230170=CARTESIAN_POINT('Ctrl Pts',(6.24516367136208,4.85711338707234,127.859611706086));
#230171=CARTESIAN_POINT('Ctrl Pts',(6.40141946301403,4.65095833923383,127.850098225546));
#230172=CARTESIAN_POINT('Ctrl Pts',(6.49428166457669,4.52038543862774,127.844017516621));
#230173=CARTESIAN_POINT('Ctrl Pts',(6.5966257938236,4.36681154544922,127.836689064041));
#230174=CARTESIAN_POINT('Ctrl Pts',(6.61004693563552,4.34646919228543,127.835714853272));
#230175=CARTESIAN_POINT('Ctrl Pts',(6.62717794131313,4.32024095702252,127.834453856382));
#230176=CARTESIAN_POINT('Ctrl Pts',(6.63097433720514,4.31441174799988,127.834173294221));
#230177=CARTESIAN_POINT('Ctrl Pts',(6.63710578622756,4.30496995178391,127.833718371256));
#230178=CARTESIAN_POINT('Ctrl Pts',(6.63944559764473,4.30136044282628,127.833544343911));
#230179=CARTESIAN_POINT('Ctrl Pts',(6.64391323737766,4.2944561096564,127.833211245041));
#230180=CARTESIAN_POINT('Ctrl Pts',(6.64604156240506,4.29116160663332,127.833052208073));
#230181=CARTESIAN_POINT('Ctrl Pts',(6.65091085556426,4.28361195844812,127.832687547952));
#230182=CARTESIAN_POINT('Ctrl Pts',(6.65365018934629,4.2793557665616,127.832481812484));
#230183=CARTESIAN_POINT('Ctrl Pts',(6.66206729161779,4.26625022124334,127.831847849524));
#230184=CARTESIAN_POINT('Ctrl Pts',(6.66773148423367,4.25739220655312,127.831418699046));
#230185=CARTESIAN_POINT('Ctrl Pts',(6.70995470088925,4.19106998440169,127.828200797184));
#230186=CARTESIAN_POINT('Ctrl Pts',(6.74578694018977,4.13314864689467,127.825363928082));
#230187=CARTESIAN_POINT('Ctrl Pts',(7.0450362889,3.6351652238909,127.800797190376));
#230188=CARTESIAN_POINT('Ctrl Pts',(7.26581208746858,3.17094018161968,127.776795965506));
#230189=CARTESIAN_POINT('Ctrl Pts',(7.53520571427323,2.42547142535818,127.739808659456));
#230190=CARTESIAN_POINT('Ctrl Pts',(7.6162868986103,2.15741054967077,127.726783426014));
#230191=CARTESIAN_POINT('Ctrl Pts',(7.75515812895008,1.59157410622988,127.700264519393));
#230192=CARTESIAN_POINT('Ctrl Pts',(7.81038753440492,1.29362162286276,127.686844109572));
#230193=CARTESIAN_POINT('Ctrl Pts',(7.86901738905358,0.830327424531193,
127.666950089259));
#230194=CARTESIAN_POINT('Ctrl Pts',(7.88455565284768,0.666831886836047,
127.660110732551));
#230195=CARTESIAN_POINT('Ctrl Pts',(7.89637673781107,0.481277105799719,
127.652546478748));
#230196=CARTESIAN_POINT('Ctrl Pts',(7.89766899155654,0.459584320521321,
127.65166519196));
#230197=CARTESIAN_POINT('Ctrl Pts',(7.89983054064649,0.420592928296198,
127.650086525196));
#230198=CARTESIAN_POINT('Ctrl Pts',(7.90073243890115,0.403296313038426,
127.649388131948));
#230199=CARTESIAN_POINT('Ctrl Pts',(7.90201263261451,0.377090008239126,
127.648332844756));
#230200=CARTESIAN_POINT('Ctrl Pts',(7.90243267565847,0.368182465184135,
127.647974651587));
#230201=CARTESIAN_POINT('Ctrl Pts',(7.90313323640022,0.352772459050454,
127.647355838861));
#230202=CARTESIAN_POINT('Ctrl Pts',(7.90342079204526,0.346270334101139,
127.647095000653));
#230203=CARTESIAN_POINT('Ctrl Pts',(7.90400006973454,0.332795141442946,
127.64655497823));
#230204=CARTESIAN_POINT('Ctrl Pts',(7.90429058900953,0.325822027069712,
127.646275831647));
#230205=CARTESIAN_POINT('Ctrl Pts',(7.90497338961275,0.308894721436374,
127.645598932737));
#230206=CARTESIAN_POINT('Ctrl Pts',(7.90535609766465,0.298940143658653,
127.645201477888));
#230207=CARTESIAN_POINT('Ctrl Pts',(7.9067174889718,0.261696742733594,127.643716749595));
#230208=CARTESIAN_POINT('Ctrl Pts',(7.90757368963916,0.234403491987286,
127.642633275133));
#230209=CARTESIAN_POINT('Ctrl Pts',(7.91945394396499,-0.219240524756486,
127.624699341592));
#230210=CARTESIAN_POINT('Ctrl Pts',(7.89612500699176,-0.645814099276256,
127.60898279469));
#230211=CARTESIAN_POINT('Ctrl Pts',(7.76791458401909,-1.58640449193305,
127.575318675768));
#230212=CARTESIAN_POINT('Ctrl Pts',(7.64615516803898,-2.09605719926854,
127.557762258673));
#230213=CARTESIAN_POINT('Ctrl Pts',(7.37543293457946,-2.87740399458092,
127.528161550649));
#230214=CARTESIAN_POINT('Ctrl Pts',(7.25936692570651,-3.15880679583878,
127.516833759523));
#230215=CARTESIAN_POINT('Ctrl Pts',(7.11760984898295,-3.45312256546041,
127.503816847697));
#230216=CARTESIAN_POINT('Ctrl Pts',(7.10777788190242,-3.47331527273461,
127.502918446733));
#230217=CARTESIAN_POINT('Ctrl Pts',(7.09365552708116,-3.50200841224156,
127.501634486217));
#230218=CARTESIAN_POINT('Ctrl Pts',(7.08943552405788,-3.51054349148853,
127.501251627071));
#230219=CARTESIAN_POINT('Ctrl Pts',(7.0821353710373,-3.52524141786543,127.500590734554));
#230220=CARTESIAN_POINT('Ctrl Pts',(7.07906255460162,-3.53140790842009,
127.500312976034));
#230221=CARTESIAN_POINT('Ctrl Pts',(7.07317239281364,-3.54318963221742,
127.499781375778));
#230222=CARTESIAN_POINT('Ctrl Pts',(7.07035640564869,-3.54880554062257,
127.499527584161));
#230223=CARTESIAN_POINT('Ctrl Pts',(7.0637569968915,-3.5619276728514,127.498933652611));
#230224=CARTESIAN_POINT('Ctrl Pts',(7.05996829840127,-3.56943122678449,
127.498593321691));
#230225=CARTESIAN_POINT('Ctrl Pts',(7.04648903191586,-3.59602162649467,
127.497384810311));
#230226=CARTESIAN_POINT('Ctrl Pts',(7.03673300246097,-3.61507508330517,
127.496514311783));
#230227=CARTESIAN_POINT('Ctrl Pts',(6.89280533789541,-3.89337464818352,
127.483735041236));
#230228=CARTESIAN_POINT('Ctrl Pts',(6.74446685989942,-4.1450314520681,127.471367495351));
#230229=CARTESIAN_POINT('Ctrl Pts',(6.21520984343613,-4.93900298755645,
127.430517156432));
#230230=CARTESIAN_POINT('Ctrl Pts',(5.7800638917804,-5.44183145675548,127.401932221355));
#230231=CARTESIAN_POINT('Ctrl Pts',(4.96201057748446,-6.17686648437265,
127.356067753393));
#230232=CARTESIAN_POINT('Ctrl Pts',(4.61296617694909,-6.4417225915335,127.338096220104));
#230233=CARTESIAN_POINT('Ctrl Pts',(4.20163165313136,-6.70318668381087,
127.318349471264));
#230234=CARTESIAN_POINT('Ctrl Pts',(4.15918767725659,-6.72960460733497,
127.316328772945));
#230235=CARTESIAN_POINT('Ctrl Pts',(4.09513266996374,-6.76863614507779,
127.313304309528));
#230236=CARTESIAN_POINT('Ctrl Pts',(4.07370768947117,-6.78155236762812,
127.312296857622));
#230237=CARTESIAN_POINT('Ctrl Pts',(4.0367000966844,-6.80362403049173,127.310563797947));
#230238=CARTESIAN_POINT('Ctrl Pts',(4.02114673500226,-6.81282808798094,
127.309837588312));
#230239=CARTESIAN_POINT('Ctrl Pts',(3.98894776163817,-6.83173389032634,
127.308338589413));
#230240=CARTESIAN_POINT('Ctrl Pts',(3.97229796922217,-6.84142828942935,
127.307565896845));
#230241=CARTESIAN_POINT('Ctrl Pts',(3.92699091822985,-6.86758732303617,
127.305469802101));
#230242=CARTESIAN_POINT('Ctrl Pts',(3.89826557889077,-6.88393338142764,
127.304147919869));
#230243=CARTESIAN_POINT('Ctrl Pts',(3.78858369651143,-6.94544080420906,
127.299127093602));
#230244=CARTESIAN_POINT('Ctrl Pts',(3.70693751791876,-6.98935826053939,
127.295444353657));
#230245=CARTESIAN_POINT('Ctrl Pts',(3.5264138297107,-7.08240869392595,127.287414677762));
#230246=CARTESIAN_POINT('Ctrl Pts',(3.42724124136173,-7.13092737967312,
127.283076051168));
#230247=CARTESIAN_POINT('Ctrl Pts',(2.88398997815055,-7.3827531656119,127.259663011855));
#230248=CARTESIAN_POINT('Ctrl Pts',(2.42283147915567,-7.54667662001762,
127.241119188796));
#230249=CARTESIAN_POINT('Ctrl Pts',(1.79130519476014,-7.70725587816562,
127.21592414503));
#230250=CARTESIAN_POINT('Ctrl Pts',(1.63189710549168,-7.7425756436185,127.209573584054));
#230251=CARTESIAN_POINT('Ctrl Pts',(1.39275569657107,-7.78784807750668,
127.19996801373));
#230252=CARTESIAN_POINT('Ctrl Pts',(1.31377670325269,-7.80155988004134,
127.196782916753));
#230253=CARTESIAN_POINT('Ctrl Pts',(1.2165217250263,-7.81692593190561,127.192835372436));
#230254=CARTESIAN_POINT('Ctrl Pts',(1.19842970397341,-7.81972009555002,
127.192099926928));
#230255=CARTESIAN_POINT('Ctrl Pts',(1.16930234122253,-7.82411511738605,
127.190914092964));
#230256=CARTESIAN_POINT('Ctrl Pts',(1.15827309312231,-7.82575547637889,
127.1904646628));
#230257=CARTESIAN_POINT('Ctrl Pts',(1.137181307991,-7.82884685202697,127.189604442218));
#230258=CARTESIAN_POINT('Ctrl Pts',(1.12711936506956,-7.8303018010742,127.189193742428));
#230259=CARTESIAN_POINT('Ctrl Pts',(1.10405064384642,-7.83359213391723,
127.188251416144));
#230260=CARTESIAN_POINT('Ctrl Pts',(1.09104205326145,-7.83541452517142,
127.187719503395));
#230261=CARTESIAN_POINT('Ctrl Pts',(1.05084674145612,-7.84094350074853,
127.186074374704));
#230262=CARTESIAN_POINT('Ctrl Pts',(1.02364531663509,-7.84454103876331,
127.184958849807));
#230263=CARTESIAN_POINT('Ctrl Pts',(0.728891764564894,-7.88196460789007,
127.172849153586));
#230264=CARTESIAN_POINT('Ctrl Pts',(0.459801317816734,-7.90222915293735,
127.161603385505));
#230265=CARTESIAN_POINT('Ctrl Pts',(-0.0547559478940852,-7.91460457148811,
127.140021188502));
#230266=CARTESIAN_POINT('Ctrl Pts',(-0.299863770029728,-7.90911158751756,
127.129706749688));
#230267=CARTESIAN_POINT('Ctrl Pts',(-0.898554161588049,-7.86782052009627,
127.104583651413));
#230268=CARTESIAN_POINT('Ctrl Pts',(-1.25074927542086,-7.81956765641137,
127.089875604971));
#230269=CARTESIAN_POINT('Ctrl Pts',(-1.67626220352074,-7.73177647893193,
127.072188351917));
#230270=CARTESIAN_POINT('Ctrl Pts',(-1.75376135362985,-7.71456698522073,
127.068969444003));
#230271=CARTESIAN_POINT('Ctrl Pts',(-1.8637342825626,-7.68840350646528,
127.064402981761));
#230272=CARTESIAN_POINT('Ctrl Pts',(-1.89642975140006,-7.68040416671623,
127.063045500704));
#230273=CARTESIAN_POINT('Ctrl Pts',(-1.95294211941689,-7.66619487222827,
127.060699158801));
#230274=CARTESIAN_POINT('Ctrl Pts',(-1.97678288955216,-7.66008199387467,
127.059709308781));
#230275=CARTESIAN_POINT('Ctrl Pts',(-2.02259379101185,-7.64810776449011,
127.05780714235));
#230276=CARTESIAN_POINT('Ctrl Pts',(-2.04456793619461,-7.64226275251456,
127.056894669422));
#230277=CARTESIAN_POINT('Ctrl Pts',(-2.09650191950617,-7.62820854890854,
127.05473784476));
#230278=CARTESIAN_POINT('Ctrl Pts',(-2.12643923724366,-7.61991746300815,
127.053494328278));
#230279=CARTESIAN_POINT('Ctrl Pts',(-2.23252328786504,-7.5898638074851,
127.04908656302));
#230280=CARTESIAN_POINT('Ctrl Pts',(-2.30839150132203,-7.56713430920068,
127.045931880051));
#230281=CARTESIAN_POINT('Ctrl Pts',(-3.03914081070575,-7.33619496612101,
127.01549514784));
#230282=CARTESIAN_POINT('Ctrl Pts',(-3.66464783006157,-7.04461455593648,
126.989021916552));
#230283=CARTESIAN_POINT('Ctrl Pts',(-4.59368502364438,-6.45392132999017,
126.947938407626));
#230284=CARTESIAN_POINT('Ctrl Pts',(-4.92481142097114,-6.20493822861273,
126.93278793703));
#230285=CARTESIAN_POINT('Ctrl Pts',(-5.36753093011396,-5.81419018685479,
126.910404200392));
#230286=CARTESIAN_POINT('Ctrl Pts',(-5.49615527167176,-5.6927558299386,
126.903602584133));
#230287=CARTESIAN_POINT('Ctrl Pts',(-5.6395138915521,-5.54802006408539,
126.89554647607));
#230288=CARTESIAN_POINT('Ctrl Pts',(-5.65833265448537,-5.52882583521377,
126.894479062799));
#230289=CARTESIAN_POINT('Ctrl Pts',(-5.69073115102466,-5.49544226563643,
126.892623513879));
#230290=CARTESIAN_POINT('Ctrl Pts',(-5.70435660203371,-5.48129751763507,
126.89183760204));
#230291=CARTESIAN_POINT('Ctrl Pts',(-5.72379092210334,-5.46097156425398,
126.890708438992));
#230292=CARTESIAN_POINT('Ctrl Pts',(-5.72964280082457,-5.45483146575721,
126.890367364076));
#230293=CARTESIAN_POINT('Ctrl Pts',(-5.73975253569239,-5.44418958380439,
126.889776240866));
#230294=CARTESIAN_POINT('Ctrl Pts',(-5.74401500532617,-5.43969218005195,
126.889526430404));
#230295=CARTESIAN_POINT('Ctrl Pts',(-5.75217934210085,-5.43105755424641,
126.889046818237));
#230296=CARTESIAN_POINT('Ctrl Pts',(-5.75608204260536,-5.42692112157854,
126.88881706019));
#230297=CARTESIAN_POINT('Ctrl Pts',(-5.7652332045074,-5.41720092137577,
126.888277145113));
#230298=CARTESIAN_POINT('Ctrl Pts',(-5.7704780132899,-5.41161373552023,
126.887966795852));
#230299=CARTESIAN_POINT('Ctrl Pts',(-5.78842963191154,-5.39243447843413,
126.886901402197));
#230300=CARTESIAN_POINT('Ctrl Pts',(-5.80109654213844,-5.37880526777141,
126.886144222325));
#230301=CARTESIAN_POINT('Ctrl Pts',(-5.95525445125142,-5.21175807362279,
126.876861053795));
#230302=CARTESIAN_POINT('Ctrl Pts',(-6.09064397040441,-5.05287151888935,
126.867955198233));
#230303=CARTESIAN_POINT('Ctrl Pts',(-6.61329874990684,-4.38794922039038,
126.830730231465));
#230304=CARTESIAN_POINT('Ctrl Pts',(-6.94506665078206,-3.84134086028336,
126.800556618191));
#230305=CARTESIAN_POINT('Ctrl Pts',(-7.31101016087678,-3.0324721531888,
126.760497488015));
#230306=CARTESIAN_POINT('Ctrl Pts',(-7.40342598805415,-2.79929506686485,
126.749404632981));
#230307=CARTESIAN_POINT('Ctrl Pts',(-7.55002935522304,-2.37102711631056,
126.729951183344));
#230308=CARTESIAN_POINT('Ctrl Pts',(-7.60810174612933,-2.17750045052778,
126.721484453114));
#230309=CARTESIAN_POINT('Ctrl Pts',(-7.66808127750534,-1.94572629862531,
126.71172144012));
#230310=CARTESIAN_POINT('Ctrl Pts',(-7.67719924844319,-1.90943265273781,
126.710203361392));
#230311=CARTESIAN_POINT('Ctrl Pts',(-7.68900508906434,-1.86098804947727,
126.708191115238));
#230312=CARTESIAN_POINT('Ctrl Pts',(-7.69192223051535,-1.84889377234421,
126.707689920086));
#230313=CARTESIAN_POINT('Ctrl Pts',(-7.69667972412839,-1.82896337147814,
126.706865899581));
#230314=CARTESIAN_POINT('Ctrl Pts',(-7.69853666327623,-1.82113125136086,
126.706542566226));
#230315=CARTESIAN_POINT('Ctrl Pts',(-7.7021220354579,-1.80590553551546,
126.70591494185));
#230316=CARTESIAN_POINT('Ctrl Pts',(-7.70385178353016,-1.7985122601993,
126.705610610834));
#230317=CARTESIAN_POINT('Ctrl Pts',(-7.70783537877509,-1.78137441591975,
126.704906153957));
#230318=CARTESIAN_POINT('Ctrl Pts',(-7.71008139752591,-1.77162803105467,
126.704506268054));
#230319=CARTESIAN_POINT('Ctrl Pts',(-7.71727126903328,-1.74015563091299,
126.703217366535));
#230320=CARTESIAN_POINT('Ctrl Pts',(-7.7221418392687,-1.71841289676821,
126.702330592599));
#230321=CARTESIAN_POINT('Ctrl Pts',(-7.76689541662674,-1.51459514854758,
126.694051812421));
#230322=CARTESIAN_POINT('Ctrl Pts',(-7.80042507303443,-1.33117876678049,
126.686856591788));
#230323=CARTESIAN_POINT('Ctrl Pts',(-7.88306478053682,-0.76709537174334,
126.665387565063));
#230324=CARTESIAN_POINT('Ctrl Pts',(-7.91099226863457,-0.383891627020796,
126.651734473559));
#230325=CARTESIAN_POINT('Ctrl Pts',(-7.91101426730382,0.708199051772036,
126.613702437656));
#230326=CARTESIAN_POINT('Ctrl Pts',(-7.81588990038079,1.41326583717628,
126.590301005153));
#230327=CARTESIAN_POINT('Ctrl Pts',(-7.61746168952565,2.13538151381546,
126.560816417889));
#230328=CARTESIAN_POINT('Ctrl Pts',(-7.6063777508781,2.17453308484879,126.55919916733));
#230329=CARTESIAN_POINT('Ctrl Pts',(-7.59208350190564,2.22357756120768,
126.55715056772));
#230330=CARTESIAN_POINT('Ctrl Pts',(-7.58915499447128,2.23355222436618,
126.556732752421));
#230331=CARTESIAN_POINT('Ctrl Pts',(-7.58450896284928,2.24926224272562,
126.556072881872));
#230332=CARTESIAN_POINT('Ctrl Pts',(-7.58280456724606,2.25500149418048,
126.555831432977));
#230333=CARTESIAN_POINT('Ctrl Pts',(-7.57978263261094,2.26513515914518,
126.555404443827));
#230334=CARTESIAN_POINT('Ctrl Pts',(-7.57846778156442,2.26953037664025,
126.555219025959));
#230335=CARTESIAN_POINT('Ctrl Pts',(-7.57544770128083,2.2795938590567,126.554793979892));
#230336=CARTESIAN_POINT('Ctrl Pts',(-7.5737399334249,2.2852613543439,126.554554237531));
#230337=CARTESIAN_POINT('Ctrl Pts',(-7.56902133132096,2.30085738958276,
126.553893503882));
#230338=CARTESIAN_POINT('Ctrl Pts',(-7.56599733051227,2.3107819097504,126.553471928932));
#230339=CARTESIAN_POINT('Ctrl Pts',(-7.54981573579065,2.363516270765,126.551226031607));
#230340=CARTESIAN_POINT('Ctrl Pts',(-7.53631446872862,2.40621921828136,
126.549386881569));
#230341=CARTESIAN_POINT('Ctrl Pts',(-7.39096090504319,2.85272896677761,
126.529957533555));
#230342=CARTESIAN_POINT('Ctrl Pts',(-7.22715509754713,3.2453918524543,126.511208152868));
#230343=CARTESIAN_POINT('Ctrl Pts',(-6.86000178534438,3.95807821467675,
126.475898437962));
#230344=CARTESIAN_POINT('Ctrl Pts',(-6.66363747992839,4.28041658329275,
126.45936982166));
#230345=CARTESIAN_POINT('Ctrl Pts',(-6.27435983061465,4.82731319347053,
126.43079429022));
#230346=CARTESIAN_POINT('Ctrl Pts',(-6.09043360899482,5.05738840377083,
126.41857293624));
#230347=CARTESIAN_POINT('Ctrl Pts',(-5.87027557670261,5.30330670016279,
126.405211577054));
#230348=CARTESIAN_POINT('Ctrl Pts',(-5.84626637383349,5.32976235996558,
126.403769856501));
#230349=CARTESIAN_POINT('Ctrl Pts',(-5.81086544632176,5.36824348084719,
126.401666042111));
#230350=CARTESIAN_POINT('Ctrl Pts',(-5.79961395061265,5.38039713508329,
126.401000586597));
#230351=CARTESIAN_POINT('Ctrl Pts',(-5.77958303694581,5.4018983115835,126.399821490751));
#230352=CARTESIAN_POINT('Ctrl Pts',(-5.77081891160866,5.41125997713755,
126.399307489167));
#230353=CARTESIAN_POINT('Ctrl Pts',(-5.75253539013836,5.430695137577,126.39823907915));
#230354=CARTESIAN_POINT('Ctrl Pts',(-5.74301220427366,5.44076501192947,
126.397684762572));
#230355=CARTESIAN_POINT('Ctrl Pts',(-5.71828436490337,5.46677511802796,
126.396251000655));
#230356=CARTESIAN_POINT('Ctrl Pts',(-5.7030394825771,5.48267698615574,126.395372498548));
#230357=CARTESIAN_POINT('Ctrl Pts',(-5.64018706117961,5.54769226704856,
126.3917723908));
#230358=CARTESIAN_POINT('Ctrl Pts',(-5.59200937496956,5.59625150501233,
126.389063644655));
#230359=CARTESIAN_POINT('Ctrl Pts',(-5.28132847130631,5.9013744344875,126.371910686583));
#230360=CARTESIAN_POINT('Ctrl Pts',(-5.00186045676111,6.14003766881747,
126.357914364024));
#230361=CARTESIAN_POINT('Ctrl Pts',(-4.20805161089058,6.72765252395125,
126.321041319045));
#230362=CARTESIAN_POINT('Ctrl Pts',(-3.66760652037844,7.03687367189595,
126.298944615369));
#230363=CARTESIAN_POINT('Ctrl Pts',(-3.03316223698029,7.30675061343535,
126.272497743083));
#230364=CARTESIAN_POINT('Ctrl Pts',(-2.9693473124092,7.33291578826961,126.269830195637));
#230365=CARTESIAN_POINT('Ctrl Pts',(-2.83060933891404,7.38769265284646,
126.264002142958));
#230366=CARTESIAN_POINT('Ctrl Pts',(-2.75557729732104,7.41600601436807,
126.260832426404));
#230367=CARTESIAN_POINT('Ctrl Pts',(-2.66780466630403,7.44761108379233,
126.257092841365));
#230368=CARTESIAN_POINT('Ctrl Pts',(-2.65546900418735,7.45201831440564,
126.256566553534));
#230369=CARTESIAN_POINT('Ctrl Pts',(-2.63579973910678,7.45899062179729,
126.255726168407));
#230370=CARTESIAN_POINT('Ctrl Pts',(-2.62847317615797,7.46157557908572,
126.255412866643));
#230371=CARTESIAN_POINT('Ctrl Pts',(-2.61555026313918,7.46611364464712,
126.254859762644));
#230372=CARTESIAN_POINT('Ctrl Pts',(-2.60995549682393,7.46807126627389,
126.254620143966));
#230373=CARTESIAN_POINT('Ctrl Pts',(-2.59839782086855,7.4721007496869,126.254124798445));
#230374=CARTESIAN_POINT('Ctrl Pts',(-2.59243462225202,7.47417176535386,
126.253869037066));
#230375=CARTESIAN_POINT('Ctrl Pts',(-2.57719177669453,7.47944516079605,
126.253214781764));
#230376=CARTESIAN_POINT('Ctrl Pts',(-2.56790865275239,7.48263740382877,
126.25281586661));
#230377=CARTESIAN_POINT('Ctrl Pts',(-2.53025175244799,7.49550837629793,
126.251195719941));
#230378=CARTESIAN_POINT('Ctrl Pts',(-2.50182925168449,7.50504297860175,
126.249968387091));
#230379=CARTESIAN_POINT('Ctrl Pts',(-1.96233797832857,7.68261535319951,
126.226577702406));
#230380=CARTESIAN_POINT('Ctrl Pts',(-1.43560690508122,7.79821362571434,
126.201763077198));
#230381=CARTESIAN_POINT('Ctrl Pts',(-0.242384383227391,7.93505644900924,
126.146467779436));
#230382=CARTESIAN_POINT('Ctrl Pts',(0.423580290964235,7.92746650860418,
126.116472646456));
#230383=CARTESIAN_POINT('Ctrl Pts',(1.1191512611547,7.83153344762973,126.087793321047));
#230384=CARTESIAN_POINT('Ctrl Pts',(1.15741101766778,7.82597057751608,126.086223319548));
#230385=CARTESIAN_POINT('Ctrl Pts',(1.20974125700984,7.81796974329931,126.084086086151));
#230386=CARTESIAN_POINT('Ctrl Pts',(1.22384786437571,7.81577387235536,126.083510966305));
#230387=CARTESIAN_POINT('Ctrl Pts',(1.24675004053743,7.81214533582886,126.082578889327));
#230388=CARTESIAN_POINT('Ctrl Pts',(1.25554923730463,7.8107359784526,126.082221170149));
#230389=CARTESIAN_POINT('Ctrl Pts',(1.2711831518416,7.80820481069186,126.08158628911));
#230390=CARTESIAN_POINT('Ctrl Pts',(1.2780188052648,7.80708888798852,126.081308934571));
#230391=CARTESIAN_POINT('Ctrl Pts',(1.29236970587251,7.80472674569952,126.08072714508));
#230392=CARTESIAN_POINT('Ctrl Pts',(1.29988463863055,7.80347864470588,126.080422772211));
#230393=CARTESIAN_POINT('Ctrl Pts',(1.31959816694817,7.80017529975924,126.079625070633));
#230394=CARTESIAN_POINT('Ctrl Pts',(1.33179378740152,7.79810229087045,126.079132326472));
#230395=CARTESIAN_POINT('Ctrl Pts',(1.38563700533262,7.78882003769183,126.076960158398));
#230396=CARTESIAN_POINT('Ctrl Pts',(1.42723167206808,7.78130563064428,126.075290803443));
#230397=CARTESIAN_POINT('Ctrl Pts',(1.71886458447717,7.72620273096711,126.063645608632));
#230398=CARTESIAN_POINT('Ctrl Pts',(1.96654838197397,7.66690325542648,126.054068337391));
#230399=CARTESIAN_POINT('Ctrl Pts',(2.49584048831774,7.51283806250312,126.034052310584));
#230400=CARTESIAN_POINT('Ctrl Pts',(2.77584130099618,7.41395125901815,126.023752515233));
#230401=CARTESIAN_POINT('Ctrl Pts',(3.61632879469066,7.06280977758361,125.992773847716));
#230402=CARTESIAN_POINT('Ctrl Pts',(4.15346714379324,6.76089412248895,125.972994549617));
#230403=CARTESIAN_POINT('Ctrl Pts',(4.78049522831162,6.30529257617258,125.944337511789));
#230404=CARTESIAN_POINT('Ctrl Pts',(4.90783321278726,6.2066912423356,125.93818072848));
#230405=CARTESIAN_POINT('Ctrl Pts',(5.04180582154404,6.09625084585802,125.931230435219));
#230406=CARTESIAN_POINT('Ctrl Pts',(5.05152600353584,6.08819885924942,125.930723405208));
#230407=CARTESIAN_POINT('Ctrl Pts',(5.06499450138001,6.0769873895547,125.930016948436));
#230408=CARTESIAN_POINT('Ctrl Pts',(5.06875925986301,6.07384759416623,125.929819052233));
#230409=CARTESIAN_POINT('Ctrl Pts',(5.07523295571971,6.06843834392309,125.92947802287));
#230410=CARTESIAN_POINT('Ctrl Pts',(5.07794329912441,6.06617056631375,125.929335021411));
#230411=CARTESIAN_POINT('Ctrl Pts',(5.0832410797306,6.06173180975138,125.929055065595));
#230412=CARTESIAN_POINT('Ctrl Pts',(5.08582864712844,6.0595609890459,125.928918123732));
#230413=CARTESIAN_POINT('Ctrl Pts',(5.09198807914528,6.05438685417333,125.928591658655));
#230414=CARTESIAN_POINT('Ctrl Pts',(5.09555865380275,6.05138205567481,125.928402016528));
#230415=CARTESIAN_POINT('Ctrl Pts',(5.10646400061859,6.04218822222675,125.927821602148));
#230416=CARTESIAN_POINT('Ctrl Pts',(5.11379011570926,6.03598904515685,125.927430020175));
#230417=CARTESIAN_POINT('Ctrl Pts',(5.13061987867352,6.02169548379129,125.926526672995));
#230418=CARTESIAN_POINT('Ctrl Pts',(5.14011566234969,6.01359192272387,125.926014187021));
#230419=CARTESIAN_POINT('Ctrl Pts',(5.22977800981316,5.93670787657084,125.92114901409));
#230420=CARTESIAN_POINT('Ctrl Pts',(5.30857532463509,5.8663535969376,125.916675488758));
#230421=CARTESIAN_POINT('Ctrl Pts',(5.56386229537344,5.629064390629,125.901596668344));
#230422=CARTESIAN_POINT('Ctrl Pts',(5.73406596567516,5.4555845485758,125.890590673001));
#230423=CARTESIAN_POINT('Ctrl Pts',(6.48542865046835,4.61569677749745,125.838603978893));
#230424=CARTESIAN_POINT('Ctrl Pts',(6.96044867438516,3.86243057686019,125.796530733588));
#230425=CARTESIAN_POINT('Ctrl Pts',(7.3227405149124,2.99408999409558,125.757970640054));
#230426=CARTESIAN_POINT('Ctrl Pts',(7.34390566987932,2.94179422116596,125.755678995068));
#230427=CARTESIAN_POINT('Ctrl Pts',(7.36912031472889,2.87752430720629,125.752899412685));
#230428=CARTESIAN_POINT('Ctrl Pts',(7.37370256471094,2.86576182554553,125.752392199559));
#230429=CARTESIAN_POINT('Ctrl Pts',(7.38122018740419,2.8463269357938,125.751556601288));
#230430=CARTESIAN_POINT('Ctrl Pts',(7.38417178995237,2.83866085635588,125.751227630263));
#230431=CARTESIAN_POINT('Ctrl Pts',(7.38947458345409,2.82482388619503,125.750634983135));
#230432=CARTESIAN_POINT('Ctrl Pts',(7.39182999628302,2.81865462834243,125.750371154981));
#230433=CARTESIAN_POINT('Ctrl Pts',(7.39684247611021,2.80547653121,125.749808457064));
#230434=CARTESIAN_POINT('Ctrl Pts',(7.39949731320232,2.7984668473823,125.749509667759));
#230435=CARTESIAN_POINT('Ctrl Pts',(7.40663135107487,2.77954940353425,125.748704706606));
#230436=CARTESIAN_POINT('Ctrl Pts',(7.41109180531551,2.76763456993157,125.74819920882));
#230437=CARTESIAN_POINT('Ctrl Pts',(7.43274263263046,2.70937289584864,125.745734652526));
#230438=CARTESIAN_POINT('Ctrl Pts',(7.44952727736881,2.66287588808511,125.743790149399));
#230439=CARTESIAN_POINT('Ctrl Pts',(7.52666926068978,2.44273708639808,125.734686542393));
#230440=CARTESIAN_POINT('Ctrl Pts',(7.58139981358505,2.26717819798533,125.727728087577));
#230441=CARTESIAN_POINT('Ctrl Pts',(7.68390267132705,1.89294645775595,125.713428158753));
#230442=CARTESIAN_POINT('Ctrl Pts',(7.73019685524648,1.69400959082773,125.706135425957));
#230443=CARTESIAN_POINT('Ctrl Pts',(7.8906155727032,0.859557701313235,125.676411561693));
#230444=CARTESIAN_POINT('Ctrl Pts',(7.93442306835519,0.213160889392909,
125.655658793264));
#230445=CARTESIAN_POINT('Ctrl Pts',(7.88902818395549,-0.618216988985789,
125.625194202305));
#230446=CARTESIAN_POINT('Ctrl Pts',(7.87219328848059,-0.804687226644158,
125.618097166479));
#230447=CARTESIAN_POINT('Ctrl Pts',(7.84712950857229,-1.00331938405422,
125.610084652234));
#230448=CARTESIAN_POINT('Ctrl Pts',(7.84546374974153,-1.01626269274336,
125.609560462585));
#230449=CARTESIAN_POINT('Ctrl Pts',(7.84310285809497,-1.03425554626636,
125.608828850098));
#230450=CARTESIAN_POINT('Ctrl Pts',(7.84243489118831,-1.039308402198,125.608623076003));
#230451=CARTESIAN_POINT('Ctrl Pts',(7.84127352707207,-1.04802870538149,
125.608267401965));
#230452=CARTESIAN_POINT('Ctrl Pts',(7.84078243810846,-1.05169646372878,
125.608117638843));
#230453=CARTESIAN_POINT('Ctrl Pts',(7.83976133595189,-1.05928222254363,
125.607807551754));
#230454=CARTESIAN_POINT('Ctrl Pts',(7.83923095876655,-1.06320017244497,
125.60764720639));
#230455=CARTESIAN_POINT('Ctrl Pts',(7.83800044054134,-1.07223915677601,
125.607276844314));
#230456=CARTESIAN_POINT('Ctrl Pts',(7.83729821802299,-1.07735990123007,
125.607066706063));
#230457=CARTESIAN_POINT('Ctrl Pts',(7.83506463134977,-1.09352990539793,
125.606402135226));
#230458=CARTESIAN_POINT('Ctrl Pts',(7.83351492122607,-1.10457657404098,
125.605946641682));
#230459=CARTESIAN_POINT('Ctrl Pts',(7.82985426549375,-1.13027532998632,
125.604883588209));
#230460=CARTESIAN_POINT('Ctrl Pts',(7.82772555260544,-1.1449248044948,125.604275023228));
#230461=CARTESIAN_POINT('Ctrl Pts',(7.80588674127882,-1.29230798273358,
125.598127122476));
#230462=CARTESIAN_POINT('Ctrl Pts',(7.78284450949898,-1.42451936879187,
125.592405240124));
#230463=CARTESIAN_POINT('Ctrl Pts',(7.71766242252076,-1.74942798209611,
125.577936324642));
#230464=CARTESIAN_POINT('Ctrl Pts',(7.6716576810272,-1.94125538724996,125.569036602514));
#230465=CARTESIAN_POINT('Ctrl Pts',(7.61139715877473,-2.15667724440141,
125.558775271194));
#230466=CARTESIAN_POINT('Ctrl Pts',(7.60412911015608,-2.18216495924209,
125.557556878738));
#230467=CARTESIAN_POINT('Ctrl Pts',(7.33933782944703,-3.09335109922466,
125.513854436762));
#230468=CARTESIAN_POINT('Ctrl Pts',(6.92890690384614,-3.92756140772201,
125.470039969002));
#230469=CARTESIAN_POINT('Ctrl Pts',(6.34918129601219,-4.71966878076143,
125.429720159627));
#230470=CARTESIAN_POINT('Ctrl Pts',(6.31393553024771,-4.76671740775451,
125.427326073275));
#230471=CARTESIAN_POINT('Ctrl Pts',(6.26993631507333,-4.82410640934887,
125.424406056187));
#230472=CARTESIAN_POINT('Ctrl Pts',(6.26167694933377,-4.83482221269164,
125.423860833575));
#230473=CARTESIAN_POINT('Ctrl Pts',(6.24795055717997,-4.8525368318491,125.422959510497));
#230474=CARTESIAN_POINT('Ctrl Pts',(6.24249917792306,-4.85954770361516,
125.422602796284));
#230475=CARTESIAN_POINT('Ctrl Pts',(6.23261263798222,-4.87221842786834,
125.421958103453));
#230476=CARTESIAN_POINT('Ctrl Pts',(6.22818154835895,-4.87788143613881,
125.421669965117));
#230477=CARTESIAN_POINT('Ctrl Pts',(6.21866957763577,-4.89000380598412,
125.421053162674));
#230478=CARTESIAN_POINT('Ctrl Pts',(6.21358633757495,-4.89646131041344,
125.420724592106));
#230479=CARTESIAN_POINT('Ctrl Pts',(6.1997614458816,-4.91396759303291,125.419833820536));
#230480=CARTESIAN_POINT('Ctrl Pts',(6.19100030819866,-4.92500098250914,
125.419272390178));
#230481=CARTESIAN_POINT('Ctrl Pts',(6.14695158364825,-4.98017072500174,
125.416464940225));
#230482=CARTESIAN_POINT('Ctrl Pts',(6.11122088074866,-5.02395200349827,
125.414236534867));
#230483=CARTESIAN_POINT('Ctrl Pts',(5.7011711531951,-5.51554290317883,125.389199272512));
#230484=CARTESIAN_POINT('Ctrl Pts',(5.27884737525716,-5.92101422831183,
125.368570731182));
#230485=CARTESIAN_POINT('Ctrl Pts',(4.62759298230258,-6.42071255103389,
125.340091601594));
#230486=CARTESIAN_POINT('Ctrl Pts',(4.43304170897174,-6.55654676419223,
125.331916077587));
#230487=CARTESIAN_POINT('Ctrl Pts',(3.9029302434727,-6.89227159343943,125.309869422917));
#230488=CARTESIAN_POINT('Ctrl Pts',(3.55816876208995,-7.07642026883306,
125.295702547856));
#230489=CARTESIAN_POINT('Ctrl Pts',(3.17654355457447,-7.24528948411616,
125.279114606962));
#230490=CARTESIAN_POINT('Ctrl Pts',(3.15182002323524,-7.25607877455861,
125.278037265548));
#230491=CARTESIAN_POINT('Ctrl Pts',(3.11829418162056,-7.27050569708356,
125.276573105993));
#230492=CARTESIAN_POINT('Ctrl Pts',(3.10953961624805,-7.2742542620215,125.276190472615));
#230493=CARTESIAN_POINT('Ctrl Pts',(3.09472605600223,-7.28056556300747,
125.275542535977));
#230494=CARTESIAN_POINT('Ctrl Pts',(3.08867058271744,-7.28313657088273,
125.275277536421));
#230495=CARTESIAN_POINT('Ctrl Pts',(3.07653209712454,-7.28827241785366,
125.274746066624));
#230496=CARTESIAN_POINT('Ctrl Pts',(3.07044906753319,-7.29083720191749,
125.274479594698));
#230497=CARTESIAN_POINT('Ctrl Pts',(3.05672608281624,-7.29660299523593,
125.273878156989));
#230498=CARTESIAN_POINT('Ctrl Pts',(3.04908430099351,-7.29979962329984,
125.273543036924));
#230499=CARTESIAN_POINT('Ctrl Pts',(3.0330918954078,-7.30645990092626,125.272841302842));
#230500=CARTESIAN_POINT('Ctrl Pts',(3.02474032887015,-7.30992124937225,
125.272474610134));
#230501=CARTESIAN_POINT('Ctrl Pts',(3.00290228599648,-7.31892830274964,
125.271515185256));
#230502=CARTESIAN_POINT('Ctrl Pts',(2.98940640453432,-7.32445103647046,
125.270921684209));
#230503=CARTESIAN_POINT('Ctrl Pts',(2.94924672293705,-7.3407555450251,125.269154013925));
#230504=CARTESIAN_POINT('Ctrl Pts',(2.92253943223886,-7.35142921142041,
125.267976386931));
#230505=CARTESIAN_POINT('Ctrl Pts',(2.60007143107992,-7.47826976341001,
125.25373636806));
#230506=CARTESIAN_POINT('Ctrl Pts',(2.29763746982637,-7.57665751945182,
125.240181771873));
#230507=CARTESIAN_POINT('Ctrl Pts',(1.45057484115349,-7.79682816944643,
125.202597374796));
#230508=CARTESIAN_POINT('Ctrl Pts',(0.897688609357691,-7.87965090294242,
125.178601302641));
#230509=CARTESIAN_POINT('Ctrl Pts',(0.0971795667018823,-7.91415727650146,
125.145046872331));
#230510=CARTESIAN_POINT('Ctrl Pts',(-0.146689868489533,-7.91339462922862,
125.134955670431));
#230511=CARTESIAN_POINT('Ctrl Pts',(-0.64365607723417,-7.88885644262455,
125.114465558586));
#230512=CARTESIAN_POINT('Ctrl Pts',(-0.896429603056834,-7.86414441545999,
125.104070149568));
#230513=CARTESIAN_POINT('Ctrl Pts',(-1.18672555369331,-7.82158352019872,
125.092194347674));
#230514=CARTESIAN_POINT('Ctrl Pts',(-1.22582750031856,-7.81555073313311,
125.090595930217));
#230515=CARTESIAN_POINT('Ctrl Pts',(-1.28971095214331,-7.80520334624525,
125.087986425344));
#230516=CARTESIAN_POINT('Ctrl Pts',(-1.31451996793325,-7.80106344515821,
125.086973507251));
#230517=CARTESIAN_POINT('Ctrl Pts',(-1.35899786597839,-7.79342318211579,
125.085158363482));
#230518=CARTESIAN_POINT('Ctrl Pts',(-1.37867401338701,-7.78996649946024,
125.084355670738));
#230519=CARTESIAN_POINT('Ctrl Pts',(-1.42049180787295,-7.78245659765812,
125.082650299644));
#230520=CARTESIAN_POINT('Ctrl Pts',(-1.44262968623985,-7.77838333221277,
125.081747850522));
#230521=CARTESIAN_POINT('Ctrl Pts',(-1.50213999685694,-7.76717091840272,
125.079322818319));
#230522=CARTESIAN_POINT('Ctrl Pts',(-1.53947888135586,-7.75985653464033,
125.077802227096));
#230523=CARTESIAN_POINT('Ctrl Pts',(-1.72718887287239,-7.72167750091729,
125.070162110732));
#230524=CARTESIAN_POINT('Ctrl Pts',(-1.87669336224166,-7.68670983110924,
125.064091345553));
#230525=CARTESIAN_POINT('Ctrl Pts',(-2.30394429057833,-7.5735708609033,
125.046743009256));
#230526=CARTESIAN_POINT('Ctrl Pts',(-2.57855601481965,-7.48452993172522,
125.035599852609));
#230527=CARTESIAN_POINT('Ctrl Pts',(-3.08357957310658,-7.28967647439913,
125.014780023421));
#230528=CARTESIAN_POINT('Ctrl Pts',(-3.31496465206026,-7.1874093931488,
125.005102184807));
#230529=CARTESIAN_POINT('Ctrl Pts',(-3.73716307085386,-6.97607543468883,
124.98682640429));
#230530=CARTESIAN_POINT('Ctrl Pts',(-3.9291014515391,-6.86980152526605,
124.978262080794));
#230531=CARTESIAN_POINT('Ctrl Pts',(-4.13703042743721,-6.74310651858173,
124.9685227118));
#230532=CARTESIAN_POINT('Ctrl Pts',(-4.15763202068206,-6.73042363120194,
124.96755251749));
#230533=CARTESIAN_POINT('Ctrl Pts',(-4.1885546364534,-6.71119068935444,
124.966088102444));
#230534=CARTESIAN_POINT('Ctrl Pts',(-4.19891916745838,-6.7047108987106,
124.96559588623));
#230535=CARTESIAN_POINT('Ctrl Pts',(-4.21741437817623,-6.69308819004384,
124.964715104109));
#230536=CARTESIAN_POINT('Ctrl Pts',(-4.22555078204119,-6.6879544065977,
124.964326785112));
#230537=CARTESIAN_POINT('Ctrl Pts',(-4.24322686942633,-6.67675628701435,
124.963481350817));
#230538=CARTESIAN_POINT('Ctrl Pts',(-4.25276295636639,-6.67068632283051,
124.963024088149));
#230539=CARTESIAN_POINT('Ctrl Pts',(-4.27808715726214,-6.6544904443003,
124.961806724255));
#230540=CARTESIAN_POINT('Ctrl Pts',(-4.29385229608871,-6.64432880384139,
124.961045714642));
#230541=CARTESIAN_POINT('Ctrl Pts',(-4.36754330930282,-6.59645842799155,
124.957473969921));
#230542=CARTESIAN_POINT('Ctrl Pts',(-4.4250090261526,-6.5580479782329,124.954646380474));
#230543=CARTESIAN_POINT('Ctrl Pts',(-4.58510779903765,-6.44797450463757,
124.94665712134));
#230544=CARTESIAN_POINT('Ctrl Pts',(-4.68655337529715,-6.37462198529496,
124.941463532283));
#230545=CARTESIAN_POINT('Ctrl Pts',(-5.10302764582345,-6.05816404192636,
124.919648133921));
#230546=CARTESIAN_POINT('Ctrl Pts',(-5.4012281631724,-5.79387438274418,
124.902838930953));
#230547=CARTESIAN_POINT('Ctrl Pts',(-5.845150387183,-5.33625109209956,124.876237546936));
#230548=CARTESIAN_POINT('Ctrl Pts',(-6.00412150467398,-5.15673226477471,
124.866320311031));
#230549=CARTESIAN_POINT('Ctrl Pts',(-6.22816821441472,-4.87929461809403,
124.85172904736));
#230550=CARTESIAN_POINT('Ctrl Pts',(-6.29961111500287,-4.78669986413973,
124.84697174565));
#230551=CARTESIAN_POINT('Ctrl Pts',(-6.39291386402894,-4.66006458744514,
124.84060828002));
#230552=CARTESIAN_POINT('Ctrl Pts',(-6.4166030629926,-4.62739179070427,
124.838978869244));
#230553=CARTESIAN_POINT('Ctrl Pts',(-6.45360327963279,-4.57552958646275,
124.836411546804));
#230554=CARTESIAN_POINT('Ctrl Pts',(-6.46708105707976,-4.55646012739608,
124.835471578598));
#230555=CARTESIAN_POINT('Ctrl Pts',(-6.49300110364074,-4.51943964445777,
124.833654425817));
#230556=CARTESIAN_POINT('Ctrl Pts',(-6.50545385162708,-4.50149622006467,
124.83277712069));
#230557=CARTESIAN_POINT('Ctrl Pts',(-6.53495007711042,-4.45861646415103,
124.830688686846));
#230558=CARTESIAN_POINT('Ctrl Pts',(-6.5519253836605,-4.43363361811748,
124.829478377923));
#230559=CARTESIAN_POINT('Ctrl Pts',(-6.60258213841443,-4.35815492018115,
124.825840736919));
#230560=CARTESIAN_POINT('Ctrl Pts',(-6.63582601931868,-4.30736790917346,
124.823418461358));
#230561=CARTESIAN_POINT('Ctrl Pts',(-6.86437293930103,-3.94928794181919,
124.806507319531));
#230562=CARTESIAN_POINT('Ctrl Pts',(-7.03884933118497,-3.62920176066911,
124.79218606703));
#230563=CARTESIAN_POINT('Ctrl Pts',(-7.2831758316515,-3.09653266062842,
124.769528622915));
#230564=CARTESIAN_POINT('Ctrl Pts',(-7.36716716733706,-2.89102336224576,
124.761060749494));
#230565=CARTESIAN_POINT('Ctrl Pts',(-7.65413306094499,-2.09478266867559,
124.7291235553));
#230566=CARTESIAN_POINT('Ctrl Pts',(-7.79554110652291,-1.48435692690218,
124.706647573883));
#230567=CARTESIAN_POINT('Ctrl Pts',(-7.867901392112,-0.825543785212832,
124.681116428796));
#230568=CARTESIAN_POINT('Ctrl Pts',(-7.87181494712228,-0.787352686920916,
124.679630987546));
#230569=CARTESIAN_POINT('Ctrl Pts',(-7.88413564961273,-0.657828510897786,
124.67457114074));
#230570=CARTESIAN_POINT('Ctrl Pts',(-7.89123225152605,-0.566379839892654,
124.670961737013));
#230571=CARTESIAN_POINT('Ctrl Pts',(-7.89757522177108,-0.460892176095586,
124.66673776609));
#230572=CARTESIAN_POINT('Ctrl Pts',(-7.89837642923913,-0.446951631147566,
124.666178337471));
#230573=CARTESIAN_POINT('Ctrl Pts',(-7.89958770502583,-0.424855009915973,
124.665289590344));
#230574=CARTESIAN_POINT('Ctrl Pts',(-7.90002206211765,-0.416700259522344,
124.664961162986));
#230575=CARTESIAN_POINT('Ctrl Pts',(-7.90075589471278,-0.402509399242728,
124.664388857424));
#230576=CARTESIAN_POINT('Ctrl Pts',(-7.90106108202511,-0.396473583194797,
124.664145193218));
#230577=CARTESIAN_POINT('Ctrl Pts',(-7.90163835793126,-0.384791136831793,
124.663673093381));
#230578=CARTESIAN_POINT('Ctrl Pts',(-7.90191131102326,-0.379144551623895,
124.66344469075));
#230579=CARTESIAN_POINT('Ctrl Pts',(-7.90247644215173,-0.367187939756693,
124.662960579307));
#230580=CARTESIAN_POINT('Ctrl Pts',(-7.90276711538835,-0.360877848446002,
124.662704812686));
#230581=CARTESIAN_POINT('Ctrl Pts',(-7.90344019104552,-0.345875481302911,
124.662096050663));
#230582=CARTESIAN_POINT('Ctrl Pts',(-7.90381581133093,-0.337182920321436,
124.661742790166));
#230583=CARTESIAN_POINT('Ctrl Pts',(-7.90477362281569,-0.314135897118142,
124.660804714397));
#230584=CARTESIAN_POINT('Ctrl Pts',(-7.90533105252766,-0.299780479742971,
124.660218910609));
#230585=CARTESIAN_POINT('Ctrl Pts',(-7.90928581584208,-0.190238895561674,
124.655736901715));
#230586=CARTESIAN_POINT('Ctrl Pts',(-7.91100275360645,-0.0950102628663944,
124.6517680464));
#230587=CARTESIAN_POINT('Ctrl Pts',(-7.9109999966855,0.000229002203636593,
124.647722132928));
#230588=CARTESIAN_POINT('',(-7.91099929352038,0.00334333966528006,120.642331508237));
#230589=CARTESIAN_POINT('Ctrl Pts',(-7.9109999968515,0.000223194498397833,
124.647722379649));
#230590=CARTESIAN_POINT('Ctrl Pts',(-7.9109779547213,0.781493759624896,
124.614532803849));
#230591=CARTESIAN_POINT('Ctrl Pts',(-7.79522920292053,1.55848580366607,
124.577023027943));
#230592=CARTESIAN_POINT('Ctrl Pts',(-7.47181302200089,2.61985210386416,
124.527212159827));
#230593=CARTESIAN_POINT('Ctrl Pts',(-7.35671161125456,2.92753127098832,
124.512897498815));
#230594=CARTESIAN_POINT('Ctrl Pts',(-7.21432761035792,3.24620264622964,
124.498308490905));
#230595=CARTESIAN_POINT('Ctrl Pts',(-7.20575912924286,3.26517838250959,
124.497440615841));
#230596=CARTESIAN_POINT('Ctrl Pts',(-7.15602231928925,3.3741760935384,124.492460348662));
#230597=CARTESIAN_POINT('Ctrl Pts',(-7.11324132989328,3.46345469444898,
124.488400335366));
#230598=CARTESIAN_POINT('Ctrl Pts',(-7.06108777803045,3.56724754729824,
124.483701071417));
#230599=CARTESIAN_POINT('Ctrl Pts',(-7.05333057653428,3.58256101908969,
124.483008281119));
#230600=CARTESIAN_POINT('Ctrl Pts',(-7.04138885304668,3.6059460166166,124.48195112539));
#230601=CARTESIAN_POINT('Ctrl Pts',(-7.03724018074677,3.6140357349824,124.481585562906));
#230602=CARTESIAN_POINT('Ctrl Pts',(-7.02966017629616,3.62875385151286,
124.480920734683));
#230603=CARTESIAN_POINT('Ctrl Pts',(-7.02623339412023,3.63538457398943,
124.480621317035));
#230604=CARTESIAN_POINT('Ctrl Pts',(-7.01881700278139,3.64968541504211,
124.479975753209));
#230605=CARTESIAN_POINT('Ctrl Pts',(-7.01482419166842,3.65735386691965,
124.479629715001));
#230606=CARTESIAN_POINT('Ctrl Pts',(-7.00399690581999,3.67806541196798,
124.478695450042));
#230607=CARTESIAN_POINT('Ctrl Pts',(-6.99713855775811,3.69109602121912,
124.478108026931));
#230608=CARTESIAN_POINT('Ctrl Pts',(-6.965027527371,3.75169467706055,124.47537788186));
#230609=CARTESIAN_POINT('Ctrl Pts',(-6.93932564449243,3.79902370942493,
124.473250351369));
#230610=CARTESIAN_POINT('Ctrl Pts',(-6.49044987221057,4.60585462122559,
124.437052605469));
#230611=CARTESIAN_POINT('Ctrl Pts',(-5.94546002243732,5.29068073938031,
124.408192297818));
#230612=CARTESIAN_POINT('Ctrl Pts',(-5.15244489468381,6.00630827580459,
124.370743145328));
#230613=CARTESIAN_POINT('Ctrl Pts',(-4.99992161593218,6.13385737063263,
124.363667144406));
#230614=CARTESIAN_POINT('Ctrl Pts',(-4.72974173976885,6.34301926840573,
124.351086125048));
#230615=CARTESIAN_POINT('Ctrl Pts',(-4.61437451620979,6.42743299954095,
124.345700058648));
#230616=CARTESIAN_POINT('Ctrl Pts',(-4.46187281779876,6.53279519216821,
124.338487462888));
#230617=CARTESIAN_POINT('Ctrl Pts',(-4.42676342051837,6.55663691562303,
124.336820743516));
#230618=CARTESIAN_POINT('Ctrl Pts',(-4.37620780220931,6.59037652112767,
124.334409797168));
#230619=CARTESIAN_POINT('Ctrl Pts',(-4.36091630829756,6.60050500807277,
124.333679174745));
#230620=CARTESIAN_POINT('Ctrl Pts',(-4.33734526110926,6.61599988151902,
124.332551005164));
#230621=CARTESIAN_POINT('Ctrl Pts',(-4.32909058793893,6.62140415821417,
124.332155549122));
#230622=CARTESIAN_POINT('Ctrl Pts',(-4.31370567184137,6.63143548764466,
124.331417855976));
#230623=CARTESIAN_POINT('Ctrl Pts',(-4.3065780317186,6.63606652362331,124.331075833448));
#230624=CARTESIAN_POINT('Ctrl Pts',(-4.29486682013669,6.64364882548795,
124.330513460949));
#230625=CARTESIAN_POINT('Ctrl Pts',(-4.290287624824,6.64660686479829,124.330293466414));
#230626=CARTESIAN_POINT('Ctrl Pts',(-4.28150357158588,6.65226827146771,
124.329871272427));
#230627=CARTESIAN_POINT('Ctrl Pts',(-4.27729920021973,6.65497239218263,
124.329669112033));
#230628=CARTESIAN_POINT('Ctrl Pts',(-4.26754069604263,6.66123569045777,
124.329199703399));
#230629=CARTESIAN_POINT('Ctrl Pts',(-4.2619846737903,6.66479190644462,124.328932304617));
#230630=CARTESIAN_POINT('Ctrl Pts',(-4.24466179740084,6.675849155748,124.328098173599));
#230631=CARTESIAN_POINT('Ctrl Pts',(-4.23287958013209,6.68332598196764,
124.327530233364));
#230632=CARTESIAN_POINT('Ctrl Pts',(-4.14063557463364,6.74152093161513,
124.32307945167));
#230633=CARTESIAN_POINT('Ctrl Pts',(-4.05928678219419,6.79081418519741,
124.319128777842));
#230634=CARTESIAN_POINT('Ctrl Pts',(-3.73132011221571,6.9815464442122,124.303158560153));
#230635=CARTESIAN_POINT('Ctrl Pts',(-3.47805134277313,7.11111020427043,
124.290740059382));
#230636=CARTESIAN_POINT('Ctrl Pts',(-2.98296903435455,7.33159058642938,
124.266910467727));
#230637=CARTESIAN_POINT('Ctrl Pts',(-2.74258321459801,7.42486126728823,
124.255526911098));
#230638=CARTESIAN_POINT('Ctrl Pts',(-2.03509896471989,7.66031191385824,
124.222969203287));
#230639=CARTESIAN_POINT('Ctrl Pts',(-1.55883606936582,7.77123575444322,
124.20228203286));
#230640=CARTESIAN_POINT('Ctrl Pts',(-1.03333637487193,7.84333703034172,
124.180773679725));
#230641=CARTESIAN_POINT('Ctrl Pts',(-0.991271441883657,7.84876428529563,
124.179060209349));
#230642=CARTESIAN_POINT('Ctrl Pts',(-0.9313419451915,7.85600696723329,124.176630097689));
#230643=CARTESIAN_POINT('Ctrl Pts',(-0.913511921898627,7.85810023222889,
124.175908488046));
#230644=CARTESIAN_POINT('Ctrl Pts',(-0.882750407504784,7.86160555670332,
124.174665849921));
#230645=CARTESIAN_POINT('Ctrl Pts',(-0.869822295907359,7.86304644433966,
124.174144316529));
#230646=CARTESIAN_POINT('Ctrl Pts',(-0.84507559853392,7.86574278030027,
124.173147336595));
#230647=CARTESIAN_POINT('Ctrl Pts',(-0.833257626124414,7.86700349449899,
124.172671800173));
#230648=CARTESIAN_POINT('Ctrl Pts',(-0.805567205088771,7.86989434924505,
124.171558909382));
#230649=CARTESIAN_POINT('Ctrl Pts',(-0.789692563204766,7.87150311235881,
124.170921921583));
#230650=CARTESIAN_POINT('Ctrl Pts',(-0.73485975367032,7.87689241808011,
124.168725115327));
#230651=CARTESIAN_POINT('Ctrl Pts',(-0.695878252535864,7.88043187326883,
124.167169290571));
#230652=CARTESIAN_POINT('Ctrl Pts',(-0.311668414623715,7.91244441285793,
124.151889982918));
#230653=CARTESIAN_POINT('Ctrl Pts',(0.0350609493567653,7.91850381125998,
124.138565662273));
#230654=CARTESIAN_POINT('Ctrl Pts',(0.889346997484526,7.87730375127847,
124.106403859199));
#230655=CARTESIAN_POINT('Ctrl Pts',(1.39404755510762,7.80381155641685,124.088030599812));
#230656=CARTESIAN_POINT('Ctrl Pts',(2.10999840140295,7.62784379124977,124.06061675839));
#230657=CARTESIAN_POINT('Ctrl Pts',(2.32933896935196,7.56374687982564,124.052011594808));
#230658=CARTESIAN_POINT('Ctrl Pts',(2.63316213845387,7.46049145608525,124.03951493596));
#230659=CARTESIAN_POINT('Ctrl Pts',(2.72020353117039,7.4291969675305,124.035866151867));
#230660=CARTESIAN_POINT('Ctrl Pts',(2.81980195693749,7.39140278156724,124.031594659746));
#230661=CARTESIAN_POINT('Ctrl Pts',(2.83291644346128,7.38638630027789,124.031030275854));
#230662=CARTESIAN_POINT('Ctrl Pts',(2.85267824203587,7.37876675394805,124.030176814855));
#230663=CARTESIAN_POINT('Ctrl Pts',(2.85933553844508,7.37618954745027,124.029888787257));
#230664=CARTESIAN_POINT('Ctrl Pts',(2.87133338504519,7.37152619648332,124.02936875746));
#230665=CARTESIAN_POINT('Ctrl Pts',(2.87667517788921,7.36944324859127,124.029136887228));
#230666=CARTESIAN_POINT('Ctrl Pts',(2.88798910528333,7.36501738514403,124.028645062199));
#230667=CARTESIAN_POINT('Ctrl Pts',(2.89396066149947,7.36267300951799,124.028385046485));
#230668=CARTESIAN_POINT('Ctrl Pts',(2.90962676414748,7.35650064441232,124.027701771248));
#230669=CARTESIAN_POINT('Ctrl Pts',(2.91931658906666,7.35266076256004,124.027278007647));
#230670=CARTESIAN_POINT('Ctrl Pts',(2.95992905620287,7.3364739242029,124.025497021018));
#230671=CARTESIAN_POINT('Ctrl Pts',(2.99078087645229,7.32395107571189,124.024132168789));
#230672=CARTESIAN_POINT('Ctrl Pts',(3.49425201402917,7.11587889232877,124.001652450288));
#230673=CARTESIAN_POINT('Ctrl Pts',(3.94679577579872,6.87518143711971,123.9781489169));
#230674=CARTESIAN_POINT('Ctrl Pts',(4.76057938958845,6.33539835606597,123.933187011665));
#230675=CARTESIAN_POINT('Ctrl Pts',(5.12488966443246,6.0444985594457,123.911859840813));
#230676=CARTESIAN_POINT('Ctrl Pts',(5.58444055249789,5.60596157415513,123.884324687986));
#230677=CARTESIAN_POINT('Ctrl Pts',(5.70353818750872,5.48474596580471,123.877113003325));
#230678=CARTESIAN_POINT('Ctrl Pts',(5.87833219753157,5.2949875045911,123.8664224604));
#230679=CARTESIAN_POINT('Ctrl Pts',(5.93693356543073,5.22919712920106,123.862818594296));
#230680=CARTESIAN_POINT('Ctrl Pts',(6.00465085098008,5.15056644532237,123.858629551144));
#230681=CARTESIAN_POINT('Ctrl Pts',(6.01484129881088,5.1386623457643,123.857998486431));
#230682=CARTESIAN_POINT('Ctrl Pts',(6.03040433910354,5.12037246166174,123.857033660691));
#230683=CARTESIAN_POINT('Ctrl Pts',(6.03580227994053,5.11400835717489,123.856698821679));
#230684=CARTESIAN_POINT('Ctrl Pts',(6.04519873533077,5.10289445301531,123.856115607461));
#230685=CARTESIAN_POINT('Ctrl Pts',(6.04920174194431,5.09814847113668,123.855867041629));
#230686=CARTESIAN_POINT('Ctrl Pts',(6.05755991692645,5.08821527917915,123.855347812337));
#230687=CARTESIAN_POINT('Ctrl Pts',(6.06191402042494,5.08302717715645,123.855077194077));
#230688=CARTESIAN_POINT('Ctrl Pts',(6.07393722820976,5.06866358640106,123.85432955633));
#230689=CARTESIAN_POINT('Ctrl Pts',(6.08159221362435,5.05947627261939,123.853853134371));
#230690=CARTESIAN_POINT('Ctrl Pts',(6.11153404319872,5.02337473353192,123.85198800684));
#230691=CARTESIAN_POINT('Ctrl Pts',(6.13366345153975,4.99633013108507,123.850605943454));
#230692=CARTESIAN_POINT('Ctrl Pts',(6.48879128108573,4.55640899259165,123.828366083917));
#230693=CARTESIAN_POINT('Ctrl Pts',(6.77962536888392,4.11120925782116,123.809411418267));
#230694=CARTESIAN_POINT('Ctrl Pts',(7.15889177034146,3.37941764166433,123.781259172598));
#230695=CARTESIAN_POINT('Ctrl Pts',(7.27941941898504,3.11130978001857,123.771475590845));
#230696=CARTESIAN_POINT('Ctrl Pts',(7.49529320832895,2.54941108509627,123.751162180277));
#230697=CARTESIAN_POINT('Ctrl Pts',(7.58891455534187,2.25549864566818,123.740634500011));
#230698=CARTESIAN_POINT('Ctrl Pts',(7.71082118838906,1.77799031810052,123.72271601438));
#230699=CARTESIAN_POINT('Ctrl Pts',(7.75021433846112,1.59755505973086,123.715762995025));
#230700=CARTESIAN_POINT('Ctrl Pts',(7.78799888847079,1.38985472168838,123.707391889824));
#230701=CARTESIAN_POINT('Ctrl Pts',(7.79260947140494,1.3637669990782,123.706333879372));
#230702=CARTESIAN_POINT('Ctrl Pts',(7.79827583549108,1.33073824266183,123.704985528162));
#230703=CARTESIAN_POINT('Ctrl Pts',(7.79945357933817,1.32381801619597,123.704702529612));
#230704=CARTESIAN_POINT('Ctrl Pts',(7.80121165741433,1.31340405786741,123.704275907768));
#230705=CARTESIAN_POINT('Ctrl Pts',(7.80179886163868,1.30991147237225,123.704132702567));
#230706=CARTESIAN_POINT('Ctrl Pts',(7.80293527413752,1.30312442336521,123.70385416754));
#230707=CARTESIAN_POINT('Ctrl Pts',(7.80348474189081,1.2998300035608,123.703718853636));
#230708=CARTESIAN_POINT('Ctrl Pts',(7.80463071578757,1.2929322218325,123.703435296959));
#230709=CARTESIAN_POINT('Ctrl Pts',(7.80522681294202,1.28932879379447,123.703287029064));
#230710=CARTESIAN_POINT('Ctrl Pts',(7.80669366051943,1.28042335202764,123.702920262012));
#230711=CARTESIAN_POINT('Ctrl Pts',(7.80756150178545,1.27512088247368,123.702701583056));
#230712=CARTESIAN_POINT('Ctrl Pts',(7.81100622341778,1.25393843247833,123.701826816964));
#230713=CARTESIAN_POINT('Ctrl Pts',(7.81354004740365,1.23805158810275,123.701168091365));
#230714=CARTESIAN_POINT('Ctrl Pts',(7.85521455938794,0.971531837579941,
123.690074249616));
#230715=CARTESIAN_POINT('Ctrl Pts',(7.88232314874255,0.71918660285763,123.678936860042));
#230716=CARTESIAN_POINT('Ctrl Pts',(7.9375050194115,-0.21597568715271,123.63651840214));
#230717=CARTESIAN_POINT('Ctrl Pts',(7.8892490030556,-0.900315089013139,
123.603552535456));
#230718=CARTESIAN_POINT('Ctrl Pts',(7.7043471289416,-1.81346362295349,123.562112929261));
#230719=CARTESIAN_POINT('Ctrl Pts',(7.64361287548753,-2.0544616709585,123.551387302088));
#230720=CARTESIAN_POINT('Ctrl Pts',(7.54183995843612,-2.39063690095441,
123.536772056054));
#230721=CARTESIAN_POINT('Ctrl Pts',(7.51012847813366,-2.48846662142211,
123.532560418863));
#230722=CARTESIAN_POINT('Ctrl Pts',(7.47134590554917,-2.6006079590647,123.52777847616));
#230723=CARTESIAN_POINT('Ctrl Pts',(7.46612908571469,-2.61554733786892,
123.527142371222));
#230724=CARTESIAN_POINT('Ctrl Pts',(7.45815127397746,-2.63817499481411,
123.526180316297));
#230725=CARTESIAN_POINT('Ctrl Pts',(7.45542315605889,-2.64587476904186,
123.525853194773));
#230726=CARTESIAN_POINT('Ctrl Pts',(7.45048961413376,-2.65973086484823,
123.525264968006));
#230727=CARTESIAN_POINT('Ctrl Pts',(7.44828847559589,-2.66588869766385,
123.525003710119));
#230728=CARTESIAN_POINT('Ctrl Pts',(7.44354431968846,-2.67910905091557,
123.524443148316));
#230729=CARTESIAN_POINT('Ctrl Pts',(7.44099887945694,-2.68617069863672,
123.52414393127));
#230730=CARTESIAN_POINT('Ctrl Pts',(7.43409569635163,-2.7052366384214,123.523336621567));
#230731=CARTESIAN_POINT('Ctrl Pts',(7.42971892115776,-2.71723404348389,
123.522829209811));
#230732=CARTESIAN_POINT('Ctrl Pts',(7.41015062029799,-2.77047296015645,
123.520580158316));
#230733=CARTESIAN_POINT('Ctrl Pts',(7.39464447526628,-2.81159844346842,
123.51884979564));
#230734=CARTESIAN_POINT('Ctrl Pts',(7.1417046519609,-3.4658773384298,123.491426009096));
#230735=CARTESIAN_POINT('Ctrl Pts',(6.82906537484602,-4.04724494525259,
123.468859418155));
#230736=CARTESIAN_POINT('Ctrl Pts',(6.21542807790977,-4.91056682792052,
123.43287648409));
#230737=CARTESIAN_POINT('Ctrl Pts',(5.95818056363805,-5.21969881286509,
123.419283873117));
#230738=CARTESIAN_POINT('Ctrl Pts',(5.57157553089353,-5.61828229777972,
123.398802386977));
#230739=CARTESIAN_POINT('Ctrl Pts',(5.46136432201779,-5.72547329681315,
123.392954751863));
#230740=CARTESIAN_POINT('Ctrl Pts',(5.33654046893791,-5.83999171455548,
123.386225414379));
#230741=CARTESIAN_POINT('Ctrl Pts',(5.32494217755777,-5.85056904937764,
123.385599160833));
#230742=CARTESIAN_POINT('Ctrl Pts',(5.30734593751664,-5.86652068581035,
123.384647420858));
#230743=CARTESIAN_POINT('Ctrl Pts',(5.30137108343511,-5.87192051148682,
123.384323971569));
#230744=CARTESIAN_POINT('Ctrl Pts',(5.29027343966927,-5.88191935738502,
123.383722659039));
#230745=CARTESIAN_POINT('Ctrl Pts',(5.28515291475787,-5.88652079417768,
123.383444999238));
#230746=CARTESIAN_POINT('Ctrl Pts',(5.2769033003488,-5.89391467089273,123.382997336465));
#230747=CARTESIAN_POINT('Ctrl Pts',(5.27377797509923,-5.89671132566469,
123.382827665984));
#230748=CARTESIAN_POINT('Ctrl Pts',(5.26772999789093,-5.90211462154354,
123.382499184284));
#230749=CARTESIAN_POINT('Ctrl Pts',(5.26480763057314,-5.90472158102898,
123.38234039803));
#230750=CARTESIAN_POINT('Ctrl Pts',(5.2581390967781,-5.91066150116706,123.381977919533));
#230751=CARTESIAN_POINT('Ctrl Pts',(5.25439169807175,-5.91399306944942,
123.381774119674));
#230752=CARTESIAN_POINT('Ctrl Pts',(5.24466723866885,-5.92262191450342,
123.381244997225));
#230753=CARTESIAN_POINT('Ctrl Pts',(5.23868533309739,-5.92791369424147,
123.380919254649));
#230754=CARTESIAN_POINT('Ctrl Pts',(5.20241893046063,-5.95989831560864,
123.378942875465));
#230755=CARTESIAN_POINT('Ctrl Pts',(5.17193898792222,-5.98636765107903,
123.377275494925));
#230756=CARTESIAN_POINT('Ctrl Pts',(4.62835579432831,-6.45117499725341,
123.347448589511));
#230757=CARTESIAN_POINT('Ctrl Pts',(4.06147261782022,-6.82229419530351,
123.315129351093));
#230758=CARTESIAN_POINT('Ctrl Pts',(3.13391786840199,-7.27250982956716,
123.267321414984));
#230759=CARTESIAN_POINT('Ctrl Pts',(2.80325758701635,-7.40625558932694,
123.251100110583));
#230760=CARTESIAN_POINT('Ctrl Pts',(2.28864457235289,-7.57498176602784,
123.227465605274));
#230761=CARTESIAN_POINT('Ctrl Pts',(2.11062401390143,-7.62650084401321,
123.219564390662));
#230762=CARTESIAN_POINT('Ctrl Pts',(1.83675877070318,-7.69543191045217,
123.207827347008));
#230763=CARTESIAN_POINT('Ctrl Pts',(1.74213673484754,-7.71740342048326,
123.203846425385));
#230764=CARTESIAN_POINT('Ctrl Pts',(1.63088699677973,-7.74108548292331,
123.199249923026));
#230765=CARTESIAN_POINT('Ctrl Pts',(1.61463133211905,-7.74449239885322,
123.198580372193));
#230766=CARTESIAN_POINT('Ctrl Pts',(1.58977803918717,-7.74961958163247,
123.197559852473));
#230767=CARTESIAN_POINT('Ctrl Pts',(1.5811881275716,-7.7513767796288,123.197207711041));
#230768=CARTESIAN_POINT('Ctrl Pts',(1.5655553574462,-7.75454763493599,123.196567890951));
#230769=CARTESIAN_POINT('Ctrl Pts',(1.5585134669104,-7.7559659858414,123.196280063718));
#230770=CARTESIAN_POINT('Ctrl Pts',(1.54332698516611,-7.7590032718011,123.195660162825));
#230771=CARTESIAN_POINT('Ctrl Pts',(1.53518175316004,-7.7606189791965,123.195328191658));
#230772=CARTESIAN_POINT('Ctrl Pts',(1.51319640903882,-7.76494407683624,
123.194433518295));
#230773=CARTESIAN_POINT('Ctrl Pts',(1.4993515421814,-7.76762929369715,123.193871580708));
#230774=CARTESIAN_POINT('Ctrl Pts',(1.43523658337371,-7.77988660895136,
123.191276000259));
#230775=CARTESIAN_POINT('Ctrl Pts',(1.38488102837438,-7.78900791874657,
123.189256582271));
#230776=CARTESIAN_POINT('Ctrl Pts',(0.47310283919901,-7.94504399997736,
123.153024448447));
#230777=CARTESIAN_POINT('Ctrl Pts',(-0.406594615782335,-7.94871893386163,
123.12424842017));
#230778=CARTESIAN_POINT('Ctrl Pts',(-1.60915479404307,-7.75327332410205,
123.081082630441));
#230779=CARTESIAN_POINT('Ctrl Pts',(-1.94525298587466,-7.67584699683704,
123.06842094574));
#230780=CARTESIAN_POINT('Ctrl Pts',(-2.30099187303705,-7.56902107345386,
123.053652347881));
#230781=CARTESIAN_POINT('Ctrl Pts',(-2.32669775838299,-7.5611587161149,
123.052578450725));
#230782=CARTESIAN_POINT('Ctrl Pts',(-2.36213750553983,-7.55012133779748,
123.051089016778));
#230783=CARTESIAN_POINT('Ctrl Pts',(-2.37190618617987,-7.5470581588716,
123.050677530728));
#230784=CARTESIAN_POINT('Ctrl Pts',(-2.38837376874113,-7.54185926527456,
123.049982313534));
#230785=CARTESIAN_POINT('Ctrl Pts',(-2.39507583352584,-7.53973356211778,
123.049698935686));
#230786=CARTESIAN_POINT('Ctrl Pts',(-2.40832298395694,-7.5355124997351,
123.049137967277));
#230787=CARTESIAN_POINT('Ctrl Pts',(-2.4148681917356,-7.53341754086006,
123.048860390748));
#230788=CARTESIAN_POINT('Ctrl Pts',(-2.42928176201579,-7.52878339968553,
123.048248228249));
#230789=CARTESIAN_POINT('Ctrl Pts',(-2.43714888598366,-7.52624040711141,
123.047913512924));
#230790=CARTESIAN_POINT('Ctrl Pts',(-2.463816484596,-7.51757409563833,123.046776940226));
#230791=CARTESIAN_POINT('Ctrl Pts',(-2.48259791271204,-7.51139265048349,
123.045973151054));
#230792=CARTESIAN_POINT('Ctrl Pts',(-2.67867321445553,-7.4460435629207,
123.037548020464));
#230793=CARTESIAN_POINT('Ctrl Pts',(-2.85383543268809,-7.3806824797968,
123.029734754841));
#230794=CARTESIAN_POINT('Ctrl Pts',(-3.47074672944409,-7.12523809573485,
123.001461008212));
#230795=CARTESIAN_POINT('Ctrl Pts',(-3.89728795680806,-6.90117791265394,
122.980568108106));
#230796=CARTESIAN_POINT('Ctrl Pts',(-4.59883555721635,-6.44675787271908,
122.944895026799));
#230797=CARTESIAN_POINT('Ctrl Pts',(-4.88349938083753,-6.2338930023871,
122.929964564455));
#230798=CARTESIAN_POINT('Ctrl Pts',(-5.43705503987908,-5.75869711831123,
122.899695845164));
#230799=CARTESIAN_POINT('Ctrl Pts',(-5.7035349141928,-5.49489421934162,
122.88431788687));
#230800=CARTESIAN_POINT('Ctrl Pts',(-5.98158904736257,-5.17752491559607,
122.867229592199));
#230801=CARTESIAN_POINT('Ctrl Pts',(-6.01253124463689,-5.1415600598388,
122.865312504795));
#230802=CARTESIAN_POINT('Ctrl Pts',(-6.05896052812327,-5.0866018791294,
122.862412079936));
#230803=CARTESIAN_POINT('Ctrl Pts',(-6.07468587693151,-5.06781144672001,
122.861425489038));
#230804=CARTESIAN_POINT('Ctrl Pts',(-6.10304025392766,-5.03360881148736,
122.859638820471));
#230805=CARTESIAN_POINT('Ctrl Pts',(-6.11569882533755,-5.01822138695761,
122.858838336318));
#230806=CARTESIAN_POINT('Ctrl Pts',(-6.14281807100243,-4.98500092921588,
122.857117241277));
#230807=CARTESIAN_POINT('Ctrl Pts',(-6.15725952746218,-4.96715242701767,
122.856196906606));
#230808=CARTESIAN_POINT('Ctrl Pts',(-6.19605855126245,-4.91877067747951,
122.853713855975));
#230809=CARTESIAN_POINT('Ctrl Pts',(-6.22026807789476,-4.8881194346548,
122.852153255539));
#230810=CARTESIAN_POINT('Ctrl Pts',(-6.33669188766635,-4.73845175375869,
122.844592532332));
#230811=CARTESIAN_POINT('Ctrl Pts',(-6.42572371753769,-4.61699739160262,
122.838638996535));
#230812=CARTESIAN_POINT('Ctrl Pts',(-6.5157098365615,-4.48659206573222,
122.832419858857));
#230813=CARTESIAN_POINT('Ctrl Pts',(-6.52017360701209,-4.48010258510469,
122.832110809568));
#230814=CARTESIAN_POINT('Ctrl Pts',(-6.91668414056494,-3.90180325662953,
122.804609239786));
#230815=CARTESIAN_POINT('Ctrl Pts',(-7.23185592982941,-3.28097163589568,
122.778748434194));
#230816=CARTESIAN_POINT('Ctrl Pts',(-7.48606138635359,-2.55891115136077,
122.74848965973));
#230817=CARTESIAN_POINT('Ctrl Pts',(-7.50911960040304,-2.49043448998333,
122.745615501153));
#230818=CARTESIAN_POINT('Ctrl Pts',(-7.53666802528933,-2.4047600570583,
122.742006557392));
#230819=CARTESIAN_POINT('Ctrl Pts',(-7.54204283422624,-2.38784960533014,
122.741293578467));
#230820=CARTESIAN_POINT('Ctrl Pts',(-7.55066845398457,-2.36039164347064,
122.740134834693));
#230821=CARTESIAN_POINT('Ctrl Pts',(-7.55395415199241,-2.34985520430915,
122.739689943871));
#230822=CARTESIAN_POINT('Ctrl Pts',(-7.56023399076726,-2.32956799576375,
122.73883288756));
#230823=CARTESIAN_POINT('Ctrl Pts',(-7.56323134486293,-2.31981823973345,
122.738420798884));
#230824=CARTESIAN_POINT('Ctrl Pts',(-7.57005098372382,-2.29748169541128,
122.737476277375));
#230825=CARTESIAN_POINT('Ctrl Pts',(-7.5738607445911,-2.28489112584598,
122.736943559449));
#230826=CARTESIAN_POINT('Ctrl Pts',(-7.58389567627036,-2.25142662428004,
122.73552687063));
#230827=CARTESIAN_POINT('Ctrl Pts',(-7.59006605464234,-2.23053642713359,
122.734641702204));
#230828=CARTESIAN_POINT('Ctrl Pts',(-7.63305346135819,-2.08275598001856,
122.728374903688));
#230829=CARTESIAN_POINT('Ctrl Pts',(-7.66677230964546,-1.95498820016653,
122.72293111468));
#230830=CARTESIAN_POINT('Ctrl Pts',(-7.75481273958398,-1.58395380557029,
122.707105036482));
#230831=CARTESIAN_POINT('Ctrl Pts',(-7.80085936015728,-1.3388880784233,
122.696633733668));
#230832=CARTESIAN_POINT('Ctrl Pts',(-7.88568895207708,-0.730257288688616,
122.670817739835));
#230833=CARTESIAN_POINT('Ctrl Pts',(-7.91099667283217,-0.365387611985288,
122.655518059375));
#230834=CARTESIAN_POINT('Ctrl Pts',(-7.91100007201382,0.00786949525208386,
122.640138565923));
#230835=CARTESIAN_POINT('Ctrl Pts',(-7.91098818603604,0.0158110199212082,
122.639811462769));
#230836=CARTESIAN_POINT('Ctrl Pts',(-7.91044581199246,0.196452996655032,
122.632373620344));
#230837=CARTESIAN_POINT('Ctrl Pts',(-7.90427221289167,0.369092327641354,
122.625320690788));
#230838=CARTESIAN_POINT('Ctrl Pts',(-7.88927449177412,0.587729650601402,
122.616444553963));
#230839=CARTESIAN_POINT('Ctrl Pts',(-7.8856879896008,0.634037152709973,
122.614567707779));
#230840=CARTESIAN_POINT('Ctrl Pts',(-7.8793478000732,0.707491008283121,
122.611594981302));
#230841=CARTESIAN_POINT('Ctrl Pts',(-7.87686112252303,0.734659202661326,
122.610496414201));
#230842=CARTESIAN_POINT('Ctrl Pts',(-7.87193000201876,0.78562806661664,
122.608437065062));
#230843=CARTESIAN_POINT('Ctrl Pts',(-7.86951802707497,0.809431554486408,
122.607475970054));
#230844=CARTESIAN_POINT('Ctrl Pts',(-7.86380648047646,0.863357915580631,
122.605299985629));
#230845=CARTESIAN_POINT('Ctrl Pts',(-7.86044173736246,0.893473533137972,
122.604085751629));
#230846=CARTESIAN_POINT('Ctrl Pts',(-7.84975865666005,0.984355673137799,
122.600423954416));
#230847=CARTESIAN_POINT('Ctrl Pts',(-7.84190805761375,1.0450574803776,122.597981548252));
#230848=CARTESIAN_POINT('Ctrl Pts',(-7.78152407357358,1.47286360546611,
122.580783040251));
#230849=CARTESIAN_POINT('Ctrl Pts',(-7.7039359498709,1.83598210164303,122.566200270977));
#230850=CARTESIAN_POINT('Ctrl Pts',(-7.51235336307921,2.50023321942439,
122.539493705509));
#230851=CARTESIAN_POINT('Ctrl Pts',(-7.40491614676532,2.80247125685759,
122.527362143228));
#230852=CARTESIAN_POINT('Ctrl Pts',(-7.11527040245073,3.48319761801135,
122.499707862931));
#230853=CARTESIAN_POINT('Ctrl Pts',(-6.92069050588661,3.8553555720628,122.484356951973));
#230854=CARTESIAN_POINT('Ctrl Pts',(-6.68252037080982,4.23422235476954,
122.467445318905));
#230855=CARTESIAN_POINT('Ctrl Pts',(-6.66737282621719,4.2580344105564,122.466376461572));
#230856=CARTESIAN_POINT('Ctrl Pts',(-6.64245729175586,4.29674288475144,
122.464628568916));
#230857=CARTESIAN_POINT('Ctrl Pts',(-6.63276580421925,4.31168830896625,
122.463951160691));
#230858=CARTESIAN_POINT('Ctrl Pts',(-6.61914728454546,4.33253510886889,
122.463002565876));
#230859=CARTESIAN_POINT('Ctrl Pts',(-6.61526265261768,4.33846416151682,
122.462732354847));
#230860=CARTESIAN_POINT('Ctrl Pts',(-6.60473339329572,4.35448778329756,
122.462000937356));
#230861=CARTESIAN_POINT('Ctrl Pts',(-6.59807360247052,4.36457234866685,
122.461539371968));
#230862=CARTESIAN_POINT('Ctrl Pts',(-6.58548624673853,4.38353805779245,
122.460668915294));
#230863=CARTESIAN_POINT('Ctrl Pts',(-6.57956375607474,4.39242254218495,
122.460260151324));
#230864=CARTESIAN_POINT('Ctrl Pts',(-6.51961042651408,4.48196677973715,
122.456130014865));
#230865=CARTESIAN_POINT('Ctrl Pts',(-6.46411805795101,4.56163603970415,
122.452370827905));
#230866=CARTESIAN_POINT('Ctrl Pts',(-6.39996873261838,4.65021205389714,
122.448075082794));
#230867=CARTESIAN_POINT('Ctrl Pts',(-6.39273963457286,4.66014505005677,
122.447591677118));
#230868=CARTESIAN_POINT('Ctrl Pts',(-6.36899470625122,4.69261206435841,
122.446005994529));
#230869=CARTESIAN_POINT('Ctrl Pts',(-6.35238272888113,4.7150753121587,122.444899999383));
#230870=CARTESIAN_POINT('Ctrl Pts',(-6.3201710065246,4.75815381920606,122.442760948201));
#230871=CARTESIAN_POINT('Ctrl Pts',(-6.30458850050066,4.77878155390664,
122.441728625597));
#230872=CARTESIAN_POINT('Ctrl Pts',(-6.28296776955826,4.80711272951643,
122.440299137008));
#230873=CARTESIAN_POINT('Ctrl Pts',(-6.27701584665144,4.81488201801712,
122.439905911582));
#230874=CARTESIAN_POINT('Ctrl Pts',(-6.2675037806945,4.82725089359206,122.439277916591));
#230875=CARTESIAN_POINT('Ctrl Pts',(-6.2639529451683,4.83185764806973,122.439043584145));
#230876=CARTESIAN_POINT('Ctrl Pts',(-6.25665572952526,4.84130328862421,
122.438562204498));
#230877=CARTESIAN_POINT('Ctrl Pts',(-6.25290880962877,4.84614175075723,
122.438315131578));
#230878=CARTESIAN_POINT('Ctrl Pts',(-6.24424224347191,4.85730625209324,
122.437743880566));
#230879=CARTESIAN_POINT('Ctrl Pts',(-6.23931859640703,4.86362916695968,
122.43741950822));
#230880=CARTESIAN_POINT('Ctrl Pts',(-6.22386241231381,4.88341580033775,
122.436401733714));
#230881=CARTESIAN_POINT('Ctrl Pts',(-6.21329588228058,4.89685281374519,
122.435706643586));
#230882=CARTESIAN_POINT('Ctrl Pts',(-6.00455084528704,5.16054172602848,
122.421986641349));
#230883=CARTESIAN_POINT('Ctrl Pts',(-5.79149153027634,5.39855247604332,
122.408047337165));
#230884=CARTESIAN_POINT('Ctrl Pts',(-5.45536921920309,5.73118839155223,
122.386726740543));
#230885=CARTESIAN_POINT('Ctrl Pts',(-5.34292530557486,5.83615636523896,
122.379699543903));
#230886=CARTESIAN_POINT('Ctrl Pts',(-5.11254968953585,6.03897424631014,
122.365602196726));
#230887=CARTESIAN_POINT('Ctrl Pts',(-4.99468956531507,6.13681108108331,
122.358535302134));
#230888=CARTESIAN_POINT('Ctrl Pts',(-4.52643316128406,6.50308478059612,
122.331164786358));
#230889=CARTESIAN_POINT('Ctrl Pts',(-4.15663155711402,6.7454562686423,122.311074659838));
#230890=CARTESIAN_POINT('Ctrl Pts',(-3.54761463452131,7.07541341267905,
122.281089942063));
#230891=CARTESIAN_POINT('Ctrl Pts',(-3.32112236743532,7.18451148461951,
122.270536729567));
#230892=CARTESIAN_POINT('Ctrl Pts',(-3.06806777786713,7.29187484766734,
122.259382560491));
#230893=CARTESIAN_POINT('Ctrl Pts',(-3.04628684506019,7.30100096927076,
122.258427475878));
#230894=CARTESIAN_POINT('Ctrl Pts',(-3.01562164643922,7.31368844585405,
122.25708975166));
#230895=CARTESIAN_POINT('Ctrl Pts',(-3.00677138638473,7.31733137340926,
122.256704480644));
#230896=CARTESIAN_POINT('Ctrl Pts',(-2.99139556123321,7.32362773625407,
122.256036535657));
#230897=CARTESIAN_POINT('Ctrl Pts',(-2.98487303083925,7.32628852920094,
122.255753624758));
#230898=CARTESIAN_POINT('Ctrl Pts',(-2.9712886529523,7.3318089710388,122.255165315012));
#230899=CARTESIAN_POINT('Ctrl Pts',(-2.96422620885145,7.3346671383326,122.254859964059));
#230900=CARTESIAN_POINT('Ctrl Pts',(-2.94757725135526,7.34137698824372,
122.254141324682));
#230901=CARTESIAN_POINT('Ctrl Pts',(-2.93798729005412,7.34522010702862,
122.253728311872));
#230902=CARTESIAN_POINT('Ctrl Pts',(-2.90657488088151,7.3577370783932,122.252378497575));
#230903=CARTESIAN_POINT('Ctrl Pts',(-2.88472124707806,7.36633258760392,
122.251444210902));
#230904=CARTESIAN_POINT('Ctrl Pts',(-2.48294963364251,7.5222959841929,122.234354330079));
#230905=CARTESIAN_POINT('Ctrl Pts',(-2.0922287848583,7.64019631154346,122.219195962468));
#230906=CARTESIAN_POINT('Ctrl Pts',(-1.1405021448231,7.84884777212554,122.184404599306));
#230907=CARTESIAN_POINT('Ctrl Pts',(-0.575458860413354,7.91037125879405,
122.165480450824));
#230908=CARTESIAN_POINT('Ctrl Pts',(0.120836509500774,7.9111378257672,122.140761480949));
#230909=CARTESIAN_POINT('Ctrl Pts',(0.250363447632309,7.90809836448072,
122.136098413506));
#230910=CARTESIAN_POINT('Ctrl Pts',(0.583797563593487,7.89207395525814,
122.123819557991));
#230911=CARTESIAN_POINT('Ctrl Pts',(0.787381334560894,7.8743685428624,122.116054207754));
#230912=CARTESIAN_POINT('Ctrl Pts',(1.005581907044,7.8468446584285,122.107268112165));
#230913=CARTESIAN_POINT('Ctrl Pts',(1.02110745928984,7.84483942579828,122.106640565912));
#230914=CARTESIAN_POINT('Ctrl Pts',(1.04302689041769,7.84194220723988,122.105751296554));
#230915=CARTESIAN_POINT('Ctrl Pts',(1.04942585670393,7.84108844783441,122.105491295826));
#230916=CARTESIAN_POINT('Ctrl Pts',(1.06057388418235,7.83958717083396,122.105037652468));
#230917=CARTESIAN_POINT('Ctrl Pts',(1.06532342094417,7.83894316738814,122.104844165728));
#230918=CARTESIAN_POINT('Ctrl Pts',(1.07524832612742,7.83758823408588,122.104439398932));
#230919=CARTESIAN_POINT('Ctrl Pts',(1.08042358097314,7.83687649356574,122.104228083419));
#230920=CARTESIAN_POINT('Ctrl Pts',(1.09268381698111,7.8351779971384,122.103726880192));
#230921=CARTESIAN_POINT('Ctrl Pts',(1.09976816505213,7.83418675762804,122.103436798779));
#230922=CARTESIAN_POINT('Ctrl Pts',(1.12325330600757,7.83086824133311,122.102473618676));
#230923=CARTESIAN_POINT('Ctrl Pts',(1.13964806417693,7.82849906984852,122.101798742745));
#230924=CARTESIAN_POINT('Ctrl Pts',(1.6030606347084,7.7600457269014,122.082654632283));
#230925=CARTESIAN_POINT('Ctrl Pts',(2.04358792758315,7.65583608302759,122.062722469412));
#230926=CARTESIAN_POINT('Ctrl Pts',(2.82399970385248,7.39903071538375,122.026536444565));
#230927=CARTESIAN_POINT('Ctrl Pts',(3.16669395516515,7.25897376123151,122.010306476261));
#230928=CARTESIAN_POINT('Ctrl Pts',(3.77536257405946,6.95887577122387,121.981352237365));
#230929=CARTESIAN_POINT('Ctrl Pts',(4.04415426640064,6.80618455789069,121.968508741788));
#230930=CARTESIAN_POINT('Ctrl Pts',(4.33058821635751,6.62049703507536,121.954689112334));
#230931=CARTESIAN_POINT('Ctrl Pts',(4.35772494816115,6.60266677837436,121.953378273905));
#230932=CARTESIAN_POINT('Ctrl Pts',(4.39839518690331,6.57558434539542,121.951411026019));
#230933=CARTESIAN_POINT('Ctrl Pts',(4.41201087066399,6.56645640989891,121.950751970742));
#230934=CARTESIAN_POINT('Ctrl Pts',(4.4355396067671,6.55057655854401,121.94961224369));
#230935=CARTESIAN_POINT('Ctrl Pts',(4.44546584197748,6.54384430600786,121.949131158936));
#230936=CARTESIAN_POINT('Ctrl Pts',(4.46605167600794,6.52981395713853,121.948132881055));
#230937=CARTESIAN_POINT('Ctrl Pts',(4.47670878808498,6.5225122702391,121.947615764887));
#230938=CARTESIAN_POINT('Ctrl Pts',(4.50171548402078,6.50528885214098,121.946401582238));
#230939=CARTESIAN_POINT('Ctrl Pts',(4.51605024174706,6.49534568484078,121.945704961867));
#230940=CARTESIAN_POINT('Ctrl Pts',(4.5461665180098,6.47430792672925,121.944240051328));
#230941=CARTESIAN_POINT('Ctrl Pts',(4.56194058858483,6.46320285998722,121.943471979079));
#230942=CARTESIAN_POINT('Ctrl Pts',(4.60451906794802,6.432993749524,121.941396442249));
#230943=CARTESIAN_POINT('Ctrl Pts',(4.63124523176377,6.41377985677793,121.940091143748));
#230944=CARTESIAN_POINT('Ctrl Pts',(5.10264219299502,6.07040177178243,121.917022707642));
#230945=CARTESIAN_POINT('Ctrl Pts',(5.51242335048445,5.70087479389796,121.896383173171));
#230946=CARTESIAN_POINT('Ctrl Pts',(6.13444507014976,5.00964810986327,121.862115279552));
#230947=CARTESIAN_POINT('Ctrl Pts',(6.36770087344635,4.70960326530832,121.848305379942));
#230948=CARTESIAN_POINT('Ctrl Pts',(6.65766201550409,4.27548413925649,121.828635140419));
#230949=CARTESIAN_POINT('Ctrl Pts',(6.73359393454971,4.15486929477825,121.823197269));
#230950=CARTESIAN_POINT('Ctrl Pts',(6.8520463974024,3.95492893328371,121.814144550234));
#230951=CARTESIAN_POINT('Ctrl Pts',(6.89654526902927,3.87681123296082,121.810598276778));
#230952=CARTESIAN_POINT('Ctrl Pts',(6.94684523472325,3.78490206751853,121.806399573757));
#230953=CARTESIAN_POINT('Ctrl Pts',(6.95395141588179,3.77183007010281,121.805801788944));
#230954=CARTESIAN_POINT('Ctrl Pts',(6.96459014680506,3.752127600154,121.804899775356));
#230955=CARTESIAN_POINT('Ctrl Pts',(6.96815021998524,3.74551197462206,121.804596728551));
#230956=CARTESIAN_POINT('Ctrl Pts',(6.97447576682979,3.73371708229041,121.804056111107));
#230957=CARTESIAN_POINT('Ctrl Pts',(6.97724491150819,3.72853978351801,121.803818700568));
#230958=CARTESIAN_POINT('Ctrl Pts',(6.98306334205063,3.71763224308012,121.803318284873));
#230959=CARTESIAN_POINT('Ctrl Pts',(6.98611134303106,3.71190132362431,121.803055223426));
#230960=CARTESIAN_POINT('Ctrl Pts',(6.99412617491511,3.69678681703955,121.802361056737));
#230961=CARTESIAN_POINT('Ctrl Pts',(6.9990811648969,3.68739699069471,121.801929424484));
#230962=CARTESIAN_POINT('Ctrl Pts',(7.02123286621443,3.64521346335347,121.799988505945));
#230963=CARTESIAN_POINT('Ctrl Pts',(7.03821791531186,3.61230960265677,121.798469621436));
#230964=CARTESIAN_POINT('Ctrl Pts',(7.15661591513859,3.37894071928148,121.787655443127));
#230965=CARTESIAN_POINT('Ctrl Pts',(7.24966354982402,3.17438824039553,121.777909970264));
#230966=CARTESIAN_POINT('Ctrl Pts',(7.52384049416456,2.49648673551076,121.745288336194));
#230967=CARTESIAN_POINT('Ctrl Pts',(7.66824717562286,2.00963183637676,121.721500248117));
#230968=CARTESIAN_POINT('Ctrl Pts',(7.85627549181512,1.0441796902873,121.67688117192));
#230969=CARTESIAN_POINT('Ctrl Pts',(7.90493716167581,0.568724338412397,
121.656054115293));
#230970=CARTESIAN_POINT('Ctrl Pts',(7.91082541849235,0.0609205216541271,
121.635412214022));
#230971=CARTESIAN_POINT('Ctrl Pts',(7.91100267697548,0.0301128819094594,
121.634165787443));
#230972=CARTESIAN_POINT('Ctrl Pts',(7.9109989717153,-0.0120481679108156,
121.632467999411));
#230973=CARTESIAN_POINT('Ctrl Pts',(7.91097353544595,-0.0234011056981993,
121.632011618229));
#230974=CARTESIAN_POINT('Ctrl Pts',(7.91089443484175,-0.0414064914464311,
121.631289062771));
#230975=CARTESIAN_POINT('Ctrl Pts',(7.91085681782842,-0.0480589725781283,
121.631022369591));
#230976=CARTESIAN_POINT('Ctrl Pts',(7.91076765403138,-0.0609513096375462,
121.630506048172));
#230977=CARTESIAN_POINT('Ctrl Pts',(7.91071711576061,-0.0671911666543467,
121.630256387449));
#230978=CARTESIAN_POINT('Ctrl Pts',(7.91057931389433,-0.0820364512229167,
121.629662981486));
#230979=CARTESIAN_POINT('Ctrl Pts',(7.91048539106875,-0.090641817347533,
121.629319452342));
#230980=CARTESIAN_POINT('Ctrl Pts',(7.91016526583808,-0.116157053060414,
121.628302206005));
#230981=CARTESIAN_POINT('Ctrl Pts',(7.90989888219174,-0.133066419785025,
121.627629793095));
#230982=CARTESIAN_POINT('Ctrl Pts',(7.90733248462793,-0.268416575690285,
121.62226125425));
#230983=CARTESIAN_POINT('Ctrl Pts',(7.90242652814297,-0.386795831909862,
121.617650510753));
#230984=CARTESIAN_POINT('Ctrl Pts',(7.87550275685157,-0.807685907948852,
121.601532546116));
#230985=CARTESIAN_POINT('Ctrl Pts',(7.838752817635,-1.10899703523779,121.590513181226));
#230986=CARTESIAN_POINT('Ctrl Pts',(7.72652858173331,-1.72971435303638,
121.568389622819));
#230987=CARTESIAN_POINT('Ctrl Pts',(7.64831463857171,-2.04803485573906,
121.557371101431));
#230988=CARTESIAN_POINT('Ctrl Pts',(7.37710215899867,-2.91553484378619,
121.526828009285));
#230989=CARTESIAN_POINT('Ctrl Pts',(7.14297834487907,-3.44958953269405,
121.507473592931));
#230990=CARTESIAN_POINT('Ctrl Pts',(6.83406459812971,-3.9850778406863,121.483125923467));
#230991=CARTESIAN_POINT('Ctrl Pts',(6.81539079688638,-4.01693073461318,
121.481657456047));
#230992=CARTESIAN_POINT('Ctrl Pts',(6.79266004772222,-4.05508897899298,
121.479872573196));
#230993=CARTESIAN_POINT('Ctrl Pts',(6.78881596659692,-4.06152125716694,
121.479570813516));
#230994=CARTESIAN_POINT('Ctrl Pts',(6.78252669647948,-4.07201118061901,
121.479077235551));
#230995=CARTESIAN_POINT('Ctrl Pts',(6.78008698448998,-4.07607211983111,
121.478885799908));
#230996=CARTESIAN_POINT('Ctrl Pts',(6.7757246782787,-4.08331849450716,121.478543556785));
#230997=CARTESIAN_POINT('Ctrl Pts',(6.77380347979196,-4.08650477308932,
121.478392847718));
#230998=CARTESIAN_POINT('Ctrl Pts',(6.76974430110557,-4.09322613172561,
121.478074459256));
#230999=CARTESIAN_POINT('Ctrl Pts',(6.76760579893498,-4.09676089342325,
121.477906742798));
#231000=CARTESIAN_POINT('Ctrl Pts',(6.76190013653118,-4.10617520783546,
121.477459314837));
#231001=CARTESIAN_POINT('Ctrl Pts',(6.7583280884598,-4.11205176788634,121.477179253055));
#231002=CARTESIAN_POINT('Ctrl Pts',(6.74131377542368,-4.13996083416053,
121.475845546104));
#231003=CARTESIAN_POINT('Ctrl Pts',(6.72777154754702,-4.16193189512592,
121.474784829611));
#231004=CARTESIAN_POINT('Ctrl Pts',(6.61968634619532,-4.33538449827017,
121.4663281675));
#231005=CARTESIAN_POINT('Ctrl Pts',(6.52015239408849,-4.48368268114007,
121.458597008266));
#231006=CARTESIAN_POINT('Ctrl Pts',(6.2030659638144,-4.92320738865209,121.434473295189));
#231007=CARTESIAN_POINT('Ctrl Pts',(5.97038900287542,-5.20292551545113,
121.417448469429));
#231008=CARTESIAN_POINT('Ctrl Pts',(5.51399504814044,-5.68050181870736,
121.386586269516));
#231009=CARTESIAN_POINT('Ctrl Pts',(5.29671763167392,-5.88362461205754,
121.372753714829));
#231010=CARTESIAN_POINT('Ctrl Pts',(4.74755264420394,-6.34187810277763,
121.340373559345));
#231011=CARTESIAN_POINT('Ctrl Pts',(4.40583709701723,-6.58387036294046,
121.322275461513));
#231012=CARTESIAN_POINT('Ctrl Pts',(4.02229809609323,-6.81218288859636,
121.304180485345));
#231013=CARTESIAN_POINT('Ctrl Pts',(3.99796724913797,-6.82649072214591,
121.303041327586));
#231014=CARTESIAN_POINT('Ctrl Pts',(3.96432550431203,-6.84603230705104,
121.30147816504));
#231015=CARTESIAN_POINT('Ctrl Pts',(3.95507996229367,-6.85137778453623,
121.301049805927));
#231016=CARTESIAN_POINT('Ctrl Pts',(3.94033139021809,-6.85986513635622,
121.300368442024));
#231017=CARTESIAN_POINT('Ctrl Pts',(3.93483537760024,-6.86301913921076,
121.300114965952));
#231018=CARTESIAN_POINT('Ctrl Pts',(3.92413198207343,-6.86914442506605,
121.299622164204));
#231019=CARTESIAN_POINT('Ctrl Pts',(3.9189249996244,-6.87211639836691,121.29938281182));
#231020=CARTESIAN_POINT('Ctrl Pts',(3.90645763308859,-6.87921358086701,
121.298810637208));
#231021=CARTESIAN_POINT('Ctrl Pts',(3.89919407915302,-6.88333322337214,
121.298478030675));
#231022=CARTESIAN_POINT('Ctrl Pts',(3.87819984434484,-6.89519654996592,
121.297518824582));
#231023=CARTESIAN_POINT('Ctrl Pts',(3.86445248517939,-6.90291072585189,
121.296893364907));
#231024=CARTESIAN_POINT('Ctrl Pts',(3.75553865260428,-6.96359916532429,
121.291958890076));
#231025=CARTESIAN_POINT('Ctrl Pts',(3.65930826977888,-7.01464526115448,
121.287724321613));
#231026=CARTESIAN_POINT('Ctrl Pts',(3.2855917547353,-7.20310167547326,121.27172759516));
#231027=CARTESIAN_POINT('Ctrl Pts',(3.00117445277655,-7.32616947697695,
121.260500695372));
#231028=CARTESIAN_POINT('Ctrl Pts',(2.50274438743094,-7.5079278073775,121.241891596508));
#231029=CARTESIAN_POINT('Ctrl Pts',(2.29214902980414,-7.57487724898308,
121.234333891815));
#231030=CARTESIAN_POINT('Ctrl Pts',(1.5032710671529,-7.7897485842773,121.20651751995));
#231031=CARTESIAN_POINT('Ctrl Pts',(0.911699572768521,-7.88090210862725,
121.186730995063));
#231032=CARTESIAN_POINT('Ctrl Pts',(0.279910596700759,-7.90612719985605,
121.161811108329));
#231033=CARTESIAN_POINT('Ctrl Pts',(0.244205810922867,-7.90731058482555,
121.160389670526));
#231034=CARTESIAN_POINT('Ctrl Pts',(0.201021844090053,-7.90844909587385,
121.158653266416));
#231035=CARTESIAN_POINT('Ctrl Pts',(0.19354865470272,-7.90863552080794,
121.15835214945));
#231036=CARTESIAN_POINT('Ctrl Pts',(0.181217921522819,-7.90892563320714,
121.157854290361));
#231037=CARTESIAN_POINT('Ctrl Pts',(0.176360501279567,-7.9090354392975,
121.157657909331));
#231038=CARTESIAN_POINT('Ctrl Pts',(0.167604170880889,-7.90922531287796,
121.157303433255));
#231039=CARTESIAN_POINT('Ctrl Pts',(0.1637052929805,-7.90930697247932,121.157145431423));
#231040=CARTESIAN_POINT('Ctrl Pts',(0.155387770111011,-7.90947502510971,
121.156808011483));
#231041=CARTESIAN_POINT('Ctrl Pts',(0.150969111767284,-7.90956059835645,
121.156628545817));
#231042=CARTESIAN_POINT('Ctrl Pts',(0.139068748611965,-7.90978108909305,
121.156144639855));
#231043=CARTESIAN_POINT('Ctrl Pts',(0.131586936268826,-7.90990909376826,
121.155839801669));
#231044=CARTESIAN_POINT('Ctrl Pts',(0.0952926185785408,-7.91047853630061,
121.154358135146));
#231045=CARTESIAN_POINT('Ctrl Pts',(0.0664783595287169,-7.91077315709305,
121.153172983271));
#231046=CARTESIAN_POINT('Ctrl Pts',(-0.168834078612055,-7.91189346920868,
121.143425676321));
#231047=CARTESIAN_POINT('Ctrl Pts',(-0.375277098152051,-7.90479084434174,
121.134442993002));
#231048=CARTESIAN_POINT('Ctrl Pts',(-0.968561250397912,-7.86108649676241,
121.107825735296));
#231049=CARTESIAN_POINT('Ctrl Pts',(-1.35329239147617,-7.80406132204472,
121.08959886076));
#231050=CARTESIAN_POINT('Ctrl Pts',(-1.89414786949916,-7.6826851470739,
121.063753164238));
#231051=CARTESIAN_POINT('Ctrl Pts',(-2.05485124326905,-7.64127183462109,
121.056040772332));
#231052=CARTESIAN_POINT('Ctrl Pts',(-2.7316186001039,-7.44397265820379,
121.023603861077));
#231053=CARTESIAN_POINT('Ctrl Pts',(-3.23238283406999,-7.24060217193323,
120.999836659265));
#231054=CARTESIAN_POINT('Ctrl Pts',(-3.73967447955794,-6.9713693769398,
120.976442565805));
#231055=CARTESIAN_POINT('Ctrl Pts',(-3.77060883421412,-6.95468656833446,
120.975018271509));
#231056=CARTESIAN_POINT('Ctrl Pts',(-3.81221651153987,-6.93188845221738,
120.973105428234));
#231057=CARTESIAN_POINT('Ctrl Pts',(-3.82298800621975,-6.92595372139532,
120.972610488452));
#231058=CARTESIAN_POINT('Ctrl Pts',(-3.83990025473975,-6.9165841669824,
120.97183378794));
#231059=CARTESIAN_POINT('Ctrl Pts',(-3.84605031808688,-6.91316623960174,
120.971551427864));
#231060=CARTESIAN_POINT('Ctrl Pts',(-3.85786739276228,-6.9065781935953,
120.971009043686));
#231061=CARTESIAN_POINT('Ctrl Pts',(-3.86353507539164,-6.90340929438943,
120.97074897656));
#231062=CARTESIAN_POINT('Ctrl Pts',(-3.8768687802879,-6.8959326261873,120.970137309157));
#231063=CARTESIAN_POINT('Ctrl Pts',(-3.88453154161697,-6.8916190425264,
120.969785916111));
#231064=CARTESIAN_POINT('Ctrl Pts',(-3.90675208817579,-6.87906163733155,
120.968767303249));
#231065=CARTESIAN_POINT('Ctrl Pts',(-3.92129097492854,-6.87078437902002,
120.968101275036));
#231066=CARTESIAN_POINT('Ctrl Pts',(-4.02074624998288,-6.81374413891597,
120.963548158711));
#231067=CARTESIAN_POINT('Ctrl Pts',(-4.10477880738604,-6.76345336197736,
120.959715985035));
#231068=CARTESIAN_POINT('Ctrl Pts',(-4.36497496643559,-6.60109829921007,
120.94788078816));
#231069=CARTESIAN_POINT('Ctrl Pts',(-4.53765361511666,-6.48361099897565,
120.940073704662));
#231070=CARTESIAN_POINT('Ctrl Pts',(-4.7862127345976,-6.29969622197205,
120.928792257694));
#231071=CARTESIAN_POINT('Ctrl Pts',(-4.86579257352607,-6.23843474185694,
120.925172774717));
#231072=CARTESIAN_POINT('Ctrl Pts',(-4.99528101553143,-6.13476752973713,
120.919251507299));
#231073=CARTESIAN_POINT('Ctrl Pts',(-5.04586705509031,-6.09322827852271,
120.916929955196));
#231074=CARTESIAN_POINT('Ctrl Pts',(-5.24247012639813,-5.92765812084226,
120.907859911089));
#231075=CARTESIAN_POINT('Ctrl Pts',(-5.38447832765632,-5.79896701108558,
120.901205784861));
#231076=CARTESIAN_POINT('Ctrl Pts',(-5.66188234169319,-5.52859308021142,
120.887780004742));
#231077=CARTESIAN_POINT('Ctrl Pts',(-5.79696653936588,-5.38678296949157,
120.881013477701));
#231078=CARTESIAN_POINT('Ctrl Pts',(-6.19111456957088,-4.94099509235523,
120.860145242084));
#231079=CARTESIAN_POINT('Ctrl Pts',(-6.43256020973177,-4.62228501768219,
120.845708533327));
#231080=CARTESIAN_POINT('Ctrl Pts',(-6.6648584408398,-4.26197703409882,
120.828688052114));
#231081=CARTESIAN_POINT('Ctrl Pts',(-6.68065958892634,-4.23716576319373,
120.827514060391));
#231082=CARTESIAN_POINT('Ctrl Pts',(-6.70216550551455,-4.20297739517431,
120.825894226977));
#231083=CARTESIAN_POINT('Ctrl Pts',(-6.70798979449527,-4.19367551954443,
120.825453290249));
#231084=CARTESIAN_POINT('Ctrl Pts',(-6.71721563633876,-4.17887268599546,
120.824751277155));
#231085=CARTESIAN_POINT('Ctrl Pts',(-6.72062984310777,-4.17337960680574,
120.824490703421));
#231086=CARTESIAN_POINT('Ctrl Pts',(-6.72724740495691,-4.1627035058646,
120.823984138275));
#231087=CARTESIAN_POINT('Ctrl Pts',(-6.73045151642247,-4.15752095726362,
120.823738176592));
#231088=CARTESIAN_POINT('Ctrl Pts',(-6.73808350622551,-4.14514451153135,
120.823150666014));
#231089=CARTESIAN_POINT('Ctrl Pts',(-6.7425058516263,-4.13794722036546,
120.822808906037));
#231090=CARTESIAN_POINT('Ctrl Pts',(-6.75566779606539,-4.11644926109138,
120.821787800096));
#231091=CARTESIAN_POINT('Ctrl Pts',(-6.76437346158028,-4.10212793044029,
120.821107192135));
#231092=CARTESIAN_POINT('Ctrl Pts',(-6.83844620973009,-3.97939693315188,
120.815271857149));
#231093=CARTESIAN_POINT('Ctrl Pts',(-6.90124648880263,-3.8694627342908,
120.810027589514));
#231094=CARTESIAN_POINT('Ctrl Pts',(-7.1790169352521,-3.35492611327057,
120.785521548263));
#231095=CARTESIAN_POINT('Ctrl Pts',(-7.36122042076578,-2.9336400575739,
120.765632169292));
#231096=CARTESIAN_POINT('Ctrl Pts',(-7.72075526074726,-1.8537327561986,
120.716815077764));
#231097=CARTESIAN_POINT('Ctrl Pts',(-7.85148547063976,-1.1834784090553,
120.688520336153));
#231098=CARTESIAN_POINT('Ctrl Pts',(-7.90226451682542,-0.389270818588789,
120.655930261483));
#231099=CARTESIAN_POINT('Ctrl Pts',(-7.90711381548192,-0.273619773638637,
120.651209371742));
#231100=CARTESIAN_POINT('Ctrl Pts',(-7.91047403648233,-0.105305139888183,
120.644377508997));
#231101=CARTESIAN_POINT('Ctrl Pts',(-7.91099940645487,-0.0526978673707179,
120.642247651637));
#231102=CARTESIAN_POINT('Ctrl Pts',(-7.91099999949736,-8.91784084347633E-5,
120.64012317337));
#231103=CARTESIAN_POINT('',(-7.91099999889219,0.000132392670232489,118.642430830134));
#231104=CARTESIAN_POINT('Ctrl Pts',(-7.91099929352038,0.00334333966528006,
120.642331508237));
#231105=CARTESIAN_POINT('Ctrl Pts',(-7.91091098853137,0.212290313526421,
120.633939442701));
#231106=CARTESIAN_POINT('Ctrl Pts',(-7.90254028181684,0.421122619949147,
120.625547377165));
#231107=CARTESIAN_POINT('Ctrl Pts',(-7.88593972319406,0.62918652413254,
120.617155311629));
#231108=CARTESIAN_POINT('Ctrl Pts',(-7.86910331169471,0.840206501748585,
120.6086440156));
#231109=CARTESIAN_POINT('Ctrl Pts',(-7.84380147092849,1.05043578307963,
120.60013271957));
#231110=CARTESIAN_POINT('Ctrl Pts',(-7.81014299452937,1.25920109792034,
120.591621423541));
#231111=CARTESIAN_POINT('Ctrl Pts',(-7.77687976097489,1.46551493528119,
120.583210073475));
#231112=CARTESIAN_POINT('Ctrl Pts',(-7.73545518240527,1.67039873955153,
120.574798723409));
#231113=CARTESIAN_POINT('Ctrl Pts',(-7.68602535642838,1.87321520929656,
120.566387373343));
#231114=CARTESIAN_POINT('Ctrl Pts',(-7.63571452237108,2.07964656024245,
120.557826104332));
#231115=CARTESIAN_POINT('Ctrl Pts',(-7.57711049069753,2.28393590058186,
120.549264835321));
#231116=CARTESIAN_POINT('Ctrl Pts',(-7.51043042045454,2.48542871543543,
120.54070356631));
#231117=CARTESIAN_POINT('Ctrl Pts',(-7.44375035021156,2.686921530289,120.532142297299));
#231118=CARTESIAN_POINT('Ctrl Pts',(-7.36899437388891,2.88561754922279,
120.523581028288));
#231119=CARTESIAN_POINT('Ctrl Pts',(-7.28643086389093,3.08088400718651,
120.515019759277));
#231120=CARTESIAN_POINT('Ctrl Pts',(-7.20254663432856,3.27927402701565,
120.506321540716));
#231121=CARTESIAN_POINT('Ctrl Pts',(-7.110535319717,3.4742852672912,120.497623322156));
#231122=CARTESIAN_POINT('Ctrl Pts',(-7.01068098269354,3.66527941075426,
120.488925103595));
#231123=CARTESIAN_POINT('Ctrl Pts',(-6.91091438109058,3.85610574025963,
120.480234527586));
#231124=CARTESIAN_POINT('Ctrl Pts',(-6.80331862294041,4.04292181806838,
120.471543951577));
#231125=CARTESIAN_POINT('Ctrl Pts',(-6.68822440143792,4.22511246667001,
120.462853375567));
#231126=CARTESIAN_POINT('Ctrl Pts',(-6.57036992268928,4.41167251845644,
120.453954377058));
#231127=CARTESIAN_POINT('Ctrl Pts',(-6.44465290972965,4.59338228731657,
120.445055378548));
#231128=CARTESIAN_POINT('Ctrl Pts',(-6.31147843001338,4.76960805805632,
120.436156380038));
#231129=CARTESIAN_POINT('Ctrl Pts',(-6.18180622154059,4.94119937893348,
120.427491410651));
#231130=CARTESIAN_POINT('Ctrl Pts',(-6.04506393641537,5.10759126157416,
120.418826441263));
#231131=CARTESIAN_POINT('Ctrl Pts',(-5.90167009850677,5.26822655628923,
120.410161471876));
#231132=CARTESIAN_POINT('Ctrl Pts',(-5.75246694971074,5.43536966459033,
120.401145458805));
#231133=CARTESIAN_POINT('Ctrl Pts',(-5.59606220092296,5.59627984384596,
120.392129445734));
#231134=CARTESIAN_POINT('Ctrl Pts',(-5.43297594668917,5.75036462867329,
120.383113432664));
#231135=CARTESIAN_POINT('Ctrl Pts',(-5.26988969245527,5.90444941350073,
120.374097419593));
#231136=CARTESIAN_POINT('Ctrl Pts',(-5.10012208988998,6.05170856300526,
120.365081406522));
#231137=CARTESIAN_POINT('Ctrl Pts',(-4.92424059686758,6.1915890968443,120.356065393452));
#231138=CARTESIAN_POINT('Ctrl Pts',(-4.77187701342577,6.31276557211311,
120.348254952249));
#231139=CARTESIAN_POINT('Ctrl Pts',(-4.61499064308439,6.42835209568637,
120.340444511047));
#231140=CARTESIAN_POINT('Ctrl Pts',(-4.45403904311079,6.53800100966991,
120.332634069845));
#231141=CARTESIAN_POINT('Ctrl Pts',(-4.29309904742363,6.64764201818742,
120.32482419176));
#231142=CARTESIAN_POINT('Ctrl Pts',(-4.12809469697285,6.75134607155191,
120.317014313675));
#231143=CARTESIAN_POINT('Ctrl Pts',(-3.95951323902655,6.84880835693141,
120.30920443559));
#231144=CARTESIAN_POINT('Ctrl Pts',(-3.79091417992887,6.94628081809453,
120.301393742096));
#231145=CARTESIAN_POINT('Ctrl Pts',(-3.61873757474325,7.03751003765976,
120.293583048601));
#231146=CARTESIAN_POINT('Ctrl Pts',(-3.44349613871934,7.12223668117151,
120.285772355107));
#231147=CARTESIAN_POINT('Ctrl Pts',(-3.26813034162216,7.20702345142362,
120.27795611871));
#231148=CARTESIAN_POINT('Ctrl Pts',(-3.08969568584033,7.28529827283452,
120.270139882314));
#231149=CARTESIAN_POINT('Ctrl Pts',(-2.90872658560965,7.35684923388862,
120.262323645917));
#231150=CARTESIAN_POINT('Ctrl Pts',(-2.7276905784827,7.42842664836888,120.254504519744));
#231151=CARTESIAN_POINT('Ctrl Pts',(-2.54411859056901,7.49327512860597,
120.246685393572));
#231152=CARTESIAN_POINT('Ctrl Pts',(-2.35856127198287,7.5512323316332,120.238866267399));
#231153=CARTESIAN_POINT('Ctrl Pts',(-2.17279761910007,7.60925398137056,
120.231038446587));
#231154=CARTESIAN_POINT('Ctrl Pts',(-1.9850445641325,7.66036894975479,120.223210625776));
#231155=CARTESIAN_POINT('Ctrl Pts',(-1.79586513157526,7.70446555117175,
120.215382804964));
#231156=CARTESIAN_POINT('Ctrl Pts',(-1.64867029273373,7.73877579331218,
120.209292212518));
#231157=CARTESIAN_POINT('Ctrl Pts',(-1.50061219689754,7.76883818722276,
120.203201620073));
#231158=CARTESIAN_POINT('Ctrl Pts',(-1.3519584093979,7.79462182913695,120.197111027627));
#231159=CARTESIAN_POINT('Ctrl Pts',(-1.15384637310099,7.82898388535286,
120.188994048625));
#231160=CARTESIAN_POINT('Ctrl Pts',(-0.954282375878709,7.85581318678384,
120.180877069623));
#231161=CARTESIAN_POINT('Ctrl Pts',(-0.753866334332839,7.87499882856878,
120.172760090621));
#231162=CARTESIAN_POINT('Ctrl Pts',(-0.553596890164613,7.89417043672271,
120.164649048907));
#231163=CARTESIAN_POINT('Ctrl Pts',(-0.352476962419628,7.90570950263969,
120.156538007194));
#231164=CARTESIAN_POINT('Ctrl Pts',(-0.151114232342218,7.90955659242562,
120.14842696548));
#231165=CARTESIAN_POINT('Ctrl Pts',(0.0501298381038666,7.91340141518699,
120.140320703465));
#231166=CARTESIAN_POINT('Ctrl Pts',(0.251616105748743,7.90956329425575,
120.132214441451));
#231167=CARTESIAN_POINT('Ctrl Pts',(0.452733642698382,7.89803477130666,
120.124108179436));
#231168=CARTESIAN_POINT('Ctrl Pts',(0.653761229303729,7.8865114045196,120.116005542968));
#231169=CARTESIAN_POINT('Ctrl Pts',(0.854420094469794,7.86730451340781,
120.1079029065));
#231170=CARTESIAN_POINT('Ctrl Pts',(1.05410060874855,7.84045871787078,120.099800270033));
#231171=CARTESIAN_POINT('Ctrl Pts',(1.25372015268909,7.81362111941417,120.091700107619));
#231172=CARTESIAN_POINT('Ctrl Pts',(1.45236162407149,7.77914931137497,120.083599945206));
#231173=CARTESIAN_POINT('Ctrl Pts',(1.64942122828133,7.73713969188194,120.075499782793));
#231174=CARTESIAN_POINT('Ctrl Pts',(1.84840028926463,7.69472087818084,120.067320720842));
#231175=CARTESIAN_POINT('Ctrl Pts',(2.04576617395715,7.64461667052208,120.059141658892));
#231176=CARTESIAN_POINT('Ctrl Pts',(2.24090766890899,7.58697922887791,120.050962596941));
#231177=CARTESIAN_POINT('Ctrl Pts',(2.43416566604806,7.52989810148817,120.042862478965));
#231178=CARTESIAN_POINT('Ctrl Pts',(2.625241717471,7.46542863287169,120.03476236099));
#231179=CARTESIAN_POINT('Ctrl Pts',(2.81355695240561,7.39376888167125,120.026662243014));
#231180=CARTESIAN_POINT('Ctrl Pts',(3.00189753125902,7.32209948632854,120.018561034905));
#231181=CARTESIAN_POINT('Ctrl Pts',(3.18747625277086,7.24323799259667,120.010459826796));
#231182=CARTESIAN_POINT('Ctrl Pts',(3.36973331737352,7.15743098952291,120.002358618687));
#231183=CARTESIAN_POINT('Ctrl Pts',(3.55203844894086,7.07160135642272,119.994255274032));
#231184=CARTESIAN_POINT('Ctrl Pts',(3.73101988639512,6.97882269759998,119.986151929378));
#231185=CARTESIAN_POINT('Ctrl Pts',(3.90614107532493,6.8793882649302,119.978048584723));
#231186=CARTESIAN_POINT('Ctrl Pts',(4.08415480859021,6.77831143531962,119.969811393995));
#231187=CARTESIAN_POINT('Ctrl Pts',(4.25817935482203,6.67035720521288,119.961574203266));
#231188=CARTESIAN_POINT('Ctrl Pts',(4.42768062329741,6.55588020772776,119.953337012537));
#231189=CARTESIAN_POINT('Ctrl Pts',(4.59464480656754,6.44311669533496,119.945223115604));
#231190=CARTESIAN_POINT('Ctrl Pts',(4.75721993336558,6.32402453276771,119.93710921867));
#231191=CARTESIAN_POINT('Ctrl Pts',(4.91492768655627,6.19898433906093,119.928995321737));
#231192=CARTESIAN_POINT('Ctrl Pts',(5.07623008501358,6.07109409434934,119.92069648411));
#231193=CARTESIAN_POINT('Ctrl Pts',(5.23244030786489,5.93698167287731,119.912397646484));
#231194=CARTESIAN_POINT('Ctrl Pts',(5.38308501857763,5.79709553852316,119.904098808857));
#231195=CARTESIAN_POINT('Ctrl Pts',(5.53372972929025,5.65720940416911,119.895799971231));
#231196=CARTESIAN_POINT('Ctrl Pts',(5.67880870147179,5.51154983408021,119.887501133604));
#231197=CARTESIAN_POINT('Ctrl Pts',(5.81789105147127,5.36060301768472,119.879202295978));
#231198=CARTESIAN_POINT('Ctrl Pts',(5.95069117764302,5.21647433232227,119.871278309333));
#231199=CARTESIAN_POINT('Ctrl Pts',(6.0783092372046,5.06721585926902,119.863354322688));
#231200=CARTESIAN_POINT('Ctrl Pts',(6.20032688890408,4.9132339116648,119.855430336044));
#231201=CARTESIAN_POINT('Ctrl Pts',(6.32221389513008,4.75941683401319,119.847514833688));
#231202=CARTESIAN_POINT('Ctrl Pts',(6.43851222620911,4.60088662091117,119.839599331332));
#231203=CARTESIAN_POINT('Ctrl Pts',(6.54884061410087,4.43808603016018,119.831683828976));
#231204=CARTESIAN_POINT('Ctrl Pts',(6.65906907508675,4.27543289157104,119.823775495869));
#231205=CARTESIAN_POINT('Ctrl Pts',(6.76333817336143,4.10851736181211,119.815867162762));
#231206=CARTESIAN_POINT('Ctrl Pts',(6.86130698010753,3.93781506989952,119.807958829655));
#231207=CARTESIAN_POINT('Ctrl Pts',(6.95918939571486,3.76726330717961,119.800057470298));
#231208=CARTESIAN_POINT('Ctrl Pts',(7.05078242589187,3.59293173501396,119.79215611094));
#231209=CARTESIAN_POINT('Ctrl Pts',(7.13578851470322,3.41532476836824,119.784254751582));
#231210=CARTESIAN_POINT('Ctrl Pts',(7.22075083607071,3.23780924697133,119.776357460431));
#231211=CARTESIAN_POINT('Ctrl Pts',(7.29913282465987,3.05702199843288,119.768460169279));
#231212=CARTESIAN_POINT('Ctrl Pts',(7.37068263227046,2.87349239329888,119.760562878128));
#231213=CARTESIAN_POINT('Ctrl Pts',(7.44220811533019,2.69002518211625,119.752668271792));
#231214=CARTESIAN_POINT('Ctrl Pts',(7.50690592054313,2.50381779018915,119.744773665457));
#231215=CARTESIAN_POINT('Ctrl Pts',(7.5645720438335,2.31542021966913,119.736879059121));
#231216=CARTESIAN_POINT('Ctrl Pts',(7.60506605087208,2.18312465146743,119.731335349465));
#231217=CARTESIAN_POINT('Ctrl Pts',(7.64209368900089,2.04974954280903,119.725791639809));
#231218=CARTESIAN_POINT('Ctrl Pts',(7.67559886220684,1.9154903044623,119.720247930153));
#231219=CARTESIAN_POINT('Ctrl Pts',(7.72709100046858,1.70915514477309,119.711728127484));
#231220=CARTESIAN_POINT('Ctrl Pts',(7.77021027758681,1.50093760967826,119.703208324815));
#231221=CARTESIAN_POINT('Ctrl Pts',(7.80486517080185,1.29151100096133,119.694688522146));
#231222=CARTESIAN_POINT('Ctrl Pts',(7.83958274037241,1.08170562620691,119.686153310681));
#231223=CARTESIAN_POINT('Ctrl Pts',(7.86580528925962,0.870687053414497,
119.677618099217));
#231224=CARTESIAN_POINT('Ctrl Pts',(7.88349314166519,0.659133435138885,
119.669082887752));
#231225=CARTESIAN_POINT('Ctrl Pts',(7.90210781074785,0.436494727671951,
119.660100444133));
#231226=CARTESIAN_POINT('Ctrl Pts',(7.91126947324658,0.213263758363993,
119.651118000514));
#231227=CARTESIAN_POINT('Ctrl Pts',(7.91099396437362,-0.00977218728067248,
119.642135556896));
#231228=CARTESIAN_POINT('Ctrl Pts',(7.91073107405129,-0.222592888874181,
119.633564517159));
#231229=CARTESIAN_POINT('Ctrl Pts',(7.90187616522459,-0.435235809622482,
119.624993477421));
#231230=CARTESIAN_POINT('Ctrl Pts',(7.88449626961741,-0.647023627380878,
119.616422437684));
#231231=CARTESIAN_POINT('Ctrl Pts',(7.86709456537519,-0.85907720066102,
119.607840642838));
#231232=CARTESIAN_POINT('Ctrl Pts',(7.84114652881282,-1.07027327980192,
119.599258847991));
#231233=CARTESIAN_POINT('Ctrl Pts',(7.80677070269115,-1.27994226260526,
119.590677053144));
#231234=CARTESIAN_POINT('Ctrl Pts',(7.77233737656482,-1.48996195603431,
119.582080903639));
#231235=CARTESIAN_POINT('Ctrl Pts',(7.72944811778225,-1.69844920048983,
119.573484754134));
#231236=CARTESIAN_POINT('Ctrl Pts',(7.67827243744755,-1.90474496359311,
119.564888604629));
#231237=CARTESIAN_POINT('Ctrl Pts',(7.67113828848329,-1.93350363753839,
119.563690257862));
#231238=CARTESIAN_POINT('Ctrl Pts',(7.66384318186019,-1.96221974818347,
119.562491911095));
#231239=CARTESIAN_POINT('Ctrl Pts',(7.6563876530204,-1.99089153563845,119.561293564328));
#231240=CARTESIAN_POINT('Ctrl Pts',(7.60718904108358,-2.18009503479242,
119.553385741981));
#231241=CARTESIAN_POINT('Ctrl Pts',(7.55090996100169,-2.36771584605605,
119.545477919635));
#231242=CARTESIAN_POINT('Ctrl Pts',(7.48766754116734,-2.55318542079281,
119.537570097288));
#231243=CARTESIAN_POINT('Ctrl Pts',(7.42448973161107,-2.73846551446876,
119.529670353801));
#231244=CARTESIAN_POINT('Ctrl Pts',(7.35436286295951,-2.92159842557687,
119.521770610313));
#231245=CARTESIAN_POINT('Ctrl Pts',(7.27745470569158,-3.10202740262033,
119.513870866826));
#231246=CARTESIAN_POINT('Ctrl Pts',(7.20061083917921,-3.28230555151149,
119.505977727065));
#231247=CARTESIAN_POINT('Ctrl Pts',(7.11699711146433,-3.45988395372397,
119.498084587305));
#231248=CARTESIAN_POINT('Ctrl Pts',(7.02683065685552,-3.63422232669872,
119.490191447545));
#231249=CARTESIAN_POINT('Ctrl Pts',(6.93672283806905,-3.80844732631406,
119.482303440744));
#231250=CARTESIAN_POINT('Ctrl Pts',(6.84007094039396,-3.97943618941263,
119.474415433942));
#231251=CARTESIAN_POINT('Ctrl Pts',(6.73713974614513,-4.14666963247755,
119.466527427141));
#231252=CARTESIAN_POINT('Ctrl Pts',(6.63425638482468,-4.3138253608578,119.458643085959));
#231253=CARTESIAN_POINT('Ctrl Pts',(6.52509972209648,-4.47722885365726,
119.450758744776));
#231254=CARTESIAN_POINT('Ctrl Pts',(6.409980050507,-4.63638617374592,119.442874403593));
#231255=CARTESIAN_POINT('Ctrl Pts',(6.29489251298313,-4.79549906726788,
119.434992263215));
#231256=CARTESIAN_POINT('Ctrl Pts',(6.17384548609188,-4.9503678712725,119.427110122837));
#231257=CARTESIAN_POINT('Ctrl Pts',(6.04719223231534,-5.10052812024647,
119.419227982459));
#231258=CARTESIAN_POINT('Ctrl Pts',(5.92052512982028,-5.25070478827767,
119.41134498022));
#231259=CARTESIAN_POINT('Ctrl Pts',(5.78825079264541,-5.3961716043426,119.40346197798));
#231260=CARTESIAN_POINT('Ctrl Pts',(5.6507627768379,-5.53649718142286,119.395578975741));
#231261=CARTESIAN_POINT('Ctrl Pts',(5.51325817950287,-5.67683968225028,
119.387695022785));
#231262=CARTESIAN_POINT('Ctrl Pts',(5.37053889165724,-5.81203946155636,
119.379811069828));
#231263=CARTESIAN_POINT('Ctrl Pts',(5.22303531336471,-5.94170203858669,
119.371927116872));
#231264=CARTESIAN_POINT('Ctrl Pts',(5.075489139727,-6.07140205892714,119.364040887227));
#231265=CARTESIAN_POINT('Ctrl Pts',(4.92315618160286,-6.19556146279644,
119.356154657582));
#231266=CARTESIAN_POINT('Ctrl Pts',(4.76650006525322,-6.31382595008296,
119.348268427937));
#231267=CARTESIAN_POINT('Ctrl Pts',(4.60977236485902,-6.43214447835125,
119.340378594678));
#231268=CARTESIAN_POINT('Ctrl Pts',(4.44871784478241,-6.54456251468769,
119.332488761419));
#231269=CARTESIAN_POINT('Ctrl Pts',(4.28382944230653,-6.65076885098465,
119.324598928159));
#231270=CARTESIAN_POINT('Ctrl Pts',(4.11875088070683,-6.75709767075257,
119.316699995875));
#231271=CARTESIAN_POINT('Ctrl Pts',(3.9498298952369,-6.85720029470447,119.30880106359));
#231272=CARTESIAN_POINT('Ctrl Pts',(3.77758538487601,-6.95081071961905,
119.300902131305));
#231273=CARTESIAN_POINT('Ctrl Pts',(3.60522710958061,-7.04448297282552,
119.292997981893));
#231274=CARTESIAN_POINT('Ctrl Pts',(3.4295412413218,-7.131654325894,119.285093832481));
#231275=CARTESIAN_POINT('Ctrl Pts',(3.25106724203831,-7.21210668166698,
119.27718968307));
#231276=CARTESIAN_POINT('Ctrl Pts',(3.07234865058636,-7.29266929448711,
119.269274701306));
#231277=CARTESIAN_POINT('Ctrl Pts',(2.89083461439281,-7.36649438833812,
119.261359719543));
#231278=CARTESIAN_POINT('Ctrl Pts',(2.70708146099895,-7.43341314360475,
119.25344473778));
#231279=CARTESIAN_POINT('Ctrl Pts',(2.62923165916585,-7.46176428610328,
119.25009143608));
#231280=CARTESIAN_POINT('Ctrl Pts',(2.55098010368526,-7.4888764183176,119.246738134379));
#231281=CARTESIAN_POINT('Ctrl Pts',(2.47236966538131,-7.5147394657235,119.243384832678));
#231282=CARTESIAN_POINT('Ctrl Pts',(2.29044769764415,-7.57459228651009,
119.235624549732));
#231283=CARTESIAN_POINT('Ctrl Pts',(2.10603030035115,-7.62794040411432,
119.227864266785));
#231284=CARTESIAN_POINT('Ctrl Pts',(1.91963366571711,-7.67456367420621,
119.220103983839));
#231285=CARTESIAN_POINT('Ctrl Pts',(1.73346136875679,-7.72113083086035,
119.212353040781));
#231286=CARTESIAN_POINT('Ctrl Pts',(1.54531491949674,-7.76098916388495,
119.204602097723));
#231287=CARTESIAN_POINT('Ctrl Pts',(1.35572989318228,-7.79396673438705,
119.196851154665));
#231288=CARTESIAN_POINT('Ctrl Pts',(1.16633456184877,-7.82691130819247,
119.189107967046));
#231289=CARTESIAN_POINT('Ctrl Pts',(0.975503869296235,-7.85298876381619,
119.181364779426));
#231290=CARTESIAN_POINT('Ctrl Pts',(0.783788036869903,-7.87207706474344,
119.173621591807));
#231291=CARTESIAN_POINT('Ctrl Pts',(0.592225175821566,-7.89115013498442,
119.16588458253));
#231292=CARTESIAN_POINT('Ctrl Pts',(0.399778936163565,-7.90324511807019,
119.158147573253));
#231293=CARTESIAN_POINT('Ctrl Pts',(0.207009301237229,-7.90829110169835,
119.150410563976));
#231294=CARTESIAN_POINT('Ctrl Pts',(0.0143544498453649,-7.91333408072552,
119.142678161655));
#231295=CARTESIAN_POINT('Ctrl Pts',(-0.178623055673287,-7.91133640881234,
119.134945759334));
#231296=CARTESIAN_POINT('Ctrl Pts',(-0.371358452897033,-7.9022790319921,
119.127213357014));
#231297=CARTESIAN_POINT('Ctrl Pts',(-0.564018081155927,-7.89322521584662,
119.119483994488));
#231298=CARTESIAN_POINT('Ctrl Pts',(-0.75643543260841,-7.87711723920018,
119.111754631962));
#231299=CARTESIAN_POINT('Ctrl Pts',(-0.948045998137102,-7.85398814523018,
119.104025269437));
#231300=CARTESIAN_POINT('Ctrl Pts',(-1.13965648890694,-7.83085906028424,
119.096295909927));
#231301=CARTESIAN_POINT('Ctrl Pts',(-1.3304598366005,-7.80070889512617,
119.088566550417));
#231302=CARTESIAN_POINT('Ctrl Pts',(-1.5198964984915,-7.76362258445587,
119.080837190907));
#231303=CARTESIAN_POINT('Ctrl Pts',(-1.709342655628,-7.72653441488656,119.073107443974));
#231304=CARTESIAN_POINT('Ctrl Pts',(-1.89742163769417,-7.6825094755358,
119.065377697041));
#231305=CARTESIAN_POINT('Ctrl Pts',(-2.08358411429127,-7.63168384032469,
119.057647950107));
#231306=CARTESIAN_POINT('Ctrl Pts',(-2.26979003381238,-7.58084634443012,
119.049916399359));
#231307=CARTESIAN_POINT('Ctrl Pts',(-2.45407821065823,-7.52320508683362,
119.04218484861));
#231308=CARTESIAN_POINT('Ctrl Pts',(-2.63591444857387,-7.45894603947498,
119.034453297861));
#231309=CARTESIAN_POINT('Ctrl Pts',(-2.81782644964922,-7.39466021819865,
119.026718525715));
#231310=CARTESIAN_POINT('Ctrl Pts',(-2.9972841391664,-7.32375123608725,
119.018983753569));
#231311=CARTESIAN_POINT('Ctrl Pts',(-3.17377322716147,-7.24645323607026,
119.011248981423));
#231312=CARTESIAN_POINT('Ctrl Pts',(-3.35047277848421,-7.16906305814872,
119.003504985557));
#231313=CARTESIAN_POINT('Ctrl Pts',(-3.52419632934436,-7.08526879055976,
118.995760989692));
#231314=CARTESIAN_POINT('Ctrl Pts',(-3.694453207486,-6.99535106322023,118.988016993826));
#231315=CARTESIAN_POINT('Ctrl Pts',(-3.86482059088245,-6.90537497476495,
118.980267971719));
#231316=CARTESIAN_POINT('Ctrl Pts',(-4.0317165097013,-6.80926768825269,
118.972518949611));
#231317=CARTESIAN_POINT('Ctrl Pts',(-4.19467935553122,-6.7073531369893,
118.964769927504));
#231318=CARTESIAN_POINT('Ctrl Pts',(-4.35789124697762,-6.60528283628425,
118.957009063065));
#231319=CARTESIAN_POINT('Ctrl Pts',(-4.51715776492919,-6.49738774640278,
118.949248198626));
#231320=CARTESIAN_POINT('Ctrl Pts',(-4.6720495024841,-6.38403277296867,
118.941487334188));
#231321=CARTESIAN_POINT('Ctrl Pts',(-4.77856717819169,-6.30607956196659,
118.936150256468));
#231322=CARTESIAN_POINT('Ctrl Pts',(-4.88301665375129,-6.22554509245663,
118.930813178748));
#231323=CARTESIAN_POINT('Ctrl Pts',(-4.98526863013717,-6.14255791062406,
118.925476101028));
#231324=CARTESIAN_POINT('Ctrl Pts',(-5.13739362236662,-6.01909404383501,
118.917535883779));
#231325=CARTESIAN_POINT('Ctrl Pts',(-5.28513570249431,-5.8898081660217,
118.90959566653));
#231326=CARTESIAN_POINT('Ctrl Pts',(-5.42802194939112,-5.75504115684052,
118.901655449281));
#231327=CARTESIAN_POINT('Ctrl Pts',(-5.57074417390803,-5.62042884978118,
118.893724346788));
#231328=CARTESIAN_POINT('Ctrl Pts',(-5.7086214224054,-5.48034817828785,
118.885793244296));
#231329=CARTESIAN_POINT('Ctrl Pts',(-5.84121220755203,-5.33518143518523,
118.877862141803));
#231330=CARTESIAN_POINT('Ctrl Pts',(-5.97367496823488,-5.19015485939834,
118.869938697272));
#231331=CARTESIAN_POINT('Ctrl Pts',(-6.10086120575228,-5.04005224749073,
118.862015252741));
#231332=CARTESIAN_POINT('Ctrl Pts',(-6.22236458861824,-4.88529425176311,
118.85409180821));
#231333=CARTESIAN_POINT('Ctrl Pts',(-6.34377280199706,-4.7306574727353,
118.846174569845));
#231334=CARTESIAN_POINT('Ctrl Pts',(-6.45950681961976,-4.57137284403264,
118.83825733148));
#231335=CARTESIAN_POINT('Ctrl Pts',(-6.56919888362942,-4.40789598644547,
118.830340093115));
#231336=CARTESIAN_POINT('Ctrl Pts',(-6.67882041729674,-4.24452424201149,
118.822427945414));
#231337=CARTESIAN_POINT('Ctrl Pts',(-6.7824075511453,-4.07696592563811,
118.814515797714));
#231338=CARTESIAN_POINT('Ctrl Pts',(-6.87963422419451,-3.90570786686506,
118.806603650014));
#231339=CARTESIAN_POINT('Ctrl Pts',(-6.97682642627412,-3.73451052632038,
118.798694307504));
#231340=CARTESIAN_POINT('Ctrl Pts',(-7.06766249101362,-3.55961635387914,
118.790784964995));
#231341=CARTESIAN_POINT('Ctrl Pts',(-7.15186067466932,-3.38153957393944,
118.782875622486));
#231342=CARTESIAN_POINT('Ctrl Pts',(-7.23604290927774,-3.20349652578421,
118.774967778186));
#231343=CARTESIAN_POINT('Ctrl Pts',(-7.31358962186788,-3.02227238087351,
118.767059933886));
#231344=CARTESIAN_POINT('Ctrl Pts',(-7.38426575303584,-2.83840453222265,
118.759152089586));
#231345=CARTESIAN_POINT('Ctrl Pts',(-7.45494016611141,-2.65454115328379,
118.75124443752));
#231346=CARTESIAN_POINT('Ctrl Pts',(-7.51874420845123,-2.46803451864746,
118.743336785455));
#231347=CARTESIAN_POINT('Ctrl Pts',(-7.57549145837475,-2.27944075687244,
118.735429133389));
#231348=CARTESIAN_POINT('Ctrl Pts',(-7.63226697869891,-2.09075304127216,
118.727517541882));
#231349=CARTESIAN_POINT('Ctrl Pts',(-7.68197858067864,-1.89997644855941,
118.719605950375));
#231350=CARTESIAN_POINT('Ctrl Pts',(-7.72448986496527,-1.70768185738702,
118.711694358868));
#231351=CARTESIAN_POINT('Ctrl Pts',(-7.76701132841194,-1.5153412220301,
118.703780872961));
#231352=CARTESIAN_POINT('Ctrl Pts',(-7.80232897046963,-1.32148219976192,
118.695867387054));
#231353=CARTESIAN_POINT('Ctrl Pts',(-7.83035771582106,-1.12668497916744,
118.687953901147));
#231354=CARTESIAN_POINT('Ctrl Pts',(-7.85841247724998,-0.931706949210253,
118.680033070001));
#231355=CARTESIAN_POINT('Ctrl Pts',(-7.87916478002963,-0.735789321072113,
118.672112238854));
#231356=CARTESIAN_POINT('Ctrl Pts',(-7.89258143142248,-0.539517699770027,
118.664191407707));
#231357=CARTESIAN_POINT('Ctrl Pts',(-7.90486777183239,-0.359781349654463,
118.656937881849));
#231358=CARTESIAN_POINT('Ctrl Pts',(-7.9110030092443,-0.179748378292146,
118.649684355992));
#231359=CARTESIAN_POINT('Ctrl Pts',(-7.91099999889219,0.000132392670232489,
118.642430830134));
#231360=CARTESIAN_POINT('',(-7.91099996199236,-0.000775472076273572,114.634517289408));
#231361=CARTESIAN_POINT('Ctrl Pts',(-7.91099999750142,0.000198827776959343,
118.644324710193));
#231362=CARTESIAN_POINT('Ctrl Pts',(-7.91099106136341,0.355751702830156,
118.631767639541));
#231363=CARTESIAN_POINT('Ctrl Pts',(-7.88701277954247,0.710905018268822,
118.618770631039));
#231364=CARTESIAN_POINT('Ctrl Pts',(-7.83644873986753,1.08370568293652,
118.60384143357));
#231365=CARTESIAN_POINT('Ctrl Pts',(-7.83359517610902,1.10414377095752,
118.603019502035));
#231366=CARTESIAN_POINT('Ctrl Pts',(-7.82901350979031,1.1360470478016,118.601731273111));
#231367=CARTESIAN_POINT('Ctrl Pts',(-7.82734010322373,1.14752008178653,
118.601266946033));
#231368=CARTESIAN_POINT('Ctrl Pts',(-7.82449765892094,1.16671262214085,
118.60048847286));
#231369=CARTESIAN_POINT('Ctrl Pts',(-7.82334240166554,1.17443417138983,
118.600174808686));
#231370=CARTESIAN_POINT('Ctrl Pts',(-7.82122460117877,1.18844741145488,
118.599604725457));
#231371=CARTESIAN_POINT('Ctrl Pts',(-7.82026589108492,1.19473968057792,
118.599348437834));
#231372=CARTESIAN_POINT('Ctrl Pts',(-7.81829152397392,1.20759377912051,
118.598824263193));
#231373=CARTESIAN_POINT('Ctrl Pts',(-7.81727519732579,1.21415550000509,
118.598556353796));
#231374=CARTESIAN_POINT('Ctrl Pts',(-7.81503628937616,1.22849123963937,
118.597970324945));
#231375=CARTESIAN_POINT('Ctrl Pts',(-7.81381036744397,1.23626472540433,
118.597652095217));
#231376=CARTESIAN_POINT('Ctrl Pts',(-7.81042331473759,1.25753548323976,
118.596780079973));
#231377=CARTESIAN_POINT('Ctrl Pts',(-7.8082388020532,1.27102897474806,118.596225538105));
#231378=CARTESIAN_POINT('Ctrl Pts',(-7.79738594568447,1.33698187922346,
118.593508576135));
#231379=CARTESIAN_POINT('Ctrl Pts',(-7.78822393567046,1.38935809875853,
118.591330811541));
#231380=CARTESIAN_POINT('Ctrl Pts',(-7.70012354868957,1.86471476825476,
118.571400921319));
#231381=CARTESIAN_POINT('Ctrl Pts',(-7.58732784647485,2.28068047838237,
118.552822236139));
#231382=CARTESIAN_POINT('Ctrl Pts',(-7.41540952306428,2.75706883980788,
118.531032738851));
#231383=CARTESIAN_POINT('Ctrl Pts',(-7.38851018548077,2.8283642379192,118.527756104055));
#231384=CARTESIAN_POINT('Ctrl Pts',(-7.13734293989879,3.46602276743735,
118.498325232205));
#231385=CARTESIAN_POINT('Ctrl Pts',(-6.84938009783869,4.00512489118188,
118.472784453132));
#231386=CARTESIAN_POINT('Ctrl Pts',(-6.36931748935878,4.69790541579123,
118.438088876225));
#231387=CARTESIAN_POINT('Ctrl Pts',(-6.22778336131068,4.88397770089324,
118.428519820094));
#231388=CARTESIAN_POINT('Ctrl Pts',(-6.05541147508588,5.09089212345301,
118.417608050055));
#231389=CARTESIAN_POINT('Ctrl Pts',(-6.03241913001597,5.11811588370871,
118.416166635528));
#231390=CARTESIAN_POINT('Ctrl Pts',(-5.99391169001065,5.16309009869847,
118.413775754193));
#231391=CARTESIAN_POINT('Ctrl Pts',(-5.97849981594452,5.18092816683152,
118.412824908859));
#231392=CARTESIAN_POINT('Ctrl Pts',(-5.94816135999849,5.21572697584266,
118.410964943565));
#231393=CARTESIAN_POINT('Ctrl Pts',(-5.93324139611308,5.23269318710021,
118.410055741633));
#231394=CARTESIAN_POINT('Ctrl Pts',(-5.90500037625875,5.26453133395445,
118.408345054883));
#231395=CARTESIAN_POINT('Ctrl Pts',(-5.89169530800487,5.27941720363808,
118.407543348253));
#231396=CARTESIAN_POINT('Ctrl Pts',(-5.86159034698265,5.31284345481193,
118.405738840661));
#231397=CARTESIAN_POINT('Ctrl Pts',(-5.84475855154929,5.33135484192352,
118.404736519601));
#231398=CARTESIAN_POINT('Ctrl Pts',(-5.79517202648474,5.3853723835909,118.401802790383));
#231399=CARTESIAN_POINT('Ctrl Pts',(-5.76217947365969,5.42065884166639,
118.399875013768));
#231400=CARTESIAN_POINT('Ctrl Pts',(-5.4453582577686,5.753346819243,118.381587992475));
#231401=CARTESIAN_POINT('Ctrl Pts',(-5.13907273323627,6.02850500968855,
118.365645121367));
#231402=CARTESIAN_POINT('Ctrl Pts',(-4.59084093686234,6.4487442649206,118.339066656222));
#231403=CARTESIAN_POINT('Ctrl Pts',(-4.36003503901393,6.60698230071374,
118.328372571815));
#231404=CARTESIAN_POINT('Ctrl Pts',(-3.96026396694388,6.85097363783537,
118.310219311058));
#231405=CARTESIAN_POINT('Ctrl Pts',(-3.79572699290668,6.94348499568284,
118.302842968806));
#231406=CARTESIAN_POINT('Ctrl Pts',(-3.59628254169681,7.046414007054,118.293895506484));
#231407=CARTESIAN_POINT('Ctrl Pts',(-3.564410431711,7.06258994430526,118.292465440846));
#231408=CARTESIAN_POINT('Ctrl Pts',(-3.51985132493643,7.0848264111623,118.290464814799));
#231409=CARTESIAN_POINT('Ctrl Pts',(-3.50725597643418,7.09107002782422,
118.28989915939));
#231410=CARTESIAN_POINT('Ctrl Pts',(-3.48560266717887,7.10173194463671,
118.288926507233));
#231411=CARTESIAN_POINT('Ctrl Pts',(-3.47655276299725,7.10616657926794,
118.288519930332));
#231412=CARTESIAN_POINT('Ctrl Pts',(-3.46144228021639,7.11353524484304,
118.287840989445));
#231413=CARTESIAN_POINT('Ctrl Pts',(-3.45538637631346,7.11647885748803,
118.287568863956));
#231414=CARTESIAN_POINT('Ctrl Pts',(-3.437701886152,7.1250469191751,118.286774142821));
#231415=CARTESIAN_POINT('Ctrl Pts',(-3.42606329110939,7.13065061424208,
118.286251043711));
#231416=CARTESIAN_POINT('Ctrl Pts',(-3.39079549424877,7.14752490594762,
118.284665763407));
#231417=CARTESIAN_POINT('Ctrl Pts',(-3.36712409314705,7.15870670548321,
118.283601519787));
#231418=CARTESIAN_POINT('Ctrl Pts',(-3.15742247371022,7.25649447877688,
118.274173061075));
#231419=CARTESIAN_POINT('Ctrl Pts',(-2.96814693131328,7.33594773395008,
118.265661294186));
#231420=CARTESIAN_POINT('Ctrl Pts',(-2.67972256895294,7.4440297723605,118.252791580943));
#231421=CARTESIAN_POINT('Ctrl Pts',(-2.58274988674574,7.47822807565744,
118.248480890511));
#231422=CARTESIAN_POINT('Ctrl Pts',(-2.14481439325722,7.62313541998329,
118.229115938397));
#231423=CARTESIAN_POINT('Ctrl Pts',(-1.79722396849072,7.71248440121074,
118.21403978491));
#231424=CARTESIAN_POINT('Ctrl Pts',(-1.26691953518036,7.81098961437478,
118.191673498208));
#231425=CARTESIAN_POINT('Ctrl Pts',(-1.08798416761233,7.8379165674423,118.184228848384));
#231426=CARTESIAN_POINT('Ctrl Pts',(-0.813143558300402,7.86968173154199,
118.172940058753));
#231427=CARTESIAN_POINT('Ctrl Pts',(-0.717813786335819,7.87894895602759,
118.169050867178));
#231428=CARTESIAN_POINT('Ctrl Pts',(-0.594684962985234,7.88866530395628,
118.164058056211));
#231429=CARTESIAN_POINT('Ctrl Pts',(-0.567020027395226,7.89070204596984,
118.162938230848));
#231430=CARTESIAN_POINT('Ctrl Pts',(-0.512440120997703,7.8944317952196,
118.160732663178));
#231431=CARTESIAN_POINT('Ctrl Pts',(-0.485526069874737,7.89613276791149,
118.15964685432));
#231432=CARTESIAN_POINT('Ctrl Pts',(-0.434433687490773,7.89909960280163,
118.157588831313));
#231433=CARTESIAN_POINT('Ctrl Pts',(-0.410257223797544,7.90039215345614,
118.156616362609));
#231434=CARTESIAN_POINT('Ctrl Pts',(-0.355166678512057,7.90308390729053,
118.154403381692));
#231435=CARTESIAN_POINT('Ctrl Pts',(-0.324249529550282,7.90441274646032,
118.153163572298));
#231436=CARTESIAN_POINT('Ctrl Pts',(-0.24342019827765,7.90741181145971,
118.149927406893));
#231437=CARTESIAN_POINT('Ctrl Pts',(-0.193498505245793,7.90879088808833,
118.147933849117));
#231438=CARTESIAN_POINT('Ctrl Pts',(0.100507788589648,7.91412732279716,
118.136219368982));
#231439=CARTESIAN_POINT('Ctrl Pts',(0.344661485737856,7.90725769782168,
118.126584499178));
#231440=CARTESIAN_POINT('Ctrl Pts',(0.899194143444628,7.86591915778065,
118.104810475318));
#231441=CARTESIAN_POINT('Ctrl Pts',(1.20864364230712,7.82434818916022,118.092788265135));
#231442=CARTESIAN_POINT('Ctrl Pts',(1.93502465328261,7.68263484486815,118.064750749951));
#231443=CARTESIAN_POINT('Ctrl Pts',(2.34785991602701,7.56668706509408,118.04898910486));
#231444=CARTESIAN_POINT('Ctrl Pts',(2.97075612076491,7.3358241341791,118.024252212511));
#231445=CARTESIAN_POINT('Ctrl Pts',(3.1884335535939,7.24386588900238,118.015401345471));
#231446=CARTESIAN_POINT('Ctrl Pts',(3.47991695237149,7.10504127987971,118.002959158468));
#231447=CARTESIAN_POINT('Ctrl Pts',(3.5575510323201,7.06648878177986,117.99958536408));
#231448=CARTESIAN_POINT('Ctrl Pts',(3.67666333569253,7.00487811512001,117.994295836328));
#231449=CARTESIAN_POINT('Ctrl Pts',(3.71859486811153,6.98270884330381,117.992411636314));
#231450=CARTESIAN_POINT('Ctrl Pts',(3.77084777518922,6.95447849467578,117.990033082974));
#231451=CARTESIAN_POINT('Ctrl Pts',(3.78135862597255,6.9487690288601,117.989553068733));
#231452=CARTESIAN_POINT('Ctrl Pts',(3.79698649552106,6.94023405367322,117.98883698945));
#231453=CARTESIAN_POINT('Ctrl Pts',(3.8021134238384,6.93742666116076,117.988601688154));
#231454=CARTESIAN_POINT('Ctrl Pts',(3.81204023105679,6.93197665165687,117.988145346754));
#231455=CARTESIAN_POINT('Ctrl Pts',(3.81684048634643,6.92933472448194,117.987924336257));
#231456=CARTESIAN_POINT('Ctrl Pts',(3.82679765568827,6.92384108919891,117.987465181269));
#231457=CARTESIAN_POINT('Ctrl Pts',(3.83195413425719,6.92098860270391,117.987227003008));
#231458=CARTESIAN_POINT('Ctrl Pts',(3.84448670292844,6.91403747434703,117.986647144444));
#231459=CARTESIAN_POINT('Ctrl Pts',(3.85185942211341,6.90993279252586,117.986305197405));
#231460=CARTESIAN_POINT('Ctrl Pts',(3.87958544538451,6.89443846542512,117.985016106696));
#231461=CARTESIAN_POINT('Ctrl Pts',(3.89989478618646,6.88297069747746,117.984065434212));
#231462=CARTESIAN_POINT('Ctrl Pts',(4.12761216870934,6.75305754506152,117.973330748972));
#231463=CARTESIAN_POINT('Ctrl Pts',(4.32956761866814,6.62538888642573,117.963042008483));
#231464=CARTESIAN_POINT('Ctrl Pts',(4.59286943636232,6.44175709700302,117.948780094229));
#231465=CARTESIAN_POINT('Ctrl Pts',(4.65958468824241,6.39366516472849,117.945091026266));
#231466=CARTESIAN_POINT('Ctrl Pts',(5.14334612085052,6.03335038877545,117.917840476475));
#231467=CARTESIAN_POINT('Ctrl Pts',(5.52939826495414,5.68164675462671,117.89340905128));
#231468=CARTESIAN_POINT('Ctrl Pts',(5.94470320214601,5.2205684201839,117.865422654086));
#231469=CARTESIAN_POINT('Ctrl Pts',(6.00992587536757,5.1453495925788,117.860966317115));
#231470=CARTESIAN_POINT('Ctrl Pts',(6.22010001454147,4.89351336443058,117.846417871602));
#231471=CARTESIAN_POINT('Ctrl Pts',(6.35882649361934,4.71184179482672,117.836510816682));
#231472=CARTESIAN_POINT('Ctrl Pts',(6.57359713123326,4.40378964132639,117.820690995779));
#231473=CARTESIAN_POINT('Ctrl Pts',(6.65431589229357,4.28084400348727,117.814615313237));
#231474=CARTESIAN_POINT('Ctrl Pts',(6.7415008771862,4.13961891592254,117.807895559324));
#231475=CARTESIAN_POINT('Ctrl Pts',(6.75138031963018,4.12348670812215,117.807131681476));
#231476=CARTESIAN_POINT('Ctrl Pts',(6.76611132695088,4.09923748124737,117.805988996535));
#231477=CARTESIAN_POINT('Ctrl Pts',(6.77100632422291,4.09114699986086,117.805608673903));
#231478=CARTESIAN_POINT('Ctrl Pts',(6.77939101909424,4.07723245685653,117.80495614661));
#231479=CARTESIAN_POINT('Ctrl Pts',(6.78288774104903,4.07141265282832,117.804683697482));
#231480=CARTESIAN_POINT('Ctrl Pts',(6.79006506406966,4.05943209416671,117.804123807184));
#231481=CARTESIAN_POINT('Ctrl Pts',(6.793744783667,4.0532708170304,117.803836396795));
#231482=CARTESIAN_POINT('Ctrl Pts',(6.80360455741841,4.03671058624747,117.803065305712));
#231483=CARTESIAN_POINT('Ctrl Pts',(6.80976916296643,4.02630243269858,117.80258216138));
#231484=CARTESIAN_POINT('Ctrl Pts',(6.83214921944812,3.98831811979547,117.80082433255));
#231485=CARTESIAN_POINT('Ctrl Pts',(6.84822133197127,3.96065764729153,117.799554608042));
#231486=CARTESIAN_POINT('Ctrl Pts',(7.10145378703417,3.51868881962593,117.779428478398));
#231487=CARTESIAN_POINT('Ctrl Pts',(7.30081185460424,3.08383307414289,117.761961722015));
#231488=CARTESIAN_POINT('Ctrl Pts',(7.54591783043798,2.38956664829265,117.736053227547));
#231489=CARTESIAN_POINT('Ctrl Pts',(7.62005041465412,2.14143377204158,117.72714044994));
#231490=CARTESIAN_POINT('Ctrl Pts',(7.7746470775141,1.51311465575999,117.704784800351));
#231491=CARTESIAN_POINT('Ctrl Pts',(7.83952366448432,1.12981844899826,117.691341788531));
#231492=CARTESIAN_POINT('Ctrl Pts',(7.89065725190166,0.588032903391812,
117.671094480529));
#231493=CARTESIAN_POINT('Ctrl Pts',(7.90071746309055,0.432336532810252,
117.665131225176));
#231494=CARTESIAN_POINT('Ctrl Pts',(7.90710741650846,0.249590867320354,
117.657874724475));
#231495=CARTESIAN_POINT('Ctrl Pts',(7.90790969886776,0.222727332230216,
117.656801624431));
#231496=CARTESIAN_POINT('Ctrl Pts',(7.90879013129322,0.187176691278592,
117.655373513505));
#231497=CARTESIAN_POINT('Ctrl Pts',(7.90899088733893,0.178492570427434,
117.655024031185));
#231498=CARTESIAN_POINT('Ctrl Pts',(7.90929714994126,0.164227736506731,
117.654448942656));
#231499=CARTESIAN_POINT('Ctrl Pts',(7.90941105408813,0.15864719582357,117.654223706849));
#231500=CARTESIAN_POINT('Ctrl Pts',(7.90961887598819,0.147908263766134,
117.653789787719));
#231501=CARTESIAN_POINT('Ctrl Pts',(7.90971365389144,0.142749890159383,
117.653581141884));
#231502=CARTESIAN_POINT('Ctrl Pts',(7.90991898797164,0.130945723813463,
117.653103199151));
#231503=CARTESIAN_POINT('Ctrl Pts',(7.91002621472679,0.124299882584173,
117.652833759609));
#231504=CARTESIAN_POINT('Ctrl Pts',(7.91028800089844,0.106699438788301,
117.6521192689));
#231505=CARTESIAN_POINT('Ctrl Pts',(7.91042817966825,0.0957446605316113,
117.65167361203));
#231506=CARTESIAN_POINT('Ctrl Pts',(7.91119881181689,0.0238476818519216,
117.648742671783));
#231507=CARTESIAN_POINT('Ctrl Pts',(7.91114775289066,-0.0370987612768795,
117.64622956681));
#231508=CARTESIAN_POINT('Ctrl Pts',(7.90253949227138,-0.731677882831249,
117.617307792944));
#231509=CARTESIAN_POINT('Ctrl Pts',(7.81858423180687,-1.36207962219676,
117.588648613337));
#231510=CARTESIAN_POINT('Ctrl Pts',(7.56087480386716,-2.36127938693626,
117.543835652452));
#231511=CARTESIAN_POINT('Ctrl Pts',(7.43246074688659,-2.73880128897324,
117.526996031401));
#231512=CARTESIAN_POINT('Ctrl Pts',(7.24899631664689,-3.16871611595521,
117.507924261073));
#231513=CARTESIAN_POINT('Ctrl Pts',(7.22100175680082,-3.23200297625685,
117.50511813878));
#231514=CARTESIAN_POINT('Ctrl Pts',(7.18350805555592,-3.3138446784607,117.501488821225));
#231515=CARTESIAN_POINT('Ctrl Pts',(7.17476119706971,-3.33274005993869,
117.500650857603));
#231516=CARTESIAN_POINT('Ctrl Pts',(7.15998080358407,-3.36434150006342,
117.49924925356));
#231517=CARTESIAN_POINT('Ctrl Pts',(7.15398781086243,-3.37706636598281,
117.49868483027));
#231518=CARTESIAN_POINT('Ctrl Pts',(7.14249132531801,-3.40130880809513,
117.497609415941));
#231519=CARTESIAN_POINT('Ctrl Pts',(7.13699383239629,-3.41282917499417,
117.497098312037));
#231520=CARTESIAN_POINT('Ctrl Pts',(7.12436207501018,-3.43913587332755,
117.495931058534));
#231521=CARTESIAN_POINT('Ctrl Pts',(7.11720961159171,-3.45391341495088,
117.495275255922));
#231522=CARTESIAN_POINT('Ctrl Pts',(7.09843807119191,-3.49239096266952,
117.493567317545));
#231523=CARTESIAN_POINT('Ctrl Pts',(7.08674627335765,-3.51605531130416,
117.492516540184));
#231524=CARTESIAN_POINT('Ctrl Pts',(7.01899887444197,-3.65146617617828,
117.48650091363));
#231525=CARTESIAN_POINT('Ctrl Pts',(6.96041832273227,-3.76193143988808,
117.48158249291));
#231526=CARTESIAN_POINT('Ctrl Pts',(6.50594743903832,-4.57193782554782,
117.445400334699));
#231527=CARTESIAN_POINT('Ctrl Pts',(6.00815002531249,-5.20884137922286,
117.416855312353));
#231528=CARTESIAN_POINT('Ctrl Pts',(5.25144028937711,-5.92130102609426,
117.377900198792));
#231529=CARTESIAN_POINT('Ctrl Pts',(5.07277967403856,-6.07505782159162,
117.368908928476));
#231530=CARTESIAN_POINT('Ctrl Pts',(4.869018078646,-6.23515344034737,117.358619864292));
#231531=CARTESIAN_POINT('Ctrl Pts',(4.85043754468806,-6.24961847523805,
117.357681303783));
#231532=CARTESIAN_POINT('Ctrl Pts',(4.81797107495771,-6.27466177812577,
117.356040334179));
#231533=CARTESIAN_POINT('Ctrl Pts',(4.80411414303069,-6.28527748025144,
117.355339645518));
#231534=CARTESIAN_POINT('Ctrl Pts',(4.78394628551389,-6.30062228091296,
117.354319244729));
#231535=CARTESIAN_POINT('Ctrl Pts',(4.77766319066552,-6.30538798373337,
117.354001265694));
#231536=CARTESIAN_POINT('Ctrl Pts',(4.76662596985367,-6.31373370374274,
117.353442524444));
#231537=CARTESIAN_POINT('Ctrl Pts',(4.76187490398588,-6.31731777076396,
117.353201956901));
#231538=CARTESIAN_POINT('Ctrl Pts',(4.75271520623512,-6.32421137831187,
117.352738051876));
#231539=CARTESIAN_POINT('Ctrl Pts',(4.74830714863814,-6.32752168002281,
117.352514751499));
#231540=CARTESIAN_POINT('Ctrl Pts',(4.73788966803902,-6.33532783835822,
117.351986908061));
#231541=CARTESIAN_POINT('Ctrl Pts',(4.73187730740598,-6.33981975083672,
117.351682172163));
#231542=CARTESIAN_POINT('Ctrl Pts',(4.71404106577142,-6.35310593126007,
117.350777837566));
#231543=CARTESIAN_POINT('Ctrl Pts',(4.70219903592498,-6.36187569558878,
117.350177023742));
#231544=CARTESIAN_POINT('Ctrl Pts',(4.58750552195451,-6.44631824317775,
117.344353539543));
#231545=CARTESIAN_POINT('Ctrl Pts',(4.4828751043067,-6.51951333781007,117.338997906481));
#231546=CARTESIAN_POINT('Ctrl Pts',(3.77788377971231,-6.98769751229932,
117.302592190623));
#231547=CARTESIAN_POINT('Ctrl Pts',(3.12788074321745,-7.30183359653573,
117.268182605252));
#231548=CARTESIAN_POINT('Ctrl Pts',(2.06047679600729,-7.6486135496008,117.217945719112));
#231549=CARTESIAN_POINT('Ctrl Pts',(1.6675675797021,-7.74378044474482,117.200585561463));
#231550=CARTESIAN_POINT('Ctrl Pts',(1.24807344246182,-7.81195789220473,
117.183383375346));
#231551=CARTESIAN_POINT('Ctrl Pts',(1.2270647875249,-7.81528537189074,117.182525210302));
#231552=CARTESIAN_POINT('Ctrl Pts',(1.1967009664676,-7.81996912681385,117.181289691594));
#231553=CARTESIAN_POINT('Ctrl Pts',(1.18735647995318,-7.82139341407987,
117.180910113993));
#231554=CARTESIAN_POINT('Ctrl Pts',(1.17107986425141,-7.82384445522013,
117.180250085218));
#231555=CARTESIAN_POINT('Ctrl Pts',(1.16414889214334,-7.82487875082973,
117.179969387414));
#231556=CARTESIAN_POINT('Ctrl Pts',(1.15078112595938,-7.82685544265866,
117.179428694516));
#231557=CARTESIAN_POINT('Ctrl Pts',(1.14434452809189,-7.82779911095196,
117.17916865798));
#231558=CARTESIAN_POINT('Ctrl Pts',(1.12912078655872,-7.83001188208366,
117.178554349693));
#231559=CARTESIAN_POINT('Ctrl Pts',(1.12033264672264,-7.83127413551633,
117.178200302552));
#231560=CARTESIAN_POINT('Ctrl Pts',(1.08965398358835,-7.83562785913713,
117.17696634175));
#231561=CARTESIAN_POINT('Ctrl Pts',(1.06775254546759,-7.83864237371611,
117.176088951324));
#231562=CARTESIAN_POINT('Ctrl Pts',(0.805858833662692,-7.87357144223106,
117.165639040871));
#231563=CARTESIAN_POINT('Ctrl Pts',(0.564526587492866,-7.89454608600728,
117.156434420372));
#231564=CARTESIAN_POINT('Ctrl Pts',(0.145341007530778,-7.9116540109927,
117.141033286342));
#231565=CARTESIAN_POINT('Ctrl Pts',(-0.0321131525079635,-7.91292396362523,
117.134693378899));
#231566=CARTESIAN_POINT('Ctrl Pts',(-0.643731356682046,-7.89672401144403,
117.113266199803));
#231567=CARTESIAN_POINT('Ctrl Pts',(-1.07631913203097,-7.84947012280132,
117.098889930226));
#231568=CARTESIAN_POINT('Ctrl Pts',(-1.79285545265694,-7.71082703231405,
117.074231231002));
#231569=CARTESIAN_POINT('Ctrl Pts',(-2.07949576055718,-7.6385119413124,
117.064115062868));
#231570=CARTESIAN_POINT('Ctrl Pts',(-2.50146469555151,-7.50653921648612,
117.048041704247));
#231571=CARTESIAN_POINT('Ctrl Pts',(-2.64027226680974,-7.45884809696728,
117.042554986074));
#231572=CARTESIAN_POINT('Ctrl Pts',(-2.83502650192841,-7.38581739387184,
117.034471799829));
#231573=CARTESIAN_POINT('Ctrl Pts',(-2.89213340522334,-7.3636429723869,
117.032053752685));
#231574=CARTESIAN_POINT('Ctrl Pts',(-2.95735547313544,-7.3374417313818,
117.02923101093));
#231575=CARTESIAN_POINT('Ctrl Pts',(-2.96572959458317,-7.33406098463771,
117.028867425563));
#231576=CARTESIAN_POINT('Ctrl Pts',(-2.97837683812393,-7.32892991734553,
117.028316528112));
#231577=CARTESIAN_POINT('Ctrl Pts',(-2.98265427175697,-7.32719017210704,
117.028129900035));
#231578=CARTESIAN_POINT('Ctrl Pts',(-2.99003802969178,-7.32417946568983,
117.027807203405));
#231579=CARTESIAN_POINT('Ctrl Pts',(-2.99314507737281,-7.32291026917352,
117.027671249974));
#231580=CARTESIAN_POINT('Ctrl Pts',(-2.99956967780685,-7.32028111507021,
117.027389790423));
#231581=CARTESIAN_POINT('Ctrl Pts',(-3.00288711481493,-7.3189208788771,
117.027244266028));
#231582=CARTESIAN_POINT('Ctrl Pts',(-3.01192748369076,-7.31520690924474,
117.026847179475));
#231583=CARTESIAN_POINT('Ctrl Pts',(-3.01764854630388,-7.31284872961152,
117.026595322878));
#231584=CARTESIAN_POINT('Ctrl Pts',(-3.03959018839673,-7.30377441472172,
117.025627235336));
#231585=CARTESIAN_POINT('Ctrl Pts',(-3.05579105679746,-7.29701104711736,
117.024907910446));
#231586=CARTESIAN_POINT('Ctrl Pts',(-3.32972063923137,-7.18158157554029,
117.012670490454));
#231587=CARTESIAN_POINT('Ctrl Pts',(-3.58150902964062,-7.05938510572658,
117.000303881305));
#231588=CARTESIAN_POINT('Ctrl Pts',(-4.39139741732715,-6.61184077083736,
116.958142560529));
#231589=CARTESIAN_POINT('Ctrl Pts',(-4.91618635689275,-6.23153857999667,
116.927118721136));
#231590=CARTESIAN_POINT('Ctrl Pts',(-5.64869545453544,-5.54995726483783,
116.882521687796));
#231591=CARTESIAN_POINT('Ctrl Pts',(-5.89189262578322,-5.29107112524182,
116.867376604445));
#231592=CARTESIAN_POINT('Ctrl Pts',(-6.12934645588315,-5.00154151460192,
116.852257870871));
#231593=CARTESIAN_POINT('Ctrl Pts',(-6.1417247765091,-4.98633355040616,
116.851468613838));
#231594=CARTESIAN_POINT('Ctrl Pts',(-6.15964961833961,-4.96414313748657,
116.850324022488));
#231595=CARTESIAN_POINT('Ctrl Pts',(-6.16524102892711,-4.95719714820035,
116.849966742657));
#231596=CARTESIAN_POINT('Ctrl Pts',(-6.17500898340934,-4.94502071333443,
116.849342164551));
#231597=CARTESIAN_POINT('Ctrl Pts',(-6.17919064944181,-4.93979440044247,
116.849074645101));
#231598=CARTESIAN_POINT('Ctrl Pts',(-6.18727890687082,-4.92965922622586,
116.848556935472));
#231599=CARTESIAN_POINT('Ctrl Pts',(-6.19118630045289,-4.92475101415718,
116.848306710809));
#231600=CARTESIAN_POINT('Ctrl Pts',(-6.20047101662896,-4.91305964735328,
116.847711836219));
#231601=CARTESIAN_POINT('Ctrl Pts',(-6.20584305880946,-4.90627229743856,
116.847367413248));
#231602=CARTESIAN_POINT('Ctrl Pts',(-6.22485761261875,-4.88216701172168,
116.846147471742));
#231603=CARTESIAN_POINT('Ctrl Pts',(-6.23843892300201,-4.86480080193035,
116.845274573557));
#231604=CARTESIAN_POINT('Ctrl Pts',(-6.41907148236379,-4.63182839979569,
116.833643578032));
#231605=CARTESIAN_POINT('Ctrl Pts',(-6.57494330844314,-4.40777163193627,
116.82337100424));
#231606=CARTESIAN_POINT('Ctrl Pts',(-7.03711628433842,-3.66417917277177,
116.791608251754));
#231607=CARTESIAN_POINT('Ctrl Pts',(-7.29572840442103,-3.11761675966364,
116.771846710286));
#231608=CARTESIAN_POINT('Ctrl Pts',(-7.54888038781228,-2.37318918425704,
116.744651907063));
#231609=CARTESIAN_POINT('Ctrl Pts',(-7.60191489861735,-2.19738645611294,
116.738193583418));
#231610=CARTESIAN_POINT('Ctrl Pts',(-7.69456579927984,-1.84654485218379,
116.724958823021));
#231611=CARTESIAN_POINT('Ctrl Pts',(-7.73443734509595,-1.67168832178477,
116.718196782917));
#231612=CARTESIAN_POINT('Ctrl Pts',(-7.7732525378035,-1.47008277402918,
116.710052860398));
#231613=CARTESIAN_POINT('Ctrl Pts',(-7.77804688671567,-1.44450164271278,
116.709013138756));
#231614=CARTESIAN_POINT('Ctrl Pts',(-7.78399089626607,-1.41189848776171,
116.707679380905));
#231615=CARTESIAN_POINT('Ctrl Pts',(-7.785257449136,-1.4048978834481,116.707392491511));
#231616=CARTESIAN_POINT('Ctrl Pts',(-7.78728089775761,-1.3936269329508,
116.706929802121));
#231617=CARTESIAN_POINT('Ctrl Pts',(-7.78804373070418,-1.38935764197675,
116.706754357048));
#231618=CARTESIAN_POINT('Ctrl Pts',(-7.78948829260269,-1.38123439617448,
116.706420187271));
#231619=CARTESIAN_POINT('Ctrl Pts',(-7.79017067329978,-1.37738055689878,
116.706261501239));
#231620=CARTESIAN_POINT('Ctrl Pts',(-7.79171732410764,-1.3686077176383,
116.705899933774));
#231621=CARTESIAN_POINT('Ctrl Pts',(-7.7925797957553,-1.36368840655859,
116.705696946694));
#231622=CARTESIAN_POINT('Ctrl Pts',(-7.79479823308611,-1.3509641966725,
116.705171287491));
#231623=CARTESIAN_POINT('Ctrl Pts',(-7.79614713170791,-1.34315809012247,
116.704848204382));
#231624=CARTESIAN_POINT('Ctrl Pts',(-7.80414132568621,-1.29647774260131,
116.702912646225));
#231625=CARTESIAN_POINT('Ctrl Pts',(-7.81050746845904,-1.25755689700789,
116.701284206284));
#231626=CARTESIAN_POINT('Ctrl Pts',(-7.83736072539268,-1.08530818055408,
116.694017681966));
#231627=CARTESIAN_POINT('Ctrl Pts',(-7.85472588874391,-0.951522278462937,
116.688216164074));
#231628=CARTESIAN_POINT('Ctrl Pts',(-7.89686769496231,-0.545828745646157,
116.670279010351));
#231629=CARTESIAN_POINT('Ctrl Pts',(-7.91099797524739,-0.273027730968651,
116.657756563083));
#231630=CARTESIAN_POINT('Ctrl Pts',(-7.91100408729714,0.551041996280015,
116.619499028887));
#231631=CARTESIAN_POINT('Ctrl Pts',(-7.85342008312486,1.10069144869308,
116.593514735652));
#231632=CARTESIAN_POINT('Ctrl Pts',(-7.66828776789497,1.97438093723589,
116.55388855431));
#231633=CARTESIAN_POINT('Ctrl Pts',(-7.57580094590423,2.30393055830503,
116.539315625526));
#231634=CARTESIAN_POINT('Ctrl Pts',(-7.45403472262007,2.64988726639005,
116.524436848088));
#231635=CARTESIAN_POINT('Ctrl Pts',(-7.44569009647523,2.67324431589141,
116.52343429898));
#231636=CARTESIAN_POINT('Ctrl Pts',(-7.43397644084802,2.70555109095403,
116.522050281538));
#231637=CARTESIAN_POINT('Ctrl Pts',(-7.430700866726,2.71453440922827,116.521665725253));
#231638=CARTESIAN_POINT('Ctrl Pts',(-7.42504364712464,2.72996246208796,
116.521005773071));
#231639=CARTESIAN_POINT('Ctrl Pts',(-7.42266988142133,2.73641006391288,
116.520730116758));
#231640=CARTESIAN_POINT('Ctrl Pts',(-7.41776515605248,2.7496788947595,116.520163130622));
#231641=CARTESIAN_POINT('Ctrl Pts',(-7.41523317934636,2.75649974259466,
116.519871834794));
#231642=CARTESIAN_POINT('Ctrl Pts',(-7.40933846995057,2.77231250037182,
116.519196900343));
#231643=CARTESIAN_POINT('Ctrl Pts',(-7.40596876883543,2.78130180992139,
116.518813492929));
#231644=CARTESIAN_POINT('Ctrl Pts',(-7.39526430162284,2.80970059510629,
116.517603124158));
#231645=CARTESIAN_POINT('Ctrl Pts',(-7.38786950617857,2.82908743113183,
116.516778152512));
#231646=CARTESIAN_POINT('Ctrl Pts',(-7.27096223413252,3.13199734876724,
116.503908168259));
#231647=CARTESIAN_POINT('Ctrl Pts',(-7.14527194433361,3.40901883395341,
116.492423735195));
#231648=CARTESIAN_POINT('Ctrl Pts',(-6.65157175957509,4.34912683230948,
116.453714151767));
#231649=CARTESIAN_POINT('Ctrl Pts',(-6.20465549154878,4.96592284120455,
116.429108283361));
#231650=CARTESIAN_POINT('Ctrl Pts',(-5.53303647572045,5.65792324817929,
116.393563996317));
#231651=CARTESIAN_POINT('Ctrl Pts',(-5.38345208318239,5.80043333589012,
116.385663185485));
#231652=CARTESIAN_POINT('Ctrl Pts',(-5.21366624438295,5.94995740033911,
116.376635657692));
#231653=CARTESIAN_POINT('Ctrl Pts',(-5.19883960965301,5.9629166922425,116.375847253632));
#231654=CARTESIAN_POINT('Ctrl Pts',(-5.17722312525201,5.98166877761607,
116.374697857564));
#231655=CARTESIAN_POINT('Ctrl Pts',(-5.17047155105633,5.98750570711496,
116.374338869533));
#231656=CARTESIAN_POINT('Ctrl Pts',(-5.15854834532258,5.99777845466058,
116.37370493254));
#231657=CARTESIAN_POINT('Ctrl Pts',(-5.15338082673286,6.0022190460331,116.373430194714));
#231658=CARTESIAN_POINT('Ctrl Pts',(-5.14269500475926,6.01137769565537,
116.372862100054));
#231659=CARTESIAN_POINT('Ctrl Pts',(-5.13717593098592,6.01609484346085,
116.37256870429));
#231660=CARTESIAN_POINT('Ctrl Pts',(-5.12304901319749,6.02813549426118,
116.37181776975));
#231661=CARTESIAN_POINT('Ctrl Pts',(-5.11443196842435,6.03544814970255,
116.371359773613));
#231662=CARTESIAN_POINT('Ctrl Pts',(-5.07932765454066,6.06510944796254,
116.369494278859));
#231663=CARTESIAN_POINT('Ctrl Pts',(-5.05270951696767,6.08730223801123,
116.368080446881));
#231664=CARTESIAN_POINT('Ctrl Pts',(-4.68633612855896,6.38870621274969,
116.348637543071));
#231665=CARTESIAN_POINT('Ctrl Pts',(-4.32402926779007,6.63928189438814,
116.329666587344));
#231666=CARTESIAN_POINT('Ctrl Pts',(-3.30519487839172,7.22499118250048,
116.279100202995));
#231667=CARTESIAN_POINT('Ctrl Pts',(-2.61955682074068,7.50085520269922,
116.248171834691));
#231668=CARTESIAN_POINT('Ctrl Pts',(-1.89627838422932,7.68037391716766,
116.217541625687));
#231669=CARTESIAN_POINT('Ctrl Pts',(-1.88685333038075,7.68269482198705,
116.217142757027));
#231670=CARTESIAN_POINT('Ctrl Pts',(-1.87487060133419,7.6856221698276,116.216635999221));
#231671=CARTESIAN_POINT('Ctrl Pts',(-1.87231686649916,7.68624469168908,
116.216528020317));
#231672=CARTESIAN_POINT('Ctrl Pts',(-1.84801861994013,7.69215502737025,
116.215500817408));
#231673=CARTESIAN_POINT('Ctrl Pts',(-1.82625205199896,7.69735183224469,
116.214582115104));
#231674=CARTESIAN_POINT('Ctrl Pts',(-1.62966687413072,7.74340607890182,
116.206298408681));
#231675=CARTESIAN_POINT('Ctrl Pts',(-1.45352483222994,7.77839436669596,
116.198974218713));
#231676=CARTESIAN_POINT('Ctrl Pts',(-1.23645257876753,7.81388122531212,
116.190075664475));
#231677=CARTESIAN_POINT('Ctrl Pts',(-1.19651251468582,7.82009671333895,
116.188443559855));
#231678=CARTESIAN_POINT('Ctrl Pts',(-1.13351802968146,7.82940603269124,
116.185877446158));
#231679=CARTESIAN_POINT('Ctrl Pts',(-1.11049468977524,7.83270473696248,
116.184941274263));
#231680=CARTESIAN_POINT('Ctrl Pts',(-1.06773950438045,7.83863825048239,
116.183205887279));
#231681=CARTESIAN_POINT('Ctrl Pts',(-1.04801162450513,7.84130020523693,
116.182406383934));
#231682=CARTESIAN_POINT('Ctrl Pts',(-1.00434710887154,7.84702429035397,
116.180639504024));
#231683=CARTESIAN_POINT('Ctrl Pts',(-0.980406068816571,7.8500514185209,
116.179672520702));
#231684=CARTESIAN_POINT('Ctrl Pts',(-0.911203864228038,7.85847989353954,
116.176882516298));
#231685=CARTESIAN_POINT('Ctrl Pts',(-0.865909271209853,7.86359967732496,
116.175062670449));
#231686=CARTESIAN_POINT('Ctrl Pts',(-0.51051986847832,7.90066255561776,
116.16083119563));
#231687=CARTESIAN_POINT('Ctrl Pts',(-0.198821857089528,7.9146432303336,
116.148644461999));
#231688=CARTESIAN_POINT('Ctrl Pts',(0.605481302614832,7.90316424123078,
116.117528490128));
#231689=CARTESIAN_POINT('Ctrl Pts',(1.0963210825232,7.8501381644512,116.098896770273));
#231690=CARTESIAN_POINT('Ctrl Pts',(1.67993384796268,7.73125791559428,116.075496097349));
#231691=CARTESIAN_POINT('Ctrl Pts',(1.78043303949063,7.70873428241009,116.071417821523));
#231692=CARTESIAN_POINT('Ctrl Pts',(1.90038524812652,7.67938002748687,116.066471526625));
#231693=CARTESIAN_POINT('Ctrl Pts',(1.92028907071842,7.67442711736106,116.065648149467));
#231694=CARTESIAN_POINT('Ctrl Pts',(1.95151933237095,7.66652660995701,116.064351957554));
#231695=CARTESIAN_POINT('Ctrl Pts',(1.96285874595188,7.66363122208441,116.063880448144));
#231696=CARTESIAN_POINT('Ctrl Pts',(1.98297704826265,7.65844666592033,116.063042373965));
#231697=CARTESIAN_POINT('Ctrl Pts',(1.99175851255851,7.65616753577282,116.06267604507));
#231698=CARTESIAN_POINT('Ctrl Pts',(2.01199766409598,7.65087751461665,116.061830569766));
#231699=CARTESIAN_POINT('Ctrl Pts',(2.02345253884151,7.64785598491124,116.061351181139));
#231700=CARTESIAN_POINT('Ctrl Pts',(2.05539752532561,7.63935284597185,116.060011892445));
#231701=CARTESIAN_POINT('Ctrl Pts',(2.07587239655663,7.63381455627029,116.059150745043));
#231702=CARTESIAN_POINT('Ctrl Pts',(2.19427285377355,7.6012766056243,116.054155593316));
#231703=CARTESIAN_POINT('Ctrl Pts',(2.29169226216281,7.57247551490085,116.049984701333));
#231704=CARTESIAN_POINT('Ctrl Pts',(3.07537074969939,7.32428054813343,116.016010232481));
#231705=CARTESIAN_POINT('Ctrl Pts',(3.72929909166269,7.01394285862001,115.985323118855));
#231706=CARTESIAN_POINT('Ctrl Pts',(4.4340344111253,6.5527153421695,115.950840748322));
#231707=CARTESIAN_POINT('Ctrl Pts',(4.53433946016617,6.48371080111128,115.94588661242));
#231708=CARTESIAN_POINT('Ctrl Pts',(4.66554275193139,6.38891558801009,115.939337404855));
#231709=CARTESIAN_POINT('Ctrl Pts',(4.69789316259605,6.36516546634541,115.937716828595));
#231710=CARTESIAN_POINT('Ctrl Pts',(4.74901718379636,6.32703058558189,115.935146199785));
#231711=CARTESIAN_POINT('Ctrl Pts',(4.76790935285062,6.31280608366394,115.934194150021));
#231712=CARTESIAN_POINT('Ctrl Pts',(4.8040634292249,6.28532967600904,115.932368031252));
#231713=CARTESIAN_POINT('Ctrl Pts',(4.82133499118411,6.27209083751342,115.931493808739));
#231714=CARTESIAN_POINT('Ctrl Pts',(4.8619262619239,6.24071045094472,115.929434747549));
#231715=CARTESIAN_POINT('Ctrl Pts',(4.88519942403692,6.22250918069546,115.928250662501));
#231716=CARTESIAN_POINT('Ctrl Pts',(4.95335885297179,6.16858556519661,115.924772106377));
#231717=CARTESIAN_POINT('Ctrl Pts',(4.99795928003246,6.1325047809436,115.922482054546));
#231718=CARTESIAN_POINT('Ctrl Pts',(5.29105529554038,5.89007497406277,115.9073332087));
#231719=CARTESIAN_POINT('Ctrl Pts',(5.52711392368034,5.66915070942462,115.894610970461));
#231720=CARTESIAN_POINT('Ctrl Pts',(6.04561773586974,5.1206313754462,115.865284889384));
#231721=CARTESIAN_POINT('Ctrl Pts',(6.31604723636686,4.78308756775227,115.848975329558));
#231722=CARTESIAN_POINT('Ctrl Pts',(6.80110145347412,4.0642909548411,115.816679950595));
#231723=CARTESIAN_POINT('Ctrl Pts',(7.01440397740474,3.68395865398956,115.800747199353));
#231724=CARTESIAN_POINT('Ctrl Pts',(7.24604930290235,3.17703979059333,115.779398427923));
#231725=CARTESIAN_POINT('Ctrl Pts',(7.29419230869431,3.06489305539442,115.774664457431));
#231726=CARTESIAN_POINT('Ctrl Pts',(7.35465435202675,2.91454667321587,115.76825671222));
#231727=CARTESIAN_POINT('Ctrl Pts',(7.36930569792999,2.87730019509821,115.766664326652));
#231728=CARTESIAN_POINT('Ctrl Pts',(7.38786235728985,2.82905407115898,115.764593601695));
#231729=CARTESIAN_POINT('Ctrl Pts',(7.39202698827084,2.81815438731001,115.764125256874));
#231730=CARTESIAN_POINT('Ctrl Pts',(7.39860856941201,2.80081408869812,115.763379272603));
#231731=CARTESIAN_POINT('Ctrl Pts',(7.40104126787672,2.79437944339012,115.763102256927));
#231732=CARTESIAN_POINT('Ctrl Pts',(7.40538965800088,2.78283215846149,115.762604775946));
#231733=CARTESIAN_POINT('Ctrl Pts',(7.40730845767646,2.77772068819915,115.762384435846));
#231734=CARTESIAN_POINT('Ctrl Pts',(7.41177149021943,2.76579415269531,115.761870013816));
#231735=CARTESIAN_POINT('Ctrl Pts',(7.41431161497342,2.75897756314154,115.76157576481));
#231736=CARTESIAN_POINT('Ctrl Pts',(7.42152727769009,2.73953193447622,115.76073567853));
#231737=CARTESIAN_POINT('Ctrl Pts',(7.42617996176327,2.72689448384872,115.760188895453));
#231738=CARTESIAN_POINT('Ctrl Pts',(7.45540179618182,2.64689374860291,115.756721986674));
#231739=CARTESIAN_POINT('Ctrl Pts',(7.47908620445817,2.57921149367012,115.753763979841));
#231740=CARTESIAN_POINT('Ctrl Pts',(7.54245218844816,2.38991601454081,115.745401233506));
#231741=CARTESIAN_POINT('Ctrl Pts',(7.5801074716033,2.26765333164216,115.739902186985));
#231742=CARTESIAN_POINT('Ctrl Pts',(7.73439086533888,1.71982677533538,115.714975137089));
#231743=CARTESIAN_POINT('Ctrl Pts',(7.81825523334347,1.28587061474553,115.694500122485));
#231744=CARTESIAN_POINT('Ctrl Pts',(7.93617808370223,0.191071703140395,
115.643818837889));
#231745=CARTESIAN_POINT('Ctrl Pts',(7.92448362114155,-0.471424432176066,
115.614208221002));
#231746=CARTESIAN_POINT('Ctrl Pts',(7.82468018388264,-1.16621094109064,
115.585532600301));
#231747=CARTESIAN_POINT('Ctrl Pts',(7.81840945810377,-1.20753532105886,
115.583834959094));
#231748=CARTESIAN_POINT('Ctrl Pts',(7.80968069518058,-1.26213732931399,
115.581602119156));
#231749=CARTESIAN_POINT('Ctrl Pts',(7.80751580608146,-1.27546075547408,
115.581058093484));
#231750=CARTESIAN_POINT('Ctrl Pts',(7.80410213840577,-1.2961351811532,115.580215155254));
#231751=CARTESIAN_POINT('Ctrl Pts',(7.80287705393131,-1.30349003682376,
115.579915527765));
#231752=CARTESIAN_POINT('Ctrl Pts',(7.80040367636901,-1.3182106424387,115.579316316699));
#231753=CARTESIAN_POINT('Ctrl Pts',(7.79915534389789,-1.32557637813875,
115.579016734656));
#231754=CARTESIAN_POINT('Ctrl Pts',(7.79637675627202,-1.34183152337952,
115.578356136219));
#231755=CARTESIAN_POINT('Ctrl Pts',(7.79484172660835,-1.35072011188928,
115.577995264611));
#231756=CARTESIAN_POINT('Ctrl Pts',(7.79036153311696,-1.37640067812506,
115.576953666647));
#231757=CARTESIAN_POINT('Ctrl Pts',(7.78737727918901,-1.39318583090562,
115.576274123805));
#231758=CARTESIAN_POINT('Ctrl Pts',(7.7805302828666,-1.43098781887351,115.574746517097));
#231759=CARTESIAN_POINT('Ctrl Pts',(7.77663659196238,-1.45199894821325,
115.573899393291));
#231760=CARTESIAN_POINT('Ctrl Pts',(7.69822988312715,-1.8657334624993,115.557256207842));
#231761=CARTESIAN_POINT('Ctrl Pts',(7.59414053067719,-2.25228252782829,
115.542415552671));
#231762=CARTESIAN_POINT('Ctrl Pts',(7.31079790781519,-3.05632339119236,
115.511997211471));
#231763=CARTESIAN_POINT('Ctrl Pts',(7.12395142877413,-3.46961022634724,
115.496641631285));
#231764=CARTESIAN_POINT('Ctrl Pts',(6.69339881047408,-4.23863840243437,
115.465933509126));
#231765=CARTESIAN_POINT('Ctrl Pts',(6.45397361302279,-4.5949765053536,115.450649427798));
#231766=CARTESIAN_POINT('Ctrl Pts',(6.17009874320876,-4.95121489076884,
115.432577596861));
#231767=CARTESIAN_POINT('Ctrl Pts',(6.15319497420201,-4.97220665071132,
115.431501705299));
#231768=CARTESIAN_POINT('Ctrl Pts',(6.13049376049492,-5.00010485333914,
115.430057593258));
#231769=CARTESIAN_POINT('Ctrl Pts',(6.12479115658163,-5.00708853318127,
115.429694893127));
#231770=CARTESIAN_POINT('Ctrl Pts',(6.11587393287609,-5.01797096157041,
115.429127856254));
#231771=CARTESIAN_POINT('Ctrl Pts',(6.11266748315087,-5.0218764196521,115.428923985847));
#231772=CARTESIAN_POINT('Ctrl Pts',(6.10624008707155,-5.02968971655229,
115.428515376684));
#231773=CARTESIAN_POINT('Ctrl Pts',(6.10301912585457,-5.03359754003327,
115.4283106371));
#231774=CARTESIAN_POINT('Ctrl Pts',(6.09575118258457,-5.04239812363682,
115.427848717581));
#231775=CARTESIAN_POINT('Ctrl Pts',(6.09170206060011,-5.04728910622151,
115.427591418237));
#231776=CARTESIAN_POINT('Ctrl Pts',(6.0797430800045,-5.06169914748906,115.426831638858));
#231777=CARTESIAN_POINT('Ctrl Pts',(6.07181678906869,-5.0712044975632,115.426328254952));
#231778=CARTESIAN_POINT('Ctrl Pts',(6.01035696262352,-5.14455756669678,
115.422426782989));
#231779=CARTESIAN_POINT('Ctrl Pts',(5.95584122856075,-5.20757313703596,
115.418976270473));
#231780=CARTESIAN_POINT('Ctrl Pts',(5.75987758249643,-5.42698777974775,
115.406643068526));
#231781=CARTESIAN_POINT('Ctrl Pts',(5.61318586084218,-5.57857727366622,
115.397538209988));
#231782=CARTESIAN_POINT('Ctrl Pts',(5.02384194107628,-6.14079180232958,
115.361963182065));
#231783=CARTESIAN_POINT('Ctrl Pts',(4.54075735063141,-6.50614616445817,
115.335064517024));
#231784=CARTESIAN_POINT('Ctrl Pts',(3.81219784840903,-6.93611923707059,
115.299364313218));
#231785=CARTESIAN_POINT('Ctrl Pts',(3.59802625861965,-7.04959700554827,
115.289356587062));
#231786=CARTESIAN_POINT('Ctrl Pts',(3.34874178334811,-7.16735429477087,
115.278200890594));
#231787=CARTESIAN_POINT('Ctrl Pts',(3.3184167396995,-7.18144480453668,115.276851763404));
#231788=CARTESIAN_POINT('Ctrl Pts',(3.27313711282507,-7.20213590449756,
115.274848782527));
#231789=CARTESIAN_POINT('Ctrl Pts',(3.25825004737886,-7.20888304644383,
115.274192074306));
#231790=CARTESIAN_POINT('Ctrl Pts',(3.23187625813565,-7.22073783491047,
115.273031843864));
#231791=CARTESIAN_POINT('Ctrl Pts',(3.22039808343036,-7.22586432295078,
115.272527962703));
#231792=CARTESIAN_POINT('Ctrl Pts',(3.19631413314722,-7.23655213441936,
115.271472899743));
#231793=CARTESIAN_POINT('Ctrl Pts',(3.18370594656166,-7.24210793064462,
115.270921823337));
#231794=CARTESIAN_POINT('Ctrl Pts',(3.15124059877901,-7.25631261698167,
115.269506021122));
#231795=CARTESIAN_POINT('Ctrl Pts',(3.13136228680717,-7.26491296166915,
115.268642194305));
#231796=CARTESIAN_POINT('Ctrl Pts',(3.05112354510443,-7.299237714403,115.265167355863));
#231797=CARTESIAN_POINT('Ctrl Pts',(2.99047875962188,-7.32429266539306,
115.26256811104));
#231798=CARTESIAN_POINT('Ctrl Pts',(2.61111738579847,-7.47552576778342,
115.246472167339));
#231799=CARTESIAN_POINT('Ctrl Pts',(2.28478438932175,-7.5816354859581,115.233361119966));
#231800=CARTESIAN_POINT('Ctrl Pts',(1.25156839153174,-7.84479454699652,
115.193426027796));
#231801=CARTESIAN_POINT('Ctrl Pts',(0.529441153454571,-7.92633254788837,
115.16797477931));
#231802=CARTESIAN_POINT('Ctrl Pts',(-0.268644741614546,-7.90679345215649,
115.136730508297));
#231803=CARTESIAN_POINT('Ctrl Pts',(-0.343635540229735,-7.90388935155108,
115.133761118866));
#231804=CARTESIAN_POINT('Ctrl Pts',(-0.431377775716765,-7.89924038487294,
115.130238355869));
#231805=CARTESIAN_POINT('Ctrl Pts',(-0.444181646725833,-7.89853075614155,
115.129723083334));
#231806=CARTESIAN_POINT('Ctrl Pts',(-0.464659020671794,-7.89734588975695,
115.128897003468));
#231807=CARTESIAN_POINT('Ctrl Pts',(-0.472333683808938,-7.89689059051496,
115.128586949863));
#231808=CARTESIAN_POINT('Ctrl Pts',(-0.485910869848464,-7.89606526083035,
115.128037626513));
#231809=CARTESIAN_POINT('Ctrl Pts',(-0.491813671303911,-7.89569979730756,
115.127798532412));
#231810=CARTESIAN_POINT('Ctrl Pts',(-0.504049436572287,-7.89492846305252,
115.127302350654));
#231811=CARTESIAN_POINT('Ctrl Pts',(-0.510382331353193,-7.89452159074639,
115.127045224189));
#231812=CARTESIAN_POINT('Ctrl Pts',(-0.526660673205268,-7.89345607963703,
115.126383469426));
#231813=CARTESIAN_POINT('Ctrl Pts',(-0.53660535924529,-7.89278626551327,
115.125978400691));
#231814=CARTESIAN_POINT('Ctrl Pts',(-0.577681147846379,-7.88994165806629,
115.124301941963));
#231815=CARTESIAN_POINT('Ctrl Pts',(-0.608800231849868,-7.8876014804734,
115.123023898075));
#231816=CARTESIAN_POINT('Ctrl Pts',(-0.806611886662481,-7.87154830411064,
115.114845593408));
#231817=CARTESIAN_POINT('Ctrl Pts',(-0.972822283090363,-7.85273838432535,
115.10770321241));
#231818=CARTESIAN_POINT('Ctrl Pts',(-1.53342911841054,-7.77122529965061,
115.082855369394));
#231819=CARTESIAN_POINT('Ctrl Pts',(-1.9236259172581,-7.68394359205734,
115.064367310476));
#231820=CARTESIAN_POINT('Ctrl Pts',(-2.48644572906544,-7.51247424939248,
115.037296477165));
#231821=CARTESIAN_POINT('Ctrl Pts',(-2.66531074734442,-7.45089276487872,
115.028625332138));
#231822=CARTESIAN_POINT('Ctrl Pts',(-3.10707470391562,-7.28085190283259,
115.007202796167));
#231823=CARTESIAN_POINT('Ctrl Pts',(-3.36666689719746,-7.16451609057546,
114.994615008494));
#231824=CARTESIAN_POINT('Ctrl Pts',(-3.78775697637102,-6.9478518277163,
114.974392549006));
#231825=CARTESIAN_POINT('Ctrl Pts',(-3.95290901590641,-6.85523631441762,
114.966512262409));
#231826=CARTESIAN_POINT('Ctrl Pts',(-4.13260102551079,-6.74581163034636,
114.957997317052));
#231827=CARTESIAN_POINT('Ctrl Pts',(-4.1505701404222,-6.73477047172949,
114.957146473416));
#231828=CARTESIAN_POINT('Ctrl Pts',(-4.17570032534715,-6.71919040250287,
114.955957432969));
#231829=CARTESIAN_POINT('Ctrl Pts',(-4.18289849710914,-6.71471168671104,
114.955616951716));
#231830=CARTESIAN_POINT('Ctrl Pts',(-4.19606622369326,-6.7064893123318,
114.954994288249));
#231831=CARTESIAN_POINT('Ctrl Pts',(-4.20203799873123,-6.70274923502462,
114.954711969922));
#231832=CARTESIAN_POINT('Ctrl Pts',(-4.21348485984275,-6.69555884275751,
114.954170946286));
#231833=CARTESIAN_POINT('Ctrl Pts',(-4.21896072303947,-6.69210977933483,
114.953912193484));
#231834=CARTESIAN_POINT('Ctrl Pts',(-4.23266503850478,-6.68345438264078,
114.953264762467));
#231835=CARTESIAN_POINT('Ctrl Pts',(-4.24088813305018,-6.67823956270512,
114.952876409895));
#231836=CARTESIAN_POINT('Ctrl Pts',(-4.26845541248025,-6.66068583825584,
114.951574916135));
#231837=CARTESIAN_POINT('Ctrl Pts',(-4.28775562699343,-6.64827790779195,
114.950664432149));
#231838=CARTESIAN_POINT('Ctrl Pts',(-4.33333962483289,-6.61869130680911,
114.948515608679));
#231839=CARTESIAN_POINT('Ctrl Pts',(-4.35957573720787,-6.60143971724083,
114.947280105852));
#231840=CARTESIAN_POINT('Ctrl Pts',(-4.4514990035468,-6.54020844609792,
114.942955340218));
#231841=CARTESIAN_POINT('Ctrl Pts',(-4.51662993087941,-6.49540025134938,
114.939898483332));
#231842=CARTESIAN_POINT('Ctrl Pts',(-4.75263610153431,-6.32776826274899,
114.928840264551));
#231843=CARTESIAN_POINT('Ctrl Pts',(-4.91926806430558,-6.19911366247368,
114.9210716483));
#231844=CARTESIAN_POINT('Ctrl Pts',(-5.62990843038554,-5.60371659717378,
114.887794713049));
#231845=CARTESIAN_POINT('Ctrl Pts',(-6.11409611074967,-5.07101836013405,
114.865051970489));
#231846=CARTESIAN_POINT('Ctrl Pts',(-6.56508929603143,-4.41473451404926,
114.837176956544));
#231847=CARTESIAN_POINT('Ctrl Pts',(-6.60924966540691,-4.34834413795392,
114.834354473511));
#231848=CARTESIAN_POINT('Ctrl Pts',(-6.66676497367065,-4.25897529064251,
114.830537115142));
#231849=CARTESIAN_POINT('Ctrl Pts',(-6.68101918163342,-4.23657980178738,
114.829579016298));
#231850=CARTESIAN_POINT('Ctrl Pts',(-6.80519630601589,-4.03929374743746,
114.821122362088));
#231851=CARTESIAN_POINT('Ctrl Pts',(-6.90833533183499,-3.86024372311409,
114.813333872112));
#231852=CARTESIAN_POINT('Ctrl Pts',(-7.01059455247853,-3.66546939655364,
114.804533461345));
#231853=CARTESIAN_POINT('Ctrl Pts',(-7.01681583177302,-3.65354587420396,
114.803993446183));
#231854=CARTESIAN_POINT('Ctrl Pts',(-7.02532525838795,-3.63713505176211,
114.803248370268));
#231855=CARTESIAN_POINT('Ctrl Pts',(-7.02763960207304,-3.63266128259242,
114.803045067803));
#231856=CARTESIAN_POINT('Ctrl Pts',(-7.03158701590246,-3.62501279771316,
114.802697172362));
#231857=CARTESIAN_POINT('Ctrl Pts',(-7.03322221503302,-3.62183917639508,
114.802552723377));
#231858=CARTESIAN_POINT('Ctrl Pts',(-7.03639337664261,-3.61567428787935,
114.802271938727));
#231859=CARTESIAN_POINT('Ctrl Pts',(-7.03792958139306,-3.612683146107,114.80213561962));
#231860=CARTESIAN_POINT('Ctrl Pts',(-7.04159169017628,-3.60554145938853,
114.801809937061));
#231861=CARTESIAN_POINT('Ctrl Pts',(-7.04371581839078,-3.60139003944941,
114.801620453943));
#231862=CARTESIAN_POINT('Ctrl Pts',(-7.05013163271111,-3.58882351104592,
114.801046375671));
#231863=CARTESIAN_POINT('Ctrl Pts',(-7.05441188517672,-3.58040265678223,
114.800661003337));
#231864=CARTESIAN_POINT('Ctrl Pts',(-7.09488796807132,-3.50041674956804,
114.796994230623));
#231865=CARTESIAN_POINT('Ctrl Pts',(-7.13000746507062,-3.42831523567537,
114.793641160497));
#231866=CARTESIAN_POINT('Ctrl Pts',(-7.2732033674255,-3.12260841572409,
114.779269377551));
#231867=CARTESIAN_POINT('Ctrl Pts',(-7.37093551387112,-2.88434765136892,
114.767696025035));
#231868=CARTESIAN_POINT('Ctrl Pts',(-7.75725811981538,-1.79388099260181,
114.714525136329));
#231869=CARTESIAN_POINT('Ctrl Pts',(-7.91091024119016,-0.900670596073987,
114.671494346077));
#231870=CARTESIAN_POINT('Ctrl Pts',(-7.91099996068087,-0.00078873785590905,
114.634517834504));
#231871=CARTESIAN_POINT('',(-7.9109991388093,-0.00369130851947151,110.642331508237));
#231872=CARTESIAN_POINT('Ctrl Pts',(-7.91099996199236,-0.000775472076273572,
114.634517289408));
#231873=CARTESIAN_POINT('Ctrl Pts',(-7.91100579301261,0.0587098433008668,
114.632073016955));
#231874=CARTESIAN_POINT('Ctrl Pts',(-7.91034069134381,0.118194551747119,
114.629651328104));
#231875=CARTESIAN_POINT('Ctrl Pts',(-7.90873371509585,0.189730367056336,
114.626765571885));
#231876=CARTESIAN_POINT('Ctrl Pts',(-7.90843513499218,0.201792730061897,
114.626279883153));
#231877=CARTESIAN_POINT('Ctrl Pts',(-7.90789406828848,0.221800803016074,
114.625475757813));
#231878=CARTESIAN_POINT('Ctrl Pts',(-7.90766720070255,0.229746893208682,
114.625156795512));
#231879=CARTESIAN_POINT('Ctrl Pts',(-7.90723782622641,0.244031087484476,
114.624584117389));
#231880=CARTESIAN_POINT('Ctrl Pts',(-7.90703967495095,0.250369309574613,
114.624330255095));
#231881=CARTESIAN_POINT('Ctrl Pts',(-7.90662188692477,0.26323758628399,
114.623815348885));
#231882=CARTESIAN_POINT('Ctrl Pts',(-7.90640178086051,0.269767621334624,
114.623554320976));
#231883=CARTESIAN_POINT('Ctrl Pts',(-7.90591094537004,0.2838127436196,114.622993451409));
#231884=CARTESIAN_POINT('Ctrl Pts',(-7.90563758973299,0.291327736056126,
114.622693698393));
#231885=CARTESIAN_POINT('Ctrl Pts',(-7.90486880189324,0.311664679003659,
114.621883444601));
#231886=CARTESIAN_POINT('Ctrl Pts',(-7.90435288791472,0.324485859066189,
114.62137363334));
#231887=CARTESIAN_POINT('Ctrl Pts',(-7.90190864088364,0.381759868535767,
114.619100680168));
#231888=CARTESIAN_POINT('Ctrl Pts',(-7.89963647416791,0.42619764157554,
114.617349112525));
#231889=CARTESIAN_POINT('Ctrl Pts',(-7.89468230275719,0.509329481031571,
114.614094014422));
#231890=CARTESIAN_POINT('Ctrl Pts',(-7.89209041820312,0.54802743451356,
114.612587550955));
#231891=CARTESIAN_POINT('Ctrl Pts',(-7.81733217323739,1.55327480754709,
114.573674500102));
#231892=CARTESIAN_POINT('Ctrl Pts',(-7.56849444604616,2.49814016768892,
114.543782118253));
#231893=CARTESIAN_POINT('Ctrl Pts',(-7.10941212781202,3.47155414636616,
114.504878466237));
#231894=CARTESIAN_POINT('Ctrl Pts',(-7.06168512508699,3.56763658370474,
114.500926450934));
#231895=CARTESIAN_POINT('Ctrl Pts',(-6.98097845923512,3.72214401841444,
114.494340019431));
#231896=CARTESIAN_POINT('Ctrl Pts',(-6.94918270954362,3.7811738352896,114.491767443643));
#231897=CARTESIAN_POINT('Ctrl Pts',(-6.89136646568287,3.88531862618823,
114.487115164482));
#231898=CARTESIAN_POINT('Ctrl Pts',(-6.86564328632307,3.93059468982792,
114.485053796574));
#231899=CARTESIAN_POINT('Ctrl Pts',(-6.83508019006939,3.98317414802832,
114.482610273899));
#231900=CARTESIAN_POINT('Ctrl Pts',(-6.83067229322775,3.9907284445824,114.482257994627));
#231901=CARTESIAN_POINT('Ctrl Pts',(-6.82387818863219,4.00232801319199,
114.481715229317));
#231902=CARTESIAN_POINT('Ctrl Pts',(-6.8215008676627,4.00637853563081,114.481525351874));
#231903=CARTESIAN_POINT('Ctrl Pts',(-6.81733971998819,4.01345393323815,
114.481193074807));
#231904=CARTESIAN_POINT('Ctrl Pts',(-6.81555748141575,4.01647974592083,
114.481050783049));
#231905=CARTESIAN_POINT('Ctrl Pts',(-6.81181828103429,4.02281835415367,
114.480752301782));
#231906=CARTESIAN_POINT('Ctrl Pts',(-6.80986091639393,4.02613090989576,
114.480596085081));
#231907=CARTESIAN_POINT('Ctrl Pts',(-6.80503103664114,4.0342911821173,114.480210689479));
#231908=CARTESIAN_POINT('Ctrl Pts',(-6.80215576108304,4.0391372535984,114.479981325427));
#231909=CARTESIAN_POINT('Ctrl Pts',(-6.79090572551468,4.05805230379196,
114.479084166217));
#231910=CARTESIAN_POINT('Ctrl Pts',(-6.78249252699713,4.07209825359602,
114.478413817637));
#231911=CARTESIAN_POINT('Ctrl Pts',(-6.63298928719216,4.31994727149369,
114.466513280177));
#231912=CARTESIAN_POINT('Ctrl Pts',(-6.4799417815432,4.5462973459964,114.454515669699));
#231913=CARTESIAN_POINT('Ctrl Pts',(-5.87335454313425,5.35039084591772,
114.408882386469));
#231914=CARTESIAN_POINT('Ctrl Pts',(-5.3517385198692,5.87214573423439,114.373516066576));
#231915=CARTESIAN_POINT('Ctrl Pts',(-4.59652138720038,6.44210921363292,
114.331716605015));
#231916=CARTESIAN_POINT('Ctrl Pts',(-4.42240137194119,6.5628618071467,114.322586989178));
#231917=CARTESIAN_POINT('Ctrl Pts',(-4.17581324947497,6.71959543969107,
114.310353468899));
#231918=CARTESIAN_POINT('Ctrl Pts',(-4.10733697760519,6.76166862729888,
114.307026582574));
#231919=CARTESIAN_POINT('Ctrl Pts',(-4.01060801158991,6.81908910515552,
114.302423249038));
#231920=CARTESIAN_POINT('Ctrl Pts',(-3.98288606977512,6.83531794679929,
114.30111483139));
#231921=CARTESIAN_POINT('Ctrl Pts',(-3.93491757888023,6.86300851502499,
114.298869329601));
#231922=CARTESIAN_POINT('Ctrl Pts',(-3.91471800823017,6.87455054225053,
114.297929357534));
#231923=CARTESIAN_POINT('Ctrl Pts',(-3.88557154431861,6.89103469951997,
114.296581040933));
#231924=CARTESIAN_POINT('Ctrl Pts',(-3.87666562177488,6.89604880449441,
114.296170121529));
#231925=CARTESIAN_POINT('Ctrl Pts',(-3.86185654992293,6.90434867531953,
114.295488597606));
#231926=CARTESIAN_POINT('Ctrl Pts',(-3.85595887604933,6.90764415622845,
114.295217646786));
#231927=CARTESIAN_POINT('Ctrl Pts',(-3.84363773274675,6.91450822364827,
114.294652555092));
#231928=CARTESIAN_POINT('Ctrl Pts',(-3.83721349720302,6.91807542404162,
114.294358463703));
#231929=CARTESIAN_POINT('Ctrl Pts',(-3.82307638848506,6.92589961938682,
114.293712487471));
#231930=CARTESIAN_POINT('Ctrl Pts',(-3.81536135049653,6.93015269498555,
114.293360741866));
#231931=CARTESIAN_POINT('Ctrl Pts',(-3.78929796087774,6.94446396720245,
114.292175083953));
#231932=CARTESIAN_POINT('Ctrl Pts',(-3.77091674154496,6.9544622915754,114.29134328938));
#231933=CARTESIAN_POINT('Ctrl Pts',(-3.601009096742,7.04601057820812,114.283694589688));
#231934=CARTESIAN_POINT('Ctrl Pts',(-3.44689474323059,7.12267172868053,
114.277051155367));
#231935=CARTESIAN_POINT('Ctrl Pts',(-2.96804520552956,7.34168068513377,
114.257193781941));
#231936=CARTESIAN_POINT('Ctrl Pts',(-2.63613776309559,7.46728644781195,
114.244518838581));
#231937=CARTESIAN_POINT('Ctrl Pts',(-2.09530135947347,7.63138400505904,
114.224743324583));
#231938=CARTESIAN_POINT('Ctrl Pts',(-1.89132700684193,7.68447736819271,
114.21746962895));
#231939=CARTESIAN_POINT('Ctrl Pts',(-1.62476059199439,7.74260523093262,
114.208006019346));
#231940=CARTESIAN_POINT('Ctrl Pts',(-1.56389071776369,7.75512917519444,
114.205847639701));
#231941=CARTESIAN_POINT('Ctrl Pts',(-1.31352031196943,7.80357513776435,
114.196962878063));
#231942=CARTESIAN_POINT('Ctrl Pts',(-1.12288841265363,7.83327764592251,
114.190182831868));
#231943=CARTESIAN_POINT('Ctrl Pts',(-0.687675239913562,7.88487438375678,
114.174356538105));
#231944=CARTESIAN_POINT('Ctrl Pts',(-0.442777007086627,7.90241052361514,
114.165183665185));
#231945=CARTESIAN_POINT('Ctrl Pts',(-0.155869012230444,7.90957368998094,
114.153849163629));
#231946=CARTESIAN_POINT('Ctrl Pts',(-0.114280351862891,7.91028387781438,
114.152193782938));
#231947=CARTESIAN_POINT('Ctrl Pts',(-0.0605925824389661,7.91077719715592,
114.150042179127));
#231948=CARTESIAN_POINT('Ctrl Pts',(-0.0484964426018806,7.91086059903049,
114.149556452277));
#231949=CARTESIAN_POINT('Ctrl Pts',(-0.028962908378574,7.91095047793766,
114.148770564981));
#231950=CARTESIAN_POINT('Ctrl Pts',(-0.0215255885499998,7.91097421074427,
114.148470988327));
#231951=CARTESIAN_POINT('Ctrl Pts',(-0.00733222728977448,7.91099948695315,
114.147898614442));
#231952=CARTESIAN_POINT('Ctrl Pts',(-0.00057619281659804,7.91100286384868,
114.147625878188));
#231953=CARTESIAN_POINT('Ctrl Pts',(0.0148661919916847,7.91099080073623,
114.147001835228));
#231954=CARTESIAN_POINT('Ctrl Pts',(0.0235525222599233,7.91096970864169,
114.146650345047));
#231955=CARTESIAN_POINT('Ctrl Pts',(0.0495855861933373,7.91086361823253,
114.145595552935));
#231956=CARTESIAN_POINT('Ctrl Pts',(0.0669320404917187,7.91073587055013,
114.144890895756));
#231957=CARTESIAN_POINT('Ctrl Pts',(0.194657404993967,7.90937510308107,
114.139689462875));
#231958=CARTESIAN_POINT('Ctrl Pts',(0.304997985822899,7.90588901972775,
114.13512522899));
#231959=CARTESIAN_POINT('Ctrl Pts',(1.09639089180065,7.86429362762633,114.102004080089));
#231960=CARTESIAN_POINT('Ctrl Pts',(1.77007917957722,7.74054731432652,114.072103532186));
#231961=CARTESIAN_POINT('Ctrl Pts',(2.83006584447053,7.40003837323588,114.025016898902));
#231962=CARTESIAN_POINT('Ctrl Pts',(3.22912425618619,7.23481935467894,114.007178696705));
#231963=CARTESIAN_POINT('Ctrl Pts',(3.78239419646353,6.95081176089013,113.981649947119));
#231964=CARTESIAN_POINT('Ctrl Pts',(3.94885073586882,6.85761399384283,113.973866711315));
#231965=CARTESIAN_POINT('Ctrl Pts',(4.14594900292095,6.73770195786656,113.964534479781));
#231966=CARTESIAN_POINT('Ctrl Pts',(4.17996152825557,6.71665411127056,113.962919657506));
#231967=CARTESIAN_POINT('Ctrl Pts',(4.23321824147934,6.68313624250312,113.960384163536));
#231968=CARTESIAN_POINT('Ctrl Pts',(4.2525702571977,6.67083899726109,113.959461363264));
#231969=CARTESIAN_POINT('Ctrl Pts',(4.28864117034431,6.64769697164591,113.957738537487));
#231970=CARTESIAN_POINT('Ctrl Pts',(4.30537307481393,6.63687281813398,113.956938256227));
#231971=CARTESIAN_POINT('Ctrl Pts',(4.34202380469651,6.61296591453171,113.955182752732));
#231972=CARTESIAN_POINT('Ctrl Pts',(4.36192478765904,6.59985613923829,113.954227892123));
#231973=CARTESIAN_POINT('Ctrl Pts',(4.41196168130757,6.56656914924889,113.951822881017));
#231974=CARTESIAN_POINT('Ctrl Pts',(4.44201869468206,6.54627422289323,113.950374319441));
#231975=CARTESIAN_POINT('Ctrl Pts',(4.57838253454433,6.45282778709755,113.943784143384));
#231976=CARTESIAN_POINT('Ctrl Pts',(4.68303016132383,6.37728800460461,113.938676077267));
#231977=CARTESIAN_POINT('Ctrl Pts',(4.80702283426289,6.28308554109769,113.932551686855));
#231978=CARTESIAN_POINT('Ctrl Pts',(4.82817976111648,6.26684231858872,113.93150406539));
#231979=CARTESIAN_POINT('Ctrl Pts',(4.96923849630088,6.15740619421311,113.92450108791));
#231980=CARTESIAN_POINT('Ctrl Pts',(5.08651863851926,6.06088370682491,113.918590781271));
#231981=CARTESIAN_POINT('Ctrl Pts',(5.46944203580366,5.72678704840285,113.898915528615));
#231982=CARTESIAN_POINT('Ctrl Pts',(5.72179992401643,5.47465892143718,113.885327865333));
#231983=CARTESIAN_POINT('Ctrl Pts',(6.07000405933151,5.07629995589437,113.864890759587));
#231984=CARTESIAN_POINT('Ctrl Pts',(6.17941382012483,4.94253107216828,113.858177721761));
#231985=CARTESIAN_POINT('Ctrl Pts',(6.3348634033076,4.739234244161,113.848083508332));
#231986=CARTESIAN_POINT('Ctrl Pts',(6.38432734639594,4.67238692080265,113.844780672652));
#231987=CARTESIAN_POINT('Ctrl Pts',(6.44349862771441,4.58972644649087,113.840705371846));
#231988=CARTESIAN_POINT('Ctrl Pts',(6.45421670093369,4.5746420835081,113.839962020496));
#231989=CARTESIAN_POINT('Ctrl Pts',(6.47133139950275,4.55037538488,113.838766659207));
#231990=CARTESIAN_POINT('Ctrl Pts',(6.47776159667329,4.5412168987171,113.838315637896));
#231991=CARTESIAN_POINT('Ctrl Pts',(6.48999081757093,4.52372007798592,113.83745423802));
#231992=CARTESIAN_POINT('Ctrl Pts',(6.49579326097076,4.51538415487991,113.837043954804));
#231993=CARTESIAN_POINT('Ctrl Pts',(6.50901879890834,4.49630579227316,113.836105214814));
#231994=CARTESIAN_POINT('Ctrl Pts',(6.51643137622854,4.48555611040658,113.83557647929));
#231995=CARTESIAN_POINT('Ctrl Pts',(6.53911203131193,4.45248986350638,113.833950744053));
#231996=CARTESIAN_POINT('Ctrl Pts',(6.5542922866093,4.43011340171523,113.832851512073));
#231997=CARTESIAN_POINT('Ctrl Pts',(6.75070031431382,4.13737878876414,113.818485516664));
#231998=CARTESIAN_POINT('Ctrl Pts',(6.91518644639465,3.8561697374287,113.804855829073));
#231999=CARTESIAN_POINT('Ctrl Pts',(7.21748503516139,3.25745604314694,113.776689335002));
#232000=CARTESIAN_POINT('Ctrl Pts',(7.35275217020087,2.93941361845353,113.762181398554));
#232001=CARTESIAN_POINT('Ctrl Pts',(7.52026980655846,2.46082240106188,113.741162802782));
#232002=CARTESIAN_POINT('Ctrl Pts',(7.56903033656544,2.30648778501472,113.734500536522));
#232003=CARTESIAN_POINT('Ctrl Pts',(7.64225117447324,2.04730926579286,113.723496288921));
#232004=CARTESIAN_POINT('Ctrl Pts',(7.6693668485218,1.94326806808357,113.719127008371));
#232005=CARTESIAN_POINT('Ctrl Pts',(7.70314522095087,1.80191714298028,113.713250661925));
#232006=CARTESIAN_POINT('Ctrl Pts',(7.7116725865063,1.7650658969837,113.711724083907));
#232007=CARTESIAN_POINT('Ctrl Pts',(7.72548792944276,1.70335061883701,113.709176208486));
#232008=CARTESIAN_POINT('Ctrl Pts',(7.73092093279273,1.67851976889971,113.708153429652));
#232009=CARTESIAN_POINT('Ctrl Pts',(7.74137010793287,1.6296360119952,113.706144383823));
#232010=CARTESIAN_POINT('Ctrl Pts',(7.74639408238674,1.60558506606705,113.705158048417));
#232011=CARTESIAN_POINT('Ctrl Pts',(7.75803435389844,1.54853373846273,113.702823213518));
#232012=CARTESIAN_POINT('Ctrl Pts',(7.76455226704611,1.51551373425353,113.70147570528));
#232013=CARTESIAN_POINT('Ctrl Pts',(7.78552595448471,1.40557192378669,113.697001212718));
#232014=CARTESIAN_POINT('Ctrl Pts',(7.79905095799791,1.32847698549921,113.693883241214));
#232015=CARTESIAN_POINT('Ctrl Pts',(7.82919408090104,1.14028798327482,113.686313235545));
#232016=CARTESIAN_POINT('Ctrl Pts',(7.84459450253147,1.02901602708435,113.681871853586));
#232017=CARTESIAN_POINT('Ctrl Pts',(7.8869454455207,0.666297187546621,113.667474118777));
#232018=CARTESIAN_POINT('Ctrl Pts',(7.90421231435547,0.413875400263871,
113.657590547339));
#232019=CARTESIAN_POINT('Ctrl Pts',(7.91979847995507,-0.35155158898817,
113.628087938584));
#232020=CARTESIAN_POINT('Ctrl Pts',(7.88037992427006,-0.863957579144894,
113.609069262493));
#232021=CARTESIAN_POINT('Ctrl Pts',(7.72354327689219,-1.75662499191642,
113.575415831525));
#232022=CARTESIAN_POINT('Ctrl Pts',(7.6265963301856,-2.13865495738272,113.560798380348));
#232023=CARTESIAN_POINT('Ctrl Pts',(7.48686749932487,-2.55595355440418,
113.543432472595));
#232024=CARTESIAN_POINT('Ctrl Pts',(7.47171377836206,-2.59991858269763,
113.541584504388));
#232025=CARTESIAN_POINT('Ctrl Pts',(7.45224156219398,-2.65483617775734,
113.539250503246));
#232026=CARTESIAN_POINT('Ctrl Pts',(7.44828490189104,-2.66591662481712,
113.538778267818));
#232027=CARTESIAN_POINT('Ctrl Pts',(7.44196836605903,-2.68348196585731,
113.538027510647));
#232028=CARTESIAN_POINT('Ctrl Pts',(7.43962469023442,-2.68997269327859,
113.537749626476));
#232029=CARTESIAN_POINT('Ctrl Pts',(7.43520624940313,-2.70215946577246,
113.537226993314));
#232030=CARTESIAN_POINT('Ctrl Pts',(7.43313342314835,-2.70785621166325,
113.536982322144));
#232031=CARTESIAN_POINT('Ctrl Pts',(7.42847473227035,-2.72061402950442,
113.536433555154));
#232032=CARTESIAN_POINT('Ctrl Pts',(7.42588534587853,-2.72767380287272,
113.536129316073));
#232033=CARTESIAN_POINT('Ctrl Pts',(7.41930857286423,-2.74552612063222,
113.5353585125));
#232034=CARTESIAN_POINT('Ctrl Pts',(7.41530770804152,-2.75631365625485,
113.534891388578));
#232035=CARTESIAN_POINT('Ctrl Pts',(7.39350705716242,-2.81470375604336,
113.532355451843));
#232036=CARTESIAN_POINT('Ctrl Pts',(7.37527268616106,-2.8621419372535,113.530268074772));
#232037=CARTESIAN_POINT('Ctrl Pts',(7.06207546961965,-3.65407877049914,
113.494917796717));
#232038=CARTESIAN_POINT('Ctrl Pts',(6.65623160066468,-4.34967469766674,
113.45644601264));
#232039=CARTESIAN_POINT('Ctrl Pts',(5.97030351323842,-5.19844402966377,
113.407170975701));
#232040=CARTESIAN_POINT('Ctrl Pts',(5.77535354513684,-5.41420866481935,
113.394344478153));
#232041=CARTESIAN_POINT('Ctrl Pts',(5.44712486492886,-5.73952770551166,
113.374651660728));
#232042=CARTESIAN_POINT('Ctrl Pts',(5.32138803970804,-5.85629418175103,
113.367499111816));
#232043=CARTESIAN_POINT('Ctrl Pts',(5.17489428439722,-5.98371966829777,
113.359591597057));
#232044=CARTESIAN_POINT('Ctrl Pts',(5.15777616691329,-5.99848121994882,
113.358673907399));
#232045=CARTESIAN_POINT('Ctrl Pts',(5.12703394914865,-6.02476241733021,
113.35703705698));
#232046=CARTESIAN_POINT('Ctrl Pts',(5.11343373696757,-6.03630969416128,
113.356316813134));
#232047=CARTESIAN_POINT('Ctrl Pts',(5.0927654891225,-6.05373811887285,113.355228113205));
#232048=CARTESIAN_POINT('Ctrl Pts',(5.08572611306931,-6.05965307939724,
113.354858337285));
#232049=CARTESIAN_POINT('Ctrl Pts',(5.07347880131543,-6.06990772643741,
113.354216761166));
#232050=CARTESIAN_POINT('Ctrl Pts',(5.068275577176,-6.07425300995367,113.35394474324));
#232051=CARTESIAN_POINT('Ctrl Pts',(5.05753096490723,-6.08320256485267,
113.353384166553));
#232052=CARTESIAN_POINT('Ctrl Pts',(5.05198885911748,-6.08780596550942,
113.35309564171));
#232053=CARTESIAN_POINT('Ctrl Pts',(5.03860339487771,-6.09889337415696,
113.35240028448));
#232054=CARTESIAN_POINT('Ctrl Pts',(5.03075378928449,-6.10536983914922,
113.351993744307));
#232055=CARTESIAN_POINT('Ctrl Pts',(5.00653612553713,-6.12527266351154,
113.350743274616));
#232056=CARTESIAN_POINT('Ctrl Pts',(4.99012659490277,-6.13864852830099,
113.349901293058));
#232057=CARTESIAN_POINT('Ctrl Pts',(4.79600797862402,-6.29558727980826,
113.340003036966));
#232058=CARTESIAN_POINT('Ctrl Pts',(4.6122078953207,-6.43145859270225,113.331246159529));
#232059=CARTESIAN_POINT('Ctrl Pts',(4.00092727158216,-6.84363698581708,
113.303803107243));
#232060=CARTESIAN_POINT('Ctrl Pts',(3.55260747045815,-7.08673381874128,
113.286252489727));
#232061=CARTESIAN_POINT('Ctrl Pts',(2.76546831356759,-7.41995871267594,
113.256727579886));
#232062=CARTESIAN_POINT('Ctrl Pts',(2.43839833890373,-7.53377705021515,
113.244770397935));
#232063=CARTESIAN_POINT('Ctrl Pts',(1.99246000084619,-7.65686890110851,
113.227864562993));
#232064=CARTESIAN_POINT('Ctrl Pts',(1.87930374257606,-7.68542478218803,
113.223523303817));
#232065=CARTESIAN_POINT('Ctrl Pts',(1.65573706542054,-7.7366109670845,113.214783950523));
#232066=CARTESIAN_POINT('Ctrl Pts',(1.54539125460966,-7.75940593302801,
113.210391989784));
#232067=CARTESIAN_POINT('Ctrl Pts',(1.4219204773644,-7.78217381090321,113.205365827969));
#232068=CARTESIAN_POINT('Ctrl Pts',(1.40924180057216,-7.78447972645805,
113.204848499986));
#232069=CARTESIAN_POINT('Ctrl Pts',(1.39020422224186,-7.78789412385165,
113.204069947982));
#232070=CARTESIAN_POINT('Ctrl Pts',(1.38384946323937,-7.78902582654478,
113.203809772315));
#232071=CARTESIAN_POINT('Ctrl Pts',(1.37292371749809,-7.79095777169169,
113.203361954382));
#232072=CARTESIAN_POINT('Ctrl Pts',(1.3683533913763,-7.79176177321571,113.203174479009));
#232073=CARTESIAN_POINT('Ctrl Pts',(1.35894567521188,-7.79340822502756,
113.202788269167));
#232074=CARTESIAN_POINT('Ctrl Pts',(1.35410820455498,-7.79425019359295,
113.202589513716));
#232075=CARTESIAN_POINT('Ctrl Pts',(1.34246884811117,-7.79626487703156,
113.202110898841));
#232076=CARTESIAN_POINT('Ctrl Pts',(1.33566621359169,-7.79743319345547,
113.20183084932));
#232077=CARTESIAN_POINT('Ctrl Pts',(1.31083141469081,-7.80166498553403,
113.200807299654));
#232078=CARTESIAN_POINT('Ctrl Pts',(1.29279025653177,-7.80467480995383,
113.20006152277));
#232079=CARTESIAN_POINT('Ctrl Pts',(1.26045590306844,-7.80995399213806,
113.198721115593));
#232080=CARTESIAN_POINT('Ctrl Pts',(1.2461665678263,-7.81224675265937,113.198127434967));
#232081=CARTESIAN_POINT('Ctrl Pts',(1.21194253084613,-7.81764180033606,
113.196702487885));
#232082=CARTESIAN_POINT('Ctrl Pts',(1.19200214780665,-7.82070705796359,
113.19586978872));
#232083=CARTESIAN_POINT('Ctrl Pts',(1.14785007464116,-7.82732138117898,
113.194020886138));
#232084=CARTESIAN_POINT('Ctrl Pts',(1.12363324185207,-7.8308344459447,113.193003374296));
#232085=CARTESIAN_POINT('Ctrl Pts',(1.09246134556991,-7.83520888751034,
113.191689564798));
#232086=CARTESIAN_POINT('Ctrl Pts',(1.08552074697029,-7.836173480087,113.19139677846));
#232087=CARTESIAN_POINT('Ctrl Pts',(0.623368918795017,-7.8997767734597,
113.171884217319));
#232088=CARTESIAN_POINT('Ctrl Pts',(0.163577765085867,-7.92264390551656,
113.151450610919));
#232089=CARTESIAN_POINT('Ctrl Pts',(-0.898434728084774,-7.88293565769442,
113.104720070733));
#232090=CARTESIAN_POINT('Ctrl Pts',(-1.4967817999997,-7.79151050136518,
113.078861926769));
#232091=CARTESIAN_POINT('Ctrl Pts',(-2.11315342300981,-7.62363166501894,
113.053003877987));
#232092=CARTESIAN_POINT('Ctrl Pts',(-2.14728713903963,-7.61408793751334,
113.05157365325));
#232093=CARTESIAN_POINT('Ctrl Pts',(-2.19739786157058,-7.59971329487891,
113.049476175118));
#232094=CARTESIAN_POINT('Ctrl Pts',(-2.21342541982846,-7.59506072653445,
113.048805642436));
#232095=CARTESIAN_POINT('Ctrl Pts',(-2.24172040840283,-7.58674992854055,
113.047622417813));
#232096=CARTESIAN_POINT('Ctrl Pts',(-2.25399389143973,-7.58311258034037,
113.047109348872));
#232097=CARTESIAN_POINT('Ctrl Pts',(-2.27796830204144,-7.57594421789799,
113.046107463507));
#232098=CARTESIAN_POINT('Ctrl Pts',(-2.28966998029559,-7.57241584701241,
113.045618601314));
#232099=CARTESIAN_POINT('Ctrl Pts',(-2.32120563157643,-7.56282721783734,
113.044301498395));
#232100=CARTESIAN_POINT('Ctrl Pts',(-2.34102405948631,-7.55671605052908,
113.043474161789));
#232101=CARTESIAN_POINT('Ctrl Pts',(-2.41274696555027,-7.53429049698047,
113.04048120297));
#232102=CARTESIAN_POINT('Ctrl Pts',(-2.46450733505366,-7.51751853335709,
113.038323353573));
#232103=CARTESIAN_POINT('Ctrl Pts',(-2.63161917342696,-7.46145765772914,
113.031361970042));
#232104=CARTESIAN_POINT('Ctrl Pts',(-2.74623821627457,-7.42003681844865,
113.026596196436));
#232105=CARTESIAN_POINT('Ctrl Pts',(-3.50596448740633,-7.12547164732345,
112.995030906438));
#232106=CARTESIAN_POINT('Ctrl Pts',(-4.11633637035354,-6.79116331465217,
112.97009834102));
#232107=CARTESIAN_POINT('Ctrl Pts',(-4.87228790323076,-6.23733444900761,
112.935328497478));
#232108=CARTESIAN_POINT('Ctrl Pts',(-5.06244668973513,-6.08400816683078,
112.926157016051));
#232109=CARTESIAN_POINT('Ctrl Pts',(-5.31653554654547,-5.85896326461784,
112.912949759176));
#232110=CARTESIAN_POINT('Ctrl Pts',(-5.38671863427287,-5.7945027620374,
112.909192719125));
#232111=CARTESIAN_POINT('Ctrl Pts',(-5.46596082754466,-5.71903779309484,
112.90480524425));
#232112=CARTESIAN_POINT('Ctrl Pts',(-5.47617691671409,-5.70925629313809,
112.904236760569));
#232113=CARTESIAN_POINT('Ctrl Pts',(-5.49159668429594,-5.69441301241333,
112.903374324352));
#232114=CARTESIAN_POINT('Ctrl Pts',(-5.49681974719299,-5.689371350627,112.903081429476));
#232115=CARTESIAN_POINT('Ctrl Pts',(-5.50619738609891,-5.68029443683308,
112.902554165535));
#232116=CARTESIAN_POINT('Ctrl Pts',(-5.51035448844059,-5.67626179411214,
112.902319936223));
#232117=CARTESIAN_POINT('Ctrl Pts',(-5.51865199128004,-5.66819500515379,
112.901851424256));
#232118=CARTESIAN_POINT('Ctrl Pts',(-5.52279240573574,-5.66416087873738,
112.901617142688));
#232119=CARTESIAN_POINT('Ctrl Pts',(-5.53431224342692,-5.65291212554321,
112.900963909187));
#232120=CARTESIAN_POINT('Ctrl Pts',(-5.54168196012169,-5.64568760722472,
112.900544411812));
#232121=CARTESIAN_POINT('Ctrl Pts',(-5.57105765272962,-5.6167777371395,
112.898865822621));
#232122=CARTESIAN_POINT('Ctrl Pts',(-5.59295045321362,-5.59497816870379,
112.897600269055));
#232123=CARTESIAN_POINT('Ctrl Pts',(-5.95483986629369,-5.23038330241046,
112.876427902634));
#232124=CARTESIAN_POINT('Ctrl Pts',(-6.26280943483639,-4.85737050485626,
112.854380724581));
#232125=CARTESIAN_POINT('Ctrl Pts',(-6.76209061921953,-4.12561112994304,
112.813612699308));
#232126=CARTESIAN_POINT('Ctrl Pts',(-6.96358060813342,-3.77559485417696,
112.795024123401));
#232127=CARTESIAN_POINT('Ctrl Pts',(-7.24248234946587,-3.19211813449322,
112.766406024907));
#232128=CARTESIAN_POINT('Ctrl Pts',(-7.33726930677978,-2.96777042969169,
112.755910608214));
#232129=CARTESIAN_POINT('Ctrl Pts',(-7.45853864341839,-2.63922769003488,
112.741315591248));
#232130=CARTESIAN_POINT('Ctrl Pts',(-7.49348088077412,-2.538319718117,112.736933747415));
#232131=CARTESIAN_POINT('Ctrl Pts',(-7.53144841134671,-2.42104886094696,
112.731955751157));
#232132=CARTESIAN_POINT('Ctrl Pts',(-7.536477120866,-2.40534932410206,112.73129166691));
#232133=CARTESIAN_POINT('Ctrl Pts',(-7.54402950109423,-2.38151473439015,
112.730287005249));
#232134=CARTESIAN_POINT('Ctrl Pts',(-7.54658915234622,-2.37339118347494,
112.729945207109));
#232135=CARTESIAN_POINT('Ctrl Pts',(-7.55117534686139,-2.35875357345477,
112.729330445335));
#232136=CARTESIAN_POINT('Ctrl Pts',(-7.55320659083397,-2.352241002922,112.72905732236));
#232137=CARTESIAN_POINT('Ctrl Pts',(-7.55755256641395,-2.33824327032506,
112.728471139));
#232138=CARTESIAN_POINT('Ctrl Pts',(-7.55986460862298,-2.33075727717245,
112.728158170108));
#232139=CARTESIAN_POINT('Ctrl Pts',(-7.5660831471851,-2.31051612502935,
112.72731335008));
#232140=CARTESIAN_POINT('Ctrl Pts',(-7.5699685163275,-2.29775447301757,
112.72678221624));
#232141=CARTESIAN_POINT('Ctrl Pts',(-7.5871089106869,-2.24094079504664,
112.724424333573));
#232142=CARTESIAN_POINT('Ctrl Pts',(-7.60001194797521,-2.1967830467125,
112.722609536252));
#232143=CARTESIAN_POINT('Ctrl Pts',(-7.79914576292799,-1.49253143542186,
112.693943712674));
#232144=CARTESIAN_POINT('Ctrl Pts',(-7.89914780911132,-0.811104103549981,
112.670432777604));
#232145=CARTESIAN_POINT('Ctrl Pts',(-7.91070713680184,-0.0811266043454294,
112.645890246744));
#232146=CARTESIAN_POINT('Ctrl Pts',(-7.91103662902964,-0.0369916938798452,
112.644407443864));
#232147=CARTESIAN_POINT('Ctrl Pts',(-7.91052058691599,0.534480418306826,
112.625201902882));
#232148=CARTESIAN_POINT('Ctrl Pts',(-7.85731819019845,1.06039377385093,
112.607529184521));
#232149=CARTESIAN_POINT('Ctrl Pts',(-7.73864859412972,1.64373732978102,
112.584496245443));
#232150=CARTESIAN_POINT('Ctrl Pts',(-7.72421915107394,1.7102609329705,112.581817198238));
#232151=CARTESIAN_POINT('Ctrl Pts',(-7.70665313769354,1.78648300389155,
112.578679037429));
#232152=CARTESIAN_POINT('Ctrl Pts',(-7.70435375008926,1.79637340202614,
112.578270505813));
#232153=CARTESIAN_POINT('Ctrl Pts',(-7.70094117000557,1.81092491873939,
112.577667447668));
#232154=CARTESIAN_POINT('Ctrl Pts',(-7.6998427657516,1.81558953172193,112.577473830222));
#232155=CARTESIAN_POINT('Ctrl Pts',(-7.69787999262547,1.82389105855173,
112.577128710674));
#232156=CARTESIAN_POINT('Ctrl Pts',(-7.69701728212897,1.82752836717775,
112.576977311413));
#232157=CARTESIAN_POINT('Ctrl Pts',(-7.69521172663924,1.83511688544628,
112.576661057798));
#232158=CARTESIAN_POINT('Ctrl Pts',(-7.69426841608465,1.83906798193346,
112.576496174422));
#232159=CARTESIAN_POINT('Ctrl Pts',(-7.69179523779342,1.84939178429493,
112.57606477155));
#232160=CARTESIAN_POINT('Ctrl Pts',(-7.69026050025146,1.85576329022109,
112.575797945626));
#232161=CARTESIAN_POINT('Ctrl Pts',(-7.68341105032408,1.88404456345179,
112.574611038228));
#232162=CARTESIAN_POINT('Ctrl Pts',(-7.67801065730547,1.90593326498587,
112.573685631838));
#232163=CARTESIAN_POINT('Ctrl Pts',(-7.63785730026498,2.06574111364481,
112.566881422263));
#232164=CARTESIAN_POINT('Ctrl Pts',(-7.59948583546931,2.20271673573322,
112.560788600797));
#232165=CARTESIAN_POINT('Ctrl Pts',(-7.50078270262243,2.52169021405716,
112.546119576812));
#232166=CARTESIAN_POINT('Ctrl Pts',(-7.43748560225496,2.70267715976454,
112.537422201172));
#232167=CARTESIAN_POINT('Ctrl Pts',(-7.16885069260496,3.38962428088298,
112.50344593749));
#232168=CARTESIAN_POINT('Ctrl Pts',(-6.91789734176502,3.87617714141812,
112.477449769005));
#232169=CARTESIAN_POINT('Ctrl Pts',(-6.40795510046922,4.65513353462324,
112.435601828651));
#232170=CARTESIAN_POINT('Ctrl Pts',(-6.17382596418324,4.96146035562347,
112.419040055832));
#232171=CARTESIAN_POINT('Ctrl Pts',(-5.9013024602782,5.26870055621896,112.40240956427));
#232172=CARTESIAN_POINT('Ctrl Pts',(-5.88422300577274,5.28776851937222,
112.40137717493));
#232173=CARTESIAN_POINT('Ctrl Pts',(-5.86086320639216,5.31359469386752,
112.399978445572));
#232174=CARTESIAN_POINT('Ctrl Pts',(-5.85466325138469,5.32042519996339,
112.399608468074));
#232175=CARTESIAN_POINT('Ctrl Pts',(-5.84412313802294,5.3319965359537,112.398981626152));
#232176=CARTESIAN_POINT('Ctrl Pts',(-5.83978913068446,5.33674294127286,
112.398724482531));
#232177=CARTESIAN_POINT('Ctrl Pts',(-5.83142113724213,5.34588478297197,
112.398229166124));
#232178=CARTESIAN_POINT('Ctrl Pts',(-5.82738795495744,5.35028094732624,
112.397990957017));
#232179=CARTESIAN_POINT('Ctrl Pts',(-5.81784620955809,5.36065785097451,
112.39742862973));
#232180=CARTESIAN_POINT('Ctrl Pts',(-5.81233338603798,5.3666346739256,112.397104706412));
#232181=CARTESIAN_POINT('Ctrl Pts',(-5.79618724268989,5.38408573226781,
112.396158802609));
#232182=CARTESIAN_POINT('Ctrl Pts',(-5.78552906125236,5.39553697142363,
112.395537961112));
#232183=CARTESIAN_POINT('Ctrl Pts',(-5.70765179494423,5.47871287801388,
112.391027296917));
#232184=CARTESIAN_POINT('Ctrl Pts',(-5.63913361408311,5.54921226987187,
112.387197779424));
#232185=CARTESIAN_POINT('Ctrl Pts',(-5.41503067902359,5.77135672064771,
112.37509383494));
#232186=CARTESIAN_POINT('Ctrl Pts',(-5.25450415597635,5.91788052226589,
112.367055924889));
#232187=CARTESIAN_POINT('Ctrl Pts',(-4.9208061765846,6.19817268219947,112.351383868402));
#232188=CARTESIAN_POINT('Ctrl Pts',(-4.74771440858341,6.33173679699968,
112.343759134459));
#232189=CARTESIAN_POINT('Ctrl Pts',(-4.41354777934905,6.5681751577929,112.329690138851));
#232190=CARTESIAN_POINT('Ctrl Pts',(-4.25384838785275,6.67271335445584,
112.323222706623));
#232191=CARTESIAN_POINT('Ctrl Pts',(-3.69173636729675,7.0122800344171,112.300903630733));
#232192=CARTESIAN_POINT('Ctrl Pts',(-3.27248271782822,7.21746215752754,
112.285047760965));
#232193=CARTESIAN_POINT('Ctrl Pts',(-2.76508760558085,7.4124393604572,112.264126196738));
#232194=CARTESIAN_POINT('Ctrl Pts',(-2.69210259560071,7.43925732745265,
112.261075767721));
#232195=CARTESIAN_POINT('Ctrl Pts',(-2.60975324957411,7.46814566053639,
112.257575271975));
#232196=CARTESIAN_POINT('Ctrl Pts',(-2.60076441714839,7.47128075198408,
112.257192390781));
#232197=CARTESIAN_POINT('Ctrl Pts',(-2.58712288988608,7.47601099142808,
112.256610138986));
#232198=CARTESIAN_POINT('Ctrl Pts',(-2.58247437606134,7.47761802234531,
112.256411521769));
#232199=CARTESIAN_POINT('Ctrl Pts',(-2.57436915886316,7.4804116056973,112.256064851282));
#232200=CARTESIAN_POINT('Ctrl Pts',(-2.57091312191444,7.48160010133083,
112.255916918622));
#232201=CARTESIAN_POINT('Ctrl Pts',(-2.5636862234181,7.48407975868727,112.255607342027));
#232202=CARTESIAN_POINT('Ctrl Pts',(-2.5599152079401,7.48537046608772,112.25544567017));
#232203=CARTESIAN_POINT('Ctrl Pts',(-2.55097397450865,7.48842323973973,
112.255062024824));
#232204=CARTESIAN_POINT('Ctrl Pts',(-2.5458029095474,7.49018280027567,112.254839898448));
#232205=CARTESIAN_POINT('Ctrl Pts',(-2.52863953070263,7.49600316366971,
112.254101817632));
#232206=CARTESIAN_POINT('Ctrl Pts',(-2.51663934455676,7.50004051401404,
112.253584448281));
#232207=CARTESIAN_POINT('Ctrl Pts',(-2.30543729789122,7.57053350963195,
112.244456206782));
#232208=CARTESIAN_POINT('Ctrl Pts',(-2.10369098035574,7.62905563255482,
112.235384477075));
#232209=CARTESIAN_POINT('Ctrl Pts',(-1.41324078680129,7.79987023753732,
112.20370808742));
#232210=CARTESIAN_POINT('Ctrl Pts',(-0.916279749184769,7.87373114606134,
112.179928462444));
#232211=CARTESIAN_POINT('Ctrl Pts',(0.1846609846624,7.93166019708067,112.128819944313));
#232212=CARTESIAN_POINT('Ctrl Pts',(0.786726088605145,7.89471988969007,
112.101987522156));
#232213=CARTESIAN_POINT('Ctrl Pts',(1.41984442582819,7.7826534291933,112.075734421887));
#232214=CARTESIAN_POINT('Ctrl Pts',(1.46076240340292,7.77507722550135,112.074045601871));
#232215=CARTESIAN_POINT('Ctrl Pts',(1.51454879200776,7.76467876872756,112.071835775343));
#232216=CARTESIAN_POINT('Ctrl Pts',(1.52747224572763,7.76214680134332,112.071305582399));
#232217=CARTESIAN_POINT('Ctrl Pts',(1.54746249932182,7.75817844690892,112.070486648974));
#232218=CARTESIAN_POINT('Ctrl Pts',(1.55453372987065,7.75676465312302,112.070197193081));
#232219=CARTESIAN_POINT('Ctrl Pts',(1.56794197680835,7.75406479008347,112.069648766825));
#232220=CARTESIAN_POINT('Ctrl Pts',(1.57427936616429,7.7527806165897,112.069389736666));
#232221=CARTESIAN_POINT('Ctrl Pts',(1.58892828366458,7.74979353857117,112.06879140686));
#232222=CARTESIAN_POINT('Ctrl Pts',(1.59723866800853,7.74808502916086,112.068452285077));
#232223=CARTESIAN_POINT('Ctrl Pts',(1.62052090852031,7.74325944656354,112.067503076921));
#232224=CARTESIAN_POINT('Ctrl Pts',(1.63548653414615,7.74011231647928,112.066893943067));
#232225=CARTESIAN_POINT('Ctrl Pts',(1.721757171729,7.72170903245117,112.063388271127));
#232226=CARTESIAN_POINT('Ctrl Pts',(1.79285871039398,7.70551076413261,112.060521660518));
#232227=CARTESIAN_POINT('Ctrl Pts',(1.99695951658718,7.656034716535,112.052352417551));
#232228=CARTESIAN_POINT('Ctrl Pts',(2.12933290619281,7.62027941527067,112.047127790685));
#232229=CARTESIAN_POINT('Ctrl Pts',(2.58701521984609,7.48379674542077,112.029255871272));
#232230=CARTESIAN_POINT('Ctrl Pts',(2.90670469264634,7.36552424538543,112.017131959862));
#232231=CARTESIAN_POINT('Ctrl Pts',(3.52866640681707,7.08859914083725,111.993349623488));
#232232=CARTESIAN_POINT('Ctrl Pts',(3.8302831698902,6.93027054635327,111.981712036828));
#232233=CARTESIAN_POINT('Ctrl Pts',(4.43647602569573,6.56036509885454,111.956694794425));
#232234=CARTESIAN_POINT('Ctrl Pts',(4.7382920730877,6.34581052912333,111.943224246407));
#232235=CARTESIAN_POINT('Ctrl Pts',(5.04737757370442,6.09170063017525,111.927344412878));
#232236=CARTESIAN_POINT('Ctrl Pts',(5.07064496526052,6.0723468729355,111.926136824991));
#232237=CARTESIAN_POINT('Ctrl Pts',(5.1022974516512,6.04570963937785,111.924477864752));
#232238=CARTESIAN_POINT('Ctrl Pts',(5.1107792804007,6.03854117104392,111.924031715948));
#232239=CARTESIAN_POINT('Ctrl Pts',(5.12419651889446,6.02715299288839,111.92332344986));
#232240=CARTESIAN_POINT('Ctrl Pts',(5.12914189238221,6.02294501149395,111.923061851703));
#232241=CARTESIAN_POINT('Ctrl Pts',(5.13912362365291,6.01443042129828,111.922532752217));
#232242=CARTESIAN_POINT('Ctrl Pts',(5.14415976185402,6.01012356412406,111.922265240131));
#232243=CARTESIAN_POINT('Ctrl Pts',(5.15563377340891,6.0002861122001,111.921654482681));
#232244=CARTESIAN_POINT('Ctrl Pts',(5.16206816534394,5.99475147854484,111.921311064176));
#232245=CARTESIAN_POINT('Ctrl Pts',(5.17555368921598,5.98311390284775,111.920589398495));
#232246=CARTESIAN_POINT('Ctrl Pts',(5.18260295955651,5.97700882776834,111.92021106186));
#232247=CARTESIAN_POINT('Ctrl Pts',(5.20116649400566,5.96087420366462,111.919211871433));
#232248=CARTESIAN_POINT('Ctrl Pts',(5.21266251780874,5.95082377846834,111.918590161127));
#232249=CARTESIAN_POINT('Ctrl Pts',(5.2471467513808,5.92049925814134,111.916716544574));
#232250=CARTESIAN_POINT('Ctrl Pts',(5.27004619179904,5.90012488064244,111.915460683213));
#232251=CARTESIAN_POINT('Ctrl Pts',(5.56022372823688,5.63890734391712,111.899402005965));
#232252=CARTESIAN_POINT('Ctrl Pts',(5.81088135188796,5.38024221944273,111.88398235848));
#232253=CARTESIAN_POINT('Ctrl Pts',(6.38462290335778,4.70113133761827,111.8457484389));
#232254=CARTESIAN_POINT('Ctrl Pts',(6.68477048956573,4.26355829717568,111.823047272943));
#232255=CARTESIAN_POINT('Ctrl Pts',(6.95537383710379,3.76933179892526,111.799485201527));
#232256=CARTESIAN_POINT('Ctrl Pts',(6.97158180182717,3.73926926230999,111.798059076561));
#232257=CARTESIAN_POINT('Ctrl Pts',(7.18577932424425,3.33574161648553,111.779008338274));
#232258=CARTESIAN_POINT('Ctrl Pts',(7.35372820958812,2.94708229346627,111.761636113289));
#232259=CARTESIAN_POINT('Ctrl Pts',(7.50849735888368,2.49193793688402,111.742135234959));
#232260=CARTESIAN_POINT('Ctrl Pts',(7.52657140659689,2.43680327303146,111.739787948531));
#232261=CARTESIAN_POINT('Ctrl Pts',(7.55206797975294,2.35603520327152,111.736371061823));
#232262=CARTESIAN_POINT('Ctrl Pts',(7.55996986438192,2.33055536420826,111.735296269418));
#232263=CARTESIAN_POINT('Ctrl Pts',(7.57364094954481,2.28567135550215,111.733408432078));
#232264=CARTESIAN_POINT('Ctrl Pts',(7.57946482655216,2.26628412247278,111.732594783776));
#232265=CARTESIAN_POINT('Ctrl Pts',(7.59133159270417,2.22622316008193,111.730917152477));
#232266=CARTESIAN_POINT('Ctrl Pts',(7.59736459568749,2.20554666973773,111.730053287685));
#232267=CARTESIAN_POINT('Ctrl Pts',(7.61260208808465,2.15251984859686,111.727842906393));
#232268=CARTESIAN_POINT('Ctrl Pts',(7.62168486080764,2.1201349356626,111.726497799911));
#232269=CARTESIAN_POINT('Ctrl Pts',(7.64094068252225,2.04975451102119,111.723584834628));
#232270=CARTESIAN_POINT('Ctrl Pts',(7.65103745866591,2.01173902279244,111.722017889209));
#232271=CARTESIAN_POINT('Ctrl Pts',(7.7771514331278,1.52221938418228,111.701921376334));
#232272=CARTESIAN_POINT('Ctrl Pts',(7.85332464510056,1.06138845881248,111.683947989645));
#232273=CARTESIAN_POINT('Ctrl Pts',(7.91810388045191,0.204746528739609,
111.650939998041));
#232274=CARTESIAN_POINT('Ctrl Pts',(7.91850164150383,-0.188683439909868,
111.635914772417));
#232275=CARTESIAN_POINT('Ctrl Pts',(7.88661785189892,-0.622023875752945,
111.618622994193));
#232276=CARTESIAN_POINT('Ctrl Pts',(7.88323461667545,-0.663526015734557,
111.616959081432));
#232277=CARTESIAN_POINT('Ctrl Pts',(7.87819218186543,-0.719883505418238,
111.61468739305));
#232278=CARTESIAN_POINT('Ctrl Pts',(7.87681828539855,-0.734763914900181,
111.614086417659));
#232279=CARTESIAN_POINT('Ctrl Pts',(7.87442117027659,-0.759946987317319,
111.613067409755));
#232280=CARTESIAN_POINT('Ctrl Pts',(7.87341987113188,-0.770251726726619,
111.612649890272));
#232281=CARTESIAN_POINT('Ctrl Pts',(7.87139186024123,-0.790705533046299,
111.611820090674));
#232282=CARTESIAN_POINT('Ctrl Pts',(7.87036574130037,-0.800854640311396,
111.611407824644));
#232283=CARTESIAN_POINT('Ctrl Pts',(7.86783801239251,-0.825381724815755,
111.610410273401));
#232284=CARTESIAN_POINT('Ctrl Pts',(7.86631661806772,-0.839757609815118,
111.609824556499));
#232285=CARTESIAN_POINT('Ctrl Pts',(7.86100591509645,-0.888658152848299,
111.607828793702));
#232286=CARTESIAN_POINT('Ctrl Pts',(7.85702866795913,-0.923161846681067,
111.606414824047));
#232287=CARTESIAN_POINT('Ctrl Pts',(7.84687561329931,-1.00641893485256,
111.602989880116));
#232288=CARTESIAN_POINT('Ctrl Pts',(7.84047250443339,-1.05514302689035,
111.600974695536));
#232289=CARTESIAN_POINT('Ctrl Pts',(7.81437345816508,-1.24036604674837,
111.593276721959));
#232290=CARTESIAN_POINT('Ctrl Pts',(7.79156355174329,-1.3763999970876,111.587546066637));
#232291=CARTESIAN_POINT('Ctrl Pts',(7.72064885037628,-1.74065442281843,
111.572047336249));
#232292=CARTESIAN_POINT('Ctrl Pts',(7.66598971947217,-1.96745962859462,
111.562234882232));
#232293=CARTESIAN_POINT('Ctrl Pts',(7.50660473977578,-2.52029470362026,
111.538080029504));
#232294=CARTESIAN_POINT('Ctrl Pts',(7.39058422396799,-2.84258238656474,
111.523798477966));
#232295=CARTESIAN_POINT('Ctrl Pts',(7.19327508315327,-3.29604682436632,
111.503480505372));
#232296=CARTESIAN_POINT('Ctrl Pts',(7.12846730226794,-3.43396070733405,
111.497266942646));
#232297=CARTESIAN_POINT('Ctrl Pts',(7.03958940059646,-3.6097217990437,111.489292499587));
#232298=CARTESIAN_POINT('Ctrl Pts',(7.01912568190696,-3.64935406408052,
111.487490549286));
#232299=CARTESIAN_POINT('Ctrl Pts',(6.98579420650509,-3.71258977160168,
111.48460877309));
#232300=CARTESIAN_POINT('Ctrl Pts',(6.97313945824269,-3.73630427156449,
111.4835265408));
#232301=CARTESIAN_POINT('Ctrl Pts',(6.95000413926029,-3.77913198934423,
111.481569156271));
#232302=CARTESIAN_POINT('Ctrl Pts',(6.93956497578531,-3.79826724686233,
111.480693547084));
#232303=CARTESIAN_POINT('Ctrl Pts',(6.91463924627986,-3.84351097183807,
111.478620616649));
#232304=CARTESIAN_POINT('Ctrl Pts',(6.90008367977602,-3.86958107767362,
111.477424080412));
#232305=CARTESIAN_POINT('Ctrl Pts',(6.85635964697601,-3.94686290188376,
111.473870477624));
#232306=CARTESIAN_POINT('Ctrl Pts',(6.82676604488052,-3.99783188732277,
111.471518125612));
#232307=CARTESIAN_POINT('Ctrl Pts',(6.62569997611054,-4.33538366262448,
111.455873394658));
#232308=CARTESIAN_POINT('Ctrl Pts',(6.43679086253933,-4.61120213876708,
111.442724663278));
#232309=CARTESIAN_POINT('Ctrl Pts',(5.950388605081,-5.2329955114721,111.412095534704));
#232310=CARTESIAN_POINT('Ctrl Pts',(5.63930299689599,-5.56683474593546,
111.394960583603));
#232311=CARTESIAN_POINT('Ctrl Pts',(4.93344773447329,-6.20407109166134,
111.359605980503));
#232312=CARTESIAN_POINT('Ctrl Pts',(4.53533003857126,-6.50077865161586,
111.341503892046));
#232313=CARTESIAN_POINT('Ctrl Pts',(4.10713212375609,-6.76131797390543,
111.321831028263));
#232314=CARTESIAN_POINT('Ctrl Pts',(4.10214553370757,-6.76434453929955,
111.321601888493));
#232315=CARTESIAN_POINT('Ctrl Pts',(4.09341197903241,-6.76963208170764,
111.32120049619));
#232316=CARTESIAN_POINT('Ctrl Pts',(4.0896664743973,-6.77189547171881,111.321028329485));
#232317=CARTESIAN_POINT('Ctrl Pts',(4.06155894517909,-6.78884888918424,
111.319736139082));
#232318=CARTESIAN_POINT('Ctrl Pts',(4.03711987854779,-6.80341042194274,
111.318611510874));
#232319=CARTESIAN_POINT('Ctrl Pts',(3.98759450182436,-6.8325583166099,111.316329332017));
#232320=CARTESIAN_POINT('Ctrl Pts',(3.96250542414426,-6.84713909591076,
111.315171591118));
#232321=CARTESIAN_POINT('Ctrl Pts',(3.92843139823489,-6.86669157390015,
111.313596377551));
#232322=CARTESIAN_POINT('Ctrl Pts',(3.91951599262595,-6.87178439737819,
111.313183962083));
#232323=CARTESIAN_POINT('Ctrl Pts',(3.90545208116505,-6.87978197229042,
111.312532932222));
#232324=CARTESIAN_POINT('Ctrl Pts',(3.90031017346697,-6.88269834404029,
111.31229481438));
#232325=CARTESIAN_POINT('Ctrl Pts',(3.8900333939987,-6.88851188241089,111.311818706654));
#232326=CARTESIAN_POINT('Ctrl Pts',(3.88489854310113,-6.89140907725707,
111.311580718258));
#232327=CARTESIAN_POINT('Ctrl Pts',(3.87322205158826,-6.89798001074148,
111.311039306507));
#232328=CARTESIAN_POINT('Ctrl Pts',(3.86667841954505,-6.90165018592094,
111.31073572721));
#232329=CARTESIAN_POINT('Ctrl Pts',(3.84739268711605,-6.91243107993378,
111.309840486735));
#232330=CARTESIAN_POINT('Ctrl Pts',(3.83463616454897,-6.91951583605683,
111.309247669123));
#232331=CARTESIAN_POINT('Ctrl Pts',(3.80576419757159,-6.93544647657645,
111.307904295135));
#232332=CARTESIAN_POINT('Ctrl Pts',(3.78963740938042,-6.94427154238952,
111.307152784459));
#232333=CARTESIAN_POINT('Ctrl Pts',(3.73853757340752,-6.97200390219291,
111.304767461512));
#232334=CARTESIAN_POINT('Ctrl Pts',(3.70345306045986,-6.99070360849325,
111.303123732742));
#232335=CARTESIAN_POINT('Ctrl Pts',(3.56958117391429,-7.06076540902813,
111.29682383237));
#232336=CARTESIAN_POINT('Ctrl Pts',(3.46985809830789,-7.11030242170683,
111.292072624146));
#232337=CARTESIAN_POINT('Ctrl Pts',(3.13213093139495,-7.26927014301055,
111.2758602999));
#232338=CARTESIAN_POINT('Ctrl Pts',(2.88975138593265,-7.36897930136424,
111.264029474646));
#232339=CARTESIAN_POINT('Ctrl Pts',(2.10174187432691,-7.64828276653502,
111.225770356771));
#232340=CARTESIAN_POINT('Ctrl Pts',(1.5412703510745,-7.78062527016558,111.198985420755));
#232341=CARTESIAN_POINT('Ctrl Pts',(0.867232250670853,-7.86402227863397,
111.169160921739));
#232342=CARTESIAN_POINT('Ctrl Pts',(0.762815493206369,-7.8748366125221,
111.16460217229));
#232343=CARTESIAN_POINT('Ctrl Pts',(0.445424056729578,-7.90133613885045,
111.150940046646));
#232344=CARTESIAN_POINT('Ctrl Pts',(0.231995195635322,-7.91048054978834,
111.142020878728));
#232345=CARTESIAN_POINT('Ctrl Pts',(-0.00235140532270151,-7.91102698930574,
111.132515582081));
#232346=CARTESIAN_POINT('Ctrl Pts',(-0.0231495041654061,-7.91099346879504,
111.131674450472));
#232347=CARTESIAN_POINT('Ctrl Pts',(-0.0540324159673709,-7.91082190484312,
111.130429073522));
#232348=CARTESIAN_POINT('Ctrl Pts',(-0.0641174088612166,-7.91074659377375,
111.130022960402));
#232349=CARTESIAN_POINT('Ctrl Pts',(-0.0813818067504496,-7.91058465298454,
111.129328713199));
#232350=CARTESIAN_POINT('Ctrl Pts',(-0.0885612775438487,-7.91050753434852,
111.129040295934));
#232351=CARTESIAN_POINT('Ctrl Pts',(-0.102528298626715,-7.91033849003725,
111.128479764394));
#232352=CARTESIAN_POINT('Ctrl Pts',(-0.109315854686147,-7.91024760188971,
111.128207619409));
#232353=CARTESIAN_POINT('Ctrl Pts',(-0.125549181610145,-7.91000933292641,
111.127557360462));
#232354=CARTESIAN_POINT('Ctrl Pts',(-0.134994831181229,-7.90985376857823,
111.127179490808));
#232355=CARTESIAN_POINT('Ctrl Pts',(-0.16330912476675,-7.90933671585864,
111.126048263469));
#232356=CARTESIAN_POINT('Ctrl Pts',(-0.182176835170889,-7.90892462739567,
111.125296415184));
#232357=CARTESIAN_POINT('Ctrl Pts',(-0.346466217203392,-7.90474817736555,
111.118766631609));
#232358=CARTESIAN_POINT('Ctrl Pts',(-0.491763757892237,-7.89704081335171,
111.113107615084));
#232359=CARTESIAN_POINT('Ctrl Pts',(-1.02375288340134,-7.85408063664059,
111.092753650817));
#232360=CARTESIAN_POINT('Ctrl Pts',(-1.40792547580746,-7.7943844299036,
111.078795147707));
#232361=CARTESIAN_POINT('Ctrl Pts',(-1.85159402073955,-7.69155572615592,
111.062854385325));
#232362=CARTESIAN_POINT('Ctrl Pts',(-1.91681306457954,-7.67556236793706,
111.060514799688));
#232363=CARTESIAN_POINT('Ctrl Pts',(-2.03647610356062,-7.64459765425372,
111.056221222414));
#232364=CARTESIAN_POINT('Ctrl Pts',(-2.09097850024661,-7.6298700616622,
111.054265278994));
#232365=CARTESIAN_POINT('Ctrl Pts',(-2.19196070026748,-7.60141943631396,
111.050635652101));
#232366=CARTESIAN_POINT('Ctrl Pts',(-2.23848101643335,-7.58785028227303,
111.048961312495));
#232367=CARTESIAN_POINT('Ctrl Pts',(-2.32524980233874,-7.56167395148363,
111.045830831975));
#232368=CARTESIAN_POINT('Ctrl Pts',(-2.36552779220756,-7.54917067337047,
111.044374604609));
#232369=CARTESIAN_POINT('Ctrl Pts',(-2.44102271524304,-7.52507166964829,
111.041637080661));
#232370=CARTESIAN_POINT('Ctrl Pts',(-2.47626184338731,-7.51354928169662,
111.040355954133));
#232371=CARTESIAN_POINT('Ctrl Pts',(-2.81608528283476,-7.39978441996949,
111.027961215968));
#232372=CARTESIAN_POINT('Ctrl Pts',(-3.11424351042991,-7.2793279900415,
111.016779634582));
#232373=CARTESIAN_POINT('Ctrl Pts',(-3.59223945019578,-7.05146181911222,
110.997327884815));
#232374=CARTESIAN_POINT('Ctrl Pts',(-3.77662592146045,-6.95445130273584,
110.989419127928));
#232375=CARTESIAN_POINT('Ctrl Pts',(-3.970578985214,-6.8424170131216,110.980471380863));
#232376=CARTESIAN_POINT('Ctrl Pts',(-3.98416605645883,-6.8345145320256,
110.979841303779));
#232377=CARTESIAN_POINT('Ctrl Pts',(-4.00330987262827,-6.82330366355085,
110.978949037186));
#232378=CARTESIAN_POINT('Ctrl Pts',(-4.00888631224433,-6.82002883838947,
110.978688585846));
#232379=CARTESIAN_POINT('Ctrl Pts',(-4.01859119105505,-6.81431352663,110.978234378188));
#232380=CARTESIAN_POINT('Ctrl Pts',(-4.0227214431666,-6.81187611385912,
110.978040778753));
#232381=CARTESIAN_POINT('Ctrl Pts',(-4.03104700064761,-6.80695268526882,
110.977649938508));
#232382=CARTESIAN_POINT('Ctrl Pts',(-4.03524222936281,-6.80446654272952,
110.977452691322));
#232383=CARTESIAN_POINT('Ctrl Pts',(-4.04382060397708,-6.79937217232032,
110.977048744196));
#232384=CARTESIAN_POINT('Ctrl Pts',(-4.04820353142919,-6.79676358150146,
110.976842026174));
#232385=CARTESIAN_POINT('Ctrl Pts',(-4.06274919730392,-6.78808736370599,
110.976154899337));
#232386=CARTESIAN_POINT('Ctrl Pts',(-4.07290080979013,-6.7820011861529,
110.97567357628));
#232387=CARTESIAN_POINT('Ctrl Pts',(-4.14367277157242,-6.73935519264396,
110.972305878843));
#232388=CARTESIAN_POINT('Ctrl Pts',(-4.2038125001105,-6.70200660272594,
110.969381783264));
#232389=CARTESIAN_POINT('Ctrl Pts',(-4.39431525120925,-6.5801256287458,
110.959937956363));
#232390=CARTESIAN_POINT('Ctrl Pts',(-4.5226901008181,-6.49255966865117,
110.953299013851));
#232391=CARTESIAN_POINT('Ctrl Pts',(-4.78121643000406,-6.3048261755347,
110.939471899504));
#232392=CARTESIAN_POINT('Ctrl Pts',(-4.91099821715921,-6.20426938742024,
110.932277328013));
#232393=CARTESIAN_POINT('Ctrl Pts',(-5.38933714422978,-5.80922712670214,
110.904990526582));
#232394=CARTESIAN_POINT('Ctrl Pts',(-5.71534656372106,-5.48880020943202,
110.884849278843));
#232395=CARTESIAN_POINT('Ctrl Pts',(-6.20145865784987,-4.92045328379064,
110.853027434505));
#232396=CARTESIAN_POINT('Ctrl Pts',(-6.37860261586297,-4.68853850562576,
110.84092226146));
#232397=CARTESIAN_POINT('Ctrl Pts',(-6.56259133278112,-4.41787137633144,
110.827674004635));
#232398=CARTESIAN_POINT('Ctrl Pts',(-6.58243787344046,-4.38824613782523,
110.826235016445));
#232399=CARTESIAN_POINT('Ctrl Pts',(-6.61120130874972,-4.34467629869567,
110.824134432034));
#232400=CARTESIAN_POINT('Ctrl Pts',(-6.62027573997042,-4.33083641049326,
110.823469488958));
#232401=CARTESIAN_POINT('Ctrl Pts',(-6.63630348094039,-4.30622357861167,
110.822290983533));
#232402=CARTESIAN_POINT('Ctrl Pts',(-6.64327414588325,-4.2954620268234,
110.82177706116));
#232403=CARTESIAN_POINT('Ctrl Pts',(-6.65772833241956,-4.27302781452356,
110.820708501143));
#232404=CARTESIAN_POINT('Ctrl Pts',(-6.66520739301084,-4.26135232778572,
110.820153956034));
#232405=CARTESIAN_POINT('Ctrl Pts',(-6.68450323710811,-4.23105470184876,
110.818718929504));
#232406=CARTESIAN_POINT('Ctrl Pts',(-6.69627292924543,-4.21240267298676,
110.817839394459));
#232407=CARTESIAN_POINT('Ctrl Pts',(-6.74432992799329,-4.13553391334734,
110.814230331489));
#232408=CARTESIAN_POINT('Ctrl Pts',(-6.77993768657995,-4.07689490615675,
110.811513743266));
#232409=CARTESIAN_POINT('Ctrl Pts',(-7.00209447447337,-3.70008437201776,
110.794283977837));
#232410=CARTESIAN_POINT('Ctrl Pts',(-7.16696771580084,-3.36965062731502,
110.780223435643));
#232411=CARTESIAN_POINT('Ctrl Pts',(-7.49821346624278,-2.57041591087699,
110.747930290955));
#232412=CARTESIAN_POINT('Ctrl Pts',(-7.64466414307928,-2.09507407916465,
110.730037128669));
#232413=CARTESIAN_POINT('Ctrl Pts',(-7.7538733298244,-1.56940062958409,
110.709936685136));
#232414=CARTESIAN_POINT('Ctrl Pts',(-7.76182688411091,-1.52957946506288,
110.708411634109));
#232415=CARTESIAN_POINT('Ctrl Pts',(-7.79560845134439,-1.35339287706458,
110.701648713176));
#232416=CARTESIAN_POINT('Ctrl Pts',(-7.81815132214717,-1.21642568737082,
110.696350802941));
#232417=CARTESIAN_POINT('Ctrl Pts',(-7.84945358411972,-0.989055971269558,
110.68741255796));
#232418=CARTESIAN_POINT('Ctrl Pts',(-7.86028052091558,-0.898967564056434,
110.683834002599));
#232419=CARTESIAN_POINT('Ctrl Pts',(-7.87108054967468,-0.793873155461385,
110.679600336813));
#232420=CARTESIAN_POINT('Ctrl Pts',(-7.87256377471032,-0.779027095671503,
110.679000902662));
#232421=CARTESIAN_POINT('Ctrl Pts',(-7.87473154053604,-0.756690648616988,
110.678096878959));
#232422=CARTESIAN_POINT('Ctrl Pts',(-7.87544741611877,-0.749203289281413,
110.677793479182));
#232423=CARTESIAN_POINT('Ctrl Pts',(-7.87670319390409,-0.735868385275503,
110.677252465814));
#232424=CARTESIAN_POINT('Ctrl Pts',(-7.87724726570195,-0.730021232607731,
110.67701501319));
#232425=CARTESIAN_POINT('Ctrl Pts',(-7.87828431509094,-0.71873988627927,
110.676556433943));
#232426=CARTESIAN_POINT('Ctrl Pts',(-7.87877818209959,-0.713305776377036,
110.676335342184));
#232427=CARTESIAN_POINT('Ctrl Pts',(-7.87983326485453,-0.701561721111284,
110.675857088325));
#232428=CARTESIAN_POINT('Ctrl Pts',(-7.88039252403279,-0.695251607182838,
110.675599849153));
#232429=CARTESIAN_POINT('Ctrl Pts',(-7.88172741698934,-0.679981476153497,
110.674976674643));
#232430=CARTESIAN_POINT('Ctrl Pts',(-7.88249535100039,-0.671020807569307,
110.674610431649));
#232431=CARTESIAN_POINT('Ctrl Pts',(-7.88452897022534,-0.646806156399707,
110.673619179338));
#232432=CARTESIAN_POINT('Ctrl Pts',(-7.88576566332396,-0.631549827668696,
110.672992990196));
#232433=CARTESIAN_POINT('Ctrl Pts',(-7.90289099036284,-0.412388850801295,
110.663972883019));
#232434=CARTESIAN_POINT('Ctrl Pts',(-7.91090819443579,-0.207985776564891,
110.655206635585));
#232435=CARTESIAN_POINT('Ctrl Pts',(-7.91099921610637,-0.0035217558676004,
110.646171848042));
#232436=CARTESIAN_POINT('',(-7.91099910237999,-0.00376857307924841,108.642331508237));
#232437=CARTESIAN_POINT('Ctrl Pts',(-7.9109991388093,-0.00369130851947151,
110.642331508237));
#232438=CARTESIAN_POINT('Ctrl Pts',(-7.91108984706874,0.190709392081641,
110.634473652374));
#232439=CARTESIAN_POINT('Ctrl Pts',(-7.90401071543908,0.385365611992972,
110.626615796511));
#232440=CARTESIAN_POINT('Ctrl Pts',(-7.88973162020115,0.579703338957264,
110.618757940648));
#232441=CARTESIAN_POINT('Ctrl Pts',(-7.87546640843135,0.773852112658492,
110.610907724926));
#232442=CARTESIAN_POINT('Ctrl Pts',(-7.85401520049234,0.967682664111825,
110.603057509203));
#232443=CARTESIAN_POINT('Ctrl Pts',(-7.82539986755185,1.16061962456248,
110.595207293481));
#232444=CARTESIAN_POINT('Ctrl Pts',(-7.79680686265294,1.35340603969237,
110.587363203143));
#232445=CARTESIAN_POINT('Ctrl Pts',(-7.76106091824334,1.54529990849815,
110.579519112806));
#232446=CARTESIAN_POINT('Ctrl Pts',(-7.71823583503914,1.73572941287452,
110.571675022469));
#232447=CARTESIAN_POINT('Ctrl Pts',(-7.67543594727013,1.92604688117582,
110.563835547074));
#232448=CARTESIAN_POINT('Ctrl Pts',(-7.62556529419268,2.11490136119825,
110.555996071679));
#232449=CARTESIAN_POINT('Ctrl Pts',(-7.56874906919273,2.30172946446671,
110.548156596284));
#232450=CARTESIAN_POINT('Ctrl Pts',(-7.51195536767827,2.4884835040311,110.540320228668));
#232451=CARTESIAN_POINT('Ctrl Pts',(-7.44822168199577,2.67321243338912,
110.532483861052));
#232452=CARTESIAN_POINT('Ctrl Pts',(-7.3777235947799,2.85536609894912,110.524647493437));
#232453=CARTESIAN_POINT('Ctrl Pts',(-7.30722777829498,3.0375138973717,110.516811378229));
#232454=CARTESIAN_POINT('Ctrl Pts',(-7.2299681116985,3.21708626780124,110.508975263022));
#232455=CARTESIAN_POINT('Ctrl Pts',(-7.14616922654664,3.39355070472768,
110.501139147814));
#232456=CARTESIAN_POINT('Ctrl Pts',(-7.06236815198715,3.57001975212819,
110.493302827873));
#232457=CARTESIAN_POINT('Ctrl Pts',(-6.97202766773697,3.74338038774425,
110.485466507932));
#232458=CARTESIAN_POINT('Ctrl Pts',(-6.87541949451138,3.91312250951754,
110.477630187991));
#232459=CARTESIAN_POINT('Ctrl Pts',(-6.77879200126569,4.08289857687842,
110.469792300917));
#232460=CARTESIAN_POINT('Ctrl Pts',(-6.67589449477884,4.24905438453467,
110.461954413843));
#232461=CARTESIAN_POINT('Ctrl Pts',(-6.56704344752397,4.41110659113249,
110.454116526768));
#232462=CARTESIAN_POINT('Ctrl Pts',(-6.45815170657815,4.57321938054122,
110.44627570952));
#232463=CARTESIAN_POINT('Ctrl Pts',(-6.34330218571348,4.73122522240785,
110.438434892271));
#232464=CARTESIAN_POINT('Ctrl Pts',(-6.22285335870696,4.88467164464814,
110.430594075023));
#232465=CARTESIAN_POINT('Ctrl Pts',(-6.10227040815279,5.03828893429358,
110.422744526778));
#232466=CARTESIAN_POINT('Ctrl Pts',(-5.97607591239378,5.18733638688799,
110.414894978533));
#232467=CARTESIAN_POINT('Ctrl Pts',(-5.84466789434017,5.33139552133109,
110.407045430289));
#232468=CARTESIAN_POINT('Ctrl Pts',(-5.71318149038901,5.47554058816038,
110.399191199728));
#232469=CARTESIAN_POINT('Ctrl Pts',(-5.57647561008188,5.61469115706509,
110.391336969167));
#232470=CARTESIAN_POINT('Ctrl Pts',(-5.43498356081272,5.74846716035636,
110.383482738607));
#232471=CARTESIAN_POINT('Ctrl Pts',(-5.29328537013972,5.8824380634548,110.375617065127));
#232472=CARTESIAN_POINT('Ctrl Pts',(-5.14678734116829,6.01101852628486,
110.367751391646));
#232473=CARTESIAN_POINT('Ctrl Pts',(-4.99595517980301,6.13386932053491,
110.359885718166));
#232474=CARTESIAN_POINT('Ctrl Pts',(-4.88124835895589,6.22729650422978,
110.353903927608));
#232475=CARTESIAN_POINT('Ctrl Pts',(-4.76403555096897,6.31741078624118,
110.34792213705));
#232476=CARTESIAN_POINT('Ctrl Pts',(-4.64453177222975,6.40408038806106,
110.341940346492));
#232477=CARTESIAN_POINT('Ctrl Pts',(-4.4894974013035,6.5165183991293,110.334180063545));
#232478=CARTESIAN_POINT('Ctrl Pts',(-4.33010429121461,6.62352136419305,
110.326419780599));
#232479=CARTESIAN_POINT('Ctrl Pts',(-4.16677701121442,6.7247223242908,110.318659497652));
#232480=CARTESIAN_POINT('Ctrl Pts',(-4.0036463037658,6.82580148397071,110.310908554594));
#232481=CARTESIAN_POINT('Ctrl Pts',(-3.83659115209274,6.92109235121469,
110.303157611536));
#232482=CARTESIAN_POINT('Ctrl Pts',(-3.6660692748929,7.01026797431356,110.295406668478));
#232483=CARTESIAN_POINT('Ctrl Pts',(-3.49571801846821,7.09935437006993,
110.287663480859));
#232484=CARTESIAN_POINT('Ctrl Pts',(-3.32190725683863,7.18233753736193,
110.27992029324));
#232485=CARTESIAN_POINT('Ctrl Pts',(-3.1451238635176,7.25893359131575,110.27217710562));
#232486=CARTESIAN_POINT('Ctrl Pts',(-2.96848152687951,7.33546852875237,
110.264440096343));
#232487=CARTESIAN_POINT('Ctrl Pts',(-2.78887160832139,7.40562635746628,
110.256703087066));
#232488=CARTESIAN_POINT('Ctrl Pts',(-2.60680585660291,7.46916891133015,
110.248966077789));
#232489=CARTESIAN_POINT('Ctrl Pts',(-2.42484851485477,7.53267362915778,
110.241233675469));
#232490=CARTESIAN_POINT('Ctrl Pts',(-2.24043858962186,7.58957079784827,
110.233501273148));
#232491=CARTESIAN_POINT('Ctrl Pts',(-2.05410818262262,7.63967018752006,
110.225768870827));
#232492=CARTESIAN_POINT('Ctrl Pts',(-1.86785102663061,7.68974988190532,
110.218039508302));
#232493=CARTESIAN_POINT('Ctrl Pts',(-1.67967523874005,7.733037026691,110.210310145776));
#232494=CARTESIAN_POINT('Ctrl Pts',(-1.49012855330268,7.76939108905145,
110.20258078325));
#232495=CARTESIAN_POINT('Ctrl Pts',(-1.30058194181951,7.80574513722787,
110.19485142374));
#232496=CARTESIAN_POINT('Ctrl Pts',(-1.10966478426686,7.83516602950222,
110.18712206423));
#232497=CARTESIAN_POINT('Ctrl Pts',(-0.917935896002376,7.85756417032851,
110.179392704721));
#232498=CARTESIAN_POINT('Ctrl Pts',(-0.726197397598077,7.87996343382998,
110.171662957787));
#232499=CARTESIAN_POINT('Ctrl Pts',(-0.533647444270986,7.8953392022199,
110.163933210854));
#232500=CARTESIAN_POINT('Ctrl Pts',(-0.340850706672871,7.90365369912932,
110.156203463921));
#232501=CARTESIAN_POINT('Ctrl Pts',(-0.148008977977571,7.91197013631192,
110.148471913172));
#232502=CARTESIAN_POINT('Ctrl Pts',(0.0450792907685641,7.91322200498196,
110.140740362423));
#232503=CARTESIAN_POINT('Ctrl Pts',(0.237848639590673,7.90742366543268,
110.133008811675));
#232504=CARTESIAN_POINT('Ctrl Pts',(0.430698306918309,7.90162290997046,
110.125274039529));
#232505=CARTESIAN_POINT('Ctrl Pts',(0.623228431069579,7.88876610768087,
110.117539267383));
#232506=CARTESIAN_POINT('Ctrl Pts',(0.814877834195721,7.86891956467573,
110.109804495237));
#232507=CARTESIAN_POINT('Ctrl Pts',(1.00675577933338,7.84904935465788,110.102060499371));
#232508=CARTESIAN_POINT('Ctrl Pts',(1.19775054866705,7.82217279439749,110.094316503505));
#232509=CARTESIAN_POINT('Ctrl Pts',(1.38730929452159,7.7884076627597,110.08657250764));
#232510=CARTESIAN_POINT('Ctrl Pts',(1.5769910735121,7.75462061585753,110.078823485532));
#232511=CARTESIAN_POINT('Ctrl Pts',(1.76523462286795,7.71393616716581,110.071074463425));
#232512=CARTESIAN_POINT('Ctrl Pts',(1.95150158229113,7.66652219551442,110.063325441317));
#232513=CARTESIAN_POINT('Ctrl Pts',(2.13805320150523,7.61903576414554,110.055564576879));
#232514=CARTESIAN_POINT('Ctrl Pts',(2.32262185483804,7.56479937075622,110.04780371244));
#232515=CARTESIAN_POINT('Ctrl Pts',(2.50468736810706,7.50402972995476,110.040042848002));
#232516=CARTESIAN_POINT('Ctrl Pts',(2.62989220863503,7.46223898634344,110.034705770282));
#232517=CARTESIAN_POINT('Ctrl Pts',(2.75391369809306,7.41735954922493,110.029368692562));
#232518=CARTESIAN_POINT('Ctrl Pts',(2.87658951799054,7.36947445514176,110.024031614842));
#232519=CARTESIAN_POINT('Ctrl Pts',(3.06079135591703,7.29757338819333,110.016017814519));
#232520=CARTESIAN_POINT('Ctrl Pts',(3.2425232983405,7.21867327368883,110.008004014196));
#232521=CARTESIAN_POINT('Ctrl Pts',(3.42122357856288,7.13296223356646,109.999990213873));
#232522=CARTESIAN_POINT('Ctrl Pts',(3.59972016156027,7.04734889391217,109.991985548336));
#232523=CARTESIAN_POINT('Ctrl Pts',(3.77519166916802,6.95494024196256,109.9839808828));
#232524=CARTESIAN_POINT('Ctrl Pts',(3.9470940922213,6.85597325163625,109.975976217263));
#232525=CARTESIAN_POINT('Ctrl Pts',(4.11882975007928,6.7571022707156,109.967979317176));
#232526=CARTESIAN_POINT('Ctrl Pts',(4.28700293523296,6.65168579631498,109.959982417089));
#232527=CARTESIAN_POINT('Ctrl Pts',(4.4510917630098,6.5400078835783,109.951985517002));
#232528=CARTESIAN_POINT('Ctrl Pts',(4.61504924455739,6.42841936433006,109.943995018098));
#232529=CARTESIAN_POINT('Ctrl Pts',(4.77492860934756,6.31057958338252,109.936004519195));
#232530=CARTESIAN_POINT('Ctrl Pts',(4.93023428250269,6.18681751142178,109.928014020291));
#232531=CARTESIAN_POINT('Ctrl Pts',(5.08544197471628,6.06313351983049,109.920028562521));
#232532=CARTESIAN_POINT('Ctrl Pts',(5.2360814660925,5.93353489277946,109.91204310475));
#232533=CARTESIAN_POINT('Ctrl Pts',(5.38168745955893,5.79839297457719,109.90405764698));
#232534=CARTESIAN_POINT('Ctrl Pts',(5.53206752517141,5.65882007622024,109.895810365155));
#232535=CARTESIAN_POINT('Ctrl Pts',(5.6770781182688,5.51333442269674,109.887563083331));
#232536=CARTESIAN_POINT('Ctrl Pts',(5.8162441027465,5.36238990910457,109.879315801506));
#232537=CARTESIAN_POINT('Ctrl Pts',(5.95090076998973,5.21633636581053,109.871335751723));
#232538=CARTESIAN_POINT('Ctrl Pts',(6.08008541267052,5.06517244672517,109.863355701939));
#232539=CARTESIAN_POINT('Ctrl Pts',(6.2034053625291,4.90934648483332,109.855375652156));
#232540=CARTESIAN_POINT('Ctrl Pts',(6.32671551924724,4.75353289746425,109.847396236088));
#232541=CARTESIAN_POINT('Ctrl Pts',(6.44416170370999,4.59305826745981,109.83941682002));
#232542=CARTESIAN_POINT('Ctrl Pts',(6.5553918727083,4.42840359443783,109.831437403952));
#232543=CARTESIAN_POINT('Ctrl Pts',(6.66663030299142,4.26373669218741,109.823457395237));
#232544=CARTESIAN_POINT('Ctrl Pts',(6.77165161057924,4.09488940555458,109.815477386521));
#232545=CARTESIAN_POINT('Ctrl Pts',(6.87014717706925,3.92237157411271,109.807497377806));
#232546=CARTESIAN_POINT('Ctrl Pts',(6.96866519646812,3.74981441575203,109.79951554998));
#232547=CARTESIAN_POINT('Ctrl Pts',(7.06065434426004,3.57358533551647,109.791533722153));
#232548=CARTESIAN_POINT('Ctrl Pts',(7.14585185770023,3.39421894223136,109.783551894327));
#232549=CARTESIAN_POINT('Ctrl Pts',(7.23111271932207,3.2147191819687,109.775564131652));
#232550=CARTESIAN_POINT('Ctrl Pts',(7.30957171547397,3.03207775126201,109.767576368978));
#232551=CARTESIAN_POINT('Ctrl Pts',(7.38101375529517,2.84685035506672,109.759588606303));
#232552=CARTESIAN_POINT('Ctrl Pts',(7.45248726073062,2.66154137814094,109.751597325534));
#232553=CARTESIAN_POINT('Ctrl Pts',(7.51693753527625,2.47364447953964,109.743606044765));
#232554=CARTESIAN_POINT('Ctrl Pts',(7.57419913373819,2.28373126319181,109.735614763996));
#232555=CARTESIAN_POINT('Ctrl Pts',(7.6315146077514,2.09363936375619,109.727615964495));
#232556=CARTESIAN_POINT('Ctrl Pts',(7.68162780970203,1.90152768005897,109.719617164993));
#232557=CARTESIAN_POINT('Ctrl Pts',(7.72442400785416,1.70797972671993,109.711618365491));
#232558=CARTESIAN_POINT('Ctrl Pts',(7.73422488482039,1.66365476890481,109.709786538058));
#232559=CARTESIAN_POINT('Ctrl Pts',(7.74364222166496,1.61925451409568,109.707954710625));
#232560=CARTESIAN_POINT('Ctrl Pts',(7.75267502192603,1.57478601860831,109.706122883193));
#232561=CARTESIAN_POINT('Ctrl Pts',(7.79274781062006,1.37750759201822,109.697996230159));
#232562=CARTESIAN_POINT('Ctrl Pts',(7.82531900144262,1.17853770587763,109.689869577126));
#232563=CARTESIAN_POINT('Ctrl Pts',(7.850255474966,0.978473289245222,109.681742924093));
#232564=CARTESIAN_POINT('Ctrl Pts',(7.87517072144489,0.778579176415713,
109.673623188832));
#232565=CARTESIAN_POINT('Ctrl Pts',(7.89246416802303,0.577592705525485,
109.66550345357));
#232566=CARTESIAN_POINT('Ctrl Pts',(7.90205380306755,0.376120583624052,
109.657383718309));
#232567=CARTESIAN_POINT('Ctrl Pts',(7.91163648259541,0.174794592695505,
109.649269872422));
#232568=CARTESIAN_POINT('Ctrl Pts',(7.913526476612,-0.0270160294569833,
109.641156026535));
#232569=CARTESIAN_POINT('Ctrl Pts',(7.90769357227617,-0.228699293794433,
109.633042180648));
#232570=CARTESIAN_POINT('Ctrl Pts',(7.90186481243599,-0.430239254665368,
109.624934099951));
#232571=CARTESIAN_POINT('Ctrl Pts',(7.88832411098061,-0.631651720315048,
109.616826019253));
#232572=CARTESIAN_POINT('Ctrl Pts',(7.86709333146714,-0.832324164004231,
109.608717938556));
#232573=CARTESIAN_POINT('Ctrl Pts',(7.84587167068052,-1.03291041786692,
109.60061334032));
#232574=CARTESIAN_POINT('Ctrl Pts',(7.81696655103517,-1.23275696702579,
109.592508742084));
#232575=CARTESIAN_POINT('Ctrl Pts',(7.7804517929624,-1.43125500781244,109.584404143848));
#232576=CARTESIAN_POINT('Ctrl Pts',(7.74394844833724,-1.62969100390513,
109.576302078873));
#232577=CARTESIAN_POINT('Ctrl Pts',(7.69984026663045,-1.82677901903057,
109.568200013898));
#232578=CARTESIAN_POINT('Ctrl Pts',(7.64825251602038,-2.02191850755365,
109.560097948923));
#232579=CARTESIAN_POINT('Ctrl Pts',(7.62081094021264,-2.12572096073413,
109.555788138405));
#232580=CARTESIAN_POINT('Ctrl Pts',(7.59125381393921,-2.22897221777876,
109.551478327886));
#232581=CARTESIAN_POINT('Ctrl Pts',(7.55960584956201,-2.33158323876029,
109.547168517368));
#232582=CARTESIAN_POINT('Ctrl Pts',(7.49873986594993,-2.52892675972239,
109.538879805548));
#232583=CARTESIAN_POINT('Ctrl Pts',(7.43016362405021,-2.7238163790082,109.530591093729));
#232584=CARTESIAN_POINT('Ctrl Pts',(7.35410670943434,-2.91565352987162,
109.522302381909));
#232585=CARTESIAN_POINT('Ctrl Pts',(7.27800594875135,-3.10760127297554,
109.514008891728));
#232586=CARTESIAN_POINT('Ctrl Pts',(7.19441601513077,-3.29649276321163,
109.505715401548));
#232587=CARTESIAN_POINT('Ctrl Pts',(7.10361425212357,-3.48175035822888,
109.497421911367));
#232588=CARTESIAN_POINT('Ctrl Pts',(7.01275466831162,-3.66712592169601,
109.489123140052));
#232589=CARTESIAN_POINT('Ctrl Pts',(6.91467421693953,-3.84886270843043,
109.480824368738));
#232590=CARTESIAN_POINT('Ctrl Pts',(6.80969610124708,-4.02640782940083,
109.472525597423));
#232591=CARTESIAN_POINT('Ctrl Pts',(6.70459578496858,-4.20415962314003,
109.464217165859));
#232592=CARTESIAN_POINT('Ctrl Pts',(6.59258190387364,-4.37770974581563,
109.455908734296));
#232593=CARTESIAN_POINT('Ctrl Pts',(6.47402183737178,-4.54653299220772,
109.447600302732));
#232594=CARTESIAN_POINT('Ctrl Pts',(6.35538863498052,-4.71546038022727,
109.439286745965));
#232595=CARTESIAN_POINT('Ctrl Pts',(6.23020135995381,-4.87965483613162,
109.430973189197));
#232596=CARTESIAN_POINT('Ctrl Pts',(6.09886844428007,-5.03862329405213,
109.422659632429));
#232597=CARTESIAN_POINT('Ctrl Pts',(5.96739194339273,-5.19776555090089,
109.414336986518));
#232598=CARTESIAN_POINT('Ctrl Pts',(5.82975656395019,-5.35167016876399,
109.406014340606));
#232599=CARTESIAN_POINT('Ctrl Pts',(5.68640953515548,-5.49987887125642,
109.397691694694));
#232600=CARTESIAN_POINT('Ctrl Pts',(5.63199664509901,-5.55613719695694,
109.394532513643));
#232601=CARTESIAN_POINT('Ctrl Pts',(5.57676114622288,-5.6115752026096,109.391373332593));
#232602=CARTESIAN_POINT('Ctrl Pts',(5.52072881163614,-5.66616928694957,
109.388214151543));
#232603=CARTESIAN_POINT('Ctrl Pts',(5.36645418003875,-5.81648396348526,
109.379515932983));
#232604=CARTESIAN_POINT('Ctrl Pts',(5.20599955280938,-5.96053179738248,
109.370817714422));
#232605=CARTESIAN_POINT('Ctrl Pts',(5.03987436346788,-6.09783464850099,
109.362119495862));
#232606=CARTESIAN_POINT('Ctrl Pts',(4.87389513737398,-6.23501686065962,
109.353428919853));
#232607=CARTESIAN_POINT('Ctrl Pts',(4.70225547390781,-6.36546577795881,
109.344738343843));
#232608=CARTESIAN_POINT('Ctrl Pts',(4.5254988093669,-6.48874267685341,109.336047767834));
#232609=CARTESIAN_POINT('Ctrl Pts',(4.34450306263844,-6.61497607477224,
109.327148769324));
#232610=CARTESIAN_POINT('Ctrl Pts',(4.15814197773161,-6.73368897836446,
109.318249770815));
#232611=CARTESIAN_POINT('Ctrl Pts',(3.96703473234633,-6.8444544291242,109.309350772305));
#232612=CARTESIAN_POINT('Ctrl Pts',(3.78095329529558,-6.95230692949065,
109.300685802918));
#232613=CARTESIAN_POINT('Ctrl Pts',(3.5903723669843,-7.05262452970903,109.29202083353));
#232614=CARTESIAN_POINT('Ctrl Pts',(3.39589382667509,-7.14505606121814,
109.283355864143));
#232615=CARTESIAN_POINT('Ctrl Pts',(3.19353638223454,-7.24123226900009,
109.274339851072));
#232616=CARTESIAN_POINT('Ctrl Pts',(2.98695913189684,-7.3288699941815,109.265323838002));
#232617=CARTESIAN_POINT('Ctrl Pts',(2.77687127159029,-7.40762491902881,
109.256307824931));
#232618=CARTESIAN_POINT('Ctrl Pts',(2.56678341128373,-7.48637984387611,
109.24729181186));
#232619=CARTESIAN_POINT('Ctrl Pts',(2.35318517926726,-7.55625180730581,
109.23827579879));
#232620=CARTESIAN_POINT('Ctrl Pts',(2.13681410900544,-7.61695125779044,
109.229259785719));
#232621=CARTESIAN_POINT('Ctrl Pts',(1.94937499274639,-7.66953431033291,
109.221449344517));
#232622=CARTESIAN_POINT('Ctrl Pts',(1.7599356938672,-7.71521066824004,109.213638903314));
#232623=CARTESIAN_POINT('Ctrl Pts',(1.56905280285073,-7.75383739201863,
109.205828462112));
#232624=CARTESIAN_POINT('Ctrl Pts',(1.37818367410655,-7.79246133088818,
109.198018584027));
#232625=CARTESIAN_POINT('Ctrl Pts',(1.18587150571842,-7.82403657819675,
109.190208705942));
#232626=CARTESIAN_POINT('Ctrl Pts',(0.992683632893948,-7.84847120176818,
109.182398827856));
#232627=CARTESIAN_POINT('Ctrl Pts',(0.799475589824402,-7.87290837649533,
109.174588134362));
#232628=CARTESIAN_POINT('Ctrl Pts',(0.605392009711438,-7.89020339912728,
109.166777440868));
#232629=CARTESIAN_POINT('Ctrl Pts',(0.411006059568197,-7.90031613411756,
109.158966747373));
#232630=CARTESIAN_POINT('Ctrl Pts',(0.216482162341099,-7.91043604566716,
109.151150510976));
#232631=CARTESIAN_POINT('Ctrl Pts',(0.0216558185147771,-7.91336346825997,
109.14333427458));
#232632=CARTESIAN_POINT('Ctrl Pts',(-0.172898201283247,-7.90911039321067,
109.135518038183));
#232633=CARTESIAN_POINT('Ctrl Pts',(-0.367524150519129,-7.90485574573795,
109.12769891201));
#232634=CARTESIAN_POINT('Ctrl Pts',(-0.561877223508443,-7.89341532807992,
109.119879785837));
#232635=CARTESIAN_POINT('Ctrl Pts',(-0.755386913642639,-7.8748531167697,
109.112060659664));
#232636=CARTESIAN_POINT('Ctrl Pts',(-0.949111780877585,-7.85627026482484,
109.104232838853));
#232637=CARTESIAN_POINT('Ctrl Pts',(-1.14199104230984,-7.83054984194879,
109.096405018041));
#232638=CARTESIAN_POINT('Ctrl Pts',(-1.33346243683517,-7.79780731549258,
109.088577197229));
#232639=CARTESIAN_POINT('Ctrl Pts',(-1.48244058248134,-7.77233133832476,
109.082486604784));
#232640=CARTESIAN_POINT('Ctrl Pts',(-1.63056657031458,-7.74260527241938,
109.076396012339));
#232641=CARTESIAN_POINT('Ctrl Pts',(-1.777581798872,-7.70870442735477,109.070305419894));
#232642=CARTESIAN_POINT('Ctrl Pts',(-1.973510115189,-7.66352451259077,109.062188440892));
#232643=CARTESIAN_POINT('Ctrl Pts',(-2.16785460434176,-7.61083846189063,
109.05407146189));
#232644=CARTESIAN_POINT('Ctrl Pts',(-2.36001930486389,-7.55077677333066,
109.045954482888));
#232645=CARTESIAN_POINT('Ctrl Pts',(-2.55204344357749,-7.49075901781118,
109.037843441174));
#232646=CARTESIAN_POINT('Ctrl Pts',(-2.74189066777205,-7.42337647672191,
109.029732399461));
#232647=CARTESIAN_POINT('Ctrl Pts',(-2.92897782586889,-7.3488101006604,
109.021621357747));
#232648=CARTESIAN_POINT('Ctrl Pts',(-3.11595473668627,-7.27428766529575,
109.013515095732));
#232649=CARTESIAN_POINT('Ctrl Pts',(-3.30017452750284,-7.19258995484459,
109.005408833718));
#232650=CARTESIAN_POINT('Ctrl Pts',(-3.48107121657821,-7.10394708490363,
108.997302571703));
#232651=CARTESIAN_POINT('Ctrl Pts',(-3.66188699913664,-7.0153438607179,
108.989199935235));
#232652=CARTESIAN_POINT('Ctrl Pts',(-3.83938235646557,-6.91980181257971,
108.981097298767));
#232653=CARTESIAN_POINT('Ctrl Pts',(-4.01301270567199,-6.81759855257811,
108.9729946623));
#232654=CARTESIAN_POINT('Ctrl Pts',(-4.18659003868377,-6.71542649926331,
108.964894499886));
#232655=CARTESIAN_POINT('Ctrl Pts',(-4.35630444132098,-6.6065974533241,
108.956794337473));
#232656=CARTESIAN_POINT('Ctrl Pts',(-4.52163679432532,-6.4914344870917,
108.94869417506));
#232657=CARTESIAN_POINT('Ctrl Pts',(-4.68857956518314,-6.37514977733172,
108.940515113109));
#232658=CARTESIAN_POINT('Ctrl Pts',(-4.85105417908357,-6.25240726675152,
108.932336051159));
#232659=CARTESIAN_POINT('Ctrl Pts',(-5.00855630989213,-6.12358430093354,
108.924156989208));
#232660=CARTESIAN_POINT('Ctrl Pts',(-5.16453823650683,-5.99600472916932,
108.916056871232));
#232661=CARTESIAN_POINT('Ctrl Pts',(-5.31564300692924,-5.86246178414278,
108.907956753257));
#232662=CARTESIAN_POINT('Ctrl Pts',(-5.46141390999176,-5.7233625696568,
108.899856635281));
#232663=CARTESIAN_POINT('Ctrl Pts',(-5.60720443125477,-5.58424463486231,
108.891755427172));
#232664=CARTESIAN_POINT('Ctrl Pts',(-5.74765942142636,-5.43956916075739,
108.883654219063));
#232665=CARTESIAN_POINT('Ctrl Pts',(-5.8823585729667,-5.28978058326101,
108.875553010954));
#232666=CARTESIAN_POINT('Ctrl Pts',(-6.01709324894237,-5.13995250176944,
108.867449666299));
#232667=CARTESIAN_POINT('Ctrl Pts',(-6.14606884454124,-4.98500886612771,
108.859346321645));
#232668=CARTESIAN_POINT('Ctrl Pts',(-6.26890457849071,-4.82542810388656,
108.851242976991));
#232669=CARTESIAN_POINT('Ctrl Pts',(-6.39376923771602,-4.66321148454064,
108.843005786262));
#232670=CARTESIAN_POINT('Ctrl Pts',(-6.51228922049973,-4.49620348422213,
108.834768595533));
#232671=CARTESIAN_POINT('Ctrl Pts',(-6.62410982722081,-4.32493814949031,
108.826531404804));
#232672=CARTESIAN_POINT('Ctrl Pts',(-6.73425670955243,-4.1562363044069,
108.818417507871));
#232673=CARTESIAN_POINT('Ctrl Pts',(-6.83790322830827,-3.9834039747118,
108.810303610938));
#232674=CARTESIAN_POINT('Ctrl Pts',(-6.93475617044715,-3.80697752245075,
108.802189714004));
#232675=CARTESIAN_POINT('Ctrl Pts',(-7.03381668934199,-3.6265297681358,
108.793890876378));
#232676=CARTESIAN_POINT('Ctrl Pts',(-7.12577008698123,-3.44232241763237,
108.785592038751));
#232677=CARTESIAN_POINT('Ctrl Pts',(-7.21035405914674,-3.25495243310038,
108.777293201124));
#232678=CARTESIAN_POINT('Ctrl Pts',(-7.2949380313122,-3.06758244856853,
108.768994363498));
#232679=CARTESIAN_POINT('Ctrl Pts',(-7.37215247684972,-2.87705017327477,
108.760695525871));
#232680=CARTESIAN_POINT('Ctrl Pts',(-7.44178885452139,-2.68397087255454,
108.752396688245));
#232681=CARTESIAN_POINT('Ctrl Pts',(-7.51210891726181,-2.48899593281056,
108.744016373213));
#232682=CARTESIAN_POINT('Ctrl Pts',(-7.57483708588991,-2.29104890570404,
108.735636058181));
#232683=CARTESIAN_POINT('Ctrl Pts',(-7.62972938591883,-2.09072965675782,
108.727255743149));
#232684=CARTESIAN_POINT('Ctrl Pts',(-7.6844870541156,-1.89090172166594,
108.718895982132));
#232685=CARTESIAN_POINT('Ctrl Pts',(-7.73144712293042,-1.68871344245385,
108.710536221115));
#232686=CARTESIAN_POINT('Ctrl Pts',(-7.77041471610678,-1.48478151244931,
108.702176460098));
#232687=CARTESIAN_POINT('Ctrl Pts',(-7.80932420579393,-1.28115365964657,
108.693829164087));
#232688=CARTESIAN_POINT('Ctrl Pts',(-7.84026492959831,-1.07578761402196,
108.685481868076));
#232689=CARTESIAN_POINT('Ctrl Pts',(-7.86309182568463,-0.86931463858117,
108.677134572065));
#232690=CARTESIAN_POINT('Ctrl Pts',(-7.88587227225744,-0.663261806519804,
108.668804261624));
#232691=CARTESIAN_POINT('Ctrl Pts',(-7.90057179809203,-0.456106816128255,
108.660473951183));
#232692=CARTESIAN_POINT('Ctrl Pts',(-7.90709640401639,-0.248490357139009,
108.652143640742));
#232693=CARTESIAN_POINT('Ctrl Pts',(-7.90965814519557,-0.166974379218875,
108.648872929907));
#232694=CARTESIAN_POINT('Ctrl Pts',(-7.91096022151875,-0.0853873852617121,
108.645602219072));
#232695=CARTESIAN_POINT('Ctrl Pts',(-7.91099910237999,-0.00376857307924841,
108.642331508237));
#232696=CARTESIAN_POINT('',(-7.9109999968991,0.000221500451111772,104.648002515785));
#232697=CARTESIAN_POINT('Ctrl Pts',(-7.91099992240033,-0.00110805323541054,
108.640263793438));
#232698=CARTESIAN_POINT('Ctrl Pts',(-7.91103873502507,0.275996567276769,
108.628470434012));
#232699=CARTESIAN_POINT('Ctrl Pts',(-7.89651817900392,0.552923481285257,
108.616947714325));
#232700=CARTESIAN_POINT('Ctrl Pts',(-7.86419060080753,0.859896389659774,
108.604418225675));
#232701=CARTESIAN_POINT('Ctrl Pts',(-7.86070010247159,0.891240440873543,
108.603141580458));
#232702=CARTESIAN_POINT('Ctrl Pts',(-7.85483141328906,0.941221228490136,
108.601109894987));
#232703=CARTESIAN_POINT('Ctrl Pts',(-7.8525741142427,0.959871718574376,
108.600352662609));
#232704=CARTESIAN_POINT('Ctrl Pts',(-7.84858713101809,0.991857786608685,
108.599055460503));
#232705=CARTESIAN_POINT('Ctrl Pts',(-7.8468898438213,1.00519729520292,108.598514913088));
#232706=CARTESIAN_POINT('Ctrl Pts',(-7.84363450499322,1.03027126275294,
108.597499655182));
#232707=CARTESIAN_POINT('Ctrl Pts',(-7.84208411189063,1.042006672573,108.597024810785));
#232708=CARTESIAN_POINT('Ctrl Pts',(-7.83879483978766,1.06648101827162,
108.596035178665));
#232709=CARTESIAN_POINT('Ctrl Pts',(-7.83705123336003,1.07921928699073,
108.595520474955));
#232710=CARTESIAN_POINT('Ctrl Pts',(-7.8329608358385,1.10856980663129,108.594335363788));
#232711=CARTESIAN_POINT('Ctrl Pts',(-7.83059223562941,1.12517896961357,
108.593665333842));
#232712=CARTESIAN_POINT('Ctrl Pts',(-7.82287099903963,1.17811660385707,
108.591531620703));
#232713=CARTESIAN_POINT('Ctrl Pts',(-7.81731822947769,1.21441554684441,
108.590071294421));
#232714=CARTESIAN_POINT('Ctrl Pts',(-7.77186678921918,1.49829794897225,
108.578669750233));
#232715=CARTESIAN_POINT('Ctrl Pts',(-7.72046783173518,1.74390193891802,
108.56892819052));
#232716=CARTESIAN_POINT('Ctrl Pts',(-7.63974451673771,2.05504663766676,
108.556670802049));
#232717=CARTESIAN_POINT('Ctrl Pts',(-7.6210859948363,2.12319602660876,108.553990904865));
#232718=CARTESIAN_POINT('Ctrl Pts',(-7.427318355995,2.79543227659978,108.527580834253));
#232719=CARTESIAN_POINT('Ctrl Pts',(-7.18168134098618,3.37681864169952,
108.505142366302));
#232720=CARTESIAN_POINT('Ctrl Pts',(-6.79114594000115,4.06071716895559,
108.475448713363));
#232721=CARTESIAN_POINT('Ctrl Pts',(-6.70835558352547,4.19607549754085,
108.469381483872));
#232722=CARTESIAN_POINT('Ctrl Pts',(-6.58149380023279,4.39012759383339,
108.460298291023));
#232723=CARTESIAN_POINT('Ctrl Pts',(-6.54058491359736,4.450845933314,108.45739888142));
#232724=CARTESIAN_POINT('Ctrl Pts',(-6.49130915152878,4.52183601243383,
108.453932159361));
#232725=CARTESIAN_POINT('Ctrl Pts',(-6.48375118393902,4.53266654478494,
108.4534011235));
#232726=CARTESIAN_POINT('Ctrl Pts',(-6.47211043316828,4.54925899559632,
108.452584218525));
#232727=CARTESIAN_POINT('Ctrl Pts',(-6.46804697642293,4.55503448708368,
108.452299244677));
#232728=CARTESIAN_POINT('Ctrl Pts',(-6.46094003579209,4.56510707231958,
108.451801138602));
#232729=CARTESIAN_POINT('Ctrl Pts',(-6.45789998108347,4.56940658751058,
108.451588168021));
#232730=CARTESIAN_POINT('Ctrl Pts',(-6.45104300225777,4.57908382450968,
108.451108018865));
#232731=CARTESIAN_POINT('Ctrl Pts',(-6.44722364479174,4.5844598114236,108.450840724202));
#232732=CARTESIAN_POINT('Ctrl Pts',(-6.43696948745215,4.59885502825793,
108.450123481599));
#232733=CARTESIAN_POINT('Ctrl Pts',(-6.43052246923753,4.60786550631417,
108.449672941324));
#232734=CARTESIAN_POINT('Ctrl Pts',(-6.40251233371481,4.64683974470204,
108.447717137723));
#232735=CARTESIAN_POINT('Ctrl Pts',(-6.38075879291021,4.6766655810871,108.446202399004));
#232736=CARTESIAN_POINT('Ctrl Pts',(-6.04550344391281,5.12963369117308,
108.422906836292));
#232737=CARTESIAN_POINT('Ctrl Pts',(-5.69078527475396,5.52050764703951,
108.398612357703));
#232738=CARTESIAN_POINT('Ctrl Pts',(-5.20377896721509,5.95998249015012,
108.368410768895));
#232739=CARTESIAN_POINT('Ctrl Pts',(-5.10547413383884,6.04440577611858,
108.362450626835));
#232740=CARTESIAN_POINT('Ctrl Pts',(-4.90816870987172,6.20560074887935,
108.350797086165));
#232741=CARTESIAN_POINT('Ctrl Pts',(-4.80932894074798,6.28251199023904,
108.345103034362));
#232742=CARTESIAN_POINT('Ctrl Pts',(-4.35446348790882,6.61943367019816,
108.319612266744));
#232743=CARTESIAN_POINT('Ctrl Pts',(-3.97888238939687,6.85177580012234,
108.30054629876));
#232744=CARTESIAN_POINT('Ctrl Pts',(-3.56737078471907,7.06103509720357,
108.28186461619));
#232745=CARTESIAN_POINT('Ctrl Pts',(-3.54885081543075,7.07036129615967,
108.281028164409));
#232746=CARTESIAN_POINT('Ctrl Pts',(-3.52192312336513,7.08378895893593,
108.279818197952));
#232747=CARTESIAN_POINT('Ctrl Pts',(-3.5135445339305,7.08794845569086,108.279442585562));
#232748=CARTESIAN_POINT('Ctrl Pts',(-3.49889094563807,7.09519076764042,
108.278787181001));
#232749=CARTESIAN_POINT('Ctrl Pts',(-3.49261920997549,7.09828013909828,
108.278507152115));
#232750=CARTESIAN_POINT('Ctrl Pts',(-3.48048088232119,7.10423933157402,
108.277966118088));
#232751=CARTESIAN_POINT('Ctrl Pts',(-3.47461481772515,7.10711020888153,
108.277705074956));
#232752=CARTESIAN_POINT('Ctrl Pts',(-3.4606775910403,7.11390976810636,108.277085858546));
#232753=CARTESIAN_POINT('Ctrl Pts',(-3.4526032752741,7.11783198749361,108.276727918619));
#232754=CARTESIAN_POINT('Ctrl Pts',(-3.42410351819002,7.13161626520489,
108.275467293829));
#232755=CARTESIAN_POINT('Ctrl Pts',(-3.40364226453461,7.14140425993823,
108.274567279731));
#232756=CARTESIAN_POINT('Ctrl Pts',(-3.14118878751259,7.2655692271866,108.263086904772));
#232757=CARTESIAN_POINT('Ctrl Pts',(-2.89357510000623,7.36768639682128,
108.252958957398));
#232758=CARTESIAN_POINT('Ctrl Pts',(-2.57932830896192,7.47899063788279,
108.240813946756));
#232759=CARTESIAN_POINT('Ctrl Pts',(-2.51714118479853,7.50014906161037,
108.238443646858));
#232760=CARTESIAN_POINT('Ctrl Pts',(-2.19799388570766,7.60431855984757,
108.226433759326));
#232761=CARTESIAN_POINT('Ctrl Pts',(-1.93716269534709,7.67491023532557,
108.21713528707));
#232762=CARTESIAN_POINT('Ctrl Pts',(-1.38764946739131,7.79382591865973,
108.198080457563));
#232763=CARTESIAN_POINT('Ctrl Pts',(-1.09887246608668,7.83975578017106,
108.188363963765));
#232764=CARTESIAN_POINT('Ctrl Pts',(-0.700385917824278,7.88068088575683,
108.174758441005));
#232765=CARTESIAN_POINT('Ctrl Pts',(-0.592337749857318,7.88953782200925,
108.171048541025));
#232766=CARTESIAN_POINT('Ctrl Pts',(-0.314452245628844,7.90657600209386,
108.161387492466));
#232767=CARTESIAN_POINT('Ctrl Pts',(-0.144475853018282,7.91150723820138,
108.155363818877));
#232768=CARTESIAN_POINT('Ctrl Pts',(0.187106768751399,7.91043756433375,
108.143183952302));
#232769=CARTESIAN_POINT('Ctrl Pts',(0.348630174924865,7.90496568590167,
108.137051732549));
#232770=CARTESIAN_POINT('Ctrl Pts',(0.534418261830269,7.89296671673951,
108.129659991877));
#232771=CARTESIAN_POINT('Ctrl Pts',(0.558965607863358,7.8912663047917,108.12867653007));
#232772=CARTESIAN_POINT('Ctrl Pts',(0.590338561631365,7.88894595903172,
108.127410452302));
#232773=CARTESIAN_POINT('Ctrl Pts',(0.597172087466627,7.88843162227037,
108.127134124868));
#232774=CARTESIAN_POINT('Ctrl Pts',(0.608136860096736,7.88759201103033,
108.126689838761));
#232775=CARTESIAN_POINT('Ctrl Pts',(0.612268548044961,7.88727236742977,
108.126522219328));
#232776=CARTESIAN_POINT('Ctrl Pts',(0.620106816447516,7.88665977209606,
108.126203833095));
#232777=CARTESIAN_POINT('Ctrl Pts',(0.62381344674858,7.88636745328055,108.126053104729));
#232778=CARTESIAN_POINT('Ctrl Pts',(0.632225982206083,7.8856980410878,108.125710631178));
#232779=CARTESIAN_POINT('Ctrl Pts',(0.636931727599009,7.88531935067549,
108.125518789118));
#232780=CARTESIAN_POINT('Ctrl Pts',(0.649162501104753,7.88432407076801,
108.12501946115));
#232781=CARTESIAN_POINT('Ctrl Pts',(0.656686931967718,7.88370092521737,
108.124711576769));
#232782=CARTESIAN_POINT('Ctrl Pts',(0.703284094136714,7.87977474760893,
108.12280066378));
#232783=CARTESIAN_POINT('Ctrl Pts',(0.742332056170847,7.87619207484784,
108.121180818793));
#232784=CARTESIAN_POINT('Ctrl Pts',(1.41346791099696,7.80957984843392,108.093042480294));
#232785=CARTESIAN_POINT('Ctrl Pts',(2.03569442888879,7.67093968598267,108.062612667835));
#232786=CARTESIAN_POINT('Ctrl Pts',(2.96431042009534,7.34295900447116,108.016850928095));
#232787=CARTESIAN_POINT('Ctrl Pts',(3.28594820497965,7.20477357306866,108.000888183592));
#232788=CARTESIAN_POINT('Ctrl Pts',(3.76235179774446,6.96153204860795,107.977525606507));
#232789=CARTESIAN_POINT('Ctrl Pts',(3.92429314252192,6.871546360986,107.969631878361));
#232790=CARTESIAN_POINT('Ctrl Pts',(4.1608200758466,6.7290241366952,107.958185208574));
#232791=CARTESIAN_POINT('Ctrl Pts',(4.2378917494425,6.68075323887232,107.954468582145));
#232792=CARTESIAN_POINT('Ctrl Pts',(4.32703034228173,6.6227612661145,107.95018390057));
#232793=CARTESIAN_POINT('Ctrl Pts',(4.33992015838255,6.61432168809432,107.949564657672));
#232794=CARTESIAN_POINT('Ctrl Pts',(4.35953318542118,6.60139808750223,107.948622924706));
#232795=CARTESIAN_POINT('Ctrl Pts',(4.36627427855076,6.59694135410258,107.948299337124));
#232796=CARTESIAN_POINT('Ctrl Pts',(4.37797530973959,6.5891796690172,107.947737815821));
#232797=CARTESIAN_POINT('Ctrl Pts',(4.38293835716385,6.58587943108554,107.94749969231));
#232798=CARTESIAN_POINT('Ctrl Pts',(4.3932653591498,6.57899552352798,107.947004309274));
#232799=CARTESIAN_POINT('Ctrl Pts',(4.39862867085935,6.57541089443683,107.946747088763));
#232800=CARTESIAN_POINT('Ctrl Pts',(4.41333821012827,6.56555355940951,107.946041780672));
#232801=CARTESIAN_POINT('Ctrl Pts',(4.42267546161771,6.55926744851141,107.94559423582));
#232802=CARTESIAN_POINT('Ctrl Pts',(4.45853858813226,6.53501194915719,107.943875898615));
#232803=CARTESIAN_POINT('Ctrl Pts',(4.48496880332076,6.51690128693292,107.942610842156));
#232804=CARTESIAN_POINT('Ctrl Pts',(4.89793005599667,6.23022744570043,107.922863249005));
#232805=CARTESIAN_POINT('Ctrl Pts',(5.25986804256149,5.92784147446614,107.905896997823));
#232806=CARTESIAN_POINT('Ctrl Pts',(5.88870573742271,5.29925640496127,107.875153710368));
#232807=CARTESIAN_POINT('Ctrl Pts',(6.16067256109226,4.98046914351487,107.861257713819));
#232808=CARTESIAN_POINT('Ctrl Pts',(6.5041830885523,4.50637771722822,107.840893692222));
#232809=CARTESIAN_POINT('Ctrl Pts',(6.59790289879245,4.36801000032904,107.834976730553));
#232810=CARTESIAN_POINT('Ctrl Pts',(6.77360042566366,4.09004006785996,107.822931937608));
#232811=CARTESIAN_POINT('Ctrl Pts',(6.85581345453315,3.95068431762628,107.816819418618));
#232812=CARTESIAN_POINT('Ctrl Pts',(6.94897101629516,3.78110166830769,107.809172012608));
#232813=CARTESIAN_POINT('Ctrl Pts',(6.96408210029957,3.75319710018941,107.807907019386));
#232814=CARTESIAN_POINT('Ctrl Pts',(6.98259895475755,3.7185064811697,107.806325246385));
#232815=CARTESIAN_POINT('Ctrl Pts',(6.98616351772885,3.71180520990043,107.806019272557));
#232816=CARTESIAN_POINT('Ctrl Pts',(6.99179952197368,3.7011728126672,107.805533156125));
#232817=CARTESIAN_POINT('Ctrl Pts',(6.99387731307706,3.69724503842611,107.805353436468));
#232818=CARTESIAN_POINT('Ctrl Pts',(6.99777107736904,3.68986939258878,107.805015694776));
#232819=CARTESIAN_POINT('Ctrl Pts',(6.99958781534629,3.6864219238682,107.804857723265));
#232820=CARTESIAN_POINT('Ctrl Pts',(7.00364775616464,3.67870389909681,107.804503827751));
#232821=CARTESIAN_POINT('Ctrl Pts',(7.0058896000552,3.67443263393524,107.804307814972));
#232822=CARTESIAN_POINT('Ctrl Pts',(7.01154737807487,3.6636291711,107.803811628789));
#232823=CARTESIAN_POINT('Ctrl Pts',(7.0149580844537,3.65709425787,107.803511117356));
#232824=CARTESIAN_POINT('Ctrl Pts',(7.03325238932924,3.62192261280943,107.801891764651));
#232825=CARTESIAN_POINT('Ctrl Pts',(7.04796958381711,3.59320014377403,107.800562339287));
#232826=CARTESIAN_POINT('Ctrl Pts',(7.12749364942584,3.43563048217298,107.793234334793));
#232827=CARTESIAN_POINT('Ctrl Pts',(7.18894028813037,3.30512567014109,107.787038317953));
#232828=CARTESIAN_POINT('Ctrl Pts',(7.4183074295358,2.78127997775518,107.76188067631));
#232829=CARTESIAN_POINT('Ctrl Pts',(7.55777777231555,2.37629257217556,107.741836642829));
#232830=CARTESIAN_POINT('Ctrl Pts',(7.77977682550361,1.50915383640564,107.70008038683));
#232831=CARTESIAN_POINT('Ctrl Pts',(7.85535940108023,1.0468406587608,107.678493895438));
#232832=CARTESIAN_POINT('Ctrl Pts',(7.90997527459674,0.304581900445095,
107.646009680833));
#232833=CARTESIAN_POINT('Ctrl Pts',(7.91578989370547,0.0277468338463155,
107.634351180613));
#232834=CARTESIAN_POINT('Ctrl Pts',(7.9064400872044,-0.269345212587889,
107.622317401591));
#232835=CARTESIAN_POINT('Ctrl Pts',(7.90571517811777,-0.289843452246066,
107.621489507664));
#232836=CARTESIAN_POINT('Ctrl Pts',(7.90453573154146,-0.319886171443628,
107.620279588133));
#232837=CARTESIAN_POINT('Ctrl Pts',(7.90414361179751,-0.329432935214876,
107.619895620958));
#232838=CARTESIAN_POINT('Ctrl Pts',(7.90342273555931,-0.346241098539175,
107.619220499723));
#232839=CARTESIAN_POINT('Ctrl Pts',(7.90310126553972,-0.353502789597305,
107.618929119408));
#232840=CARTESIAN_POINT('Ctrl Pts',(7.90245581468323,-0.367641808360402,
107.618362352575));
#232841=CARTESIAN_POINT('Ctrl Pts',(7.90213286333426,-0.374519175480841,
107.618086934321));
#232842=CARTESIAN_POINT('Ctrl Pts',(7.90124490809039,-0.392915916150992,
107.617350899372));
#232843=CARTESIAN_POINT('Ctrl Pts',(7.90066369005516,-0.40443450998918,
107.616890786659));
#232844=CARTESIAN_POINT('Ctrl Pts',(7.89847412950154,-0.446020224598346,
107.615232264973));
#232845=CARTESIAN_POINT('Ctrl Pts',(7.89671931283085,-0.47607954669343,
107.614038402662));
#232846=CARTESIAN_POINT('Ctrl Pts',(7.86571194561248,-0.959744910370648,
107.594906568759));
#232847=CARTESIAN_POINT('Ctrl Pts',(7.7975888032411,-1.41003513985752,107.578264325206));
#232848=CARTESIAN_POINT('Ctrl Pts',(7.58725278814174,-2.28353343489317,
107.546570453044));
#232849=CARTESIAN_POINT('Ctrl Pts',(7.44721451720778,-2.70553365907301,
107.531531091355));
#232850=CARTESIAN_POINT('Ctrl Pts',(7.20643314004819,-3.26794230015215,
107.509857433568));
#232851=CARTESIAN_POINT('Ctrl Pts',(7.13543824782143,-3.42018172434063,
107.503809955386));
#232852=CARTESIAN_POINT('Ctrl Pts',(7.00605114640692,-3.67604102710862,
107.493171890933));
#232853=CARTESIAN_POINT('Ctrl Pts',(6.95006750951079,-3.78081892361137,
107.488673223691));
#232854=CARTESIAN_POINT('Ctrl Pts',(6.85431285779781,-3.95071240251598,
107.481089960115));
#232855=CARTESIAN_POINT('Ctrl Pts',(6.81592269819971,-4.01658194226487,
107.478078882162));
#232856=CARTESIAN_POINT('Ctrl Pts',(6.76897605576573,-4.09452094408914,
107.474438564009));
#232857=CARTESIAN_POINT('Ctrl Pts',(6.76132936770407,-4.10713571521006,
107.473846908367));
#232858=CARTESIAN_POINT('Ctrl Pts',(6.74946852356746,-4.12657970302851,
107.472931225491));
#232859=CARTESIAN_POINT('Ctrl Pts',(6.74527916281771,-4.13342405412287,
107.47260818683));
#232860=CARTESIAN_POINT('Ctrl Pts',(6.73760441535231,-4.14591990148936,
107.472017115026));
#232861=CARTESIAN_POINT('Ctrl Pts',(6.7341223107259,-4.15157341151867,107.471749210262));
#232862=CARTESIAN_POINT('Ctrl Pts',(6.72649503477134,-4.16392213611211,
107.471162984036));
#232863=CARTESIAN_POINT('Ctrl Pts',(6.722346978254,-4.17061555551253,107.47084455181));
#232864=CARTESIAN_POINT('Ctrl Pts',(6.71095974935212,-4.18892918029538,
107.469971460658));
#232865=CARTESIAN_POINT('Ctrl Pts',(6.70370041068931,-4.20053677953207,
107.469416042334));
#232866=CARTESIAN_POINT('Ctrl Pts',(6.66797846229726,-4.25732731242629,
107.466688836095));
#232867=CARTESIAN_POINT('Ctrl Pts',(6.63908929562512,-4.30223962712991,
107.464501566807));
#232868=CARTESIAN_POINT('Ctrl Pts',(6.58888862297852,-4.37857384122342,
107.460735000138));
#232869=CARTESIAN_POINT('Ctrl Pts',(6.56780135620763,-4.41014143448753,
107.45916277701));
#232870=CARTESIAN_POINT('Ctrl Pts',(6.20055389179387,-4.95143398638683,
107.431963150861));
#232871=CARTESIAN_POINT('Ctrl Pts',(5.79623539046615,-5.41915562713048,
107.404994415516));
#232872=CARTESIAN_POINT('Ctrl Pts',(4.83576913553289,-6.29839676295077,
107.349534007919));
#232873=CARTESIAN_POINT('Ctrl Pts',(4.27168591407825,-6.69381927325144,
107.321238455584));
#232874=CARTESIAN_POINT('Ctrl Pts',(3.61329227770282,-7.03784573737825,
107.291112721341));
#232875=CARTESIAN_POINT('Ctrl Pts',(3.56261742480398,-7.06363297806015,
107.288812973398));
#232876=CARTESIAN_POINT('Ctrl Pts',(3.48806994162967,-7.10056213624238,
107.285457312797));
#232877=CARTESIAN_POINT('Ctrl Pts',(3.46441283942842,-7.11213457776606,
107.284396424292));
#232878=CARTESIAN_POINT('Ctrl Pts',(3.42258077192787,-7.13233949573637,
107.282527506461));
#232879=CARTESIAN_POINT('Ctrl Pts',(3.40442985449154,-7.14102115886371,
107.28171889948));
#232880=CARTESIAN_POINT('Ctrl Pts',(3.36647713574723,-7.1589965196296,107.280032940486));
#232881=CARTESIAN_POINT('Ctrl Pts',(3.34666950340663,-7.16827752755352,
107.279155747152));
#232882=CARTESIAN_POINT('Ctrl Pts',(3.29491923141385,-7.19226423531588,
107.276870967726));
#232883=CARTESIAN_POINT('Ctrl Pts',(3.26291652864971,-7.20683934286083,
107.275464984431));
#232884=CARTESIAN_POINT('Ctrl Pts',(3.13137239188303,-7.26569314518026,
107.269713769935));
#232885=CARTESIAN_POINT('Ctrl Pts',(3.03101787363149,-7.30812705245861,
107.265391631183));
#232886=CARTESIAN_POINT('Ctrl Pts',(2.54191271345103,-7.50313201839154,
107.244618304176));
#232887=CARTESIAN_POINT('Ctrl Pts',(2.14236799683754,-7.62683289746065,
107.228566496144));
#232888=CARTESIAN_POINT('Ctrl Pts',(1.38380201505628,-7.79734104755768,
107.19869571647));
#232889=CARTESIAN_POINT('Ctrl Pts',(1.02771569940745,-7.85221115989053,
107.184898193211));
#232890=CARTESIAN_POINT('Ctrl Pts',(0.636243390613084,-7.885442646872,107.169290064976));
#232891=CARTESIAN_POINT('Ctrl Pts',(0.603323693710573,-7.88802965806492,
107.167974041639));
#232892=CARTESIAN_POINT('Ctrl Pts',(0.545574648575651,-7.89220427193122,
107.165658296055));
#232893=CARTESIAN_POINT('Ctrl Pts',(0.520752102115117,-7.89388099804546,
107.164660592043));
#232894=CARTESIAN_POINT('Ctrl Pts',(0.483553537086185,-7.89621748438922,
107.163161668438));
#232895=CARTESIAN_POINT('Ctrl Pts',(0.471183228782001,-7.8969652998838,
107.162662589451));
#232896=CARTESIAN_POINT('Ctrl Pts',(0.449699379641437,-7.89821339127977,
107.161794789531));
#232897=CARTESIAN_POINT('Ctrl Pts',(0.440586622502075,-7.89872696918875,
107.161426373192));
#232898=CARTESIAN_POINT('Ctrl Pts',(0.421614874633604,-7.89976324773733,
107.160658712896));
#232899=CARTESIAN_POINT('Ctrl Pts',(0.411755754750705,-7.90028326521258,
107.160259409931));
#232900=CARTESIAN_POINT('Ctrl Pts',(0.387650715497898,-7.90150943602075,
107.159282252419));
#232901=CARTESIAN_POINT('Ctrl Pts',(0.373403826394887,-7.90219551930367,
107.15870396621));
#232902=CARTESIAN_POINT('Ctrl Pts',(0.318793541002406,-7.90467735621073,
107.156484532693));
#232903=CARTESIAN_POINT('Ctrl Pts',(0.278418668647009,-7.90620240274193,
107.154837821285));
#232904=CARTESIAN_POINT('Ctrl Pts',(-0.204184554541389,-7.92073003251255,
107.135092149863));
#232905=CARTESIAN_POINT('Ctrl Pts',(-0.64673452237051,-7.89692217675445,
107.11639802416));
#232906=CARTESIAN_POINT('Ctrl Pts',(-1.52627019509153,-7.77514674138457,
107.079150398024));
#232907=CARTESIAN_POINT('Ctrl Pts',(-1.96164221014638,-7.67687388076254,
107.06067053362));
#232908=CARTESIAN_POINT('Ctrl Pts',(-2.43873907987548,-7.52592070714098,
107.040373534423));
#232909=CARTESIAN_POINT('Ctrl Pts',(-2.49087158751566,-7.50882744353128,
107.038154318542));
#232910=CARTESIAN_POINT('Ctrl Pts',(-2.57035493869958,-7.48184749096272,
107.034767813482));
#232911=CARTESIAN_POINT('Ctrl Pts',(-2.59783590945898,-7.47235003088363,
107.033596391875));
#232912=CARTESIAN_POINT('Ctrl Pts',(-2.64576447948011,-7.45548949433536,
107.031552206265));
#232913=CARTESIAN_POINT('Ctrl Pts',(-2.66623523094143,-7.44819326933813,
107.030678745979));
#232914=CARTESIAN_POINT('Ctrl Pts',(-2.71246395269402,-7.4315013316775,
107.028705285011));
#232915=CARTESIAN_POINT('Ctrl Pts',(-2.73820368409924,-7.42205586935601,
107.027605816433));
#232916=CARTESIAN_POINT('Ctrl Pts',(-2.80809453530494,-7.39599563343376,
107.024618356802));
#232917=CARTESIAN_POINT('Ctrl Pts',(-2.8521470691761,-7.37911942267261,
107.022733079687));
#232918=CARTESIAN_POINT('Ctrl Pts',(-3.07346578284434,-7.29205581791694,
107.013247174728));
#232919=CARTESIAN_POINT('Ctrl Pts',(-3.24830584242651,-7.21587002555126,
107.005706037657));
#232920=CARTESIAN_POINT('Ctrl Pts',(-3.77951932133691,-6.96117266607116,
106.982517896535));
#232921=CARTESIAN_POINT('Ctrl Pts',(-4.12529559172205,-6.76200026881434,
106.967113041625));
#232922=CARTESIAN_POINT('Ctrl Pts',(-4.86171080274688,-6.26022164824975,
106.933419392483));
#232923=CARTESIAN_POINT('Ctrl Pts',(-5.24200821832247,-5.94541369153949,
106.915415277217));
#232924=CARTESIAN_POINT('Ctrl Pts',(-5.76934720705291,-5.41870947773786,
106.887452742756));
#232925=CARTESIAN_POINT('Ctrl Pts',(-5.93947616884499,-5.2316719454731,
106.877841336039));
#232926=CARTESIAN_POINT('Ctrl Pts',(-6.11595503219677,-5.01792939687397,
106.866864840891));
#232927=CARTESIAN_POINT('Ctrl Pts',(-6.1314676699316,-4.99896245089779,
106.865890824048));
#232928=CARTESIAN_POINT('Ctrl Pts',(-6.15837983118452,-4.96574384173874,
106.864184421783));
#232929=CARTESIAN_POINT('Ctrl Pts',(-6.1698186627513,-4.9515241803991,106.863453810908));
#232930=CARTESIAN_POINT('Ctrl Pts',(-6.18634520589159,-4.93083377791806,
106.862390311236));
#232931=CARTESIAN_POINT('Ctrl Pts',(-6.19147222782832,-4.92439441995835,
106.862059265456));
#232932=CARTESIAN_POINT('Ctrl Pts',(-6.20041443411364,-4.91312728395238,
106.861479901779));
#232933=CARTESIAN_POINT('Ctrl Pts',(-6.20423405847917,-4.90830302756795,
106.861231795986));
#232934=CARTESIAN_POINT('Ctrl Pts',(-6.21161085229062,-4.89896363118827,
106.860751396426));
#232935=CARTESIAN_POINT('Ctrl Pts',(-6.2151687374642,-4.89444906037574,
106.860519137558));
#232936=CARTESIAN_POINT('Ctrl Pts',(-6.22360565992347,-4.88371948632657,
106.859967037557));
#232937=CARTESIAN_POINT('Ctrl Pts',(-6.22848030713842,-4.87750105016458,
106.859646981988));
#232938=CARTESIAN_POINT('Ctrl Pts',(-6.24564908641879,-4.85553166274263,
106.858515923529));
#232939=CARTESIAN_POINT('Ctrl Pts',(-6.25789278847942,-4.83974152993287,
106.857702414895));
#232940=CARTESIAN_POINT('Ctrl Pts',(-6.39663409473134,-4.65940660462988,
106.848403022673));
#232941=CARTESIAN_POINT('Ctrl Pts',(-6.51664717035395,-4.49002052532004,
106.839541008427));
#232942=CARTESIAN_POINT('Ctrl Pts',(-7.01202511022542,-3.72908808634762,
106.799567769173));
#232943=CARTESIAN_POINT('Ctrl Pts',(-7.31454443108464,-3.09388440706398,
106.766224853787));
#232944=CARTESIAN_POINT('Ctrl Pts',(-7.65456465755592,-2.03906803536624,
106.716724569656));
#232945=CARTESIAN_POINT('Ctrl Pts',(-7.74947821176049,-1.64189127308883,
106.699223689447));
#232946=CARTESIAN_POINT('Ctrl Pts',(-7.8170113916222,-1.21605898354082,
106.681733974598));
#232947=CARTESIAN_POINT('Ctrl Pts',(-7.82056771317408,-1.19297410010201,
106.680789590397));
#232948=CARTESIAN_POINT('Ctrl Pts',(-7.82554619124114,-1.15967843630591,
106.679432848613));
#232949=CARTESIAN_POINT('Ctrl Pts',(-7.82705069238963,-1.1494801984557,
106.679018011163));
#232950=CARTESIAN_POINT('Ctrl Pts',(-7.82963189998488,-1.13174347704899,
106.678297779692));
#232951=CARTESIAN_POINT('Ctrl Pts',(-7.83071766183087,-1.1242063370153,
106.677992113259));
#232952=CARTESIAN_POINT('Ctrl Pts',(-7.83278765151611,-1.10968838254856,
106.677404095344));
#232953=CARTESIAN_POINT('Ctrl Pts',(-7.83377343359339,-1.10270779970503,
106.677121697347));
#232954=CARTESIAN_POINT('Ctrl Pts',(-7.83607844635828,-1.08622630689846,
106.676455730402));
#232955=CARTESIAN_POINT('Ctrl Pts',(-7.83738973243673,-1.07672428689971,
106.676072400833));
#232956=CARTESIAN_POINT('Ctrl Pts',(-7.84188612439639,-1.04369848310175,
106.674742213561));
#232957=CARTESIAN_POINT('Ctrl Pts',(-7.84498264260371,-1.0201626639204,
106.673798021626));
#232958=CARTESIAN_POINT('Ctrl Pts',(-7.88029792735005,-0.742067385307632,
106.662685436911));
#232959=CARTESIAN_POINT('Ctrl Pts',(-7.90022083930181,-0.48608988570781,
106.6528967295));
#232960=CARTESIAN_POINT('Ctrl Pts',(-7.90988634133631,-0.153173819004711,
106.64059170563));
#232961=CARTESIAN_POINT('Ctrl Pts',(-7.91099715275511,-0.0767364826541508,
106.637794989213));
#232962=CARTESIAN_POINT('Ctrl Pts',(-7.91102938135051,0.790196293314509,
106.606350262785));
#232963=CARTESIAN_POINT('Ctrl Pts',(-7.79258590487049,1.57613321728681,
106.58086546829));
#232964=CARTESIAN_POINT('Ctrl Pts',(-7.50519677351402,2.5080075256058,106.544753891518));
#232965=CARTESIAN_POINT('Ctrl Pts',(-7.44455740994452,2.68265623579281,
106.537691872609));
#232966=CARTESIAN_POINT('Ctrl Pts',(-7.3727793296357,2.86814294067703,106.529744565052));
#232967=CARTESIAN_POINT('Ctrl Pts',(-7.3676665108513,2.88125131716837,106.529180605833));
#232968=CARTESIAN_POINT('Ctrl Pts',(-7.3600084237171,2.90073164601198,106.528339125464));
#232969=CARTESIAN_POINT('Ctrl Pts',(-7.35748977246574,2.90711408909429,
106.528062885616));
#232970=CARTESIAN_POINT('Ctrl Pts',(-7.35315863246845,2.91804782778047,
106.527588742163));
#232971=CARTESIAN_POINT('Ctrl Pts',(-7.35135021106269,2.92260073797181,
106.52739103125));
#232972=CARTESIAN_POINT('Ctrl Pts',(-7.34781997390163,2.93146451102109,
106.527005592267));
#232973=CARTESIAN_POINT('Ctrl Pts',(-7.34609858995707,2.93577554569997,
106.526817884429));
#232974=CARTESIAN_POINT('Ctrl Pts',(-7.34196621085253,2.94609828625504,
106.526367840101));
#232975=CARTESIAN_POINT('Ctrl Pts',(-7.33955162717348,2.95210854564664,
106.526105337571));
#232976=CARTESIAN_POINT('Ctrl Pts',(-7.33226968124424,2.97017023923109,
106.525315077434));
#232977=CARTESIAN_POINT('Ctrl Pts',(-7.32738001305489,2.98221261314124,
106.524786303965));
#232978=CARTESIAN_POINT('Ctrl Pts',(-7.28341895743385,3.08971995996512,
106.520049261661));
#232979=CARTESIAN_POINT('Ctrl Pts',(-7.24251460184595,3.18442179584331,
106.515760472332));
#232980=CARTESIAN_POINT('Ctrl Pts',(-7.11836742029221,3.45707317657846,
106.503127241869));
#232981=CARTESIAN_POINT('Ctrl Pts',(-7.03033483765897,3.63275336009474,
106.494629001122));
#232982=CARTESIAN_POINT('Ctrl Pts',(-6.69432060971354,4.24525435998921,
106.464094987481));
#232983=CARTESIAN_POINT('Ctrl Pts',(-6.41138994498458,4.66157014886894,
106.441741829819));
#232984=CARTESIAN_POINT('Ctrl Pts',(-5.87827101674219,5.30479762552317,
106.405964457483));
#232985=CARTESIAN_POINT('Ctrl Pts',(-5.64963788844624,5.5476627118158,106.392075004085));
#232986=CARTESIAN_POINT('Ctrl Pts',(-5.37958556859561,5.80045902386594,
106.377097101586));
#232987=CARTESIAN_POINT('Ctrl Pts',(-5.35263982014906,5.8253337037841,106.375616971292));
#232988=CARTESIAN_POINT('Ctrl Pts',(-5.31314392962237,5.86128849073682,
106.373467815168));
#232989=CARTESIAN_POINT('Ctrl Pts',(-5.30073015043904,5.87251743831149,
106.372795215984));
#232990=CARTESIAN_POINT('Ctrl Pts',(-5.2787226818941,5.89229776978474,106.371607859246));
#232991=CARTESIAN_POINT('Ctrl Pts',(-5.26914363052744,5.90086532316607,
106.371092723231));
#232992=CARTESIAN_POINT('Ctrl Pts',(-5.24924849801795,5.91857256095623,
106.37002625383));
#232993=CARTESIAN_POINT('Ctrl Pts',(-5.23892932179173,5.92770870706984,
106.369475003028));
#232994=CARTESIAN_POINT('Ctrl Pts',(-5.21231740947151,5.95114595639587,
106.368058232583));
#232995=CARTESIAN_POINT('Ctrl Pts',(-5.19598964395698,5.96540716099233,
106.367193614298));
#232996=CARTESIAN_POINT('Ctrl Pts',(-5.12989719699649,6.02265724473699,
106.363712111768));
#232997=CARTESIAN_POINT('Ctrl Pts',(-5.07965541254064,6.06509246355605,
106.361107051081));
#232998=CARTESIAN_POINT('Ctrl Pts',(-4.76329969222687,6.32560418624132,
106.344955672411));
#232999=CARTESIAN_POINT('Ctrl Pts',(-4.48371817320108,6.52675881440461,
106.331798129946));
#233000=CARTESIAN_POINT('Ctrl Pts',(-3.58102953646378,7.09077010431463,
106.291937392995));
#233001=CARTESIAN_POINT('Ctrl Pts',(-2.92093090641103,7.38720445521934,
106.266584319917));
#233002=CARTESIAN_POINT('Ctrl Pts',(-2.15652665017984,7.61177809132325,
106.235417926028));
#233003=CARTESIAN_POINT('Ctrl Pts',(-2.08282331128198,7.63227485800151,
106.23239195626));
#233004=CARTESIAN_POINT('Ctrl Pts',(-1.99635611025489,7.6549754903757,106.228807945466));
#233005=CARTESIAN_POINT('Ctrl Pts',(-1.98386846629955,7.65822129369446,
106.228289515305));
#233006=CARTESIAN_POINT('Ctrl Pts',(-1.96390478998727,7.66335817005293,
106.227459332426));
#233007=CARTESIAN_POINT('Ctrl Pts',(-1.95643380733656,7.66526889441129,
106.227148345312));
#233008=CARTESIAN_POINT('Ctrl Pts',(-1.94322459476225,7.66862661729123,
106.226597937897));
#233009=CARTESIAN_POINT('Ctrl Pts',(-1.93748750576447,7.67007810819928,
106.22635869551));
#233010=CARTESIAN_POINT('Ctrl Pts',(-1.92560447395457,7.6730703474208,106.22586276639));
#233011=CARTESIAN_POINT('Ctrl Pts',(-1.9194582994686,7.67461015184991,106.225606042095));
#233012=CARTESIAN_POINT('Ctrl Pts',(-1.90368193109016,7.67854247693966,
106.224946494069));
#233013=CARTESIAN_POINT('Ctrl Pts',(-1.8940490910787,7.68092426107118,106.224543235584));
#233014=CARTESIAN_POINT('Ctrl Pts',(-1.85445816777126,7.69063437540362,
106.222883522267));
#233015=CARTESIAN_POINT('Ctrl Pts',(-1.82446210215475,7.69780554392879,
106.221620580557));
#233016=CARTESIAN_POINT('Ctrl Pts',(-1.63459563038937,7.74202487858123,
106.213588539659));
#233017=CARTESIAN_POINT('Ctrl Pts',(-1.47367156421402,7.77426092177394,
106.206586974652));
#233018=CARTESIAN_POINT('Ctrl Pts',(-1.20709355409295,7.81908785293875,
106.194742855578));
#233019=CARTESIAN_POINT('Ctrl Pts',(-1.10197456548786,7.83459383796254,
106.190014529623));
#233020=CARTESIAN_POINT('Ctrl Pts',(-0.702892945268238,7.88527135087547,
106.171921255509));
#233021=CARTESIAN_POINT('Ctrl Pts',(-0.40735150003555,7.90604966999354,
106.158239887809));
#233022=CARTESIAN_POINT('Ctrl Pts',(0.525300154104513,7.9191780831024,106.11532311649));
#233023=CARTESIAN_POINT('Ctrl Pts',(1.1607973920164,7.85124920709851,106.08668483371));
#233024=CARTESIAN_POINT('Ctrl Pts',(1.8142596067873,7.7002288587693,106.059319162972));
#233025=CARTESIAN_POINT('Ctrl Pts',(1.84712776248553,7.69241064072372,106.057947622848));
#233026=CARTESIAN_POINT('Ctrl Pts',(1.89455480527723,7.68080785516156,106.05597558122));
#233027=CARTESIAN_POINT('Ctrl Pts',(1.90915433449321,7.67719199633291,106.055369488809));
#233028=CARTESIAN_POINT('Ctrl Pts',(1.93251613700216,7.67133522771092,106.054401167716));
#233029=CARTESIAN_POINT('Ctrl Pts',(1.94128499780341,7.6691208983641,106.054038054395));
#233030=CARTESIAN_POINT('Ctrl Pts',(1.95680196831877,7.66517420508086,106.053396116162));
#233031=CARTESIAN_POINT('Ctrl Pts',(1.96355161491631,7.66344795724127,106.053117087429));
#233032=CARTESIAN_POINT('Ctrl Pts',(1.97754727053993,7.65984881083601,106.05253893333));
#233033=CARTESIAN_POINT('Ctrl Pts',(1.98479292159966,7.65797454101705,106.052239854154));
#233034=CARTESIAN_POINT('Ctrl Pts',(2.0034281351389,7.65312585001196,106.051471250138));
#233035=CARTESIAN_POINT('Ctrl Pts',(2.01481375722863,7.6501362794441,106.051002233295));
#233036=CARTESIAN_POINT('Ctrl Pts',(2.06193104225221,7.6376520131301,106.049063677032));
#233037=CARTESIAN_POINT('Ctrl Pts',(2.09760287671754,7.62793223077538,106.047601706348));
#233038=CARTESIAN_POINT('Ctrl Pts',(2.6927296947057,7.46128296862159,106.023303392563));
#233039=CARTESIAN_POINT('Ctrl Pts',(3.23329596615774,7.24344069571108,106.002787542959));
#233040=CARTESIAN_POINT('Ctrl Pts',(4.28225978382236,6.67966685589333,105.962405803492));
#233041=CARTESIAN_POINT('Ctrl Pts',(4.78411066943029,6.32991630018231,105.942707858317));
#233042=CARTESIAN_POINT('Ctrl Pts',(5.34797797119683,5.83125500655345,105.914651969039));
#233043=CARTESIAN_POINT('Ctrl Pts',(5.45258717427359,5.73355841250004,105.909149629697));
#233044=CARTESIAN_POINT('Ctrl Pts',(5.56320027988232,5.62448873297047,105.902929287309));
#233045=CARTESIAN_POINT('Ctrl Pts',(5.57189712225385,5.61587333520914,105.902437435402));
#233046=CARTESIAN_POINT('Ctrl Pts',(5.58400324881667,5.60382477658801,105.901748820162));
#233047=CARTESIAN_POINT('Ctrl Pts',(5.58742947392514,5.60040858180962,105.901553487847));
#233048=CARTESIAN_POINT('Ctrl Pts',(5.59334089972586,5.59450363746438,105.901215701231));
#233049=CARTESIAN_POINT('Ctrl Pts',(5.59582758202459,5.59201636642067,105.901073372909));
#233050=CARTESIAN_POINT('Ctrl Pts',(5.60097058972605,5.58686527536336,105.900778515686));
#233051=CARTESIAN_POINT('Ctrl Pts',(5.60362667471784,5.58420121792964,105.90062596638));
#233052=CARTESIAN_POINT('Ctrl Pts',(5.60976505086272,5.578035627464,105.900272784378));
#233053=CARTESIAN_POINT('Ctrl Pts',(5.61324593990732,5.57453275216906,105.900072034171));
#233054=CARTESIAN_POINT('Ctrl Pts',(5.62445523817989,5.56323150840667,105.899424049908));
#233055=CARTESIAN_POINT('Ctrl Pts',(5.63217064158063,5.55542036249916,105.898975709172));
#233056=CARTESIAN_POINT('Ctrl Pts',(5.65022540051358,5.53706528775738,105.897921137895));
#233057=CARTESIAN_POINT('Ctrl Pts',(5.66055151266958,5.52650844964806,105.897313809371));
#233058=CARTESIAN_POINT('Ctrl Pts',(5.76846167151175,5.41556743033146,105.890923812287));
#233059=CARTESIAN_POINT('Ctrl Pts',(5.86338912345694,5.31264381674667,105.884930644053));
#233060=CARTESIAN_POINT('Ctrl Pts',(6.09968377031884,5.04239431792184,105.869173144019));
#233061=CARTESIAN_POINT('Ctrl Pts',(6.23692216167477,4.8716193354395,105.8591979773));
#233062=CARTESIAN_POINT('Ctrl Pts',(6.8832363307184,3.99522352431714,105.808859777952));
#233063=CARTESIAN_POINT('Ctrl Pts',(7.28072424632657,3.21442699816221,105.76758485744));
#233064=CARTESIAN_POINT('Ctrl Pts',(7.55984904695948,2.33145893135083,105.729643859279));
#233065=CARTESIAN_POINT('Ctrl Pts',(7.57606398208699,2.27821708350046,105.727383447469));
#233066=CARTESIAN_POINT('Ctrl Pts',(7.59524851848286,2.21275365167149,105.724637086493));
#233067=CARTESIAN_POINT('Ctrl Pts',(7.59875236105398,2.20069110461088,105.72413239445));
#233068=CARTESIAN_POINT('Ctrl Pts',(7.60449470778101,2.18074491863104,105.723300094403));
#233069=CARTESIAN_POINT('Ctrl Pts',(7.60674971108511,2.17286607831082,105.722971908503));
#233070=CARTESIAN_POINT('Ctrl Pts',(7.61079922003587,2.15863378516567,105.722380112604));
#233071=CARTESIAN_POINT('Ctrl Pts',(7.61259802133791,2.15228156893393,105.722116352455));
#233072=CARTESIAN_POINT('Ctrl Pts',(7.61642573634328,2.13869969535905,105.721553192547));
#233073=CARTESIAN_POINT('Ctrl Pts',(7.61845231355171,2.13146938301492,105.721253874663));
#233074=CARTESIAN_POINT('Ctrl Pts',(7.62390082857731,2.11192342197791,105.720446011161));
#233075=CARTESIAN_POINT('Ctrl Pts',(7.62730322434541,2.09960232193685,105.719938148063));
#233076=CARTESIAN_POINT('Ctrl Pts',(7.64389842426363,2.03893340594918,105.717444212544));
#233077=CARTESIAN_POINT('Ctrl Pts',(7.65666161261057,1.99046869587584,105.715473120214));
#233078=CARTESIAN_POINT('Ctrl Pts',(7.75852917657752,1.58816964382418,105.699281176271));
#233079=CARTESIAN_POINT('Ctrl Pts',(7.82352071955822,1.22866433344624,105.685927409384));
#233080=CARTESIAN_POINT('Ctrl Pts',(7.93763427257802,0.192405542143997,
105.649285448962));
#233081=CARTESIAN_POINT('Ctrl Pts',(7.92495832516765,-0.487766230684799,
105.627630277317));
#233082=CARTESIAN_POINT('Ctrl Pts',(7.81662282161649,-1.21994165280978,
105.600446807928));
#233083=CARTESIAN_POINT('Ctrl Pts',(7.80671165764907,-1.28183570373121,
105.598115851771));
#233084=CARTESIAN_POINT('Ctrl Pts',(7.7761730217504,-1.45903165265274,105.591330826772));
#233085=CARTESIAN_POINT('Ctrl Pts',(7.75371964680885,-1.57399789660289,
105.58679236994));
#233086=CARTESIAN_POINT('Ctrl Pts',(7.7264518578499,-1.69881604967526,105.581673062458));
#233087=CARTESIAN_POINT('Ctrl Pts',(7.72415932861255,-1.70920945089628,
105.581245320184));
#233088=CARTESIAN_POINT('Ctrl Pts',(7.72071617951667,-1.7246708910578,105.580606806497));
#233089=CARTESIAN_POINT('Ctrl Pts',(7.71958155801904,-1.72974234380659,
105.580397019714));
#233090=CARTESIAN_POINT('Ctrl Pts',(7.71762464156699,-1.73844895884471,
105.580036263015));
#233091=CARTESIAN_POINT('Ctrl Pts',(7.71680477217257,-1.74208467036115,
105.579885439235));
#233092=CARTESIAN_POINT('Ctrl Pts',(7.71520002201614,-1.74917757490215,
105.579590850105));
#233093=CARTESIAN_POINT('Ctrl Pts',(7.71441538577593,-1.75263482330744,
105.579447099397));
#233094=CARTESIAN_POINT('Ctrl Pts',(7.71254792291515,-1.76083765004398,
105.579105649553));
#233095=CARTESIAN_POINT('Ctrl Pts',(7.71146304075051,-1.76558275479234,
105.578907828254));
#233096=CARTESIAN_POINT('Ctrl Pts',(7.708213801506,-1.77973429361479,105.57831696162));
#233097=CARTESIAN_POINT('Ctrl Pts',(7.70603661477569,-1.78913774085468,
105.577923160743));
#233098=CARTESIAN_POINT('Ctrl Pts',(7.70102677212553,-1.81059686812671,
105.577021828845));
#233099=CARTESIAN_POINT('Ctrl Pts',(7.69818301210616,-1.82264990403977,
105.576513655977));
#233100=CARTESIAN_POINT('Ctrl Pts',(7.57485364604281,-2.33993328393579,
105.554623326156));
#233101=CARTESIAN_POINT('Ctrl Pts',(7.40494280283978,-2.83203348029344,
105.530541066803));
#233102=CARTESIAN_POINT('Ctrl Pts',(7.07044660336402,-3.55977902504154,
105.493182458441));
#233103=CARTESIAN_POINT('Ctrl Pts',(6.93924064256329,-3.80922412902051,
105.480018041427));
#233104=CARTESIAN_POINT('Ctrl Pts',(6.53193628424697,-4.49239820047406,
105.443551223091));
#233105=CARTESIAN_POINT('Ctrl Pts',(6.22648357998664,-4.90702200725167,
105.421002888292));
#233106=CARTESIAN_POINT('Ctrl Pts',(5.86053602123054,-5.31405314187601,
105.398720871085));
#233107=CARTESIAN_POINT('Ctrl Pts',(5.8379803753811,-5.338822756332,105.397363782543));
#233108=CARTESIAN_POINT('Ctrl Pts',(5.80709295227768,-5.37231214995567,
105.395527236734));
#233109=CARTESIAN_POINT('Ctrl Pts',(5.79889773800933,-5.38115707062436,
105.395042020107));
#233110=CARTESIAN_POINT('Ctrl Pts',(5.78592113716253,-5.39509837054032,
105.394276954471));
#233111=CARTESIAN_POINT('Ctrl Pts',(5.78115318128632,-5.40020719307048,
105.393996536657));
#233112=CARTESIAN_POINT('Ctrl Pts',(5.77193337049546,-5.41005993405388,
105.393455616101));
#233113=CARTESIAN_POINT('Ctrl Pts',(5.76748242170962,-5.41480469075562,
105.393195075228));
#233114=CARTESIAN_POINT('Ctrl Pts',(5.75693097140843,-5.42602487438298,
105.39257883588));
#233115=CARTESIAN_POINT('Ctrl Pts',(5.7508253838328,-5.43249551792844,105.392223354427));
#233116=CARTESIAN_POINT('Ctrl Pts',(5.73287003091193,-5.45146023799775,
105.391181181241));
#233117=CARTESIAN_POINT('Ctrl Pts',(5.72099033823889,-5.4639259761035,105.390495768138));
#233118=CARTESIAN_POINT('Ctrl Pts',(5.63178002833542,-5.55692726994508,
105.385379182763));
#233119=CARTESIAN_POINT('Ctrl Pts',(5.55279124185217,-5.63585819828866,
105.381019901706));
#233120=CARTESIAN_POINT('Ctrl Pts',(5.28767653392548,-5.88979229701464,
105.366912647368));
#233121=CARTESIAN_POINT('Ctrl Pts',(5.09474011491395,-6.05745911481499,
105.357468760778));
#233122=CARTESIAN_POINT('Ctrl Pts',(4.57684193019832,-6.46524648868583,
105.333749233714));
#233123=CARTESIAN_POINT('Ctrl Pts',(4.24100692455315,-6.69034838433158,
105.319903515494));
#233124=CARTESIAN_POINT('Ctrl Pts',(3.48134165673463,-7.11925831866761,
105.28959733606));
#233125=CARTESIAN_POINT('Ctrl Pts',(3.05354484548062,-7.31296500264657,
105.273082543309));
#233126=CARTESIAN_POINT('Ctrl Pts',(2.56900603686614,-7.48238727103136,
105.252846144022));
#233127=CARTESIAN_POINT('Ctrl Pts',(2.52677018845004,-7.49675553868532,
105.251072604673));
#233128=CARTESIAN_POINT('Ctrl Pts',(2.4723408612444,-7.51475970462628,105.248776428497));
#233129=CARTESIAN_POINT('Ctrl Pts',(2.46025653384522,-7.51872466166755,
105.248265964616));
#233130=CARTESIAN_POINT('Ctrl Pts',(2.44098501128724,-7.52499635554101,
105.247450880783));
#233131=CARTESIAN_POINT('Ctrl Pts',(2.43380395840812,-7.52732198513062,
105.247146934833));
#233132=CARTESIAN_POINT('Ctrl Pts',(2.42036191966919,-7.53165402839776,
105.24657757588));
#233133=CARTESIAN_POINT('Ctrl Pts',(2.41410173600743,-7.53366292274778,
105.246312249702));
#233134=CARTESIAN_POINT('Ctrl Pts',(2.40025408827323,-7.53808760345943,
105.245724984674));
#233135=CARTESIAN_POINT('Ctrl Pts',(2.39266547079637,-7.54049974140044,
105.245402921272));
#233136=CARTESIAN_POINT('Ctrl Pts',(2.37077548636033,-7.54742137806952,
105.244473238611));
#233137=CARTESIAN_POINT('Ctrl Pts',(2.35646495883801,-7.55190166510348,
105.243864643656));
#233138=CARTESIAN_POINT('Ctrl Pts',(2.26472938666755,-7.58033575969529,
105.239958402624));
#233139=CARTESIAN_POINT('Ctrl Pts',(2.1869540430832,-7.6031388906577,105.236624193573));
#233140=CARTESIAN_POINT('Ctrl Pts',(1.93621839925187,-7.67248709825828,
105.225825885811));
#233141=CARTESIAN_POINT('Ctrl Pts',(1.76202529855718,-7.71435440278824,
105.218250464062));
#233142=CARTESIAN_POINT('Ctrl Pts',(1.20945729845843,-7.82747116259094,
105.19418733778));
#233143=CARTESIAN_POINT('Ctrl Pts',(0.827216387842954,-7.87704313949055,
105.177523376986));
#233144=CARTESIAN_POINT('Ctrl Pts',(0.036421668452692,-7.92138414684184,
105.143655816423));
#233145=CARTESIAN_POINT('Ctrl Pts',(-0.371204159468807,-7.91276686889032,
105.126533007308));
#233146=CARTESIAN_POINT('Ctrl Pts',(-0.858048411075272,-7.86475753657331,
105.106266630712));
#233147=CARTESIAN_POINT('Ctrl Pts',(-0.93960255654408,-7.85543158153127,
105.102876101318));
#233148=CARTESIAN_POINT('Ctrl Pts',(-1.29360066034414,-7.80935911466337,
105.088159693386));
#233149=CARTESIAN_POINT('Ctrl Pts',(-1.56417635887421,-7.7596939649725,
105.076891859814));
#233150=CARTESIAN_POINT('Ctrl Pts',(-1.87102985666812,-7.68666438936108,
105.064122432468));
#233151=CARTESIAN_POINT('Ctrl Pts',(-1.91036781084693,-7.67698228520684,
105.062485534636));
#233152=CARTESIAN_POINT('Ctrl Pts',(-1.974282255296,-7.66072957486322,105.05982611255));
#233153=CARTESIAN_POINT('Ctrl Pts',(-1.99890439893648,-7.65434185622841,
105.058801638611));
#233154=CARTESIAN_POINT('Ctrl Pts',(-2.04283668993195,-7.64271807234374,
105.056973735756));
#233155=CARTESIAN_POINT('Ctrl Pts',(-2.06215857266666,-7.63752730266007,
105.056169813212));
#233156=CARTESIAN_POINT('Ctrl Pts',(-2.10301072108604,-7.62638615963095,
105.054470077423));
#233157=CARTESIAN_POINT('Ctrl Pts',(-2.12453590533921,-7.62041777984972,
105.05357447487));
#233158=CARTESIAN_POINT('Ctrl Pts',(-2.18190424527362,-7.60424905061849,
105.051187474993));
#233159=CARTESIAN_POINT('Ctrl Pts',(-2.21770115747607,-7.59388644587783,
105.049697960601));
#233160=CARTESIAN_POINT('Ctrl Pts',(-2.39130335690778,-7.54229930308727,
105.04247345317));
#233161=CARTESIAN_POINT('Ctrl Pts',(-2.52804145945883,-7.49757413247492,
105.036780862694));
#233162=CARTESIAN_POINT('Ctrl Pts',(-3.34045228452211,-7.20709186589195,
105.00287759895));
#233163=CARTESIAN_POINT('Ctrl Pts',(-3.98122994099946,-6.87390125026642,
104.976111044038));
#233164=CARTESIAN_POINT('Ctrl Pts',(-4.62130200982151,-6.4211936314609,
104.945084104855));
#233165=CARTESIAN_POINT('Ctrl Pts',(-4.67399071621715,-6.38294371955429,
104.942492321192));
#233166=CARTESIAN_POINT('Ctrl Pts',(-4.74030581851302,-6.33354017279517,
104.939176438108));
#233167=CARTESIAN_POINT('Ctrl Pts',(-4.75437573115943,-6.32298519501784,
104.938469776438));
#233168=CARTESIAN_POINT('Ctrl Pts',(-4.77714382200755,-6.30578604948514,
104.937321117851));
#233169=CARTESIAN_POINT('Ctrl Pts',(-4.78586357399881,-6.29917063177192,
104.936879982036));
#233170=CARTESIAN_POINT('Ctrl Pts',(-4.8018291474333,-6.28700573700533,
104.936070057323));
#233171=CARTESIAN_POINT('Ctrl Pts',(-4.80907915385023,-6.2814617717345,
104.9357014255));
#233172=CARTESIAN_POINT('Ctrl Pts',(-4.82620302928776,-6.2683203917819,
104.934828770343));
#233173=CARTESIAN_POINT('Ctrl Pts',(-4.83606856834782,-6.26071218112536,
104.934324448011));
#233174=CARTESIAN_POINT('Ctrl Pts',(-4.86494801153547,-6.23833163554391,
104.932843608189));
#233175=CARTESIAN_POINT('Ctrl Pts',(-4.88391244348126,-6.22349580104308,
104.93186539077));
#233176=CARTESIAN_POINT('Ctrl Pts',(-5.03410132235224,-6.10489410735503,
104.924073269472));
#233177=CARTESIAN_POINT('Ctrl Pts',(-5.1620697590268,-5.99707778083458,
104.917159603426));
#233178=CARTESIAN_POINT('Ctrl Pts',(-5.51401379139163,-5.68094039309349,
104.897458256518));
#233179=CARTESIAN_POINT('Ctrl Pts',(-5.72946565181466,-5.46357519450972,
104.884569955401));
#233180=CARTESIAN_POINT('Ctrl Pts',(-6.2222095992506,-4.90516957865222,
104.853335283329));
#233181=CARTESIAN_POINT('Ctrl Pts',(-6.48474069979273,-4.55244363872441,
104.835134214252));
#233182=CARTESIAN_POINT('Ctrl Pts',(-6.74295310230439,-4.13750896575956,
104.815309969591));
#233183=CARTESIAN_POINT('Ctrl Pts',(-6.76884418641868,-4.09501470091643,
104.813296488418));
#233184=CARTESIAN_POINT('Ctrl Pts',(-6.81020937420422,-4.02565894796312,
104.810036569524));
#233185=CARTESIAN_POINT('Ctrl Pts',(-6.8259294723996,-3.99894592772647,
104.808787237415));
#233186=CARTESIAN_POINT('Ctrl Pts',(-6.85365205280577,-3.95119741858366,
104.806564990027));
#233187=CARTESIAN_POINT('Ctrl Pts',(-6.86571567901906,-3.93019792386195,
104.805591377464));
#233188=CARTESIAN_POINT('Ctrl Pts',(-6.89099281711486,-3.88572574132131,
104.803537182765));
#233189=CARTESIAN_POINT('Ctrl Pts',(-6.90418326365567,-3.86224028381423,
104.80245687244));
#233190=CARTESIAN_POINT('Ctrl Pts',(-6.93906173231599,-3.79938984672886,
104.799577516735));
#233191=CARTESIAN_POINT('Ctrl Pts',(-6.96053471602924,-3.75990657128227,
104.797780860364));
#233192=CARTESIAN_POINT('Ctrl Pts',(-7.07015882352115,-3.55417821031327,
104.78847972497));
#233193=CARTESIAN_POINT('Ctrl Pts',(-7.15269509877856,-3.3850084880439,
104.781034422208));
#233194=CARTESIAN_POINT('Ctrl Pts',(-7.34803107395479,-2.94551802114772,
104.762095799163));
#233195=CARTESIAN_POINT('Ctrl Pts',(-7.45199992584659,-2.67158043128907,
104.750698482321));
#233196=CARTESIAN_POINT('Ctrl Pts',(-7.78611126941897,-1.61854911264299,
104.708410644666));
#233197=CARTESIAN_POINT('Ctrl Pts',(-7.91102272519647,-0.811531069090435,
104.679708267495));
#233198=CARTESIAN_POINT('Ctrl Pts',(-7.9109999968991,0.000221500451111772,
104.648002515785));
#233199=CARTESIAN_POINT('',(-7.91099875017949,0.00164077279768504,100.640436842002));
#233200=CARTESIAN_POINT('Ctrl Pts',(-7.91099999680876,0.00022470367903259,
104.648002390672));
#233201=CARTESIAN_POINT('Ctrl Pts',(-7.91099856279906,0.0507109744170651,
104.646030477437));
#233202=CARTESIAN_POINT('Ctrl Pts',(-7.91051384011523,0.101195664386328,
104.644044926041));
#233203=CARTESIAN_POINT('Ctrl Pts',(-7.90900130355969,0.180073065026429,
104.640917243705));
#233204=CARTESIAN_POINT('Ctrl Pts',(-7.90830372159879,0.208470985230131,
104.639786037387));
#233205=CARTESIAN_POINT('Ctrl Pts',(-7.90716408160562,0.246516605544437,
104.638262975117));
#233206=CARTESIAN_POINT('Ctrl Pts',(-7.90685727935303,0.256168329812173,
104.63787594103));
#233207=CARTESIAN_POINT('Ctrl Pts',(-7.90630759975512,0.272517998349415,
104.637219184298));
#233208=CARTESIAN_POINT('Ctrl Pts',(-7.9060738805796,0.279216252838261,
104.636949796477));
#233209=CARTESIAN_POINT('Ctrl Pts',(-7.9056254789115,0.291615036211121,
104.636450537674));
#233210=CARTESIAN_POINT('Ctrl Pts',(-7.9054131420722,0.297315648930616,
104.636220754024));
#233211=CARTESIAN_POINT('Ctrl Pts',(-7.90497519624272,0.308740942716914,
104.635759730748));
#233212=CARTESIAN_POINT('Ctrl Pts',(-7.90474953415147,0.314465618209801,
104.635528489254));
#233213=CARTESIAN_POINT('Ctrl Pts',(-7.90421395854293,0.327687350318683,
104.63499383911));
#233214=CARTESIAN_POINT('Ctrl Pts',(-7.90389959728831,0.335184214230046,
104.6346902605));
#233215=CARTESIAN_POINT('Ctrl Pts',(-7.90307842516679,0.354123702037099,
104.633922223714));
#233216=CARTESIAN_POINT('Ctrl Pts',(-7.90255742967426,0.365565670643811,
104.633457213143));
#233217=CARTESIAN_POINT('Ctrl Pts',(-7.89961883478154,0.427158283451147,
104.63094840743));
#233218=CARTESIAN_POINT('Ctrl Pts',(-7.89674872372343,0.477285407664686,
104.628886511833));
#233219=CARTESIAN_POINT('Ctrl Pts',(-7.89124278339187,0.559693766779013,
104.625459169533));
#233220=CARTESIAN_POINT('Ctrl Pts',(-7.88888556293277,0.591991795322786,
104.624106200033));
#233221=CARTESIAN_POINT('Ctrl Pts',(-7.81394376102194,1.53871583977549,
104.584164654968));
#233222=CARTESIAN_POINT('Ctrl Pts',(-7.58307770621705,2.43363324719075,
104.539481595288));
#233223=CARTESIAN_POINT('Ctrl Pts',(-7.06830902794243,3.56800813626424,
104.484658793237));
#233224=CARTESIAN_POINT('Ctrl Pts',(-6.91418053371399,3.85821386152608,
104.470723979871));
#233225=CARTESIAN_POINT('Ctrl Pts',(-6.729989376434,4.15833279892066,104.456437009841));
#233226=CARTESIAN_POINT('Ctrl Pts',(-6.71743496433179,4.17858303565186,
104.45547354415));
#233227=CARTESIAN_POINT('Ctrl Pts',(-6.69927320480545,4.2075845252691,104.454094427105));
#233228=CARTESIAN_POINT('Ctrl Pts',(-6.69373985410061,4.21638183476724,
104.453676180859));
#233229=CARTESIAN_POINT('Ctrl Pts',(-6.68411429059146,4.23161852737457,
104.452951949115));
#233230=CARTESIAN_POINT('Ctrl Pts',(-6.6800300747075,4.23806293161227,104.452645682624));
#233231=CARTESIAN_POINT('Ctrl Pts',(-6.67216473705474,4.25043387691242,
104.452057853155));
#233232=CARTESIAN_POINT('Ctrl Pts',(-6.66838502724493,4.2563613038736,104.451776240816));
#233233=CARTESIAN_POINT('Ctrl Pts',(-6.65947143203441,4.27029879087911,
104.451114163599));
#233234=CARTESIAN_POINT('Ctrl Pts',(-6.65433098260269,4.27830465164008,
104.450733931261));
#233235=CARTESIAN_POINT('Ctrl Pts',(-6.63655634382299,4.30587777277385,
104.449424607447));
#233236=CARTESIAN_POINT('Ctrl Pts',(-6.62385013637651,4.32539858058769,
104.448498071353));
#233237=CARTESIAN_POINT('Ctrl Pts',(-6.48042408747497,4.54363282285369,
104.438143967653));
#233238=CARTESIAN_POINT('Ctrl Pts',(-6.34088766361146,4.73641741648619,
104.429041182139));
#233239=CARTESIAN_POINT('Ctrl Pts',(-5.92541193619878,5.25910261397333,
104.404250217426));
#233240=CARTESIAN_POINT('Ctrl Pts',(-5.63096950902634,5.57322839518147,
104.389248594054));
#233241=CARTESIAN_POINT('Ctrl Pts',(-5.0198060940556,6.12710838409801,104.360735954042));
#233242=CARTESIAN_POINT('Ctrl Pts',(-4.70771333084289,6.37003308490911,
104.347227078248));
#233243=CARTESIAN_POINT('Ctrl Pts',(-4.28277127253056,6.65244967306423,
104.328694539707));
#233244=CARTESIAN_POINT('Ctrl Pts',(-4.18535822962497,6.71416349795983,
104.324435906049));
#233245=CARTESIAN_POINT('Ctrl Pts',(-4.00908370712365,6.82051111454271,
104.316657700916));
#233246=CARTESIAN_POINT('Ctrl Pts',(-3.93073784819223,6.86596119122125,
104.313176083664));
#233247=CARTESIAN_POINT('Ctrl Pts',(-3.82464060989635,6.92509927962185,
104.308408775803));
#233248=CARTESIAN_POINT('Ctrl Pts',(-3.79756307748602,6.93998490532024,
104.307187490177));
#233249=CARTESIAN_POINT('Ctrl Pts',(-3.75763579788348,6.96163091256331,
104.305379517897));
#233250=CARTESIAN_POINT('Ctrl Pts',(-3.74485439548694,6.9685147129493,104.304799726108));
#233251=CARTESIAN_POINT('Ctrl Pts',(-3.72470916890797,6.97929308740188,
104.303884366577));
#233252=CARTESIAN_POINT('Ctrl Pts',(-3.71735797276682,6.98321130242447,
104.303550023251));
#233253=CARTESIAN_POINT('Ctrl Pts',(-3.70493776233799,6.98980615156952,
104.302984612616));
#233254=CARTESIAN_POINT('Ctrl Pts',(-3.69987199112979,6.99248890655688,
104.302753855288));
#233255=CARTESIAN_POINT('Ctrl Pts',(-3.68992392858131,6.99774341141572,
104.302300418817));
#233256=CARTESIAN_POINT('Ctrl Pts',(-3.68504185269115,7.00031556391699,
104.302077759935));
#233257=CARTESIAN_POINT('Ctrl Pts',(-3.67570639597185,7.00522153611013,
104.301651747489));
#233258=CARTESIAN_POINT('Ctrl Pts',(-3.67125347194643,7.00755622338647,
104.30144843665));
#233259=CARTESIAN_POINT('Ctrl Pts',(-3.66096760333801,7.01293665358347,
104.30097856469));
#233260=CARTESIAN_POINT('Ctrl Pts',(-3.65513308335295,7.0159793644559,104.30071185706));
#233261=CARTESIAN_POINT('Ctrl Pts',(-3.6373081905813,7.02524680301354,104.299896514485));
#233262=CARTESIAN_POINT('Ctrl Pts',(-3.62530570182206,7.03144807857554,
104.299346766615));
#233263=CARTESIAN_POINT('Ctrl Pts',(-3.53762387447654,7.07646609753964,
104.295325673824));
#233264=CARTESIAN_POINT('Ctrl Pts',(-3.46134046951723,7.11409000268569,
104.291800150482));
#233265=CARTESIAN_POINT('Ctrl Pts',(-3.0728898455068,7.29795167383479,104.273764399361));
#233266=CARTESIAN_POINT('Ctrl Pts',(-2.75201623198666,7.42490008742438,
104.258618476405));
#233267=CARTESIAN_POINT('Ctrl Pts',(-2.1696589011589,7.61234768296996,104.231678047842));
#233268=CARTESIAN_POINT('Ctrl Pts',(-1.91143081212576,7.68125603244696,
104.219909252492));
#233269=CARTESIAN_POINT('Ctrl Pts',(-1.22663432146542,7.82731543238694,
104.189517994866));
#233270=CARTESIAN_POINT('Ctrl Pts',(-0.796335537854923,7.88272771644739,
104.171274756551));
#233271=CARTESIAN_POINT('Ctrl Pts',(-0.324223379771767,7.90445170920404,
104.152124786385));
#233272=CARTESIAN_POINT('Ctrl Pts',(-0.284797795784741,7.90597039412212,
104.150531596297));
#233273=CARTESIAN_POINT('Ctrl Pts',(-0.227937076194581,7.90773479698451,
104.148241983106));
#233274=CARTESIAN_POINT('Ctrl Pts',(-0.210510091046111,7.90821790510105,
104.147541350046));
#233275=CARTESIAN_POINT('Ctrl Pts',(-0.180168731504492,7.90895865901514,
104.146323363445));
#233276=CARTESIAN_POINT('Ctrl Pts',(-0.167255078335444,7.90924228872335,
104.145805558265));
#233277=CARTESIAN_POINT('Ctrl Pts',(-0.142339721462338,7.90972847091561,
104.144807614446));
#233278=CARTESIAN_POINT('Ctrl Pts',(-0.130338140694001,7.9099353379086,
104.144327402964));
#233279=CARTESIAN_POINT('Ctrl Pts',(-0.101912637977869,7.91036058629731,
104.143191168144));
#233280=CARTESIAN_POINT('Ctrl Pts',(-0.0854884000907424,7.91055513391577,
104.14253555087));
#233281=CARTESIAN_POINT('Ctrl Pts',(-0.0365220996372178,7.91098262979195,
104.140583510531));
#233282=CARTESIAN_POINT('Ctrl Pts',(-0.00397896140958066,7.91106593422137,
104.139289557121));
#233283=CARTESIAN_POINT('Ctrl Pts',(0.265172390769217,7.91009411696947,
104.128614061184));
#233284=CARTESIAN_POINT('Ctrl Pts',(0.501628880047005,7.89862519981647,
104.119409741103));
#233285=CARTESIAN_POINT('Ctrl Pts',(0.869731726890195,7.86417193643272,
104.105280080266));
#233286=CARTESIAN_POINT('Ctrl Pts',(1.00190843403903,7.84842748188554,104.100245908461));
#233287=CARTESIAN_POINT('Ctrl Pts',(1.55519146677457,7.768316618034,104.079271341737));
#233288=CARTESIAN_POINT('Ctrl Pts',(1.97113404522159,7.6733301071319,104.063783212418));
#233289=CARTESIAN_POINT('Ctrl Pts',(2.73437620430371,7.43284509590422,104.034220593727));
#233290=CARTESIAN_POINT('Ctrl Pts',(3.08289374782533,7.29518540987065,104.020225438879));
#233291=CARTESIAN_POINT('Ctrl Pts',(3.43990939998329,7.12400278452517,104.004411689016));
#233292=CARTESIAN_POINT('Ctrl Pts',(3.45944719899067,7.11453564331709,104.003541369252));
#233293=CARTESIAN_POINT('Ctrl Pts',(3.48671095917665,7.10118598856891,104.002319750827));
#233294=CARTESIAN_POINT('Ctrl Pts',(3.49446999995576,7.09737100451646,104.001971276511));
#233295=CARTESIAN_POINT('Ctrl Pts',(3.50756641124125,7.09090504702358,104.001381697063));
#233296=CARTESIAN_POINT('Ctrl Pts',(3.5129070788213,7.0882607436867,104.001140876701));
#233297=CARTESIAN_POINT('Ctrl Pts',(3.52356175478686,7.08297033742241,104.000659647086));
#233298=CARTESIAN_POINT('Ctrl Pts',(3.52887578287247,7.08032428278593,104.000419240006));
#233299=CARTESIAN_POINT('Ctrl Pts',(3.54163519371704,7.07395295899538,103.999841048));
#233300=CARTESIAN_POINT('Ctrl Pts',(3.54907767468588,7.07022191800212,103.999503009955));
#233301=CARTESIAN_POINT('Ctrl Pts',(3.57385322992119,7.05775253784545,103.998375057308));
#233302=CARTESIAN_POINT('Ctrl Pts',(3.59115994348341,7.04896219635039,103.997582817923));
#233303=CARTESIAN_POINT('Ctrl Pts',(3.83329365681737,6.92485564972529,103.986436202659));
#233304=CARTESIAN_POINT('Ctrl Pts',(4.05245611547913,6.79892076316857,103.975505902935));
#233305=CARTESIAN_POINT('Ctrl Pts',(4.56722792948259,6.46938632805474,103.94820276911));
#233306=CARTESIAN_POINT('Ctrl Pts',(4.85575974172369,6.25572683493918,103.931573477293));
#233307=CARTESIAN_POINT('Ctrl Pts',(5.15286335876065,6.0027426646834,103.913640516303));
#233308=CARTESIAN_POINT('Ctrl Pts',(5.17680861947608,5.98210438037257,103.912188917948));
#233309=CARTESIAN_POINT('Ctrl Pts',(5.22640822618295,5.93883392210798,103.90916967635));
#233310=CARTESIAN_POINT('Ctrl Pts',(5.25204079594768,5.91617771809421,103.907602331527));
#233311=CARTESIAN_POINT('Ctrl Pts',(5.30532414013013,5.86846225314133,103.904330296113));
#233312=CARTESIAN_POINT('Ctrl Pts',(5.33294623210903,5.84337213905091,103.9026260946));
#233313=CARTESIAN_POINT('Ctrl Pts',(5.43364752316816,5.75059282155087,103.896385459182));
#233314=CARTESIAN_POINT('Ctrl Pts',(5.50562483596642,5.68171971596473,103.891870968999));
#233315=CARTESIAN_POINT('Ctrl Pts',(5.76890783400206,5.42008925136928,103.875182903006));
#233316=CARTESIAN_POINT('Ctrl Pts',(5.95155836003378,5.21887302516532,103.8632588778));
#233317=CARTESIAN_POINT('Ctrl Pts',(6.1926277985352,4.92414461470119,103.847130175559));
#233318=CARTESIAN_POINT('Ctrl Pts',(6.25999151387548,4.83821731243413,103.842574098278));
#233319=CARTESIAN_POINT('Ctrl Pts',(6.36208009351487,4.70229268679639,103.835591715106));
#233320=CARTESIAN_POINT('Ctrl Pts',(6.39804167997069,4.65324429973269,103.833116142368));
#233321=CARTESIAN_POINT('Ctrl Pts',(6.44159415716992,4.59238307454727,103.830097668308));
#233322=CARTESIAN_POINT('Ctrl Pts',(6.44972335417145,4.58095909678863,103.829533367071));
#233323=CARTESIAN_POINT('Ctrl Pts',(6.4624351487452,4.56299427224818,103.828649539093));
#233324=CARTESIAN_POINT('Ctrl Pts',(6.46703826642925,4.55646802264023,103.828329198393));
#233325=CARTESIAN_POINT('Ctrl Pts',(6.47518844514143,4.54487555909633,103.827761484695));
#233326=CARTESIAN_POINT('Ctrl Pts',(6.47873945917347,4.5398121401828,103.82751395516));
#233327=CARTESIAN_POINT('Ctrl Pts',(6.48690492084252,4.52813985185878,103.826944355564));
#233328=CARTESIAN_POINT('Ctrl Pts',(6.49151521651011,4.52152807846796,103.826622449939));
#233329=CARTESIAN_POINT('Ctrl Pts',(6.50409138720802,4.50343330588449,103.825743503475));
#233330=CARTESIAN_POINT('Ctrl Pts',(6.51203696916498,4.49193620041532,103.825187264728));
#233331=CARTESIAN_POINT('Ctrl Pts',(6.5503517340364,4.43618014658881,103.822500473582));
#233332=CARTESIAN_POINT('Ctrl Pts',(6.58030075290248,4.3916334413438,103.820386491526));
#233333=CARTESIAN_POINT('Ctrl Pts',(7.05923587615508,3.66335659088304,103.786343125768));
#233334=CARTESIAN_POINT('Ctrl Pts',(7.39993753790598,2.91443620786812,103.759385090456));
#233335=CARTESIAN_POINT('Ctrl Pts',(7.71172542169029,1.79724950940332,103.72018394223));
#233336=CARTESIAN_POINT('Ctrl Pts',(7.78218057985076,1.46234420252986,103.708445527195));
#233337=CARTESIAN_POINT('Ctrl Pts',(7.85067348193007,0.985145992251968,
103.690557359683));
#233338=CARTESIAN_POINT('Ctrl Pts',(7.86690185332629,0.845835671858197,
103.685196374146));
#233339=CARTESIAN_POINT('Ctrl Pts',(7.88075095986239,0.691308964782714,
103.679028342368));
#233340=CARTESIAN_POINT('Ctrl Pts',(7.88204121753958,0.67643921777803,103.678432544102));
#233341=CARTESIAN_POINT('Ctrl Pts',(7.88421951830941,0.650482359094225,
103.677388430876));
#233342=CARTESIAN_POINT('Ctrl Pts',(7.88512627787465,0.639396818784932,
103.676941218081));
#233343=CARTESIAN_POINT('Ctrl Pts',(7.88640790162829,0.623310959897841,
103.676290355448));
#233344=CARTESIAN_POINT('Ctrl Pts',(7.88680139831528,0.618312095057415,
103.676087822521));
#233345=CARTESIAN_POINT('Ctrl Pts',(7.88748295600495,0.609547278036952,
103.675732230945));
#233346=CARTESIAN_POINT('Ctrl Pts',(7.88777307362143,0.605781482372149,
103.675579296627));
#233347=CARTESIAN_POINT('Ctrl Pts',(7.88832632982372,0.598532302763836,
103.675284597));
#233348=CARTESIAN_POINT('Ctrl Pts',(7.88858985826301,0.595048948634216,
103.67514285544));
#233349=CARTESIAN_POINT('Ctrl Pts',(7.88920743610251,0.586813207691831,
103.674807416396));
#233350=CARTESIAN_POINT('Ctrl Pts',(7.88955949643506,0.582060703364394,
103.674613597783));
#233351=CARTESIAN_POINT('Ctrl Pts',(7.89060365468852,0.567790481269341,
103.674030874639));
#233352=CARTESIAN_POINT('Ctrl Pts',(7.89128282285799,0.558271863926252,
103.673641183815));
#233353=CARTESIAN_POINT('Ctrl Pts',(7.89769805773642,0.466010384051799,
103.669854506698));
#233354=CARTESIAN_POINT('Ctrl Pts',(7.90214955815526,0.383186204922131,
103.666381108505));
#233355=CARTESIAN_POINT('Ctrl Pts',(7.90865809644378,0.211857040404911,
103.659067299869));
#233356=CARTESIAN_POINT('Ctrl Pts',(7.91053339141874,0.123356217289581,
103.655218422766));
#233357=CARTESIAN_POINT('Ctrl Pts',(7.91121929855272,-0.0323641323097026,
103.648345580546));
#233358=CARTESIAN_POINT('Ctrl Pts',(7.91065882071714,-0.0995735600014991,
103.645346260282));
#233359=CARTESIAN_POINT('Ctrl Pts',(7.8961248419811,-0.788878025552247,
103.614305342894));
#233360=CARTESIAN_POINT('Ctrl Pts',(7.80965904895405,-1.40727843097387,
103.584347076154));
#233361=CARTESIAN_POINT('Ctrl Pts',(7.55285147873897,-2.3852765581267,103.538585254946));
#233362=CARTESIAN_POINT('Ctrl Pts',(7.42649934882145,-2.7535935370278,103.521697350389));
#233363=CARTESIAN_POINT('Ctrl Pts',(7.25336652174135,-3.15835874717134,
103.503695342208));
#233364=CARTESIAN_POINT('Ctrl Pts',(7.23272041880199,-3.20535666629566,
103.501613199467));
#233365=CARTESIAN_POINT('Ctrl Pts',(7.20632040626865,-3.26389847753996,
103.499029364916));
#233366=CARTESIAN_POINT('Ctrl Pts',(7.20099403039541,-3.27563307558965,
103.498511931872));
#233367=CARTESIAN_POINT('Ctrl Pts',(7.19250900617055,-3.29420581194,103.497693742401));
#233368=CARTESIAN_POINT('Ctrl Pts',(7.18936923592317,-3.3010525177982,103.497392288688));
#233369=CARTESIAN_POINT('Ctrl Pts',(7.18346023549913,-3.31388949674716,
103.496827397877));
#233370=CARTESIAN_POINT('Ctrl Pts',(7.18069328030043,-3.31988080602141,
103.496563876918));
#233371=CARTESIAN_POINT('Ctrl Pts',(7.1744874467493,-3.33327429027718,103.495975060171));
#233372=CARTESIAN_POINT('Ctrl Pts',(7.1710446009528,-3.34067462490496,103.495649911749));
#233373=CARTESIAN_POINT('Ctrl Pts',(7.16231902368869,-3.35935445233318,
103.494829656243));
#233374=CARTESIAN_POINT('Ctrl Pts',(7.15702108632424,-3.37062684160759,
103.494335113704));
#233375=CARTESIAN_POINT('Ctrl Pts',(7.1284459263344,-3.43105490744321,103.491686348234));
#233376=CARTESIAN_POINT('Ctrl Pts',(7.1046885926265,-3.47998265277427,103.489550005416));
#233377=CARTESIAN_POINT('Ctrl Pts',(6.6913439719332,-4.30937826213792,103.453465180375));
#233378=CARTESIAN_POINT('Ctrl Pts',(6.17591090397008,-5.0202366280083,103.425449145322));
#233379=CARTESIAN_POINT('Ctrl Pts',(5.31291829388461,-5.87131380340866,
103.383204681555));
#233380=CARTESIAN_POINT('Ctrl Pts',(5.05583059861422,-6.09409204115545,
103.370916884798));
#233381=CARTESIAN_POINT('Ctrl Pts',(4.77700366462205,-6.30589122877165,
103.356925986993));
#233382=CARTESIAN_POINT('Ctrl Pts',(4.76874656532475,-6.31213786245352,
103.356511089101));
#233383=CARTESIAN_POINT('Ctrl Pts',(4.75380217986812,-6.32339747957587,
103.355759084553));
#233384=CARTESIAN_POINT('Ctrl Pts',(4.74711917306056,-6.32841610555495,
103.355422401079));
#233385=CARTESIAN_POINT('Ctrl Pts',(4.73677481239256,-6.33615863138277,
103.354900670716));
#233386=CARTESIAN_POINT('Ctrl Pts',(4.73311900186257,-6.33888999268804,
103.354716171604));
#233387=CARTESIAN_POINT('Ctrl Pts',(4.72664529908826,-6.34371795975544,
103.354389262554));
#233388=CARTESIAN_POINT('Ctrl Pts',(4.72382836705896,-6.3458158573037,103.354246946765));
#233389=CARTESIAN_POINT('Ctrl Pts',(4.7179254964359,-6.350205885402,103.353948587294));
#233390=CARTESIAN_POINT('Ctrl Pts',(4.71483928317156,-6.35249764350017,
103.35379251677));
#233391=CARTESIAN_POINT('Ctrl Pts',(4.70627433926906,-6.35884811371101,
103.353359170894));
#233392=CARTESIAN_POINT('Ctrl Pts',(4.70079204118598,-6.36290198531067,
103.353081549041));
#233393=CARTESIAN_POINT('Ctrl Pts',(4.67910162181106,-6.37889757883909,
103.351982214688));
#233394=CARTESIAN_POINT('Ctrl Pts',(4.6628533061964,-6.39078440719886,103.351156634531));
#233395=CARTESIAN_POINT('Ctrl Pts',(4.58430860231699,-6.44778658794271,
103.347156532625));
#233396=CARTESIAN_POINT('Ctrl Pts',(4.52140358945253,-6.49205253341382,
103.343925065604));
#233397=CARTESIAN_POINT('Ctrl Pts',(3.7799890484064,-6.99777975226504,103.305611214986));
#233398=CARTESIAN_POINT('Ctrl Pts',(3.03429820035792,-7.35189984798089,
103.265416322383));
#233399=CARTESIAN_POINT('Ctrl Pts',(1.85212738361698,-7.70217831327837,
103.209768699113));
#233400=CARTESIAN_POINT('Ctrl Pts',(1.44821630912633,-7.78823878177506,
103.191934582948));
#233401=CARTESIAN_POINT('Ctrl Pts',(1.0029135740568,-7.84725681012048,103.173630553383));
#233402=CARTESIAN_POINT('Ctrl Pts',(0.966401122414857,-7.85183698247721,
103.17213913985));
#233403=CARTESIAN_POINT('Ctrl Pts',(0.917869532185374,-7.85758119600065,
103.170169068317));
#233404=CARTESIAN_POINT('Ctrl Pts',(0.905878083954368,-7.85897268277096,
103.169683286687));
#233405=CARTESIAN_POINT('Ctrl Pts',(0.886165495587429,-7.861214413295,103.168886339391));
#233406=CARTESIAN_POINT('Ctrl Pts',(0.878446225545652,-7.86208074027702,
103.168574670828));
#233407=CARTESIAN_POINT('Ctrl Pts',(0.863473223257752,-7.86373882042247,
103.167970918973));
#233408=CARTESIAN_POINT('Ctrl Pts',(0.856219648621964,-7.86453190957875,
103.167678794207));
#233409=CARTESIAN_POINT('Ctrl Pts',(0.839452891192355,-7.86634167687495,
103.167004368767));
#233410=CARTESIAN_POINT('Ctrl Pts',(0.829938931949276,-7.86735113643263,
103.166622293782));
#233411=CARTESIAN_POINT('Ctrl Pts',(0.799407250082365,-7.87053463991475,
103.16539811773));
#233412=CARTESIAN_POINT('Ctrl Pts',(0.778382560432509,-7.87264174645171,
103.164558103741));
#233413=CARTESIAN_POINT('Ctrl Pts',(0.588071873843842,-7.89094496635586,
103.156981022727));
#233414=CARTESIAN_POINT('Ctrl Pts',(0.418308055782274,-7.90176331958711,
103.150413222566));
#233415=CARTESIAN_POINT('Ctrl Pts',(-0.403606746036275,-7.92757536723379,
103.11938390534));
#233416=CARTESIAN_POINT('Ctrl Pts',(-1.05553335628941,-7.86735086313065,
103.097339395148));
#233417=CARTESIAN_POINT('Ctrl Pts',(-2.12828068574673,-7.63237771293475,
103.058986557528));
#233418=CARTESIAN_POINT('Ctrl Pts',(-2.55503929820115,-7.50030469541763,
103.042958264038));
#233419=CARTESIAN_POINT('Ctrl Pts',(-2.98617108620706,-7.3257812154942,
103.024393920752));
#233420=CARTESIAN_POINT('Ctrl Pts',(-3.00390650107437,-7.31852675739403,
103.023626608601));
#233421=CARTESIAN_POINT('Ctrl Pts',(-3.02986154852273,-7.3077999160061,
103.02249849452));
#233422=CARTESIAN_POINT('Ctrl Pts',(-3.03810201411643,-7.30437791784378,
103.022139561492));
#233423=CARTESIAN_POINT('Ctrl Pts',(-3.0526018685897,-7.29832781661137,
103.021506650064));
#233424=CARTESIAN_POINT('Ctrl Pts',(-3.05886370532628,-7.29570558059861,
103.021232884531));
#233425=CARTESIAN_POINT('Ctrl Pts',(-3.07105377248945,-7.29058235845154,
103.020699090741));
#233426=CARTESIAN_POINT('Ctrl Pts',(-3.0769823432685,-7.28808219340441,
103.020439091882));
#233427=CARTESIAN_POINT('Ctrl Pts',(-3.09283884890406,-7.28137247632975,
103.019742663581));
#233428=CARTESIAN_POINT('Ctrl Pts',(-3.1027612219825,-7.27714985983386,
103.019305776717));
#233429=CARTESIAN_POINT('Ctrl Pts',(-3.13865286153165,-7.26178887611833,
103.017721565155));
#233430=CARTESIAN_POINT('Ctrl Pts',(-3.16457089638142,-7.25053173824833,
103.016570200961));
#233431=CARTESIAN_POINT('Ctrl Pts',(-3.19779651205155,-7.23588856398032,
103.015085105061));
#233432=CARTESIAN_POINT('Ctrl Pts',(-3.2051601592962,-7.23262982570161,
103.014755392923));
#233433=CARTESIAN_POINT('Ctrl Pts',(-3.2619736801147,-7.20738353728301,
103.012207127141));
#233434=CARTESIAN_POINT('Ctrl Pts',(-3.31120122605761,-7.18490055991174,
103.009973350813));
#233435=CARTESIAN_POINT('Ctrl Pts',(-3.94319510893822,-6.88838461801055,
102.980987952697));
#233436=CARTESIAN_POINT('Ctrl Pts',(-4.49062304349641,-6.54469026475956,
102.952760980972));
#233437=CARTESIAN_POINT('Ctrl Pts',(-5.50682005398615,-5.71855902207885,
102.897065596));
#233438=CARTESIAN_POINT('Ctrl Pts',(-5.96826747919322,-5.23515192693193,
102.869623944422));
#233439=CARTESIAN_POINT('Ctrl Pts',(-6.39728147384622,-4.65423489949048,
102.840338928498));
#233440=CARTESIAN_POINT('Ctrl Pts',(-6.43035613571116,-4.60843061997615,
102.838053873666));
#233441=CARTESIAN_POINT('Ctrl Pts',(-6.47808662648472,-4.54081542283715,
102.834715548258));
#233442=CARTESIAN_POINT('Ctrl Pts',(-6.4931288398232,-4.51927969037552,
102.833657374142));
#233443=CARTESIAN_POINT('Ctrl Pts',(-6.51949723061543,-4.48112500449891,
102.831791550131));
#233444=CARTESIAN_POINT('Ctrl Pts',(-6.53086780992325,-4.46453705303625,
102.830983328874));
#233445=CARTESIAN_POINT('Ctrl Pts',(-6.55297129153682,-4.43202628305051,
102.82940503384));
#233446=CARTESIAN_POINT('Ctrl Pts',(-6.56370971706843,-4.41610738929351,
102.82863489187));
#233447=CARTESIAN_POINT('Ctrl Pts',(-6.59258900098856,-4.3729580197519,
102.826554531845));
#233448=CARTESIAN_POINT('Ctrl Pts',(-6.61061908642994,-4.34565379250885,
102.825245792869));
#233449=CARTESIAN_POINT('Ctrl Pts',(-6.67781929904982,-4.24250172548014,
102.82033002271));
#233450=CARTESIAN_POINT('Ctrl Pts',(-6.72585796795107,-4.16592442597223,
102.816738317277));
#233451=CARTESIAN_POINT('Ctrl Pts',(-7.07466814903248,-3.58812826170221,
102.790045765497));
#233452=CARTESIAN_POINT('Ctrl Pts',(-7.32036832004342,-3.05578212128145,
102.767863114709));
#233453=CARTESIAN_POINT('Ctrl Pts',(-7.58488708107624,-2.2620704651583,
102.735557422931));
#233454=CARTESIAN_POINT('Ctrl Pts',(-7.65311370151086,-2.01923700958277,
102.725745559407));
#233455=CARTESIAN_POINT('Ctrl Pts',(-7.71488270195008,-1.75072989100462,
102.714720533781));
#233456=CARTESIAN_POINT('Ctrl Pts',(-7.72003533668219,-1.72786708207051,
102.71378035885));
#233457=CARTESIAN_POINT('Ctrl Pts',(-7.72770188568035,-1.6931307839507,
102.712349521941));
#233458=CARTESIAN_POINT('Ctrl Pts',(-7.73029018825794,-1.68127388892119,
102.711860708968));
#233459=CARTESIAN_POINT('Ctrl Pts',(-7.73497830944983,-1.65955812141931,
102.710964733365));
#233460=CARTESIAN_POINT('Ctrl Pts',(-7.73708659056542,-1.64970109274918,
102.710557768769));
#233461=CARTESIAN_POINT('Ctrl Pts',(-7.74162646825939,-1.62827527626141,
102.709672598544));
#233462=CARTESIAN_POINT('Ctrl Pts',(-7.74405098329987,-1.61670501832905,
102.709194234072));
#233463=CARTESIAN_POINT('Ctrl Pts',(-7.75061729057285,-1.58501563038258,
102.707883116761));
#233464=CARTESIAN_POINT('Ctrl Pts',(-7.75470666316061,-1.56488577739826,
102.707049226575));
#233465=CARTESIAN_POINT('Ctrl Pts',(-7.77465135531449,-1.46471021113542,
102.70289464383));
#233466=CARTESIAN_POINT('Ctrl Pts',(-7.78934576149673,-1.38443924166108,
102.699550520324));
#233467=CARTESIAN_POINT('Ctrl Pts',(-7.87480650209391,-0.87304733133862,
102.678180618591));
#233468=CARTESIAN_POINT('Ctrl Pts',(-7.91099794134262,-0.436916952793712,
102.659700643657));
#233469=CARTESIAN_POINT('Ctrl Pts',(-7.91100187939347,0.39883330248103,
102.62470123059));
#233470=CARTESIAN_POINT('Ctrl Pts',(-7.88083747844167,0.797143536104756,
102.60819774669));
#233471=CARTESIAN_POINT('Ctrl Pts',(-7.81323238038289,1.24089423252288,
102.589989098022));
#233472=CARTESIAN_POINT('Ctrl Pts',(-7.80523718402587,1.29022915286847,
102.587966737174));
#233473=CARTESIAN_POINT('Ctrl Pts',(-7.79151592948249,1.37009680287536,
102.584695328422));
#233474=CARTESIAN_POINT('Ctrl Pts',(-7.78607661021762,1.40067724967215,
102.58344335199));
#233475=CARTESIAN_POINT('Ctrl Pts',(-7.77607457087018,1.45505056163304,
102.581218151917));
#233476=CARTESIAN_POINT('Ctrl Pts',(-7.77158239377341,1.47885596653092,
102.580244223992));
#233477=CARTESIAN_POINT('Ctrl Pts',(-7.76187149030842,1.52905054522422,
102.578191150712));
#233478=CARTESIAN_POINT('Ctrl Pts',(-7.75662736691001,1.55543450474728,
102.577112272865));
#233479=CARTESIAN_POINT('Ctrl Pts',(-7.74229560252635,1.62566442327177,
102.574240982736));
#233480=CARTESIAN_POINT('Ctrl Pts',(-7.73297008100907,1.66946092060796,
102.572450935911));
#233481=CARTESIAN_POINT('Ctrl Pts',(-7.68295317455581,1.89494518442984,
102.563235249841));
#233482=CARTESIAN_POINT('Ctrl Pts',(-7.6362284295309,2.07523569441124,102.555867671847));
#233483=CARTESIAN_POINT('Ctrl Pts',(-7.49972722740747,2.53452890355054,
102.53699703844));
#233484=CARTESIAN_POINT('Ctrl Pts',(-7.40073267581886,2.81049976478382,
102.525589659905));
#233485=CARTESIAN_POINT('Ctrl Pts',(-7.02146138931647,3.70767714527854,
102.488296404378));
#233486=CARTESIAN_POINT('Ctrl Pts',(-6.67638465996493,4.29809312752179,
102.463720830186));
#233487=CARTESIAN_POINT('Ctrl Pts',(-6.23457465709597,4.86987961159506,
102.436319917697));
#233488=CARTESIAN_POINT('Ctrl Pts',(-6.20890253554617,4.90256849530669,
102.434738169464));
#233489=CARTESIAN_POINT('Ctrl Pts',(-6.10195314371166,5.03656204672705,
102.428185914335));
#233490=CARTESIAN_POINT('Ctrl Pts',(-6.01844655447808,5.13605770748313,
102.423157561885));
#233491=CARTESIAN_POINT('Ctrl Pts',(-5.90440814510291,5.26532930148985,
102.416347424745));
#233492=CARTESIAN_POINT('Ctrl Pts',(-5.87602907808068,5.29698125276088,
102.414657098464));
#233493=CARTESIAN_POINT('Ctrl Pts',(-5.83945024768144,5.33712291348064,
102.412481937956));
#233494=CARTESIAN_POINT('Ctrl Pts',(-5.83148442588626,5.3458254346334,102.412008462973));
#233495=CARTESIAN_POINT('Ctrl Pts',(-5.81877741454235,5.35964542362705,
102.411253462516));
#233496=CARTESIAN_POINT('Ctrl Pts',(-5.8140488545878,5.36477451372134,102.410972572135));
#233497=CARTESIAN_POINT('Ctrl Pts',(-5.80520351071806,5.37434366795355,
102.410447234914));
#233498=CARTESIAN_POINT('Ctrl Pts',(-5.80108839944702,5.37878527584707,
102.410202873932));
#233499=CARTESIAN_POINT('Ctrl Pts',(-5.7919210052747,5.38865726162878,102.409658582466));
#233500=CARTESIAN_POINT('Ctrl Pts',(-5.78686618005038,5.39408526335588,
102.40935851925));
#233501=CARTESIAN_POINT('Ctrl Pts',(-5.77215563246439,5.4098373519546,102.408485408739));
#233502=CARTESIAN_POINT('Ctrl Pts',(-5.76247989330666,5.42014264533532,
102.407911293879));
#233503=CARTESIAN_POINT('Ctrl Pts',(-5.69327704984363,5.49345343175236,
102.403805859608));
#233504=CARTESIAN_POINT('Ctrl Pts',(-5.63274766968862,5.55550067434415,
102.400217473694));
#233505=CARTESIAN_POINT('Ctrl Pts',(-5.50115260115514,5.6860335944813,102.392401707212));
#233506=CARTESIAN_POINT('Ctrl Pts',(-5.42980399486493,5.75420588246586,
102.388160238178));
#233507=CARTESIAN_POINT('Ctrl Pts',(-5.2009692151596,5.96480698302112,102.374591413487));
#233508=CARTESIAN_POINT('Ctrl Pts',(-5.03901820523858,6.1022365583234,102.365039929599));
#233509=CARTESIAN_POINT('Ctrl Pts',(-4.72998454330482,6.34377959355142,
102.347158727323));
#233510=CARTESIAN_POINT('Ctrl Pts',(-4.58448810909778,6.44971013081252,
102.338869827913));
#233511=CARTESIAN_POINT('Ctrl Pts',(-4.21505235557019,6.69986107379129,
102.318311539271));
#233512=CARTESIAN_POINT('Ctrl Pts',(-3.98719583838662,6.83791494789822,
102.30605718336));
#233513=CARTESIAN_POINT('Ctrl Pts',(-3.34039932236877,7.18645409918913,
102.272862972789));
#233514=CARTESIAN_POINT('Ctrl Pts',(-2.90903097865722,7.37163620290902,
102.252513452378));
#233515=CARTESIAN_POINT('Ctrl Pts',(-2.43382828036063,7.52737624484211,
102.232159260673));
#233516=CARTESIAN_POINT('Ctrl Pts',(-2.40383661911475,7.53700754725137,
102.230882760506));
#233517=CARTESIAN_POINT('Ctrl Pts',(-2.36232313823307,7.55006588313637,
102.229126958453));
#233518=CARTESIAN_POINT('Ctrl Pts',(-2.35085002852569,7.55364611257992,
102.228642872158));
#233519=CARTESIAN_POINT('Ctrl Pts',(-2.33252782886062,7.55931784029084,
102.227871652406));
#233520=CARTESIAN_POINT('Ctrl Pts',(-2.32568400180237,7.56142620191684,
102.227583992884));
#233521=CARTESIAN_POINT('Ctrl Pts',(-2.31161823966552,7.56573850509155,
102.226993623821));
#233522=CARTESIAN_POINT('Ctrl Pts',(-2.30439599164131,7.56794140618736,
102.226690946953));
#233523=CARTESIAN_POINT('Ctrl Pts',(-2.2876884973557,7.57301132498179,102.225991803485));
#233524=CARTESIAN_POINT('Ctrl Pts',(-2.27820098751611,7.57587087077092,
102.225595570017));
#233525=CARTESIAN_POINT('Ctrl Pts',(-2.24838926943168,7.58479508919877,
102.224352965685));
#233526=CARTESIAN_POINT('Ctrl Pts',(-2.22804595622366,7.59079587905936,
102.223508583431));
#233527=CARTESIAN_POINT('Ctrl Pts',(-1.93967888770246,7.67459813288947,
102.21158930663));
#233528=CARTESIAN_POINT('Ctrl Pts',(-1.66773477143276,7.73824839675354,
102.200967327439));
#233529=CARTESIAN_POINT('Ctrl Pts',(-1.04120858234931,7.85031891247838,
102.177558147338));
#233530=CARTESIAN_POINT('Ctrl Pts',(-0.685569232694082,7.88933668721038,
102.165033497741));
#233531=CARTESIAN_POINT('Ctrl Pts',(0.200288488043677,7.92615338159678,
102.134329103512));
#233532=CARTESIAN_POINT('Ctrl Pts',(0.729912487050044,7.89500940809927,
102.1164249202));
#233533=CARTESIAN_POINT('Ctrl Pts',(1.25961206677603,7.81008012785519,102.096281326143));
#233534=CARTESIAN_POINT('Ctrl Pts',(1.2668097509104,7.80891587974101,102.096007175324));
#233535=CARTESIAN_POINT('Ctrl Pts',(1.4124556869612,7.78515052287668,102.090450744091));
#233536=CARTESIAN_POINT('Ctrl Pts',(1.55027814469175,7.75888119596976,102.085026916877));
#233537=CARTESIAN_POINT('Ctrl Pts',(1.70170778145885,7.72582216769708,102.078829765815));
#233538=CARTESIAN_POINT('Ctrl Pts',(1.71607562164115,7.72264345912536,102.078239515518));
#233539=CARTESIAN_POINT('Ctrl Pts',(1.7370121538997,7.71795019533945,102.077376206797));
#233540=CARTESIAN_POINT('Ctrl Pts',(1.74358796998982,7.71646728957164,102.077104593953));
#233541=CARTESIAN_POINT('Ctrl Pts',(1.75520785429415,7.71383128934848,102.07662382984));
#233542=CARTESIAN_POINT('Ctrl Pts',(1.76025270800759,7.71268164622881,102.076414833685));
#233543=CARTESIAN_POINT('Ctrl Pts',(1.77069669266934,7.71029084494988,102.07598161241));
#233544=CARTESIAN_POINT('Ctrl Pts',(1.77609565399494,7.70904896331476,102.075757355286));
#233545=CARTESIAN_POINT('Ctrl Pts',(1.78994617449935,7.70584771199722,102.075181268141));
#233546=CARTESIAN_POINT('Ctrl Pts',(1.79839580930444,7.70388011201673,102.07482907832));
#233547=CARTESIAN_POINT('Ctrl Pts',(1.83308879923478,7.69574124130955,102.073380033605));
#233548=CARTESIAN_POINT('Ctrl Pts',(1.85930356880884,7.68944978614791,102.072278040451));
#233549=CARTESIAN_POINT('Ctrl Pts',(2.28203767147829,7.58570691828012,102.054398901662));
#233550=CARTESIAN_POINT('Ctrl Pts',(2.67044368233444,7.45783788462449,102.036466466933));
#233551=CARTESIAN_POINT('Ctrl Pts',(3.44286892389733,7.13543148933909,101.999609686033));
#233552=CARTESIAN_POINT('Ctrl Pts',(3.82445678386896,6.93839271341209,101.980754192444));
#233553=CARTESIAN_POINT('Ctrl Pts',(4.42631998245801,6.56280349170204,101.950621160848));
#233554=CARTESIAN_POINT('Ctrl Pts',(4.65636340831698,6.4016397219293,101.938981919964));
#233555=CARTESIAN_POINT('Ctrl Pts',(4.90521568994917,6.20677302409815,101.926188403912));
#233556=CARTESIAN_POINT('Ctrl Pts',(4.93292050130342,6.18477709298296,101.924760940064));
#233557=CARTESIAN_POINT('Ctrl Pts',(4.97332711524278,6.15225247519126,101.922673985416));
#233558=CARTESIAN_POINT('Ctrl Pts',(4.98614488966889,6.14186879177211,101.922011209933));
#233559=CARTESIAN_POINT('Ctrl Pts',(5.00886148136085,6.12334809181335,101.920835198596));
#233560=CARTESIAN_POINT('Ctrl Pts',(5.01877317113523,6.11522698276815,101.920321607922));
#233561=CARTESIAN_POINT('Ctrl Pts',(5.03836342062967,6.0990960700042,101.919305537106));
#233562=CARTESIAN_POINT('Ctrl Pts',(5.04804271775977,6.09108722234195,101.91880303773));
#233563=CARTESIAN_POINT('Ctrl Pts',(5.07361051612564,6.06982910104522,101.917474401017));
#233564=CARTESIAN_POINT('Ctrl Pts',(5.08946621847528,6.05654048122313,101.916649133686));
#233565=CARTESIAN_POINT('Ctrl Pts',(5.12366176531408,6.02765217987515,101.914866288702));
#233566=CARTESIAN_POINT('Ctrl Pts',(5.14198291557133,6.01203063773482,101.913909181455));
#233567=CARTESIAN_POINT('Ctrl Pts',(5.19371847814885,5.9675087845616,101.911200850268));
#233568=CARTESIAN_POINT('Ctrl Pts',(5.22696265822815,5.93841175193622,101.909453864303));
#233569=CARTESIAN_POINT('Ctrl Pts',(5.52036923748019,5.67723431109448,101.893974210245));
#233570=CARTESIAN_POINT('Ctrl Pts',(5.76517584834386,5.42846488015547,101.880649165779));
#233571=CARTESIAN_POINT('Ctrl Pts',(6.45725438298539,4.6253671540124,101.840972210185));
#233572=CARTESIAN_POINT('Ctrl Pts',(6.84685192552972,4.02624094089903,101.815902131309));
#233573=CARTESIAN_POINT('Ctrl Pts',(7.18517506317434,3.31112301665101,101.784986786309));
#233574=CARTESIAN_POINT('Ctrl Pts',(7.21817601057139,3.23855073962787,101.781835454439));
#233575=CARTESIAN_POINT('Ctrl Pts',(7.2553048004979,3.1535129856508,101.778115831283));
#233576=CARTESIAN_POINT('Ctrl Pts',(7.26050601423933,3.14151942751638,101.777590602707));
#233577=CARTESIAN_POINT('Ctrl Pts',(7.26874780859433,3.12238475129894,101.776751592231));
#233578=CARTESIAN_POINT('Ctrl Pts',(7.27180766180947,3.11525192708304,101.776438601797));
#233579=CARTESIAN_POINT('Ctrl Pts',(7.27718527533521,3.10266507810156,101.775885861194));
#233580=CARTESIAN_POINT('Ctrl Pts',(7.27950741625484,3.0972129237221,101.775646293822));
#233581=CARTESIAN_POINT('Ctrl Pts',(7.28429171179521,3.08594477357375,101.775150873258));
#233582=CARTESIAN_POINT('Ctrl Pts',(7.28675303170178,3.08012842958827,101.774894985129));
#233583=CARTESIAN_POINT('Ctrl Pts',(7.29302770226996,3.06525114409266,101.77424003234));
#233584=CARTESIAN_POINT('Ctrl Pts',(7.29683112650615,3.05618604677874,101.773840544676));
#233585=CARTESIAN_POINT('Ctrl Pts',(7.31220815353637,3.01934403891531,101.772215231213));
#233586=CARTESIAN_POINT('Ctrl Pts',(7.32364002342858,2.99150852884265,101.770983254459));
#233587=CARTESIAN_POINT('Ctrl Pts',(7.39400863805198,2.81734665774431,101.76324690483));
#233588=CARTESIAN_POINT('Ctrl Pts',(7.44870777131684,2.66937232956217,101.756528986003));
#233589=CARTESIAN_POINT('Ctrl Pts',(7.55034841383505,2.36689721658937,101.742578557181));
#233590=CARTESIAN_POINT('Ctrl Pts',(7.59705694754,2.21239364416783,101.735351855512));
#233591=CARTESIAN_POINT('Ctrl Pts',(7.74818226930986,1.65104929743155,101.708985866782));
#233592=CARTESIAN_POINT('Ctrl Pts',(7.82489407101931,1.23747193192573,101.689394229412));
#233593=CARTESIAN_POINT('Ctrl Pts',(7.91789163871733,0.344833207250371,
101.648678974404));
#233594=CARTESIAN_POINT('Ctrl Pts',(7.92427681924457,-0.133634858413372,
101.627825307441));
#233595=CARTESIAN_POINT('Ctrl Pts',(7.88508760549069,-0.640517685923892,
101.607160831464));
#233596=CARTESIAN_POINT('Ctrl Pts',(7.88253435228384,-0.67120910767514,
101.605914841393));
#233597=CARTESIAN_POINT('Ctrl Pts',(7.87879480672726,-0.713191590711058,
101.604217552401));
#233598=CARTESIAN_POINT('Ctrl Pts',(7.87776335400397,-0.724495956737221,
101.603761237555));
#233599=CARTESIAN_POINT('Ctrl Pts',(7.87608884883206,-0.742421509477063,
101.603038761364));
#233600=CARTESIAN_POINT('Ctrl Pts',(7.87546177138539,-0.749044151009626,
101.602772081318));
#233601=CARTESIAN_POINT('Ctrl Pts',(7.87423027473622,-0.761877627958302,
101.60225576882));
#233602=CARTESIAN_POINT('Ctrl Pts',(7.87362685891368,-0.76808855374721,
101.602006103922));
#233603=CARTESIAN_POINT('Ctrl Pts',(7.87217370794623,-0.782864091843354,
101.601412662297));
#233604=CARTESIAN_POINT('Ctrl Pts',(7.87131734290475,-0.791428052501767,
101.601069101744));
#233605=CARTESIAN_POINT('Ctrl Pts',(7.86873647369019,-0.816819093280207,
101.60005167175));
#233606=CARTESIAN_POINT('Ctrl Pts',(7.86697196910218,-0.833642108832534,
101.599379107306));
#233607=CARTESIAN_POINT('Ctrl Pts',(7.85240618867708,-0.968348243311931,
101.594005944533));
#233608=CARTESIAN_POINT('Ctrl Pts',(7.83700965915583,-1.08593850964951,
101.589390895411));
#233609=CARTESIAN_POINT('Ctrl Pts',(7.77286734457607,-1.50278645074296,
101.573273389498));
#233610=CARTESIAN_POINT('Ctrl Pts',(7.70957128178513,-1.79954562662366,
101.562258176574));
#233611=CARTESIAN_POINT('Ctrl Pts',(7.54094529476901,-2.41452676150146,
101.539892668084));
#233612=CARTESIAN_POINT('Ctrl Pts',(7.43212754990713,-2.73116889940196,
101.52864950722));
#233613=CARTESIAN_POINT('Ctrl Pts',(7.11194622163099,-3.50041007324661,
101.500650247815));
#233614=CARTESIAN_POINT('Ctrl Pts',(6.87720564042173,-3.94164935676828,
101.483978674308));
#233615=CARTESIAN_POINT('Ctrl Pts',(6.54343090002309,-4.44735243440443,
101.461005824069));
#233616=CARTESIAN_POINT('Ctrl Pts',(6.48251811389525,-4.53567950711822,
101.456835107277));
#233617=CARTESIAN_POINT('Ctrl Pts',(6.41374667588285,-4.63118591508616,
101.452118980389));
#233618=CARTESIAN_POINT('Ctrl Pts',(6.40764605564784,-4.63962298317432,
101.45170055808));
#233619=CARTESIAN_POINT('Ctrl Pts',(6.39857649093828,-4.65211405052788,
101.451078377201));
#233620=CARTESIAN_POINT('Ctrl Pts',(6.39562028900442,-4.65617733426838,
101.45087555884));
#233621=CARTESIAN_POINT('Ctrl Pts',(6.39055905157771,-4.66312006394169,
101.450528279605));
#233622=CARTESIAN_POINT('Ctrl Pts',(6.38845593314939,-4.66600091219,101.450383961609));
#233623=CARTESIAN_POINT('Ctrl Pts',(6.38436565832623,-4.6715958146759,101.450103258707));
#233624=CARTESIAN_POINT('Ctrl Pts',(6.3823787178263,-4.67431002577608,101.449966890001));
#233625=CARTESIAN_POINT('Ctrl Pts',(6.37762800742196,-4.6807909401577,101.449640808239));
#233626=CARTESIAN_POINT('Ctrl Pts',(6.37486264897097,-4.68455643932611,
101.449450974682));
#233627=CARTESIAN_POINT('Ctrl Pts',(6.36646991971447,-4.69596335369723,
101.448874764895));
#233628=CARTESIAN_POINT('Ctrl Pts',(6.36083217682909,-4.70359703572875,
101.448487602911));
#233629=CARTESIAN_POINT('Ctrl Pts',(6.30634394596092,-4.77709870130758,
101.444744948415));
#233630=CARTESIAN_POINT('Ctrl Pts',(6.25648745007733,-4.84221125115305,
101.441314497804));
#233631=CARTESIAN_POINT('Ctrl Pts',(6.04709338346306,-5.10704623643425,
101.42692937531));
#233632=CARTESIAN_POINT('Ctrl Pts',(5.87894232339324,-5.29974324115202,
101.415433776848));
#233633=CARTESIAN_POINT('Ctrl Pts',(5.38839993552569,-5.80977022876024,
101.382909401637));
#233634=CARTESIAN_POINT('Ctrl Pts',(5.04767316277967,-6.1081341353459,101.361453787479));
#233635=CARTESIAN_POINT('Ctrl Pts',(4.29437812931619,-6.66146616863703,
101.31862644187));
#233636=CARTESIAN_POINT('Ctrl Pts',(3.88007721994675,-6.91100077140361,
101.297469322006));
#233637=CARTESIAN_POINT('Ctrl Pts',(3.4157194414029,-7.13567658226366,101.276513985717));
#233638=CARTESIAN_POINT('Ctrl Pts',(3.3857926746578,-7.14992500596311,101.275174590178));
#233639=CARTESIAN_POINT('Ctrl Pts',(3.34544088367246,-7.168826722035,101.273383388001));
#233640=CARTESIAN_POINT('Ctrl Pts',(3.33509428821022,-7.17364603022635,
101.272925405188));
#233641=CARTESIAN_POINT('Ctrl Pts',(3.31885505554017,-7.1811673245369,101.272208616958));
#233642=CARTESIAN_POINT('Ctrl Pts',(3.31296948657951,-7.18388447874465,
101.271949248665));
#233643=CARTESIAN_POINT('Ctrl Pts',(3.30167254460052,-7.18908303250905,
101.271452205972));
#233644=CARTESIAN_POINT('Ctrl Pts',(3.29626169898942,-7.19156556335742,
101.271214489748));
#233645=CARTESIAN_POINT('Ctrl Pts',(3.283557158442,-7.19737713806493,101.270657156856));
#233646=CARTESIAN_POINT('Ctrl Pts',(3.27626118810353,-7.20070120947605,
101.27033772433));
#233647=CARTESIAN_POINT('Ctrl Pts',(3.25520317792186,-7.21025668709693,
101.269417579976));
#233648=CARTESIAN_POINT('Ctrl Pts',(3.24142828893996,-7.21645978818696,
101.26881791364));
#233649=CARTESIAN_POINT('Ctrl Pts',(3.15046166060022,-7.25711082546121,
101.264872477449));
#233650=CARTESIAN_POINT('Ctrl Pts',(3.07273840968515,-7.29035976228189,
101.261570940128));
#233651=CARTESIAN_POINT('Ctrl Pts',(2.88724006504119,-7.36621975279476,
101.253847458992));
#233652=CARTESIAN_POINT('Ctrl Pts',(2.77903142017497,-7.40772126812446,
101.249465127804));
#233653=CARTESIAN_POINT('Ctrl Pts',(2.44335492168077,-7.52807291845652,
101.236210422009));
#233654=CARTESIAN_POINT('Ctrl Pts',(2.21316579638061,-7.59893223573594,
101.227598202347));
#233655=CARTESIAN_POINT('Ctrl Pts',(1.77359216019747,-7.71257318030026,
101.211741840146));
#233656=CARTESIAN_POINT('Ctrl Pts',(1.56501277292218,-7.75758672043848,
101.204459063132));
#233657=CARTESIAN_POINT('Ctrl Pts',(0.843337834297487,-7.88303692392558,
101.179553616392));
#233658=CARTESIAN_POINT('Ctrl Pts',(0.324348801329683,-7.92137482742682,
101.162206499269));
#233659=CARTESIAN_POINT('Ctrl Pts',(-0.289570996963616,-7.90626944439895,
101.138779869489));
#233660=CARTESIAN_POINT('Ctrl Pts',(-0.384498837347121,-7.90222166003217,
101.135072887155));
#233661=CARTESIAN_POINT('Ctrl Pts',(-0.490500094864129,-7.89578722828145,
101.13081544588));
#233662=CARTESIAN_POINT('Ctrl Pts',(-0.501671496325903,-7.89508530693915,
101.130365281096));
#233663=CARTESIAN_POINT('Ctrl Pts',(-0.517958829930785,-7.89402723258194,
101.129706811677));
#233664=CARTESIAN_POINT('Ctrl Pts',(-0.523075888615181,-7.89368981609708,
101.129499629186));
#233665=CARTESIAN_POINT('Ctrl Pts',(-0.532128305799828,-7.89308406298051,
101.129132568178));
#233666=CARTESIAN_POINT('Ctrl Pts',(-0.536063803374957,-7.89281775779167,
101.128972808994));
#233667=CARTESIAN_POINT('Ctrl Pts',(-0.544220148336621,-7.8922597100486,
101.128641334026));
#233668=CARTESIAN_POINT('Ctrl Pts',(-0.548440963185407,-7.89196752467198,
101.128469592478));
#233669=CARTESIAN_POINT('Ctrl Pts',(-0.559285397234625,-7.8912080783103,
101.128027812686));
#233670=CARTESIAN_POINT('Ctrl Pts',(-0.565908654739779,-7.8907358645897,
101.127757488203));
#233671=CARTESIAN_POINT('Ctrl Pts',(-0.593197575522974,-7.88875573081618,
101.126641640268));
#233672=CARTESIAN_POINT('Ctrl Pts',(-0.61385770409917,-7.88717497255999,
101.12579196133));
#233673=CARTESIAN_POINT('Ctrl Pts',(-0.753104107237202,-7.87597045092066,
101.120033393248));
#233674=CARTESIAN_POINT('Ctrl Pts',(-0.871461354364118,-7.86375411968934,
101.114982979528));
#233675=CARTESIAN_POINT('Ctrl Pts',(-1.08260098832937,-7.83713615329232,
101.105747771662));
#233676=CARTESIAN_POINT('Ctrl Pts',(-1.17549072621089,-7.82374261657887,
101.101606061657));
#233677=CARTESIAN_POINT('Ctrl Pts',(-1.53075431254588,-7.76604851520293,
101.085516908151));
#233678=CARTESIAN_POINT('Ctrl Pts',(-1.79106248980866,-7.71017525459716,
101.073209770356));
#233679=CARTESIAN_POINT('Ctrl Pts',(-2.28268868290962,-7.57840776136125,
101.049502601147));
#233680=CARTESIAN_POINT('Ctrl Pts',(-2.5143101455397,-7.50474374979458,
101.038128959809));
#233681=CARTESIAN_POINT('Ctrl Pts',(-3.28983456199195,-7.21815750692779,
100.999877728158));
#233682=CARTESIAN_POINT('Ctrl Pts',(-3.81347202669742,-6.95574799272295,
100.973920874342));
#233683=CARTESIAN_POINT('Ctrl Pts',(-4.33557801248443,-6.61726108430481,
100.948545863192));
#233684=CARTESIAN_POINT('Ctrl Pts',(-4.36748846147104,-6.59624329089312,
100.946996316995));
#233685=CARTESIAN_POINT('Ctrl Pts',(-4.40982095516389,-6.56791915650795,
100.944942244192));
#233686=CARTESIAN_POINT('Ctrl Pts',(-4.4203791717025,-6.5608178517136,100.94443006455));
#233687=CARTESIAN_POINT('Ctrl Pts',(-4.43681988137679,-6.5497023639132,
100.943632716053));
#233688=CARTESIAN_POINT('Ctrl Pts',(-4.44271414226381,-6.54570567365332,
100.943346892146));
#233689=CARTESIAN_POINT('Ctrl Pts',(-4.45395900011319,-6.53805874691654,
100.942801678425));
#233690=CARTESIAN_POINT('Ctrl Pts',(-4.45931052480181,-6.53440988892394,
100.942542237217));
#233691=CARTESIAN_POINT('Ctrl Pts',(-4.47178264438394,-6.52588350143272,
100.941937659609));
#233692=CARTESIAN_POINT('Ctrl Pts',(-4.47889975675041,-6.52100087888946,
100.941592715021));
#233693=CARTESIAN_POINT('Ctrl Pts',(-4.49916215136364,-6.50705124798289,
100.940610801492));
#233694=CARTESIAN_POINT('Ctrl Pts',(-4.51228802361258,-6.49795604816645,
100.939974894551));
#233695=CARTESIAN_POINT('Ctrl Pts',(-4.5945843211533,-6.44056156446588,
100.93598886539));
#233696=CARTESIAN_POINT('Ctrl Pts',(-4.66300714312354,-6.39119732710762,
100.932679179627));
#233697=CARTESIAN_POINT('Ctrl Pts',(-4.8633003566092,-6.24176496604875,
100.922994221195));
#233698=CARTESIAN_POINT('Ctrl Pts',(-4.99283644703769,-6.1386405678132,
100.91673605773));
#233699=CARTESIAN_POINT('Ctrl Pts',(-5.2203720428819,-5.94552765317669,
100.905688859674));
#233700=CARTESIAN_POINT('Ctrl Pts',(-5.31951653473187,-5.85698972296726,
100.900854958894));
#233701=CARTESIAN_POINT('Ctrl Pts',(-5.4754042868905,-5.71055389101984,
100.893180731596));
#233702=CARTESIAN_POINT('Ctrl Pts',(-5.53356892741414,-5.65421020308583,
100.890299810085));
#233703=CARTESIAN_POINT('Ctrl Pts',(-5.6301574641391,-5.55772735127853,
100.88547448177));
#233704=CARTESIAN_POINT('Ctrl Pts',(-5.66904172099806,-5.51805875374475,
100.883520213622));
#233705=CARTESIAN_POINT('Ctrl Pts',(-5.82426224927152,-5.35633465765741,
100.87566179634));
#233706=CARTESIAN_POINT('Ctrl Pts',(-5.93710100204922,-5.23098309301972,
100.869817809879));
#233707=CARTESIAN_POINT('Ctrl Pts',(-6.40439639780243,-4.67725316296863,
100.844713339013));
#233708=CARTESIAN_POINT('Ctrl Pts',(-6.71716813747526,-4.21576381357372,
100.825549076382));
#233709=CARTESIAN_POINT('Ctrl Pts',(-6.99909288721042,-3.6876070460383,
100.801926127745));
#233710=CARTESIAN_POINT('Ctrl Pts',(-7.01890916942798,-3.64974806723266,
100.80022659775));
#233711=CARTESIAN_POINT('Ctrl Pts',(-7.04424482897284,-3.60037480095434,
100.798003637669));
#233712=CARTESIAN_POINT('Ctrl Pts',(-7.05004463053605,-3.58900468418872,
100.797491266714));
#233713=CARTESIAN_POINT('Ctrl Pts',(-7.05924784888435,-3.57085401082569,
100.796672678039));
#233714=CARTESIAN_POINT('Ctrl Pts',(-7.06266908545917,-3.56408248325716,
100.796367137267));
#233715=CARTESIAN_POINT('Ctrl Pts',(-7.06880227926466,-3.55189976946472,
100.795817182549));
#233716=CARTESIAN_POINT('Ctrl Pts',(-7.07151777975968,-3.5464903673905,
100.795572900397));
#233717=CARTESIAN_POINT('Ctrl Pts',(-7.0778583946688,-3.53382333454048,
100.795000669654));
#233718=CARTESIAN_POINT('Ctrl Pts',(-7.08147855523264,-3.52656324003484,
100.794672540845));
#233719=CARTESIAN_POINT('Ctrl Pts',(-7.09183220061157,-3.50571917055118,
100.793730043452));
#233720=CARTESIAN_POINT('Ctrl Pts',(-7.09853779442751,-3.49212142431141,
100.793114683854));
#233721=CARTESIAN_POINT('Ctrl Pts',(-7.14228136989907,-3.40277066038664,
100.789068090054));
#233722=CARTESIAN_POINT('Ctrl Pts',(-7.17814465131622,-3.32645008950581,
100.785597243056));
#233723=CARTESIAN_POINT('Ctrl Pts',(-7.29088143511305,-3.07621849122254,
100.774196362235));
#233724=CARTESIAN_POINT('Ctrl Pts',(-7.36270576718467,-2.90010908661768,
100.766141509891));
#233725=CARTESIAN_POINT('Ctrl Pts',(-7.55347100807023,-2.37944768237302,
100.74245318307));
#233726=CARTESIAN_POINT('Ctrl Pts',(-7.65503992796993,-2.02905456234268,
100.726689666936));
#233727=CARTESIAN_POINT('Ctrl Pts',(-7.85114185618216,-1.12268161320065,
100.687022433179));
#233728=CARTESIAN_POINT('Ctrl Pts',(-7.91111634621678,-0.561322702383242,
100.663574107347));
#233729=CARTESIAN_POINT('Ctrl Pts',(-7.91099983056044,0.00163733706294327,
100.640435112007));
#233730=CARTESIAN_POINT('',(-7.91099993049747,-0.00104838700544144,96.6489168813118));
#233731=CARTESIAN_POINT('Ctrl Pts',(-7.91099982986448,0.00164069624814921,
100.640434973936));
#233732=CARTESIAN_POINT('Ctrl Pts',(-7.91096023546984,0.19255430968084,
100.632587971187));
#233733=CARTESIAN_POINT('Ctrl Pts',(-7.90400977593744,0.383408260987037,
100.624780623492));
#233734=CARTESIAN_POINT('Ctrl Pts',(-7.8873653218863,0.612270292793292,
100.615476921052));
#233735=CARTESIAN_POINT('Ctrl Pts',(-7.88428860421902,0.650691828228059,
100.613916925416));
#233736=CARTESIAN_POINT('Ctrl Pts',(-7.87877355984505,0.713765910890866,
100.611359113911));
#233737=CARTESIAN_POINT('Ctrl Pts',(-7.87650001950903,0.738432143384031,
100.610359623253));
#233738=CARTESIAN_POINT('Ctrl Pts',(-7.87223995113123,0.782390741714969,
100.608579777024));
#233739=CARTESIAN_POINT('Ctrl Pts',(-7.87029826045928,0.801687229967151,
100.607798954133));
#233740=CARTESIAN_POINT('Ctrl Pts',(-7.86625559152413,0.840432403845676,
100.606232088795));
#233741=CARTESIAN_POINT('Ctrl Pts',(-7.86415339494466,0.859880828874222,
100.605446065014));
#233742=CARTESIAN_POINT('Ctrl Pts',(-7.85950111331594,0.901476706684397,
100.603765929368));
#233743=CARTESIAN_POINT('Ctrl Pts',(-7.85692949952443,0.923621592483535,
100.602872060322));
#233744=CARTESIAN_POINT('Ctrl Pts',(-7.84983281857965,0.982557772622428,
100.60049468345));
#233745=CARTESIAN_POINT('Ctrl Pts',(-7.84514270547983,1.0193287026047,100.599013031406));
#233746=CARTESIAN_POINT('Ctrl Pts',(-7.82346948154017,1.1802299907184,100.592536243785));
#233747=CARTESIAN_POINT('Ctrl Pts',(-7.80379728290522,1.30398089468504,
100.587572388907));
#233748=CARTESIAN_POINT('Ctrl Pts',(-7.75836584760931,1.55167389131786,
100.577657856124));
#233749=CARTESIAN_POINT('Ctrl Pts',(-7.73255454181628,1.67556955297553,
100.572709248115));
#233750=CARTESIAN_POINT('Ctrl Pts',(-7.59159063495157,2.27928256392769,
100.548590938514));
#233751=CARTESIAN_POINT('Ctrl Pts',(-7.43469521165725,2.74821270809098,
100.529910196967));
#233752=CARTESIAN_POINT('Ctrl Pts',(-7.1695975457342,3.34769501792203,100.504413824522));
#233753=CARTESIAN_POINT('Ctrl Pts',(-7.09950850309346,3.49387574897339,
100.498053363241));
#233754=CARTESIAN_POINT('Ctrl Pts',(-7.01533074305503,3.65643213440784,
100.490744838756));
#233755=CARTESIAN_POINT('Ctrl Pts',(-7.00560672173067,3.67502868588438,
100.489905178286));
#233756=CARTESIAN_POINT('Ctrl Pts',(-6.98979872709786,3.70496969744956,
100.488547308002));
#233757=CARTESIAN_POINT('Ctrl Pts',(-6.9837608580399,3.71633838355598,100.488030315602));
#233758=CARTESIAN_POINT('Ctrl Pts',(-6.97302851061909,3.73642776950073,
100.487114230615));
#233759=CARTESIAN_POINT('Ctrl Pts',(-6.96834537976743,3.74515443662742,
100.486715452006));
#233760=CARTESIAN_POINT('Ctrl Pts',(-6.95880334648676,3.76285544933195,
100.485904891098));
#233761=CARTESIAN_POINT('Ctrl Pts',(-6.95394344125953,3.77182923296794,
100.485493083175));
#233762=CARTESIAN_POINT('Ctrl Pts',(-6.94443918135528,3.7892979812476,100.484689738828));
#233763=CARTESIAN_POINT('Ctrl Pts',(-6.93979656828717,3.79779387597702,
100.484298247024));
#233764=CARTESIAN_POINT('Ctrl Pts',(-6.92731576297593,3.82053421150891,
100.483248282758));
#233765=CARTESIAN_POINT('Ctrl Pts',(-6.91944924769304,3.83476302359058,
100.482589112759));
#233766=CARTESIAN_POINT('Ctrl Pts',(-6.89057304786241,3.88661562627595,
100.480179072825));
#233767=CARTESIAN_POINT('Ctrl Pts',(-6.86930001876524,3.92409163489703,
100.478422022591));
#233768=CARTESIAN_POINT('Ctrl Pts',(-6.64766062351281,4.3072208662608,100.46030956319));
#233769=CARTESIAN_POINT('Ctrl Pts',(-6.42169184364047,4.63739229359507,
100.44346866117));
#233770=CARTESIAN_POINT('Ctrl Pts',(-5.96602809492469,5.20562917588908,
100.412884643212));
#233771=CARTESIAN_POINT('Ctrl Pts',(-5.74449774991016,5.44911187076498,
100.399145479457));
#233772=CARTESIAN_POINT('Ctrl Pts',(-5.42666627675313,5.7574472525951,100.380916287786));
#233773=CARTESIAN_POINT('Ctrl Pts',(-5.34317300155922,5.83501572310704,
100.376250082258));
#233774=CARTESIAN_POINT('Ctrl Pts',(-5.21627036529305,5.94790456427658,
100.369332801011));
#233775=CARTESIAN_POINT('Ctrl Pts',(-5.17411546769705,5.98461146713653,
100.367062654732));
#233776=CARTESIAN_POINT('Ctrl Pts',(-5.1058083335103,6.04282950737379,100.363427290814));
#233777=CARTESIAN_POINT('Ctrl Pts',(-5.07990097745954,6.0646247423254,100.362058244942));
#233778=CARTESIAN_POINT('Ctrl Pts',(-5.0300631220844,6.10600870457515,100.359442930052));
#233779=CARTESIAN_POINT('Ctrl Pts',(-5.00615611258032,6.12562472717346,
100.358196316416));
#233780=CARTESIAN_POINT('Ctrl Pts',(-4.96361053217489,6.16011851997093,
100.355991590398));
#233781=CARTESIAN_POINT('Ctrl Pts',(-4.94501857496561,6.17505311657867,
100.355032754206));
#233782=CARTESIAN_POINT('Ctrl Pts',(-4.9081789387263,6.2043726831379,100.35314177561));
#233783=CARTESIAN_POINT('Ctrl Pts',(-4.88993484882807,6.21876177898432,
100.352209588863));
#233784=CARTESIAN_POINT('Ctrl Pts',(-4.84563703741152,6.25338395230157,
100.349956359648));
#233785=CARTESIAN_POINT('Ctrl Pts',(-4.81951961431992,6.27353487681995,
100.348636335107));
#233786=CARTESIAN_POINT('Ctrl Pts',(-4.71960596046138,6.34963118858123,
100.343617814228));
#233787=CARTESIAN_POINT('Ctrl Pts',(-4.64495512298455,6.4044428923088,100.339932770767));
#233788=CARTESIAN_POINT('Ctrl Pts',(-4.00382955789243,6.85807617367311,
100.308784172112));
#233789=CARTESIAN_POINT('Ctrl Pts',(-3.38815291966685,7.18222672768204,
100.282174738854));
#233790=CARTESIAN_POINT('Ctrl Pts',(-2.59522661509475,7.47475215743371,
100.25068241293));
#233791=CARTESIAN_POINT('Ctrl Pts',(-2.45083247678041,7.52333312808928,
100.245033985847));
#233792=CARTESIAN_POINT('Ctrl Pts',(-2.10295085362331,7.62929786193549,
100.231533932811));
#233793=CARTESIAN_POINT('Ctrl Pts',(-1.8983918469589,7.68275302980015,100.223683795367));
#233794=CARTESIAN_POINT('Ctrl Pts',(-1.53143011979826,7.7630948525063,100.209503204147));
#233795=CARTESIAN_POINT('Ctrl Pts',(-1.36986667422358,7.79322669320617,
100.203225893888));
#233796=CARTESIAN_POINT('Ctrl Pts',(-1.133747753138,7.82969375200893,100.193883556768));
#233797=CARTESIAN_POINT('Ctrl Pts',(-1.05985207079162,7.84003835478334,
100.190935869139));
#233798=CARTESIAN_POINT('Ctrl Pts',(-0.972312000439411,7.8510327847856,
100.187405704028));
#233799=CARTESIAN_POINT('Ctrl Pts',(-0.958797150394343,7.85269472446193,
100.186859625132));
#233800=CARTESIAN_POINT('Ctrl Pts',(-0.938023925078069,7.85519480991179,
100.186018532465));
#233801=CARTESIAN_POINT('Ctrl Pts',(-0.930768530941449,7.85605781082663,
100.185724442232));
#233802=CARTESIAN_POINT('Ctrl Pts',(-0.917560494371384,7.85761030139283,
100.185188461757));
#233803=CARTESIAN_POINT('Ctrl Pts',(-0.911608239238141,7.85830308191866,
100.18494669616));
#233804=CARTESIAN_POINT('Ctrl Pts',(-0.899573157417448,7.85968998225093,
100.184457399832));
#233805=CARTESIAN_POINT('Ctrl Pts',(-0.893490301216162,7.86038380513328,
100.184209857895));
#233806=CARTESIAN_POINT('Ctrl Pts',(-0.876143865552452,7.86234197894077,
100.18350325106));
#233807=CARTESIAN_POINT('Ctrl Pts',(-0.86487839329727,7.86358918242859,
100.183043518891));
#233808=CARTESIAN_POINT('Ctrl Pts',(-0.816829930576569,7.86880414023008,
100.181079026328));
#233809=CARTESIAN_POINT('Ctrl Pts',(-0.780022424271394,7.8725380078429,
100.179564924014));
#233810=CARTESIAN_POINT('Ctrl Pts',(-0.224304485055795,7.92497625101821,
100.15654980273));
#233811=CARTESIAN_POINT('Ctrl Pts',(0.298060922999434,7.9225331701876,100.132655270803));
#233812=CARTESIAN_POINT('Ctrl Pts',(1.06634897471536,7.84283261612408,100.097071085168));
#233813=CARTESIAN_POINT('Ctrl Pts',(1.31503426755326,7.80498641397619,100.085477695556));
#233814=CARTESIAN_POINT('Ctrl Pts',(1.85597674654879,7.69607071133398,100.060416919684));
#233815=CARTESIAN_POINT('Ctrl Pts',(2.14685390951061,7.62005203710519,100.047048990688));
#233816=CARTESIAN_POINT('Ctrl Pts',(2.62390216677596,7.46588418059872,100.025509850565));
#233817=CARTESIAN_POINT('Ctrl Pts',(2.81266930532603,7.39683634955653,100.017088756561));
#233818=CARTESIAN_POINT('Ctrl Pts',(3.0331269876078,7.30653494035904,100.007374046455));
#233819=CARTESIAN_POINT('Ctrl Pts',(3.0675418510025,7.29215326207337,100.005860975287));
#233820=CARTESIAN_POINT('Ctrl Pts',(3.11328449126638,7.27265667194257,100.003854320117));
#233821=CARTESIAN_POINT('Ctrl Pts',(3.12470350337861,7.26775779792038,100.003353757792));
#233822=CARTESIAN_POINT('Ctrl Pts',(3.14349753140918,7.25964248463101,100.002530507865));
#233823=CARTESIAN_POINT('Ctrl Pts',(3.15087924723518,7.25644166960989,100.002207314142));
#233824=CARTESIAN_POINT('Ctrl Pts',(3.16521909690143,7.25019770382553,100.001579767771));
#233825=CARTESIAN_POINT('Ctrl Pts',(3.17217775552793,7.24715578442172,100.001275375576));
#233826=CARTESIAN_POINT('Ctrl Pts',(3.18829898843479,7.24008085437079,100.00057049629));
#233827=CARTESIAN_POINT('Ctrl Pts',(3.19745831785828,7.23604045897654,100.000170250051));
#233828=CARTESIAN_POINT('Ctrl Pts',(3.22702408934927,7.22293120499226,99.9988790214673));
#233829=CARTESIAN_POINT('Ctrl Pts',(3.24739988830144,7.21379329068528,99.9979902922486));
#233830=CARTESIAN_POINT('Ctrl Pts',(3.43888197075628,7.12694381546557,99.9896488369977));
#233831=CARTESIAN_POINT('Ctrl Pts',(3.60721234484717,7.04324228866929,99.9823962327537));
#233832=CARTESIAN_POINT('Ctrl Pts',(4.15179580001342,6.74780032986943,99.9590748360825));
#233833=CARTESIAN_POINT('Ctrl Pts',(4.51371678957193,6.51126794739829,99.9438470014857));
#233834=CARTESIAN_POINT('Ctrl Pts',(5.137337119906,6.02660449699065,99.9164663258873));
#233835=CARTESIAN_POINT('Ctrl Pts',(5.40487010043764,5.7878806761234,99.9042473250419));
#233836=CARTESIAN_POINT('Ctrl Pts',(5.88871201849955,5.29324198779827,99.8796720404773));
#233837=CARTESIAN_POINT('Ctrl Pts',(6.10678053655651,5.04009540122998,99.8673918878904));
#233838=CARTESIAN_POINT('Ctrl Pts',(6.31704554425798,4.76225485964231,99.8534600037516));
#233839=CARTESIAN_POINT('Ctrl Pts',(6.32585640097968,4.75054486835573,99.8528721743785));
#233840=CARTESIAN_POINT('Ctrl Pts',(6.33870991425516,4.73336285403977,99.8520087892971));
#233841=CARTESIAN_POINT('Ctrl Pts',(6.34277816544282,4.72790994294913,99.8517346568589));
#233842=CARTESIAN_POINT('Ctrl Pts',(6.34992304013808,4.71830743690253,99.8512516996337));
#233843=CARTESIAN_POINT('Ctrl Pts',(6.35300264680384,4.71416005820049,99.8510430376621));
#233844=CARTESIAN_POINT('Ctrl Pts',(6.3589876728035,4.70608336710477,99.8506365538977));
#233845=CARTESIAN_POINT('Ctrl Pts',(6.36189351831942,4.70215437245911,99.8504387551703));
#233846=CARTESIAN_POINT('Ctrl Pts',(6.36884313030786,4.69273956530613,99.8499646431162));
#233847=CARTESIAN_POINT('Ctrl Pts',(6.37288344732606,4.68725122141114,99.84968814743));
#233848=CARTESIAN_POINT('Ctrl Pts',(6.38742618768309,4.66744288239805,99.8486898422931));
#233849=CARTESIAN_POINT('Ctrl Pts',(6.39788742897885,4.65309282118608,99.8479658975196));
#233850=CARTESIAN_POINT('Ctrl Pts',(6.59607267379569,4.37930309005527,99.8341415875694));
#233851=CARTESIAN_POINT('Ctrl Pts',(6.76791206266958,4.10874856729093,99.8202918854046));
#233852=CARTESIAN_POINT('Ctrl Pts',(7.28392490375116,3.17568071141,99.773568527802));
#233853=CARTESIAN_POINT('Ctrl Pts',(7.55086697149216,2.47490991569367,99.7405964551002));
#233854=CARTESIAN_POINT('Ctrl Pts',(7.72785658031028,1.69328082791274,99.7077940101454));
#233855=CARTESIAN_POINT('Ctrl Pts',(7.73948218054723,1.63932393455125,99.705545978589));
#233856=CARTESIAN_POINT('Ctrl Pts',(7.75617294865802,1.55772005116019,99.7021695033285));
#233857=CARTESIAN_POINT('Ctrl Pts',(7.7616569364702,1.53016083476523,99.7010332132753));
#233858=CARTESIAN_POINT('Ctrl Pts',(7.77028942712613,1.48553837139456,99.6991996670909));
#233859=CARTESIAN_POINT('Ctrl Pts',(7.77352881588373,1.46849303221902,99.6985007481623));
#233860=CARTESIAN_POINT('Ctrl Pts',(7.77950328594373,1.43648218407326,99.697190901113));
#233861=CARTESIAN_POINT('Ctrl Pts',(7.78225132278862,1.42151918453863,99.6965797419789));
#233862=CARTESIAN_POINT('Ctrl Pts',(7.78719022445499,1.39418337778344,99.6954652019882));
#233863=CARTESIAN_POINT('Ctrl Pts',(7.78939480403437,1.38181310988924,99.6949615797102));
#233864=CARTESIAN_POINT('Ctrl Pts',(7.79367717755843,1.35744806240517,99.6939710521882));
#233865=CARTESIAN_POINT('Ctrl Pts',(7.79575677550779,1.3454536365777,99.6934841167464));
#233866=CARTESIAN_POINT('Ctrl Pts',(7.80068641527391,1.31662596415432,99.6923154106822));
#233867=CARTESIAN_POINT('Ctrl Pts',(7.8035096696653,1.29978818154354,99.6916341021497));
#233868=CARTESIAN_POINT('Ctrl Pts',(7.81196278365642,1.24835374853814,99.6895568025498));
#233869=CARTESIAN_POINT('Ctrl Pts',(7.81741726274164,1.21372854269824,99.6881637263018));
#233870=CARTESIAN_POINT('Ctrl Pts',(7.8699728466667,0.865043447338463,99.6741866319982));
#233871=CARTESIAN_POINT('Ctrl Pts',(7.89835393063116,0.548445323193617,
99.6619342042612));
#233872=CARTESIAN_POINT('Ctrl Pts',(7.91355981181843,0.0278849011738598,
99.6422731571413));
#233873=CARTESIAN_POINT('Ctrl Pts',(7.91166564659692,-0.175372486071327,
99.6347132313587));
#233874=CARTESIAN_POINT('Ctrl Pts',(7.8832111618767,-0.769677659078231,
99.6127308376387));
#233875=CARTESIAN_POINT('Ctrl Pts',(7.83542876299146,-1.15908018817654,
99.5985028876602));
#233876=CARTESIAN_POINT('Ctrl Pts',(7.72328594211843,-1.7228713241323,99.5769567466913));
#233877=CARTESIAN_POINT('Ctrl Pts',(7.68135370557434,-1.90111347503911,
99.569997129403));
#233878=CARTESIAN_POINT('Ctrl Pts',(7.61171910769348,-2.15694033404288,
99.5596387933831));
#233879=CARTESIAN_POINT('Ctrl Pts',(7.58892865381696,-2.2358042651679,99.5563937149455));
#233880=CARTESIAN_POINT('Ctrl Pts',(7.5609307579242,-2.32732305800264,99.5525552474811));
#233881=CARTESIAN_POINT('Ctrl Pts',(7.55691231170079,-2.34033819197734,
99.5520076436016));
#233882=CARTESIAN_POINT('Ctrl Pts',(7.55073336070051,-2.36016902707431,
99.5511705683462));
#233883=CARTESIAN_POINT('Ctrl Pts',(7.5485971855968,-2.36699232147678,99.5508820625613));
#233884=CARTESIAN_POINT('Ctrl Pts',(7.54470016031182,-2.37938113100547,
99.5503573316974));
#233885=CARTESIAN_POINT('Ctrl Pts',(7.54294239308565,-2.38494761576678,
99.5501212310643));
#233886=CARTESIAN_POINT('Ctrl Pts',(7.53940962896568,-2.39609217524037,
99.5496478677686));
#233887=CARTESIAN_POINT('Ctrl Pts',(7.5376345988578,-2.40167023536674,99.5494106038559));
#233888=CARTESIAN_POINT('Ctrl Pts',(7.53260285631892,-2.41742204018513,
99.5487396353783));
#233889=CARTESIAN_POINT('Ctrl Pts',(7.52933173364635,-2.42759114238872,
99.548305334509));
#233890=CARTESIAN_POINT('Ctrl Pts',(7.51566860466237,-2.46977311584975,
99.5464990224979));
#233891=CARTESIAN_POINT('Ctrl Pts',(7.50509305138797,-2.50172581620905,
99.5451192383404));
#233892=CARTESIAN_POINT('Ctrl Pts',(7.47546495840238,-2.58936450532054,
99.5413011268957));
#233893=CARTESIAN_POINT('Ctrl Pts',(7.45599461415861,-2.64490626933408,
99.5388434919309));
#233894=CARTESIAN_POINT('Ctrl Pts',(7.41483006416666,-2.75826555426406,
99.5337437480003));
#233895=CARTESIAN_POINT('Ctrl Pts',(7.39307572047373,-2.81605483236703,
99.5310999296479));
#233896=CARTESIAN_POINT('Ctrl Pts',(7.32034902315607,-3.00259650935262,
99.5224361035409));
#233897=CARTESIAN_POINT('Ctrl Pts',(7.26667347405529,-3.13026348803249,
99.5163048980458));
#233898=CARTESIAN_POINT('Ctrl Pts',(7.17064345063041,-3.34287084919879,
99.5058269500449));
#233899=CARTESIAN_POINT('Ctrl Pts',(7.13005949495648,-3.42858047214099,
99.5015275139111));
#233900=CARTESIAN_POINT('Ctrl Pts',(6.88998130185354,-3.91289596976146,
99.4768753221282));
#233901=CARTESIAN_POINT('Ctrl Pts',(6.6586083678323,-4.29482940987859,99.4560914384027));
#233902=CARTESIAN_POINT('Ctrl Pts',(6.21101513240632,-4.90982206506857,
99.4219182485195));
#233903=CARTESIAN_POINT('Ctrl Pts',(6.01068739264013,-5.15312788475656,
99.4081664314626));
#233904=CARTESIAN_POINT('Ctrl Pts',(5.71651722666356,-5.4698373363519,99.3900952982096));
#233905=CARTESIAN_POINT('Ctrl Pts',(5.63475595446019,-5.55402706363005,
99.385271299003));
#233906=CARTESIAN_POINT('Ctrl Pts',(5.53912969880361,-5.64820748531026,
99.3798499028787));
#233907=CARTESIAN_POINT('Ctrl Pts',(5.52707197193466,-5.66000715892489,
99.3791701996506));
#233908=CARTESIAN_POINT('Ctrl Pts',(5.50881265324479,-5.67776171276216,
99.3781467505668));
#233909=CARTESIAN_POINT('Ctrl Pts',(5.50263898623424,-5.68374516522876,
99.3778017136442));
#233910=CARTESIAN_POINT('Ctrl Pts',(5.49196857140927,-5.6940531374733,99.3772070839257));
#233911=CARTESIAN_POINT('Ctrl Pts',(5.48747644596681,-5.69838241757312,
99.37695727658));
#233912=CARTESIAN_POINT('Ctrl Pts',(5.47818135732832,-5.70731936333021,
99.3764414590151));
#233913=CARTESIAN_POINT('Ctrl Pts',(5.47337768998806,-5.71192629170408,
99.3761754820137));
#233914=CARTESIAN_POINT('Ctrl Pts',(5.46035216943453,-5.72438681984994,
99.3754558735074));
#233915=CARTESIAN_POINT('Ctrl Pts',(5.4521191748671,-5.73222877962892,99.3750027647687));
#233916=CARTESIAN_POINT('Ctrl Pts',(5.42143795171448,-5.76132686785586,
99.3733206128278));
#233917=CARTESIAN_POINT('Ctrl Pts',(5.39888195022409,-5.78246923543712,
99.3720966601603));
#233918=CARTESIAN_POINT('Ctrl Pts',(5.04709138507091,-6.10835949678001,
99.3532022000819));
#233919=CARTESIAN_POINT('Ctrl Pts',(4.69263200080543,-6.3847047074283,99.3368612160111));
#233920=CARTESIAN_POINT('Ctrl Pts',(3.88614493821585,-6.90982399311899,
99.3034611752654));
#233921=CARTESIAN_POINT('Ctrl Pts',(3.42941544221314,-7.1475084261507,99.2867281387099));
#233922=CARTESIAN_POINT('Ctrl Pts',(2.60105305861641,-7.48079302035889,
99.255968514802));
#233923=CARTESIAN_POINT('Ctrl Pts',(2.23953732057409,-7.5968514818461,99.2423844352822));
#233924=CARTESIAN_POINT('Ctrl Pts',(1.85981077478459,-7.6892887085244,99.2267247401516));
#233925=CARTESIAN_POINT('Ctrl Pts',(1.84847536837143,-7.69202156592872,
99.2262560152875));
#233926=CARTESIAN_POINT('Ctrl Pts',(1.83214727308278,-7.69591993558362,
99.2255789765829));
#233927=CARTESIAN_POINT('Ctrl Pts',(1.82715938058704,-7.697105682194,99.2253719052564));
#233928=CARTESIAN_POINT('Ctrl Pts',(1.81849337666459,-7.69915690947033,
99.225011698268));
#233929=CARTESIAN_POINT('Ctrl Pts',(1.81481578590579,-7.70002460650264,
99.224858699838));
#233930=CARTESIAN_POINT('Ctrl Pts',(1.80773920795675,-7.70168891502091,
99.2245640269751));
#233931=CARTESIAN_POINT('Ctrl Pts',(1.80434031152366,-7.70248591221495,
99.2244223766094));
#233932=CARTESIAN_POINT('Ctrl Pts',(1.7963091734363,-7.70436350251064,99.224087393977));
#233933=CARTESIAN_POINT('Ctrl Pts',(1.79167651200185,-7.70544216131351,
99.2238939413955));
#233934=CARTESIAN_POINT('Ctrl Pts',(1.77778162721461,-7.70866420781675,
99.2233130508399));
#233935=CARTESIAN_POINT('Ctrl Pts',(1.76851654688455,-7.71079506955878,
99.2229248334365));
#233936=CARTESIAN_POINT('Ctrl Pts',(1.67944262186945,-7.73111205921468,
99.2191842455526));
#233937=CARTESIAN_POINT('Ctrl Pts',(1.59936259321271,-7.74807457002135,
99.21575745885));
#233938=CARTESIAN_POINT('Ctrl Pts',(1.43020006478053,-7.78117233083112,
99.2084082275603));
#233939=CARTESIAN_POINT('Ctrl Pts',(1.34107442021528,-7.79702721544461,
99.2044722658504));
#233940=CARTESIAN_POINT('Ctrl Pts',(0.700655315249088,-7.89964870131146,
99.1758383943272));
#233941=CARTESIAN_POINT('Ctrl Pts',(0.141825726839241,-7.92939184287613,
99.1491257633281));
#233942=CARTESIAN_POINT('Ctrl Pts',(-0.973481152622563,-7.87073580655182,
99.0975471492314));
#233943=CARTESIAN_POINT('Ctrl Pts',(-1.52686931451837,-7.78235180979279,
99.0728578235253));
#233944=CARTESIAN_POINT('Ctrl Pts',(-2.08598445585518,-7.63105507017697,
99.049463581974));
#233945=CARTESIAN_POINT('Ctrl Pts',(-2.10554850234315,-7.6256801760249,
99.0486467751139));
#233946=CARTESIAN_POINT('Ctrl Pts',(-2.13380177437203,-7.61780104440447,
99.0474697323074));
#233947=CARTESIAN_POINT('Ctrl Pts',(-2.14250763910446,-7.61535710138263,
99.0471073921225));
#233948=CARTESIAN_POINT('Ctrl Pts',(-2.1576703064623,-7.61107252141526,
99.0464769234216));
#233949=CARTESIAN_POINT('Ctrl Pts',(-2.16412898211825,-7.60923858389849,
99.0462085611167));
#233950=CARTESIAN_POINT('Ctrl Pts',(-2.17658598708254,-7.60568428086476,
99.04569133181));
#233951=CARTESIAN_POINT('Ctrl Pts',(-2.18258462879476,-7.60396503659365,
99.0454424258822));
#233952=CARTESIAN_POINT('Ctrl Pts',(-2.19677609137676,-7.59987950731469,
99.0448539569747));
#233953=CARTESIAN_POINT('Ctrl Pts',(-2.20496714134393,-7.59750706663638,
99.0445146095644));
#233954=CARTESIAN_POINT('Ctrl Pts',(-2.23359623278323,-7.58916479068351,
99.0433295954024));
#233955=CARTESIAN_POINT('Ctrl Pts',(-2.25401408461351,-7.58312566606434,
99.0424863548141));
#233956=CARTESIAN_POINT('Ctrl Pts',(-2.50165455647137,-7.50879083467617,
99.0322815345335));
#233957=CARTESIAN_POINT('Ctrl Pts',(-2.7257267695169,-7.430386305272,99.0232843372393));
#233958=CARTESIAN_POINT('Ctrl Pts',(-3.36248708663502,-7.17488946805482,
98.9981342048862));
#233959=CARTESIAN_POINT('Ctrl Pts',(-3.76405924365229,-6.97260634749538,
98.9828461197481));
#233960=CARTESIAN_POINT('Ctrl Pts',(-4.44829276479744,-6.55151445461675,
98.9555519163607));
#233961=CARTESIAN_POINT('Ctrl Pts',(-4.73742075356699,-6.34558668965958,
98.9435402885199));
#233962=CARTESIAN_POINT('Ctrl Pts',(-5.13331199052824,-6.02143794191036,
98.9250121428385));
#233963=CARTESIAN_POINT('Ctrl Pts',(-5.25188040644678,-5.91830670462849,
98.9191615399376));
#233964=CARTESIAN_POINT('Ctrl Pts',(-5.41408500718829,-5.76850599128377,
98.9105930697671));
#233965=CARTESIAN_POINT('Ctrl Pts',(-5.46035168459495,-5.72473028919786,
98.9080811320816));
#233966=CARTESIAN_POINT('Ctrl Pts',(-5.51268111550295,-5.67400672767969,
98.9051542295632));
#233967=CARTESIAN_POINT('Ctrl Pts',(-5.51926752755478,-5.66760014321294,
98.9047842535048));
#233968=CARTESIAN_POINT('Ctrl Pts',(-5.5292703590938,-5.65783644499864,
98.904219971643));
#233969=CARTESIAN_POINT('Ctrl Pts',(-5.53269494532087,-5.65448765001137,
98.9040263546194));
#233970=CARTESIAN_POINT('Ctrl Pts',(-5.53889840986603,-5.64841044645443,
98.903674853146));
#233971=CARTESIAN_POINT('Ctrl Pts',(-5.54167832137827,-5.64568308964385,
98.9035170549776));
#233972=CARTESIAN_POINT('Ctrl Pts',(-5.54723310881171,-5.64022526074605,
98.9032011813543));
#233973=CARTESIAN_POINT('Ctrl Pts',(-5.55000798553273,-5.6374947907625,
98.9030431060562));
#233974=CARTESIAN_POINT('Ctrl Pts',(-5.55781025307834,-5.62980604018116,
98.9025978474072));
#233975=CARTESIAN_POINT('Ctrl Pts',(-5.5628330116419,-5.62484308610008,
98.9023102850551));
#233976=CARTESIAN_POINT('Ctrl Pts',(-5.58344643933767,-5.60442048115203,
98.9011263504067));
#233977=CARTESIAN_POINT('Ctrl Pts',(-5.59897922821195,-5.58890281309652,
98.9002253240061));
#233978=CARTESIAN_POINT('Ctrl Pts',(-5.86631334291494,-5.31959600633263,
98.8845666665892));
#233979=CARTESIAN_POINT('Ctrl Pts',(-6.10066765185181,-5.04911259935259,
98.8685226913661));
#233980=CARTESIAN_POINT('Ctrl Pts',(-6.69309835078859,-4.26365127268738,
98.8232132369111));
#233981=CARTESIAN_POINT('Ctrl Pts',(-7.00960794333514,-3.72045981521665,
98.7934149495998));
#233982=CARTESIAN_POINT('Ctrl Pts',(-7.35484544840114,-2.92380076940478,
98.75492403291));
#233983=CARTESIAN_POINT('Ctrl Pts',(-7.44075692707853,-2.69768646678838,
98.7444989868383));
#233984=CARTESIAN_POINT('Ctrl Pts',(-7.550036890349,-2.36487633127673,98.72989041988));
#233985=CARTESIAN_POINT('Ctrl Pts',(-7.58176676333027,-2.26108626392274,
98.7254343652156));
#233986=CARTESIAN_POINT('Ctrl Pts',(-7.61601334419074,-2.14022290563121,
98.7203565950744));
#233987=CARTESIAN_POINT('Ctrl Pts',(-7.62062124952954,-2.12375731209143,
98.7196672013442));
#233988=CARTESIAN_POINT('Ctrl Pts',(-7.62753875605779,-2.09872633275612,
98.7186227498849));
#233989=CARTESIAN_POINT('Ctrl Pts',(-7.62988737694411,-2.09017183761961,
98.7182664330955));
#233990=CARTESIAN_POINT('Ctrl Pts',(-7.63411346212787,-2.07467692449907,
98.7176221671726));
#233991=CARTESIAN_POINT('Ctrl Pts',(-7.63599586152115,-2.06773786947747,
98.7173340592915));
#233992=CARTESIAN_POINT('Ctrl Pts',(-7.63973606186033,-2.05387567444613,
98.7167593245844));
#233993=CARTESIAN_POINT('Ctrl Pts',(-7.64159391833699,-2.04695255649828,
98.7164726961863));
#233994=CARTESIAN_POINT('Ctrl Pts',(-7.64678290024241,-2.02751081094486,
98.7156689171046));
#233995=CARTESIAN_POINT('Ctrl Pts',(-7.65009269695545,-2.01498648679361,
98.7151524516002));
#233996=CARTESIAN_POINT('Ctrl Pts',(-7.66348630798549,-1.96379615665739,
98.7130468941747));
#233997=CARTESIAN_POINT('Ctrl Pts',(-7.67330793795192,-1.92506183944342,
98.7114662001646));
#233998=CARTESIAN_POINT('Ctrl Pts',(-7.83465082278898,-1.26790187120604,
98.6848547863644));
#233999=CARTESIAN_POINT('Ctrl Pts',(-7.91126395176661,-0.633492366055027,
98.6625003051799));
#234000=CARTESIAN_POINT('Ctrl Pts',(-7.91075951849226,0.580304530698811,
98.6204359102891));
#234001=CARTESIAN_POINT('Ctrl Pts',(-7.84739031158016,1.15557940886955,
98.6006317366358));
#234002=CARTESIAN_POINT('Ctrl Pts',(-7.71335515118168,1.757743456605,98.5762582055363));
#234003=CARTESIAN_POINT('Ctrl Pts',(-7.70440106902857,1.79658393760866,
98.5746717819013));
#234004=CARTESIAN_POINT('Ctrl Pts',(-7.69227254215473,1.84743562531875,
98.572577199154));
#234005=CARTESIAN_POINT('Ctrl Pts',(-7.68936269813695,1.85950975985054,
98.5720785621658));
#234006=CARTESIAN_POINT('Ctrl Pts',(-7.68482596966916,1.87814175921411,
98.5713071280592));
#234007=CARTESIAN_POINT('Ctrl Pts',(-7.68321908987238,1.88470450429724,
98.5710350280134));
#234008=CARTESIAN_POINT('Ctrl Pts',(-7.6800154285328,1.89771656496042,98.57049478961));
#234009=CARTESIAN_POINT('Ctrl Pts',(-7.67841892584772,1.90416594400465,
98.5702266609676));
#234010=CARTESIAN_POINT('Ctrl Pts',(-7.67484704966503,1.9185176865934,98.5696292010279));
#234011=CARTESIAN_POINT('Ctrl Pts',(-7.67286759325506,1.92641902123219,
98.5692997326672));
#234012=CARTESIAN_POINT('Ctrl Pts',(-7.66713118536377,1.9491677574386,98.568349633106));
#234013=CARTESIAN_POINT('Ctrl Pts',(-7.66334332624633,1.96400728635094,
98.5677279860783));
#234014=CARTESIAN_POINT('Ctrl Pts',(-7.63762184366257,2.06356786049756,
98.5635449985875));
#234015=CARTESIAN_POINT('Ctrl Pts',(-7.6143271519258,2.14792951666858,98.559940960607));
#234016=CARTESIAN_POINT('Ctrl Pts',(-7.53290945425882,2.42479444226227,
98.5479441496123));
#234017=CARTESIAN_POINT('Ctrl Pts',(-7.46884772032344,2.61546608751238,
98.5394126252318));
#234018=CARTESIAN_POINT('Ctrl Pts',(-7.18228964197923,3.37161084358709,
98.5048277067009));
#234019=CARTESIAN_POINT('Ctrl Pts',(-6.90223805758939,3.91308229123864,
98.4785408188109));
#234020=CARTESIAN_POINT('Ctrl Pts',(-6.35227453621796,4.73021506270681,
98.4372334871509));
#234021=CARTESIAN_POINT('Ctrl Pts',(-6.11943619234049,5.02780619090267,
98.4216783506842));
#234022=CARTESIAN_POINT('Ctrl Pts',(-5.76790613931722,5.41633309822399,
98.4002314792745));
#234023=CARTESIAN_POINT('Ctrl Pts',(-5.66656294665684,5.52227043042734,
98.3942629212634));
#234024=CARTESIAN_POINT('Ctrl Pts',(-5.53481890949836,5.65253907112872,
98.386770247152));
#234025=CARTESIAN_POINT('Ctrl Pts',(-5.50710436812444,5.67954397892837,
98.3852082756454));
#234026=CARTESIAN_POINT('Ctrl Pts',(-5.46285891864407,5.72202815476593,
98.3827369772734));
#234027=CARTESIAN_POINT('Ctrl Pts',(-5.44645781661382,5.73764159080866,
98.3818256973729));
#234028=CARTESIAN_POINT('Ctrl Pts',(-5.41692386788539,5.76551642164585,
98.3801932629011));
#234029=CARTESIAN_POINT('Ctrl Pts',(-5.40381587091827,5.77780389368341,
98.3794717259426));
#234030=CARTESIAN_POINT('Ctrl Pts',(-5.3730905909535,5.80640983352979,98.3777873636261));
#234031=CARTESIAN_POINT('Ctrl Pts',(-5.35544062395208,5.82269296644172,
98.3768250709696));
#234032=CARTESIAN_POINT('Ctrl Pts',(-5.30448889330591,5.86927128003635,
98.3740621746716));
#234033=CARTESIAN_POINT('Ctrl Pts',(-5.27100222259598,5.89936296373868,
98.3722646494586));
#234034=CARTESIAN_POINT('Ctrl Pts',(-5.018182867237,6.12267944868293,98.3588280874195));
#234035=CARTESIAN_POINT('Ctrl Pts',(-4.78854518601225,6.30390394360081,
98.347384382168));
#234036=CARTESIAN_POINT('Ctrl Pts',(-4.23922784188059,6.69003833336223,
98.3213739389234));
#234037=CARTESIAN_POINT('Ctrl Pts',(-3.91378536103238,6.88548817053646,
98.3069321195091));
#234038=CARTESIAN_POINT('Ctrl Pts',(-3.37027584951745,7.16087537501986,
98.2833691991164));
#234039=CARTESIAN_POINT('Ctrl Pts',(-3.16052785769293,7.25589094003613,
98.2743920270559));
#234040=CARTESIAN_POINT('Ctrl Pts',(-2.9239651804909,7.35084768426346,98.264196330924));
#234041=CARTESIAN_POINT('Ctrl Pts',(-2.9009441869084,7.359963102801,98.2632033756447));
#234042=CARTESIAN_POINT('Ctrl Pts',(-2.86635641441423,7.37347102613003,
98.2617100591796));
#234043=CARTESIAN_POINT('Ctrl Pts',(-2.85482152969534,7.37794470702236,
98.26121181385));
#234044=CARTESIAN_POINT('Ctrl Pts',(-2.83385991618032,7.38601792542614,
98.2603059996657));
#234045=CARTESIAN_POINT('Ctrl Pts',(-2.82443669508371,7.38962652466335,
98.2598986532406));
#234046=CARTESIAN_POINT('Ctrl Pts',(-2.80414202162799,7.39735382921292,
98.2590210746002));
#234047=CARTESIAN_POINT('Ctrl Pts',(-2.793268346663,7.4014666178071,98.258550703452));
#234048=CARTESIAN_POINT('Ctrl Pts',(-2.76347310470483,7.41266116696907,
98.2572613925988));
#234049=CARTESIAN_POINT('Ctrl Pts',(-2.74453345209575,7.41969442105172,
98.256441350015));
#234050=CARTESIAN_POINT('Ctrl Pts',(-2.64429797543389,7.45648063494276,
98.2520992652728));
#234051=CARTESIAN_POINT('Ctrl Pts',(-2.56254564372747,7.48496992095989,
98.248550527013));
#234052=CARTESIAN_POINT('Ctrl Pts',(-1.74597568241153,7.75458437176633,
98.2130885188211));
#234053=CARTESIAN_POINT('Ctrl Pts',(-0.979994912125664,7.88807472567979,
98.1800996860991));
#234054=CARTESIAN_POINT('Ctrl Pts',(-0.11266906910052,7.91075844304539,
98.1447001808409));
#234055=CARTESIAN_POINT('Ctrl Pts',(-0.0184703696052005,7.91153920400532,
98.140874882418));
#234056=CARTESIAN_POINT('Ctrl Pts',(0.112854666247831,7.91028216295921,
98.1355653958916));
#234057=CARTESIAN_POINT('Ctrl Pts',(0.149985983955524,7.9096652453795,98.1340667765302));
#234058=CARTESIAN_POINT('Ctrl Pts',(0.209845807586467,7.90824903923447,
98.1316547065531));
#234059=CARTESIAN_POINT('Ctrl Pts',(0.232577541969286,7.90761315569268,
98.1307396243286));
#234060=CARTESIAN_POINT('Ctrl Pts',(0.2798873420992,7.90608556337504,98.1288369007036));
#234061=CARTESIAN_POINT('Ctrl Pts',(0.304464636199621,7.90517723706595,
98.1278494343586));
#234062=CARTESIAN_POINT('Ctrl Pts',(0.362583305398953,7.90275784954741,
98.1255165253629));
#234063=CARTESIAN_POINT('Ctrl Pts',(0.396120120879567,7.90114783703582,
98.1241720635184));
#234064=CARTESIAN_POINT('Ctrl Pts',(0.50912983468625,7.89500121727345,98.1196467527056));
#234065=CARTESIAN_POINT('Ctrl Pts',(0.58854453687307,7.88947861837628,98.1164753329699));
#234066=CARTESIAN_POINT('Ctrl Pts',(1.4058058867571,7.82023655966428,98.0838966156612));
#234067=CARTESIAN_POINT('Ctrl Pts',(2.13136554546537,7.65439675169261,98.0555044122154));
#234068=CARTESIAN_POINT('Ctrl Pts',(3.27965524196717,7.21571060593309,98.0097666865299));
#234069=CARTESIAN_POINT('Ctrl Pts',(3.71888922375843,6.9994590252055,97.9919305696375));
#234070=CARTESIAN_POINT('Ctrl Pts',(4.20739686260769,6.69991615517711,97.9695994867845));
#234071=CARTESIAN_POINT('Ctrl Pts',(4.27873687350113,6.6545830104007,97.9662686094557));
#234072=CARTESIAN_POINT('Ctrl Pts',(4.360714858569,6.60062667585319,97.9623450994737));
#234073=CARTESIAN_POINT('Ctrl Pts',(4.37207501447554,6.59310751139124,97.9617992255817));
#234074=CARTESIAN_POINT('Ctrl Pts',(4.39013133139129,6.58108904169181,97.9609280440195));
#234075=CARTESIAN_POINT('Ctrl Pts',(4.39684015749924,6.57660875454432,97.9606035740156));
#234076=CARTESIAN_POINT('Ctrl Pts',(4.40865086101335,6.56869518262951,97.9600309538032));
#234077=CARTESIAN_POINT('Ctrl Pts',(4.41375561663168,6.56526619208987,97.9597829971299));
#234078=CARTESIAN_POINT('Ctrl Pts',(4.42428499844677,6.55817551511852,97.9592705819181));
#234079=CARTESIAN_POINT('Ctrl Pts',(4.42970908801492,6.55451304292014,97.9590060874393));
#234080=CARTESIAN_POINT('Ctrl Pts',(4.44355022691304,6.54514215382548,97.9583297838862));
#234081=CARTESIAN_POINT('Ctrl Pts',(4.45196080951082,6.53942423934994,97.9579175317485));
#234082=CARTESIAN_POINT('Ctrl Pts',(4.48598101578233,6.51619963353444,97.9562446562215));
#234083=CARTESIAN_POINT('Ctrl Pts',(4.51149836492469,6.49855874815916,97.9549775978314));
#234084=CARTESIAN_POINT('Ctrl Pts',(4.67020082270343,6.38745788995528,97.9470161588127));
#234085=CARTESIAN_POINT('Ctrl Pts',(4.80056165880585,6.29007078007476,97.9400957798574));
#234086=CARTESIAN_POINT('Ctrl Pts',(5.0105694808423,6.12285096499516,97.9283795543114));
#234087=CARTESIAN_POINT('Ctrl Pts',(5.09198896246024,6.05530822655395,97.9236909798669));
#234088=CARTESIAN_POINT('Ctrl Pts',(5.92484526801671,5.3357218490174,97.8743665997887));
#234089=CARTESIAN_POINT('Ctrl Pts',(6.54849355655855,4.54882784412921,97.8269174948143));
#234090=CARTESIAN_POINT('Ctrl Pts',(7.03460941131951,3.61953669074862,97.7839044136457));
#234091=CARTESIAN_POINT('Ctrl Pts',(7.05889369760388,3.57194559470995,97.7817293111931));
#234092=CARTESIAN_POINT('Ctrl Pts',(7.0892341465826,3.51096792056043,97.7789770680554));
#234093=CARTESIAN_POINT('Ctrl Pts',(7.09573739736807,3.49780607163347,97.7783850472086));
#234094=CARTESIAN_POINT('Ctrl Pts',(7.1060076491603,3.47687371902962,97.7774467335431));
#234095=CARTESIAN_POINT('Ctrl Pts',(7.10979861526511,3.4691150483896,97.7770996449198));
#234096=CARTESIAN_POINT('Ctrl Pts',(7.11684287507102,3.45463807229611,97.7764533121912));
#234097=CARTESIAN_POINT('Ctrl Pts',(7.12009937642411,3.44792134324858,97.7761539619172));
#234098=CARTESIAN_POINT('Ctrl Pts',(7.12730666041352,3.43300213477449,97.7754901991866));
#234099=CARTESIAN_POINT('Ctrl Pts',(7.13125280234399,3.42479741863431,97.7751259406742));
#234100=CARTESIAN_POINT('Ctrl Pts',(7.14262458273126,3.40104863639578,97.7740738110491));
#234101=CARTESIAN_POINT('Ctrl Pts',(7.15001364417631,3.38548706239659,97.7733871494345));
#234102=CARTESIAN_POINT('Ctrl Pts',(7.20007158751687,3.27916872577874,97.7687144354425));
#234103=CARTESIAN_POINT('Ctrl Pts',(7.24106301463303,3.18763010576617,97.7647838694452));
#234104=CARTESIAN_POINT('Ctrl Pts',(7.34321002655226,2.94737780978454,97.7546939204284));
#234105=CARTESIAN_POINT('Ctrl Pts',(7.40159291619605,2.79753372194274,97.748622991563));
#234106=CARTESIAN_POINT('Ctrl Pts',(7.63187235469365,2.14870062388225,97.723145516042));
#234107=CARTESIAN_POINT('Ctrl Pts',(7.75817701686813,1.63496272931137,97.7050806169576));
#234108=CARTESIAN_POINT('Ctrl Pts',(7.90389431250101,0.609046105023389,
97.6692394029842));
#234109=CARTESIAN_POINT('Ctrl Pts',(7.92668861058478,0.0999348723505103,
97.6515101950275));
#234110=CARTESIAN_POINT('Ctrl Pts',(7.89887480416477,-0.438943935195724,
97.6301551041058));
#234111=CARTESIAN_POINT('Ctrl Pts',(7.89708177687097,-0.470100303620692,
97.628911041364));
#234112=CARTESIAN_POINT('Ctrl Pts',(7.89451090860682,-0.510594041807843,
97.6272826608688));
#234113=CARTESIAN_POINT('Ctrl Pts',(7.8939007354984,-0.519942245465121,
97.6269059444848));
#234114=CARTESIAN_POINT('Ctrl Pts',(7.8928946411101,-0.534946097686244,
97.6263000617729));
#234115=CARTESIAN_POINT('Ctrl Pts',(7.89250924110129,-0.540602462055626,
97.62607136149));
#234116=CARTESIAN_POINT('Ctrl Pts',(7.89177204775266,-0.551253129868674,
97.6256401971175));
#234117=CARTESIAN_POINT('Ctrl Pts',(7.89142159289779,-0.556247525711506,
97.625437791544));
#234118=CARTESIAN_POINT('Ctrl Pts',(7.89080204757728,-0.564958343760852,
97.6250843914673));
#234119=CARTESIAN_POINT('Ctrl Pts',(7.89053507191685,-0.568674918575564,
97.6249334881673));
#234120=CARTESIAN_POINT('Ctrl Pts',(7.88962166897656,-0.581265941003144,
97.6244218509768));
#234121=CARTESIAN_POINT('Ctrl Pts',(7.88896289663079,-0.590139465232265,
97.6240605902673));
#234122=CARTESIAN_POINT('Ctrl Pts',(7.8861055456265,-0.627767454678214,
97.6225258225581));
#234123=CARTESIAN_POINT('Ctrl Pts',(7.88376473312284,-0.656510667787545,
97.6213463887688));
#234124=CARTESIAN_POINT('Ctrl Pts',(7.86570444006156,-0.864230520872862,
97.6127749223484));
#234125=CARTESIAN_POINT('Ctrl Pts',(7.84404957395355,-1.04263214272784,
97.6051567750496));
#234126=CARTESIAN_POINT('Ctrl Pts',(7.78432733841987,-1.42522089297506,
97.5884649572146));
#234127=CARTESIAN_POINT('Ctrl Pts',(7.74425435782694,-1.6289653605696,97.5793562952375));
#234128=CARTESIAN_POINT('Ctrl Pts',(7.60156699884515,-2.22875593543653,
97.5522195903049));
#234129=CARTESIAN_POINT('Ctrl Pts',(7.47620376402859,-2.61869773090331,
97.5341911939636));
#234130=CARTESIAN_POINT('Ctrl Pts',(7.20091743896093,-3.29113722886374,
97.5031479440812));
#234131=CARTESIAN_POINT('Ctrl Pts',(7.06299073186216,-3.57756580146288,
97.4899292018986));
#234132=CARTESIAN_POINT('Ctrl Pts',(6.89052104924574,-3.88663843036336,
97.4755994736329));
#234133=CARTESIAN_POINT('Ctrl Pts',(6.87261491027139,-3.91821425397549,
97.4741344588587));
#234134=CARTESIAN_POINT('Ctrl Pts',(6.84616946736213,-3.96410929476055,
97.4720031321892));
#234135=CARTESIAN_POINT('Ctrl Pts',(6.83780129532769,-3.97852640116299,
97.4713333309792));
#234136=CARTESIAN_POINT('Ctrl Pts',(6.82290663583917,-4.00400186264425,
97.4701492163409));
#234137=CARTESIAN_POINT('Ctrl Pts',(6.81639868405345,-4.01507096557286,
97.469634531202));
#234138=CARTESIAN_POINT('Ctrl Pts',(6.8028344951548,-4.03801369523629,97.4685673344463));
#234139=CARTESIAN_POINT('Ctrl Pts',(6.79577405242389,-4.04988478862642,
97.4680149089954));
#234140=CARTESIAN_POINT('Ctrl Pts',(6.77748307365309,-4.08045585650678,
97.4665916220001));
#234141=CARTESIAN_POINT('Ctrl Pts',(6.76620620198897,-4.09912801067916,
97.465721677794));
#234142=CARTESIAN_POINT('Ctrl Pts',(6.7201009909639,-4.17476000254316,97.4621950614631));
#234143=CARTESIAN_POINT('Ctrl Pts',(6.68462906274458,-4.23132519085822,
97.459550601175));
#234144=CARTESIAN_POINT('Ctrl Pts',(6.45728884726687,-4.58385741142495,
97.4430216263116));
#234145=CARTESIAN_POINT('Ctrl Pts',(6.24651789831679,-4.86717169079069,
97.4295475751767));
#234146=CARTESIAN_POINT('Ctrl Pts',(5.91429754827461,-5.25645286689566,
97.4104048282614));
#234147=CARTESIAN_POINT('Ctrl Pts',(5.80743553853075,-5.37428187207255,
97.4045137992596));
#234148=CARTESIAN_POINT('Ctrl Pts',(5.31623529636951,-5.88412160894045,
97.3784050879208));
#234149=CARTESIAN_POINT('Ctrl Pts',(4.89529163319778,-6.23869281471567,
97.3586364561451));
#234150=CARTESIAN_POINT('Ctrl Pts',(4.37641363173298,-6.59067753915491,
97.3341219362174));
#234151=CARTESIAN_POINT('Ctrl Pts',(4.31110396341263,-6.63358190113328,
97.3310320996757));
#234152=CARTESIAN_POINT('Ctrl Pts',(4.23324072961883,-6.6830976208728,97.3273329669173));
#234153=CARTESIAN_POINT('Ctrl Pts',(4.22129038384432,-6.69065231327108,
97.3267648059197));
#234154=CARTESIAN_POINT('Ctrl Pts',(4.20316790516017,-6.70204098425758,
97.3259024807639));
#234155=CARTESIAN_POINT('Ctrl Pts',(4.19701060101924,-6.70589858319689,
97.3256093713385));
#234156=CARTESIAN_POINT('Ctrl Pts',(4.18597430524439,-6.7127917541905,97.3250837675339));
#234157=CARTESIAN_POINT('Ctrl Pts',(4.18109729939925,-6.71583050649923,
97.3248514172835));
#234158=CARTESIAN_POINT('Ctrl Pts',(4.17158418683911,-6.72174353327335,
97.3243980255361));
#234159=CARTESIAN_POINT('Ctrl Pts',(4.16694840879681,-6.72461833215975,
97.3241770082256));
#234160=CARTESIAN_POINT('Ctrl Pts',(4.15419726639016,-6.73250748792315,
97.3235688575524));
#234161=CARTESIAN_POINT('Ctrl Pts',(4.14607581571627,-6.73751195414856,
97.3231812679069));
#234162=CARTESIAN_POINT('Ctrl Pts',(4.11422975906141,-6.75705621947615,
97.321660411413));
#234163=CARTESIAN_POINT('Ctrl Pts',(4.09043774722936,-6.7714853815049,97.3205219548706));
#234164=CARTESIAN_POINT('Ctrl Pts',(3.94713314485832,-6.85736460318705,
97.3136489570119));
#234165=CARTESIAN_POINT('Ctrl Pts',(3.82584460669583,-6.92576468231635,
97.3077515178323));
#234166=CARTESIAN_POINT('Ctrl Pts',(3.65800909225906,-7.01466045760386,
97.2995043446516));
#234167=CARTESIAN_POINT('Ctrl Pts',(3.61297598823876,-7.03796108349436,
97.2972843908482));
#234168=CARTESIAN_POINT('Ctrl Pts',(3.3912744158515,-7.14998333623823,97.2863318644217));
#234169=CARTESIAN_POINT('Ctrl Pts',(3.21155198915956,-7.23249142353882,
97.2773820831093));
#234170=CARTESIAN_POINT('Ctrl Pts',(2.4974465171754,-7.52845837444701,97.2420287634282));
#234171=CARTESIAN_POINT('Ctrl Pts',(1.94345023894368,-7.69012622675716,
97.2151970324276));
#234172=CARTESIAN_POINT('Ctrl Pts',(1.11296720159382,-7.8369004144202,97.1784567016048));
#234173=CARTESIAN_POINT('Ctrl Pts',(0.846919968658294,-7.87009843947016,
97.1671615363555));
#234174=CARTESIAN_POINT('Ctrl Pts',(0.557157220673652,-7.89138814892926,
97.1553923440016));
#234175=CARTESIAN_POINT('Ctrl Pts',(0.534625753112108,-7.89294662348092,
97.1544806030023));
#234176=CARTESIAN_POINT('Ctrl Pts',(0.503146392704338,-7.89498859990009,
97.1532115153219));
#234177=CARTESIAN_POINT('Ctrl Pts',(0.494203994516476,-7.8955534129998,
97.1528515363164));
#234178=CARTESIAN_POINT('Ctrl Pts',(0.47874625648298,-7.89650337930094,
97.1522301985457));
#234179=CARTESIAN_POINT('Ctrl Pts',(0.472231372786632,-7.89689566400964,
97.1519686087453));
#234180=CARTESIAN_POINT('Ctrl Pts',(0.458734057238549,-7.89769162361928,
97.151427238254));
#234181=CARTESIAN_POINT('Ctrl Pts',(0.451751558753382,-7.89809410215934,
97.1511474965939));
#234182=CARTESIAN_POINT('Ctrl Pts',(0.43541242072116,-7.89901416874995,
97.1504936506222));
#234183=CARTESIAN_POINT('Ctrl Pts',(0.426055367752419,-7.89952439319272,
97.1501197857091));
#234184=CARTESIAN_POINT('Ctrl Pts',(0.395900672461138,-7.90111494442952,
97.148916796736));
#234185=CARTESIAN_POINT('Ctrl Pts',(0.375099582037465,-7.90212977746612,
97.148089801807));
#234186=CARTESIAN_POINT('Ctrl Pts',(-0.0983086388039994,-7.92335268774623,
97.1293323925826));
#234187=CARTESIAN_POINT('Ctrl Pts',(-0.55183535311112,-7.90472804229589,
97.112765214267));
#234188=CARTESIAN_POINT('Ctrl Pts',(-1.0870814065756,-7.83643092504216,
97.0939974216306));
#234189=CARTESIAN_POINT('Ctrl Pts',(-1.17265761534474,-7.82408269597081,
97.0910185094886));
#234190=CARTESIAN_POINT('Ctrl Pts',(-1.32685541977588,-7.79924596596974,
97.0856747036307));
#234191=CARTESIAN_POINT('Ctrl Pts',(-1.39554654178061,-7.78724809551117,
97.0833027570642));
#234192=CARTESIAN_POINT('Ctrl Pts',(-1.52138513928129,-7.76355007276849,
97.078964124061));
#234193=CARTESIAN_POINT('Ctrl Pts',(-1.57857888554986,-7.75212301359285,
97.0769947437771));
#234194=CARTESIAN_POINT('Ctrl Pts',(-1.68441625714541,-7.72975731292474,
97.073349291532));
#234195=CARTESIAN_POINT('Ctrl Pts',(-1.73309285279156,-7.71898927457733,
97.0716722408739));
#234196=CARTESIAN_POINT('Ctrl Pts',(-1.82377949637822,-7.69802687663649,
97.0685431431637));
#234197=CARTESIAN_POINT('Ctrl Pts',(-1.86581403278651,-7.68794689375911,
97.067090872675));
#234198=CARTESIAN_POINT('Ctrl Pts',(-1.94450794494458,-7.668392487707,97.0643658513458));
#234199=CARTESIAN_POINT('Ctrl Pts',(-1.98118600098433,-7.65899840184089,
97.0630932223467));
#234200=CARTESIAN_POINT('Ctrl Pts',(-2.05011182788473,-7.64081667948913,
97.0606950561623));
#234201=CARTESIAN_POINT('Ctrl Pts',(-2.08237409248248,-7.63208727479302,
97.0595697927056));
#234202=CARTESIAN_POINT('Ctrl Pts',(-2.38991179157687,-7.54677965773142,
97.0488104032862));
#234203=CARTESIAN_POINT('Ctrl Pts',(-2.66089297880733,-7.45554804472596,
97.0390838333108));
#234204=CARTESIAN_POINT('Ctrl Pts',(-2.95544793416656,-7.33827163696595,
97.0277046475114));
#234205=CARTESIAN_POINT('Ctrl Pts',(-2.98449431646108,-7.32650644949623,
97.0265735405876));
#234206=CARTESIAN_POINT('Ctrl Pts',(-3.20204233674662,-7.23688061067491,
97.0180291766725));
#234207=CARTESIAN_POINT('Ctrl Pts',(-3.387527165248,-7.15193429327303,97.0103331980211));
#234208=CARTESIAN_POINT('Ctrl Pts',(-3.58147309248776,-7.05387490738756,
97.0016389137599));
#234209=CARTESIAN_POINT('Ctrl Pts',(-3.59342140412005,-7.04779563618024,
97.0011006137207));
#234210=CARTESIAN_POINT('Ctrl Pts',(-3.609831478186,-7.03939365292522,97.00035754079));
#234211=CARTESIAN_POINT('Ctrl Pts',(-3.6143066253133,-7.0370969809812,97.000154513961));
#234212=CARTESIAN_POINT('Ctrl Pts',(-3.62195261705451,-7.03316379535545,
96.9998069694008));
#234213=CARTESIAN_POINT('Ctrl Pts',(-3.62512455528011,-7.03152939914952,
96.9996625950277));
#234214=CARTESIAN_POINT('Ctrl Pts',(-3.63128403903065,-7.0283503426705,
96.9993818570926));
#234215=CARTESIAN_POINT('Ctrl Pts',(-3.63427170745572,-7.02680592216284,
96.9992455098853));
#234216=CARTESIAN_POINT('Ctrl Pts',(-3.64043672014641,-7.02361404807074,
96.9989637966468));
#234217=CARTESIAN_POINT('Ctrl Pts',(-3.64361393596606,-7.02196634108187,
96.9988184131689));
#234218=CARTESIAN_POINT('Ctrl Pts',(-3.65358671515299,-7.01678585785531,
96.998361449238));
#234219=CARTESIAN_POINT('Ctrl Pts',(-3.66037824053363,-7.01324538252634,
96.9980493384985));
#234220=CARTESIAN_POINT('Ctrl Pts',(-3.6990555269746,-6.99301112497675,
96.996266720671));
#234221=CARTESIAN_POINT('Ctrl Pts',(-3.73083172242819,-6.97611001635202,
96.9947821322729));
#234222=CARTESIAN_POINT('Ctrl Pts',(-3.82266437292896,-6.92645922350291,
96.9904361626955));
#234223=CARTESIAN_POINT('Ctrl Pts',(-3.88241162748855,-6.89314730079322,
96.9875392229692));
#234224=CARTESIAN_POINT('Ctrl Pts',(-4.12028799247174,-6.75644625445476,
96.9757511101894));
#234225=CARTESIAN_POINT('Ctrl Pts',(-4.29477302543572,-6.64689805947475,
96.9665269777069));
#234226=CARTESIAN_POINT('Ctrl Pts',(-5.08515710944068,-6.10654252811286,
96.9227603463567));
#234227=CARTESIAN_POINT('Ctrl Pts',(-5.64209332043876,-5.59605366965307,
96.8865898642591));
#234228=CARTESIAN_POINT('Ctrl Pts',(-6.13647518402876,-4.99283365392006,
96.8528472234301));
#234229=CARTESIAN_POINT('Ctrl Pts',(-6.15422668879896,-4.97093647769951,
96.8516322777974));
#234230=CARTESIAN_POINT('Ctrl Pts',(-6.29891077143058,-4.79050002478239,
96.8417023983538));
#234231=CARTESIAN_POINT('Ctrl Pts',(-6.41981772064854,-4.62721477507735,
96.8332327952869));
#234232=CARTESIAN_POINT('Ctrl Pts',(-6.54584743837429,-4.44254667765714,
96.8242003543207));
#234233=CARTESIAN_POINT('Ctrl Pts',(-6.55731602983917,-4.42560122054253,
96.8233763921531));
#234234=CARTESIAN_POINT('Ctrl Pts',(-6.57339052286024,-4.40165063478374,
96.8222186196142));
#234235=CARTESIAN_POINT('Ctrl Pts',(-6.5780511785332,-4.39468246519611,
96.8218825865981));
#234236=CARTESIAN_POINT('Ctrl Pts',(-6.58614125202555,-4.3825452522256,
96.8212986836526));
#234237=CARTESIAN_POINT('Ctrl Pts',(-6.58957567821953,-4.37737956552921,
96.8210506110078));
#234238=CARTESIAN_POINT('Ctrl Pts',(-6.59672942018752,-4.36659219452174,
96.8205334843954));
#234239=CARTESIAN_POINT('Ctrl Pts',(-6.60044763497629,-4.36096978373847,
96.8202644750014));
#234240=CARTESIAN_POINT('Ctrl Pts',(-6.60922164385051,-4.34766544655475,
96.8196291391425));
#234241=CARTESIAN_POINT('Ctrl Pts',(-6.61427124313944,-4.33997943493695,
96.8192630625266));
#234242=CARTESIAN_POINT('Ctrl Pts',(-6.63088592528815,-4.31459382460092,
96.81805713107));
#234243=CARTESIAN_POINT('Ctrl Pts',(-6.64239350312258,-4.29685659344748,
96.8172195869929));
#234244=CARTESIAN_POINT('Ctrl Pts',(-6.86078402861689,-3.95726591806099,
96.8012797745708));
#234245=CARTESIAN_POINT('Ctrl Pts',(-7.04412841430869,-3.62085730145171,
96.7871615447161));
#234246=CARTESIAN_POINT('Ctrl Pts',(-7.47772863296214,-2.66654043363741,
96.7501634853319));
#234247=CARTESIAN_POINT('Ctrl Pts',(-7.67544320725768,-2.02837060757967,
96.7288386857934));
#234248=CARTESIAN_POINT('Ctrl Pts',(-7.7952034678766,-1.34882487862752,
96.7037970958478));
#234249=CARTESIAN_POINT('Ctrl Pts',(-7.79935834272993,-1.32458864760173,
96.702900643586));
#234250=CARTESIAN_POINT('Ctrl Pts',(-7.83365740191113,-1.11875740237589,
96.695256090629));
#234251=CARTESIAN_POINT('Ctrl Pts',(-7.85756594021687,-0.936191805727175,
96.6882699676156));
#234252=CARTESIAN_POINT('Ctrl Pts',(-7.87632171246219,-0.740031256710166,
96.6803832776849));
#234253=CARTESIAN_POINT('Ctrl Pts',(-7.87752705804985,-0.727088321453079,
96.6798611270636));
#234254=CARTESIAN_POINT('Ctrl Pts',(-7.87915986638815,-0.709074532588748,
96.6791319020082));
#234255=CARTESIAN_POINT('Ctrl Pts',(-7.87961432542802,-0.704006374364151,
96.6789264618666));
#234256=CARTESIAN_POINT('Ctrl Pts',(-7.88039063958191,-0.695253942890348,
96.67857120983));
#234257=CARTESIAN_POINT('Ctrl Pts',(-7.88071480206095,-0.691569870654439,
96.6784215339873));
#234258=CARTESIAN_POINT('Ctrl Pts',(-7.88136168965207,-0.684158544125279,
96.6781201416991));
#234259=CARTESIAN_POINT('Ctrl Pts',(-7.88168435440607,-0.680431285311236,
96.6779684217495));
#234260=CARTESIAN_POINT('Ctrl Pts',(-7.88233353941262,-0.672869810082374,
96.6776603346862));
#234261=CARTESIAN_POINT('Ctrl Pts',(-7.88265990628726,-0.669035581699117,
96.6775039587012));
#234262=CARTESIAN_POINT('Ctrl Pts',(-7.8834049525076,-0.660206391793181,
96.677143517224));
#234263=CARTESIAN_POINT('Ctrl Pts',(-7.88382168202179,-0.655211271916484,
96.6769393393908));
#234264=CARTESIAN_POINT('Ctrl Pts',(-7.88488188966348,-0.642355655122257,
96.676413202506));
#234265=CARTESIAN_POINT('Ctrl Pts',(-7.88551835968058,-0.634494601941113,
96.6760908436201));
#234266=CARTESIAN_POINT('Ctrl Pts',(-7.88854611848681,-0.596390395890846,
96.6745252785793));
#234267=CARTESIAN_POINT('Ctrl Pts',(-7.89077515304799,-0.566134970075116,
96.6732729651777));
#234268=CARTESIAN_POINT('Ctrl Pts',(-7.90491782061927,-0.35782676751667,
96.6645907929568));
#234269=CARTESIAN_POINT('Ctrl Pts',(-7.91097706688777,-0.179439737976786,
96.6568546686882));
#234270=CARTESIAN_POINT('Ctrl Pts',(-7.91099993502481,-0.00101392183331238,
96.6489153477367));
#234271=CARTESIAN_POINT('',(-7.91099714745356,0.0067181084832415,92.642331465206));
#234272=CARTESIAN_POINT('Ctrl Pts',(-7.91099992838748,-0.00106444979291354,
96.6489175960477));
#234273=CARTESIAN_POINT('Ctrl Pts',(-7.91112606604236,0.936391675789824,
96.6072042977785));
#234274=CARTESIAN_POINT('Ctrl Pts',(-7.74464776818924,1.86658964603236,
96.5613040616377));
#234275=CARTESIAN_POINT('Ctrl Pts',(-7.37225732492007,2.87261232096405,
96.515391247615));
#234276=CARTESIAN_POINT('Ctrl Pts',(-7.32225597777836,2.997774072022,96.5097266405357));
#234277=CARTESIAN_POINT('Ctrl Pts',(-7.24051843157264,3.18811121311503,
96.5011836088845));
#234278=CARTESIAN_POINT('Ctrl Pts',(-7.21104498509999,3.25422661382722,
96.4982295178264));
#234279=CARTESIAN_POINT('Ctrl Pts',(-7.17426417101405,3.33377975320426,
96.4946900890407));
#234280=CARTESIAN_POINT('Ctrl Pts',(-7.16782048081803,3.34761159582746,
96.4940752459597));
#234281=CARTESIAN_POINT('Ctrl Pts',(-7.15773495856991,3.3690982649268,96.4931209798907));
#234282=CARTESIAN_POINT('Ctrl Pts',(-7.15412079098113,3.37676599196542,
96.4927806083711));
#234283=CARTESIAN_POINT('Ctrl Pts',(-7.14772809875032,3.3902722360213,96.4921813557626));
#234284=CARTESIAN_POINT('Ctrl Pts',(-7.14495473036879,3.39611317674163,
96.4919222979246));
#234285=CARTESIAN_POINT('Ctrl Pts',(-7.1386091011567,3.40943541241606,96.491331646539));
#234286=CARTESIAN_POINT('Ctrl Pts',(-7.13503223232001,3.41691451090665,
96.4910002117557));
#234287=CARTESIAN_POINT('Ctrl Pts',(-7.12536407475329,3.43704888841134,
96.4901083768383));
#234288=CARTESIAN_POINT('Ctrl Pts',(-7.11925081768732,3.44969361778151,
96.4895487330531));
#234289=CARTESIAN_POINT('Ctrl Pts',(-7.09094902630095,3.50783771305206,
96.4869773193002));
#234290=CARTESIAN_POINT('Ctrl Pts',(-7.06835754716253,3.55314019128705,
96.4849794532567));
#234291=CARTESIAN_POINT('Ctrl Pts',(-6.61660128359404,4.43768038779073,
96.446068835574));
#234292=CARTESIAN_POINT('Ctrl Pts',(-6.04138787031093,5.19363179699353,
96.415640779593));
#234293=CARTESIAN_POINT('Ctrl Pts',(-5.26929880219813,5.90164866033169,
96.3779414276778));
#234294=CARTESIAN_POINT('Ctrl Pts',(-5.19043195064273,5.97112903773125,
96.3741077306436));
#234295=CARTESIAN_POINT('Ctrl Pts',(-4.97893972581641,6.15009343639504,
96.3638096700428));
#234296=CARTESIAN_POINT('Ctrl Pts',(-4.84410764189707,6.2568448589424,96.3572078913845));
#234297=CARTESIAN_POINT('Ctrl Pts',(-4.68436825884356,6.37505544805819,
96.3493060686769));
#234298=CARTESIAN_POINT('Ctrl Pts',(-4.66276429612681,6.39087373120974,
96.3482363535364));
#234299=CARTESIAN_POINT('Ctrl Pts',(-4.6328027838359,6.41257856468144,96.346751778361));
#234300=CARTESIAN_POINT('Ctrl Pts',(-4.62451337066542,6.41855915027333,
96.3463409337103));
#234301=CARTESIAN_POINT('Ctrl Pts',(-4.61112630960793,6.42817815409404,
96.3456772852174));
#234302=CARTESIAN_POINT('Ctrl Pts',(-4.60603587731121,6.43182662395389,
96.3454248975896));
#234303=CARTESIAN_POINT('Ctrl Pts',(-4.59549690655387,6.4393613014867,96.3449023016151));
#234304=CARTESIAN_POINT('Ctrl Pts',(-4.59004775928498,6.4432466471813,96.3446320585883));
#234305=CARTESIAN_POINT('Ctrl Pts',(-4.57735381027875,6.45227339910649,
96.3440024452216));
#234306=CARTESIAN_POINT('Ctrl Pts',(-4.57010527186256,6.45740952121629,
96.3436428652483));
#234307=CARTESIAN_POINT('Ctrl Pts',(-4.5475074369631,6.47336464001756,96.342521704661));
#234308=CARTESIAN_POINT('Ctrl Pts',(-4.53212831028888,6.48414116322664,
96.3417584835249));
#234309=CARTESIAN_POINT('Ctrl Pts',(-4.3909636874175,6.58231102930137,96.3347518365509));
#234310=CARTESIAN_POINT('Ctrl Pts',(-4.26270643225895,6.66608669771378,
96.3283788878));
#234311=CARTESIAN_POINT('Ctrl Pts',(-4.02232137531487,6.81332703208748,
96.3165035678335));
#234312=CARTESIAN_POINT('Ctrl Pts',(-3.9109166285087,6.87787937850078,96.3110259757728));
#234313=CARTESIAN_POINT('Ctrl Pts',(-3.46203577043441,7.12354535458856,
96.289141026107));
#234314=CARTESIAN_POINT('Ctrl Pts',(-3.11317458882525,7.28277005616153,
96.2725728543569));
#234315=CARTESIAN_POINT('Ctrl Pts',(-2.08033885132131,7.66633901058044,
96.2255394957139));
#234316=CARTESIAN_POINT('Ctrl Pts',(-1.37554052595554,7.8235868619562,96.1958601734888));
#234317=CARTESIAN_POINT('Ctrl Pts',(-0.602047832060468,7.88826666571952,
96.1643803485787));
#234318=CARTESIAN_POINT('Ctrl Pts',(-0.544824503784611,7.89242541302795,
96.1620596381402));
#234319=CARTESIAN_POINT('Ctrl Pts',(-0.461180203914722,7.89759029111265,
96.1586792652638));
#234320=CARTESIAN_POINT('Ctrl Pts',(-0.43479160321472,7.8990870266449,96.1576145229645));
#234321=CARTESIAN_POINT('Ctrl Pts',(-0.388289055237259,7.90149087051021,
96.1557412037622));
#234322=CARTESIAN_POINT('Ctrl Pts',(-0.368178241835084,7.90245348939801,
96.1549320402608));
#234323=CARTESIAN_POINT('Ctrl Pts',(-0.328934248886238,7.90418179919584,
96.1533549476245));
#234324=CARTESIAN_POINT('Ctrl Pts',(-0.309801532411928,7.90495481756091,
96.1525869441367));
#234325=CARTESIAN_POINT('Ctrl Pts',(-0.263717667904164,7.90664917616683,
96.1507391886713));
#234326=CARTESIAN_POINT('Ctrl Pts',(-0.236764218452382,7.90750219189215,
96.149660198029));
#234327=CARTESIAN_POINT('Ctrl Pts',(-0.137199209179035,7.91014367509163,
96.1456806500123));
#234328=CARTESIAN_POINT('Ctrl Pts',(-0.0645680399432022,7.91106994535592,
96.1427898437642));
#234329=CARTESIAN_POINT('Ctrl Pts',(0.498073740995025,7.9104962780555,96.120481805984));
#234330=CARTESIAN_POINT('Ctrl Pts',(0.98697778256932,7.86447193005222,96.1016773502992));
#234331=CARTESIAN_POINT('Ctrl Pts',(1.79946607830078,7.71098572564421,96.0699039738262));
#234332=CARTESIAN_POINT('Ctrl Pts',(2.12610682622432,7.62738718828368,96.0569589182298));
#234333=CARTESIAN_POINT('Ctrl Pts',(2.47688655717082,7.51332022770222,96.0422997172878));
#234334=CARTESIAN_POINT('Ctrl Pts',(2.50729986178603,7.50322565586212,96.0410222380319));
#234335=CARTESIAN_POINT('Ctrl Pts',(2.56067202756923,7.4851500005111,96.0387680455842));
#234336=CARTESIAN_POINT('Ctrl Pts',(2.58365709671294,7.47724733882676,96.0377932027137));
#234337=CARTESIAN_POINT('Ctrl Pts',(2.61821093918432,7.46518878328519,96.0363212942662));
#234338=CARTESIAN_POINT('Ctrl Pts',(2.62980701394639,7.46111165713496,96.0358262512677));
#234339=CARTESIAN_POINT('Ctrl Pts',(2.65090079563317,7.45363989612313,96.0349238126177));
#234340=CARTESIAN_POINT('Ctrl Pts',(2.66040161203556,7.45025408904559,96.0345166311289));
#234341=CARTESIAN_POINT('Ctrl Pts',(2.68060190583431,7.44301174081976,96.0336493938243));
#234342=CARTESIAN_POINT('Ctrl Pts',(2.69129959076237,7.43915027831298,96.0331892230564));
#234343=CARTESIAN_POINT('Ctrl Pts',(2.71412200616947,7.43085657169618,96.032205605208));
#234344=CARTESIAN_POINT('Ctrl Pts',(2.72624428552801,7.4264176927865,96.0316820082028));
#234345=CARTESIAN_POINT('Ctrl Pts',(2.77985113925099,7.40663924567325,96.0293616004284));
#234346=CARTESIAN_POINT('Ctrl Pts',(2.82121726741933,7.39098169060062,96.0275578514512));
#234347=CARTESIAN_POINT('Ctrl Pts',(3.19822882969589,7.24465222577795,96.0110046246551));
#234348=CARTESIAN_POINT('Ctrl Pts',(3.52470983348601,7.0915488473174,95.9958584135305));
#234349=CARTESIAN_POINT('Ctrl Pts',(4.18664986221276,6.7240932347035,95.9640538006204));
#234350=CARTESIAN_POINT('Ctrl Pts',(4.51870293257877,6.50559800253946,95.9474516459493));
#234351=CARTESIAN_POINT('Ctrl Pts',(4.95021052194207,6.17262273574143,95.9250761000726));
#234352=CARTESIAN_POINT('Ctrl Pts',(5.06490071532491,6.0788681044449,95.9190394777778));
#234353=CARTESIAN_POINT('Ctrl Pts',(5.2089409687579,5.95421290498354,95.9113300281022));
#234354=CARTESIAN_POINT('Ctrl Pts',(5.24076595283447,5.92622051441109,95.909618272721));
#234355=CARTESIAN_POINT('Ctrl Pts',(5.2920429269082,5.88038258476053,95.9068460750739));
#234356=CARTESIAN_POINT('Ctrl Pts',(5.31163317732874,5.86269312505263,95.9057835474417));
#234357=CARTESIAN_POINT('Ctrl Pts',(5.34913245400674,5.82849006121531,95.9037429265578));
#234358=CARTESIAN_POINT('Ctrl Pts',(5.36705445168012,5.81199113223914,95.9027646502257));
#234359=CARTESIAN_POINT('Ctrl Pts',(5.40801773433818,5.77392942592453,95.9005215797971));
#234360=CARTESIAN_POINT('Ctrl Pts',(5.43100679776116,5.75231101404095,95.8992575449625));
#234361=CARTESIAN_POINT('Ctrl Pts',(5.50440143074161,5.68246010973172,95.8952047075492));
#234362=CARTESIAN_POINT('Ctrl Pts',(5.55429872883775,5.63369805110749,95.8924229352468));
#234363=CARTESIAN_POINT('Ctrl Pts',(5.69604626380118,5.49146156812846,95.8844377955807));
#234364=CARTESIAN_POINT('Ctrl Pts',(5.78622769704016,5.39635642092132,95.879254874931));
#234365=CARTESIAN_POINT('Ctrl Pts',(6.07802218370891,5.07290204212425,95.8620839095294));
#234366=CARTESIAN_POINT('Ctrl Pts',(6.26881218279405,4.83515163644925,95.8502122673796));
#234367=CARTESIAN_POINT('Ctrl Pts',(6.74045963660932,4.17241449987347,95.8190606844011));
#234368=CARTESIAN_POINT('Ctrl Pts',(6.99480803763235,3.73034910938752,95.8003027982792));
#234369=CARTESIAN_POINT('Ctrl Pts',(7.28775531029806,3.08427629279857,95.7739133009784));
#234370=CARTESIAN_POINT('Ctrl Pts',(7.36359426547428,2.89855381132946,95.766419754105));
#234371=CARTESIAN_POINT('Ctrl Pts',(7.49385953923858,2.54131603198224,95.7519303800023));
#234372=CARTESIAN_POINT('Ctrl Pts',(7.54965268590818,2.37043403216245,95.7449673268109));
#234373=CARTESIAN_POINT('Ctrl Pts',(7.60415937881971,2.18196087762608,95.7371294163135));
#234374=CARTESIAN_POINT('Ctrl Pts',(7.60869274489973,2.16609968348544,95.7364685886054));
#234375=CARTESIAN_POINT('Ctrl Pts',(7.61532303176484,2.14262420739654,95.7354885867236));
#234376=CARTESIAN_POINT('Ctrl Pts',(7.61745822982439,2.13502072321874,95.7351708731105));
#234377=CARTESIAN_POINT('Ctrl Pts',(7.62119291660905,2.12164450619232,95.7346113982401));
#234378=CARTESIAN_POINT('Ctrl Pts',(7.62279724313438,2.11587312300213,95.7343698252611));
#234379=CARTESIAN_POINT('Ctrl Pts',(7.62612263656586,2.10385752474214,95.7338665069474));
#234380=CARTESIAN_POINT('Ctrl Pts',(7.62784259260812,2.09761300873886,95.7336047180498));
#234381=CARTESIAN_POINT('Ctrl Pts',(7.63221434299466,2.0816643402125,95.7329355410488));
#234382=CARTESIAN_POINT('Ctrl Pts',(7.63485529473338,2.07195724617636,95.732527719397));
#234383=CARTESIAN_POINT('Ctrl Pts',(7.64502282531641,2.03430202973873,95.7309435835658));
#234384=CARTESIAN_POINT('Ctrl Pts',(7.65241445697131,2.0063179448237,95.7297617478609));
#234385=CARTESIAN_POINT('Ctrl Pts',(7.76121732718517,1.58504988589116,95.711894281484));
#234386=CARTESIAN_POINT('Ctrl Pts',(7.83232820882552,1.18464516550145,95.6937280205191));
#234387=CARTESIAN_POINT('Ctrl Pts',(7.91015132266054,0.39983138607443,95.6576537711324));
#234388=CARTESIAN_POINT('Ctrl Pts',(7.92023283714517,0.0167780115089239,
95.6398635594541));
#234389=CARTESIAN_POINT('Ctrl Pts',(7.88516424848162,-0.741448352493183,
95.6054171829064));
#234390=CARTESIAN_POINT('Ctrl Pts',(7.84097021598678,-1.11570189230857,
95.5887936846303));
#234391=CARTESIAN_POINT('Ctrl Pts',(7.74314841723535,-1.62741318513683,
95.5668612218789));
#234392=CARTESIAN_POINT('Ctrl Pts',(7.71211531104413,-1.76864391508049,
95.5608899635125));
#234393=CARTESIAN_POINT('Ctrl Pts',(7.67268046905092,-1.92723911293059,
95.5542734488224));
#234394=CARTESIAN_POINT('Ctrl Pts',(7.66806746468618,-1.9455121540871,95.5535124401826));
#234395=CARTESIAN_POINT('Ctrl Pts',(7.66104546727304,-1.97291472005736,
95.552373193876));
#234396=CARTESIAN_POINT('Ctrl Pts',(7.65868537131834,-1.9820566410106,95.5519934541954));
#234397=CARTESIAN_POINT('Ctrl Pts',(7.6546005299008,-1.99776319822395,95.5513415947661));
#234398=CARTESIAN_POINT('Ctrl Pts',(7.65288369451128,-2.00432986982757,
95.5510692319275));
#234399=CARTESIAN_POINT('Ctrl Pts',(7.64933285576365,-2.01784029117552,
95.5505092134893));
#234400=CARTESIAN_POINT('Ctrl Pts',(7.64749784344183,-2.02478376964562,
95.5502215893161));
#234401=CARTESIAN_POINT('Ctrl Pts',(7.64306137320567,-2.04147880356667,
95.5495304717041));
#234402=CARTESIAN_POINT('Ctrl Pts',(7.64045070154433,-2.05122790987058,
95.5491272627168));
#234403=CARTESIAN_POINT('Ctrl Pts',(7.63239534645694,-2.08108050505075,
95.5478937279424));
#234404=CARTESIAN_POINT('Ctrl Pts',(7.62688990363295,-2.10116757996013,
95.5470652784247));
#234405=CARTESIAN_POINT('Ctrl Pts',(7.56374376454962,-2.32804319796375,
95.5377255944393));
#234406=CARTESIAN_POINT('Ctrl Pts',(7.49778631868551,-2.53243227134478,
95.5294778723722));
#234407=CARTESIAN_POINT('Ctrl Pts',(7.15868178240451,-3.45323355992984,
95.4928152974298));
#234408=CARTESIAN_POINT('Ctrl Pts',(6.79065580776811,-4.13018923469821,
95.4676558548608));
#234409=CARTESIAN_POINT('Ctrl Pts',(6.13344078174204,-5.00733610958948,
95.4286956010771));
#234410=CARTESIAN_POINT('Ctrl Pts',(5.91956726488576,-5.25844314229553,
95.4165614002616));
#234411=CARTESIAN_POINT('Ctrl Pts',(5.68023469576563,-5.50627644462431,
95.4027889115777));
#234412=CARTESIAN_POINT('Ctrl Pts',(5.66977288703903,-5.51704829490635,
95.4021866736221));
#234413=CARTESIAN_POINT('Ctrl Pts',(5.65447897966661,-5.53270600051181,
95.4013060602173));
#234414=CARTESIAN_POINT('Ctrl Pts',(5.64967103983775,-5.53761549412487,
95.4010291914705));
#234415=CARTESIAN_POINT('Ctrl Pts',(5.64129585698006,-5.54614531779369,
95.4005468573699));
#234416=CARTESIAN_POINT('Ctrl Pts',(5.63773150519665,-5.54976849131596,
95.4003415697169));
#234417=CARTESIAN_POINT('Ctrl Pts',(5.63039136479274,-5.55721539593551,
95.3999187938522));
#234418=CARTESIAN_POINT('Ctrl Pts',(5.62661516729661,-5.56103871920512,
95.3997012807777));
#234419=CARTESIAN_POINT('Ctrl Pts',(5.61713125484368,-5.57062143881782,
95.3991549729164));
#234420=CARTESIAN_POINT('Ctrl Pts',(5.61141858342267,-5.57637590462522,
95.3988258803135));
#234421=CARTESIAN_POINT('Ctrl Pts',(5.59023512029023,-5.59764883397976,
95.397605508479));
#234422=CARTESIAN_POINT('Ctrl Pts',(5.57470880854338,-5.6131116909807,95.3967109529389));
#234423=CARTESIAN_POINT('Ctrl Pts',(5.53746368343128,-5.64989763898267,
95.3945652868947));
#234424=CARTESIAN_POINT('Ctrl Pts',(5.51568574554323,-5.67116020753079,
95.393310859427));
#234425=CARTESIAN_POINT('Ctrl Pts',(5.47610709162652,-5.70935861366829,
95.3910323080453));
#234426=CARTESIAN_POINT('Ctrl Pts',(5.45834906073824,-5.72633828666108,
95.3900104089556));
#234427=CARTESIAN_POINT('Ctrl Pts',(4.98593981003197,-6.17384712607264,
95.3628433557496));
#234428=CARTESIAN_POINT('Ctrl Pts',(4.48185296354909,-6.54897051752987,
95.3345431406337));
#234429=CARTESIAN_POINT('Ctrl Pts',(3.56009478625329,-7.07815934688124,
95.2883918433917));
#234430=CARTESIAN_POINT('Ctrl Pts',(3.16401394654728,-7.26386119618355,
95.2699906132983));
#234431=CARTESIAN_POINT('Ctrl Pts',(2.71754108066484,-7.4297008454467,95.2506916782674));
#234432=CARTESIAN_POINT('Ctrl Pts',(2.68037536293075,-7.44318964732422,
95.2490951157419));
#234433=CARTESIAN_POINT('Ctrl Pts',(2.62666406241629,-7.46222898019171,
95.2468015484371));
#234434=CARTESIAN_POINT('Ctrl Pts',(2.61019896470891,-7.46800420574946,
95.2461003132636));
#234435=CARTESIAN_POINT('Ctrl Pts',(2.58150971520609,-7.47796065094888,
95.2448816232682));
#234436=CARTESIAN_POINT('Ctrl Pts',(2.56929419624123,-7.48216648044811,
95.2443637152936));
#234437=CARTESIAN_POINT('Ctrl Pts',(2.54571295048071,-7.49022099566367,
95.2433658170558));
#234438=CARTESIAN_POINT('Ctrl Pts',(2.5343486649334,-7.49407378103334,95.2428857534428));
#234439=CARTESIAN_POINT('Ctrl Pts',(2.50742182570655,-7.50313441842114,
95.2417502455319));
#234440=CARTESIAN_POINT('Ctrl Pts',(2.49185173220609,-7.50831973612383,
95.2410952060604));
#234441=CARTESIAN_POINT('Ctrl Pts',(2.43756177918868,-7.52621247840697,
95.2388164978652));
#234442=CARTESIAN_POINT('Ctrl Pts',(2.39875971449485,-7.53866921695688,
95.2371971626599));
#234443=CARTESIAN_POINT('Ctrl Pts',(1.84431488878029,-7.71195011490613,
95.2141861639005));
#234444=CARTESIAN_POINT('Ctrl Pts',(1.31361063968508,-7.81985605369122,
95.1938664240161));
#234445=CARTESIAN_POINT('Ctrl Pts',(0.370468989098573,-7.91282198341236,
95.1589041990029));
#234446=CARTESIAN_POINT('Ctrl Pts',(-0.0375636228363237,-7.92139958600949,
95.1441088451984));
#234447=CARTESIAN_POINT('Ctrl Pts',(-0.599349254782895,-7.889789511908,
95.1228751832535));
#234448=CARTESIAN_POINT('Ctrl Pts',(-0.753977925213433,-7.87651652901819,
95.1169357260577));
#234449=CARTESIAN_POINT('Ctrl Pts',(-0.979708179982585,-7.85043230877517,
95.1080297989279));
#234450=CARTESIAN_POINT('Ctrl Pts',(-1.05118730491298,-7.84118106037849,
95.1051748027151));
#234451=CARTESIAN_POINT('Ctrl Pts',(-1.13554506277208,-7.8290887923174,
95.1017559347112));
#234452=CARTESIAN_POINT('Ctrl Pts',(-1.1485567254491,-7.82719051470026,
95.1012271993877));
#234453=CARTESIAN_POINT('Ctrl Pts',(-1.16853655918385,-7.82422475419203,
95.1004130982736));
#234454=CARTESIAN_POINT('Ctrl Pts',(-1.17550817160751,-7.82318037835862,
95.1001286181859));
#234455=CARTESIAN_POINT('Ctrl Pts',(-1.18819096737012,-7.82126310800646,
95.0996103253936));
#234456=CARTESIAN_POINT('Ctrl Pts',(-1.19390261284005,-7.82039327210771,
95.0993766318645));
#234457=CARTESIAN_POINT('Ctrl Pts',(-1.20632168409,-7.81848802878117,95.0988678798762));
#234458=CARTESIAN_POINT('Ctrl Pts',(-1.21302873682976,-7.81745024576097,
95.0985927279567));
#234459=CARTESIAN_POINT('Ctrl Pts',(-1.23122537547122,-7.81461069612075,
95.0978451362602));
#234460=CARTESIAN_POINT('Ctrl Pts',(-1.24271230964406,-7.81279222625603,
95.0973720289084));
#234461=CARTESIAN_POINT('Ctrl Pts',(-1.29684933164786,-7.80409950590402,
95.095136617336));
#234462=CARTESIAN_POINT('Ctrl Pts',(-1.339446092445,-7.79690139389565,95.0933610546442));
#234463=CARTESIAN_POINT('Ctrl Pts',(-2.16340539959627,-7.65071518909409,
95.0586629026643));
#234464=CARTESIAN_POINT('Ctrl Pts',(-2.91942620267822,-7.3953036560385,
95.020389810409));
#234465=CARTESIAN_POINT('Ctrl Pts',(-3.79709335058799,-6.94288160360653,
94.9760591146227));
#234466=CARTESIAN_POINT('Ctrl Pts',(-3.96613406190936,-6.84772294323324,
94.9674986720219));
#234467=CARTESIAN_POINT('Ctrl Pts',(-4.26507314195986,-6.66465302452364,
94.9523845130701));
#234468=CARTESIAN_POINT('Ctrl Pts',(-4.39617833532916,-6.57891089801474,
94.9457644321755));
#234469=CARTESIAN_POINT('Ctrl Pts',(-4.59032185486511,-6.44354517049231,
94.9359820711478));
#234470=CARTESIAN_POINT('Ctrl Pts',(-4.65528919948562,-6.39676575101305,
94.9327120108043));
#234471=CARTESIAN_POINT('Ctrl Pts',(-4.73177696848006,-6.33990854298436,
94.9288655419062));
#234472=CARTESIAN_POINT('Ctrl Pts',(-4.74399095416185,-6.33077431624114,
94.9282514208236));
#234473=CARTESIAN_POINT('Ctrl Pts',(-4.76277516646231,-6.31664166012848,
94.9273070967002));
#234474=CARTESIAN_POINT('Ctrl Pts',(-4.76936407885932,-6.31166819728203,
94.9269758857795));
#234475=CARTESIAN_POINT('Ctrl Pts',(-4.78137133039626,-6.30257530922573,
94.9263723555379));
#234476=CARTESIAN_POINT('Ctrl Pts',(-4.78679215669524,-6.29845919066783,
94.9260999025356));
#234477=CARTESIAN_POINT('Ctrl Pts',(-4.79860650162472,-6.28946431118315,
94.9255061470036));
#234478=CARTESIAN_POINT('Ctrl Pts',(-4.80499790990156,-6.28458278372031,
94.9251849575151));
#234479=CARTESIAN_POINT('Ctrl Pts',(-4.82241370065629,-6.27123913142877,
94.9243098195065));
#234480=CARTESIAN_POINT('Ctrl Pts',(-4.83342327031411,-6.26275767026416,
94.9237566615132));
#234481=CARTESIAN_POINT('Ctrl Pts',(-4.88621376775106,-6.22186724335033,
94.9211045844746));
#234482=CARTESIAN_POINT('Ctrl Pts',(-4.9276918808517,-6.18906857678055,
94.9190217227572));
#234483=CARTESIAN_POINT('Ctrl Pts',(-5.7128860395509,-5.55528133793307,
94.8795995642244));
#234484=CARTESIAN_POINT('Ctrl Pts',(-6.34176891206572,-4.82493001242914,
94.8494209936139));
#234485=CARTESIAN_POINT('Ctrl Pts',(-6.92332855934655,-3.83263788035091,
94.809624523115));
#234486=CARTESIAN_POINT('Ctrl Pts',(-7.0152673793104,-3.66164016699497,
94.8027556528994));
#234487=CARTESIAN_POINT('Ctrl Pts',(-7.16716401441824,-3.35236174937193,
94.7900332542353));
#234488=CARTESIAN_POINT('Ctrl Pts',(-7.22963522771145,-3.21542204489982,
94.7843003702489));
#234489=CARTESIAN_POINT('Ctrl Pts',(-7.29732526497413,-3.05508106954919,
94.7773856129795));
#234490=CARTESIAN_POINT('Ctrl Pts',(-7.30639360304725,-3.03332966533883,
94.7764433395965));
#234491=CARTESIAN_POINT('Ctrl Pts',(-7.31793311761285,-3.00529888929421,
94.7752232247743));
#234492=CARTESIAN_POINT('Ctrl Pts',(-7.32049372070677,-2.99905622027662,
94.7749511256988));
#234493=CARTESIAN_POINT('Ctrl Pts',(-7.32460511466163,-2.98899613448557,
94.7745120299967));
#234494=CARTESIAN_POINT('Ctrl Pts',(-7.32616092007986,-2.98518075678214,
94.7743453585601));
#234495=CARTESIAN_POINT('Ctrl Pts',(-7.3291168040358,-2.97791566931651,
94.774027719301));
#234496=CARTESIAN_POINT('Ctrl Pts',(-7.33051743008273,-2.97446618200943,
94.7738767872619));
#234497=CARTESIAN_POINT('Ctrl Pts',(-7.33370471017912,-2.96660056601358,
94.773532361148));
#234498=CARTESIAN_POINT('Ctrl Pts',(-7.3354897991977,-2.96218383969471,
94.7733387659113));
#234499=CARTESIAN_POINT('Ctrl Pts',(-7.34099629414028,-2.94852398550127,
94.7727394274853));
#234500=CARTESIAN_POINT('Ctrl Pts',(-7.34470419931075,-2.93927550706612,
94.7723328024397));
#234501=CARTESIAN_POINT('Ctrl Pts',(-7.37323238705918,-2.86772774479975,
94.7691807564148));
#234502=CARTESIAN_POINT('Ctrl Pts',(-7.39727637142868,-2.80512388474049,
94.7663856983754));
#234503=CARTESIAN_POINT('Ctrl Pts',(-7.61554935348937,-2.21447216511167,
94.7397271656991));
#234504=CARTESIAN_POINT('Ctrl Pts',(-7.75371053990945,-1.66745036305818,
94.7130116411022));
#234505=CARTESIAN_POINT('Ctrl Pts',(-7.88453464447883,-0.744659888212214,
94.6695735779369));
#234506=CARTESIAN_POINT('Ctrl Pts',(-7.9107087703331,-0.375673156917667,
94.6525943800661));
#234507=CARTESIAN_POINT('Ctrl Pts',(-7.91122201221791,0.280936946069419,
94.623756332697));
#234508=CARTESIAN_POINT('Ctrl Pts',(-7.89581557996747,0.567873452934318,
94.6116136198462));
#234509=CARTESIAN_POINT('Ctrl Pts',(-7.86242790963038,0.875584398980283,
94.5990981324223));
#234510=CARTESIAN_POINT('Ctrl Pts',(-7.85992245178328,0.897797158235373,
94.5981974599803));
#234511=CARTESIAN_POINT('Ctrl Pts',(-7.85631024691878,0.928647469896319,
94.5969503791823));
#234512=CARTESIAN_POINT('Ctrl Pts',(-7.8552833490821,0.937294150986242,
94.5966012667754));
#234513=CARTESIAN_POINT('Ctrl Pts',(-7.85349040312374,0.952181188843237,
94.5960009134457));
#234514=CARTESIAN_POINT('Ctrl Pts',(-7.85273118888152,0.958422351461388,
94.595749441133));
#234515=CARTESIAN_POINT('Ctrl Pts',(-7.85114927927588,0.971298457531457,
94.5952310752899));
#234516=CARTESIAN_POINT('Ctrl Pts',(-7.85032561128993,0.977933277945624,
94.5949642149399));
#234517=CARTESIAN_POINT('Ctrl Pts',(-7.84838972364556,0.993367206418321,
94.5943440092636));
#234518=CARTESIAN_POINT('Ctrl Pts',(-7.84727111468852,1.00216551242569,
94.5939908807898));
#234519=CARTESIAN_POINT('Ctrl Pts',(-7.8436644668592,1.03015692778844,94.5928687707562));
#234520=CARTESIAN_POINT('Ctrl Pts',(-7.84112078192757,1.04934286821054,
94.5921016757835));
#234521=CARTESIAN_POINT('Ctrl Pts',(-7.79599753792367,1.38036059113958,
94.5789013097026));
#234522=CARTESIAN_POINT('Ctrl Pts',(-7.73491601324756,1.68940011153656,
94.5671229575886));
#234523=CARTESIAN_POINT('Ctrl Pts',(-7.50536082086748,2.57073160343405,
94.5344139622122));
#234524=CARTESIAN_POINT('Ctrl Pts',(-7.29046929547689,3.12859702176804,
94.5149473897396));
#234525=CARTESIAN_POINT('Ctrl Pts',(-6.85953880646736,3.95521445890848,
94.4824994298255));
#234526=CARTESIAN_POINT('Ctrl Pts',(-6.68525380758608,4.24315121881615,
94.4703740778455));
#234527=CARTESIAN_POINT('Ctrl Pts',(-6.48045185030031,4.53741810511691,
94.4561222977885));
#234528=CARTESIAN_POINT('Ctrl Pts',(-6.46762349377499,4.55568497405468,
94.4552295474633));
#234529=CARTESIAN_POINT('Ctrl Pts',(-6.45066188073635,4.57962132901756,
94.4540487470388));
#234530=CARTESIAN_POINT('Ctrl Pts',(-6.44659815367386,4.58533995045091,
94.4537658194258));
#234531=CARTESIAN_POINT('Ctrl Pts',(-6.44027350929476,4.59421518885608,
94.4533254485057));
#234532=CARTESIAN_POINT('Ctrl Pts',(-6.43801785676583,4.59737557220386,
94.4531683861077));
#234533=CARTESIAN_POINT('Ctrl Pts',(-6.43349447941282,4.60370339603459,
94.4528534101656));
#234534=CARTESIAN_POINT('Ctrl Pts',(-6.431226739806,4.60687082480029,94.4526954955576));
#234535=CARTESIAN_POINT('Ctrl Pts',(-6.4261559439075,4.61394233639957,94.4523423800092));
#234536=CARTESIAN_POINT('Ctrl Pts',(-6.42335166963501,4.61784553953872,
94.4521470920519));
#234537=CARTESIAN_POINT('Ctrl Pts',(-6.41513421398519,4.62926125392239,
94.4515748205565));
#234538=CARTESIAN_POINT('Ctrl Pts',(-6.4097114136782,4.6367667972927,94.4511971552335));
#234539=CARTESIAN_POINT('Ctrl Pts',(-6.37004643354941,4.69146341368938,
94.4484347146137));
#234540=CARTESIAN_POINT('Ctrl Pts',(-6.33529745322873,4.73828306195219,
94.4460145727601));
#234541=CARTESIAN_POINT('Ctrl Pts',(-6.22106550429026,4.88869234459986,
94.4380700166816));
#234542=CARTESIAN_POINT('Ctrl Pts',(-6.13953740350233,4.99069596489229,
94.4324173013784));
#234543=CARTESIAN_POINT('Ctrl Pts',(-5.9120210914342,5.26133651859309,94.4167930238903));
#234544=CARTESIAN_POINT('Ctrl Pts',(-5.7613674939071,5.42589080614565,94.4066063155981));
#234545=CARTESIAN_POINT('Ctrl Pts',(-5.42125914027264,5.76722458469051,
94.3843126146277));
#234546=CARTESIAN_POINT('Ctrl Pts',(-5.22965678887514,5.94151659274608,
94.3721757143731));
#234547=CARTESIAN_POINT('Ctrl Pts',(-4.92331560667846,6.19386287784564,
94.35371361287));
#234548=CARTESIAN_POINT('Ctrl Pts',(-4.81449526407076,6.27882237541689,
94.3473218559523));
#234549=CARTESIAN_POINT('Ctrl Pts',(-4.55761183383273,6.46877257752144,
94.3326639334802));
#234550=CARTESIAN_POINT('Ctrl Pts',(-4.40804484790486,6.57160477402897,
94.3244455144689));
#234551=CARTESIAN_POINT('Ctrl Pts',(-4.24042784836438,6.67854731801089,
94.3156103218769));
#234552=CARTESIAN_POINT('Ctrl Pts',(-4.22575609915171,6.68784030992249,
94.3148400144216));
#234553=CARTESIAN_POINT('Ctrl Pts',(-4.16886558809881,6.72361244143509,
94.3118649551015));
#234554=CARTESIAN_POINT('Ctrl Pts',(-4.12642719504461,6.74974097780123,
94.3096708344453));
#234555=CARTESIAN_POINT('Ctrl Pts',(-3.84115024000805,6.92168456783268,
94.2950914254933));
#234556=CARTESIAN_POINT('Ctrl Pts',(-3.59086528591821,7.05477575493315,
94.283126780237));
#234557=CARTESIAN_POINT('Ctrl Pts',(-3.31246037903762,7.18415543647104,
94.2706781561009));
#234558=CARTESIAN_POINT('Ctrl Pts',(-3.29091508140821,7.1940503916617,94.2697201186449));
#234559=CARTESIAN_POINT('Ctrl Pts',(-3.26078498605123,7.20772434532195,
94.268387722456));
#234560=CARTESIAN_POINT('Ctrl Pts',(-3.25223756431176,7.21158510935278,
94.2680105683121));
#234561=CARTESIAN_POINT('Ctrl Pts',(-3.23746076469172,7.21822799180887,
94.2673599623386));
#234562=CARTESIAN_POINT('Ctrl Pts',(-3.23123462486104,7.22101726518295,
94.2670862666242));
#234563=CARTESIAN_POINT('Ctrl Pts',(-3.21833691026475,7.22677534281028,
94.2665201902334));
#234564=CARTESIAN_POINT('Ctrl Pts',(-3.21166481579589,7.22974297155696,
94.2662278497354));
#234565=CARTESIAN_POINT('Ctrl Pts',(-3.1960575149201,7.23665895205102,94.2655451635215));
#234566=CARTESIAN_POINT('Ctrl Pts',(-3.18711907641673,7.24060000418424,
94.265155065939));
#234567=CARTESIAN_POINT('Ctrl Pts',(-3.15834831084868,7.25322174079708,
94.2639022562941));
#234568=CARTESIAN_POINT('Ctrl Pts',(-3.13848756604615,7.26183761048352,
94.2630417389403));
#234569=CARTESIAN_POINT('Ctrl Pts',(-2.68902687998292,7.45463164397244,
94.2436638462352));
#234570=CARTESIAN_POINT('Ctrl Pts',(-2.24395415014403,7.6004689903636,94.2265305156132));
#234571=CARTESIAN_POINT('Ctrl Pts',(-1.3296458246873,7.81267736419065,94.1934214767998));
#234572=CARTESIAN_POINT('Ctrl Pts',(-0.862131941818696,7.87798156403184,
94.1775059102993));
#234573=CARTESIAN_POINT('Ctrl Pts',(-0.272659089714595,7.90719670582171,
94.1564748440106));
#234574=CARTESIAN_POINT('Ctrl Pts',(-0.1536026088649,7.91040502904463,94.152175192663));
#234575=CARTESIAN_POINT('Ctrl Pts',(0.173987047569121,7.91183457340231,
94.1401085122769));
#234576=CARTESIAN_POINT('Ctrl Pts',(0.382413096933918,7.90450208480821,
94.1321371875806));
#234577=CARTESIAN_POINT('Ctrl Pts',(0.610010060304839,7.88747096059922,
94.1230303318664));
#234578=CARTESIAN_POINT('Ctrl Pts',(0.629683288720923,7.88592476350584,
94.1222402588328));
#234579=CARTESIAN_POINT('Ctrl Pts',(0.658252937186033,7.88357177065612,
94.1210888734911));
#234580=CARTESIAN_POINT('Ctrl Pts',(0.667154185192994,7.88282348431344,
94.1207295751329));
#234581=CARTESIAN_POINT('Ctrl Pts',(0.682843879193456,7.88147775969365,
94.1200952758218));
#234582=CARTESIAN_POINT('Ctrl Pts',(0.689632865342825,7.88088662211402,
94.1198204867809));
#234583=CARTESIAN_POINT('Ctrl Pts',(0.703650088699174,7.87964784870312,
94.1192524667211));
#234584=CARTESIAN_POINT('Ctrl Pts',(0.710878214463638,7.87899903735989,
94.1189591971604));
#234585=CARTESIAN_POINT('Ctrl Pts',(0.729346540244259,7.87731566187197,
94.118208957556));
#234586=CARTESIAN_POINT('Ctrl Pts',(0.740585419917201,7.87626698677392,
94.1177515317865));
#234587=CARTESIAN_POINT('Ctrl Pts',(0.786208646362108,7.87191146949555,
94.1158912075553));
#234588=CARTESIAN_POINT('Ctrl Pts',(0.820573170336826,7.86840351364132,
94.1144820194374));
#234589=CARTESIAN_POINT('Ctrl Pts',(1.28752181315138,7.81764479271208,94.0952332723437));
#234590=CARTESIAN_POINT('Ctrl Pts',(1.7155016658782,7.73500590644631,94.0764696006769));
#234591=CARTESIAN_POINT('Ctrl Pts',(2.83724127996136,7.42068775152626,94.0263430553656));
#234592=CARTESIAN_POINT('Ctrl Pts',(3.50939901040711,7.12746512953161,93.99562021129));
#234593=CARTESIAN_POINT('Ctrl Pts',(4.32027635140846,6.63083506586048,93.9565187478429));
#234594=CARTESIAN_POINT('Ctrl Pts',(4.50382027500275,6.50756229891525,93.9474824738646));
#234595=CARTESIAN_POINT('Ctrl Pts',(4.71589951209192,6.35184896037064,93.9368345450673));
#234596=CARTESIAN_POINT('Ctrl Pts',(4.74963557114221,6.3266622628682,93.9351341412914));
#234597=CARTESIAN_POINT('Ctrl Pts',(4.80175903272139,6.28709598381034,93.9324965560913));
#234598=CARTESIAN_POINT('Ctrl Pts',(4.82028647950243,6.27290235677451,93.9315569489415));
#234599=CARTESIAN_POINT('Ctrl Pts',(4.85399777920864,6.24683903919197,93.9298434857699));
#234600=CARTESIAN_POINT('Ctrl Pts',(4.86920157744939,6.23499546292231,93.9290692832884));
#234601=CARTESIAN_POINT('Ctrl Pts',(4.90254001282529,6.20882890938538,93.9273684571031));
#234602=CARTESIAN_POINT('Ctrl Pts',(4.92065548939076,6.19448178318537,93.9264421766341));
#234603=CARTESIAN_POINT('Ctrl Pts',(4.97057067787954,6.15459273426823,93.9238840693339));
#234604=CARTESIAN_POINT('Ctrl Pts',(5.0022361887982,6.12888388883201,93.9222546363481));
#234605=CARTESIAN_POINT('Ctrl Pts',(5.18338321580237,5.97947370517252,93.9128940434347));
#234606=CARTESIAN_POINT('Ctrl Pts',(5.32847424731431,5.85054970465887,93.9052434734407));
#234607=CARTESIAN_POINT('Ctrl Pts',(5.78435237888315,5.41442849967996,93.8805882002261));
#234608=CARTESIAN_POINT('Ctrl Pts',(6.07446599011095,5.08680976318078,93.8639396131964));
#234609=CARTESIAN_POINT('Ctrl Pts',(6.42623309184015,4.61629002832633,93.8412951881687));
#234610=CARTESIAN_POINT('Ctrl Pts',(6.51295253341472,4.49311179998054,93.8354669276539));
#234611=CARTESIAN_POINT('Ctrl Pts',(6.66866209012494,4.25795029522806,93.8244363427727));
#234612=CARTESIAN_POINT('Ctrl Pts',(6.73847891609442,4.14657634858243,93.8192504351364));
#234613=CARTESIAN_POINT('Ctrl Pts',(6.81572015897925,4.01625229528203,93.8131858969797));
#234614=CARTESIAN_POINT('Ctrl Pts',(6.82588706981406,3.99894854842869,93.8123807425546));
#234615=CARTESIAN_POINT('Ctrl Pts',(6.84233364529022,3.97071155448646,93.8110667822638));
#234616=CARTESIAN_POINT('Ctrl Pts',(6.84865319825554,3.9598016782416,93.8105591017631));
#234617=CARTESIAN_POINT('Ctrl Pts',(6.85999224575863,3.94011796308261,93.8096431594107));
#234618=CARTESIAN_POINT('Ctrl Pts',(6.86502106191644,3.93134951303079,93.8092351443102));
#234619=CARTESIAN_POINT('Ctrl Pts',(6.87571337677937,3.9126228799643,93.808363789536));
#234620=CARTESIAN_POINT('Ctrl Pts',(6.8813720760621,3.90266198769901,93.8079003286378));
#234621=CARTESIAN_POINT('Ctrl Pts',(6.89638197394832,3.87610622965771,93.8066648367283));
#234622=CARTESIAN_POINT('Ctrl Pts',(6.90569488926282,3.85948985309928,93.8058918683782));
#234623=CARTESIAN_POINT('Ctrl Pts',(6.94834410286881,3.78274529019253,93.8023225813965));
#234624=CARTESIAN_POINT('Ctrl Pts',(6.98095541691311,3.72221828863484,93.7995096908244));
#234625=CARTESIAN_POINT('Ctrl Pts',(7.07125692281705,3.5492555711758,93.7914857241954));
#234626=CARTESIAN_POINT('Ctrl Pts',(7.12704743643019,3.43585268210878,93.7862417623378));
#234627=CARTESIAN_POINT('Ctrl Pts',(7.35122789373618,2.95119201350464,93.7639673073234));
#234628=CARTESIAN_POINT('Ctrl Pts',(7.49350800194589,2.56854587001984,93.7467441039212));
#234629=CARTESIAN_POINT('Ctrl Pts',(7.64593524376229,2.03593124103031,93.7236458965112));
#234630=CARTESIAN_POINT('Ctrl Pts',(7.68229223272481,1.89413005387359,93.7175737724449));
#234631=CARTESIAN_POINT('Ctrl Pts',(7.71960480154008,1.72977298279587,93.7106255511862));
#234632=CARTESIAN_POINT('Ctrl Pts',(7.72442378518012,1.70812471857691,93.7097121331885));
#234633=CARTESIAN_POINT('Ctrl Pts',(7.76451305479354,1.52439270026603,93.7019746958401));
#234634=CARTESIAN_POINT('Ctrl Pts',(7.79476892142191,1.36125493476479,93.6952034887261));
#234635=CARTESIAN_POINT('Ctrl Pts',(7.82666707831053,1.15291719469416,93.6866679830586));
#234636=CARTESIAN_POINT('Ctrl Pts',(7.83308239195482,1.1084926169771,93.6848542737141));
#234637=CARTESIAN_POINT('Ctrl Pts',(7.84272740284494,1.03743314714883,93.6819627300506));
#234638=CARTESIAN_POINT('Ctrl Pts',(7.84620026418977,1.01083236508913,93.6808824325776));
#234639=CARTESIAN_POINT('Ctrl Pts',(7.85247858747658,0.96076000607758,93.6788527840488));
#234640=CARTESIAN_POINT('Ctrl Pts',(7.8553142823438,0.937292529382736,93.6779031400515));
#234641=CARTESIAN_POINT('Ctrl Pts',(7.86148233222033,0.884252322759162,
93.6757602553155));
#234642=CARTESIAN_POINT('Ctrl Pts',(7.86475308579494,0.854672766203541,
93.6745676348455));
#234643=CARTESIAN_POINT('Ctrl Pts',(7.87395177301604,0.766954777258875,
93.6710377259206));
#234644=CARTESIAN_POINT('Ctrl Pts',(7.87940250714819,0.708768184263577,
93.6687050577511));
#234645=CARTESIAN_POINT('Ctrl Pts',(7.91181445717617,0.315943863752889,
93.6530090742436));
#234646=CARTESIAN_POINT('Ctrl Pts',(7.91809547976187,-0.0200691808325795,
93.6397912824133));
#234647=CARTESIAN_POINT('Ctrl Pts',(7.88246650305884,-0.812204302438391,
93.6090295604024));
#234648=CARTESIAN_POINT('Ctrl Pts',(7.82236783998412,-1.26630810601944,
93.5918342402346));
#234649=CARTESIAN_POINT('Ctrl Pts',(7.63483161802273,-2.11200403984446,
93.5596322899469));
#234650=CARTESIAN_POINT('Ctrl Pts',(7.51545073566851,-2.50383510961908,
93.544615627285));
#234651=CARTESIAN_POINT('Ctrl Pts',(7.35759270602529,-2.90694396725511,
93.5279838569819));
#234652=CARTESIAN_POINT('Ctrl Pts',(7.34876577606518,-2.92918678397641,
93.5270620579119));
#234653=CARTESIAN_POINT('Ctrl Pts',(7.29645218561974,-3.05928595740922,
93.5216449017439));
#234654=CARTESIAN_POINT('Ctrl Pts',(7.25069345143284,-3.16621037333604,
93.5170899067403));
#234655=CARTESIAN_POINT('Ctrl Pts',(7.19573428570986,-3.28718790017869,
93.5117818568856));
#234656=CARTESIAN_POINT('Ctrl Pts',(7.18882533294422,-3.30226990554375,
93.5111173324279));
#234657=CARTESIAN_POINT('Ctrl Pts',(7.17858516789987,-3.32443939852791,
93.5101362872784));
#234658=CARTESIAN_POINT('Ctrl Pts',(7.17529076425434,-3.33154390262833,
93.5098212556013));
#234659=CARTESIAN_POINT('Ctrl Pts',(7.16940624213313,-3.34418487774112,
93.5092595592789));
#234660=CARTESIAN_POINT('Ctrl Pts',(7.16682024312357,-3.34972326674019,
93.5090130649506));
#234661=CARTESIAN_POINT('Ctrl Pts',(7.16140827480436,-3.36127902985214,
93.5084979161466));
#234662=CARTESIAN_POINT('Ctrl Pts',(7.15858113491976,-3.367295848212,93.5082292126132));
#234663=CARTESIAN_POINT('Ctrl Pts',(7.15121190364722,-3.38292808023746,
93.5075298386109));
#234664=CARTESIAN_POINT('Ctrl Pts',(7.14665801132307,-3.39253789288611,
93.5070986638222));
#234665=CARTESIAN_POINT('Ctrl Pts',(7.12706014445318,-3.43367955364797,
93.5052472872058));
#234666=CARTESIAN_POINT('Ctrl Pts',(7.11182690932603,-3.46512042168759,
93.5038187703604));
#234667=CARTESIAN_POINT('Ctrl Pts',(7.0087836114271,-3.67425630091621,93.4942189738057));
#234668=CARTESIAN_POINT('Ctrl Pts',(6.91454293229927,-3.84867293255867,
93.4857067873669));
#234669=CARTESIAN_POINT('Ctrl Pts',(6.5249394799104,-4.50915438052681,93.4518608291704));
#234670=CARTESIAN_POINT('Ctrl Pts',(6.18404803753021,-4.96637298060165,
93.4250847676656));
#234671=CARTESIAN_POINT('Ctrl Pts',(5.44609423212617,-5.76108094856937,
93.3757759149911));
#234672=CARTESIAN_POINT('Ctrl Pts',(5.0589376286557,-6.10387315705764,93.3532033669588));
#234673=CARTESIAN_POINT('Ctrl Pts',(4.61462806830041,-6.42574496260809,
93.3308621108159));
#234674=CARTESIAN_POINT('Ctrl Pts',(4.58802473122907,-6.4447668406944,93.3295364440292));
#234675=CARTESIAN_POINT('Ctrl Pts',(4.55132901054998,-6.47066258500791,
93.3277241909724));
#234676=CARTESIAN_POINT('Ctrl Pts',(4.54133771000652,-6.47767873984393,
93.3272324102615));
#234677=CARTESIAN_POINT('Ctrl Pts',(4.52542961294611,-6.48879492937695,
93.3264520081732));
#234678=CARTESIAN_POINT('Ctrl Pts',(4.51952341173672,-6.49291005238266,
93.3261628377541));
#234679=CARTESIAN_POINT('Ctrl Pts',(4.50804243261533,-6.50088612502279,
93.325601826317));
#234680=CARTESIAN_POINT('Ctrl Pts',(4.50246829152182,-6.50474797889296,
93.3253299525591));
#234681=CARTESIAN_POINT('Ctrl Pts',(4.48915680725946,-6.51394507889376,
93.324681894441));
#234682=CARTESIAN_POINT('Ctrl Pts',(4.48141490093967,-6.51927371855084,
93.3243059497563));
#234683=CARTESIAN_POINT('Ctrl Pts',(4.45829414707282,-6.5351267446416,93.3231860741039));
#234684=CARTESIAN_POINT('Ctrl Pts',(4.44288754249752,-6.54561063315618,
93.3224436074644));
#234685=CARTESIAN_POINT('Ctrl Pts',(4.31559528936557,-6.63157400682703,
93.3163399831584));
#234686=CARTESIAN_POINT('Ctrl Pts',(4.20182912189778,-6.704235276218,93.3110808125507));
#234687=CARTESIAN_POINT('Ctrl Pts',(3.79935886917099,-6.94701768958947,
93.2931017066865));
#234688=CARTESIAN_POINT('Ctrl Pts',(3.50174532691547,-7.10168883375342,
93.2809131527402));
#234689=CARTESIAN_POINT('Ctrl Pts',(2.97881577772075,-7.33256636260571,
93.2607083088823));
#234690=CARTESIAN_POINT('Ctrl Pts',(2.75824760198039,-7.41835195616723,
93.2525243664555));
#234691=CARTESIAN_POINT('Ctrl Pts',(1.98418392025008,-7.68010433793855,
93.224300440226));
#234692=CARTESIAN_POINT('Ctrl Pts',(1.41545544807959,-7.80495566424273,
93.2044710471174));
#234693=CARTESIAN_POINT('Ctrl Pts',(0.800849768687063,-7.87044959479491,
93.1800964019728));
#234694=CARTESIAN_POINT('Ctrl Pts',(0.763402977698106,-7.87416998292571,
93.1785993274632));
#234695=CARTESIAN_POINT('Ctrl Pts',(0.715853097766556,-7.87855175660551,
93.1766840017607));
#234696=CARTESIAN_POINT('Ctrl Pts',(0.705772841400102,-7.87946115759324,
93.1762771552465));
#234697=CARTESIAN_POINT('Ctrl Pts',(0.689790695397059,-7.88087208881772,
93.1756308497309));
#234698=CARTESIAN_POINT('Ctrl Pts',(0.683889916658087,-7.88138634158845,
93.1753919558666));
#234699=CARTESIAN_POINT('Ctrl Pts',(0.672955053347862,-7.88232694196387,
93.1749487612706));
#234700=CARTESIAN_POINT('Ctrl Pts',(0.66792112377951,-7.88275509552809,
93.174744539621));
#234701=CARTESIAN_POINT('Ctrl Pts',(0.656732302666678,-7.88369594975943,
93.1742901931732));
#234702=CARTESIAN_POINT('Ctrl Pts',(0.650577217806672,-7.88420626499466,
93.1740399655663));
#234703=CARTESIAN_POINT('Ctrl Pts',(0.632905151774223,-7.88565061249343,
93.1733207171843));
#234704=CARTESIAN_POINT('Ctrl Pts',(0.62138674353115,-7.88656661839868,
93.1728509315357));
#234705=CARTESIAN_POINT('Ctrl Pts',(0.546025504451834,-7.89239362782978,
93.169770983005));
#234706=CARTESIAN_POINT('Ctrl Pts',(0.482128174153243,-7.89655451092597,
93.1671300400059));
#234707=CARTESIAN_POINT('Ctrl Pts',(0.281070754108038,-7.90719762179349,
93.1587416628477));
#234708=CARTESIAN_POINT('Ctrl Pts',(0.143790888509328,-7.91088471384464,
93.152899873522));
#234709=CARTESIAN_POINT('Ctrl Pts',(-0.106758280771778,-7.9110902322365,
93.1421039948765));
#234710=CARTESIAN_POINT('Ctrl Pts',(-0.219993158767414,-7.9087513727691,
93.1371747867954));
#234711=CARTESIAN_POINT('Ctrl Pts',(-0.41923005130492,-7.90035393812578,
93.1284483179304));
#234712=CARTESIAN_POINT('Ctrl Pts',(-0.505257665495175,-7.89531891209549,
93.1246626849966));
#234713=CARTESIAN_POINT('Ctrl Pts',(-0.788410399395188,-7.8740997076641,
93.1121688126791));
#234714=CARTESIAN_POINT('Ctrl Pts',(-0.985013203383412,-7.85192887484135,
93.1034420305356));
#234715=CARTESIAN_POINT('Ctrl Pts',(-1.71091301869714,-7.74237420288489,
93.071276949285));
#234716=CARTESIAN_POINT('Ctrl Pts',(-2.23176868919481,-7.60860577114906,
93.0484443528242));
#234717=CARTESIAN_POINT('Ctrl Pts',(-2.77033914028371,-7.41016540461729,
93.0251942740174));
#234718=CARTESIAN_POINT('Ctrl Pts',(-2.80547177393867,-7.39693574603399,
93.0236785411096));
#234719=CARTESIAN_POINT('Ctrl Pts',(-2.85654121518628,-7.37728868596842,
93.0214761654429));
#234720=CARTESIAN_POINT('Ctrl Pts',(-2.87255324179364,-7.37106871124965,
93.0207857770316));
#234721=CARTESIAN_POINT('Ctrl Pts',(-2.90037999603011,-7.36015478738467,
93.0195861473025));
#234722=CARTESIAN_POINT('Ctrl Pts',(-2.91220388562658,-7.35548442628075,
93.0190764660169));
#234723=CARTESIAN_POINT('Ctrl Pts',(-2.92462211874586,-7.35054466603471,
93.018541207372));
#234724=CARTESIAN_POINT('Ctrl Pts',(-2.92522772180758,-7.35030368082826,
93.0185151043867));
#234725=CARTESIAN_POINT('Ctrl Pts',(-2.9259183300222,-7.35002877099245,
93.0184853375885));
#234726=CARTESIAN_POINT('Ctrl Pts',(-2.92600335660089,-7.34999492282369,
93.0184816727501));
#234727=CARTESIAN_POINT('Ctrl Pts',(-2.92617008948289,-7.34992854490085,
93.0184744861885));
#234728=CARTESIAN_POINT('Ctrl Pts',(-2.92625179421347,-7.34989601590352,
93.018470964533));
#234729=CARTESIAN_POINT('Ctrl Pts',(-2.9264120154653,-7.34983222413143,
93.0184640586447));
#234730=CARTESIAN_POINT('Ctrl Pts',(-2.92649053034446,-7.34980096213115,
93.0184606744825));
#234731=CARTESIAN_POINT('Ctrl Pts',(-2.92664450045386,-7.34973965352225,
93.0184540380389));
#234732=CARTESIAN_POINT('Ctrl Pts',(-2.92671995391438,-7.34970960772961,
93.0184507858338));
#234733=CARTESIAN_POINT('Ctrl Pts',(-2.9268679244604,-7.34965068277773,
93.0184444079907));
#234734=CARTESIAN_POINT('Ctrl Pts',(-2.92694043955458,-7.34962180451414,
93.0184412824384));
#234735=CARTESIAN_POINT('Ctrl Pts',(-2.92708265159954,-7.34956516784023,
93.0184351528047));
#234736=CARTESIAN_POINT('Ctrl Pts',(-2.92715234623792,-7.34953741044554,
93.0184321488227));
#234737=CARTESIAN_POINT('Ctrl Pts',(-2.92728903056338,-7.34948297070887,
93.0184262574505));
#234738=CARTESIAN_POINT('Ctrl Pts',(-2.92735601784517,-7.34945628941226,
93.0184233701637));
#234739=CARTESIAN_POINT('Ctrl Pts',(-2.92748739593124,-7.34940395892512,
93.0184177075061));
#234740=CARTESIAN_POINT('Ctrl Pts',(-2.92755178413494,-7.34937831085107,
93.0184149322473));
#234741=CARTESIAN_POINT('Ctrl Pts',(-2.92767806810214,-7.34932800560629,
93.0184094891609));
#234742=CARTESIAN_POINT('Ctrl Pts',(-2.92773996101404,-7.34930334964586,
93.0184068214562));
#234743=CARTESIAN_POINT('Ctrl Pts',(-2.92786135409999,-7.34925498913091,
93.0184015891805));
#234744=CARTESIAN_POINT('Ctrl Pts',(-2.92792085122977,-7.34923128585779,
93.0183990247407));
#234745=CARTESIAN_POINT('Ctrl Pts',(-2.9280231723058,-7.34919052036077,
93.0183946145088));
#234746=CARTESIAN_POINT('Ctrl Pts',(-2.92806603591217,-7.34917344273937,
93.0183927670066));
#234747=CARTESIAN_POINT('Ctrl Pts',(-2.92815134395272,-7.34913945363636,
93.0183890900708));
#234748=CARTESIAN_POINT('Ctrl Pts',(-2.9281937880129,-7.34912254231274,
93.018387260653));
#234749=CARTESIAN_POINT('Ctrl Pts',(-2.92827827463916,-7.34908887878788,
93.0183836191236));
#234750=CARTESIAN_POINT('Ctrl Pts',(-2.92832031680441,-7.34907212675436,
93.0183818070292));
#234751=CARTESIAN_POINT('Ctrl Pts',(-2.92840400405459,-7.34903878007497,
93.0183781999564));
#234752=CARTESIAN_POINT('Ctrl Pts',(-2.92844564855556,-7.34902218566965,
93.018376405003));
#234753=CARTESIAN_POINT('Ctrl Pts',(-2.92852854487242,-7.34898915251876,
93.0183728320227));
#234754=CARTESIAN_POINT('Ctrl Pts',(-2.92856979595827,-7.3489727140718,
93.0183710540272));
#234755=CARTESIAN_POINT('Ctrl Pts',(-2.92865190960521,-7.34893999120279,
93.0183675147833));
#234756=CARTESIAN_POINT('Ctrl Pts',(-2.92869277154966,-7.34892370703401,
93.0183657535615));
#234757=CARTESIAN_POINT('Ctrl Pts',(-2.92877411094629,-7.34889129113694,
93.0183622476909));
#234758=CARTESIAN_POINT('Ctrl Pts',(-2.92881458788457,-7.34887515962082,
93.0183605030644));
#234759=CARTESIAN_POINT('Ctrl Pts',(-2.9288951615487,-7.34884304734552,
93.0183570302));
#234760=CARTESIAN_POINT('Ctrl Pts',(-2.92893525742463,-7.3488270669323,
93.0183553019988));
#234761=CARTESIAN_POINT('Ctrl Pts',(-2.92901507292009,-7.34879525530777,
93.0183518618147));
#234762=CARTESIAN_POINT('Ctrl Pts',(-2.92905479198797,-7.34877942432342,
93.0183501498554));
#234763=CARTESIAN_POINT('Ctrl Pts',(-2.92913385788524,-7.34874790997645,
93.0183467419819));
#234764=CARTESIAN_POINT('Ctrl Pts',(-2.92917320398037,-7.34873222691344,
93.0183450460993));
#234765=CARTESIAN_POINT('Ctrl Pts',(-2.92925152789791,-7.34870100684924,
93.0183416702081));
#234766=CARTESIAN_POINT('Ctrl Pts',(-2.92929050505235,-7.34868547012113,
93.0183399902283));
#234767=CARTESIAN_POINT('Ctrl Pts',(-2.92936809499878,-7.34865454118845,
93.018336645974));
#234768=CARTESIAN_POINT('Ctrl Pts',(-2.92940670707883,-7.34863914927437,
93.0183349817304));
#234769=CARTESIAN_POINT('Ctrl Pts',(-2.92948357075744,-7.34860850844271,
93.0183316687811));
#234770=CARTESIAN_POINT('Ctrl Pts',(-2.92952182163013,-7.34859325982102,
93.0183300201068));
#234771=CARTESIAN_POINT('Ctrl Pts',(-2.92959796681332,-7.34856290403137,
93.0183267381275));
#234772=CARTESIAN_POINT('Ctrl Pts',(-2.92963586024538,-7.34854779721999,
93.0183251048604));
#234773=CARTESIAN_POINT('Ctrl Pts',(-2.92971129424774,-7.34851772359494,
93.0183218535356));
#234774=CARTESIAN_POINT('Ctrl Pts',(-2.92974883411642,-7.34850275706726,
93.0183202355083));
#234775=CARTESIAN_POINT('Ctrl Pts',(-2.92982356494667,-7.34847296245176,
93.018317014493));
#234776=CARTESIAN_POINT('Ctrl Pts',(-2.92986075477214,-7.34845813482306,
93.0183154115538));
#234777=CARTESIAN_POINT('Ctrl Pts',(-2.92993478907014,-7.34842861660696,
93.0183122205616));
#234778=CARTESIAN_POINT('Ctrl Pts',(-2.929971632813,-7.34841392631652,93.0183106325399));
#234779=CARTESIAN_POINT('Ctrl Pts',(-2.93004497881007,-7.34838468125426,
93.018307471216));
#234780=CARTESIAN_POINT('Ctrl Pts',(-2.93008147979078,-7.34837012699614,
93.0183058979686));
#234781=CARTESIAN_POINT('Ctrl Pts',(-2.93015414359627,-7.34834115268741,
93.0183027660496));
#234782=CARTESIAN_POINT('Ctrl Pts',(-2.93019030581279,-7.34832673288514,
93.0183012074042));
#234783=CARTESIAN_POINT('Ctrl Pts',(-2.93026229579386,-7.34829802602852,
93.0182981045294));
#234784=CARTESIAN_POINT('Ctrl Pts',(-2.9302981223905,-7.34828373944558,
93.0182965603505));
#234785=CARTESIAN_POINT('Ctrl Pts',(-2.93036944483893,-7.3482552975664,
93.0182934862488));
#234786=CARTESIAN_POINT('Ctrl Pts',(-2.93040493950912,-7.34824114274692,
93.018291956377));
#234787=CARTESIAN_POINT('Ctrl Pts',(-2.93047560123915,-7.3482129631614,
93.0182889107545));
#234788=CARTESIAN_POINT('Ctrl Pts',(-2.93051076762822,-7.34819893866832,
93.0182873950328));
#234789=CARTESIAN_POINT('Ctrl Pts',(-2.93058077644006,-7.34817101829869,
93.0182843775534));
#234790=CARTESIAN_POINT('Ctrl Pts',(-2.9306156176142,-7.34815712292548,
93.0182828758496));
#234791=CARTESIAN_POINT('Ctrl Pts',(-2.93068497957464,-7.34812945938451,
93.0182798862517));
#234792=CARTESIAN_POINT('Ctrl Pts',(-2.93071949911866,-7.34811569171746,
93.0182783984113));
#234793=CARTESIAN_POINT('Ctrl Pts',(-2.93078822079913,-7.34808828241595,
93.0182754364117));
#234794=CARTESIAN_POINT('Ctrl Pts',(-2.93082242224484,-7.34807464106212,
93.0182739622823));
#234795=CARTESIAN_POINT('Ctrl Pts',(-2.93089051117575,-7.34804748302762,
93.0182710275563));
#234796=CARTESIAN_POINT('Ctrl Pts',(-2.9309243974905,-7.34803396681884,
93.0182695670102));
#234797=CARTESIAN_POINT('Ctrl Pts',(-2.930991859484,-7.34800705776353,93.0182666593073));
#234798=CARTESIAN_POINT('Ctrl Pts',(-2.9310254341537,-7.34799366532444,
93.0182652121941));
#234799=CARTESIAN_POINT('Ctrl Pts',(-2.93109227624601,-7.34796700247158,
93.018262331211));
#234800=CARTESIAN_POINT('Ctrl Pts',(-2.93112554234659,-7.34795373259001,
93.0182608973981));
#234801=CARTESIAN_POINT('Ctrl Pts',(-2.9311917704262,-7.34792731361997,
93.018258042881));
#234802=CARTESIAN_POINT('Ctrl Pts',(-2.93122473134648,-7.3479141649586,
93.0182566222223));
#234803=CARTESIAN_POINT('Ctrl Pts',(-2.93129035228967,-7.34788798715706,
93.0182537938747));
#234804=CARTESIAN_POINT('Ctrl Pts',(-2.93132301102421,-7.34787495853552,
93.0182523862413));
#234805=CARTESIAN_POINT('Ctrl Pts',(-2.93138803078484,-7.34784901955548,
93.0182495838066));
#234806=CARTESIAN_POINT('Ctrl Pts',(-2.93142039053799,-7.34783610970937,
93.0182481890602));
#234807=CARTESIAN_POINT('Ctrl Pts',(-2.9314848154289,-7.34781040705996,
93.0182454122662));
#234808=CARTESIAN_POINT('Ctrl Pts',(-2.93151687927568,-7.34779761477617,
93.0182440302743));
#234809=CARTESIAN_POINT('Ctrl Pts',(-2.9315807153871,-7.34777214605471,
93.0182412788586));
#234810=CARTESIAN_POINT('Ctrl Pts',(-2.93161248639493,-7.34775947012286,
93.0182399094889));
#234811=CARTESIAN_POINT('Ctrl Pts',(-2.93167574011761,-7.34773423280616,
93.018237183176));
#234812=CARTESIAN_POINT('Ctrl Pts',(-2.93170722114656,-7.34772167209827,
93.0182358263053));
#234813=CARTESIAN_POINT('Ctrl Pts',(-2.93176989766444,-7.34769666414404,
93.0182331248716));
#234814=CARTESIAN_POINT('Ctrl Pts',(-2.93180109202279,-7.34768421735301,
93.0182317803573));
#234815=CARTESIAN_POINT('Ctrl Pts',(-2.93186319813986,-7.34765943607196,
93.0182291035097));
#234816=CARTESIAN_POINT('Ctrl Pts',(-2.93189410849655,-7.34764710214551,
93.0182277712367));
#234817=CARTESIAN_POINT('Ctrl Pts',(-2.93195564958619,-7.3476225454186,
93.0182251187434));
#234818=CARTESIAN_POINT('Ctrl Pts',(-2.93198627895568,-7.34761032316627,
93.0182237985818));
#234819=CARTESIAN_POINT('Ctrl Pts',(-2.93204726107688,-7.34758598860034,
93.0182211701817));
#234820=CARTESIAN_POINT('Ctrl Pts',(-2.93207761225227,-7.34757387691973,
93.0182198620111));
#234821=CARTESIAN_POINT('Ctrl Pts',(-2.94508423646356,-7.34238347122519,
93.01765926164));
#234822=CARTESIAN_POINT('Ctrl Pts',(-2.95804679217719,-7.33717080182073,
93.01710060554));
#234823=CARTESIAN_POINT('Ctrl Pts',(-2.99278063307489,-7.32309617591512,
93.0156037252995));
#234824=CARTESIAN_POINT('Ctrl Pts',(-3.01452638219254,-7.31417146483269,
93.0146666483168));
#234825=CARTESIAN_POINT('Ctrl Pts',(-3.11057424210187,-7.27425118977034,
93.0105275947787));
#234826=CARTESIAN_POINT('Ctrl Pts',(-3.18444140432334,-7.24221897759433,
93.007343811271));
#234827=CARTESIAN_POINT('Ctrl Pts',(-3.76730389164086,-6.97882090731071,
92.9822086001764));
#234828=CARTESIAN_POINT('Ctrl Pts',(-4.2509630499662,-6.69521294122317,
92.9614140314136));
#234829=CARTESIAN_POINT('Ctrl Pts',(-4.96390796320805,-6.16851943345574,
92.9288120420773));
#234830=CARTESIAN_POINT('Ctrl Pts',(-5.21479734809276,-5.95792697041818,
92.9168513746901));
#234831=CARTESIAN_POINT('Ctrl Pts',(-5.55549784949814,-5.63389724494306,
92.8991416086831));
#234832=CARTESIAN_POINT('Ctrl Pts',(-5.65638669784677,-5.53259812691413,
92.8936890529697));
#234833=CARTESIAN_POINT('Ctrl Pts',(-5.81709500917299,-5.36224342708556,
92.8845699390677));
#234834=CARTESIAN_POINT('Ctrl Pts',(-5.87856229826783,-5.29478549852349,
92.880971040315));
#234835=CARTESIAN_POINT('Ctrl Pts',(-5.94872114677814,-5.21506098677468,
92.8767153443157));
#234836=CARTESIAN_POINT('Ctrl Pts',(-5.95856302462046,-5.20381312652112,
92.8761148784572));
#234837=CARTESIAN_POINT('Ctrl Pts',(-5.97331343209403,-5.18685880837321,
92.8752095975896));
#234838=CARTESIAN_POINT('Ctrl Pts',(-5.97824581915656,-5.18117308929882,
92.8749059772487));
#234839=CARTESIAN_POINT('Ctrl Pts',(-5.98701232997471,-5.17103846959063,
92.8743647162705));
#234840=CARTESIAN_POINT('Ctrl Pts',(-5.9908496323154,-5.16659231757277,
92.8741272371414));
#234841=CARTESIAN_POINT('Ctrl Pts',(-5.99891256148631,-5.15722901508154,
92.8736270656217));
#234842=CARTESIAN_POINT('Ctrl Pts',(-6.00313710043055,-5.15231093660539,
92.8733643178286));
#234843=CARTESIAN_POINT('Ctrl Pts',(-6.0142413949916,-5.13935146083918,
92.8726718602992));
#234844=CARTESIAN_POINT('Ctrl Pts',(-6.0211110547341,-5.13130145872978,
92.8722416282666));
#234845=CARTESIAN_POINT('Ctrl Pts',(-6.05173131863672,-5.09527387727819,
92.8703155891476));
#234846=CARTESIAN_POINT('Ctrl Pts',(-6.07530296155246,-5.06714532043659,
92.8688103649413));
#234847=CARTESIAN_POINT('Ctrl Pts',(-6.23932736486503,-4.86862161718658,
92.8581700690522));
#234848=CARTESIAN_POINT('Ctrl Pts',(-6.37276443058871,-4.69260352104712,
92.8486005879175));
#234849=CARTESIAN_POINT('Ctrl Pts',(-6.63473670391265,-4.31522186172175,
92.8281266604278));
#234850=CARTESIAN_POINT('Ctrl Pts',(-6.76187851940734,-4.11313299884776,
92.8172018949812));
#234851=CARTESIAN_POINT('Ctrl Pts',(-6.93258929471882,-3.81242820574652,
92.8012972668138));
#234852=CARTESIAN_POINT('Ctrl Pts',(-6.98359222133139,-3.71817735566706,
92.7963592173527));
#234853=CARTESIAN_POINT('Ctrl Pts',(-7.05855329049864,-3.57266596325531,
92.7888296792713));
#234854=CARTESIAN_POINT('Ctrl Pts',(-7.08390243797734,-3.52213613161424,
92.7862319367448));
#234855=CARTESIAN_POINT('Ctrl Pts',(-7.13736990450129,-3.41264390853482,
92.7806434982027));
#234856=CARTESIAN_POINT('Ctrl Pts',(-7.16530403736545,-3.35359594421681,
92.777654715863));
#234857=CARTESIAN_POINT('Ctrl Pts',(-7.40717742334856,-2.82549479661754,
92.751169486616));
#234858=CARTESIAN_POINT('Ctrl Pts',(-7.57554356132076,-2.33687131199937,
92.7284906711403));
#234859=CARTESIAN_POINT('Ctrl Pts',(-7.7030955993067,-1.80205595855616,
92.7061131792509));
#234860=CARTESIAN_POINT('Ctrl Pts',(-7.71080382685018,-1.76878259633902,
92.7047302386655));
#234861=CARTESIAN_POINT('Ctrl Pts',(-7.72089515083701,-1.72390237647433,
92.7028772502103));
#234862=CARTESIAN_POINT('Ctrl Pts',(-7.72346794420973,-1.71233882460143,
92.702400923816));
#234863=CARTESIAN_POINT('Ctrl Pts',(-7.72746610123569,-1.69417656325994,
92.7016545075691));
#234864=CARTESIAN_POINT('Ctrl Pts',(-7.7289090035783,-1.68758175741215,
92.7013838367324));
#234865=CARTESIAN_POINT('Ctrl Pts',(-7.73166375920978,-1.67491346715052,
92.7008645747515));
#234866=CARTESIAN_POINT('Ctrl Pts',(-7.73297690164791,-1.66884026998875,
92.7006159410307));
#234867=CARTESIAN_POINT('Ctrl Pts',(-7.73604615324661,-1.65456377712249,
92.7000321747194));
#234868=CARTESIAN_POINT('Ctrl Pts',(-7.73779637321535,-1.64635921504607,
92.6996972375978));
#234869=CARTESIAN_POINT('Ctrl Pts',(-7.74137901547739,-1.62943283568601,
92.6990073731598));
#234870=CARTESIAN_POINT('Ctrl Pts',(-7.74320975716889,-1.62071067265692,
92.6986525019206));
#234871=CARTESIAN_POINT('Ctrl Pts',(-7.74788943436624,-1.59822646151356,
92.6977392871197));
#234872=CARTESIAN_POINT('Ctrl Pts',(-7.75071644955372,-1.58445985457751,
92.6971816703276));
#234873=CARTESIAN_POINT('Ctrl Pts',(-7.77421687419262,-1.46845275206103,
92.6924955646544));
#234874=CARTESIAN_POINT('Ctrl Pts',(-7.79290344259698,-1.36581788638988,
92.6884332824482));
#234875=CARTESIAN_POINT('Ctrl Pts',(-7.87742479802568,-0.843127933224769,
92.66814279541));
#234876=CARTESIAN_POINT('Ctrl Pts',(-7.91135110646884,-0.418615950099376,
92.6530110698391));
#234877=CARTESIAN_POINT('Ctrl Pts',(-7.91099726067231,0.00658343642006579,
92.6384370102158));
#234878=CARTESIAN_POINT('',(-7.91923391390641,-9.72790312405945E-5,90.6423314461212));
#234879=CARTESIAN_POINT('Ctrl Pts',(-7.91099714745356,0.0067181084832415,
92.642331465206));
#234880=CARTESIAN_POINT('Ctrl Pts',(-7.91079160367377,0.248758894166455,
92.6326073364901));
#234881=CARTESIAN_POINT('Ctrl Pts',(-7.89947448308587,0.490284791307527,
92.6228832077741));
#234882=CARTESIAN_POINT('Ctrl Pts',(-7.87720914932586,0.730408801820563,
92.6131590790582));
#234883=CARTESIAN_POINT('Ctrl Pts',(-7.85470833965837,0.973072339469931,
92.603332108945));
#234884=CARTESIAN_POINT('Ctrl Pts',(-7.82102660107798,1.21430427540786,
92.5935051388318));
#234885=CARTESIAN_POINT('Ctrl Pts',(-7.77638033720727,1.45321362885717,
92.5836781687186));
#234886=CARTESIAN_POINT('Ctrl Pts',(-7.73122410802533,1.69485188887608,
92.5737389515004));
#234887=CARTESIAN_POINT('Ctrl Pts',(-7.67485145389126,1.93411430807153,
92.5637997342821));
#234888=CARTESIAN_POINT('Ctrl Pts',(-7.60753419602398,2.17010240687525,
92.5538605170639));
#234889=CARTESIAN_POINT('Ctrl Pts',(-7.5741006142655,2.28730752849412,92.5489241360821));
#234890=CARTESIAN_POINT('Ctrl Pts',(-7.53796808386738,2.40370532976846,
92.5439877551003));
#234891=CARTESIAN_POINT('Ctrl Pts',(-7.49917423568835,2.51918772281624,
92.5390513741185));
#234892=CARTESIAN_POINT('Ctrl Pts',(-7.43818801125248,2.70073287678758,
92.5312910911719));
#234893=CARTESIAN_POINT('Ctrl Pts',(-7.37049778424932,2.88038206616635,
92.5235308082253));
#234894=CARTESIAN_POINT('Ctrl Pts',(-7.29623629942042,3.0575900416864,92.5157705252788));
#234895=CARTESIAN_POINT('Ctrl Pts',(-7.22206419200328,3.23458473854346,
92.5080195822209));
#234896=CARTESIAN_POINT('Ctrl Pts',(-7.14133670557192,3.4091437429375,92.500268639163));
#234897=CARTESIAN_POINT('Ctrl Pts',(-7.05423680001995,3.58073514368827,
92.4925176961052));
#234898=CARTESIAN_POINT('Ctrl Pts',(-6.96722404488927,3.75215485351964,
92.4847745084857));
#234899=CARTESIAN_POINT('Ctrl Pts',(-6.87385172440213,3.92061255348817,
92.4770313208662));
#234900=CARTESIAN_POINT('Ctrl Pts',(-6.77435153654204,4.08559448053162,
92.4692881332468));
#234901=CARTESIAN_POINT('Ctrl Pts',(-6.67493074056457,4.25044476736347,
92.4615511239699));
#234902=CARTESIAN_POINT('Ctrl Pts',(-6.56939199619968,4.41182449723104,
92.4538141146929));
#234903=CARTESIAN_POINT('Ctrl Pts',(-6.45801379380717,4.56924269863139,
92.446077105416));
#234904=CARTESIAN_POINT('Ctrl Pts',(-6.34670191090367,4.72656716629882,
92.4383447030953));
#234905=CARTESIAN_POINT('Ctrl Pts',(-6.22955770038984,4.87993451051667,
92.4306123007746));
#234906=CARTESIAN_POINT('Ctrl Pts',(-6.10690404949791,5.02888098191098,
92.4228798984539));
#234907=CARTESIAN_POINT('Ctrl Pts',(-5.98429861673466,5.1777688988304,92.4151505359283));
#234908=CARTESIAN_POINT('Ctrl Pts',(-5.8561882852263,5.32223912764058,92.4074211734027));
#234909=CARTESIAN_POINT('Ctrl Pts',(-5.72293751723684,5.46185931472087,
92.3996918108771));
#234910=CARTESIAN_POINT('Ctrl Pts',(-5.58968680123665,5.60147944732678,
92.3919624513673));
#234911=CARTESIAN_POINT('Ctrl Pts',(-5.45129589232242,5.73624927436528,
92.3842330918574));
#234912=CARTESIAN_POINT('Ctrl Pts',(-5.30816784116512,5.86577148975482,
92.3765037323475));
#234913=CARTESIAN_POINT('Ctrl Pts',(-5.16503261591601,5.99530019726283,
92.3687739854144));
#234914=CARTESIAN_POINT('Ctrl Pts',(-5.0171600413678,6.11958052746997,92.3610442384812));
#234915=CARTESIAN_POINT('Ctrl Pts',(-4.86498801307516,6.23825397307893,
92.353314491548));
#234916=CARTESIAN_POINT('Ctrl Pts',(-4.71278047387849,6.35695511235396,
92.3455829407992));
#234917=CARTESIAN_POINT('Ctrl Pts',(-4.55627176615189,6.47004654044728,
92.3378513900503));
#234918=CARTESIAN_POINT('Ctrl Pts',(-4.39593068929494,6.57721174776325,
92.3301198393014));
#234919=CARTESIAN_POINT('Ctrl Pts',(-4.23552280536625,6.68442160610585,
92.3223850671555));
#234920=CARTESIAN_POINT('Ctrl Pts',(-4.07127967099671,6.78570012743835,
92.3146502950096));
#234921=CARTESIAN_POINT('Ctrl Pts',(-3.90369674888765,6.88077558802233,
92.3069155228637));
#234922=CARTESIAN_POINT('Ctrl Pts',(-3.73591398405815,6.97596442614174,
92.2991715269981));
#234923=CARTESIAN_POINT('Ctrl Pts',(-3.56478378998337,7.06493525327135,
92.2914275311324));
#234924=CARTESIAN_POINT('Ctrl Pts',(-3.39082472169122,7.14746309586609,
92.2836835352668));
#234925=CARTESIAN_POINT('Ctrl Pts',(-3.216752745237,7.23004450317073,92.2759345131593));
#234926=CARTESIAN_POINT('Ctrl Pts',(-3.0398485657435,7.3061744546806,92.2681854910519));
#234927=CARTESIAN_POINT('Ctrl Pts',(-2.86064801984975,7.37567718291207,
92.2604364689444));
#234928=CARTESIAN_POINT('Ctrl Pts',(-2.68117361330881,7.44528612768456,
92.2526756045058));
#234929=CARTESIAN_POINT('Ctrl Pts',(-2.49939616920984,7.50824750455819,
92.2449147400672));
#234930=CARTESIAN_POINT('Ctrl Pts',(-2.3158650600953,7.56443586947697,92.2371538756286));
#234931=CARTESIAN_POINT('Ctrl Pts',(-2.18965234228518,7.60307611025098,
92.2318167979088));
#234932=CARTESIAN_POINT('Ctrl Pts',(-2.06261051400034,7.63851433241825,
92.2264797201889));
#234933=CARTESIAN_POINT('Ctrl Pts',(-1.93491995010981,7.67072394149777,
92.2211426424691));
#234934=CARTESIAN_POINT('Ctrl Pts',(-1.74318830671347,7.719087744537,92.213128842146));
#234935=CARTESIAN_POINT('Ctrl Pts',(-1.54940556761321,7.7603185217876,92.2051150418229));
#234936=CARTESIAN_POINT('Ctrl Pts',(-1.3541383791836,7.79424340459175,92.1971012414999));
#234937=CARTESIAN_POINT('Ctrl Pts',(-1.15909377229931,7.82812961703403,
92.1890965759632));
#234938=CARTESIAN_POINT('Ctrl Pts',(-0.962568414586113,7.85472647235197,
92.1810919104265));
#234939=CARTESIAN_POINT('Ctrl Pts',(-0.765142846728391,7.87391118975191,
92.1730872448899));
#234940=CARTESIAN_POINT('Ctrl Pts',(-0.567908804462299,7.89307729576129,
92.1650903448028));
#234941=CARTESIAN_POINT('Ctrl Pts',(-0.369776623316966,7.90484556132773,
92.1570934447159));
#234942=CARTESIAN_POINT('Ctrl Pts',(-0.171336154412708,7.90914438622732,
92.1490965446288));
#234943=CARTESIAN_POINT('Ctrl Pts',(0.0269454712136357,7.91343977009775,
92.1411060457251));
#234944=CARTESIAN_POINT('Ctrl Pts',(0.225534559741134,7.91027762249422,
92.1331155468214));
#234945=CARTESIAN_POINT('Ctrl Pts',(0.423836614784747,7.89963818943424,
92.1251250479177));
#234946=CARTESIAN_POINT('Ctrl Pts',(0.622013562858758,7.88900546869616,
92.1171395901474));
#234947=CARTESIAN_POINT('Ctrl Pts',(0.81990350528098,7.87090488351985,92.109154132377));
#234948=CARTESIAN_POINT('Ctrl Pts',(1.0169120070025,7.84536875933911,92.1011686746067));
#234949=CARTESIAN_POINT('Ctrl Pts',(1.22037994612897,7.81899536674473,92.0929213927822));
#234950=CARTESIAN_POINT('Ctrl Pts',(1.42290729803654,7.78469056794254,92.0846741109578));
#234951=CARTESIAN_POINT('Ctrl Pts',(1.62384370156454,7.74254820023028,92.0764268291333));
#234952=CARTESIAN_POINT('Ctrl Pts',(1.81826927566203,7.70177134799036,92.0684467793498));
#234953=CARTESIAN_POINT('Ctrl Pts',(2.01120503667431,7.65365695866286,92.0604667295663));
#234954=CARTESIAN_POINT('Ctrl Pts',(2.2020710068714,7.59834220607998,92.0524866797829));
#234955=CARTESIAN_POINT('Ctrl Pts',(2.39292181993292,7.54303184617749,92.0445072637148));
#234956=CARTESIAN_POINT('Ctrl Pts',(2.58170284843214,7.48052235570758,92.0365278476466));
#234957=CARTESIAN_POINT('Ctrl Pts',(2.76784823604333,7.41100108907237,92.0285484315785));
#234958=CARTESIAN_POINT('Ctrl Pts',(2.95400744904045,7.34147465895525,92.0205684228634));
#234959=CARTESIAN_POINT('Ctrl Pts',(3.13753031764566,7.26493553203591,92.0125884141483));
#234960=CARTESIAN_POINT('Ctrl Pts',(3.31786960790439,7.18161975218295,92.0046084054332));
#234961=CARTESIAN_POINT('Ctrl Pts',(3.49825000805026,7.09828497978377,91.9966265776067));
#234962=CARTESIAN_POINT('Ctrl Pts',(3.67544507989323,7.00817061607556,91.9886447497801));
#234963=CARTESIAN_POINT('Ctrl Pts',(3.8489305540484,6.91155949045602,91.9806629219536));
#234964=CARTESIAN_POINT('Ctrl Pts',(4.022545022454,6.81487653012067,91.9726751592792));
#234965=CARTESIAN_POINT('Ctrl Pts',(4.19244409089721,6.71168732123721,91.9646873966048));
#234966=CARTESIAN_POINT('Ctrl Pts',(4.35813006549708,6.60231954181335,91.9566996339304));
#234967=CARTESIAN_POINT('Ctrl Pts',(4.52388901409126,6.49290359293077,91.9487083531614));
#234968=CARTESIAN_POINT('Ctrl Pts',(4.68543089476072,6.37730383867855,91.9407170723923));
#234969=CARTESIAN_POINT('Ctrl Pts',(4.84228921294199,6.25588971915471,91.9327257916232));
#234970=CARTESIAN_POINT('Ctrl Pts',(4.99929511394555,6.13436136508704,91.9247269921214));
#234971=CARTESIAN_POINT('Ctrl Pts',(5.15160839303579,6.00700793154305,91.9167281926196));
#234972=CARTESIAN_POINT('Ctrl Pts',(5.29879693936175,5.87423799274515,91.9087293931178));
#234973=CARTESIAN_POINT('Ctrl Pts',(5.33250499978858,5.84383197793232,91.906897565685));
#234974=CARTESIAN_POINT('Ctrl Pts',(5.36594444023649,5.8131420336051,91.9050657382523));
#234975=CARTESIAN_POINT('Ctrl Pts',(5.39911035365196,5.7821733274858,91.9032339108195));
#234976=CARTESIAN_POINT('Ctrl Pts',(5.54624641353908,5.64478487865534,91.8951072577865));
#234977=CARTESIAN_POINT('Ctrl Pts',(5.68825553927663,5.50166497693222,91.8869806047535));
#234978=CARTESIAN_POINT('Ctrl Pts',(5.82468286059035,5.35322244760527,91.8788539517205));
#234979=CARTESIAN_POINT('Ctrl Pts',(5.96099404885058,5.20490627921566,91.870734216459));
#234980=CARTESIAN_POINT('Ctrl Pts',(6.09173269064198,5.05127674977003,91.8626144811975));
#234981=CARTESIAN_POINT('Ctrl Pts',(6.21647985837717,4.89278031086529,91.8544947459359));
#234982=CARTESIAN_POINT('Ctrl Pts',(6.34113654498359,4.73439883197893,91.8463809000491));
#234983=CARTESIAN_POINT('Ctrl Pts',(6.45981022575428,4.57115773181444,91.8382670541622));
#234984=CARTESIAN_POINT('Ctrl Pts',(6.5721210880426,4.40353782816791,91.8301532082754));
#234985=CARTESIAN_POINT('Ctrl Pts',(6.68435214928241,4.2360370247027,91.8220451275781));
#234986=CARTESIAN_POINT('Ctrl Pts',(6.79022923455868,4.06416388914116,91.8139370468808));
#234987=CARTESIAN_POINT('Ctrl Pts',(6.88941462589896,3.88842990324494,91.8058289661835));
#234988=CARTESIAN_POINT('Ctrl Pts',(6.9885574166138,3.71277139598132,91.7977243679477));
#234989=CARTESIAN_POINT('Ctrl Pts',(7.08101408766959,3.533255621941,91.7896197697119));
#234990=CARTESIAN_POINT('Ctrl Pts',(7.16649139146795,3.35042118785323,91.7815151714761));
#234991=CARTESIAN_POINT('Ctrl Pts',(7.2519419775556,3.16764390247395,91.7734131065012));
#234992=CARTESIAN_POINT('Ctrl Pts',(7.33041741232535,2.98155031436175,91.7653110415264));
#234993=CARTESIAN_POINT('Ctrl Pts',(7.40167113613748,2.79270216680357,91.7572089765515));
#234994=CARTESIAN_POINT('Ctrl Pts',(7.43957382506254,2.69224632803443,91.7528991660326));
#234995=CARTESIAN_POINT('Ctrl Pts',(7.47543385802744,2.59101143369428,91.7485893555137));
#234996=CARTESIAN_POINT('Ctrl Pts',(7.50921967833794,2.48908433414023,91.7442795449949));
#234997=CARTESIAN_POINT('Ctrl Pts',(7.57419722825957,2.29305614424353,91.7359908331753));
#234998=CARTESIAN_POINT('Ctrl Pts',(7.63147188357436,2.09455103469157,91.7277021213557));
#234999=CARTESIAN_POINT('Ctrl Pts',(7.68088318079123,1.89418968507339,91.7194134095361));
#235000=CARTESIAN_POINT('Ctrl Pts',(7.73032296313793,1.69371282909579,91.7111199193552));
#235001=CARTESIAN_POINT('Ctrl Pts',(7.77189026893824,1.4913778811092,91.7028264291743));
#235002=CARTESIAN_POINT('Ctrl Pts',(7.80547566980551,1.28781620120039,91.6945329389933));
#235003=CARTESIAN_POINT('Ctrl Pts',(7.83908245720586,1.08412489715467,91.6862341676784));
#235004=CARTESIAN_POINT('Ctrl Pts',(7.86469714640173,0.879205590369583,
91.6779353963635));
#235005=CARTESIAN_POINT('Ctrl Pts',(7.8822620206768,0.673696101663093,91.6696366250486));
#235006=CARTESIAN_POINT('Ctrl Pts',(7.8998473414792,0.467947388051725,91.6613281934849));
#235007=CARTESIAN_POINT('Ctrl Pts',(7.90936409203439,0.261607411075234,
91.6530197619213));
#235008=CARTESIAN_POINT('Ctrl Pts',(7.91080659728757,0.0553170887840625,
91.6447113303576));
#235009=CARTESIAN_POINT('Ctrl Pts',(7.91224999237583,-0.15110048737013,
91.6363977735898));
#235010=CARTESIAN_POINT('Ctrl Pts',(7.90560920453027,-0.35746805535786,
91.6280842168221));
#235011=CARTESIAN_POINT('Ctrl Pts',(7.8909306428383,-0.563147041114041,
91.6197706600543));
#235012=CARTESIAN_POINT('Ctrl Pts',(7.87623603319375,-0.769050894039098,
91.6114480141422));
#235013=CARTESIAN_POINT('Ctrl Pts',(7.85348611317857,-0.974264368778665,
91.6031253682302));
#235014=CARTESIAN_POINT('Ctrl Pts',(7.82277907762377,-1.17815470235951,
91.5948027223181));
#235015=CARTESIAN_POINT('Ctrl Pts',(7.81112303868708,-1.25554913735121,
91.5916435412688));
#235016=CARTESIAN_POINT('Ctrl Pts',(7.79832100536156,-1.33275302809533,
91.5884843602194));
#235017=CARTESIAN_POINT('Ctrl Pts',(7.78438026655081,-1.40973219645945,
91.58532517917));
#235018=CARTESIAN_POINT('Ctrl Pts',(7.74599703014416,-1.6216800464133,91.5766269606096));
#235019=CARTESIAN_POINT('Ctrl Pts',(7.69894391847647,-1.83211167553014,
91.5679287420491));
#235020=CARTESIAN_POINT('Ctrl Pts',(7.64335825120228,-2.04034204087895,
91.5592305234887));
#235021=CARTESIAN_POINT('Ctrl Pts',(7.58782142338809,-2.24838944793834,
91.5505399474793));
#235022=CARTESIAN_POINT('Ctrl Pts',(7.52376706861353,-2.45423923232996,
91.54184937147));
#235023=CARTESIAN_POINT('Ctrl Pts',(7.45138307374014,-2.65721871293632,
91.5331587954606));
#235024=CARTESIAN_POINT('Ctrl Pts',(7.37726312337087,-2.86506616671167,
91.5242597969509));
#235025=CARTESIAN_POINT('Ctrl Pts',(7.29440904556744,-3.06990368582867,
91.5153607984413));
#235026=CARTESIAN_POINT('Ctrl Pts',(7.20307723345002,-3.27102420794376,
91.5064617999317));
#235027=CARTESIAN_POINT('Ctrl Pts',(7.11414729877863,-3.46685558890633,
91.4977968305442));
#235028=CARTESIAN_POINT('Ctrl Pts',(7.01717995027879,-3.6591627506936,91.4891318611568));
#235029=CARTESIAN_POINT('Ctrl Pts',(6.91246148452419,-3.84731038843626,
91.4804668917693));
#235030=CARTESIAN_POINT('Ctrl Pts',(6.80350056224454,-4.04308044661513,
91.4714508786986));
#235031=CARTESIAN_POINT('Ctrl Pts',(6.68614748120441,-4.23434671547093,
91.4624348656279));
#235032=CARTESIAN_POINT('Ctrl Pts',(6.5607799042522,-4.42041718030781,91.4534188525572));
#235033=CARTESIAN_POINT('Ctrl Pts',(6.43541232730008,-4.60648764514457,
91.4444028394866));
#235034=CARTESIAN_POINT('Ctrl Pts',(6.30203035495867,-4.78736203649927,
91.4353868264159));
#235035=CARTESIAN_POINT('Ctrl Pts',(6.16106651317211,-4.96237648917021,
91.4263708133453));
#235036=CARTESIAN_POINT('Ctrl Pts',(6.03895158395946,-5.11398896814523,
91.4185603721431));
#235037=CARTESIAN_POINT('Ctrl Pts',(5.91119909586136,-5.26113814216653,
91.410749930941));
#235038=CARTESIAN_POINT('Ctrl Pts',(5.77817932597718,-5.40338455755741,
91.4029394897388));
#235039=CARTESIAN_POINT('Ctrl Pts',(5.64516914655071,-5.54562071726802,
91.3951296116537));
#235040=CARTESIAN_POINT('Ctrl Pts',(5.50689268232727,-5.68295456522088,
91.3873197335687));
#235041=CARTESIAN_POINT('Ctrl Pts',(5.36375856562433,-5.81498194749491,
91.3795098554836));
#235042=CARTESIAN_POINT('Ctrl Pts',(5.22060950466014,-5.9470231144049,91.3716991619894));
#235043=CARTESIAN_POINT('Ctrl Pts',(5.07260204044028,-6.0737564739082,91.3638884684953));
#235044=CARTESIAN_POINT('Ctrl Pts',(4.92017961795182,-6.19481666614045,
91.3560777750011));
#235045=CARTESIAN_POINT('Ctrl Pts',(4.76764902803233,-6.31596276942031,
91.3482615386043));
#235046=CARTESIAN_POINT('Ctrl Pts',(4.61069749646039,-6.43142744275326,
91.3404453022075));
#235047=CARTESIAN_POINT('Ctrl Pts',(4.4498000294716,-6.5408868433657,91.3326290658107));
#235048=CARTESIAN_POINT('Ctrl Pts',(4.28884307636006,-6.65038671270313,
91.3248099396382));
#235049=CARTESIAN_POINT('Ctrl Pts',(4.12393757723136,-6.75387669527379,
91.3169908134656));
#235050=CARTESIAN_POINT('Ctrl Pts',(3.95558523923625,-6.85107775573569,
91.3091716872931));
#235051=CARTESIAN_POINT('Ctrl Pts',(3.78704569837821,-6.94838690092639,
91.3013438664815));
#235052=CARTESIAN_POINT('Ctrl Pts',(3.61505197141565,-7.03939298604097,
91.2935160456699));
#235053=CARTESIAN_POINT('Ctrl Pts',(3.4401289372587,-7.12386369149743,91.2856882248584));
#235054=CARTESIAN_POINT('Ctrl Pts',(3.30402657414807,-7.18958781228949,
91.2795976324124));
#235055=CARTESIAN_POINT('Ctrl Pts',(3.16615130851551,-7.25135639975824,
91.2735070399665));
#235056=CARTESIAN_POINT('Ctrl Pts',(3.02675743534559,-7.30908068279317,
91.2674164475206));
#235057=CARTESIAN_POINT('Ctrl Pts',(2.84098615749911,-7.38601027502208,
91.2592994685186));
#235058=CARTESIAN_POINT('Ctrl Pts',(2.65214791877309,-7.45590820058209,
91.2511824895166));
#235059=CARTESIAN_POINT('Ctrl Pts',(2.46080376501156,-7.51853481937172,
91.2430655105146));
#235060=CARTESIAN_POINT('Ctrl Pts',(2.26959957285665,-7.58111562896357,
91.234954468801));
#235061=CARTESIAN_POINT('Ctrl Pts',(2.07589342409468,-7.63643563719126,
91.2268434270874));
#235062=CARTESIAN_POINT('Ctrl Pts',(1.88026521682142,-7.68430372346197,
91.2187323853738));
#235063=CARTESIAN_POINT('Ctrl Pts',(1.68475228992261,-7.73214360188379,
91.210626123359));
#235064=CARTESIAN_POINT('Ctrl Pts',(1.48731987376807,-7.77254023878968,
91.2025198613443));
#235065=CARTESIAN_POINT('Ctrl Pts',(1.28856242101603,-7.80535251523884,
91.1944135993296));
#235066=CARTESIAN_POINT('Ctrl Pts',(1.08989386305475,-7.83815011631151,
91.1863109628618));
#235067=CARTESIAN_POINT('Ctrl Pts',(0.889901766226695,-7.8633700695686,
91.178208326394));
#235068=CARTESIAN_POINT('Ctrl Pts',(0.689190725560644,-7.88092235362088,
91.1701056899262));
#235069=CARTESIAN_POINT('Ctrl Pts',(0.488540969893319,-7.89846927826839,
91.1620055275129));
#235070=CARTESIAN_POINT('Ctrl Pts',(0.287173027364239,-7.90835317547818,
91.1539053650996));
#235071=CARTESIAN_POINT('Ctrl Pts',(0.0856971434646774,-7.91053582253453,
91.1458052026864));
#235072=CARTESIAN_POINT('Ctrl Pts',(-0.117741213928936,-7.91273972963904,
91.1376261407357));
#235073=CARTESIAN_POINT('Ctrl Pts',(-0.321289296473831,-7.90709153012045,
91.1294470787851));
#235074=CARTESIAN_POINT('Ctrl Pts',(-0.524317403790099,-7.89360578316924,
91.1212680168345));
#235075=CARTESIAN_POINT('Ctrl Pts',(-0.725385892030624,-7.88025020010186,
91.1131678988588));
#235076=CARTESIAN_POINT('Ctrl Pts',(-0.925944074935925,-7.85920774109845,
91.1050677808831));
#235077=CARTESIAN_POINT('Ctrl Pts',(-1.12538375364369,-7.83054483462261,
91.0969676629074));
#235078=CARTESIAN_POINT('Ctrl Pts',(-1.32485027342461,-7.80187807062366,
91.0888664547983));
#235079=CARTESIAN_POINT('Ctrl Pts',(-1.52319767124596,-7.76558885942882,
91.0807652466892));
#235080=CARTESIAN_POINT('Ctrl Pts',(-1.71982572413473,-7.7217951590679,
91.0726640385801));
#235081=CARTESIAN_POINT('Ctrl Pts',(-1.91650563407373,-7.67798990892003,
91.0645606939256));
#235082=CARTESIAN_POINT('Ctrl Pts',(-2.11146498173309,-7.62667629233913,
91.0564573492712));
#235083=CARTESIAN_POINT('Ctrl Pts',(-2.30411600173069,-7.56802288914143,
91.0483540046167));
#235084=CARTESIAN_POINT('Ctrl Pts',(-2.49994911305512,-7.50840068502274,
91.0401168138879));
#235085=CARTESIAN_POINT('Ctrl Pts',(-2.69339664437544,-7.44119420382474,
91.0318796231591));
#235086=CARTESIAN_POINT('Ctrl Pts',(-2.88385978677335,-7.36663245521531,
91.0236424324303));
#235087=CARTESIAN_POINT('Ctrl Pts',(-3.0714720878476,-7.29318674255606,
91.0155285354969));
#235088=CARTESIAN_POINT('Ctrl Pts',(-3.25618843353923,-7.21260456913757,
91.0074146385636));
#235089=CARTESIAN_POINT('Ctrl Pts',(-3.43745874062739,-7.12515251812088,
90.9993007416302));
#235090=CARTESIAN_POINT('Ctrl Pts',(-3.62286075613152,-7.03570716560334,
90.9910019040037));
#235091=CARTESIAN_POINT('Ctrl Pts',(-3.8046574518437,-6.93907520016753,
90.9827030663772));
#235092=CARTESIAN_POINT('Ctrl Pts',(-3.98228874073508,-6.83559049281148,
90.9744042287506));
#235093=CARTESIAN_POINT('Ctrl Pts',(-4.15992002962658,-6.73210578545535,
90.9661053911241));
#235094=CARTESIAN_POINT('Ctrl Pts',(-4.33338563008723,-6.62176855699551,
90.9578065534975));
#235095=CARTESIAN_POINT('Ctrl Pts',(-4.50215861176599,-6.50495878807094,
90.949507715871));
#235096=CARTESIAN_POINT('Ctrl Pts',(-4.66330827066495,-6.39342521065219,
90.9415837292265));
#235097=CARTESIAN_POINT('Ctrl Pts',(-4.82052558239728,-6.27575117870101,
90.933659742582));
#235098=CARTESIAN_POINT('Ctrl Pts',(-4.97331335357888,-6.15224148478536,
90.9257357559375));
#235099=CARTESIAN_POINT('Ctrl Pts',(-5.1259375334243,-6.02886403388696,
90.9178202535818));
#235100=CARTESIAN_POINT('Ctrl Pts',(-5.27414135532592,-5.89966357935469,
90.909904751226));
#235101=CARTESIAN_POINT('Ctrl Pts',(-5.41745581421224,-5.76498859505012,
90.9019892488702));
#235102=CARTESIAN_POINT('Ctrl Pts',(-5.56064046996523,-5.63043558891217,
90.8940809157632));
#235103=CARTESIAN_POINT('Ctrl Pts',(-5.69894433647337,-5.49041816343139,
90.8861725826561));
#235104=CARTESIAN_POINT('Ctrl Pts',(-5.83193056651693,-5.34532570264203,
90.8782642495491));
#235105=CARTESIAN_POINT('Ctrl Pts',(-5.96479952625543,-5.20036118770943,
90.8703628901915));
#235106=CARTESIAN_POINT('Ctrl Pts',(-6.09235996748979,-5.05033081057702,
90.8624615308338));
#235107=CARTESIAN_POINT('Ctrl Pts',(-6.21421105581252,-4.89566154404259,
90.8545601714762));
#235108=CARTESIAN_POINT('Ctrl Pts',(-6.33599940615083,-4.74107191272658,
90.8466628803248));
#235109=CARTESIAN_POINT('Ctrl Pts',(-6.45208404818364,-4.58184841806269,
90.8387655891734));
#235110=CARTESIAN_POINT('Ctrl Pts',(-6.56210327760371,-4.41845239581266,
90.830868298022));
#235111=CARTESIAN_POINT('Ctrl Pts',(-6.67208510415121,-4.25511192276645,
90.8229736916865));
#235112=CARTESIAN_POINT('Ctrl Pts',(-6.77600543513875,-4.08760203167126,
90.815079085351));
#235113=CARTESIAN_POINT('Ctrl Pts',(-6.87354472814376,-3.9164146703595,
90.8071844790155));
#235114=CARTESIAN_POINT('Ctrl Pts',(-6.94203826633047,-3.79620436630813,
90.8016407693591));
#235115=CARTESIAN_POINT('Ctrl Pts',(-7.00738614932013,-3.67418133657432,
90.7960970597027));
#235116=CARTESIAN_POINT('Ctrl Pts',(-7.06949083333909,-3.5505239553247,
90.7905533500463));
#235117=CARTESIAN_POINT('Ctrl Pts',(-7.16340878593694,-3.36352279343119,
90.7821698622474));
#235118=CARTESIAN_POINT('Ctrl Pts',(-7.24982532033329,-3.17294811778614,
90.7737863744485));
#235119=CARTESIAN_POINT('Ctrl Pts',(-7.3285066088175,-2.97941468824301,
90.7654028866496));
#235120=CARTESIAN_POINT('Ctrl Pts',(-7.40729971606535,-2.78560621657449,
90.7570074845665));
#235121=CARTESIAN_POINT('Ctrl Pts',(-7.47833551473938,-2.58883084456481,
90.7486120824832));
#235122=CARTESIAN_POINT('Ctrl Pts',(-7.54142969395733,-2.38971947539844,
90.7402166804001));
#235123=CARTESIAN_POINT('Ctrl Pts',(-7.60467134316919,-2.19014272332732,
90.7318016557477));
#235124=CARTESIAN_POINT('Ctrl Pts',(-7.65993415822487,-1.98821931382836,
90.7233866310954));
#235125=CARTESIAN_POINT('Ctrl Pts',(-7.70708407564648,-1.78459408575633,
90.7149716064431));
#235126=CARTESIAN_POINT('Ctrl Pts',(-7.75428929441626,-1.58073002906592,
90.7065467119493));
#235127=CARTESIAN_POINT('Ctrl Pts',(-7.79336255777397,-1.37516043548086,
90.6981218174556));
#235128=CARTESIAN_POINT('Ctrl Pts',(-7.82422139285953,-1.16853780234929,
90.6896969229619));
#235129=CARTESIAN_POINT('Ctrl Pts',(-7.85514399266982,-0.961488217413219,
90.6812546198046));
#235130=CARTESIAN_POINT('Ctrl Pts',(-7.87781818003956,-0.753381513032924,
90.6728123166472));
#235131=CARTESIAN_POINT('Ctrl Pts',(-7.89221335862975,-0.544875492076966,
90.6643700134899));
#235132=CARTESIAN_POINT('Ctrl Pts',(-7.90473949093695,-0.363441549526122,
90.6570238450722));
#235133=CARTESIAN_POINT('Ctrl Pts',(-7.910997733292,-0.181705379616724,
90.6496776766546));
#235134=CARTESIAN_POINT('Ctrl Pts',(-7.91099999938413,-9.87136388252182E-5,
90.6423315082369));
#235135=CARTESIAN_POINT('',(-7.91135449193049,-0.00500362976431777,88.6423315082369));
#235136=CARTESIAN_POINT('Ctrl Pts',(-7.92012792240699,-9.7123266765243E-5,
90.6423314393769));
#235137=CARTESIAN_POINT('Ctrl Pts',(-7.92010724319683,0.0884449210834555,
90.6387539543251));
#235138=CARTESIAN_POINT('Ctrl Pts',(-7.91850031101797,0.17698031386293,
90.6351764692733));
#235139=CARTESIAN_POINT('Ctrl Pts',(-7.82012699933287,2.88639504458979,
90.5256294070049));
#235140=CARTESIAN_POINT('Ctrl Pts',(-4.81214997345493,8.03372540585939,
90.3136902525721));
#235141=CARTESIAN_POINT('Ctrl Pts',(4.17302520961857,8.37571682006808,89.9957815209222));
#235142=CARTESIAN_POINT('Ctrl Pts',(8.41895931796156,2.27239210928254,89.7308575778813));
#235143=CARTESIAN_POINT('Ctrl Pts',(7.62246482467963,-3.11822080623645,
89.518918423448));
#235144=CARTESIAN_POINT('Ctrl Pts',(5.21197134772341,-6.39936160446069,
89.3599640576236));
#235145=CARTESIAN_POINT('Ctrl Pts',(1.51916769345805,-8.09428556441293,
89.2010096917984));
#235146=CARTESIAN_POINT('Ctrl Pts',(-3.93614139152924,-7.78672095142201,
88.9890705373658));
#235147=CARTESIAN_POINT('Ctrl Pts',(-7.51177695944173,-3.99820861181208,
88.8028444761783));
#235148=CARTESIAN_POINT('Ctrl Pts',(-7.91518164929367,-0.685376453820117,
88.6696032035994));
#235149=CARTESIAN_POINT('Ctrl Pts',(-7.91142808499138,-0.00604239087124009,
88.6423315082369));
#235150=CARTESIAN_POINT('',(-7.911,2.36866082303777E-12,86.6423315082369));
#235151=CARTESIAN_POINT('Ctrl Pts',(-7.911,2.76390021980433E-12,88.6423315082369));
#235152=CARTESIAN_POINT('Ctrl Pts',(-7.91099999999923,2.20167589666949,
88.5537440725042));
#235153=CARTESIAN_POINT('Ctrl Pts',(-6.94214576672222,4.38610418338917,
88.4651566367715));
#235154=CARTESIAN_POINT('Ctrl Pts',(-3.67820201488045,7.34180684107751,
88.287981765306));
#235155=CARTESIAN_POINT('Ctrl Pts',(-1.40868175871484,8.0899266657138,88.1993943295733));
#235156=CARTESIAN_POINT('Ctrl Pts',(2.9730927052151,7.65454228025164,88.0222194581079));
#235157=CARTESIAN_POINT('Ctrl Pts',(5.05102072675798,6.47444880834072,87.9336320223751));
#235158=CARTESIAN_POINT('Ctrl Pts',(7.66951518847956,2.93425195367483,87.7564571509097));
#235159=CARTESIAN_POINT('Ctrl Pts',(8.18956872247087,0.601881960096832,
87.6678697151769));
#235160=CARTESIAN_POINT('Ctrl Pts',(7.3230668976124,-3.7153719823265,87.4906948437115));
#235161=CARTESIAN_POINT('Ctrl Pts',(5.94329958850049,-5.66643518936669,
87.4021074079788));
#235162=CARTESIAN_POINT('Ctrl Pts',(2.16154501637644,-7.92205913233052,
87.2249325365133));
#235163=CARTESIAN_POINT('Ctrl Pts',(-0.210816529302415,-8.20894963712996,
87.1363451007806));
#235164=CARTESIAN_POINT('Ctrl Pts',(-4.42123908576601,-6.91982244717725,
86.9591702293152));
#235165=CARTESIAN_POINT('Ctrl Pts',(-6.22631625634311,-5.35390358803376,
86.8705827935824));
#235166=CARTESIAN_POINT('Ctrl Pts',(-7.65317280859549,-2.31334857514328,
86.7354407413121));
#235167=CARTESIAN_POINT('Ctrl Pts',(-7.91100000000035,-1.15702837836302,
86.6888861247745));
#235168=CARTESIAN_POINT('Ctrl Pts',(-7.911,2.36866082303777E-12,86.6423315082369));
#235169=CARTESIAN_POINT('',(-7.911,1.97397653778353E-12,84.6423315082369));
#235170=CARTESIAN_POINT('Ctrl Pts',(-7.911,2.36866082303777E-12,86.6423315082369));
#235171=CARTESIAN_POINT('Ctrl Pts',(-7.91099999999934,2.20167589666909,
86.5537440725042));
#235172=CARTESIAN_POINT('Ctrl Pts',(-6.94214576672244,4.38610418338882,
86.4651566367715));
#235173=CARTESIAN_POINT('Ctrl Pts',(-3.67820201488082,7.34180684107733,
86.2879817653061));
#235174=CARTESIAN_POINT('Ctrl Pts',(-1.40868175871525,8.08992666571373,
86.1993943295733));
#235175=CARTESIAN_POINT('Ctrl Pts',(2.97309270521472,7.65454228025179,86.0222194581079));
#235176=CARTESIAN_POINT('Ctrl Pts',(5.05102072675766,6.47444880834097,85.9336320223751));
#235177=CARTESIAN_POINT('Ctrl Pts',(7.66951518847941,2.93425195367521,85.7564571509097));
#235178=CARTESIAN_POINT('Ctrl Pts',(8.18956872247084,0.601881960097242,
85.667869715177));
#235179=CARTESIAN_POINT('Ctrl Pts',(7.32306689761258,-3.71537198232613,
85.4906948437115));
#235180=CARTESIAN_POINT('Ctrl Pts',(5.94329958850078,-5.66643518936639,
85.4021074079788));
#235181=CARTESIAN_POINT('Ctrl Pts',(2.16154501637684,-7.92205913233041,
85.2249325365134));
#235182=CARTESIAN_POINT('Ctrl Pts',(-0.210816529302006,-8.20894963712997,
85.1363451007806));
#235183=CARTESIAN_POINT('Ctrl Pts',(-4.42123908576567,-6.91982244717747,
84.9591702293152));
#235184=CARTESIAN_POINT('Ctrl Pts',(-6.22631625634284,-5.35390358803407,
84.8705827935825));
#235185=CARTESIAN_POINT('Ctrl Pts',(-7.65317280859537,-2.31334857514366,
84.7354407413121));
#235186=CARTESIAN_POINT('Ctrl Pts',(-7.91100000000029,-1.15702837836341,
84.6888861247746));
#235187=CARTESIAN_POINT('Ctrl Pts',(-7.911,1.97397653778353E-12,84.6423315082369));
#235188=CARTESIAN_POINT('',(-7.911,1.80300219199125E-12,82.642331508237));
#235189=CARTESIAN_POINT('Ctrl Pts',(-7.911,1.97397653778353E-12,84.6423315082369));
#235190=CARTESIAN_POINT('Ctrl Pts',(-7.91099999999945,2.20167589666877,
84.5537440725042));
#235191=CARTESIAN_POINT('Ctrl Pts',(-6.94214576672259,4.38610418338862,
84.4651566367715));
#235192=CARTESIAN_POINT('Ctrl Pts',(-3.67820201488093,7.3418068410773,84.2879817653061));
#235193=CARTESIAN_POINT('Ctrl Pts',(-1.40868175871527,8.08992666571375,
84.1993943295733));
#235194=CARTESIAN_POINT('Ctrl Pts',(2.97309270521485,7.65454228025176,84.0222194581079));
#235195=CARTESIAN_POINT('Ctrl Pts',(5.05102072675784,6.47444880834085,83.9336320223751));
#235196=CARTESIAN_POINT('Ctrl Pts',(7.66951518847956,2.93425195367488,83.7564571509097));
#235197=CARTESIAN_POINT('Ctrl Pts',(8.1895687224709,0.601881960096794,83.667869715177));
#235198=CARTESIAN_POINT('Ctrl Pts',(7.32306689761233,-3.71537198232667,
83.4906948437115));
#235199=CARTESIAN_POINT('Ctrl Pts',(5.94329958850032,-5.6664351893669,83.4021074079788));
#235200=CARTESIAN_POINT('Ctrl Pts',(2.16154501637605,-7.92205913233065,
83.2249325365133));
#235201=CARTESIAN_POINT('Ctrl Pts',(-0.210816529302923,-8.20894963712997,
83.1363451007806));
#235202=CARTESIAN_POINT('Ctrl Pts',(-4.42123908576658,-6.91982244717691,
82.9591702293151));
#235203=CARTESIAN_POINT('Ctrl Pts',(-6.22631625634361,-5.35390358803321,
82.8705827935824));
#235204=CARTESIAN_POINT('Ctrl Pts',(-7.65317280859553,-2.31334857514293,
82.7354407413121));
#235205=CARTESIAN_POINT('Ctrl Pts',(-7.91100000000026,-1.15702837836313,
82.6888861247745));
#235206=CARTESIAN_POINT('Ctrl Pts',(-7.911,1.80300219199125E-12,82.642331508237));
#235207=CARTESIAN_POINT('',(-7.91099999999884,-4.25400661031056E-6,80.6423316794028));
#235208=CARTESIAN_POINT('Ctrl Pts',(-7.911,1.80300219199125E-12,82.642331508237));
#235209=CARTESIAN_POINT('Ctrl Pts',(-7.9109999999995,2.20167589666852,82.5537440725042));
#235210=CARTESIAN_POINT('Ctrl Pts',(-6.94214576672275,4.38610418338832,
82.4651566367715));
#235211=CARTESIAN_POINT('Ctrl Pts',(-3.67820201488135,7.34180684107707,
82.2879817653061));
#235212=CARTESIAN_POINT('Ctrl Pts',(-1.40868175871583,8.08992666571363,
82.1993943295733));
#235213=CARTESIAN_POINT('Ctrl Pts',(2.97309270521417,7.654542280252,82.0222194581079));
#235214=CARTESIAN_POINT('Ctrl Pts',(5.05102072675719,6.47444880834133,81.9336320223752));
#235215=CARTESIAN_POINT('Ctrl Pts',(7.6695151884792,2.93425195367576,81.7564571509097));
#235216=CARTESIAN_POINT('Ctrl Pts',(8.1895687224708,0.601881960097828,81.667869715177));
#235217=CARTESIAN_POINT('Ctrl Pts',(7.32306689761285,-3.71537198232561,
81.4906948437116));
#235218=CARTESIAN_POINT('Ctrl Pts',(5.94329958850118,-5.66643518936597,
81.4021074079788));
#235219=CARTESIAN_POINT('Ctrl Pts',(2.16154501637741,-7.92205913233026,
81.2249325365134));
#235220=CARTESIAN_POINT('Ctrl Pts',(-0.210816529301418,-8.20894963712999,
81.1363451007806));
#235221=CARTESIAN_POINT('Ctrl Pts',(-4.42123908576517,-6.91982244717778,
80.9591702293152));
#235222=CARTESIAN_POINT('Ctrl Pts',(-6.22631625634246,-5.35390358803451,
80.8705827935825));
#235223=CARTESIAN_POINT('Ctrl Pts',(-7.65317220619433,-2.31334985882827,
80.7354407983674));
#235224=CARTESIAN_POINT('Ctrl Pts',(-7.91099936803671,-1.15703121263333,
80.6888862388851));
#235225=CARTESIAN_POINT('Ctrl Pts',(-7.91099999999884,-4.25400661031052E-6,
80.6423316794028));
#235226=CARTESIAN_POINT('',(-7.92502143214218,0.00372523665453262,76.642331508237));
#235227=CARTESIAN_POINT('Ctrl Pts',(-7.91099999985351,-4.81432872164594E-5,
80.6412939480464));
#235228=CARTESIAN_POINT('Ctrl Pts',(-7.91100257635899,0.423328323470568,
80.6236424389112));
#235229=CARTESIAN_POINT('Ctrl Pts',(-7.87701747137843,0.846047094394404,
80.6062432736875));
#235230=CARTESIAN_POINT('Ctrl Pts',(-7.80305174663063,1.30302162523151,
80.5874701706095));
#235231=CARTESIAN_POINT('Ctrl Pts',(-7.79644699090499,1.34197475883232,
80.585870859129));
#235232=CARTESIAN_POINT('Ctrl Pts',(-7.78515772330068,1.40565771452233,
80.5832577175704));
#235233=CARTESIAN_POINT('Ctrl Pts',(-7.78064651787767,1.430417476116,80.5822421092159));
#235234=CARTESIAN_POINT('Ctrl Pts',(-7.77242693172883,1.4743410640839,80.5804410733706));
#235235=CARTESIAN_POINT('Ctrl Pts',(-7.76876563614406,1.49351346675973,
80.5796551494238));
#235236=CARTESIAN_POINT('Ctrl Pts',(-7.76132384667845,1.53171456920015,
80.5780896112955));
#235237=CARTESIAN_POINT('Ctrl Pts',(-7.75754423629362,1.55074330528034,
80.5773099930788));
#235238=CARTESIAN_POINT('Ctrl Pts',(-7.74987263149103,1.58863658699438,
80.5757578771316));
#235239=CARTESIAN_POINT('Ctrl Pts',(-7.7459816604466,1.60750120630538,80.5749853735629));
#235240=CARTESIAN_POINT('Ctrl Pts',(-7.73523236771968,1.65867173192364,
80.5728904426931));
#235241=CARTESIAN_POINT('Ctrl Pts',(-7.72824056966414,1.69094926191849,
80.5715695322991));
#235242=CARTESIAN_POINT('Ctrl Pts',(-7.70089308969035,1.81348487054252,
80.5665566893789));
#235243=CARTESIAN_POINT('Ctrl Pts',(-7.67915652412774,1.90342772299259,
80.5628808929967));
#235244=CARTESIAN_POINT('Ctrl Pts',(-7.60503027982869,2.18817832085411,
80.5512472965636));
#235245=CARTESIAN_POINT('Ctrl Pts',(-7.54676532599002,2.38137467340516,
80.5433614393516));
#235246=CARTESIAN_POINT('Ctrl Pts',(-7.43900827308007,2.69479122276379,
80.5305034948555));
#235247=CARTESIAN_POINT('Ctrl Pts',(-7.39382718649918,2.81639197050389,
80.5254976881248));
#235248=CARTESIAN_POINT('Ctrl Pts',(-7.2247862680274,3.23920193124665,80.5079672303777));
#235249=CARTESIAN_POINT('Ctrl Pts',(-7.08534255681913,3.5338197360161,80.4955359681529));
#235250=CARTESIAN_POINT('Ctrl Pts',(-6.85053571361749,3.95978856190524,
80.4766238781403));
#235251=CARTESIAN_POINT('Ctrl Pts',(-6.76865720522682,4.09817551814219,
80.4703190822393));
#235252=CARTESIAN_POINT('Ctrl Pts',(-6.66474863924903,4.26217805596696,
80.4625754928917));
#235253=CARTESIAN_POINT('Ctrl Pts',(-6.64669745716633,4.29027377824695,
80.4612389976533));
#235254=CARTESIAN_POINT('Ctrl Pts',(-6.62252910084508,4.32737191885125,
80.4594602801798));
#235255=CARTESIAN_POINT('Ctrl Pts',(-6.61657037883429,4.33647735338772,
80.4590225830894));
#235256=CARTESIAN_POINT('Ctrl Pts',(-6.6054303851961,4.35342379663038,80.4582058924342));
#235257=CARTESIAN_POINT('Ctrl Pts',(-6.600253885955,4.36126793112905,80.457827031843));
#235258=CARTESIAN_POINT('Ctrl Pts',(-6.58945431135344,4.37756964857835,
80.4570379642866));
#235259=CARTESIAN_POINT('Ctrl Pts',(-6.58382890329585,4.38602566351143,
80.4566276945091));
#235260=CARTESIAN_POINT('Ctrl Pts',(-6.57093528839604,4.40532642046014,
80.4556890723732));
#235261=CARTESIAN_POINT('Ctrl Pts',(-6.56365649496654,4.41616404243629,
80.4551604415119));
#235262=CARTESIAN_POINT('Ctrl Pts',(-6.54122689357849,4.44938222256679,
80.4535353428928));
#235263=CARTESIAN_POINT('Ctrl Pts',(-6.52598824372088,4.47170312814809,
80.4524366453631));
#235264=CARTESIAN_POINT('Ctrl Pts',(-6.38244623284158,4.67966064377969,
80.4421390890349));
#235265=CARTESIAN_POINT('Ctrl Pts',(-6.24637185614294,4.85980225658652,
80.4327625313605));
#235266=CARTESIAN_POINT('Ctrl Pts',(-6.0262532818032,5.12666157701905,80.4182891288265));
#235267=CARTESIAN_POINT('Ctrl Pts',(-5.94761361306142,5.21768911102217,
80.4132398388784));
#235268=CARTESIAN_POINT('Ctrl Pts',(-5.65471827256188,5.54149401266744,
80.3948989761496));
#235269=CARTESIAN_POINT('Ctrl Pts',(-5.42862294397031,5.76316344153982,
80.3816157447365));
#235270=CARTESIAN_POINT('Ctrl Pts',(-5.06385277380281,6.08022949783928,
80.3615685954509));
#235271=CARTESIAN_POINT('Ctrl Pts',(-4.93440742059983,6.18574332417144,
80.3546908858447));
#235272=CARTESIAN_POINT('Ctrl Pts',(-4.74354907268072,6.33151014012456,
80.3448753352736));
#235273=CARTESIAN_POINT('Ctrl Pts',(-4.68476521366669,6.3751277225059,80.3418944079285));
#235274=CARTESIAN_POINT('Ctrl Pts',(-4.57865220080663,6.45160315123772,
80.3365862683638));
#235275=CARTESIAN_POINT('Ctrl Pts',(-4.53155354618199,6.48477152379194,
80.3342552166449));
#235276=CARTESIAN_POINT('Ctrl Pts',(-4.45977733010866,6.53415476987012,
80.3307392659494));
#235277=CARTESIAN_POINT('Ctrl Pts',(-4.43536451914986,6.55075064256006,
80.3295496881913));
#235278=CARTESIAN_POINT('Ctrl Pts',(-4.39125503082659,6.58037673377982,
80.3274114085475));
#235279=CARTESIAN_POINT('Ctrl Pts',(-4.37159182949589,6.59345611834209,
80.326462123681));
#235280=CARTESIAN_POINT('Ctrl Pts',(-4.32907239210385,6.62146498146732,
80.3244177025369));
#235281=CARTESIAN_POINT('Ctrl Pts',(-4.30619683396836,6.63636460044106,
80.3233229281999));
#235282=CARTESIAN_POINT('Ctrl Pts',(-4.244044172706,6.67639004371176,80.3203620100793));
#235283=CARTESIAN_POINT('Ctrl Pts',(-4.2046212443013,6.70128757598071,80.3184984988389));
#235284=CARTESIAN_POINT('Ctrl Pts',(-4.0066949056698,6.82385366516267,80.309212211609));
#235285=CARTESIAN_POINT('Ctrl Pts',(-3.84499736244249,6.91625471228844,
80.3018465740832));
#235286=CARTESIAN_POINT('Ctrl Pts',(-3.11019412057477,7.3024131202901,80.269161658121));
#235287=CARTESIAN_POINT('Ctrl Pts',(-2.50574480187838,7.53125801775332,
80.2447614219016));
#235288=CARTESIAN_POINT('Ctrl Pts',(-1.64465310842037,7.7419545602089,80.2118252192316));
#235289=CARTESIAN_POINT('Ctrl Pts',(-1.40654390082939,7.78873394545177,
80.2028586642778));
#235290=CARTESIAN_POINT('Ctrl Pts',(-0.967204309309037,7.8542412640535,
80.1862134935696));
#235291=CARTESIAN_POINT('Ctrl Pts',(-0.766684728600054,7.87634304806157,
80.1785770654113));
#235292=CARTESIAN_POINT('Ctrl Pts',(-0.473931471669022,7.89732527160054,
80.1671581433925));
#235293=CARTESIAN_POINT('Ctrl Pts',(-0.382210604030192,7.90229535083546,
80.163541787853));
#235294=CARTESIAN_POINT('Ctrl Pts',(-0.275984242953884,7.90619773009887,
80.1592906049665));
#235295=CARTESIAN_POINT('Ctrl Pts',(-0.261540979114007,7.90668869772354,
80.1587112382315));
#235296=CARTESIAN_POINT('Ctrl Pts',(-0.239616753261383,7.90737382529358,
80.1578296457148));
#235297=CARTESIAN_POINT('Ctrl Pts',(-0.232136685368093,7.90759695231192,
80.1575284875577));
#235298=CARTESIAN_POINT('Ctrl Pts',(-0.218599416794738,7.90798153834219,
80.1569827578653));
#235299=CARTESIAN_POINT('Ctrl Pts',(-0.21254232003349,7.90814665251786,
80.1567383237233));
#235300=CARTESIAN_POINT('Ctrl Pts',(-0.200452568070444,7.90846231473651,
80.1562499262384));
#235301=CARTESIAN_POINT('Ctrl Pts',(-0.194419918685007,7.90861291950778,
80.1560059652401));
#235302=CARTESIAN_POINT('Ctrl Pts',(-0.177491679939836,7.90901615129111,
80.1553206535));
#235303=CARTESIAN_POINT('Ctrl Pts',(-0.166595757152461,7.90925316512054,
80.1548786993345));
#235304=CARTESIAN_POINT('Ctrl Pts',(-0.122185546973423,7.91012738878037,
80.1530737780868));
#235305=CARTESIAN_POINT('Ctrl Pts',(-0.0886681787073125,7.91057409549701,
80.1517032565867));
#235306=CARTESIAN_POINT('Ctrl Pts',(0.431899376155758,7.91420317672486,
80.1302756713965));
#235307=CARTESIAN_POINT('Ctrl Pts',(0.918131024994542,7.87261122472651,
80.1081097101464));
#235308=CARTESIAN_POINT('Ctrl Pts',(1.71809507071396,7.7290528431356,80.0707080044382));
#235309=CARTESIAN_POINT('Ctrl Pts',(2.03498180807262,7.65172974046777,80.0556413150283));
#235310=CARTESIAN_POINT('Ctrl Pts',(2.68233236071016,7.45069759872589,80.0250012436343));
#235311=CARTESIAN_POINT('Ctrl Pts',(3.01114398170241,7.32399138363621,80.0095231287553));
#235312=CARTESIAN_POINT('Ctrl Pts',(3.45681372319178,7.11714605858283,79.9888680857794));
#235313=CARTESIAN_POINT('Ctrl Pts',(3.58161216926669,7.05516731874095,79.983118444383));
#235314=CARTESIAN_POINT('Ctrl Pts',(3.72122728119742,6.98117023537433,79.976721489916));
#235315=CARTESIAN_POINT('Ctrl Pts',(3.73771061874789,6.97235897455571,79.9759668055988));
#235316=CARTESIAN_POINT('Ctrl Pts',(3.76244541255824,6.95902393023984,79.9748351427937));
#235317=CARTESIAN_POINT('Ctrl Pts',(3.77072022316311,6.95454373366976,79.9744566919036));
#235318=CARTESIAN_POINT('Ctrl Pts',(3.78494593744594,6.94680871027184,79.9738063063536));
#235319=CARTESIAN_POINT('Ctrl Pts',(3.79090067570193,6.94356097933376,79.9735341316392));
#235320=CARTESIAN_POINT('Ctrl Pts',(3.80316252834932,6.93685285534439,79.9729738183408));
#235321=CARTESIAN_POINT('Ctrl Pts',(3.80946911460674,6.93339150913244,79.9726857125224));
#235322=CARTESIAN_POINT('Ctrl Pts',(3.82465128253924,6.9250318653289,79.9719923249827));
#235323=CARTESIAN_POINT('Ctrl Pts',(3.83352219802981,6.9201250947534,79.9715873318625));
#235324=CARTESIAN_POINT('Ctrl Pts',(3.86074978334397,6.90499627561509,79.9703447389674));
#235325=CARTESIAN_POINT('Ctrl Pts',(3.8790752457855,6.89471810168413,79.9695090536308));
#235326=CARTESIAN_POINT('Ctrl Pts',(4.09045781241781,6.77505076225895,79.9598764872261));
#235327=CARTESIAN_POINT('Ctrl Pts',(4.27887820668434,6.65765484623747,79.9513616254832));
#235328=CARTESIAN_POINT('Ctrl Pts',(4.48253568863013,6.51854323401972,79.9421648413862));
#235329=CARTESIAN_POINT('Ctrl Pts',(4.50288303615596,6.5045043213996,79.9412460240785));
#235330=CARTESIAN_POINT('Ctrl Pts',(4.82464981636451,6.28026379596321,79.9267145857753));
#235331=CARTESIAN_POINT('Ctrl Pts',(5.11113909994778,6.04939959666413,79.913780307824));
#235332=CARTESIAN_POINT('Ctrl Pts',(5.57536377624048,5.61870627584345,79.891820816936));
#235333=CARTESIAN_POINT('Ctrl Pts',(5.76094534645344,5.42826383098148,79.8827114818377));
#235334=CARTESIAN_POINT('Ctrl Pts',(6.10323751740224,5.03964112773595,79.8646307840982));
#235335=CARTESIAN_POINT('Ctrl Pts',(6.26073855914029,4.84258537352525,79.8556848526237));
#235336=CARTESIAN_POINT('Ctrl Pts',(6.43649506144405,4.59975251369358,79.844551666801));
#235337=CARTESIAN_POINT('Ctrl Pts',(6.46408545864606,4.56089804033258,79.8427670650363));
#235338=CARTESIAN_POINT('Ctrl Pts',(6.5425873724176,4.44820363061286,79.8375755182173));
#235339=CARTESIAN_POINT('Ctrl Pts',(6.59259530718062,4.37374568099061,79.834126561785));
#235340=CARTESIAN_POINT('Ctrl Pts',(6.66678331916852,4.25912156138608,79.8287668203078));
#235341=CARTESIAN_POINT('Ctrl Pts',(6.6918901701621,4.2195642002757,79.8269076790374));
#235342=CARTESIAN_POINT('Ctrl Pts',(6.72231500356361,4.17067346886978,79.8245988157248));
#235343=CARTESIAN_POINT('Ctrl Pts',(6.72796707284153,4.16154962197275,79.8241674932859));
#235344=CARTESIAN_POINT('Ctrl Pts',(6.73674887488235,4.14730895566075,79.8234936132373));
#235345=CARTESIAN_POINT('Ctrl Pts',(6.73989139932079,4.14220000748476,79.8232517207053));
#235346=CARTESIAN_POINT('Ctrl Pts',(6.74542980994529,4.13317296648359,79.8228240912561));
#235347=CARTESIAN_POINT('Ctrl Pts',(6.74782810292229,4.12925634770371,79.822638477466));
#235348=CARTESIAN_POINT('Ctrl Pts',(6.75290514234691,4.12094887056766,79.8222446187083));
#235349=CARTESIAN_POINT('Ctrl Pts',(6.75558301909624,4.11655748499725,79.8220363300023));
#235350=CARTESIAN_POINT('Ctrl Pts',(6.76317037186138,4.10408782590624,79.8214446237769));
#235351=CARTESIAN_POINT('Ctrl Pts',(6.76806964329129,4.09600337695679,79.8210606994604));
#235352=CARTESIAN_POINT('Ctrl Pts',(6.78866293344535,4.06188388592323,79.8194391755199));
#235353=CARTESIAN_POINT('Ctrl Pts',(6.80422117769425,4.03576749292719,79.8181950205303));
#235354=CARTESIAN_POINT('Ctrl Pts',(7.1577974729009,3.43439040158215,79.7894893387484));
#235355=CARTESIAN_POINT('Ctrl Pts',(7.42184596227242,2.81874919018932,79.7592267335175));
#235356=CARTESIAN_POINT('Ctrl Pts',(7.7155513250587,1.79279676379647,79.7128722242424));
#235357=CARTESIAN_POINT('Ctrl Pts',(7.79630955076411,1.40051685731983,79.6959556403277));
#235358=CARTESIAN_POINT('Ctrl Pts',(7.85288679114162,0.958227425595022,
79.6777616786957));
#235359=CARTESIAN_POINT('Ctrl Pts',(7.85831801615514,0.912616439820966,
79.6758950882937));
#235360=CARTESIAN_POINT('Ctrl Pts',(7.86721243164276,0.831943879952323,
79.6726098102521));
#235361=CARTESIAN_POINT('Ctrl Pts',(7.87083919714595,0.796901763602491,
79.6711881468534));
#235362=CARTESIAN_POINT('Ctrl Pts',(7.87582995958644,0.745317959853305,
79.6691029065887));
#235363=CARTESIAN_POINT('Ctrl Pts',(7.87737615106156,0.728794477709592,
79.6684360894341));
#235364=CARTESIAN_POINT('Ctrl Pts',(7.87995923823529,0.700221159929094,
79.6672848994107));
#235365=CARTESIAN_POINT('Ctrl Pts',(7.8810205151654,0.688173604213696,79.666800101242));
#235366=CARTESIAN_POINT('Ctrl Pts',(7.88308006429568,0.664163975256677,
79.6658350872083));
#235367=CARTESIAN_POINT('Ctrl Pts',(7.88407874628551,0.652201969783695,
79.6653548655072));
#235368=CARTESIAN_POINT('Ctrl Pts',(7.88637958287595,0.623865288765077,
79.6642185808774));
#235369=CARTESIAN_POINT('Ctrl Pts',(7.88765797153187,0.607488724261065,
79.6635629240978));
#235370=CARTESIAN_POINT('Ctrl Pts',(7.8913172211549,0.558652660618702,79.6616106933338));
#235371=CARTESIAN_POINT('Ctrl Pts',(7.89354879507739,0.526182206988769,
79.6603165896497));
#235372=CARTESIAN_POINT('Ctrl Pts',(7.91035217541734,0.257450696571845,
79.6496370096787));
#235373=CARTESIAN_POINT('Ctrl Pts',(7.914514015212,0.0206532130825134,79.6404289131966));
#235374=CARTESIAN_POINT('Ctrl Pts',(7.90442008748098,-0.34893111664469,
79.6262990780623));
#235375=CARTESIAN_POINT('Ctrl Pts',(7.89743684061129,-0.481769775350074,
79.6212683118086));
#235376=CARTESIAN_POINT('Ctrl Pts',(7.85275791172879,-1.05534427903552,
79.5996837703251));
#235377=CARTESIAN_POINT('Ctrl Pts',(7.78148690974655,-1.49265501324453,
79.5836255446691));
#235378=CARTESIAN_POINT('Ctrl Pts',(7.60879453376141,-2.18227279752326,
79.5573263957851));
#235379=CARTESIAN_POINT('Ctrl Pts',(7.530320658477,-2.43932957341266,79.5472816890605));
#235380=CARTESIAN_POINT('Ctrl Pts',(7.40486466137258,-2.78602270606196,
79.5329561659184));
#235381=CARTESIAN_POINT('Ctrl Pts',(7.36901680874553,-2.87950229486924,
79.5290128007756));
#235382=CARTESIAN_POINT('Ctrl Pts',(7.32600733100514,-2.98558939354802,
79.524423554775));
#235383=CARTESIAN_POINT('Ctrl Pts',(7.3205728097602,-2.99888999038699,79.5238461099371));
#235384=CARTESIAN_POINT('Ctrl Pts',(7.31232034250548,-3.01893119898145,
79.5229728099676));
#235385=CARTESIAN_POINT('Ctrl Pts',(7.30952922738296,-3.02568287320149,
79.5226780531907));
#235386=CARTESIAN_POINT('Ctrl Pts',(7.30469928457368,-3.03732075913274,
79.5221690161413));
#235387=CARTESIAN_POINT('Ctrl Pts',(7.30266489409153,-3.04220881537479,
79.5219549206508));
#235388=CARTESIAN_POINT('Ctrl Pts',(7.29845227240776,-3.05230196165035,
79.5215122311074));
#235389=CARTESIAN_POINT('Ctrl Pts',(7.2962733764268,-3.05750677087776,79.521283609091));
#235390=CARTESIAN_POINT('Ctrl Pts',(7.29099426339513,-3.07007940409096,
79.5207305314863));
#235391=CARTESIAN_POINT('Ctrl Pts',(7.28788844837573,-3.07744485891418,
79.5204058371182));
#235392=CARTESIAN_POINT('Ctrl Pts',(7.27636477087859,-3.10465803496324,
79.519203622789));
#235393=CARTESIAN_POINT('Ctrl Pts',(7.26787699818645,-3.12447591116916,
79.5183230660393));
#235394=CARTESIAN_POINT('Ctrl Pts',(7.14598847550664,-3.4058860801337,79.5057446697801));
#235395=CARTESIAN_POINT('Ctrl Pts',(7.01863244436319,-3.66114058369329,
79.4933052538471));
#235396=CARTESIAN_POINT('Ctrl Pts',(6.6638642419253,-4.28535949515461,79.4609930872312));
#235397=CARTESIAN_POINT('Ctrl Pts',(6.41938218852172,-4.64359018436774,
79.4407712517041));
#235398=CARTESIAN_POINT('Ctrl Pts',(5.93785470884569,-5.23793751246095,
79.4059340337106));
#235399=CARTESIAN_POINT('Ctrl Pts',(5.71285582396468,-5.48246441320965,
79.3911363733515));
#235400=CARTESIAN_POINT('Ctrl Pts',(5.39597936913816,-5.78608228231994,
79.3723863000397));
#235401=CARTESIAN_POINT('Ctrl Pts',(5.31732396739807,-5.85844762209079,
79.3678840072062));
#235402=CARTESIAN_POINT('Ctrl Pts',(5.16785720904836,-5.99047067243447,
79.359608960847));
#235403=CARTESIAN_POINT('Ctrl Pts',(5.0974186777621,-6.05052151638252,79.3558198943539));
#235404=CARTESIAN_POINT('Ctrl Pts',(5.01367545102962,-6.11941432893087,
79.3514419098783));
#235405=CARTESIAN_POINT('Ctrl Pts',(5.00137958796215,-6.12946779732583,
79.3508022347687));
#235406=CARTESIAN_POINT('Ctrl Pts',(4.98254204400987,-6.14477551880341,
79.3498270059289));
#235407=CARTESIAN_POINT('Ctrl Pts',(4.97602217775554,-6.15005647810439,
79.3494903377724));
#235408=CARTESIAN_POINT('Ctrl Pts',(4.96465938491203,-6.15923021155808,
79.3489051013172));
#235409=CARTESIAN_POINT('Ctrl Pts',(4.95982025685341,-6.16312766597506,
79.3486563381076));
#235410=CARTESIAN_POINT('Ctrl Pts',(4.94971464922073,-6.17124715535377,
79.3481378303156));
#235411=CARTESIAN_POINT('Ctrl Pts',(4.94444734628547,-6.17546816049518,
79.3478681286437));
#235412=CARTESIAN_POINT('Ctrl Pts',(4.9299235427613,-6.18707645960809,79.3471259994543));
#235413=CARTESIAN_POINT('Ctrl Pts',(4.92065582837977,-6.19444973139401,
79.3466541544731));
#235414=CARTESIAN_POINT('Ctrl Pts',(4.88461966789591,-6.22298772222383,
79.3448260664416));
#235415=CARTESIAN_POINT('Ctrl Pts',(4.85773075959416,-6.24400011183762,
79.343476133452));
#235416=CARTESIAN_POINT('Ctrl Pts',(4.44257708384931,-6.56411781486267,
79.3228475060404));
#235417=CARTESIAN_POINT('Ctrl Pts',(4.02746558814835,-6.82669241445261,
79.3051735298626));
#235418=CARTESIAN_POINT('Ctrl Pts',(3.12409367736634,-7.28684725121567,
79.2703020286636));
#235419=CARTESIAN_POINT('Ctrl Pts',(2.63509451321552,-7.4775892494324,79.2532958375807));
#235420=CARTESIAN_POINT('Ctrl Pts',(1.95333413901935,-7.66827145460961,
79.2285687687574));
#235421=CARTESIAN_POINT('Ctrl Pts',(1.77413567222701,-7.7117013662272,79.221968771558));
#235422=CARTESIAN_POINT('Ctrl Pts',(1.46953484973944,-7.77434432124202,
79.2103517689428));
#235423=CARTESIAN_POINT('Ctrl Pts',(1.34488785193147,-7.7968734734457,79.2054870339007));
#235424=CARTESIAN_POINT('Ctrl Pts',(1.19883743826907,-7.81966483963672,
79.1996049120491));
#235425=CARTESIAN_POINT('Ctrl Pts',(1.17790219098917,-7.82284576220844,
79.1987574087489));
#235426=CARTESIAN_POINT('Ctrl Pts',(1.15053644910662,-7.82689139904885,
79.1976436343297));
#235427=CARTESIAN_POINT('Ctrl Pts',(1.14411713083316,-7.82783233620028,
79.1973819433387));
#235428=CARTESIAN_POINT('Ctrl Pts',(1.13367661474274,-7.82934957933406,
79.1969556187056));
#235429=CARTESIAN_POINT('Ctrl Pts',(1.12965610628783,-7.82993068830342,
79.1967912766765));
#235430=CARTESIAN_POINT('Ctrl Pts',(1.12193501216123,-7.8310405951247,79.1964753406692));
#235431=CARTESIAN_POINT('Ctrl Pts',(1.11823449465726,-7.83156986745732,
79.1963237757331));
#235432=CARTESIAN_POINT('Ctrl Pts',(1.1097815650264,-7.83277274770226,79.1959772285256));
#235433=CARTESIAN_POINT('Ctrl Pts',(1.10502894572362,-7.83344464895138,
79.1957821423553));
#235434=CARTESIAN_POINT('Ctrl Pts',(1.08994656561594,-7.83556292039606,
79.195162270552));
#235435=CARTESIAN_POINT('Ctrl Pts',(1.07961462924598,-7.8369931763136,79.1947364975708));
#235436=CARTESIAN_POINT('Ctrl Pts',(0.991580744751443,-7.84900236585298,
79.1910991662262));
#235437=CARTESIAN_POINT('Ctrl Pts',(0.913730813428599,-7.85844550016604,
79.1878195622358));
#235438=CARTESIAN_POINT('Ctrl Pts',(0.481019336274078,-7.90441647989722,
79.1692962945861));
#235439=CARTESIAN_POINT('Ctrl Pts',(0.124164678765431,-7.9180631132183,
79.1529414613027));
#235440=CARTESIAN_POINT('Ctrl Pts',(-0.767699417545959,-7.89185622959243,
79.1114295054131));
#235441=CARTESIAN_POINT('Ctrl Pts',(-1.3001184343718,-7.82179971853014,
79.0861683142335));
#235442=CARTESIAN_POINT('Ctrl Pts',(-2.13250282279253,-7.62486456022967,
79.0483503196822));
#235443=CARTESIAN_POINT('Ctrl Pts',(-2.43888402928554,-7.53246351013656,
79.034780303191));
#235444=CARTESIAN_POINT('Ctrl Pts',(-2.75705437964557,-7.41504876749888,
79.0210884355062));
#235445=CARTESIAN_POINT('Ctrl Pts',(-2.77522312111499,-7.40826792929645,
79.0203079235865));
#235446=CARTESIAN_POINT('Ctrl Pts',(-2.80167151291123,-7.39828605320154,
79.0191736570398));
#235447=CARTESIAN_POINT('Ctrl Pts',(-2.80997092654295,-7.39513780696166,
79.0188180060387));
#235448=CARTESIAN_POINT('Ctrl Pts',(-2.82451322249321,-7.3895934103642,
79.0181953149664));
#235449=CARTESIAN_POINT('Ctrl Pts',(-2.83075838963008,-7.38720330398279,
79.0179280577578));
#235450=CARTESIAN_POINT('Ctrl Pts',(-2.84286757000561,-7.38255135313997,
79.0174101562369));
#235451=CARTESIAN_POINT('Ctrl Pts',(-2.84873193109052,-7.38029043380816,
79.0171594789088));
#235452=CARTESIAN_POINT('Ctrl Pts',(-2.86270705814136,-7.37488338766276,
79.0165624253177));
#235453=CARTESIAN_POINT('Ctrl Pts',(-2.8708153500614,-7.37173086248394,
79.0162162799106));
#235454=CARTESIAN_POINT('Ctrl Pts',(-2.89969454680459,-7.36044768148992,
79.0149843427614));
#235455=CARTESIAN_POINT('Ctrl Pts',(-2.92043634053296,-7.35224252379918,
79.0141012398959));
#235456=CARTESIAN_POINT('Ctrl Pts',(-3.20672902961346,-7.2375865348228,
79.0019350136791));
#235457=CARTESIAN_POINT('Ctrl Pts',(-3.46636045451847,-7.11689080592085,
78.991187772922));
#235458=CARTESIAN_POINT('Ctrl Pts',(-4.27564698419196,-6.68585520810151,
78.958048068381));
#235459=CARTESIAN_POINT('Ctrl Pts',(-4.79488337505931,-6.32383238140299,
78.9375323694199));
#235460=CARTESIAN_POINT('Ctrl Pts',(-5.46526740481459,-5.72593604239941,
78.9061854508312));
#235461=CARTESIAN_POINT('Ctrl Pts',(-5.65574917677674,-5.53786716356691,
78.896564437832));
#235462=CARTESIAN_POINT('Ctrl Pts',(-5.88727373553365,-5.28484861679749,
78.8833381906605));
#235463=CARTESIAN_POINT('Ctrl Pts',(-5.93742176319132,-5.22844518350846,
78.8803727788504));
#235464=CARTESIAN_POINT('Ctrl Pts',(-5.99299078540164,-5.16411400801576,
78.8769598301381));
#235465=CARTESIAN_POINT('Ctrl Pts',(-5.99921485851653,-5.15688211226937,
78.8765757217058));
#235466=CARTESIAN_POINT('Ctrl Pts',(-6.00859111333249,-5.14594767539056,
78.8759943171108));
#235467=CARTESIAN_POINT('Ctrl Pts',(-6.01175300872925,-5.14225343666563,
78.8757977775455));
#235468=CARTESIAN_POINT('Ctrl Pts',(-6.01720492091928,-5.13587172799162,
78.8754580741461));
#235469=CARTESIAN_POINT('Ctrl Pts',(-6.01949655169882,-5.13318563182078,
78.8753150343466));
#235470=CARTESIAN_POINT('Ctrl Pts',(-6.02423033276859,-5.12762948145548,
78.8750190429693));
#235471=CARTESIAN_POINT('Ctrl Pts',(-6.02667223140632,-5.12475921545978,
78.8748660723277));
#235472=CARTESIAN_POINT('Ctrl Pts',(-6.03328149009823,-5.11697927815517,
78.874451271254));
#235473=CARTESIAN_POINT('Ctrl Pts',(-6.03744489983618,-5.11206627038428,
78.8741891426256));
#235474=CARTESIAN_POINT('Ctrl Pts',(-6.05291506732474,-5.09376552880462,
78.873212062682));
#235475=CARTESIAN_POINT('Ctrl Pts',(-6.06418325770431,-5.08034540977162,
78.8724942438912));
#235476=CARTESIAN_POINT('Ctrl Pts',(-6.25581268021518,-4.85057386957689,
78.8601834129765));
#235477=CARTESIAN_POINT('Ctrl Pts',(-6.42452196940388,-4.62479710659329,
78.8477772305291));
#235478=CARTESIAN_POINT('Ctrl Pts',(-6.91605885169952,-3.88804887516201,
78.8075644717317));
#235479=CARTESIAN_POINT('Ctrl Pts',(-7.19265416543083,-3.34881960892385,
78.7786731520798));
#235480=CARTESIAN_POINT('Ctrl Pts',(-7.51847192423664,-2.48196618427648,
78.7367703242711));
#235481=CARTESIAN_POINT('Ctrl Pts',(-7.61325003217029,-2.17394363535585,
78.7226463554586));
#235482=CARTESIAN_POINT('Ctrl Pts',(-7.7197734472994,-1.73382083693689,
78.7036368541788));
#235483=CARTESIAN_POINT('Ctrl Pts',(-7.74739104815025,-1.60591746136991,
78.6982454112363));
#235484=CARTESIAN_POINT('Ctrl Pts',(-7.77516574206615,-1.45980778080906,
78.6922314416077));
#235485=CARTESIAN_POINT('Ctrl Pts',(-7.7784472043781,-1.44222056831505,
78.6915099033989));
#235486=CARTESIAN_POINT('Ctrl Pts',(-7.78329611464803,-1.41573452026112,
78.6904268021478));
#235487=CARTESIAN_POINT('Ctrl Pts',(-7.78490801280894,-1.40684394051464,
78.690063833907));
#235488=CARTESIAN_POINT('Ctrl Pts',(-7.78765758572965,-1.39152897701073,
78.6894396050717));
#235489=CARTESIAN_POINT('Ctrl Pts',(-7.78880254938341,-1.38510592136462,
78.6891781145601));
#235490=CARTESIAN_POINT('Ctrl Pts',(-7.79114732821199,-1.37185725872576,
78.6886393808551));
#235491=CARTESIAN_POINT('Ctrl Pts',(-7.79234612276966,-1.36503147636626,
78.6883621700734));
#235492=CARTESIAN_POINT('Ctrl Pts',(-7.79521555091207,-1.34856635811974,
78.6876943186785));
#235493=CARTESIAN_POINT('Ctrl Pts',(-7.79687727840027,-1.33892546988532,
78.687303958776));
#235494=CARTESIAN_POINT('Ctrl Pts',(-7.80291825239022,-1.3034847726411,
78.6858714832853));
#235495=CARTESIAN_POINT('Ctrl Pts',(-7.8071873819504,-1.27766623398238,
78.6848328300586));
#235496=CARTESIAN_POINT('Ctrl Pts',(-7.87778852099861,-0.837119134097701,
78.6671922038647));
#235497=CARTESIAN_POINT('Ctrl Pts',(-7.911121397185,-0.417763042855495,
78.6516890751607));
#235498=CARTESIAN_POINT('Ctrl Pts',(-7.9107657971752,0.80931778776061,78.6081113855084));
#235499=CARTESIAN_POINT('Ctrl Pts',(-7.78704841551942,1.6115456588928,78.5820400313291));
#235500=CARTESIAN_POINT('Ctrl Pts',(-7.53082472263949,2.42333607253993,
78.5484743041727));
#235501=CARTESIAN_POINT('Ctrl Pts',(-7.51715341849031,2.46541743113994,
78.5467151783887));
#235502=CARTESIAN_POINT('Ctrl Pts',(-7.499029366238,2.51965214900101,78.5444248247676));
#235503=CARTESIAN_POINT('Ctrl Pts',(-7.49489865287078,2.53191282799997,
78.5439055131511));
#235504=CARTESIAN_POINT('Ctrl Pts',(-7.48828552227743,2.5513837591298,78.5430784072745));
#235505=CARTESIAN_POINT('Ctrl Pts',(-7.48582271498667,2.55860067787781,
78.5427713151707));
#235506=CARTESIAN_POINT('Ctrl Pts',(-7.48119017256368,2.57211176395077,
78.5421954243522));
#235507=CARTESIAN_POINT('Ctrl Pts',(-7.47902291793581,2.5784067788096,78.5419267128522));
#235508=CARTESIAN_POINT('Ctrl Pts',(-7.47412353219476,2.59257940028668,
78.5413208529498));
#235509=CARTESIAN_POINT('Ctrl Pts',(-7.4713868901299,2.60045543294256,78.5409835491894));
#235510=CARTESIAN_POINT('Ctrl Pts',(-7.46328682472605,2.62364901726336,
78.5399884594607));
#235511=CARTESIAN_POINT('Ctrl Pts',(-7.45788872603031,2.63895436488957,
78.5393295047075));
#235512=CARTESIAN_POINT('Ctrl Pts',(-7.41555206744036,2.75782500631194,
78.5341942217659));
#235513=CARTESIAN_POINT('Ctrl Pts',(-7.37650576635252,2.86062455612321,
78.5296503343627));
#235514=CARTESIAN_POINT('Ctrl Pts',(-7.22611765951461,3.23298532077706,
78.5128748958965));
#235515=CARTESIAN_POINT('Ctrl Pts',(-7.10203775847234,3.49714497454862,
78.5003688941416));
#235516=CARTESIAN_POINT('Ctrl Pts',(-6.8402469213909,3.98278658660264,78.4766408397171));
#235517=CARTESIAN_POINT('Ctrl Pts',(-6.70561605141231,4.20550622628523,
78.4654390629343));
#235518=CARTESIAN_POINT('Ctrl Pts',(-6.29207492979483,4.81912761399631,
78.4338346590945));
#235519=CARTESIAN_POINT('Ctrl Pts',(-5.98823420232389,5.19184709871647,
78.4137858705275));
#235520=CARTESIAN_POINT('Ctrl Pts',(-5.46609483454463,5.72509420642991,
78.3830335675215));
#235521=CARTESIAN_POINT('Ctrl Pts',(-5.27020516023182,5.90591560128893,
78.3721171287573));
#235522=CARTESIAN_POINT('Ctrl Pts',(-5.0347744450086,6.10217781708426,78.3597096312445));
#235523=CARTESIAN_POINT('Ctrl Pts',(-5.00378990464858,6.12761082591003,
78.3580900394602));
#235524=CARTESIAN_POINT('Ctrl Pts',(-4.95292916997448,6.16871576432185,
78.3554530592206));
#235525=CARTESIAN_POINT('Ctrl Pts',(-4.93316876673269,6.18452968850247,
78.3544337749786));
#235526=CARTESIAN_POINT('Ctrl Pts',(-4.89766319142676,6.21266577136493,
78.3526116238218));
#235527=CARTESIAN_POINT('Ctrl Pts',(-4.88194656594312,6.22502357049801,
78.3518082751982));
#235528=CARTESIAN_POINT('Ctrl Pts',(-4.84851235110195,6.25110800612759,
78.3501061071544));
#235529=CARTESIAN_POINT('Ctrl Pts',(-4.83078292597097,6.26481920321393,
78.3492075066009));
#235530=CARTESIAN_POINT('Ctrl Pts',(-4.78314784508848,6.30133573965823,
78.3468038436816));
#235531=CARTESIAN_POINT('Ctrl Pts',(-4.75313737576229,6.32400351967549,
78.3453007116829));
#235532=CARTESIAN_POINT('Ctrl Pts',(-4.60424474404896,6.43480785322636,
78.3378974764269));
#235533=CARTESIAN_POINT('Ctrl Pts',(-4.48306613196376,6.5198114146002,78.3320424486548));
#235534=CARTESIAN_POINT('Ctrl Pts',(-4.13228734119325,6.75146734349418,
78.3155318469041));
#235535=CARTESIAN_POINT('Ctrl Pts',(-3.89739906897396,6.8897310964753,78.3049938746325));
#235536=CARTESIAN_POINT('Ctrl Pts',(-3.23618606759972,7.23429034581969,
78.2762950372691));
#235537=CARTESIAN_POINT('Ctrl Pts',(-2.79776825957793,7.41487130966066,
78.2583349141204));
#235538=CARTESIAN_POINT('Ctrl Pts',(-2.30838193095897,7.56682459580615,
78.2379294587511));
#235539=CARTESIAN_POINT('Ctrl Pts',(-2.27081093874057,7.57818442915298,
78.2363603435014));
#235540=CARTESIAN_POINT('Ctrl Pts',(-2.22027471909584,7.59305482003728,
78.2342450520417));
#235541=CARTESIAN_POINT('Ctrl Pts',(-2.20738264520811,7.59681269896384,
78.2337050130071));
#235542=CARTESIAN_POINT('Ctrl Pts',(-2.18521852349263,7.60321208123391,
78.232775891817));
#235543=CARTESIAN_POINT('Ctrl Pts',(-2.17595107506911,7.60586950097858,
78.2323871958483));
#235544=CARTESIAN_POINT('Ctrl Pts',(-2.15685052196758,7.61130877408096,
78.2315856766973));
#235545=CARTESIAN_POINT('Ctrl Pts',(-2.14701683936376,7.61408852846327,
78.2311728051457));
#235546=CARTESIAN_POINT('Ctrl Pts',(-2.12417473523376,7.62049769278045,
78.2302132836744));
#235547=CARTESIAN_POINT('Ctrl Pts',(-2.1111623622684,7.62411285790008,78.2296663117233));
#235548=CARTESIAN_POINT('Ctrl Pts',(-2.06981910273436,7.6354850987078,78.2279273727684));
#235549=CARTESIAN_POINT('Ctrl Pts',(-2.04145433828004,7.64311768715359,
78.2267327072821));
#235550=CARTESIAN_POINT('Ctrl Pts',(-1.73442159322066,7.72390510879834,
78.213786200451));
#235551=CARTESIAN_POINT('Ctrl Pts',(-1.45200411177264,7.78194096436413,
78.2017515388553));
#235552=CARTESIAN_POINT('Ctrl Pts',(-0.605069694275399,7.90826592748787,
78.1658190384286));
#235553=CARTESIAN_POINT('Ctrl Pts',(-0.0356587227971045,7.93130212082995,
78.1419641412425));
#235554=CARTESIAN_POINT('Ctrl Pts',(0.616461942412507,7.88740643699264,
78.1153283554771));
#235555=CARTESIAN_POINT('Ctrl Pts',(0.701521487471995,7.88029653188009,
78.1118647858669));
#235556=CARTESIAN_POINT('Ctrl Pts',(0.818403494797568,7.86861918915918,
78.1071174435052));
#235557=CARTESIAN_POINT('Ctrl Pts',(0.850337445200649,7.86523225747011,
78.1058216273433));
#235558=CARTESIAN_POINT('Ctrl Pts',(0.905114269513804,7.8590850942827,78.1036007797293));
#235559=CARTESIAN_POINT('Ctrl Pts',(0.927967309322415,7.85641947942028,
78.1026748004428));
#235560=CARTESIAN_POINT('Ctrl Pts',(0.975057181542259,7.85071850932886,
78.1007678267073));
#235561=CARTESIAN_POINT('Ctrl Pts',(0.99929224543791,7.84767052268173,78.0997869689415));
#235562=CARTESIAN_POINT('Ctrl Pts',(1.05578587534189,7.84029951371488,78.0975017076958));
#235563=CARTESIAN_POINT('Ctrl Pts',(1.08803268423936,7.83588955813799,78.0961981751708));
#235564=CARTESIAN_POINT('Ctrl Pts',(1.19297609672135,7.82087758083035,78.0919583618356));
#235565=CARTESIAN_POINT('Ctrl Pts',(1.26555265697937,7.80946186874416,78.0890299493468));
#235566=CARTESIAN_POINT('Ctrl Pts',(1.96005892667254,7.69028561773148,78.0610211727918));
#235567=CARTESIAN_POINT('Ctrl Pts',(2.56719061568457,7.50945698518855,78.0365610937451));
#235568=CARTESIAN_POINT('Ctrl Pts',(3.75430902966473,6.99486333160442,77.9880309348258));
#235569=CARTESIAN_POINT('Ctrl Pts',(4.3266598225274,6.65603450387533,77.9643123682345));
#235570=CARTESIAN_POINT('Ctrl Pts',(4.85716263129601,6.24435535651387,77.937716232328));
#235571=CARTESIAN_POINT('Ctrl Pts',(4.86429161791076,6.23880354719328,77.9373578472209));
#235572=CARTESIAN_POINT('Ctrl Pts',(4.89394142995364,6.21563157999836,77.935863148741));
#235573=CARTESIAN_POINT('Ctrl Pts',(4.91637599876954,6.19790171527143,77.9347221742175));
#235574=CARTESIAN_POINT('Ctrl Pts',(4.94652685155057,6.17380702120838,77.9331745442123));
#235575=CARTESIAN_POINT('Ctrl Pts',(4.95432805678311,6.16754850267817,77.9327728171101));
#235576=CARTESIAN_POINT('Ctrl Pts',(4.96714959248495,6.15722239932323,77.9321103966097));
#235577=CARTESIAN_POINT('Ctrl Pts',(4.97217685776037,6.15316341760033,77.9318501137829));
#235578=CARTESIAN_POINT('Ctrl Pts',(4.98173259231435,6.14542882115636,77.9313543130794));
#235579=CARTESIAN_POINT('Ctrl Pts',(4.98626198224929,6.14175434720168,77.9311188506904));
#235580=CARTESIAN_POINT('Ctrl Pts',(4.99687068215286,6.13312855396817,77.9305662767521));
#235581=CARTESIAN_POINT('Ctrl Pts',(5.00294669666433,6.12817320442411,77.9302489660994));
#235582=CARTESIAN_POINT('Ctrl Pts',(5.02155863991474,6.11294793426166,77.9292744052347));
#235583=CARTESIAN_POINT('Ctrl Pts',(5.03407033909408,6.10264855918488,77.9286156674493));
#235584=CARTESIAN_POINT('Ctrl Pts',(5.18986049198327,5.97360018148361,77.9203671823294));
#235585=CARTESIAN_POINT('Ctrl Pts',(5.32891286915862,5.84989086019136,77.9124805312862));
#235586=CARTESIAN_POINT('Ctrl Pts',(5.54037521264345,5.64796173067632,77.8997081696442));
#235587=CARTESIAN_POINT('Ctrl Pts',(5.61579207381601,5.57298012158283,77.8949908963749));
#235588=CARTESIAN_POINT('Ctrl Pts',(6.3783837759318,4.78358785604404,77.8457688143051));
#235589=CARTESIAN_POINT('Ctrl Pts',(6.92722129838556,3.94727381964114,77.7985246399713));
#235590=CARTESIAN_POINT('Ctrl Pts',(7.32769944034608,2.98187889484434,77.7556581509835));
#235591=CARTESIAN_POINT('Ctrl Pts',(7.34768933672887,2.93227597320367,77.7534809687233));
#235592=CARTESIAN_POINT('Ctrl Pts',(7.37252596337561,2.86879723817412,77.7507264683992));
#235593=CARTESIAN_POINT('Ctrl Pts',(7.37783886699982,2.85510601026992,77.7501342403285));
#235594=CARTESIAN_POINT('Ctrl Pts',(7.38621557058701,2.833339925244,77.7491956752947));
#235595=CARTESIAN_POINT('Ctrl Pts',(7.38930431330969,2.82527473939298,77.748848541775));
#235596=CARTESIAN_POINT('Ctrl Pts',(7.39503798290656,2.8102295186254,77.74820217218));
#235597=CARTESIAN_POINT('Ctrl Pts',(7.39768624846209,2.80325077110061,77.747902829809));
#235598=CARTESIAN_POINT('Ctrl Pts',(7.40354210686122,2.7877532404858,77.7472391429869));
#235599=CARTESIAN_POINT('Ctrl Pts',(7.40674488397886,2.77923264269852,77.7468749523237));
#235600=CARTESIAN_POINT('Ctrl Pts',(7.41596365377168,2.75457811302087,77.7458231936916));
#235601=CARTESIAN_POINT('Ctrl Pts',(7.42194170262774,2.73842999950355,77.7451368339324));
#235602=CARTESIAN_POINT('Ctrl Pts',(7.46232174785929,2.62825046578179,77.7404707599168));
#235603=CARTESIAN_POINT('Ctrl Pts',(7.49498925943941,2.53359097958229,77.7365463514109));
#235604=CARTESIAN_POINT('Ctrl Pts',(7.57260763905175,2.29402402573444,77.726812988313));
#235605=CARTESIAN_POINT('Ctrl Pts',(7.61520423068091,2.14839472556766,77.7210768150218));
#235606=CARTESIAN_POINT('Ctrl Pts',(7.75536601047227,1.61246018307754,77.7005290190709));
#235607=CARTESIAN_POINT('Ctrl Pts',(7.8273168071756,1.21608559964228,77.686436597197));
#235608=CARTESIAN_POINT('Ctrl Pts',(7.90472703122433,0.469559889352466,
77.6604627762765));
#235609=CARTESIAN_POINT('Ctrl Pts',(7.91773313791556,0.121186773139081,
77.6485554836024));
#235610=CARTESIAN_POINT('Ctrl Pts',(7.90243346081503,-0.412028849165187,
77.6295378106966));
#235611=CARTESIAN_POINT('Ctrl Pts',(7.89062212084517,-0.596908325641212,
77.6227942936502));
#235612=CARTESIAN_POINT('Ctrl Pts',(7.85929075439808,-0.91264384301077,
77.6108087508214));
#235613=CARTESIAN_POINT('Ctrl Pts',(7.84295670697803,-1.04374330969894,
77.6056902902278));
#235614=CARTESIAN_POINT('Ctrl Pts',(7.82123619263469,-1.18843918424695,
77.5998393713379));
#235615=CARTESIAN_POINT('Ctrl Pts',(7.8190869927813,-1.20249817920185,77.5992688801238));
#235616=CARTESIAN_POINT('Ctrl Pts',(7.81597399459382,-1.22250062100783,
77.5984544373));
#235617=CARTESIAN_POINT('Ctrl Pts',(7.81504129596696,-1.2284489385268,77.5982118889174));
#235618=CARTESIAN_POINT('Ctrl Pts',(7.81329442963293,-1.2395071317363,77.5977603373753));
#235619=CARTESIAN_POINT('Ctrl Pts',(7.81248203709536,-1.24461728801893,
77.5975514131976));
#235620=CARTESIAN_POINT('Ctrl Pts',(7.81090337322782,-1.25448504018068,
77.5971474903222));
#235621=CARTESIAN_POINT('Ctrl Pts',(7.81013776701363,-1.25924274151509,
77.5969525208757));
#235622=CARTESIAN_POINT('Ctrl Pts',(7.80819330922427,-1.27125618240845,
77.5964596636944));
#235623=CARTESIAN_POINT('Ctrl Pts',(7.80700869243913,-1.27851097421516,
77.5961615261888));
#235624=CARTESIAN_POINT('Ctrl Pts',(7.80293571402801,-1.30323783670821,
77.5951436676677));
#235625=CARTESIAN_POINT('Ctrl Pts',(7.79999880958345,-1.32070177547351,
77.5944218827913));
#235626=CARTESIAN_POINT('Ctrl Pts',(7.7928480186949,-1.36236713931284,77.5926931657397));
#235627=CARTESIAN_POINT('Ctrl Pts',(7.78858000921853,-1.38655900952019,
77.5916840397113));
#235628=CARTESIAN_POINT('Ctrl Pts',(7.73414629470008,-1.68691610221818,
77.5790912538922));
#235629=CARTESIAN_POINT('Ctrl Pts',(7.66943194442527,-1.96023048788132,
77.5669693061806));
#235630=CARTESIAN_POINT('Ctrl Pts',(7.43972373944825,-2.74226805759188,
77.5313010349159));
#235631=CARTESIAN_POINT('Ctrl Pts',(7.23752780369644,-3.23848376741513,
77.5075350869696));
#235632=CARTESIAN_POINT('Ctrl Pts',(6.8508420050389,-3.96660545301836,77.4724651936643));
#235633=CARTESIAN_POINT('Ctrl Pts',(6.70086303092373,-4.21502598328224,
77.4604301065471));
#235634=CARTESIAN_POINT('Ctrl Pts',(6.51751906717591,-4.48409800608915,
77.4472500496257));
#235635=CARTESIAN_POINT('Ctrl Pts',(6.49726339263907,-4.51339762827026,
77.4458126449998));
#235636=CARTESIAN_POINT('Ctrl Pts',(6.46731197051676,-4.55610255684141,
77.4437139447329));
#235637=CARTESIAN_POINT('Ctrl Pts',(6.45777103912562,-4.56961572138255,
77.4430493106526));
#235638=CARTESIAN_POINT('Ctrl Pts',(6.44076050364316,-4.59354868235458,
77.4418711736407));
#235639=CARTESIAN_POINT('Ctrl Pts',(6.4333078312704,-4.60398042042706,77.4413573113864));
#235640=CARTESIAN_POINT('Ctrl Pts',(6.41774058016381,-4.62565878298052,
77.4402886988107));
#235641=CARTESIAN_POINT('Ctrl Pts',(6.4096217176148,-4.63690228162128,77.4397340414066));
#235642=CARTESIAN_POINT('Ctrl Pts',(6.3885066861093,-4.66598225008422,77.4382983443235));
#235643=CARTESIAN_POINT('Ctrl Pts',(6.37546535135251,-4.6837858187223,77.4374182527858));
#235644=CARTESIAN_POINT('Ctrl Pts',(6.32151530668096,-4.75679369269768,
77.4338042765838));
#235645=CARTESIAN_POINT('Ctrl Pts',(6.27996224929837,-4.81151913011076,
77.4310833767849));
#235646=CARTESIAN_POINT('Ctrl Pts',(6.01025098885638,-5.15728221383457,
77.4138110050535));
#235647=CARTESIAN_POINT('Ctrl Pts',(5.76262969289628,-5.43256809781041,
77.3997148571322));
#235648=CARTESIAN_POINT('Ctrl Pts',(5.04355695442311,-6.1272632909503,77.3623997314067));
#235649=CARTESIAN_POINT('Ctrl Pts',(4.53982978152938,-6.50927652500992,
77.339990075988));
#235650=CARTESIAN_POINT('Ctrl Pts',(3.89154994654811,-6.88871952010248,
77.3110870268858));
#235651=CARTESIAN_POINT('Ctrl Pts',(3.78553334723148,-6.94754296678254,
77.3063520837916));
#235652=CARTESIAN_POINT('Ctrl Pts',(3.65627492423814,-7.01542504296894,
77.3005302852983));
#235653=CARTESIAN_POINT('Ctrl Pts',(3.63428586580618,-7.02684147280587,
77.2995382200967));
#235654=CARTESIAN_POINT('Ctrl Pts',(3.60403485241907,-7.04236742279755,
77.2981707185742));
#235655=CARTESIAN_POINT('Ctrl Pts',(3.59581866938999,-7.04656613047035,
77.2977990338594));
#235656=CARTESIAN_POINT('Ctrl Pts',(3.58290827693169,-7.05313525557956,
77.2972145437632));
#235657=CARTESIAN_POINT('Ctrl Pts',(3.5782190027728,-7.05551539027658,77.2970021543736));
#235658=CARTESIAN_POINT('Ctrl Pts',(3.56843965912522,-7.0604668344007,77.2965590238204));
#235659=CARTESIAN_POINT('Ctrl Pts',(3.56334917687087,-7.06303731860187,
77.2963282471859));
#235660=CARTESIAN_POINT('Ctrl Pts',(3.55169673038865,-7.06890552134831,
77.295799720181));
#235661=CARTESIAN_POINT('Ctrl Pts',(3.5451329504574,-7.07219960814905,77.295501811451));
#235662=CARTESIAN_POINT('Ctrl Pts',(3.52554709553433,-7.08199481194364,
77.2946122801777));
#235663=CARTESIAN_POINT('Ctrl Pts',(3.51251170045875,-7.08846911466292,
77.2940194711463));
#235664=CARTESIAN_POINT('Ctrl Pts',(3.40090217233104,-7.14351887065642,
77.2889366581301));
#235665=CARTESIAN_POINT('Ctrl Pts',(3.30135504972178,-7.1900661783184,77.2843516872889));
#235666=CARTESIAN_POINT('Ctrl Pts',(3.11084011433444,-7.27435805145224,
77.2754578721429));
#235667=CARTESIAN_POINT('Ctrl Pts',(3.02008551882568,-7.31250255167785,
77.2711771876931));
#235668=CARTESIAN_POINT('Ctrl Pts',(2.7452032725329,-7.4220465724783,77.2581308631111));
#235669=CARTESIAN_POINT('Ctrl Pts',(2.55909403969478,-7.4882540376892,77.2491918114139));
#235670=CARTESIAN_POINT('Ctrl Pts',(1.82925535387079,-7.71750251658468,
77.214206600622));
#235671=CARTESIAN_POINT('Ctrl Pts',(1.27100822792951,-7.82883558825758,
77.1877376174386));
#235672=CARTESIAN_POINT('Ctrl Pts',(0.430699374555759,-7.90408857817761,
77.1509129639977));
#235673=CARTESIAN_POINT('Ctrl Pts',(0.154646174034814,-7.91430497799267,
77.1392607489023));
#235674=CARTESIAN_POINT('Ctrl Pts',(-0.144142949810752,-7.90971942074254,
77.1271552551416));
#235675=CARTESIAN_POINT('Ctrl Pts',(-0.166887518147169,-7.90927222143669,
77.1262368631341));
#235676=CARTESIAN_POINT('Ctrl Pts',(-0.19861546211328,-7.90851147079419,
77.1249600396358));
#235677=CARTESIAN_POINT('Ctrl Pts',(-0.207600598885092,-7.90828070932663,
77.1245989335158));
#235678=CARTESIAN_POINT('Ctrl Pts',(-0.223116893656547,-7.90785574886825,
77.123976173667));
#235679=CARTESIAN_POINT('Ctrl Pts',(-0.229648231400032,-7.90766877045632,
77.1237142864249));
#235680=CARTESIAN_POINT('Ctrl Pts',(-0.24316595350552,-7.90726502498545,
77.1231727894401));
#235681=CARTESIAN_POINT('Ctrl Pts',(-0.250152299030421,-7.90704709002894,
77.1228932177665));
#235682=CARTESIAN_POINT('Ctrl Pts',(-0.266477462127926,-7.90651617801907,
77.1222406102038));
#235683=CARTESIAN_POINT('Ctrl Pts',(-0.275816041442402,-7.90619591353404,
77.1218678109886));
#235684=CARTESIAN_POINT('Ctrl Pts',(-0.305820475653556,-7.90511369262563,
77.1206716738303));
#235685=CARTESIAN_POINT('Ctrl Pts',(-0.326483998381034,-7.90428724579868,
77.1198504308232));
#235686=CARTESIAN_POINT('Ctrl Pts',(-0.763086382203918,-7.88511013841454,
77.1025508603036));
#235687=CARTESIAN_POINT('Ctrl Pts',(-1.17695459106484,-7.83403434255653,
77.0872118346868));
#235688=CARTESIAN_POINT('Ctrl Pts',(-1.68121039943816,-7.73091923439417,
77.069161214131));
#235689=CARTESIAN_POINT('Ctrl Pts',(-1.77712688897886,-7.70943584865565,
77.0657542522054));
#235690=CARTESIAN_POINT('Ctrl Pts',(-1.95474462927927,-7.66616196928083,
77.0594723494524));
#235691=CARTESIAN_POINT('Ctrl Pts',(-2.03654452042719,-7.64483829336407,
77.0565900791355));
#235692=CARTESIAN_POINT('Ctrl Pts',(-2.18518747594735,-7.60353478318354,
77.051356486278));
#235693=CARTESIAN_POINT('Ctrl Pts',(-2.25213774819018,-7.58397396754472,
77.0490006799641));
#235694=CARTESIAN_POINT('Ctrl Pts',(-2.37554030182798,-7.54614131523068,
77.0446513062508));
#235695=CARTESIAN_POINT('Ctrl Pts',(-2.43206244761335,-7.52811482018747,
77.0426563428677));
#235696=CARTESIAN_POINT('Ctrl Pts',(-2.5372073317395,-7.49327339825308,
77.0389334112788));
#235697=CARTESIAN_POINT('Ctrl Pts',(-2.58587911634988,-7.47661664517903,
77.0372052789929));
#235698=CARTESIAN_POINT('Ctrl Pts',(-2.67701312719155,-7.44443184642277,
77.0339559704908));
#235699=CARTESIAN_POINT('Ctrl Pts',(-2.71951140998211,-7.42901221425867,
77.0324351507376));
#235700=CARTESIAN_POINT('Ctrl Pts',(-2.90857263975468,-7.35857549968119,
77.0256369752713));
#235701=CARTESIAN_POINT('Ctrl Pts',(-3.05361358118064,-7.2995801864152,
77.0203345320018));
#235702=CARTESIAN_POINT('Ctrl Pts',(-3.46098547768449,-7.11961457491311,
77.0049763286912));
#235703=CARTESIAN_POINT('Ctrl Pts',(-3.71855780394466,-6.9885360624109,
76.9947038083995));
#235704=CARTESIAN_POINT('Ctrl Pts',(-4.0434594698607,-6.80013906846717,
76.9803157999025));
#235705=CARTESIAN_POINT('Ctrl Pts',(-4.11782739016114,-6.75536471025688,
76.9769197222449));
#235706=CARTESIAN_POINT('Ctrl Pts',(-4.20068641771042,-6.70360152903413,
76.9730025614776));
#235707=CARTESIAN_POINT('Ctrl Pts',(-4.20991996119274,-6.69780663784926,
76.9725641580478));
#235708=CARTESIAN_POINT('Ctrl Pts',(-4.22331485818136,-6.68936147546022,
76.9719253881815));
#235709=CARTESIAN_POINT('Ctrl Pts',(-4.22748579266486,-6.68672634502883,
76.9717260929184));
#235710=CARTESIAN_POINT('Ctrl Pts',(-4.23483171764353,-6.68207568546012,
76.9713743917217));
#235711=CARTESIAN_POINT('Ctrl Pts',(-4.23800774498987,-6.68006178835826,
76.971222102372));
#235712=CARTESIAN_POINT('Ctrl Pts',(-4.24410476732026,-6.6761896100594,
76.970929307124));
#235713=CARTESIAN_POINT('Ctrl Pts',(-4.24702598169726,-6.67433167412037,
76.9707888260713));
#235714=CARTESIAN_POINT('Ctrl Pts',(-4.25324772295441,-6.67036881524532,
76.9704892018728));
#235715=CARTESIAN_POINT('Ctrl Pts',(-4.25654789250817,-6.66826336933369,
76.9703300204901));
#235716=CARTESIAN_POINT('Ctrl Pts',(-4.26913289940549,-6.66022122303928,
76.9697220274329));
#235717=CARTESIAN_POINT('Ctrl Pts',(-4.27840684348422,-6.65426760295549,
76.969271992865));
#235718=CARTESIAN_POINT('Ctrl Pts',(-4.3001165353017,-6.64026642497335,
76.9682138578564));
#235719=CARTESIAN_POINT('Ctrl Pts',(-4.31254214509926,-6.63220330302189,
76.9676046549331));
#235720=CARTESIAN_POINT('Ctrl Pts',(-4.35530968798281,-6.60427994463422,
76.9654957263624));
#235721=CARTESIAN_POINT('Ctrl Pts',(-4.38553727003681,-6.58424626172705,
76.9639840542439));
#235722=CARTESIAN_POINT('Ctrl Pts',(-4.51833140011995,-6.49491526874732,
76.9572538114778));
#235723=CARTESIAN_POINT('Ctrl Pts',(-4.61939701760682,-6.42342676278368,
76.9518950872519));
#235724=CARTESIAN_POINT('Ctrl Pts',(-4.87761245171966,-6.2315325976487,
76.9376770125713));
#235725=CARTESIAN_POINT('Ctrl Pts',(-5.03199220126173,-6.10754855743923,
76.9286502255891));
#235726=CARTESIAN_POINT('Ctrl Pts',(-5.83964539130386,-5.40748851329033,
76.8792491002531));
#235727=CARTESIAN_POINT('Ctrl Pts',(-6.39925362171106,-4.73209035673655,
76.8379236073619));
#235728=CARTESIAN_POINT('Ctrl Pts',(-6.8654387019972,-3.93099949669461,
76.7999503332903));
#235729=CARTESIAN_POINT('Ctrl Pts',(-6.89286745075898,-3.8827031946666,
76.7976946304945));
#235730=CARTESIAN_POINT('Ctrl Pts',(-6.92586940484383,-3.8231415816002,
76.7949532412712));
#235731=CARTESIAN_POINT('Ctrl Pts',(-6.93192695229304,-3.812147333986,76.7944488939623));
#235732=CARTESIAN_POINT('Ctrl Pts',(-6.94189496342214,-3.79395340536654,
76.7936170244948));
#235733=CARTESIAN_POINT('Ctrl Pts',(-6.94582044419765,-3.78676200503892,
76.793288925647));
#235734=CARTESIAN_POINT('Ctrl Pts',(-6.95288917055197,-3.77376427126368,
76.7926971957264));
#235735=CARTESIAN_POINT('Ctrl Pts',(-6.95603632939854,-3.76796008171878,
76.7924334147918));
#235736=CARTESIAN_POINT('Ctrl Pts',(-6.962748624193,-3.75554377239112,76.7918701122475));
#235737=CARTESIAN_POINT('Ctrl Pts',(-6.96631161743391,-3.74893049805985,
76.7915706727517));
#235738=CARTESIAN_POINT('Ctrl Pts',(-6.97591714162689,-3.73104069995804,
76.7907622410929));
#235739=CARTESIAN_POINT('Ctrl Pts',(-6.98194175947876,-3.71975455385849,
76.7902539329127));
#235740=CARTESIAN_POINT('Ctrl Pts',(-7.01148694758599,-3.66408176330713,
76.7877548877017));
#235741=CARTESIAN_POINT('Ctrl Pts',(-7.03461201682153,-3.61948591418087,
76.7857792028819));
#235742=CARTESIAN_POINT('Ctrl Pts',(-7.22313578221371,-3.24729211351989,
76.7695012767698));
#235743=CARTESIAN_POINT('Ctrl Pts',(-7.36598791958262,-2.90875467002388,
76.7560765859012));
#235744=CARTESIAN_POINT('Ctrl Pts',(-7.73503805004267,-1.8303709722937,
76.7160351704568));
#235745=CARTESIAN_POINT('Ctrl Pts',(-7.87673204921938,-1.06667459132602,
76.6917928232895));
#235746=CARTESIAN_POINT('Ctrl Pts',(-7.90668256405158,-0.26321844054238,
76.6609546739394));
#235747=CARTESIAN_POINT('Ctrl Pts',(-7.90766789019368,-0.231736072585083,
76.6597372276119));
#235748=CARTESIAN_POINT('Ctrl Pts',(-7.90985546229389,-0.145341961306333,
76.6563692697658));
#235749=CARTESIAN_POINT('Ctrl Pts',(-7.91067387089617,-0.0904231612133168,
76.6541983792898));
#235750=CARTESIAN_POINT('Ctrl Pts',(-7.91096236434687,-0.0261373439966448,
76.6516174170969));
#235751=CARTESIAN_POINT('Ctrl Pts',(-7.91098776064491,-0.0167731570304957,
76.6512404679346));
#235752=CARTESIAN_POINT('Ctrl Pts',(-7.91100010611559,-0.00359118555788957,
76.650708449942));
#235753=CARTESIAN_POINT('Ctrl Pts',(-7.91100091797001,0.00022660524541699,
76.6505542023486));
#235754=CARTESIAN_POINT('Ctrl Pts',(-7.91099896618133,0.00404438844160049,
76.6503997926682));
#235755=CARTESIAN_POINT('',(-7.90827614865568,-0.00626907122509836,74.6423315082369));
#235756=CARTESIAN_POINT('Ctrl Pts',(-7.92502143214218,0.00372523665453262,
76.642331508237));
#235757=CARTESIAN_POINT('Ctrl Pts',(-7.9241870030526,2.61244749534328,76.5367896921557));
#235758=CARTESIAN_POINT('Ctrl Pts',(-5.79219513848909,6.51283346952887,
76.378263087466));
#235759=CARTESIAN_POINT('Ctrl Pts',(-0.626326385655128,8.21169917704909,
76.1667516941681));
#235760=CARTESIAN_POINT('Ctrl Pts',(3.3870778892776,7.52640590708394,76.0077973283437));
#235761=CARTESIAN_POINT('Ctrl Pts',(6.55629850510655,4.98354837003805,75.8488429625187));
#235762=CARTESIAN_POINT('Ctrl Pts',(8.72532350098204,-0.030839795427598,
75.6369038080857));
#235763=CARTESIAN_POINT('Ctrl Pts',(6.69212697694097,-5.60207094650804,
75.4249646536528));
#235764=CARTESIAN_POINT('Ctrl Pts',(1.80805205364573,-8.025049431192,75.2130254992196));
#235765=CARTESIAN_POINT('Ctrl Pts',(-3.62141351739191,-7.93641147911786,
75.0010863447868));
#235766=CARTESIAN_POINT('Ctrl Pts',(-7.450008814502,-4.19522544625671,74.8108550144591));
#235767=CARTESIAN_POINT('Ctrl Pts',(-7.91343195938039,-0.787962566203169,
74.6736084727398));
#235768=CARTESIAN_POINT('Ctrl Pts',(-7.90689550057179,-0.00944669734432524,
74.6423315082369));
#235769=CARTESIAN_POINT('',(-7.90134992664127,0.00118378181009326,72.642331508237));
#235770=CARTESIAN_POINT('Ctrl Pts',(-7.911,1.34503519433338E-12,74.642331508237));
#235771=CARTESIAN_POINT('Ctrl Pts',(-7.91099999999962,2.20167589666814,
74.5537440725043));
#235772=CARTESIAN_POINT('Ctrl Pts',(-6.94214576672294,4.38610418338807,
74.4651566367715));
#235773=CARTESIAN_POINT('Ctrl Pts',(-3.67820201488151,7.34180684107701,
74.2879817653061));
#235774=CARTESIAN_POINT('Ctrl Pts',(-1.40868175871591,8.08992666571364,
74.1993943295733));
#235775=CARTESIAN_POINT('Ctrl Pts',(2.97309270521424,7.654542280252,74.0222194581079));
#235776=CARTESIAN_POINT('Ctrl Pts',(5.05102072675732,6.47444880834125,73.9336320223751));
#235777=CARTESIAN_POINT('Ctrl Pts',(7.66951518847933,2.93425195367549,73.7564571509097));
#235778=CARTESIAN_POINT('Ctrl Pts',(8.18956872247085,0.601881960097444,
73.667869715177));
#235779=CARTESIAN_POINT('Ctrl Pts',(7.32306689761263,-3.71537198232609,
73.4906948437115));
#235780=CARTESIAN_POINT('Ctrl Pts',(5.94329958850077,-5.66643518936643,
73.4021074079788));
#235781=CARTESIAN_POINT('Ctrl Pts',(2.16154501637667,-7.92205913233048,
73.2249325365133));
#235782=CARTESIAN_POINT('Ctrl Pts',(-0.210816529302271,-8.20894963712998,
73.1363451007806));
#235783=CARTESIAN_POINT('Ctrl Pts',(-4.42123908576603,-6.91982244717726,
72.9591702293152));
#235784=CARTESIAN_POINT('Ctrl Pts',(-6.22631625634318,-5.3539035880337,
72.8705827935824));
#235785=CARTESIAN_POINT('Ctrl Pts',(-7.65317280859534,-2.31334857514354,
72.7354407413121));
#235786=CARTESIAN_POINT('Ctrl Pts',(-7.91100000000017,-1.15702837836376,
72.6888861247746));
#235787=CARTESIAN_POINT('Ctrl Pts',(-7.911,1.17517107156573E-12,72.642331508237));
#235788=CARTESIAN_POINT('',(-7.921302937514,0.00357332256267995,70.6425359502471));
#235789=CARTESIAN_POINT('Ctrl Pts',(-7.89504541711033,0.00195716076996755,
72.642331508237));
#235790=CARTESIAN_POINT('Ctrl Pts',(-7.89841756211971,1.09499239008904,
72.5984880988909));
#235791=CARTESIAN_POINT('Ctrl Pts',(-7.4313217434443,3.50649690015027,72.5016599009365));
#235792=CARTESIAN_POINT('Ctrl Pts',(-5.03519156416044,6.50517613243061,
72.3518469143741));
#235793=CARTESIAN_POINT('Ctrl Pts',(-0.0564887115056478,8.72723159946603,
72.139907759941));
#235794=CARTESIAN_POINT('Ctrl Pts',(5.53353127081588,6.74627697064648,71.9279686055081));
#235795=CARTESIAN_POINT('Ctrl Pts',(8.01779672670277,1.88035637415614,71.7160294510749));
#235796=CARTESIAN_POINT('Ctrl Pts',(7.95963757450901,-2.18248761478921,
71.5570750852503));
#235797=CARTESIAN_POINT('Ctrl Pts',(5.9317470407567,-5.71302591978898,71.3981207194254));
#235798=CARTESIAN_POINT('Ctrl Pts',(1.32250398506214,-8.61939107734134,
71.1861815649926));
#235799=CARTESIAN_POINT('Ctrl Pts',(-5.61612825759075,-7.27095079450261,
70.9343199752662));
#235800=CARTESIAN_POINT('Ctrl Pts',(-7.90096779956093,-2.29930440440434,
70.7354431741484));
#235801=CARTESIAN_POINT('Ctrl Pts',(-7.921302937514,0.00357332256267995,
70.6425359502471));
#235802=CARTESIAN_POINT('',(-7.9109998986396,0.00126638231751385,66.6333051339456));
#235803=CARTESIAN_POINT('Ctrl Pts',(-7.91099908888364,0.00379679894604718,
70.6484690865411));
#235804=CARTESIAN_POINT('Ctrl Pts',(-7.91085111670076,0.312111202886401,
70.6376639763182));
#235805=CARTESIAN_POINT('Ctrl Pts',(-7.89267928218732,0.620131437501612,
70.6264055364096));
#235806=CARTESIAN_POINT('Ctrl Pts',(-7.85564523625669,0.934250163225403,
70.6137358191232));
#235807=CARTESIAN_POINT('Ctrl Pts',(-7.85469315267901,0.94222127003831,
70.6134135179521));
#235808=CARTESIAN_POINT('Ctrl Pts',(-7.85313376871219,0.955110237079679,
70.6128910660888));
#235809=CARTESIAN_POINT('Ctrl Pts',(-7.85253397562235,0.960029018171404,
70.6126913770645));
#235810=CARTESIAN_POINT('Ctrl Pts',(-7.85147662380977,0.968632858645214,
70.6123415421385));
#235811=CARTESIAN_POINT('Ctrl Pts',(-7.85102109270882,0.972318153061019,
70.6121915223589));
#235812=CARTESIAN_POINT('Ctrl Pts',(-7.85009695676984,0.979751517934062,
70.6118885756235));
#235813=CARTESIAN_POINT('Ctrl Pts',(-7.84962826330846,0.983499565505954,
70.6117356437699));
#235814=CARTESIAN_POINT('Ctrl Pts',(-7.84872081693304,0.990714261547698,
70.6114409170494));
#235815=CARTESIAN_POINT('Ctrl Pts',(-7.84828245104744,0.994180958727498,
70.6112991460335));
#235816=CARTESIAN_POINT('Ctrl Pts',(-7.84724280810808,1.00235915238736,
70.6109643378259));
#235817=CARTESIAN_POINT('Ctrl Pts',(-7.84663958513004,1.00707039507899,
70.6107711816911));
#235818=CARTESIAN_POINT('Ctrl Pts',(-7.84484102864902,1.02101761368873,
70.6101985312313));
#235819=CARTESIAN_POINT('Ctrl Pts',(-7.84363363211445,1.03025199631504,
70.6098183059978));
#235820=CARTESIAN_POINT('Ctrl Pts',(-7.83289144343958,1.1112966609469,70.6064719804277));
#235821=CARTESIAN_POINT('Ctrl Pts',(-7.82238731904701,1.18297278297795,
70.6034482681321));
#235822=CARTESIAN_POINT('Ctrl Pts',(-7.78662004678917,1.40567213821601,
70.5938754768716));
#235823=CARTESIAN_POINT('Ctrl Pts',(-7.75795657129801,1.55610757728357,
70.5871532256732));
#235824=CARTESIAN_POINT('Ctrl Pts',(-7.72306885283454,1.71411915122023,
70.5798893732315));
#235825=CARTESIAN_POINT('Ctrl Pts',(-7.7211756080123,1.72262712148943,70.5794976307331));
#235826=CARTESIAN_POINT('Ctrl Pts',(-7.70632924678631,1.78882834170141,
70.5764446503151));
#235827=CARTESIAN_POINT('Ctrl Pts',(-7.69274391390513,1.84637703676291,
70.5737623187859));
#235828=CARTESIAN_POINT('Ctrl Pts',(-7.67210176582676,1.92963356519597,
70.5698455637178));
#235829=CARTESIAN_POINT('Ctrl Pts',(-7.66555796445398,1.95546727875049,
70.5686251484955));
#235830=CARTESIAN_POINT('Ctrl Pts',(-7.50309063339445,2.58350894708661,
70.5388393957115));
#235831=CARTESIAN_POINT('Ctrl Pts',(-7.2768080497462,3.16529005472852,70.5088561641687));
#235832=CARTESIAN_POINT('Ctrl Pts',(-6.84381644008412,3.97945882441195,
70.4671975057645));
#235833=CARTESIAN_POINT('Ctrl Pts',(-6.68799608508582,4.23611270602389,
70.454075784752));
#235834=CARTESIAN_POINT('Ctrl Pts',(-6.44887509277901,4.58375298753841,
70.4363977074597));
#235835=CARTESIAN_POINT('Ctrl Pts',(-6.3774759807538,4.68258297951504,70.4313817155536));
#235836=CARTESIAN_POINT('Ctrl Pts',(-6.2935320512866,4.79329377436658,70.4257691237696));
#235837=CARTESIAN_POINT('Ctrl Pts',(-6.2832012834344,4.80682769866909,70.4250831122121));
#235838=CARTESIAN_POINT('Ctrl Pts',(-6.26756868077619,4.82717083824188,
70.4240520819537));
#235839=CARTESIAN_POINT('Ctrl Pts',(-6.26229929776086,4.83400485888472,
70.4237057423555));
#235840=CARTESIAN_POINT('Ctrl Pts',(-6.25319835101844,4.84576829432973,
70.4231096196414));
#235841=CARTESIAN_POINT('Ctrl Pts',(-6.24937212040819,4.85070181318161,
70.4228596192865));
#235842=CARTESIAN_POINT('Ctrl Pts',(-6.24146264280682,4.86087535418988,
70.4223441057653));
#235843=CARTESIAN_POINT('Ctrl Pts',(-6.23737862691588,4.86611477416117,
70.4220786243237));
#235844=CARTESIAN_POINT('Ctrl Pts',(-6.22632701103339,4.88025621712261,
70.4213621019252));
#235845=CARTESIAN_POINT('Ctrl Pts',(-6.21934690939891,4.88914847545498,
70.4209115730244));
#235846=CARTESIAN_POINT('Ctrl Pts',(-6.19346844107335,4.92197109669149,
70.4192486787925));
#235847=CARTESIAN_POINT('Ctrl Pts',(-6.17445070852578,4.945807242751,70.4180412131867));
#235848=CARTESIAN_POINT('Ctrl Pts',(-5.86704150791861,5.32656625209827,
70.3987532337327));
#235849=CARTESIAN_POINT('Ctrl Pts',(-5.54825549440634,5.65786199287062,
70.3820450583095));
#235850=CARTESIAN_POINT('Ctrl Pts',(-5.01234261201949,6.12568958486638,
70.357097805476));
#235851=CARTESIAN_POINT('Ctrl Pts',(-4.81432370874393,6.28251065701358,
70.3484290460469));
#235852=CARTESIAN_POINT('Ctrl Pts',(-4.18589931810519,6.73300550330014,
70.3217290308855));
#235853=CARTESIAN_POINT('Ctrl Pts',(-3.73370988021265,6.99389512970278,
70.3035642305113));
#235854=CARTESIAN_POINT('Ctrl Pts',(-3.24188190811885,7.21626510581342,
70.2819974320534));
#235855=CARTESIAN_POINT('Ctrl Pts',(-3.22458010991415,7.22401297686637,
70.2812371534633));
#235856=CARTESIAN_POINT('Ctrl Pts',(-3.1997706770104,7.23501593439064,70.2801448440562));
#235857=CARTESIAN_POINT('Ctrl Pts',(-3.19228549784985,7.23832171541877,
70.279815010035));
#235858=CARTESIAN_POINT('Ctrl Pts',(-3.17942350359844,7.24397830071323,
70.2792477859357));
#235859=CARTESIAN_POINT('Ctrl Pts',(-3.17404916783322,7.24633475050503,
70.2790106355001));
#235860=CARTESIAN_POINT('Ctrl Pts',(-3.16313491866869,7.25110577823717,
70.2785287542763));
#235861=CARTESIAN_POINT('Ctrl Pts',(-3.15759485083167,7.25351999229542,
70.2782840085017));
#235862=CARTESIAN_POINT('Ctrl Pts',(-3.14396060201519,7.25944285461772,
70.2776813389419));
#235863=CARTESIAN_POINT('Ctrl Pts',(-3.13586331859388,7.26294431155796,
70.2773231199561));
#235864=CARTESIAN_POINT('Ctrl Pts',(-3.10730635666155,7.27523635899781,
70.2760587630225));
#235865=CARTESIAN_POINT('Ctrl Pts',(-3.08681554067741,7.28395405524975,
70.2751497022249));
#235866=CARTESIAN_POINT('Ctrl Pts',(-2.67460507172667,7.45727478235392,
70.2568287150775));
#235867=CARTESIAN_POINT('Ctrl Pts',(-2.27030736478798,7.59013373184248,
70.2382873801141));
#235868=CARTESIAN_POINT('Ctrl Pts',(-1.51413666916433,7.77277038709964,
70.2042132127489));
#235869=CARTESIAN_POINT('Ctrl Pts',(-1.16577580760339,7.83259525855842,
70.1887346706286));
#235870=CARTESIAN_POINT('Ctrl Pts',(-0.467377151526313,7.90489220096417,
70.1586024307851));
#235871=CARTESIAN_POINT('Ctrl Pts',(-0.118163842135427,7.91781675258459,
70.1439741788804));
#235872=CARTESIAN_POINT('Ctrl Pts',(0.297091073903576,7.90569788941216,
70.1270506555417));
#235873=CARTESIAN_POINT('Ctrl Pts',(0.363378115011865,7.90292848884497,
70.1243626356777));
#235874=CARTESIAN_POINT('Ctrl Pts',(0.451347280069408,7.89814408432846,
70.1208117156702));
#235875=CARTESIAN_POINT('Ctrl Pts',(0.473066739764483,7.89687293865306,
70.119936344933));
#235876=CARTESIAN_POINT('Ctrl Pts',(0.50855295312103,7.89464915702493,70.118508341239));
#235877=CARTESIAN_POINT('Ctrl Pts',(0.522322907349464,7.89375007208344,
70.1179547687966));
#235878=CARTESIAN_POINT('Ctrl Pts',(0.54890553671837,7.89194454462674,70.1168871637592));
#235879=CARTESIAN_POINT('Ctrl Pts',(0.561718492308982,7.89104291714704,
70.1163730468352));
#235880=CARTESIAN_POINT('Ctrl Pts',(0.591182860446031,7.88889742865696,
70.1151918867361));
#235881=CARTESIAN_POINT('Ctrl Pts',(0.607832659738781,7.88763204483272,
70.114525235612));
#235882=CARTESIAN_POINT('Ctrl Pts',(0.660816081482424,7.88343654857742,
70.1124063517427));
#235883=CARTESIAN_POINT('Ctrl Pts',(0.697133653399223,7.88030801462151,
70.1109577816051));
#235884=CARTESIAN_POINT('Ctrl Pts',(1.05634167683523,7.84686180562356,70.0966678279628));
#235885=CARTESIAN_POINT('Ctrl Pts',(1.37710928346311,7.79696641204329,70.0842275348371));
#235886=CARTESIAN_POINT('Ctrl Pts',(2.05243821633732,7.64892982110479,70.0583750390849));
#235887=CARTESIAN_POINT('Ctrl Pts',(2.40505424527053,7.5454853662534,70.0450873164853));
#235888=CARTESIAN_POINT('Ctrl Pts',(3.15287494442057,7.26833028500581,70.016060340955));
#235889=CARTESIAN_POINT('Ctrl Pts',(3.54362151929933,7.0860378322976,70.0003463056089));
#235890=CARTESIAN_POINT('Ctrl Pts',(3.93709124265025,6.86175916029078,69.9823070155802));
#235891=CARTESIAN_POINT('Ctrl Pts',(3.95657128074476,6.85054522739924,69.9814078100892));
#235892=CARTESIAN_POINT('Ctrl Pts',(3.98299501487949,6.83518376637818,69.9801794085816));
#235893=CARTESIAN_POINT('Ctrl Pts',(3.98998065230025,6.83110831434241,69.9798538285351));
#235894=CARTESIAN_POINT('Ctrl Pts',(4.00155282443592,6.82433325076383,69.9793130901883));
#235895=CARTESIAN_POINT('Ctrl Pts',(4.00614291704869,6.82163970407463,69.9790982425227));
#235896=CARTESIAN_POINT('Ctrl Pts',(4.01513314368848,6.81635187838577,69.9786767176554));
#235897=CARTESIAN_POINT('Ctrl Pts',(4.01953349069685,6.81375796521284,69.9784700594784));
#235898=CARTESIAN_POINT('Ctrl Pts',(4.02984062073914,6.80766866697595,69.9779851926491));
#235899=CARTESIAN_POINT('Ctrl Pts',(4.03574536688144,6.80416985686918,69.9777068039797));
#235900=CARTESIAN_POINT('Ctrl Pts',(4.05436845635412,6.79310212386769,69.9768268127022));
#235901=CARTESIAN_POINT('Ctrl Pts',(4.06707006324639,6.78550522372069,69.9762237141692));
#235902=CARTESIAN_POINT('Ctrl Pts',(4.21455721300191,6.69672947493527,69.9691859233771));
#235903=CARTESIAN_POINT('Ctrl Pts',(4.34689781450766,6.611591881653,69.9625175395935));
#235904=CARTESIAN_POINT('Ctrl Pts',(4.49141693563802,6.51240492171535,69.954896315438));
#235905=CARTESIAN_POINT('Ctrl Pts',(4.506199088833,6.50218530335804,69.9541127497701));
#235906=CARTESIAN_POINT('Ctrl Pts',(4.88080318364001,6.24131237997012,69.9341556396123));
#235907=CARTESIAN_POINT('Ctrl Pts',(5.21918581026922,5.96123222998659,69.9138075111628));
#235908=CARTESIAN_POINT('Ctrl Pts',(5.55480054094463,5.63285685444536,69.892170887116));
#235909=CARTESIAN_POINT('Ctrl Pts',(5.57686955544724,5.61100805194178,69.8907405711576));
#235910=CARTESIAN_POINT('Ctrl Pts',(5.6224270433021,5.56537084882231,69.887772777617));
#235911=CARTESIAN_POINT('Ctrl Pts',(5.64589455701557,5.54156234309739,69.8862354991175));
#235912=CARTESIAN_POINT('Ctrl Pts',(6.11017327219273,5.0645268526137,69.8556585526467));
#235913=CARTESIAN_POINT('Ctrl Pts',(6.49529097694306,4.56016125646242,69.8275820506758));
#235914=CARTESIAN_POINT('Ctrl Pts',(6.82785898509628,3.99559549115742,69.8010072135642));
#235915=CARTESIAN_POINT('Ctrl Pts',(6.83935515565928,3.97588514861531,69.8000847404929));
#235916=CARTESIAN_POINT('Ctrl Pts',(6.85587192229252,3.94728329816932,69.7987537622991));
#235917=CARTESIAN_POINT('Ctrl Pts',(6.86096078464382,3.93843145978668,69.7983428975758));
#235918=CARTESIAN_POINT('Ctrl Pts',(6.86980668222111,3.9229752587709,69.7976273148951));
#235919=CARTESIAN_POINT('Ctrl Pts',(6.87357136062883,3.91637529901719,69.7973223334946));
#235920=CARTESIAN_POINT('Ctrl Pts',(6.88082279752194,3.90361994501233,69.7967340300147));
#235921=CARTESIAN_POINT('Ctrl Pts',(6.88431081815265,3.89746527955838,69.7964506646591));
#235922=CARTESIAN_POINT('Ctrl Pts',(6.8925556290906,3.88287158476477,69.7957799425493));
#235923=CARTESIAN_POINT('Ctrl Pts',(6.89730518859998,3.87442847140674,69.7953928345009));
#235924=CARTESIAN_POINT('Ctrl Pts',(6.91391020143407,3.84478306459198,69.7940368882096));
#235925=CARTESIAN_POINT('Ctrl Pts',(6.9256835489925,3.82353481471798,69.793070865673));
#235926=CARTESIAN_POINT('Ctrl Pts',(7.072789262075,3.55513326023804,69.7809411441152));
#235927=CARTESIAN_POINT('Ctrl Pts',(7.19492659274341,3.30096485789362,69.7702396350478));
#235928=CARTESIAN_POINT('Ctrl Pts',(7.58128415428314,2.37303127808974,69.7333540655585));
#235929=CARTESIAN_POINT('Ctrl Pts',(7.76640568090853,1.67033374921405,69.7096243617332));
#235930=CARTESIAN_POINT('Ctrl Pts',(7.89055629463045,0.646484163189275,
69.6728061963327));
#235931=CARTESIAN_POINT('Ctrl Pts',(7.9097448885582,0.33876422807075,69.6613867989229));
#235932=CARTESIAN_POINT('Ctrl Pts',(7.91102115814423,0.00989856671989338,
69.6482873074684));
#235933=CARTESIAN_POINT('Ctrl Pts',(7.91101983562758,-0.0109039421744316,
69.6474554331701));
#235934=CARTESIAN_POINT('Ctrl Pts',(7.91090166082746,-0.0403895646851279,
69.6462719175508));
#235935=CARTESIAN_POINT('Ctrl Pts',(7.91085256132498,-0.0490729706879633,
69.6459228342876));
#235936=CARTESIAN_POINT('Ctrl Pts',(7.91074445807252,-0.0638797135054466,
69.6453266790896));
#235937=CARTESIAN_POINT('Ctrl Pts',(7.91069264120539,-0.0700031059670321,
69.6450798721526));
#235938=CARTESIAN_POINT('Ctrl Pts',(7.91057391319928,-0.0823406590634978,
69.644582074641));
#235939=CARTESIAN_POINT('Ctrl Pts',(7.91050678939655,-0.0885548133708192,
69.6443310765237));
#235940=CARTESIAN_POINT('Ctrl Pts',(7.91032545937528,-0.103690573067891,
69.6437190782218));
#235941=CARTESIAN_POINT('Ctrl Pts',(7.91020348221067,-0.112612066136967,
69.6433578017747));
#235942=CARTESIAN_POINT('Ctrl Pts',(7.909732101786,-0.143292135664065,69.6421135738512));
#235943=CARTESIAN_POINT('Ctrl Pts',(7.90930801361072,-0.165049366286971,
69.641228034447));
#235944=CARTESIAN_POINT('Ctrl Pts',(7.8983543625057,-0.628797282299028,
69.622288809918));
#235945=CARTESIAN_POINT('Ctrl Pts',(7.85088131162575,-1.06912505287338,
69.6031252746552));
#235946=CARTESIAN_POINT('Ctrl Pts',(7.66733155680383,-2.01753142667131,
69.5613877935405));
#235947=CARTESIAN_POINT('Ctrl Pts',(7.51692779039415,-2.52076444398268,
69.5389928345805));
#235948=CARTESIAN_POINT('Ctrl Pts',(7.17939710997416,-3.34260898662557,
69.5021188216819));
#235949=CARTESIAN_POINT('Ctrl Pts',(7.01778261593823,-3.66981115299856,
69.4872559492473));
#235950=CARTESIAN_POINT('Ctrl Pts',(6.80359677257546,-4.03716230087435,
69.470035079886));
#235951=CARTESIAN_POINT('Ctrl Pts',(6.77240716139427,-4.08926763381848,
69.4675810678151));
#235952=CARTESIAN_POINT('Ctrl Pts',(6.72480803686864,-4.16674818254992,
69.4639147372843));
#235953=CARTESIAN_POINT('Ctrl Pts',(6.70884811750134,-4.19239674802439,
69.462698194935));
#235954=CARTESIAN_POINT('Ctrl Pts',(6.68109670412087,-4.23643067305631,
69.4606046164647));
#235955=CARTESIAN_POINT('Ctrl Pts',(6.66937527225629,-4.25485975068267,
69.4597268905245));
#235956=CARTESIAN_POINT('Ctrl Pts',(6.64496603678464,-4.292888594775,69.4579125011512));
#235957=CARTESIAN_POINT('Ctrl Pts',(6.63226747718221,-4.31248121522757,
69.4569759586562));
#235958=CARTESIAN_POINT('Ctrl Pts',(6.59739156685677,-4.36577289285717,
69.4544237054893));
#235959=CARTESIAN_POINT('Ctrl Pts',(6.5750428482299,-4.39935904425975,69.4528098497111));
#235960=CARTESIAN_POINT('Ctrl Pts',(6.4869714695125,-4.52954443347194,69.4465328692085));
#235961=CARTESIAN_POINT('Ctrl Pts',(6.41936854251691,-4.62485454626016,
69.4418912884152));
#235962=CARTESIAN_POINT('Ctrl Pts',(6.24335135893663,-4.86171394576476,
69.4302256310461));
#235963=CARTESIAN_POINT('Ctrl Pts',(6.13221700718403,-5.00116132434242,
69.4232359555068));
#235964=CARTESIAN_POINT('Ctrl Pts',(5.71411960026755,-5.49086303833126,
69.3981324807483));
#235965=CARTESIAN_POINT('Ctrl Pts',(5.38110225772349,-5.81760006731186,
69.3803421874458));
#235966=CARTESIAN_POINT('Ctrl Pts',(4.88353924823955,-6.22629454296176,
69.3551939352448));
#235967=CARTESIAN_POINT('Ctrl Pts',(4.74200440747497,-6.33475263811398,
69.3481745377593));
#235968=CARTESIAN_POINT('Ctrl Pts',(4.57707525233675,-6.45251100880464,
69.3400585268874));
#235969=CARTESIAN_POINT('Ctrl Pts',(4.55715494757008,-6.46659531431703,
69.3390792766886));
#235970=CARTESIAN_POINT('Ctrl Pts',(4.52691008564798,-6.48777025922047,
69.3375937031529));
#235971=CARTESIAN_POINT('Ctrl Pts',(4.51663325988129,-6.49492893374636,
69.3370891347679));
#235972=CARTESIAN_POINT('Ctrl Pts',(4.4988316047149,-6.50726660255448,69.3362154308485));
#235973=CARTESIAN_POINT('Ctrl Pts',(4.49131471512252,-6.51245703045414,
69.3358465995636));
#235974=CARTESIAN_POINT('Ctrl Pts',(4.47456368880782,-6.52398085342755,
69.3350248686121));
#235975=CARTESIAN_POINT('Ctrl Pts',(4.46532506753547,-6.53030768198174,
69.3345717922119));
#235976=CARTESIAN_POINT('Ctrl Pts',(4.44075388331292,-6.54705809399899,
69.3333670728325));
#235977=CARTESIAN_POINT('Ctrl Pts',(4.42539817090038,-6.55744735109239,
69.3326144633712));
#235978=CARTESIAN_POINT('Ctrl Pts',(4.35164699687575,-6.60696834574201,
69.3290011023577));
#235979=CARTESIAN_POINT('Ctrl Pts',(4.29276886255612,-6.64537414912787,
69.3261206439571));
#235980=CARTESIAN_POINT('Ctrl Pts',(3.62946871326175,-7.06554634934173,
69.2937579911157));
#235981=CARTESIAN_POINT('Ctrl Pts',(2.97646681887383,-7.36449029828657,
69.2630367198319));
#235982=CARTESIAN_POINT('Ctrl Pts',(2.1564026146062,-7.61275088441271,69.2278140258897));
#235983=CARTESIAN_POINT('Ctrl Pts',(2.01953500521352,-7.65019788485756,
69.2220273593962));
#235984=CARTESIAN_POINT('Ctrl Pts',(1.84569791994503,-7.69276910910477,
69.2147845329974));
#235985=CARTESIAN_POINT('Ctrl Pts',(1.80960141012084,-7.70134015173828,
69.2132863100638));
#235986=CARTESIAN_POINT('Ctrl Pts',(1.75171301175758,-7.71465617064854,
69.2108924238215));
#235987=CARTESIAN_POINT('Ctrl Pts',(1.72995911662299,-7.71956344398234,
69.2099948138479));
#235988=CARTESIAN_POINT('Ctrl Pts',(1.6886430240166,-7.72870016824137,69.208293708787));
#235989=CARTESIAN_POINT('Ctrl Pts',(1.6690849658518,-7.73294749320868,69.2074900069883));
#235990=CARTESIAN_POINT('Ctrl Pts',(1.62457083606776,-7.74243765749569,
69.2056642451202));
#235991=CARTESIAN_POINT('Ctrl Pts',(1.59960508898883,-7.74763414511772,
69.204642737016));
#235992=CARTESIAN_POINT('Ctrl Pts',(1.53470577950242,-7.76081552327239,
69.2019934865123));
#235993=CARTESIAN_POINT('Ctrl Pts',(1.49473483680088,-7.768612952506,69.2003679146869));
#235994=CARTESIAN_POINT('Ctrl Pts',(1.18069502603767,-7.82736159315848,
69.1876409838368));
#235995=CARTESIAN_POINT('Ctrl Pts',(0.904163748080776,-7.86410337357121,
69.1767025735591));
#235996=CARTESIAN_POINT('Ctrl Pts',(0.621624658355644,-7.88654078051388,
69.1656400708757));
#235997=CARTESIAN_POINT('Ctrl Pts',(0.616980776040272,-7.88690544007183,
69.1654582820691));
#235998=CARTESIAN_POINT('Ctrl Pts',(0.531838900574727,-7.8935155232476,
69.1621260156729));
#235999=CARTESIAN_POINT('Ctrl Pts',(0.45124995457206,-7.89853236491864,
69.1589832594708));
#236000=CARTESIAN_POINT('Ctrl Pts',(0.251691676715693,-7.90789112937733,
69.1512305752475));
#236001=CARTESIAN_POINT('Ctrl Pts',(0.132673820317266,-7.91078307719717,
69.1466329624234));
#236002=CARTESIAN_POINT('Ctrl Pts',(-0.545637791419402,-7.91195219904935,
69.1205705481882));
#236003=CARTESIAN_POINT('Ctrl Pts',(-1.10343012256314,-7.85360758320182,
69.0998390865875));
#236004=CARTESIAN_POINT('Ctrl Pts',(-1.97053418125241,-7.66864170349043,
69.0665704858109));
#236005=CARTESIAN_POINT('Ctrl Pts',(-2.28610841791605,-7.58055139623021,
69.0541934288714));
#236006=CARTESIAN_POINT('Ctrl Pts',(-2.63689963190927,-7.45872780315692,
69.0394963005347));
#236007=CARTESIAN_POINT('Ctrl Pts',(-2.67837611881163,-7.44393453748252,
69.0377430158081));
#236008=CARTESIAN_POINT('Ctrl Pts',(-2.73131691926864,-7.42455259460387,
69.0354831449151));
#236009=CARTESIAN_POINT('Ctrl Pts',(-2.74289735383468,-7.4202821676794,
69.0349874612163));
#236010=CARTESIAN_POINT('Ctrl Pts',(-2.76149128906497,-7.41337595137857,
69.0341893427003));
#236011=CARTESIAN_POINT('Ctrl Pts',(-2.7685111439795,-7.41075726098834,
69.0338875130375));
#236012=CARTESIAN_POINT('Ctrl Pts',(-2.78184230787428,-7.40576261109921,
69.0333133298286));
#236013=CARTESIAN_POINT('Ctrl Pts',(-2.78815432213501,-7.40338854535371,
69.0330410447723));
#236014=CARTESIAN_POINT('Ctrl Pts',(-2.80249444477008,-7.39797401874605,
69.0324214739287));
#236015=CARTESIAN_POINT('Ctrl Pts',(-2.81052064815655,-7.39492855818234,
69.0320740048296));
#236016=CARTESIAN_POINT('Ctrl Pts',(-2.8348322985067,-7.3856584541668,69.0310193684614));
#236017=CARTESIAN_POINT('Ctrl Pts',(-2.85110208063233,-7.37939305649343,
69.0303106729056));
#236018=CARTESIAN_POINT('Ctrl Pts',(-2.96595560202251,-7.33472710653747,
69.0252864238742));
#236019=CARTESIAN_POINT('Ctrl Pts',(-3.06377951558409,-7.29440671601176,
69.0208947170862));
#236020=CARTESIAN_POINT('Ctrl Pts',(-3.93189530091721,-6.91604768375778,
68.9807317531754));
#236021=CARTESIAN_POINT('Ctrl Pts',(-4.64451042085152,-6.4591221896803,
68.940188298803));
#236022=CARTESIAN_POINT('Ctrl Pts',(-5.51179424836091,-5.68398191777587,
68.889063945931));
#236023=CARTESIAN_POINT('Ctrl Pts',(-5.7384876831185,-5.4550266989416,68.875406972553));
#236024=CARTESIAN_POINT('Ctrl Pts',(-5.96577117693623,-5.19557736253906,
68.8614291078675));
#236025=CARTESIAN_POINT('Ctrl Pts',(-5.98084945682748,-5.17821297862073,
68.8605002544851));
#236026=CARTESIAN_POINT('Ctrl Pts',(-6.00238416534003,-5.15319372810005,
68.8591714073106));
#236027=CARTESIAN_POINT('Ctrl Pts',(-6.00890204324818,-5.14559204594074,
68.8587689064738));
#236028=CARTESIAN_POINT('Ctrl Pts',(-6.02017523553975,-5.13239369770441,
68.858072222402));
#236029=CARTESIAN_POINT('Ctrl Pts',(-6.02493721449291,-5.12680275577525,
68.8577777679882));
#236030=CARTESIAN_POINT('Ctrl Pts',(-6.03406862283743,-5.11605146335431,
68.8572128151506));
#236031=CARTESIAN_POINT('Ctrl Pts',(-6.0384392334869,-5.11089212804968,
68.8569422688286));
#236032=CARTESIAN_POINT('Ctrl Pts',(-6.04870417595842,-5.0987432165907,
68.8563065236597));
#236033=CARTESIAN_POINT('Ctrl Pts',(-6.05459302189567,-5.0917490056895,
68.855941547384));
#236034=CARTESIAN_POINT('Ctrl Pts',(-6.07483120582013,-5.06762726285238,
68.8546863338634));
#236035=CARTESIAN_POINT('Ctrl Pts',(-6.08912015881404,-5.05044908461893,
68.8537985395635));
#236036=CARTESIAN_POINT('Ctrl Pts',(-6.24603173697941,-4.86017607374578,
68.8440316301716));
#236037=CARTESIAN_POINT('Ctrl Pts',(-6.38130966668222,-4.68114520520416,
68.8354525716006));
#236038=CARTESIAN_POINT('Ctrl Pts',(-6.95852273651041,-3.84563205055615,
68.7977957767436));
#236039=CARTESIAN_POINT('Ctrl Pts',(-7.30799760753928,-3.13096923991101,
68.7724221487529));
#236040=CARTESIAN_POINT('Ctrl Pts',(-7.60119969975605,-2.19997506153997,
68.7380424742427));
#236041=CARTESIAN_POINT('Ctrl Pts',(-7.65055087496772,-2.02168066318905,
68.7313765766411));
#236042=CARTESIAN_POINT('Ctrl Pts',(-7.72310567619308,-1.71860796796184,
68.7196855727966));
#236043=CARTESIAN_POINT('Ctrl Pts',(-7.74963866285949,-1.59470134302498,
68.7148062357184));
#236044=CARTESIAN_POINT('Ctrl Pts',(-7.77718748041658,-1.44904797793527,
68.7089031571398));
#236045=CARTESIAN_POINT('Ctrl Pts',(-7.78110480732217,-1.42786312669663,
68.7080404538159));
#236046=CARTESIAN_POINT('Ctrl Pts',(-7.78613365936787,-1.40003180079594,
68.7069014025436));
#236047=CARTESIAN_POINT('Ctrl Pts',(-7.78732332842077,-1.39339936230936,
68.7066295336714));
#236048=CARTESIAN_POINT('Ctrl Pts',(-7.7892500135189,-1.38257850158291,
68.70618527683));
#236049=CARTESIAN_POINT('Ctrl Pts',(-7.78999213058395,-1.37839097916684,
68.706013184408));
#236050=CARTESIAN_POINT('Ctrl Pts',(-7.79141470495349,-1.37032601706327,
68.7056814100224));
#236051=CARTESIAN_POINT('Ctrl Pts',(-7.79209564555216,-1.36644866279891,
68.7055217563068));
#236052=CARTESIAN_POINT('Ctrl Pts',(-7.79364838751152,-1.3575682680243,
68.7051557555815));
#236053=CARTESIAN_POINT('Ctrl Pts',(-7.79451826528301,-1.35256489768235,
68.7049492957716));
#236054=CARTESIAN_POINT('Ctrl Pts',(-7.79724410386461,-1.33679643801509,
68.7042978316842));
#236055=CARTESIAN_POINT('Ctrl Pts',(-7.79908255431624,-1.3260285221321,
68.7038517934315));
#236056=CARTESIAN_POINT('Ctrl Pts',(-7.81539748347536,-1.22926329773904,
68.6998329420114));
#236057=CARTESIAN_POINT('Ctrl Pts',(-7.82847281469493,-1.14303908846525,
68.6961775526228));
#236058=CARTESIAN_POINT('Ctrl Pts',(-7.88740909033609,-0.705731820042474,
68.6773319981908));
#236059=CARTESIAN_POINT('Ctrl Pts',(-7.91108580357871,-0.352087788226273,
68.6611133316053));
#236060=CARTESIAN_POINT('Ctrl Pts',(-7.91084325809914,0.645895155136899,
68.6148376959662));
#236061=CARTESIAN_POINT('Ctrl Pts',(-7.83205366977351,1.287551949809,68.5847248809791));
#236062=CARTESIAN_POINT('Ctrl Pts',(-7.63369955591107,2.08365798852378,
68.5497839632651));
#236063=CARTESIAN_POINT('Ctrl Pts',(-7.58537104474223,2.25325349927394,
68.5424652438616));
#236064=CARTESIAN_POINT('Ctrl Pts',(-7.52587968753853,2.43831558495546,
68.5346147344285));
#236065=CARTESIAN_POINT('Ctrl Pts',(-7.52028676259635,2.45551114384552,
68.5338865712244));
#236066=CARTESIAN_POINT('Ctrl Pts',(-7.51187300612227,2.48108101839664,
68.5328056859826));
#236067=CARTESIAN_POINT('Ctrl Pts',(-7.5090970412129,2.48946996492996,68.5324513744765));
#236068=CARTESIAN_POINT('Ctrl Pts',(-7.50431104024997,2.50385238634467,
68.531844444626));
#236069=CARTESIAN_POINT('Ctrl Pts',(-7.50230786784703,2.50984812642866,
68.5315915828493));
#236070=CARTESIAN_POINT('Ctrl Pts',(-7.49838886895656,2.52153155639669,
68.5310991515472));
#236071=CARTESIAN_POINT('Ctrl Pts',(-7.49647375244883,2.52721947980096,
68.5308595569587));
#236072=CARTESIAN_POINT('Ctrl Pts',(-7.49186518133804,2.54085566966443,
68.5302854864449));
#236073=CARTESIAN_POINT('Ctrl Pts',(-7.48916554563593,2.54880184793873,
68.5299512307098));
#236074=CARTESIAN_POINT('Ctrl Pts',(-7.48098809720297,2.57274640082559,
68.5289448143863));
#236075=CARTESIAN_POINT('Ctrl Pts',(-7.47547161086222,2.58873157232257,
68.5282740319635));
#236076=CARTESIAN_POINT('Ctrl Pts',(-7.42484094801648,2.73393306583911,
68.5221907492286));
#236077=CARTESIAN_POINT('Ctrl Pts',(-7.37643059836866,2.86197959399821,
68.5168973318535));
#236078=CARTESIAN_POINT('Ctrl Pts',(-7.18770085984096,3.32451778395482,
68.4979868977521));
#236079=CARTESIAN_POINT('Ctrl Pts',(-7.02774493570683,3.65051939847605,
68.4850943589469));
#236080=CARTESIAN_POINT('Ctrl Pts',(-6.46714848361543,4.61858929916125,
68.4465955539818));
#236081=CARTESIAN_POINT('Ctrl Pts',(-5.99659176041218,5.21496642466577,
68.4228305182593));
#236082=CARTESIAN_POINT('Ctrl Pts',(-5.41788882742592,5.76473850535748,
68.3915206899993));
#236083=CARTESIAN_POINT('Ctrl Pts',(-5.38682320073879,5.79377813267851,
68.3898335427166));
#236084=CARTESIAN_POINT('Ctrl Pts',(-5.34981284122671,5.82781981604779,
68.3878138226306));
#236085=CARTESIAN_POINT('Ctrl Pts',(-5.34409242871493,5.83306586256276,
68.3875013778873));
#236086=CARTESIAN_POINT('Ctrl Pts',(-5.33487166866519,5.84149704069829,
68.3869972913447));
#236087=CARTESIAN_POINT('Ctrl Pts',(-5.3313761754734,5.84468745724451,68.3868060917488));
#236088=CARTESIAN_POINT('Ctrl Pts',(-5.32512137080621,5.85038608050914,
68.3864637726194));
#236089=CARTESIAN_POINT('Ctrl Pts',(-5.32236315397001,5.85289546822741,
68.386312753173));
#236090=CARTESIAN_POINT('Ctrl Pts',(-5.31657188311358,5.85815680776679,
68.3859955319414));
#236091=CARTESIAN_POINT('Ctrl Pts',(-5.31353846519703,5.86090835548905,
68.3858292970307));
#236092=CARTESIAN_POINT('Ctrl Pts',(-5.30558421956702,5.86811222855474,
68.3853931962922));
#236093=CARTESIAN_POINT('Ctrl Pts',(-5.30065993322906,5.87256071144008,
68.3851230177142));
#236094=CARTESIAN_POINT('Ctrl Pts',(-5.27900601782652,5.892072917125,68.3839340940201));
#236095=CARTESIAN_POINT('Ctrl Pts',(-5.26221788567267,5.9070712455425,68.3830101099492));
#236096=CARTESIAN_POINT('Ctrl Pts',(-5.14075676246417,6.01465454940284,
68.3763107600704));
#236097=CARTESIAN_POINT('Ctrl Pts',(-5.03371623520933,6.10451848928488,
68.3703303829838));
#236098=CARTESIAN_POINT('Ctrl Pts',(-4.77474578021259,6.31048865462766,
68.3558044740933));
#236099=CARTESIAN_POINT('Ctrl Pts',(-4.6208761656869,6.42401436851056,68.3471303453423));
#236100=CARTESIAN_POINT('Ctrl Pts',(-4.33253868812151,6.62102837346934,
68.3310162513777));
#236101=CARTESIAN_POINT('Ctrl Pts',(-4.19938133625408,6.70627339560469,
68.3236257276589));
#236102=CARTESIAN_POINT('Ctrl Pts',(-3.52426352970285,7.11047675268893,
68.2866947621455));
#236103=CARTESIAN_POINT('Ctrl Pts',(-2.94809399222469,7.3680567226221,68.2570999017098));
#236104=CARTESIAN_POINT('Ctrl Pts',(-2.13510524297085,7.6206754193539,68.220337585186));
#236105=CARTESIAN_POINT('Ctrl Pts',(-1.92005578446264,7.67767967531091,
68.2110276529885));
#236106=CARTESIAN_POINT('Ctrl Pts',(-1.6817592873947,7.73020532118632,68.2011469955851));
#236107=CARTESIAN_POINT('Ctrl Pts',(-1.66062283922999,7.73477345526727,
68.2002742771485));
#236108=CARTESIAN_POINT('Ctrl Pts',(-1.63086435372124,7.7410774315269,68.1990506728259));
#236109=CARTESIAN_POINT('Ctrl Pts',(-1.6222578449535,7.74288562657803,68.1986973927864));
#236110=CARTESIAN_POINT('Ctrl Pts',(-1.60730074638774,7.74600202372101,
68.1980844725638));
#236111=CARTESIAN_POINT('Ctrl Pts',(-1.6009515384415,7.7473167750308,68.1978246161593));
#236112=CARTESIAN_POINT('Ctrl Pts',(-1.58772188685668,7.75003932455502,
68.1972838356279));
#236113=CARTESIAN_POINT('Ctrl Pts',(-1.58084116856165,7.75144576980837,
68.1970029563248));
#236114=CARTESIAN_POINT('Ctrl Pts',(-1.56460831498766,7.7547413142814,68.196341203234));
#236115=CARTESIAN_POINT('Ctrl Pts',(-1.55525460735049,7.75662266311267,
68.195960584998));
#236116=CARTESIAN_POINT('Ctrl Pts',(-1.52455636074935,7.7627393637063,68.1947136965083));
#236117=CARTESIAN_POINT('Ctrl Pts',(-1.50319766024456,7.7669035870237,68.1938497643134));
#236118=CARTESIAN_POINT('Ctrl Pts',(-1.09001668140545,7.84569167623016,
68.1772058223454));
#236119=CARTESIAN_POINT('Ctrl Pts',(-0.693102082096715,7.89066962607179,
68.1624523967294));
#236120=CARTESIAN_POINT('Ctrl Pts',(0.518826306966947,7.93581068196543,
68.1193688038403));
#236121=CARTESIAN_POINT('Ctrl Pts',(1.33185625649462,7.8404272380676,68.0934236979002));
#236122=CARTESIAN_POINT('Ctrl Pts',(2.15882597486057,7.61087176665246,68.0595964409431));
#236123=CARTESIAN_POINT('Ctrl Pts',(2.20157469328526,7.59861615004263,68.0578270142458));
#236124=CARTESIAN_POINT('Ctrl Pts',(2.25549151259314,7.58266557825635,68.0555706305791));
#236125=CARTESIAN_POINT('Ctrl Pts',(2.26675834935077,7.57930510130921,68.0550977520128));
#236126=CARTESIAN_POINT('Ctrl Pts',(2.2845453985948,7.57395667973757,68.0543490884008));
#236127=CARTESIAN_POINT('Ctrl Pts',(2.29107063191087,7.57198539512595,68.0540739861473));
#236128=CARTESIAN_POINT('Ctrl Pts',(2.3026149309014,7.56848155311092,68.0535864878864));
#236129=CARTESIAN_POINT('Ctrl Pts',(2.30763504028592,7.56695242884955,68.0533742304613));
#236130=CARTESIAN_POINT('Ctrl Pts',(2.3191571192757,7.5634302736231,68.0528864547944));
#236131=CARTESIAN_POINT('Ctrl Pts',(2.32565804258392,7.56143385320787,68.0526108015917));
#236132=CARTESIAN_POINT('Ctrl Pts',(2.34362876407849,7.55588971326031,68.0518475907835));
#236133=CARTESIAN_POINT('Ctrl Pts',(2.35509304675062,7.55232427017967,68.0513593383043));
#236134=CARTESIAN_POINT('Ctrl Pts',(2.41729797498816,7.53282284874805,68.0487027932394));
#236135=CARTESIAN_POINT('Ctrl Pts',(2.46788439207697,7.51640180130833,68.0465160422651));
#236136=CARTESIAN_POINT('Ctrl Pts',(3.22548813931363,7.26200069613366,68.0134002662275));
#236137=CARTESIAN_POINT('Ctrl Pts',(3.89554266051209,6.92569504630479,67.9796939332058));
#236138=CARTESIAN_POINT('Ctrl Pts',(4.63242835971799,6.4146120779616,67.9412275467244));
#236139=CARTESIAN_POINT('Ctrl Pts',(4.75380603533181,6.32518541293356,67.9348230245944));
#236140=CARTESIAN_POINT('Ctrl Pts',(5.05832033635982,6.08711073318702,67.918582951615));
#236141=CARTESIAN_POINT('Ctrl Pts',(5.23750254302279,5.93364103221607,67.9088616113184));
#236142=CARTESIAN_POINT('Ctrl Pts',(5.41567130776306,5.76667107307951,67.8989808521852));
#236143=CARTESIAN_POINT('Ctrl Pts',(5.42176614128831,5.76094114605455,67.8986425720489));
#236144=CARTESIAN_POINT('Ctrl Pts',(5.43678649319039,5.74677513561423,67.8978082089299));
#236145=CARTESIAN_POINT('Ctrl Pts',(5.44570149350094,5.73832789901608,67.8973123840569));
#236146=CARTESIAN_POINT('Ctrl Pts',(5.47090459495785,5.71433555745963,67.8959089413582));
#236147=CARTESIAN_POINT('Ctrl Pts',(5.48714609095306,5.6987415920491,67.8950024820675));
#236148=CARTESIAN_POINT('Ctrl Pts',(5.51380260885289,5.67292822845103,67.8935113786188));
#236149=CARTESIAN_POINT('Ctrl Pts',(5.52425629561685,5.66274900349271,67.8929257618603));
#236150=CARTESIAN_POINT('Ctrl Pts',(5.54374434100569,5.64366729638782,67.8918324270314));
#236151=CARTESIAN_POINT('Ctrl Pts',(5.55278556266505,5.63477190016757,67.8913245352481));
#236152=CARTESIAN_POINT('Ctrl Pts',(5.57288692944677,5.61489938408339,67.8901938796729));
#236153=CARTESIAN_POINT('Ctrl Pts',(5.5839361206637,5.60391124342665,67.8895713978223));
#236154=CARTESIAN_POINT('Ctrl Pts',(5.61610563523402,5.57172986683852,67.8877561524365));
#236155=CARTESIAN_POINT('Ctrl Pts',(5.63713834095591,5.55044931108714,67.886565656977));
#236156=CARTESIAN_POINT('Ctrl Pts',(5.79534439179082,5.38855210386681,67.8775827990193));
#236157=CARTESIAN_POINT('Ctrl Pts',(5.9273611497005,5.2429862098085,67.8699288770248));
#236158=CARTESIAN_POINT('Ctrl Pts',(6.21560181621193,4.90034377436125,67.8527884688161));
#236159=CARTESIAN_POINT('Ctrl Pts',(6.36812510144712,4.70043234225726,67.8433996656303));
#236160=CARTESIAN_POINT('Ctrl Pts',(6.86166339913433,3.9853326508953,67.8114045045014));
#236161=CARTESIAN_POINT('Ctrl Pts',(7.15169314247932,3.43779787194358,67.7897652418953));
#236162=CARTESIAN_POINT('Ctrl Pts',(7.40411086386661,2.78738218927188,67.7626460621131));
#236163=CARTESIAN_POINT('Ctrl Pts',(7.43199621842302,2.71215574210869,67.7594860116449));
#236164=CARTESIAN_POINT('Ctrl Pts',(7.46310073176604,2.62416087587781,67.7557492950604));
#236165=CARTESIAN_POINT('Ctrl Pts',(7.46743872021903,2.61179091655468,67.7552230818424));
#236166=CARTESIAN_POINT('Ctrl Pts',(7.47391137600378,2.59318591228022,67.7544301739916));
#236167=CARTESIAN_POINT('Ctrl Pts',(7.47606904369181,2.5869588488368,67.7541645440067));
#236168=CARTESIAN_POINT('Ctrl Pts',(7.47989447129947,2.57587384769939,67.753691239994));
#236169=CARTESIAN_POINT('Ctrl Pts',(7.48156528791305,2.57101696290537,67.7534837095705));
#236170=CARTESIAN_POINT('Ctrl Pts',(7.4850685414005,2.56080104803721,67.7530468652586));
#236171=CARTESIAN_POINT('Ctrl Pts',(7.48689995501814,2.5554416722729,67.7528175029956));
#236172=CARTESIAN_POINT('Ctrl Pts',(7.49170082834321,2.54134312707155,67.7522136272554));
#236173=CARTESIAN_POINT('Ctrl Pts',(7.49466074578937,2.53260073744806,67.7518386560696));
#236174=CARTESIAN_POINT('Ctrl Pts',(7.50776894091152,2.4936602502621,67.7501660925996));
#236175=CARTESIAN_POINT('Ctrl Pts',(7.51774999166424,2.46340637151654,67.7488603165306));
#236176=CARTESIAN_POINT('Ctrl Pts',(7.59199058480113,2.23371947549876,67.7388936186771));
#236177=CARTESIAN_POINT('Ctrl Pts',(7.64848278157567,2.03187680548405,67.7298350987098));
#236178=CARTESIAN_POINT('Ctrl Pts',(7.78404461885729,1.46110020072928,67.7037944316538));
#236179=CARTESIAN_POINT('Ctrl Pts',(7.84484058863892,1.08840438157273,67.6863213086827));
#236180=CARTESIAN_POINT('Ctrl Pts',(7.91970559817353,0.260905781299018,
67.6480283852549));
#236181=CARTESIAN_POINT('Ctrl Pts',(7.92163796314033,-0.19371067842184,
67.627348210896));
#236182=CARTESIAN_POINT('Ctrl Pts',(7.86449376201347,-0.891154691847469,
67.5970828419961));
#236183=CARTESIAN_POINT('Ctrl Pts',(7.83298589056546,-1.13523765259873,
67.5867576918236));
#236184=CARTESIAN_POINT('Ctrl Pts',(7.78606359973278,-1.40060215981521,
67.5758230196328));
#236185=CARTESIAN_POINT('Ctrl Pts',(7.78187043760458,-1.4237153133273,67.5748729991635));
#236186=CARTESIAN_POINT('Ctrl Pts',(7.77582802194223,-1.45619736074891,
67.5735411965354));
#236187=CARTESIAN_POINT('Ctrl Pts',(7.77406467610899,-1.46558199795021,
67.573156804087));
#236188=CARTESIAN_POINT('Ctrl Pts',(7.77097199400565,-1.48187881184072,
67.5724899616385));
#236189=CARTESIAN_POINT('Ctrl Pts',(7.76965041770098,-1.48879244075826,
67.5722072757499));
#236190=CARTESIAN_POINT('Ctrl Pts',(7.76697205574318,-1.50270319278436,
67.5716389104792));
#236191=CARTESIAN_POINT('Ctrl Pts',(7.76561503747972,-1.50970026505496,
67.5713532384681));
#236192=CARTESIAN_POINT('Ctrl Pts',(7.76236061450086,-1.52636026625445,
67.5706735620396));
#236193=CARTESIAN_POINT('Ctrl Pts',(7.76045461798794,-1.53602151513891,
67.570279819889));
#236194=CARTESIAN_POINT('Ctrl Pts',(7.75640532548546,-1.55634692269173,
67.5694523117242));
#236195=CARTESIAN_POINT('Ctrl Pts',(7.75425806357083,-1.5670102749158,67.5690186674246));
#236196=CARTESIAN_POINT('Ctrl Pts',(7.74847284088452,-1.59543674119386,
67.5678639559954));
#236197=CARTESIAN_POINT('Ctrl Pts',(7.744795783556,-1.61319187868022,67.5671440814746));
#236198=CARTESIAN_POINT('Ctrl Pts',(7.66177140262123,-2.00725835167057,
67.5511964517676));
#236199=CARTESIAN_POINT('Ctrl Pts',(7.5551464194602,-2.37731544702658,67.5368542951744));
#236200=CARTESIAN_POINT('Ctrl Pts',(7.27803714832115,-3.12843892931088,
67.5081715834628));
#236201=CARTESIAN_POINT('Ctrl Pts',(7.10349990748246,-3.50674368655629,
67.4939707732165));
#236202=CARTESIAN_POINT('Ctrl Pts',(6.65822959460662,-4.30072865049707,
67.4624694079441));
#236203=CARTESIAN_POINT('Ctrl Pts',(6.3765508535052,-4.70827814437532,67.4451175111969));
#236204=CARTESIAN_POINT('Ctrl Pts',(6.03842161946734,-5.11100567077535,
67.4242934243672));
#236205=CARTESIAN_POINT('Ctrl Pts',(6.01800884669077,-5.13502522921731,
67.4230373549509));
#236206=CARTESIAN_POINT('Ctrl Pts',(5.99052112417736,-5.16698080711528,
67.4213480677093));
#236207=CARTESIAN_POINT('Ctrl Pts',(5.983572767746,-5.17502569385177,67.4209212287185));
#236208=CARTESIAN_POINT('Ctrl Pts',(5.97268994167827,-5.1875747346744,67.4202530052911));
#236209=CARTESIAN_POINT('Ctrl Pts',(5.96876652872789,-5.19208849044048,
67.4200121640985));
#236210=CARTESIAN_POINT('Ctrl Pts',(5.96088997743894,-5.20112947349032,
67.4195287897648));
#236211=CARTESIAN_POINT('Ctrl Pts',(5.956936790921,-5.2056566532824,67.4192862543255));
#236212=CARTESIAN_POINT('Ctrl Pts',(5.94799858625355,-5.21586915012669,
67.41873803718));
#236213=CARTESIAN_POINT('Ctrl Pts',(5.94301057178462,-5.22155183029942,
67.4184322125625));
#236214=CARTESIAN_POINT('Ctrl Pts',(5.92821800532219,-5.2383558580165,67.4175256009208));
#236215=CARTESIAN_POINT('Ctrl Pts',(5.91839035565772,-5.2494567727006,67.4169237327513));
#236216=CARTESIAN_POINT('Ctrl Pts',(5.83934248656592,-5.3382419020652,67.4120866847747));
#236217=CARTESIAN_POINT('Ctrl Pts',(5.76862843463035,-5.41457960198394,
67.4077844279173));
#236218=CARTESIAN_POINT('Ctrl Pts',(5.49525043649536,-5.69826288487768,
67.3913073584511));
#236219=CARTESIAN_POINT('Ctrl Pts',(5.2827497805174,-5.8958056576766,67.3788221045699));
#236220=CARTESIAN_POINT('Ctrl Pts',(4.91033953277173,-6.20566977208771,
67.3578988476421));
#236221=CARTESIAN_POINT('Ctrl Pts',(4.75624558076615,-6.32454744690161,
67.3494844691928));
#236222=CARTESIAN_POINT('Ctrl Pts',(4.41520973029936,-6.56812451273447,
67.3314609039004));
#236223=CARTESIAN_POINT('Ctrl Pts',(4.22701782039174,-6.69078923241248,
67.321876788765));
#236224=CARTESIAN_POINT('Ctrl Pts',(3.87301218074517,-6.90062749869307,
67.3045099823536));
#236225=CARTESIAN_POINT('Ctrl Pts',(3.70883279735146,-6.99023925194473,
67.2966985582147));
#236226=CARTESIAN_POINT('Ctrl Pts',(3.3663107793293,-7.16172562026536,67.2808366552323));
#236227=CARTESIAN_POINT('Ctrl Pts',(3.18778794893457,-7.24295325504262,
67.2727987430975));
#236228=CARTESIAN_POINT('Ctrl Pts',(2.88571549354815,-7.36706174915327,
67.2594685839598));
#236229=CARTESIAN_POINT('Ctrl Pts',(2.76379140836478,-7.41366375249362,
67.2541562109715));
#236230=CARTESIAN_POINT('Ctrl Pts',(2.57474960784972,-7.48060764359384,
67.2460268532089));
#236231=CARTESIAN_POINT('Ctrl Pts',(2.50842154757325,-7.50310920089263,
67.2431944827879));
#236232=CARTESIAN_POINT('Ctrl Pts',(2.41174137160759,-7.53448229359034,
67.2390948005035));
#236233=CARTESIAN_POINT('Ctrl Pts',(2.38162131187042,-7.54405725129403,
67.237821590573));
#236234=CARTESIAN_POINT('Ctrl Pts',(2.32817880693739,-7.56069429348718,
67.2355695773614));
#236235=CARTESIAN_POINT('Ctrl Pts',(2.30487961443618,-7.56782959132862,
67.2345901390223));
#236236=CARTESIAN_POINT('Ctrl Pts',(2.25629547181174,-7.58246314034823,
67.2325526728384));
#236237=CARTESIAN_POINT('Ctrl Pts',(2.23100523278638,-7.58994283160633,
67.2314948249496));
#236238=CARTESIAN_POINT('Ctrl Pts',(2.16507175965,-7.60908490712997,67.2287440050897));
#236239=CARTESIAN_POINT('Ctrl Pts',(2.12437152213732,-7.62054817614524,
67.2270529135127));
#236240=CARTESIAN_POINT('Ctrl Pts',(1.94170960640497,-7.67041802224471,
67.2194937961042));
#236241=CARTESIAN_POINT('Ctrl Pts',(1.79878421685514,-7.70518818957733,
67.213661751069));
#236242=CARTESIAN_POINT('Ctrl Pts',(1.26644595277864,-7.81907259721831,
67.1922041651124));
#236243=CARTESIAN_POINT('Ctrl Pts',(0.872208364421169,-7.87280390998333,
67.1768562486777));
#236244=CARTESIAN_POINT('Ctrl Pts',(0.115187498727938,-7.91839769503541,
67.1475423368327));
#236245=CARTESIAN_POINT('Ctrl Pts',(-0.246280254805599,-7.91540411195282,
67.1336047765581));
#236246=CARTESIAN_POINT('Ctrl Pts',(-0.650359760800838,-7.88434581558507,
67.11745972163));
#236247=CARTESIAN_POINT('Ctrl Pts',(-0.694424185768638,-7.88058701861995,
67.1156913336023));
#236248=CARTESIAN_POINT('Ctrl Pts',(-0.754816962548265,-7.87492491628468,
67.1132553269076));
#236249=CARTESIAN_POINT('Ctrl Pts',(-0.771174579355153,-7.87333987894532,
67.1125942822825));
#236250=CARTESIAN_POINT('Ctrl Pts',(-0.797194739895476,-7.87073668378792,
67.1115406771385));
#236251=CARTESIAN_POINT('Ctrl Pts',(-0.806860579378988,-7.86975167357119,
67.111148832676));
#236252=CARTESIAN_POINT('Ctrl Pts',(-0.826660213310985,-7.86769710457302,
67.1103452112875));
#236253=CARTESIAN_POINT('Ctrl Pts',(-0.836793803397933,-7.86662576759878,
67.109933395696));
#236254=CARTESIAN_POINT('Ctrl Pts',(-0.860155655201863,-7.86411026888412,
67.1089827750946));
#236255=CARTESIAN_POINT('Ctrl Pts',(-0.87338238647685,-7.86265230553085,
67.1084436572655));
#236256=CARTESIAN_POINT('Ctrl Pts',(-0.916897752826008,-7.85774451182423,
67.1066668870606));
#236257=CARTESIAN_POINT('Ctrl Pts',(-0.947169944042841,-7.85415300164765,
67.1054258724911));
#236258=CARTESIAN_POINT('Ctrl Pts',(-1.01999709800712,-7.84508558242687,
67.1024290527674));
#236259=CARTESIAN_POINT('Ctrl Pts',(-1.06252967968555,-7.83943827748803,
67.1006695849004));
#236260=CARTESIAN_POINT('Ctrl Pts',(-1.17140803015429,-7.82407950639369,
67.0961439175717));
#236261=CARTESIAN_POINT('Ctrl Pts',(-1.23767983905098,-7.81387006290142,
67.0933686134213));
#236262=CARTESIAN_POINT('Ctrl Pts',(-1.65065436978689,-7.74486402374802,
67.0759636208372));
#236263=CARTESIAN_POINT('Ctrl Pts',(-1.99324281375658,-7.66384753182314,
67.0610552886069));
#236264=CARTESIAN_POINT('Ctrl Pts',(-2.60648305526845,-7.47491071474089,
67.0340408817409));
#236265=CARTESIAN_POINT('Ctrl Pts',(-2.87876478489771,-7.37433145914516,
67.0219181510309));
#236266=CARTESIAN_POINT('Ctrl Pts',(-3.28341458512829,-7.19902028550096,
67.0037632786462));
#236267=CARTESIAN_POINT('Ctrl Pts',(-3.42017267821847,-7.13506303561728,
66.9976002800569));
#236268=CARTESIAN_POINT('Ctrl Pts',(-3.58996201886375,-7.04965415284804,
66.9899047700633));
#236269=CARTESIAN_POINT('Ctrl Pts',(-3.62477425119955,-7.03181787458476,
66.9883245217964));
#236270=CARTESIAN_POINT('Ctrl Pts',(-3.67981942301247,-7.00309772379881,
66.9858216165665));
#236271=CARTESIAN_POINT('Ctrl Pts',(-3.70013961194555,-6.99238268199853,
66.9848967372731));
#236272=CARTESIAN_POINT('Ctrl Pts',(-3.73799612759249,-6.97220932820111,
66.9831718698131));
#236273=CARTESIAN_POINT('Ctrl Pts',(-3.75554394271261,-6.96277298662633,
66.9823715997999));
#236274=CARTESIAN_POINT('Ctrl Pts',(-3.79457688114165,-6.94159252744235,
66.980589778873));
#236275=CARTESIAN_POINT('Ctrl Pts',(-3.81604352203695,-6.9298147426119,
66.9796086773805));
#236276=CARTESIAN_POINT('Ctrl Pts',(-3.87886938903857,-6.89496455059312,
66.9767336664274));
#236277=CARTESIAN_POINT('Ctrl Pts',(-3.92007662618697,-6.87162012708803,
66.9748433019408));
#236278=CARTESIAN_POINT('Ctrl Pts',(-4.28352552292124,-6.66138841428367,
66.9581235603776));
#236279=CARTESIAN_POINT('Ctrl Pts',(-4.59241135603751,-6.45232162554097,
66.9435541900578));
#236280=CARTESIAN_POINT('Ctrl Pts',(-5.16438029798295,-6.00324015328831,
66.9153596901105));
#236281=CARTESIAN_POINT('Ctrl Pts',(-5.42830392819344,-5.76569536736933,
66.9018413220092));
#236282=CARTESIAN_POINT('Ctrl Pts',(-6.01510779270623,-5.16141238266864,
66.8701310419566));
#236283=CARTESIAN_POINT('Ctrl Pts',(-6.32173135975657,-4.78093977203577,
66.8521917083083));
#236284=CARTESIAN_POINT('Ctrl Pts',(-6.65037668706667,-4.28576695019923,
66.8294430839026));
#236285=CARTESIAN_POINT('Ctrl Pts',(-6.70758099838292,-4.19567215426284,
66.8253222176226));
#236286=CARTESIAN_POINT('Ctrl Pts',(-6.79020240723264,-4.0595359946907,
66.8190916298904));
#236287=CARTESIAN_POINT('Ctrl Pts',(-6.81701214001228,-4.01435257407538,
66.8170230632416));
#236288=CARTESIAN_POINT('Ctrl Pts',(-6.86182486254777,-3.937084424497,66.8134801002833));
#236289=CARTESIAN_POINT('Ctrl Pts',(-6.88005786729249,-3.90513481283901,
66.8120135391104));
#236290=CARTESIAN_POINT('Ctrl Pts',(-6.90394769607149,-3.8625861131279,
66.8100571457601));
#236291=CARTESIAN_POINT('Ctrl Pts',(-6.90980430047521,-3.85209940147315,
66.8095747006156));
#236292=CARTESIAN_POINT('Ctrl Pts',(-6.91888011065777,-3.83576115231996,
66.8088225906709));
#236293=CARTESIAN_POINT('Ctrl Pts',(-6.92211583982343,-3.82991878544161,
66.808553553146));
#236294=CARTESIAN_POINT('Ctrl Pts',(-6.92826774671569,-3.81877776385261,
66.8080403301961));
#236295=CARTESIAN_POINT('Ctrl Pts',(-6.93118525482455,-3.81347984693081,
66.8077961962578));
#236296=CARTESIAN_POINT('Ctrl Pts',(-6.93795838617441,-3.8011470357459,
66.8072276912746));
#236297=CARTESIAN_POINT('Ctrl Pts',(-6.94180938619317,-3.79410961898137,
66.806903140264));
#236298=CARTESIAN_POINT('Ctrl Pts',(-6.9527057334131,-3.77412522921682,
66.8059810556304));
#236299=CARTESIAN_POINT('Ctrl Pts',(-6.95972558992607,-3.76116444344953,
66.8053825113967));
#236300=CARTESIAN_POINT('Ctrl Pts',(-7.00273206607491,-3.68122877388018,
66.8016873501654));
#236301=CARTESIAN_POINT('Ctrl Pts',(-7.03778704183263,-3.61375907952109,
66.7985527768892));
#236302=CARTESIAN_POINT('Ctrl Pts',(-7.12631986249401,-3.43718604694469,
66.7902866330243));
#236303=CARTESIAN_POINT('Ctrl Pts',(-7.17826298639787,-3.32734414118199,
66.785076987381));
#236304=CARTESIAN_POINT('Ctrl Pts',(-7.40924686813812,-2.80828752368348,
66.760272536044));
#236305=CARTESIAN_POINT('Ctrl Pts',(-7.5559495747517,-2.38558591839174,
66.7395918553351));
#236306=CARTESIAN_POINT('Ctrl Pts',(-7.8204588902342,-1.34718028490491,
66.6905596538628));
#236307=CARTESIAN_POINT('Ctrl Pts',(-7.90244011495927,-0.725350257540262,
66.6627612647477));
#236308=CARTESIAN_POINT('Ctrl Pts',(-7.91067278101759,-0.0759547027280309,
66.6364173843223));
#236309=CARTESIAN_POINT('Ctrl Pts',(-7.91086896929252,-0.0516248923044945,
66.6354339224731));
#236310=CARTESIAN_POINT('Ctrl Pts',(-7.91098474343785,-0.0180691788099223,
66.6340823436002));
#236311=CARTESIAN_POINT('Ctrl Pts',(-7.91100043565217,-0.00884386686046784,
66.6337112621352));
#236312=CARTESIAN_POINT('Ctrl Pts',(-7.91099997657907,0.000676441821172982,
66.6333288303818));
#236313=CARTESIAN_POINT('Ctrl Pts',(-7.91099994585805,0.000971412062998885,
66.6333169819085));
#236314=CARTESIAN_POINT('Ctrl Pts',(-7.9109998986396,0.00126638231751385,
66.6333051339456));
#236315=CARTESIAN_POINT('',(-7.91295189375223,-0.00166598417887076,62.642331508237));
#236316=CARTESIAN_POINT('Ctrl Pts',(-7.91099989836148,0.00126811855402201,
66.6333050642068));
#236317=CARTESIAN_POINT('Ctrl Pts',(-7.91099928203754,0.00511297881132095,
66.6331506291295));
#236318=CARTESIAN_POINT('Ctrl Pts',(-7.91099586272661,0.00895784202195827,
66.6329962807285));
#236319=CARTESIAN_POINT('Ctrl Pts',(-7.91097834218039,0.0197840586746226,
66.6325619164758));
#236320=CARTESIAN_POINT('Ctrl Pts',(-7.91095780249242,0.0267654053171677,
66.6322820999343));
#236321=CARTESIAN_POINT('Ctrl Pts',(-7.91089836532715,0.0406987012629768,
66.6317242134853));
#236322=CARTESIAN_POINT('Ctrl Pts',(-7.91085954540913,0.047650644824675,
66.6314461414183));
#236323=CARTESIAN_POINT('Ctrl Pts',(-7.91073262647501,0.0660386498407756,
66.6307113806948));
#236324=CARTESIAN_POINT('Ctrl Pts',(-7.91062889268007,0.0774746058023487,
66.6302551764811));
#236325=CARTESIAN_POINT('Ctrl Pts',(-7.91015231993077,0.11987607945988,
66.6285665006553));
#236326=CARTESIAN_POINT('Ctrl Pts',(-7.90962245622959,0.150839737555361,
66.6273388995308));
#236327=CARTESIAN_POINT('Ctrl Pts',(-7.900197246448,0.56086867718257,66.6111548963665));
#236328=CARTESIAN_POINT('Ctrl Pts',(-7.86424286935362,0.938836404484335,
66.5970875613475));
#236329=CARTESIAN_POINT('Ctrl Pts',(-7.70243067570597,1.90040547374632,
66.5624471197628));
#236330=CARTESIAN_POINT('Ctrl Pts',(-7.53748570971118,2.4749239617006,66.5429463969361));
#236331=CARTESIAN_POINT('Ctrl Pts',(-7.25936725899302,3.14686696985364,
66.517503072867));
#236332=CARTESIAN_POINT('Ctrl Pts',(-7.20610266127692,3.26699670417725,
66.5128375697959));
#236333=CARTESIAN_POINT('Ctrl Pts',(-7.0557477649952,3.58451016725992,66.5000658262069));
#236334=CARTESIAN_POINT('Ctrl Pts',(-6.95338151991874,3.77925408040659,
66.4917655908));
#236335=CARTESIAN_POINT('Ctrl Pts',(-6.83680463494965,3.98022336468596,
66.4824551501055));
#236336=CARTESIAN_POINT('Ctrl Pts',(-6.83053945494455,3.99096559749898,
66.4819551777497));
#236337=CARTESIAN_POINT('Ctrl Pts',(-6.82150622353697,4.00637033272666,
66.4812348190924));
#236338=CARTESIAN_POINT('Ctrl Pts',(-6.81875864010727,4.01104487738425,
66.4810157790753));
#236339=CARTESIAN_POINT('Ctrl Pts',(-6.81398665178543,4.01914452824442,
66.4806354617301));
#236340=CARTESIAN_POINT('Ctrl Pts',(-6.8119644618798,4.02257094401138,66.4804743316456));
#236341=CARTESIAN_POINT('Ctrl Pts',(-6.80807525375481,4.02914950840103,
66.4801644986259));
#236342=CARTESIAN_POINT('Ctrl Pts',(-6.80620862838498,4.03230188957265,
66.4800158220113));
#236343=CARTESIAN_POINT('Ctrl Pts',(-6.80181285901613,4.03971377338867,
66.4796657618743));
#236344=CARTESIAN_POINT('Ctrl Pts',(-6.79928190530546,4.0439721947542,66.4794642562782));
#236345=CARTESIAN_POINT('Ctrl Pts',(-6.79050903273192,4.05870135320307,
66.4787659501721));
#236346=CARTESIAN_POINT('Ctrl Pts',(-6.78424703371935,4.06915983701979,
66.4782677726274));
#236347=CARTESIAN_POINT('Ctrl Pts',(-6.70459932645225,4.20148862680312,
66.4719347984187));
#236348=CARTESIAN_POINT('Ctrl Pts',(-6.62796735928221,4.32136586863604,
66.4658800091696));
#236349=CARTESIAN_POINT('Ctrl Pts',(-6.10163134736442,5.09776724849869,
66.4249191932295));
#236350=CARTESIAN_POINT('Ctrl Pts',(-5.5582836757307,5.68532501686529,66.3860779366209));
#236351=CARTESIAN_POINT('Ctrl Pts',(-4.68822999498538,6.38006278782248,
66.3368595153382));
#236352=CARTESIAN_POINT('Ctrl Pts',(-4.42844028077415,6.56305198266711,
66.3233670828882));
#236353=CARTESIAN_POINT('Ctrl Pts',(-4.13860033191449,6.74213958633559,
66.3095880541551));
#236354=CARTESIAN_POINT('Ctrl Pts',(-4.11881635283361,6.75424390834694,
66.3086535133726));
#236355=CARTESIAN_POINT('Ctrl Pts',(-4.09081125123776,6.77120930915872,
66.3073390191198));
#236356=CARTESIAN_POINT('Ctrl Pts',(-4.0826342200968,6.776142710088,66.306956213113));
#236357=CARTESIAN_POINT('Ctrl Pts',(-4.06913154967501,6.78425588433564,
66.3063257396477));
#236358=CARTESIAN_POINT('Ctrl Pts',(-4.06381108015922,6.78744421544092,
66.3060777354332));
#236359=CARTESIAN_POINT('Ctrl Pts',(-4.05276234629888,6.79404760358914,
66.3055635915211));
#236360=CARTESIAN_POINT('Ctrl Pts',(-4.04703350102776,6.79746168192765,
66.3052974903903));
#236361=CARTESIAN_POINT('Ctrl Pts',(-4.03336998583586,6.80558099321663,
66.3046639841671));
#236362=CARTESIAN_POINT('Ctrl Pts',(-4.02543138095227,6.81027960482649,
66.304296839007));
#236363=CARTESIAN_POINT('Ctrl Pts',(-3.99942013968801,6.82561347232907,
66.303096890346));
#236364=CARTESIAN_POINT('Ctrl Pts',(-3.98131335864025,6.83619080168214,
66.3022663543023));
#236365=CARTESIAN_POINT('Ctrl Pts',(-3.77014495245343,6.95842423393827,
66.2926352106638));
#236366=CARTESIAN_POINT('Ctrl Pts',(-3.57247956996298,7.06194452791223,
66.2841568519467));
#236367=CARTESIAN_POINT('Ctrl Pts',(-3.20557481006159,7.23474410184379,
66.2692402124052));
#236368=CARTESIAN_POINT('Ctrl Pts',(-3.03781151028347,7.30677338981285,
66.2627147438363));
#236369=CARTESIAN_POINT('Ctrl Pts',(-2.62643559355724,7.46677790479841,
66.2472545881585));
#236370=CARTESIAN_POINT('Ctrl Pts',(-2.38070502022569,7.54872072244702,
66.2384668475955));
#236371=CARTESIAN_POINT('Ctrl Pts',(-2.03806315190372,7.64458058863521,
66.22644987999));
#236372=CARTESIAN_POINT('Ctrl Pts',(-1.94425863543611,7.6689746459748,66.2231829139045));
#236373=CARTESIAN_POINT('Ctrl Pts',(-1.64561615009179,7.74080556166402,
66.212800418588));
#236374=CARTESIAN_POINT('Ctrl Pts',(-1.43932818698111,7.78180272575495,
66.2056576871965));
#236375=CARTESIAN_POINT('Ctrl Pts',(-1.02568775950608,7.84699707928779,
66.1910044271717));
#236376=CARTESIAN_POINT('Ctrl Pts',(-0.818525101462187,7.87130267727842,
66.1835025596205));
#236377=CARTESIAN_POINT('Ctrl Pts',(-0.537657481213367,7.89304797240223,
66.1728266623332));
#236378=CARTESIAN_POINT('Ctrl Pts',(-0.464585112626584,7.89768585935518,
66.1700030700877));
#236379=CARTESIAN_POINT('Ctrl Pts',(-0.37212503434688,7.90226668471457,
66.1663600701291));
#236380=CARTESIAN_POINT('Ctrl Pts',(-0.352785772343109,7.90315367330225,
66.1655942055975));
#236381=CARTESIAN_POINT('Ctrl Pts',(-0.312288023977738,7.9048621458896,
66.1639819344647));
#236382=CARTESIAN_POINT('Ctrl Pts',(-0.291129141340385,7.90566968455202,
66.1631347154703));
#236383=CARTESIAN_POINT('Ctrl Pts',(-0.263566195959512,7.90661083426472,
66.162024448216));
#236384=CARTESIAN_POINT('Ctrl Pts',(-0.257164659908958,7.90682163462554,
66.1617661215252));
#236385=CARTESIAN_POINT('Ctrl Pts',(-0.24673449880566,7.90715241608655,
66.1613444561081));
#236386=CARTESIAN_POINT('Ctrl Pts',(-0.242706034707053,7.90727709295163,
66.1611814090509));
#236387=CARTESIAN_POINT('Ctrl Pts',(-0.23493035481804,7.90751179462669,
66.1608663409477));
#236388=CARTESIAN_POINT('Ctrl Pts',(-0.23118315154687,7.90762223453531,
66.1607143453585));
#236389=CARTESIAN_POINT('Ctrl Pts',(-0.22257610304206,7.90786978365866,
66.1603648573397));
#236390=CARTESIAN_POINT('Ctrl Pts',(-0.217716211496125,7.9080050763785,
66.1601672545491));
#236391=CARTESIAN_POINT('Ctrl Pts',(-0.204782576827038,7.90835319943292,
66.1596406678069));
#236392=CARTESIAN_POINT('Ctrl Pts',(-0.196708648547469,7.908558145283,66.1593112093463));
#236393=CARTESIAN_POINT('Ctrl Pts',(-0.142664636460765,7.90984716841232,
66.157101096545));
#236394=CARTESIAN_POINT('Ctrl Pts',(-0.0966870669104941,7.91054276674534,
66.1551974468075));
#236395=CARTESIAN_POINT('Ctrl Pts',(0.784336770407963,7.916189966033,66.1183063194036));
#236396=CARTESIAN_POINT('Ctrl Pts',(1.61495909087095,7.78930491016547,66.0769702379401));
#236397=CARTESIAN_POINT('Ctrl Pts',(2.74337863430935,7.42832616514622,66.0228037514143));
#236398=CARTESIAN_POINT('Ctrl Pts',(3.06897096605148,7.2998365964352,66.0073414646339));
#236399=CARTESIAN_POINT('Ctrl Pts',(3.46645458437597,7.11166161473437,65.9888374481187));
#236400=CARTESIAN_POINT('Ctrl Pts',(3.54722350984455,7.07172146107949,65.9850960529864));
#236401=CARTESIAN_POINT('Ctrl Pts',(3.65807087227756,7.01453047736543,65.9799856604118));
#236402=CARTESIAN_POINT('Ctrl Pts',(3.6887429159825,6.9984495472949,65.9785741896009));
#236403=CARTESIAN_POINT('Ctrl Pts',(3.73428230750769,6.9741913136386,65.9764822545273));
#236404=CARTESIAN_POINT('Ctrl Pts',(3.74923033272093,6.96616686194565,65.9757961878894));
#236405=CARTESIAN_POINT('Ctrl Pts',(3.77306354010134,6.95327370148798,65.9747032491939));
#236406=CARTESIAN_POINT('Ctrl Pts',(3.7819653411453,6.94843592507324,65.9742952399416));
#236407=CARTESIAN_POINT('Ctrl Pts',(3.79877940121627,6.93925626531247,65.9735249624555));
#236408=CARTESIAN_POINT('Ctrl Pts',(3.80669356665319,6.93491791913281,65.9731625647043));
#236409=CARTESIAN_POINT('Ctrl Pts',(3.82062462348474,6.92725023175208,65.972524928024));
#236410=CARTESIAN_POINT('Ctrl Pts',(3.82664462262819,6.92392657523965,65.9722494799569));
#236411=CARTESIAN_POINT('Ctrl Pts',(3.83833922737884,6.91745004442073,65.9717145649138));
#236412=CARTESIAN_POINT('Ctrl Pts',(3.84401429917232,6.91429802724052,65.9714550666749));
#236413=CARTESIAN_POINT('Ctrl Pts',(3.85739474054517,6.90684477085534,65.9708434222208));
#236414=CARTESIAN_POINT('Ctrl Pts',(3.86509681365737,6.90253761270633,65.9704914948044));
#236415=CARTESIAN_POINT('Ctrl Pts',(3.89179799179613,6.88754705905246,65.9692719545442));
#236416=CARTESIAN_POINT('Ctrl Pts',(3.91076022011657,6.8767979910971,65.9684067691432));
#236417=CARTESIAN_POINT('Ctrl Pts',(4.13112974345136,6.75067143333191,65.9583618148099));
#236418=CARTESIAN_POINT('Ctrl Pts',(4.32741716910721,6.62655784617023,65.9495150714584));
#236419=CARTESIAN_POINT('Ctrl Pts',(4.91624813205686,6.21689834753972,65.9230084970337));
#236420=CARTESIAN_POINT('Ctrl Pts',(5.28820020181546,5.90375139299988,65.9063730017569));
#236421=CARTESIAN_POINT('Ctrl Pts',(5.65162805358483,5.53570661753152,65.8885165635819));
#236422=CARTESIAN_POINT('Ctrl Pts',(5.67399994904702,5.51277352929593,65.8874098645691));
#236423=CARTESIAN_POINT('Ctrl Pts',(5.75178649667698,5.43206059529895,65.8835334024997));
#236424=CARTESIAN_POINT('Ctrl Pts',(5.8064625906904,5.37357630103937,65.8807575013142));
#236425=CARTESIAN_POINT('Ctrl Pts',(5.92370363505261,5.24429034524188,65.8746704726075));
#236426=CARTESIAN_POINT('Ctrl Pts',(5.98590662511264,5.17317769427676,65.8713534892865));
#236427=CARTESIAN_POINT('Ctrl Pts',(6.14748598072484,4.98163735349226,65.8624553818891));
#236428=CARTESIAN_POINT('Ctrl Pts',(6.24459398723676,4.85935565593164,65.8568115363913));
#236429=CARTESIAN_POINT('Ctrl Pts',(6.42786497879458,4.61400190357871,65.8453985960173));
#236430=CARTESIAN_POINT('Ctrl Pts',(6.51425770860047,4.49120333136278,65.8396355619922));
#236431=CARTESIAN_POINT('Ctrl Pts',(6.61321598982625,4.3416755354502,65.8325103234027));
#236432=CARTESIAN_POINT('Ctrl Pts',(6.62918256095405,4.31725731520878,65.8313441141959));
#236433=CARTESIAN_POINT('Ctrl Pts',(6.65028531994971,4.2845910596706,65.8297809597431));
#236434=CARTESIAN_POINT('Ctrl Pts',(6.65554204018736,4.27642087913969,65.8293897476216));
#236435=CARTESIAN_POINT('Ctrl Pts',(6.66417745756557,4.26294491882118,65.8287440891936));
#236436=CARTESIAN_POINT('Ctrl Pts',(6.66756490942522,4.25764474153666,65.8284900486614));
#236437=CARTESIAN_POINT('Ctrl Pts',(6.67413739240925,4.24733402468319,65.8279956645578));
#236438=CARTESIAN_POINT('Ctrl Pts',(6.67732311226754,4.24232392729733,65.8277553525936));
#236439=CARTESIAN_POINT('Ctrl Pts',(6.68469547941161,4.23070072314486,65.827197649648));
#236440=CARTESIAN_POINT('Ctrl Pts',(6.68887795458565,4.22408498605188,65.8268800720807));
#236441=CARTESIAN_POINT('Ctrl Pts',(6.70013946230265,4.20621314231168,65.8260217988697));
#236442=CARTESIAN_POINT('Ctrl Pts',(6.70719992764468,4.19494540379365,65.8254802899347));
#236443=CARTESIAN_POINT('Ctrl Pts',(6.75873844780945,4.11223275967713,65.8215026515674));
#236444=CARTESIAN_POINT('Ctrl Pts',(6.80210144272694,4.04010136496564,65.8180196892364));
#236445=CARTESIAN_POINT('Ctrl Pts',(7.24065206580134,3.28352160419392,65.7814270655434));
#236446=CARTESIAN_POINT('Ctrl Pts',(7.53231534395515,2.54419596747898,65.7456725481299));
#236447=CARTESIAN_POINT('Ctrl Pts',(7.77155637413643,1.50442303144175,65.7003807247599));
#236448=CARTESIAN_POINT('Ctrl Pts',(7.81938947944227,1.23188340388941,65.6888851675731));
#236449=CARTESIAN_POINT('Ctrl Pts',(7.85982094405236,0.900249459188929,
65.6753002819525));
#236450=CARTESIAN_POINT('Ctrl Pts',(7.86616328224149,0.843035979820562,
65.6729705514301));
#236451=CARTESIAN_POINT('Ctrl Pts',(7.87391858335319,0.765341831523711,
65.6698247753664));
#236452=CARTESIAN_POINT('Ctrl Pts',(7.87587707093603,0.744917676290511,
65.6689995147185));
#236453=CARTESIAN_POINT('Ctrl Pts',(7.87899502240439,0.711014386863049,
65.6676324427726));
#236454=CARTESIAN_POINT('Ctrl Pts',(7.88019940390992,0.697539516696597,
65.6670898403142));
#236455=CARTESIAN_POINT('Ctrl Pts',(7.88247817201753,0.671284844822668,
65.6660340688051));
#236456=CARTESIAN_POINT('Ctrl Pts',(7.88355605841738,0.658505391141245,
65.6655208386094));
#236457=CARTESIAN_POINT('Ctrl Pts',(7.88599635894217,0.62870810953524,65.6643257163679));
#236458=CARTESIAN_POINT('Ctrl Pts',(7.8873347722423,0.611688363108186,65.6636442618971));
#236459=CARTESIAN_POINT('Ctrl Pts',(7.8914037080637,0.557711225864623,65.6614868090556));
#236460=CARTESIAN_POINT('Ctrl Pts',(7.89392965852056,0.520738773124853,
65.6600145891226));
#236461=CARTESIAN_POINT('Ctrl Pts',(7.92087864991314,0.0808532449232036,
65.6425642329164));
#236462=CARTESIAN_POINT('Ctrl Pts',(7.91469074364,-0.323351698443158,65.6272324544178));
#236463=CARTESIAN_POINT('Ctrl Pts',(7.81449491258237,-1.41154484888727,
65.5868366513968));
#236464=CARTESIAN_POINT('Ctrl Pts',(7.66193549870036,-2.0864613413608,65.5629317880082));
#236465=CARTESIAN_POINT('Ctrl Pts',(7.40816993040214,-2.77579159953614,
65.5339807770892));
#236466=CARTESIAN_POINT('Ctrl Pts',(7.3920456843472,-2.81845014259915,65.5321683622193));
#236467=CARTESIAN_POINT('Ctrl Pts',(7.37177970755783,-2.8706957080847,65.5299203969703));
#236468=CARTESIAN_POINT('Ctrl Pts',(7.3679864400656,-2.88041762990786,65.529500885432));
#236469=CARTESIAN_POINT('Ctrl Pts',(7.36200658283733,-2.89565454958236,
65.5288414607508));
#236470=CARTESIAN_POINT('Ctrl Pts',(7.35983299816663,-2.90117466469663,
65.5286021617375));
#236471=CARTESIAN_POINT('Ctrl Pts',(7.35596745099794,-2.9109594483682,65.5281772715641));
#236472=CARTESIAN_POINT('Ctrl Pts',(7.35427798244231,-2.91522510400344,
65.527991799937));
#236473=CARTESIAN_POINT('Ctrl Pts',(7.35038044619573,-2.92504085019539,
65.5275644477046));
#236474=CARTESIAN_POINT('Ctrl Pts',(7.34816980341883,-2.93058990972043,
65.5273224424164));
#236475=CARTESIAN_POINT('Ctrl Pts',(7.34211661805863,-2.94573444241638,
65.5266608170033));
#236476=CARTESIAN_POINT('Ctrl Pts',(7.33826156049309,-2.95532487328022,
65.5262405819904));
#236477=CARTESIAN_POINT('Ctrl Pts',(7.31939539675772,-3.00199471076699,
65.5241893624855));
#236478=CARTESIAN_POINT('Ctrl Pts',(7.30412229548273,-3.0389667149656,65.5225450339597));
#236479=CARTESIAN_POINT('Ctrl Pts',(7.03961936363086,-3.66574160539814,
65.4943238568259));
#236480=CARTESIAN_POINT('Ctrl Pts',(6.71998699924606,-4.22321951402725,
65.4642357622994));
#236481=CARTESIAN_POINT('Ctrl Pts',(6.11980284778448,-5.02625157361758,
65.4181668020994));
#236482=CARTESIAN_POINT('Ctrl Pts',(5.88320586771784,-5.30123688484211,
65.4017552329232));
#236483=CARTESIAN_POINT('Ctrl Pts',(5.45352556843373,-5.73629129457823,
65.3751420655827));
#236484=CARTESIAN_POINT('Ctrl Pts',(5.27019089291166,-5.90517408834029,
65.3646112288012));
#236485=CARTESIAN_POINT('Ctrl Pts',(5.05751703092292,-6.08327550843033,
65.3532774873575));
#236486=CARTESIAN_POINT('Ctrl Pts',(5.03575641648895,-6.10130123532264,
65.352127534126));
#236487=CARTESIAN_POINT('Ctrl Pts',(5.00235494679588,-6.12866941044458,
65.3503770989181));
#236488=CARTESIAN_POINT('Ctrl Pts',(4.99078356062493,-6.13809605743508,
65.3497733587277));
#236489=CARTESIAN_POINT('Ctrl Pts',(4.9717771332771,-6.15349039382,65.3487860422892));
#236490=CARTESIAN_POINT('Ctrl Pts',(4.9643578828676,-6.15947746983601,65.3484017188756));
#236491=CARTESIAN_POINT('Ctrl Pts',(4.95000934790789,-6.17101347108987,
65.3476605309133));
#236492=CARTESIAN_POINT('Ctrl Pts',(4.94308151263521,-6.17656417151403,
65.3473035983366));
#236493=CARTESIAN_POINT('Ctrl Pts',(4.93042689498891,-6.18666834109502,
65.3466533065276));
#236494=CARTESIAN_POINT('Ctrl Pts',(4.92470311532453,-6.19122554554482,
65.3463598042737));
#236495=CARTESIAN_POINT('Ctrl Pts',(4.91222316801581,-6.2011336725963,65.345721228352));
#236496=CARTESIAN_POINT('Ctrl Pts',(4.9054645580108,-6.20648151116878,65.3453762727331));
#236497=CARTESIAN_POINT('Ctrl Pts',(4.88722625516582,-6.22086440501052,
65.3444477358294));
#236498=CARTESIAN_POINT('Ctrl Pts',(4.87573022864699,-6.22987874320063,
65.3438649443551));
#236499=CARTESIAN_POINT('Ctrl Pts',(4.82261822988918,-6.27128820355819,
65.3411838167773));
#236500=CARTESIAN_POINT('Ctrl Pts',(4.78070351486427,-6.30329884715531,
65.3391000675235));
#236501=CARTESIAN_POINT('Ctrl Pts',(4.05126906247565,-6.84891292170329,
65.3033767281313));
#236502=CARTESIAN_POINT('Ctrl Pts',(3.2850770636264,-7.24766466795618,65.2747982818525));
#236503=CARTESIAN_POINT('Ctrl Pts',(2.27660726844952,-7.57907220430775,
65.237707518615));
#236504=CARTESIAN_POINT('Ctrl Pts',(2.08104168511736,-7.63508588872774,
65.2305004234966));
#236505=CARTESIAN_POINT('Ctrl Pts',(1.69202090815529,-7.73045089168454,
65.215825977187));
#236506=CARTESIAN_POINT('Ctrl Pts',(1.49881412551783,-7.77022281110548,
65.2083709582009));
#236507=CARTESIAN_POINT('Ctrl Pts',(1.26996042998991,-7.80847840608513,
65.1991945472144));
#236508=CARTESIAN_POINT('Ctrl Pts',(1.23556445814071,-7.81399481257133,
65.1978072648243));
#236509=CARTESIAN_POINT('Ctrl Pts',(1.19063388305767,-7.82089667498545,
65.1959854634914));
#236510=CARTESIAN_POINT('Ctrl Pts',(1.18013101345366,-7.82248839142609,
65.1955589176149));
#236511=CARTESIAN_POINT('Ctrl Pts',(1.16305265320631,-7.82504144953598,
65.1948642434667));
#236512=CARTESIAN_POINT('Ctrl Pts',(1.15647908122443,-7.82601567181203,
65.194596598369));
#236513=CARTESIAN_POINT('Ctrl Pts',(1.14385606947641,-7.82787018690325,
65.1940821575163));
#236514=CARTESIAN_POINT('Ctrl Pts',(1.13780681934505,-7.82875175313959,
65.1938354087939));
#236515=CARTESIAN_POINT('Ctrl Pts',(1.12400070550152,-7.83074739882598,
65.193271772735));
#236516=CARTESIAN_POINT('Ctrl Pts',(1.11624320215771,-7.83185696519682,
65.192954722555));
#236517=CARTESIAN_POINT('Ctrl Pts',(1.0920313312266,-7.83528331878388,65.1919641146372));
#236518=CARTESIAN_POINT('Ctrl Pts',(1.07557135900134,-7.83755978355911,
65.1912891340108));
#236519=CARTESIAN_POINT('Ctrl Pts',(0.943143109205395,-7.85544998778699,
65.185846842098));
#236520=CARTESIAN_POINT('Ctrl Pts',(0.826851201363329,-7.86854047155583,
65.1809955164232));
#236521=CARTESIAN_POINT('Ctrl Pts',(0.226765852880969,-7.92263960998303,
65.1557123925149));
#236522=CARTESIAN_POINT('Ctrl Pts',(-0.259767247274056,-7.92162645311127,
65.1344753582925));
#236523=CARTESIAN_POINT('Ctrl Pts',(-1.16466782515643,-7.83624542502699,
65.0954252437204));
#236524=CARTESIAN_POINT('Ctrl Pts',(-1.58234017973066,-7.76269407223206,
65.0775692808003));
#236525=CARTESIAN_POINT('Ctrl Pts',(-2.3004596274304,-7.5758371962115,65.0469227699631));
#236526=CARTESIAN_POINT('Ctrl Pts',(-2.60366799199404,-7.47705444288822,
65.0339376002999));
#236527=CARTESIAN_POINT('Ctrl Pts',(-2.95311059273801,-7.33936687585642,
65.0187334165742));
#236528=CARTESIAN_POINT('Ctrl Pts',(-3.00590153086049,-7.31790436822573,
65.0164312375924));
#236529=CARTESIAN_POINT('Ctrl Pts',(-3.08563336799752,-7.28448049730058,
65.0129461245992));
#236530=CARTESIAN_POINT('Ctrl Pts',(-3.11274677424793,-7.27293592184086,
65.0117595566524));
#236531=CARTESIAN_POINT('Ctrl Pts',(-3.15976184372643,-7.25260637999799,
65.009699503751));
#236532=CARTESIAN_POINT('Ctrl Pts',(-3.17969292700168,-7.24389032943898,
65.0088253922964));
#236533=CARTESIAN_POINT('Ctrl Pts',(-3.22440136764305,-7.22411883525122,
65.0068628137169));
#236534=CARTESIAN_POINT('Ctrl Pts',(-3.2491583299682,-7.21301790359976,
65.0057747927955));
#236535=CARTESIAN_POINT('Ctrl Pts',(-3.31551299794478,-7.1828537709395,
65.0028551647272));
#236536=CARTESIAN_POINT('Ctrl Pts',(-3.35700331006319,-7.16355662619601,
65.0010259001361));
#236537=CARTESIAN_POINT('Ctrl Pts',(-3.54766651296,-7.07285892776174,64.9926018252344));
#236538=CARTESIAN_POINT('Ctrl Pts',(-3.69474612390494,-6.99715109128936,
64.9860532675792));
#236539=CARTESIAN_POINT('Ctrl Pts',(-3.86041590981725,-6.9051930250294,
64.978600167615));
#236540=CARTESIAN_POINT('Ctrl Pts',(-3.88143212040733,-6.89340165722562,
64.9776532297877));
#236541=CARTESIAN_POINT('Ctrl Pts',(-4.46523745561113,-6.56233521067544,
64.951305526274));
#236542=CARTESIAN_POINT('Ctrl Pts',(-4.98678148426048,-6.17531866429517,
64.9268440402243));
#236543=CARTESIAN_POINT('Ctrl Pts',(-5.52640283470541,-5.66148555973626,
64.8974466264646));
#236544=CARTESIAN_POINT('Ctrl Pts',(-5.59619010341347,-5.59251310861638,
64.8935498954053));
#236545=CARTESIAN_POINT('Ctrl Pts',(-5.67933048548015,-5.50722861263397,
64.8887747536335));
#236546=CARTESIAN_POINT('Ctrl Pts',(-5.69392548568271,-5.49213749944513,
64.8879313871));
#236547=CARTESIAN_POINT('Ctrl Pts',(-5.71662920404554,-5.4684742633342,
64.8866112483937));
#236548=CARTESIAN_POINT('Ctrl Pts',(-5.72477914102156,-5.45994175891446,
64.8861356913924));
#236549=CARTESIAN_POINT('Ctrl Pts',(-5.73985646487481,-5.44408581706135,
64.8852527715162));
#236550=CARTESIAN_POINT('Ctrl Pts',(-5.74678900610458,-5.43676730599287,
64.8848455656542));
#236551=CARTESIAN_POINT('Ctrl Pts',(-5.7620538604238,-5.42059076131024,
64.8839461601382));
#236552=CARTESIAN_POINT('Ctrl Pts',(-5.77037976917114,-5.41172673093397,
64.8834537642825));
#236553=CARTESIAN_POINT('Ctrl Pts',(-5.79426869206136,-5.38617600687318,
64.8820356093829));
#236554=CARTESIAN_POINT('Ctrl Pts',(-5.8097798774938,-5.36944125715782,
64.8811081784051));
#236555=CARTESIAN_POINT('Ctrl Pts',(-5.92998476284706,-5.23862361500082,
64.8738699495423));
#236556=CARTESIAN_POINT('Ctrl Pts',(-6.03137917850009,-5.12155835328291,
64.8674622120488));
#236557=CARTESIAN_POINT('Ctrl Pts',(-6.20399539181202,-4.91002356757783,
64.8560679488168));
#236558=CARTESIAN_POINT('Ctrl Pts',(-6.2766579606571,-4.81678883532281,
64.8511052233825));
#236559=CARTESIAN_POINT('Ctrl Pts',(-6.55468348287408,-4.44307031719229,
64.8314950433296));
#236560=CARTESIAN_POINT('Ctrl Pts',(-6.74355947346076,-4.15080245219404,
64.8167854207848));
#236561=CARTESIAN_POINT('Ctrl Pts',(-7.00393904565052,-3.68293868639049,
64.7944465436555));
#236562=CARTESIAN_POINT('Ctrl Pts',(-7.08940470736722,-3.51561412131933,
64.7866736813764));
#236563=CARTESIAN_POINT('Ctrl Pts',(-7.20087746185788,-3.2767401758236,
64.7758745818195));
#236564=CARTESIAN_POINT('Ctrl Pts',(-7.23193200219774,-3.20761937840966,
64.7727834161222));
#236565=CARTESIAN_POINT('Ctrl Pts',(-7.28481692959007,-3.08523502747364,
64.7673673641284));
#236566=CARTESIAN_POINT('Ctrl Pts',(-7.3070678769772,-3.03215962371616,
64.7650371399895));
#236567=CARTESIAN_POINT('Ctrl Pts',(-7.33871275733246,-2.95430496410741,
64.7616451002709));
#236568=CARTESIAN_POINT('Ctrl Pts',(-7.34856437555683,-2.92971404416638,
64.7605774682573));
#236569=CARTESIAN_POINT('Ctrl Pts',(-7.3656892497325,-2.88633827197494,
64.758700762772));
#236570=CARTESIAN_POINT('Ctrl Pts',(-7.37301461314857,-2.86757428170369,
64.7578910411445));
#236571=CARTESIAN_POINT('Ctrl Pts',(-7.38716037181644,-2.83092722492057,
64.7563136796715));
#236572=CARTESIAN_POINT('Ctrl Pts',(-7.39398769174374,-2.81304698299139,
64.7555459589759));
#236573=CARTESIAN_POINT('Ctrl Pts',(-7.41026741896729,-2.76994284460643,
64.7536996437646));
#236574=CARTESIAN_POINT('Ctrl Pts',(-7.41965602483305,-2.74469507646945,
64.7526218331671));
#236575=CARTESIAN_POINT('Ctrl Pts',(-7.45400825882142,-2.65085089625082,
64.7486288216142));
#236576=CARTESIAN_POINT('Ctrl Pts',(-7.47815115241558,-2.58195760249436,
64.7457234382332));
#236577=CARTESIAN_POINT('Ctrl Pts',(-7.77295151158238,-1.70188357189728,
64.7089081060041));
#236578=CARTESIAN_POINT('Ctrl Pts',(-7.91131782727057,-0.852277164320057,
64.6763923099968));
#236579=CARTESIAN_POINT('Ctrl Pts',(-7.91088452321688,0.311667010540729,
64.6328655054235));
#236580=CARTESIAN_POINT('Ctrl Pts',(-7.89269817734012,0.620111447589521,
64.6213625335678));
#236581=CARTESIAN_POINT('Ctrl Pts',(-7.83374141446319,1.11994740556406,
64.6021363242674));
#236582=CARTESIAN_POINT('Ctrl Pts',(-7.8038251575381,1.31228593576899,64.5945909225753));
#236583=CARTESIAN_POINT('Ctrl Pts',(-7.76339308421455,1.52117708106424,
64.5860954253086));
#236584=CARTESIAN_POINT('Ctrl Pts',(-7.75987480568725,1.53902400439993,
64.5853671660829));
#236585=CARTESIAN_POINT('Ctrl Pts',(-7.75453739664275,1.56561506436483,
64.5842782962087));
#236586=CARTESIAN_POINT('Ctrl Pts',(-7.75276494974449,1.5743685715218,64.583919236688));
#236587=CARTESIAN_POINT('Ctrl Pts',(-7.74969348264725,1.58940652656909,
64.5833013162439));
#236588=CARTESIAN_POINT('Ctrl Pts',(-7.7484016299389,1.59569243984903,64.5830426990774));
#236589=CARTESIAN_POINT('Ctrl Pts',(-7.74572574363282,1.60863292998275,
64.5825096185403));
#236590=CARTESIAN_POINT('Ctrl Pts',(-7.74434077983235,1.61528730710124,
64.5822351232398));
#236591=CARTESIAN_POINT('Ctrl Pts',(-7.7411066582929,1.63072661701824,64.5815973743376));
#236592=CARTESIAN_POINT('Ctrl Pts',(-7.73925112113987,1.6395101944426,64.5812338968571));
#236593=CARTESIAN_POINT('Ctrl Pts',(-7.7333282067922,1.66731344925635,64.580081236042));
#236594=CARTESIAN_POINT('Ctrl Pts',(-7.72920565433316,1.68632121403199,
64.5792900717738));
#236595=CARTESIAN_POINT('Ctrl Pts',(-7.61964723618212,2.1826171870924,64.5585467086464));
#236596=CARTESIAN_POINT('Ctrl Pts',(-7.47029854184898,2.64900880987656,
64.5365118008296));
#236597=CARTESIAN_POINT('Ctrl Pts',(-6.98700272257376,3.7843477583362,64.4800097007572));
#236598=CARTESIAN_POINT('Ctrl Pts',(-6.59953943876348,4.425600854941,64.4459557794708));
#236599=CARTESIAN_POINT('Ctrl Pts',(-6.09867470119871,5.0390709755064,64.4135720494977));
#236600=CARTESIAN_POINT('Ctrl Pts',(-6.06904562698734,5.07471720188722,
64.4116892524954));
#236601=CARTESIAN_POINT('Ctrl Pts',(-6.03023008971474,5.12058930394145,
64.4092646601659));
#236602=CARTESIAN_POINT('Ctrl Pts',(-6.02132819513371,5.13105413375027,
64.4087114214991));
#236603=CARTESIAN_POINT('Ctrl Pts',(-6.00710868876948,5.14768224173842,
64.407832158859));
#236604=CARTESIAN_POINT('Ctrl Pts',(-6.00180876674147,5.1538605713166,64.4075054178816));
#236605=CARTESIAN_POINT('Ctrl Pts',(-5.99227266719119,5.1649425236226,64.4069192695422));
#236606=CARTESIAN_POINT('Ctrl Pts',(-5.98803998670627,5.16984913785188,
64.4066597201374));
#236607=CARTESIAN_POINT('Ctrl Pts',(-5.97813586475046,5.18130172807505,
64.4060538353673));
#236608=CARTESIAN_POINT('Ctrl Pts',(-5.97245968736258,5.18784360772507,
64.4057076940662));
#236609=CARTESIAN_POINT('Ctrl Pts',(-5.95619543940933,5.20652632700762,
64.4047190088754));
#236610=CARTESIAN_POINT('Ctrl Pts',(-5.94558098562208,5.21864419687512,
64.404077549144));
#236611=CARTESIAN_POINT('Ctrl Pts',(-5.87742621538128,5.29597447208053,
64.3999827998908));
#236612=CARTESIAN_POINT('Ctrl Pts',(-5.81884984861185,5.36026786319395,
64.3965726682081));
#236613=CARTESIAN_POINT('Ctrl Pts',(-5.64343061171831,5.54654298153605,
64.3866675365612));
#236614=CARTESIAN_POINT('Ctrl Pts',(-5.52372580413826,5.66576608137955,
64.380296229468));
#236615=CARTESIAN_POINT('Ctrl Pts',(-5.14903647954631,6.01577594695166,
64.3613944307476));
#236616=CARTESIAN_POINT('Ctrl Pts',(-4.88273942192422,6.23386005454693,
64.3493547610119));
#236617=CARTESIAN_POINT('Ctrl Pts',(-4.49141430599195,6.513829352766,64.3328450612914));
#236618=CARTESIAN_POINT('Ctrl Pts',(-4.37767901909459,6.59080435594572,
64.328172106331));
#236619=CARTESIAN_POINT('Ctrl Pts',(-4.13509885122626,6.74592966002602,
64.3183782047864));
#236620=CARTESIAN_POINT('Ctrl Pts',(-4.00590909727489,6.82343764363281,
64.3132598398298));
#236621=CARTESIAN_POINT('Ctrl Pts',(-3.52795224875502,7.09193536610502,
64.2944501692724));
#236622=CARTESIAN_POINT('Ctrl Pts',(-3.16715975809274,7.26023678687777,
64.2805024216922));
#236623=CARTESIAN_POINT('Ctrl Pts',(-2.73330756054947,7.42410534870174,
64.2625000156496));
#236624=CARTESIAN_POINT('Ctrl Pts',(-2.67103830963621,7.44673514644921,
64.259887416779));
#236625=CARTESIAN_POINT('Ctrl Pts',(-2.5986505932255,7.47201745195604,64.2568098429536));
#236626=CARTESIAN_POINT('Ctrl Pts',(-2.58880062590436,7.47543584183412,
64.2563902086264));
#236627=CARTESIAN_POINT('Ctrl Pts',(-2.57417535563201,7.48047910779384,
64.2557658200017));
#236628=CARTESIAN_POINT('Ctrl Pts',(-2.5694051764208,7.48211891664661,64.2555619622406));
#236629=CARTESIAN_POINT('Ctrl Pts',(-2.56092520692506,7.4850249465483,64.2551991904726));
#236630=CARTESIAN_POINT('Ctrl Pts',(-2.55721603360747,7.4862929760509,64.2550403859401));
#236631=CARTESIAN_POINT('Ctrl Pts',(-2.54942625954005,7.48894954760442,
64.2547066059428));
#236632=CARTESIAN_POINT('Ctrl Pts',(-2.54534546472459,7.49033751205245,
64.2545315954107));
#236633=CARTESIAN_POINT('Ctrl Pts',(-2.53463841993553,7.49396944368319,
64.2540719988585));
#236634=CARTESIAN_POINT('Ctrl Pts',(-2.52801033725516,7.49620795314431,
64.2537870787175));
#236635=CARTESIAN_POINT('Ctrl Pts',(-2.49789626663681,7.50633392847157,
64.2524906681492));
#236636=CARTESIAN_POINT('Ctrl Pts',(-2.47437673242937,7.51411967858739,
64.2514728550875));
#236637=CARTESIAN_POINT('Ctrl Pts',(-1.96485324271369,7.68013738295354,
64.229315268551));
#236638=CARTESIAN_POINT('Ctrl Pts',(-1.46472098892859,7.7909991326682,64.2055252919042));
#236639=CARTESIAN_POINT('Ctrl Pts',(-0.739842015891198,7.87937876971255,
64.1715611967195));
#236640=CARTESIAN_POINT('Ctrl Pts',(-0.521225950115917,7.8968540061067,
64.161371288666));
#236641=CARTESIAN_POINT('Ctrl Pts',(0.193036051719969,7.92415537853956,
64.1286366094361));
#236642=CARTESIAN_POINT('Ctrl Pts',(0.688967922225117,7.89651497230842,
64.1068719336869));
#236643=CARTESIAN_POINT('Ctrl Pts',(1.21106283397772,7.81781884766206,64.0854307964007));
#236644=CARTESIAN_POINT('Ctrl Pts',(1.24297912746055,7.81280792329007,64.0841255360625));
#236645=CARTESIAN_POINT('Ctrl Pts',(1.28601085931369,7.80578148763414,64.0823729608116));
#236646=CARTESIAN_POINT('Ctrl Pts',(1.2971537384086,7.80393751534287,64.081919797525));
#236647=CARTESIAN_POINT('Ctrl Pts',(1.31466232940341,7.80100158140838,64.0812087793723));
#236648=CARTESIAN_POINT('Ctrl Pts',(1.32103069581015,7.79992568006176,64.0809503761468));
#236649=CARTESIAN_POINT('Ctrl Pts',(1.333271633079,7.79784221784928,64.0804540970928));
#236650=CARTESIAN_POINT('Ctrl Pts',(1.33914439562785,7.79683581909488,64.0802161817315));
#236651=CARTESIAN_POINT('Ctrl Pts',(1.35296391955941,7.79445153181023,64.0796567555466));
#236652=CARTESIAN_POINT('Ctrl Pts',(1.36090972923312,7.79306812229849,64.0793354338041));
#236653=CARTESIAN_POINT('Ctrl Pts',(1.3839543322968,7.78901960978687,64.0784044862969));
#236654=CARTESIAN_POINT('Ctrl Pts',(1.39904755217002,7.78632275377439,64.0777959478075));
#236655=CARTESIAN_POINT('Ctrl Pts',(1.50368860764358,7.76731140934583,64.0735851390602));
#236656=CARTESIAN_POINT('Ctrl Pts',(1.59295865842962,7.74949607460564,64.0700345685605));
#236657=CARTESIAN_POINT('Ctrl Pts',(1.86265693665639,7.69081586198631,64.0594233756925));
#236658=CARTESIAN_POINT('Ctrl Pts',(2.04198101920279,7.64515914530808,64.0525275766075));
#236659=CARTESIAN_POINT('Ctrl Pts',(2.72267036632174,7.4461901613614,64.0267759468229));
#236660=CARTESIAN_POINT('Ctrl Pts',(3.20994556004413,7.24947889792212,64.0093433961322));
#236661=CARTESIAN_POINT('Ctrl Pts',(4.09201404819325,6.78689572801275,63.97560782675));
#236662=CARTESIAN_POINT('Ctrl Pts',(4.48937105846307,6.5308479562568,63.9593846957629));
#236663=CARTESIAN_POINT('Ctrl Pts',(4.88486812349987,6.22276963296857,63.9395619379357));
#236664=CARTESIAN_POINT('Ctrl Pts',(4.90813447434176,6.20443506084648,63.9383810993536));
#236665=CARTESIAN_POINT('Ctrl Pts',(4.93716121914123,6.18129568449885,63.9368886015499));
#236666=CARTESIAN_POINT('Ctrl Pts',(4.943018773897,6.17661255407107,63.9365864259829));
#236667=CARTESIAN_POINT('Ctrl Pts',(4.95223049162175,6.16922626553811,63.9361096388008));
#236668=CARTESIAN_POINT('Ctrl Pts',(4.95558912758511,6.16652867956016,63.9359354682787));
#236669=CARTESIAN_POINT('Ctrl Pts',(4.96180051683923,6.16153147015002,63.9356127495189));
#236670=CARTESIAN_POINT('Ctrl Pts',(4.96465388512767,6.15923260052334,63.9354642607764));
#236671=CARTESIAN_POINT('Ctrl Pts',(4.97098192222929,6.15412704449034,63.935134421878));
#236672=CARTESIAN_POINT('Ctrl Pts',(4.97445581093696,6.15131939796065,63.9349529964619));
#236673=CARTESIAN_POINT('Ctrl Pts',(4.98439031213249,6.14327627298296,63.9344331523627));
#236674=CARTESIAN_POINT('Ctrl Pts',(4.99084503241679,6.1380335622422,63.934094170832));
#236675=CARTESIAN_POINT('Ctrl Pts',(5.03207959109769,6.10443361509594,63.9319208897339));
#236676=CARTESIAN_POINT('Ctrl Pts',(5.06662521464639,6.07579159826939,63.9300647209231));
#236677=CARTESIAN_POINT('Ctrl Pts',(5.17021671041445,5.98840531852886,63.9243960563845));
#236678=CARTESIAN_POINT('Ctrl Pts',(5.23849654846711,5.92876815388919,63.9205200854795));
#236679=CARTESIAN_POINT('Ctrl Pts',(5.43622834644156,5.74998200376512,63.9089196701358));
#236680=CARTESIAN_POINT('Ctrl Pts',(5.56274431072916,5.62767635967614,63.9010089206926));
#236681=CARTESIAN_POINT('Ctrl Pts',(5.98025080605423,5.19622005337958,63.8735075503733));
#236682=CARTESIAN_POINT('Ctrl Pts',(6.25039723339212,4.86791909241502,63.8532886931837));
#236683=CARTESIAN_POINT('Ctrl Pts',(6.69776412054272,4.22521799154917,63.816774740303));
#236684=CARTESIAN_POINT('Ctrl Pts',(6.88239357752927,3.91729600835116,63.8003939042679));
#236685=CARTESIAN_POINT('Ctrl Pts',(7.16526266729727,3.36337188954451,63.773238266434));
#236686=CARTESIAN_POINT('Ctrl Pts',(7.27324335869973,3.12301282987252,63.7621409097484));
#236687=CARTESIAN_POINT('Ctrl Pts',(7.37725852280909,2.85665677018606,63.7505574922953));
#236688=CARTESIAN_POINT('Ctrl Pts',(7.38538498199774,2.83558105053327,63.7496456210783));
#236689=CARTESIAN_POINT('Ctrl Pts',(7.39660898458209,2.80609636703977,63.7483763903276));
#236690=CARTESIAN_POINT('Ctrl Pts',(7.39978263573776,2.79771661117309,63.7480163932658));
#236691=CARTESIAN_POINT('Ctrl Pts',(7.40524330114572,2.78322389486852,63.7473950327189));
#236692=CARTESIAN_POINT('Ctrl Pts',(7.40753699731173,2.77711347119247,63.7471334383312));
#236693=CARTESIAN_POINT('Ctrl Pts',(7.41227289254228,2.76444939922472,63.7465920669997));
#236694=CARTESIAN_POINT('Ctrl Pts',(7.41471396852983,2.75789533514638,63.7463123289699));
#236695=CARTESIAN_POINT('Ctrl Pts',(7.42040503433178,2.74255317526491,63.7456585240878));
#236696=CARTESIAN_POINT('Ctrl Pts',(7.42364811224973,2.73376251693251,63.7452846954732));
#236697=CARTESIAN_POINT('Ctrl Pts',(7.43404694913998,2.70542056150309,63.7440819492995));
#236698=CARTESIAN_POINT('Ctrl Pts',(7.44114117546848,2.68584669556688,63.7432551448048));
#236699=CARTESIAN_POINT('Ctrl Pts',(7.60519834971592,2.22755280643899,63.7239856024463));
#236700=CARTESIAN_POINT('Ctrl Pts',(7.72318299393176,1.7758206661223,63.7069714200375));
#236701=CARTESIAN_POINT('Ctrl Pts',(7.88627796430435,0.809277563742729,
63.6725580291106));
#236702=CARTESIAN_POINT('Ctrl Pts',(7.92219366569465,0.295151974411452,
63.6553774165823));
#236703=CARTESIAN_POINT('Ctrl Pts',(7.90394648209241,-0.36435426003187,
63.631617934523));
#236704=CARTESIAN_POINT('Ctrl Pts',(7.89590136726839,-0.509767217034449,
63.6262657892029));
#236705=CARTESIAN_POINT('Ctrl Pts',(7.8736856866521,-0.777217438749315,
63.6160892520921));
#236706=CARTESIAN_POINT('Ctrl Pts',(7.86067791206208,-0.899295806154468,
63.6113060764793));
#236707=CARTESIAN_POINT('Ctrl Pts',(7.84261612746838,-1.03806969694013,
63.6057094774505));
#236708=CARTESIAN_POINT('Ctrl Pts',(7.84034227950658,-1.0551063228355,63.6050198106969));
#236709=CARTESIAN_POINT('Ctrl Pts',(7.83703858600898,-1.07925849102365,
63.6040385156898));
#236710=CARTESIAN_POINT('Ctrl Pts',(7.83605452272862,-1.08638032265145,
63.6037487159174));
#236711=CARTESIAN_POINT('Ctrl Pts',(7.83423431804553,-1.09942230161413,
63.6032172152205));
#236712=CARTESIAN_POINT('Ctrl Pts',(7.83340117040299,-1.10534286562151,
63.6029756320097));
#236713=CARTESIAN_POINT('Ctrl Pts',(7.83170255168003,-1.11731531648677,
63.6024865023705));
#236714=CARTESIAN_POINT('Ctrl Pts',(7.83083677554566,-1.12336715678453,
63.6022389442311));
#236715=CARTESIAN_POINT('Ctrl Pts',(7.82871998363456,-1.13804232999326,
63.6016378874268));
#236716=CARTESIAN_POINT('Ctrl Pts',(7.82746173544444,-1.14666460066037,
63.6012841130634));
#236717=CARTESIAN_POINT('Ctrl Pts',(7.82296046374832,-1.17715734632519,
63.6000307959122));
#236718=CARTESIAN_POINT('Ctrl Pts',(7.81964001966288,-1.1990161743014,63.5991283633749));
#236719=CARTESIAN_POINT('Ctrl Pts',(7.75138199030471,-1.63601962491467,
63.5810101149756));
#236720=CARTESIAN_POINT('Ctrl Pts',(7.65356508486526,-2.04533395711269,
63.5626869635745));
#236721=CARTESIAN_POINT('Ctrl Pts',(7.35580361962639,-2.96163149438161,
63.5204903009965));
#236722=CARTESIAN_POINT('Ctrl Pts',(7.13509633721601,-3.45970773442877,
63.4967404827161));
#236723=CARTESIAN_POINT('Ctrl Pts',(6.76173981293107,-4.11169516212418,
63.4653177398487));
#236724=CARTESIAN_POINT('Ctrl Pts',(6.65132737813032,-4.288007855659,63.4567666073274));
#236725=CARTESIAN_POINT('Ctrl Pts',(6.51446899673032,-4.488521630452,63.4469460817995));
#236726=CARTESIAN_POINT('Ctrl Pts',(6.49465540634456,-4.51714333560683,
63.4455418108436));
#236727=CARTESIAN_POINT('Ctrl Pts',(6.4652269591121,-4.55906026576051,63.4434815785605));
#236728=CARTESIAN_POINT('Ctrl Pts',(6.45575866501371,-4.57245778560391,
63.4428225343282));
#236729=CARTESIAN_POINT('Ctrl Pts',(6.43882889960544,-4.59625578493807,
63.4416508965721));
#236730=CARTESIAN_POINT('Ctrl Pts',(6.43138374031643,-4.60666777887235,
63.4411379515988));
#236731=CARTESIAN_POINT('Ctrl Pts',(6.41578064898209,-4.6283770202616,63.4400677498301));
#236732=CARTESIAN_POINT('Ctrl Pts',(6.40761806898652,-4.63967087852325,
63.4395105979607));
#236733=CARTESIAN_POINT('Ctrl Pts',(6.38653989593425,-4.66867321159473,
63.4380788212037));
#236734=CARTESIAN_POINT('Ctrl Pts',(6.37358044992413,-4.68634971520397,
63.4372051863992));
#236735=CARTESIAN_POINT('Ctrl Pts',(6.31813531142907,-4.76132070407994,
63.4334956269971));
#236736=CARTESIAN_POINT('Ctrl Pts',(6.27494889077715,-4.81809353198969,
63.4306759929381));
#236737=CARTESIAN_POINT('Ctrl Pts',(6.16251638105853,-4.96182095090556,
63.42350924253));
#236738=CARTESIAN_POINT('Ctrl Pts',(6.09219424850501,-5.04791494560045,
63.4191891293314));
#236739=CARTESIAN_POINT('Ctrl Pts',(5.88157056536384,-5.29496248111823,
63.4066978852439));
#236740=CARTESIAN_POINT('Ctrl Pts',(5.73653870245759,-5.45175459549485,
63.3986512425307));
#236741=CARTESIAN_POINT('Ctrl Pts',(5.2847659106428,-5.90214411618888,63.3749627627332));
#236742=CARTESIAN_POINT('Ctrl Pts',(4.96057340594551,-6.17711606949194,
63.3597493638944));
#236743=CARTESIAN_POINT('Ctrl Pts',(4.34783412448755,-6.61734113997531,
63.3320745106633));
#236744=CARTESIAN_POINT('Ctrl Pts',(4.06800329417708,-6.79295111586457,
63.3197635675601));
#236745=CARTESIAN_POINT('Ctrl Pts',(3.76149356967338,-6.95955761019976,
63.3058443043063));
#236746=CARTESIAN_POINT('Ctrl Pts',(3.74490748890894,-6.96849653047752,
63.3050897596108));
#236747=CARTESIAN_POINT('Ctrl Pts',(3.72212545680307,-6.98066987698059,
63.304051313161));
#236748=CARTESIAN_POINT('Ctrl Pts',(3.71595683018655,-6.98395551842405,
63.3037699324163));
#236749=CARTESIAN_POINT('Ctrl Pts',(3.70542622505697,-6.98954661138202,
63.3032892208275));
#236750=CARTESIAN_POINT('Ctrl Pts',(3.70106642277654,-6.9918561681456,63.3030900951225));
#236751=CARTESIAN_POINT('Ctrl Pts',(3.69260927855222,-6.99632611957984,
63.3027036221987));
#236752=CARTESIAN_POINT('Ctrl Pts',(3.6885121938096,-6.99848699731127,63.3025162995028));
#236753=CARTESIAN_POINT('Ctrl Pts',(3.67875456597198,-7.00362240079776,
63.3020699400994));
#236754=CARTESIAN_POINT('Ctrl Pts',(3.67309231547932,-7.00659366106113,
63.3018107373652));
#236755=CARTESIAN_POINT('Ctrl Pts',(3.65649026926341,-7.01527991253892,
63.3010501809444));
#236756=CARTESIAN_POINT('Ctrl Pts',(3.64554072945608,-7.02097615205138,
63.3005478612281));
#236757=CARTESIAN_POINT('Ctrl Pts',(3.62079133826501,-7.033777932925,63.2994107635638));
#236758=CARTESIAN_POINT('Ctrl Pts',(3.60698384511422,-7.04086851606291,
63.2987751977599));
#236759=CARTESIAN_POINT('Ctrl Pts',(3.56302228508351,-7.06328091069434,
63.2967475841615));
#236760=CARTESIAN_POINT('Ctrl Pts',(3.53279182429359,-7.07844946583242,
63.295347039574));
#236761=CARTESIAN_POINT('Ctrl Pts',(3.41031140286582,-7.13892568544084,
63.289649011473));
#236762=CARTESIAN_POINT('Ctrl Pts',(3.31728258414977,-7.18262616307382,
63.2852679933985));
#236763=CARTESIAN_POINT('Ctrl Pts',(3.03941027153567,-7.30660740985964,
63.2720774540956));
#236764=CARTESIAN_POINT('Ctrl Pts',(2.85232621806612,-7.38164984952312,
63.2630628956661));
#236765=CARTESIAN_POINT('Ctrl Pts',(2.46773212219431,-7.51911163645617,
63.2445108097419));
#236766=CARTESIAN_POINT('Ctrl Pts',(2.27021833357291,-7.58108487706883,
63.2349731810248));
#236767=CARTESIAN_POINT('Ctrl Pts',(1.81916341428423,-7.70340080464544,
63.2134207403243));
#236768=CARTESIAN_POINT('Ctrl Pts',(1.56460325517156,-7.75910833493442,
63.2014185806682));
#236769=CARTESIAN_POINT('Ctrl Pts',(0.834881445589659,-7.88142027242494,
63.1679151538222));
#236770=CARTESIAN_POINT('Ctrl Pts',(0.35574036248254,-7.91753495177006,
63.147043840901));
#236771=CARTESIAN_POINT('Ctrl Pts',(-0.155828194711189,-7.90953009500481,
63.1262136662988));
#236772=CARTESIAN_POINT('Ctrl Pts',(-0.187879696822543,-7.90883366874564,
63.12491429725));
#236773=CARTESIAN_POINT('Ctrl Pts',(-0.23202914836037,-7.90760583653871,
63.1231322284744));
#236774=CARTESIAN_POINT('Ctrl Pts',(-0.244131221362002,-7.90724146211114,
63.1226445372684));
#236775=CARTESIAN_POINT('Ctrl Pts',(-0.263407239634278,-7.90661679594143,
63.121869019027));
#236776=CARTESIAN_POINT('Ctrl Pts',(-0.270581726987097,-7.9063745206703,
63.121580653234));
#236777=CARTESIAN_POINT('Ctrl Pts',(-0.284540352484606,-7.90588412978552,
63.1210201539704));
#236778=CARTESIAN_POINT('Ctrl Pts',(-0.291324520084976,-7.90563704644275,
63.1207479898238));
#236779=CARTESIAN_POINT('Ctrl Pts',(-0.307552031188192,-7.90502511429534,
63.1200975764195));
#236780=CARTESIAN_POINT('Ctrl Pts',(-0.316995064710479,-7.90465207578622,
63.1197195726926));
#236781=CARTESIAN_POINT('Ctrl Pts',(-0.345310423768705,-7.90348268225755,
63.118587547154));
#236782=CARTESIAN_POINT('Ctrl Pts',(-0.364180647064771,-7.90263565273551,
63.1178350434298));
#236783=CARTESIAN_POINT('Ctrl Pts',(-0.528940873703219,-7.89464865451438,
63.1112812460149));
#236784=CARTESIAN_POINT('Ctrl Pts',(-0.674614125503046,-7.88353691317266,
63.1056002782559));
#236785=CARTESIAN_POINT('Ctrl Pts',(-1.23059885112246,-7.82560231641964,
63.0842897814308));
#236786=CARTESIAN_POINT('Ctrl Pts',(-1.63733325522774,-7.75071606027826,
63.0695147263373));
#236787=CARTESIAN_POINT('Ctrl Pts',(-2.13083361138616,-7.61925348107716,
63.0517066338229));
#236788=CARTESIAN_POINT('Ctrl Pts',(-2.22481279927818,-7.59234375462168,
63.0483186790001));
#236789=CARTESIAN_POINT('Ctrl Pts',(-2.56836552838068,-7.4870450350955,
63.0358962081762));
#236790=CARTESIAN_POINT('Ctrl Pts',(-2.81450281443147,-7.39803459814459,
63.0269267700972));
#236791=CARTESIAN_POINT('Ctrl Pts',(-3.42130712582622,-7.14392217001038,
63.0038838816257));
#236792=CARTESIAN_POINT('Ctrl Pts',(-3.7748223836862,-6.96359738829807,
62.9895666291405));
#236793=CARTESIAN_POINT('Ctrl Pts',(-4.13479609800248,-6.74448020904884,
62.9728232014384));
#236794=CARTESIAN_POINT('Ctrl Pts',(-4.15619181354347,-6.73131648732427,
62.971820274038));
#236795=CARTESIAN_POINT('Ctrl Pts',(-4.18574355174824,-6.71294016043397,
62.9704246304117));
#236796=CARTESIAN_POINT('Ctrl Pts',(-4.19395338992532,-6.70781407320363,
62.9700357853563));
#236797=CARTESIAN_POINT('Ctrl Pts',(-4.20706114099578,-6.69959633885935,
62.9694131936411));
#236798=CARTESIAN_POINT('Ctrl Pts',(-4.21196511642709,-6.69651434744451,
62.9691798687378));
#236799=CARTESIAN_POINT('Ctrl Pts',(-4.22153172220577,-6.69048737622925,
62.9687239344762));
#236800=CARTESIAN_POINT('Ctrl Pts',(-4.22619466705786,-6.68754290072226,
62.9685013468812));
#236801=CARTESIAN_POINT('Ctrl Pts',(-4.23739375870245,-6.68045470199821,
62.9679659025585));
#236802=CARTESIAN_POINT('Ctrl Pts',(-4.24392690555339,-6.67630626256486,
62.9676528457913));
#236803=CARTESIAN_POINT('Ctrl Pts',(-4.25752219552345,-6.66764546072879,
62.9669999443457));
#236804=CARTESIAN_POINT('Ctrl Pts',(-4.26458327482654,-6.66313145051145,
62.9666600312947));
#236805=CARTESIAN_POINT('Ctrl Pts',(-4.30680165549954,-6.63604746372577,
62.9646228786255));
#236806=CARTESIAN_POINT('Ctrl Pts',(-4.34178655075259,-6.61321071158007,
62.9629148000786));
#236807=CARTESIAN_POINT('Ctrl Pts',(-4.43693757067343,-6.5500194126596,
62.9582174495099));
#236808=CARTESIAN_POINT('Ctrl Pts',(-4.49673235460716,-6.50911415824023,
62.9552083411964));
#236809=CARTESIAN_POINT('Ctrl Pts',(-4.80376571761989,-6.29282449872205,
62.9394865049185));
#236810=CARTESIAN_POINT('Ctrl Pts',(-5.04133224417852,-6.10415977446242,
62.9264124402159));
#236811=CARTESIAN_POINT('Ctrl Pts',(-5.47447485390096,-5.71760592375576,
62.9013320093905));
#236812=CARTESIAN_POINT('Ctrl Pts',(-5.67161080174227,-5.52211260611122,
62.8893447842702));
#236813=CARTESIAN_POINT('Ctrl Pts',(-6.26986270417766,-4.86293970858322,
62.8513369290645));
#236814=CARTESIAN_POINT('Ctrl Pts',(-6.62755587378424,-4.36290146828069,
62.8261463124174));
#236815=CARTESIAN_POINT('Ctrl Pts',(-6.96576978193879,-3.75092595174726,
62.7977563571408));
#236816=CARTESIAN_POINT('Ctrl Pts',(-7.00634198489996,-3.67458382499478,
62.7942559518159));
#236817=CARTESIAN_POINT('Ctrl Pts',(-7.0602495353255,-3.5690093098751,62.789471352245));
#236818=CARTESIAN_POINT('Ctrl Pts',(-7.07467001517772,-3.54033828040014,
62.7881775800957));
#236819=CARTESIAN_POINT('Ctrl Pts',(-7.09912530616854,-3.49096976723562,
62.7859593714696));
#236820=CARTESIAN_POINT('Ctrl Pts',(-7.10924503446923,-3.47031483751352,
62.7850341544154));
#236821=CARTESIAN_POINT('Ctrl Pts',(-7.12993344383466,-3.42761835629211,
62.7831274353452));
#236822=CARTESIAN_POINT('Ctrl Pts',(-7.14049033714466,-3.40557135572353,
62.7821460549402));
#236823=CARTESIAN_POINT('Ctrl Pts',(-7.16114439327719,-3.36191919788908,
62.7802092004797));
#236824=CARTESIAN_POINT('Ctrl Pts',(-7.17124638279738,-3.3403166070579,
62.7792536884135));
#236825=CARTESIAN_POINT('Ctrl Pts',(-7.19441010128287,-3.29019275181924,
62.7770435189253));
#236826=CARTESIAN_POINT('Ctrl Pts',(-7.20740018771078,-3.26163878935312,
62.7757895847122));
#236827=CARTESIAN_POINT('Ctrl Pts',(-7.24061068202721,-3.18747038019025,
62.7725455988817));
#236828=CARTESIAN_POINT('Ctrl Pts',(-7.26057004381556,-3.14174046452932,
62.770558208481));
#236829=CARTESIAN_POINT('Ctrl Pts',(-7.39687529743503,-2.82120704187418,
62.7567143853091));
#236830=CARTESIAN_POINT('Ctrl Pts',(-7.49802459475522,-2.54019811410001,
62.7450275291352));
#236831=CARTESIAN_POINT('Ctrl Pts',(-7.71525783041505,-1.80941381150031,
62.7154074416694));
#236832=CARTESIAN_POINT('Ctrl Pts',(-7.80807617666539,-1.35392540913555,
62.6976887149269));
#236833=CARTESIAN_POINT('Ctrl Pts',(-7.86860920784648,-0.821062540347037,
62.6766127570459));
#236834=CARTESIAN_POINT('Ctrl Pts',(-7.8757884283724,-0.749073443795881,
62.6737571195273));
#236835=CARTESIAN_POINT('Ctrl Pts',(-7.88710793826565,-0.617285281893133,
62.6685050860276));
#236836=CARTESIAN_POINT('Ctrl Pts',(-7.89155790886853,-0.557518070914136,
62.6661141194771));
#236837=CARTESIAN_POINT('Ctrl Pts',(-7.89649509437854,-0.479197428151138,
62.6629651230745));
#236838=CARTESIAN_POINT('Ctrl Pts',(-7.8975967833046,-0.460684268224057,
62.6622196185075));
#236839=CARTESIAN_POINT('Ctrl Pts',(-7.89919993510043,-0.432046457029626,
62.6610644797303));
#236840=CARTESIAN_POINT('Ctrl Pts',(-7.89974705693606,-0.421924390696138,
62.66065582272));
#236841=CARTESIAN_POINT('Ctrl Pts',(-7.90079530384688,-0.401814113693694,
62.6598431448212));
#236842=CARTESIAN_POINT('Ctrl Pts',(-7.9012969467538,-0.391825948337949,
62.6594391360707));
#236843=CARTESIAN_POINT('Ctrl Pts',(-7.90224314638702,-0.372245175815101,
62.6586463530874));
#236844=CARTESIAN_POINT('Ctrl Pts',(-7.90268917938739,-0.362652656010148,
62.6582576128334));
#236845=CARTESIAN_POINT('Ctrl Pts',(-7.90364951877993,-0.341155774561508,
62.6573856093179));
#236846=CARTESIAN_POINT('Ctrl Pts',(-7.90415439594652,-0.329251063018407,
62.6569021269899));
#236847=CARTESIAN_POINT('Ctrl Pts',(-7.90536890445572,-0.298999329113977,
62.6556720296713));
#236848=CARTESIAN_POINT('Ctrl Pts',(-7.9060415591867,-0.28065098335316,
62.6549245682616));
#236849=CARTESIAN_POINT('Ctrl Pts',(-7.90953206395998,-0.175435025194458,
62.6506308328613));
#236850=CARTESIAN_POINT('Ctrl Pts',(-7.91098204786704,-0.0885293612401188,
62.6470549677864));
#236851=CARTESIAN_POINT('Ctrl Pts',(-7.91099983433237,-0.00161900995920416,
62.6434563298346));
#236852=CARTESIAN_POINT('',(-7.91119476205495,-0.00157576206492399,60.642331508237));
#236853=CARTESIAN_POINT('Ctrl Pts',(-7.91295189375223,-0.00166598417887076,
62.642331508237));
#236854=CARTESIAN_POINT('Ctrl Pts',(-7.911044428271,1.20131615954359,62.5937797499043));
#236855=CARTESIAN_POINT('Ctrl Pts',(-7.31720135608686,3.72124015044939,
62.4922432029633));
#236856=CARTESIAN_POINT('Ctrl Pts',(-3.88587637449001,7.80657458159615,
62.2847370788058));
#236857=CARTESIAN_POINT('Ctrl Pts',(3.49765847362659,8.67946754426088,62.0198131357647));
#236858=CARTESIAN_POINT('Ctrl Pts',(9.20349395763675,1.7300954411653,61.7019044041151));
#236859=CARTESIAN_POINT('Ctrl Pts',(6.8843891943671,-5.35210690193868,61.436980461074));
#236860=CARTESIAN_POINT('Ctrl Pts',(2.11872085160187,-7.94981861215979,
61.2250413066407));
#236861=CARTESIAN_POINT('Ctrl Pts',(-3.33448788563662,-8.06506802945827,
61.0131021522079));
#236862=CARTESIAN_POINT('Ctrl Pts',(-7.3506215263508,-4.4053455900463,60.8188655527398));
#236863=CARTESIAN_POINT('Ctrl Pts',(-7.9145503126708,-0.881728631901568,
60.6776137418802));
#236864=CARTESIAN_POINT('Ctrl Pts',(-7.91119476205495,-0.00157576206492399,
60.642331508237));
#236865=CARTESIAN_POINT('',(-7.911,2.06501482580279E-13,58.642331508237));
#236866=CARTESIAN_POINT('Ctrl Pts',(-7.911,1.51545442861334E-13,60.642331508237));
#236867=CARTESIAN_POINT('Ctrl Pts',(-7.91099999999996,2.20167589666687,
60.5537440725043));
#236868=CARTESIAN_POINT('Ctrl Pts',(-6.94214576672367,4.38610418338687,
60.4651566367716));
#236869=CARTESIAN_POINT('Ctrl Pts',(-3.67820201488288,7.3418068410763,60.2879817653061));
#236870=CARTESIAN_POINT('Ctrl Pts',(-1.40868175871752,8.08992666571334,
60.1993943295734));
#236871=CARTESIAN_POINT('Ctrl Pts',(2.97309270521258,7.65454228025262,60.022219458108));
#236872=CARTESIAN_POINT('Ctrl Pts',(5.05102072675584,6.47444880834238,59.9336320223752));
#236873=CARTESIAN_POINT('Ctrl Pts',(7.66951518847859,2.93425195367736,59.7564571509098));
#236874=CARTESIAN_POINT('Ctrl Pts',(8.18956872247067,0.601881960099537,
59.6678697151771));
#236875=CARTESIAN_POINT('Ctrl Pts',(7.32306689761363,-3.71537198232408,
59.4906948437116));
#236876=CARTESIAN_POINT('Ctrl Pts',(5.94329958850236,-5.66643518936472,
59.4021074079789));
#236877=CARTESIAN_POINT('Ctrl Pts',(2.16154501637906,-7.9220591323298,59.2249325365134));
#236878=CARTESIAN_POINT('Ctrl Pts',(-0.210816529299704,-8.20894963713003,
59.1363451007807));
#236879=CARTESIAN_POINT('Ctrl Pts',(-4.42123908576373,-6.91982244717871,
58.9591702293153));
#236880=CARTESIAN_POINT('Ctrl Pts',(-6.22631625634134,-5.35390358803581,
58.8705827935825));
#236881=CARTESIAN_POINT('Ctrl Pts',(-7.65317280859479,-2.31334857514567,
58.7354407413122));
#236882=CARTESIAN_POINT('Ctrl Pts',(-7.91100000000003,-1.15702837836533,
58.6888861247746));
#236883=CARTESIAN_POINT('Ctrl Pts',(-7.911,2.06501482580279E-13,58.642331508237));
#236884=CARTESIAN_POINT('',(-7.91885212407836,0.00556268397477262,56.6423315082371));
#236885=CARTESIAN_POINT('Ctrl Pts',(-7.91099992802374,0.00106714965019804,
58.642331508237));
#236886=CARTESIAN_POINT('Ctrl Pts',(-7.91096940833068,0.227315913889333,
58.6332491561257));
#236887=CARTESIAN_POINT('Ctrl Pts',(-7.90122887744838,0.453290643197541,
58.6241668040144));
#236888=CARTESIAN_POINT('Ctrl Pts',(-7.88187379827257,0.67822299290445,
58.615084451903));
#236889=CARTESIAN_POINT('Ctrl Pts',(-7.86241477327814,0.904363334426611,
58.6059533233172));
#236890=CARTESIAN_POINT('Ctrl Pts',(-7.83323770277879,1.12944994568909,
58.5968221947314));
#236891=CARTESIAN_POINT('Ctrl Pts',(-7.79449038791976,1.35271600590314,
58.5876910661456));
#236892=CARTESIAN_POINT('Ctrl Pts',(-7.75565473134637,1.57649110026798,
58.5785391190965));
#236893=CARTESIAN_POINT('Ctrl Pts',(-7.70720520429141,1.79843721837864,
58.5693871720473));
#236894=CARTESIAN_POINT('Ctrl Pts',(-7.64934062386123,2.01779806228132,
58.5602352249982));
#236895=CARTESIAN_POINT('Ctrl Pts',(-7.59135757699637,2.23760800469804,
58.5510645411237));
#236896=CARTESIAN_POINT('Ctrl Pts',(-7.52392093810813,2.45482196310906,
58.5418938572492));
#236897=CARTESIAN_POINT('Ctrl Pts',(-7.44728003336618,2.66869651789509,
58.5327231733748));
#236898=CARTESIAN_POINT('Ctrl Pts',(-7.41968444052939,2.7457049398585,58.5294211447898));
#236899=CARTESIAN_POINT('Ctrl Pts',(-7.39089601295679,2.82228059530343,
58.5261191162049));
#236900=CARTESIAN_POINT('Ctrl Pts',(-7.36092793096881,2.89838937948014,
58.5228170876199));
#236901=CARTESIAN_POINT('Ctrl Pts',(-7.28988374893415,3.0788175536841,58.5149890951589));
#236902=CARTESIAN_POINT('Ctrl Pts',(-7.21211428983778,3.2568539712332,58.5071611026978));
#236903=CARTESIAN_POINT('Ctrl Pts',(-7.12780410353066,3.4319571182769,58.4993331102368));
#236904=CARTESIAN_POINT('Ctrl Pts',(-7.04356512704589,3.60691237021398,
58.4915117294318));
#236905=CARTESIAN_POINT('Ctrl Pts',(-6.95279657486164,3.77893896953824,
58.4836903486268));
#236906=CARTESIAN_POINT('Ctrl Pts',(-6.85573177582579,3.94751349813177,
58.4758689678218));
#236907=CARTESIAN_POINT('Ctrl Pts',(-6.75873181828307,4.11597541510663,
58.4680528118771));
#236908=CARTESIAN_POINT('Ctrl Pts',(-6.65544416528475,4.28098955002536,
58.4602366559323));
#236909=CARTESIAN_POINT('Ctrl Pts',(-6.5461490106616,4.44205516964998,58.4524204999875));
#236910=CARTESIAN_POINT('Ctrl Pts',(-6.43690636184094,4.60304341274642,
58.4446080989534));
#236911=CARTESIAN_POINT('Ctrl Pts',(-6.32166215730543,4.76008662815491,
58.4367956979194));
#236912=CARTESIAN_POINT('Ctrl Pts',(-6.2007411113375,4.91271113237578,58.4289832968852));
#236913=CARTESIAN_POINT('Ctrl Pts',(-6.07985540926239,5.06529102613143,
58.4211731793301));
#236914=CARTESIAN_POINT('Ctrl Pts',(-5.95329639023129,5.21345450622929,
58.413363061775));
#236915=CARTESIAN_POINT('Ctrl Pts',(-5.82143053108722,5.35675905485076,
58.4055529442198));
#236916=CARTESIAN_POINT('Ctrl Pts',(-5.68955715861867,5.50007176853921,
58.3977423816674));
#236917=CARTESIAN_POINT('Ctrl Pts',(-5.55237657564755,5.63852473403909,
58.389931819115));
#236918=CARTESIAN_POINT('Ctrl Pts',(-5.41029407527172,5.77171023346458,
58.3821212565626));
#236919=CARTESIAN_POINT('Ctrl Pts',(-5.29957997260393,5.87549157893815,
58.3760350783068));
#236920=CARTESIAN_POINT('Ctrl Pts',(-5.18589028672745,5.97607523241643,
58.369948900051));
#236921=CARTESIAN_POINT('Ctrl Pts',(-5.06943163061923,6.07328444439063,
58.3638627217951));
#236922=CARTESIAN_POINT('Ctrl Pts',(-4.9040987450655,6.21128946741928,58.3552223557918));
#236923=CARTESIAN_POINT('Ctrl Pts',(-4.73326321401969,6.34242682809438,
58.3465819897885));
#236924=CARTESIAN_POINT('Ctrl Pts',(-4.55750201800622,6.46630469092427,
58.3379416237852));
#236925=CARTESIAN_POINT('Ctrl Pts',(-4.38144844489156,6.59038862341719,
58.329286884614));
#236926=CARTESIAN_POINT('Ctrl Pts',(-4.20045301627322,6.70718878691962,
58.3206321454429));
#236927=CARTESIAN_POINT('Ctrl Pts',(-4.01512042995576,6.81635745343155,
58.3119774062718));
#236928=CARTESIAN_POINT('Ctrl Pts',(-3.82405570793325,6.92890258828949,
58.3030549854133));
#236929=CARTESIAN_POINT('Ctrl Pts',(-3.62838151641226,7.03333651284979,
58.2941325645549));
#236930=CARTESIAN_POINT('Ctrl Pts',(-3.42878438433409,7.12933086942573,
58.2852101436964));
#236931=CARTESIAN_POINT('Ctrl Pts',(-3.23452569788872,7.22275775096684,
58.2765263628333));
#236932=CARTESIAN_POINT('Ctrl Pts',(-3.03655143037527,7.30819064082307,
58.2678425819702));
#236933=CARTESIAN_POINT('Ctrl Pts',(-2.83551318567347,7.3853764950659,58.259158801107));
#236934=CARTESIAN_POINT('Ctrl Pts',(-2.62618780777504,7.46574407951114,
58.2501170602509));
#236935=CARTESIAN_POINT('Ctrl Pts',(-2.41354078660347,7.53717026480837,
58.2410753193948));
#236936=CARTESIAN_POINT('Ctrl Pts',(-2.19832496958148,7.59942684207925,
58.2320335785387));
#236937=CARTESIAN_POINT('Ctrl Pts',(-1.9831091525595,7.66168341935013,58.2229918376826));
#236938=CARTESIAN_POINT('Ctrl Pts',(-1.76532481521441,7.71477034207186,
58.2139500968265));
#236939=CARTESIAN_POINT('Ctrl Pts',(-1.545738369841,7.75851879497635,58.2049083559704));
#236940=CARTESIAN_POINT('Ctrl Pts',(-1.3436316008017,7.79878475243088,58.1965863621979));
#236941=CARTESIAN_POINT('Ctrl Pts',(-1.13982650248577,7.83117396984472,
58.1882643684254));
#236942=CARTESIAN_POINT('Ctrl Pts',(-0.934949408664502,7.85555794347148,
58.1799423746529));
#236943=CARTESIAN_POINT('Ctrl Pts',(-0.730254536072288,7.87992022957056,
58.1716277826056));
#236944=CARTESIAN_POINT('Ctrl Pts',(-0.524489859309828,7.89629144106774,
58.1633131905582));
#236945=CARTESIAN_POINT('Ctrl Pts',(-0.31829045064656,7.90459437220072,
58.1549985985109));
#236946=CARTESIAN_POINT('Ctrl Pts',(-0.112261864260327,7.91289042491628,
58.1466908945412));
#236947=CARTESIAN_POINT('Ctrl Pts',(0.0942004442125806,7.91313151999478,
58.1383831905715));
#236948=CARTESIAN_POINT('Ctrl Pts',(0.300456894676682,7.90529231935425,
58.1300754866019));
#236949=CARTESIAN_POINT('Ctrl Pts',(0.506505241677638,7.89746102811387,
58.1217761647311));
#236950=CARTESIAN_POINT('Ctrl Pts',(0.71234785382415,7.88156572555374,58.1134768428604));
#236951=CARTESIAN_POINT('Ctrl Pts',(0.917345371216407,7.85763313408738,
58.1051775209896));
#236952=CARTESIAN_POINT('Ctrl Pts',(1.12221191552918,7.83371583317304,58.0968835015623));
#236953=CARTESIAN_POINT('Ctrl Pts',(1.32623415240593,7.80177151984718,58.0885894821349));
#236954=CARTESIAN_POINT('Ctrl Pts',(1.52877661383848,7.76187883601519,58.0802954627076));
#236955=CARTESIAN_POINT('Ctrl Pts',(1.73116887996143,7.72201573459252,58.0720075937083));
#236956=CARTESIAN_POINT('Ctrl Pts',(1.93208327441081,7.67421608263384,58.0637197247089));
#236957=CARTESIAN_POINT('Ctrl Pts',(2.13089277128065,7.61860991239897,58.0554318557095));
#236958=CARTESIAN_POINT('Ctrl Pts',(2.20667782066217,7.59741315659245,58.0522725671882));
#236959=CARTESIAN_POINT('Ctrl Pts',(2.28215710482043,7.57508257354178,58.0491132786669));
#236960=CARTESIAN_POINT('Ctrl Pts',(2.35729629640153,7.55162731939094,58.0459539901456));
#236961=CARTESIAN_POINT('Ctrl Pts',(2.54999823109176,7.49147398584543,58.0378516803192));
#236962=CARTESIAN_POINT('Ctrl Pts',(2.74038128870137,7.42394518745584,58.0297493704928));
#236963=CARTESIAN_POINT('Ctrl Pts',(2.92786907164504,7.34925191426341,58.0216470606664));
#236964=CARTESIAN_POINT('Ctrl Pts',(3.11539823756553,7.27454215450346,58.013542962469));
#236965=CARTESIAN_POINT('Ctrl Pts',(3.30003055800498,7.19266488408896,58.0054388642716));
#236966=CARTESIAN_POINT('Ctrl Pts',(3.48120979698936,7.10387917615054,57.9973347660743));
#236967=CARTESIAN_POINT('Ctrl Pts',(3.66245175319492,7.01506273404571,57.9892278625526));
#236968=CARTESIAN_POINT('Ctrl Pts',(3.84023795770216,6.91933322516687,57.981120959031));
#236969=CARTESIAN_POINT('Ctrl Pts',(4.01403644525848,6.81699584979606,57.9730140555094));
#236970=CARTESIAN_POINT('Ctrl Pts',(4.18799167277873,6.71456618158225,57.9648998407862));
#236971=CARTESIAN_POINT('Ctrl Pts',(4.35795172173338,6.60551690033114,57.956785626063));
#236972=CARTESIAN_POINT('Ctrl Pts',(4.52341217216975,6.49019747932731,57.9486714113399));
#236973=CARTESIAN_POINT('Ctrl Pts',(4.68895348846072,6.37482169800591,57.9405532309385));
#236974=CARTESIAN_POINT('Ctrl Pts',(4.84999056217602,6.25316985214359,57.9324350505371));
#236975=CARTESIAN_POINT('Ctrl Pts',(5.00605106612091,6.12563251618881,57.9243168701357));
#236976=CARTESIAN_POINT('Ctrl Pts',(5.16227939843205,5.99795802584719,57.9161899593962));
#236977=CARTESIAN_POINT('Ctrl Pts',(5.31352022438843,5.86438560526916,57.9080630486568));
#236978=CARTESIAN_POINT('Ctrl Pts',(5.45933613739997,5.72534452577998,57.8999361379174));
#236979=CARTESIAN_POINT('Ctrl Pts',(5.53670664146746,5.65156877535613,57.8956239667185));
#236980=CARTESIAN_POINT('Ctrl Pts',(5.61255044765232,5.57625398609848,57.8913117955197));
#236981=CARTESIAN_POINT('Ctrl Pts',(5.6868066934775,5.49946821347478,57.8869996243208));
#236982=CARTESIAN_POINT('Ctrl Pts',(5.8245298280504,5.35705356297878,57.8790018360174));
#236983=CARTESIAN_POINT('Ctrl Pts',(5.95702851641505,5.20932963798965,57.8710040477139));
#236984=CARTESIAN_POINT('Ctrl Pts',(6.08387878431521,5.05671236454668,57.8630062594104));
#236985=CARTESIAN_POINT('Ctrl Pts',(6.21062547912626,4.90421970292144,57.8550150012914));
#236986=CARTESIAN_POINT('Ctrl Pts',(6.33173273167485,4.74684191120925,57.8470237431723));
#236987=CARTESIAN_POINT('Ctrl Pts',(6.44681411763098,4.58503094130387,57.8390324850533));
#236988=CARTESIAN_POINT('Ctrl Pts',(6.56182105441875,4.42332465116092,57.8310463966888));
#236989=CARTESIAN_POINT('Ctrl Pts',(6.67080970098743,4.25719117061807,57.8230603083243));
#236990=CARTESIAN_POINT('Ctrl Pts',(6.77343431023401,4.08711495372282,57.8150742199598));
#236991=CARTESIAN_POINT('Ctrl Pts',(6.87600992375256,3.91711993575374,57.8070919443671));
#236992=CARTESIAN_POINT('Ctrl Pts',(6.97222738389496,3.74318621947823,57.7991096687743));
#236993=CARTESIAN_POINT('Ctrl Pts',(7.06178441053314,3.56582696427506,57.7911273931816));
#236994=CARTESIAN_POINT('Ctrl Pts',(7.15131385511121,3.38852233274378,57.7831475759957));
#236995=CARTESIAN_POINT('Ctrl Pts',(7.23418680508977,3.20779456389923,57.7751677588098));
#236996=CARTESIAN_POINT('Ctrl Pts',(7.31014687583093,3.02418148492767,57.7671879416239));
#236997=CARTESIAN_POINT('Ctrl Pts',(7.38871731538235,2.83425854013018,57.7589338979176));
#236998=CARTESIAN_POINT('Ctrl Pts',(7.45989114022406,2.64124878708016,57.7506798542112));
#236999=CARTESIAN_POINT('Ctrl Pts',(7.52343851156297,2.44577062757961,57.7424258105049));
#237000=CARTESIAN_POINT('Ctrl Pts',(7.58488293844788,2.25676133850973,57.7344449141384));
#237001=CARTESIAN_POINT('Ctrl Pts',(7.63919749948067,2.06544473941621,57.7264640177718));
#237002=CARTESIAN_POINT('Ctrl Pts',(7.68622497097408,1.87239597723734,57.7184831214053));
#237003=CARTESIAN_POINT('Ctrl Pts',(7.73326288316665,1.67930435576819,57.7105004531779));
#237004=CARTESIAN_POINT('Ctrl Pts',(7.77301040096005,1.4844801297399,57.7025177849505));
#237005=CARTESIAN_POINT('Ctrl Pts',(7.80536120397024,1.28850978869243,57.6945351167231));
#237006=CARTESIAN_POINT('Ctrl Pts',(7.83772416213384,1.0924658157924,57.6865494491711));
#237007=CARTESIAN_POINT('Ctrl Pts',(7.86268481042211,0.895275199482527,
57.6785637816192));
#237008=CARTESIAN_POINT('Ctrl Pts',(7.88018853644928,0.697531096090645,
57.6705781140673));
#237009=CARTESIAN_POINT('Ctrl Pts',(7.89770153022582,0.499682292545889,
57.6625882183204));
#237010=CARTESIAN_POINT('Ctrl Pts',(7.90774970095625,0.301279750613616,
57.6545983225735));
#237011=CARTESIAN_POINT('Ctrl Pts',(7.91033050948413,0.102918563556239,
57.6466084268267));
#237012=CARTESIAN_POINT('Ctrl Pts',(7.91291437519276,-0.0956775987018777,
57.6386090663887));
#237013=CARTESIAN_POINT('Ctrl Pts',(7.9080132038404,-0.294231973617734,
57.6306097059508));
#237014=CARTESIAN_POINT('Ctrl Pts',(7.8956765394065,-0.492151384297384,
57.6226103455129));
#237015=CARTESIAN_POINT('Ctrl Pts',(7.88333125094898,-0.69020915179793,
57.6146053930712));
#237016=CARTESIAN_POINT('Ctrl Pts',(7.86354013599447,-0.887630737857427,
57.6066004406296));
#237017=CARTESIAN_POINT('Ctrl Pts',(7.83640427237677,-1.08383074318602,
57.5985954881879));
#237018=CARTESIAN_POINT('Ctrl Pts',(7.80923299424253,-1.28028680553311,
57.5905800886301));
#237019=CARTESIAN_POINT('Ctrl Pts',(7.77469787875517,-1.47551777435169,
57.5825646890722));
#237020=CARTESIAN_POINT('Ctrl Pts',(7.73295074651253,-1.66894989499725,
57.5745492895143));
#237021=CARTESIAN_POINT('Ctrl Pts',(7.72347430418865,-1.71285826034864,
57.5727298239));
#237022=CARTESIAN_POINT('Ctrl Pts',(7.71362644739048,-1.75667400383091,
57.5709103582857));
#237023=CARTESIAN_POINT('Ctrl Pts',(7.70340930374815,-1.80039054066789,
57.5690908926713));
#237024=CARTESIAN_POINT('Ctrl Pts',(7.65982881545839,-1.98686027119019,
57.5613300935013));
#237025=CARTESIAN_POINT('Ctrl Pts',(7.60939621414596,-2.17207776286606,
57.5535692943313));
#237026=CARTESIAN_POINT('Ctrl Pts',(7.55219166053658,-2.35548766129687,
57.5458084951612));
#237027=CARTESIAN_POINT('Ctrl Pts',(7.49505655269008,-2.53867490192314,
57.5380571175247));
#237028=CARTESIAN_POINT('Ctrl Pts',(7.43116596132914,-2.72005857897147,
57.5303057398882));
#237029=CARTESIAN_POINT('Ctrl Pts',(7.36065130442519,-2.89909181894326,
57.5225543622517));
#237030=CARTESIAN_POINT('Ctrl Pts',(7.29020793793713,-3.07794405606126,
57.5148108212687));
#237031=CARTESIAN_POINT('Ctrl Pts',(7.21315396760143,-3.25445025561536,
57.5070672802857));
#237032=CARTESIAN_POINT('Ctrl Pts',(7.12967105811057,-3.42807695408672,
57.4993237393028));
#237033=CARTESIAN_POINT('Ctrl Pts',(7.04625562909086,-3.60156330752832,
57.4915864575385));
#237034=CARTESIAN_POINT('Ctrl Pts',(6.95642176167249,-3.77217447228026,
57.4838491757743));
#237035=CARTESIAN_POINT('Ctrl Pts',(6.86039987431697,-3.93939520287971,
57.4761118940101));
#237036=CARTESIAN_POINT('Ctrl Pts',(6.76443616110939,-4.10651462404036,
57.4683792998207));
#237037=CARTESIAN_POINT('Ctrl Pts',(6.66229207125565,-4.27024739094581,
57.4606467056312));
#237038=CARTESIAN_POINT('Ctrl Pts',(6.55424481595404,-4.43010111538547,
57.4529141114417));
#237039=CARTESIAN_POINT('Ctrl Pts',(6.44624115950998,-4.58989033619899,
57.4451846374821));
#237040=CARTESIAN_POINT('Ctrl Pts',(6.33233928253398,-4.74580333503905,
57.4374551635225));
#237041=CARTESIAN_POINT('Ctrl Pts',(6.21286077897892,-4.89737500514566,
57.4297256895629));
#237042=CARTESIAN_POINT('Ctrl Pts',(6.09338420221705,-5.04894423090243,
57.4219963402542));
#237043=CARTESIAN_POINT('Ctrl Pts',(5.96833139152503,-5.19617197859636,
57.4142669909454));
#237044=CARTESIAN_POINT('Ctrl Pts',(5.83806569384948,-5.33862435036384,
57.4065376416367));
#237045=CARTESIAN_POINT('Ctrl Pts',(5.70779472968696,-5.48108248131102,
57.3988079798395));
#237046=CARTESIAN_POINT('Ctrl Pts',(5.57231070061897,-5.61876458601279,
57.3910783180424));
#237047=CARTESIAN_POINT('Ctrl Pts',(5.43201534467499,-5.75127205887667,
57.3833486562453));
#237048=CARTESIAN_POINT('Ctrl Pts',(5.29168860988826,-5.88380916872407,
57.3756172656108));
#237049=CARTESIAN_POINT('Ctrl Pts',(5.14654866637825,-6.01116909522465,
57.3678858749764));
#237050=CARTESIAN_POINT('Ctrl Pts',(4.99703202626331,-6.1329920861272,57.360154484342));
#237051=CARTESIAN_POINT('Ctrl Pts',(4.84745453975904,-6.25486465337876,
57.3524199473875));
#237052=CARTESIAN_POINT('Ctrl Pts',(4.69349708817789,-6.37119557151886,
57.3446854104331));
#237053=CARTESIAN_POINT('Ctrl Pts',(4.5356270033007,-6.48166712250247,57.3369508734786));
#237054=CARTESIAN_POINT('Ctrl Pts',(4.37757100220106,-6.59226877066988,
57.3292072279213));
#237055=CARTESIAN_POINT('Ctrl Pts',(4.21559345993335,-6.69699706499938,
57.3214635823641));
#237056=CARTESIAN_POINT('Ctrl Pts',(4.05018915375438,-6.79557862281134,
57.3137199368068));
#237057=CARTESIAN_POINT('Ctrl Pts',(3.88467887056285,-6.89422334330164,
57.30597132978));
#237058=CARTESIAN_POINT('Ctrl Pts',(3.71573776374398,-6.9867133106257,57.2982227227533));
#237059=CARTESIAN_POINT('Ctrl Pts',(3.54388251592853,-7.07282247149581,
57.2904741157265));
#237060=CARTESIAN_POINT('Ctrl Pts',(3.37176687433982,-7.15906210431598,
57.2827137680689));
#237061=CARTESIAN_POINT('Ctrl Pts',(3.19672859841029,-7.23890147297845,
57.2749534204113));
#237062=CARTESIAN_POINT('Ctrl Pts',(3.01930264737507,-7.31216332719352,
57.2671930727537));
#237063=CARTESIAN_POINT('Ctrl Pts',(2.89728271706964,-7.36254719884934,
57.2618561021764));
#237064=CARTESIAN_POINT('Ctrl Pts',(2.77413383706884,-7.40982118990013,
57.2565191315991));
#237065=CARTESIAN_POINT('Ctrl Pts',(2.65003307283612,-7.45394162258297,
57.2511821610218));
#237066=CARTESIAN_POINT('Ctrl Pts',(2.46600626720784,-7.51936702378625,
57.2432680627231));
#237067=CARTESIAN_POINT('Ctrl Pts',(2.27929511676439,-7.57806579485747,
57.2353539644245));
#237068=CARTESIAN_POINT('Ctrl Pts',(2.09043302669929,-7.62981066350174,
57.2274398661259));
#237069=CARTESIAN_POINT('Ctrl Pts',(1.90178780376386,-7.68149611439238,
57.2195348554519));
#237070=CARTESIAN_POINT('Ctrl Pts',(1.71099689002177,-7.72624347717776,
57.2116298447778));
#237071=CARTESIAN_POINT('Ctrl Pts',(1.51861292999975,-7.7638737604908,57.2037248341038));
#237072=CARTESIAN_POINT('Ctrl Pts',(1.32641414860508,-7.80146782288288,
57.1958274323751));
#237073=CARTESIAN_POINT('Ctrl Pts',(1.13262571155332,-7.83195838650878,
57.1879300306464));
#237074=CARTESIAN_POINT('Ctrl Pts',(0.937814939473485,-7.85521636489412,
57.1800326289177));
#237075=CARTESIAN_POINT('Ctrl Pts',(0.74315551126932,-7.8784562747068,57.1721413624933));
#237076=CARTESIAN_POINT('Ctrl Pts',(0.547475671210005,-7.89447475287415,
57.164250096069));
#237077=CARTESIAN_POINT('Ctrl Pts',(0.351352718647428,-7.90319380169176,
57.1563588296447));
#237078=CARTESIAN_POINT('Ctrl Pts',(0.155345724235176,-7.91190769535155,
57.1484722289499));
#237079=CARTESIAN_POINT('Ctrl Pts',(-0.0411035170795087,-7.91333074393357,
57.1405856282551));
#237080=CARTESIAN_POINT('Ctrl Pts',(-0.237412516086123,-7.90743677162237,
57.1326990275604));
#237081=CARTESIAN_POINT('Ctrl Pts',(-0.433641879939017,-7.90154519027335,
57.1248156261619));
#237082=CARTESIAN_POINT('Ctrl Pts',(-0.629730770656352,-7.88834251389541,
57.1169322247635));
#237083=CARTESIAN_POINT('Ctrl Pts',(-0.825096346086271,-7.86785466437167,
57.109048823365));
#237084=CARTESIAN_POINT('Ctrl Pts',(-1.02044628527462,-7.84736845460952,
57.101166052921));
#237085=CARTESIAN_POINT('Ctrl Pts',(-1.21507268094227,-7.81959826266944,
57.0932832824769));
#237086=CARTESIAN_POINT('Ctrl Pts',(-1.40839693655226,-7.7846219605778,
57.0854005120329));
#237087=CARTESIAN_POINT('Ctrl Pts',(-1.60172168115791,-7.74964557001688,
57.0775177216501));
#237088=CARTESIAN_POINT('Ctrl Pts',(-1.79374393951702,-7.70746309385163,
57.0696349312673));
#237089=CARTESIAN_POINT('Ctrl Pts',(-1.9838943476887,-7.65820372001221,
57.0617521408846));
#237090=CARTESIAN_POINT('Ctrl Pts',(-2.17407721358866,-7.60893593784285,
57.0538680049487));
#237091=CARTESIAN_POINT('Ctrl Pts',(-2.36238725867034,-7.55258893756365,
57.0459838690128));
#237092=CARTESIAN_POINT('Ctrl Pts',(-2.54826910623883,-7.48934213146847,
57.038099733077));
#237093=CARTESIAN_POINT('Ctrl Pts',(-2.73421394201501,-7.42607389346368,
57.0302129255107));
#237094=CARTESIAN_POINT('Ctrl Pts',(-2.91772861443998,-7.3559013021761,
57.0223261179445));
#237095=CARTESIAN_POINT('Ctrl Pts',(-3.09827636154169,-7.27905245121314,
57.0144393103783));
#237096=CARTESIAN_POINT('Ctrl Pts',(-3.27900053039043,-7.20212850760149,
57.0065447962391));
#237097=CARTESIAN_POINT('Ctrl Pts',(-3.45675166563389,-7.11851540902328,
56.9986502821));
#237098=CARTESIAN_POINT('Ctrl Pts',(-3.63101535873538,-7.02848834847351,
56.9907557679609));
#237099=CARTESIAN_POINT('Ctrl Pts',(-3.80537650642813,-6.93841094151919,
56.9828568389226));
#237100=CARTESIAN_POINT('Ctrl Pts',(-3.97624602381833,-6.84191259040028,
56.9749579098842));
#237101=CARTESIAN_POINT('Ctrl Pts',(-4.14313703997129,-6.73931275932628,
56.9670589808458));
#237102=CARTESIAN_POINT('Ctrl Pts',(-4.31023184716961,-6.63658764333694,
56.9591504064051));
#237103=CARTESIAN_POINT('Ctrl Pts',(-4.47333816303147,-6.52774635631258,
56.9512418319643));
#237104=CARTESIAN_POINT('Ctrl Pts',(-4.63199996408114,-6.41315034384446,
56.9433332575236));
#237105=CARTESIAN_POINT('Ctrl Pts',(-4.69927337998713,-6.36456104788958,
56.9399799814732));
#237106=CARTESIAN_POINT('Ctrl Pts',(-4.76574818354377,-6.31493764713479,
56.9366267054228));
#237107=CARTESIAN_POINT('Ctrl Pts',(-4.83139155477593,-6.26430975003949,
56.9332734293723));
#237108=CARTESIAN_POINT('Ctrl Pts',(-4.99962145197458,-6.13456129617652,
56.9246797012525));
#237109=CARTESIAN_POINT('Ctrl Pts',(-5.16272509822018,-5.99795315184645,
56.9160859731326));
#237110=CARTESIAN_POINT('Ctrl Pts',(-5.32016110145686,-5.85489597299092,
56.9074922450127));
#237111=CARTESIAN_POINT('Ctrl Pts',(-5.47736979429696,-5.71204534399306,
56.898910924752));
#237112=CARTESIAN_POINT('Ctrl Pts',(-5.62892699136269,-5.56276442911684,
56.8903296044912));
#237113=CARTESIAN_POINT('Ctrl Pts',(-5.77432430049551,-5.40750403353591,
56.8817482842305));
#237114=CARTESIAN_POINT('Ctrl Pts',(-5.92600958060508,-5.24552911987293,
56.8727958491736));
#237115=CARTESIAN_POINT('Ctrl Pts',(-6.07099014928944,-5.07704620370147,
56.8638434141167));
#237116=CARTESIAN_POINT('Ctrl Pts',(-6.20872801391771,-4.90261332854157,
56.8548909790597));
#237117=CARTESIAN_POINT('Ctrl Pts',(-6.3402359125913,-4.7360701565984,56.8463434679921));
#237118=CARTESIAN_POINT('Ctrl Pts',(-6.46514155792974,-4.56410355985527,
56.8377959569244));
#237119=CARTESIAN_POINT('Ctrl Pts',(-6.58301392637842,-4.38723701720204,
56.8292484458567));
#237120=CARTESIAN_POINT('Ctrl Pts',(-6.70070507568962,-4.21064239240987,
56.8207140758891));
#237121=CARTESIAN_POINT('Ctrl Pts',(-6.81138438193963,-4.02916305574041,
56.8121797059214));
#237122=CARTESIAN_POINT('Ctrl Pts',(-6.91466186145532,-3.84335430863916,
56.8036453359538));
#237123=CARTESIAN_POINT('Ctrl Pts',(-7.01771448227365,-3.65795010968363,
56.7951295472618));
#237124=CARTESIAN_POINT('Ctrl Pts',(-7.11339731274083,-3.46823552599294,
56.7866137585697));
#237125=CARTESIAN_POINT('Ctrl Pts',(-7.20136432801631,-3.27479355306166,
56.7780979698777));
#237126=CARTESIAN_POINT('Ctrl Pts',(-7.21437620211279,-3.2461800711915,
56.7768383344343));
#237127=CARTESIAN_POINT('Ctrl Pts',(-7.22721933351794,-3.21748508828331,
56.7755786989909));
#237128=CARTESIAN_POINT('Ctrl Pts',(-7.23989268275838,-3.18871054536809,
56.7743190635475));
#237129=CARTESIAN_POINT('Ctrl Pts',(-7.31699601980963,-3.0136492226825,
56.7666555726807));
#237130=CARTESIAN_POINT('Ctrl Pts',(-7.38775912880493,-2.83575951975293,
56.7589920818139));
#237131=CARTESIAN_POINT('Ctrl Pts',(-7.45197484386047,-2.6555586844336,
56.7513285909471));
#237132=CARTESIAN_POINT('Ctrl Pts',(-7.51619454488105,-2.47534666378014,
56.743664624396));
#237133=CARTESIAN_POINT('Ctrl Pts',(-7.57386592148028,-2.29282356988889,
56.7360006578449));
#237134=CARTESIAN_POINT('Ctrl Pts',(-7.62483108905492,-2.10852362172718,
56.7283366912939));
#237135=CARTESIAN_POINT('Ctrl Pts',(-7.6758306922615,-1.92409914762978,
56.7206675464309));
#237136=CARTESIAN_POINT('Ctrl Pts',(-7.72011493821241,-1.73789577386895,
56.712998401568));
#237137=CARTESIAN_POINT('Ctrl Pts',(-7.75757652038701,-1.55046042527379,
56.705329256705));
#237138=CARTESIAN_POINT('Ctrl Pts',(-7.79505129506646,-1.3629590692758,
56.6976574110691));
#237139=CARTESIAN_POINT('Ctrl Pts',(-7.82569856089014,-1.17422523459191,
56.6899855654331));
#237140=CARTESIAN_POINT('Ctrl Pts',(-7.84946272487774,-0.98481263738586,
56.6823137197972));
#237141=CARTESIAN_POINT('Ctrl Pts',(-7.87325307651349,-0.795191311168729,
56.674633419936));
#237142=CARTESIAN_POINT('Ctrl Pts',(-7.89014514416397,-0.604890092031874,
56.6669531200748));
#237143=CARTESIAN_POINT('Ctrl Pts',(-7.90013541291234,-0.414465267119512,
56.6592728202137));
#237144=CARTESIAN_POINT('Ctrl Pts',(-7.90748097070979,-0.274451360317271,
56.6536257162215));
#237145=CARTESIAN_POINT('Ctrl Pts',(-7.91109634198683,-0.134370668405158,
56.6479786122293));
#237146=CARTESIAN_POINT('Ctrl Pts',(-7.91099804815405,0.00555716679354367,
56.6423315082371));
#237147=CARTESIAN_POINT('',(-7.91503681196177,-0.00538689920117852,54.6423315082371));
#237148=CARTESIAN_POINT('Ctrl Pts',(-7.9196338726488,0.00556323312257564,
56.6423315082371));
#237149=CARTESIAN_POINT('Ctrl Pts',(-7.92037954994029,0.228541081453708,
56.633342571399));
#237150=CARTESIAN_POINT('Ctrl Pts',(-7.91127946851613,0.451321298709539,
56.6243536345609));
#237151=CARTESIAN_POINT('Ctrl Pts',(-7.66531770480111,3.28740455581408,
56.5093951205063));
#237152=CARTESIAN_POINT('Ctrl Pts',(-5.21295917794468,6.99651976617628,
56.3504407546814));
#237153=CARTESIAN_POINT('Ctrl Pts',(0.108828255203027,8.23489439458598,
56.1385016002485));
#237154=CARTESIAN_POINT('Ctrl Pts',(4.03755664298072,7.19823663329124,55.9795472344238));
#237155=CARTESIAN_POINT('Ctrl Pts',(6.97493635397154,4.37898776636411,55.8205928685989));
#237156=CARTESIAN_POINT('Ctrl Pts',(8.6839076066132,-0.795229888551257,
55.6086537141659));
#237157=CARTESIAN_POINT('Ctrl Pts',(5.54732397292391,-7.53617730613503,
55.3437297711246));
#237158=CARTESIAN_POINT('Ctrl Pts',(-3.36342892092028,-8.73984422959885,
55.0258210394751));
#237159=CARTESIAN_POINT('Ctrl Pts',(-7.60611129338621,-3.71462797172983,
54.7920216185127));
#237160=CARTESIAN_POINT('Ctrl Pts',(-7.91792072111909,-0.547831146367218,
54.6641917747666));
#237161=CARTESIAN_POINT('Ctrl Pts',(-7.91503681196177,-0.00538689920117852,
54.6423315082371));
#237162=CARTESIAN_POINT('',(-7.89592422791155,-0.00169916443013902,52.6419012676071));
#237163=CARTESIAN_POINT('Ctrl Pts',(-7.91503681196177,-0.00538689920117852,
54.6423315082371));
#237164=CARTESIAN_POINT('Ctrl Pts',(-7.91093071864774,0.766942108068054,
54.6112069861583));
#237165=CARTESIAN_POINT('Ctrl Pts',(-7.59192480626818,2.8589101804051,54.5270976754714));
#237166=CARTESIAN_POINT('Ctrl Pts',(-5.11028731654404,7.07453852357992,
54.3370187875679));
#237167=CARTESIAN_POINT('Ctrl Pts',(0.58978711048592,8.70507802341358,54.1250796331348));
#237168=CARTESIAN_POINT('Ctrl Pts',(5.43791012976232,6.18501921579411,53.9131404787019));
#237169=CARTESIAN_POINT('Ctrl Pts',(7.74829280852149,2.84261021379085,53.754186112877));
#237170=CARTESIAN_POINT('Ctrl Pts',(8.14634157535645,-1.20929315616148,
53.5952317470524));
#237171=CARTESIAN_POINT('Ctrl Pts',(6.07974643190811,-6.25134587265489,
53.3832925926191));
#237172=CARTESIAN_POINT('Ctrl Pts',(-0.686725509353473,-9.33247982718465,
53.1183686495784));
#237173=CARTESIAN_POINT('Ctrl Pts',(-6.97348851421393,-5.26974137332134,
52.8537204811401));
#237174=CARTESIAN_POINT('Ctrl Pts',(-7.8979285753281,-1.31578168274657,
52.6950418899188));
#237175=CARTESIAN_POINT('Ctrl Pts',(-7.89517691866717,-0.00168164862291708,
52.6423328759138));
#237176=CARTESIAN_POINT('',(-7.91099629000672,-0.00766153195038582,48.6489215596253));
#237177=CARTESIAN_POINT('Ctrl Pts',(-7.91099973373757,-0.00205251166330671,
52.6331944121903));
#237178=CARTESIAN_POINT('Ctrl Pts',(-7.911012932558,0.048819727856465,52.6310900189783));
#237179=CARTESIAN_POINT('Ctrl Pts',(-7.91053542539201,0.099691711568022,
52.6290015797071));
#237180=CARTESIAN_POINT('Ctrl Pts',(-7.9089841469533,0.181189019281594,
52.6256809048648));
#237181=CARTESIAN_POINT('Ctrl Pts',(-7.90822311057975,0.211818222793782,
52.6244385547084));
#237182=CARTESIAN_POINT('Ctrl Pts',(-7.90695085357179,0.253313005621773,
52.6227630283582));
#237183=CARTESIAN_POINT('Ctrl Pts',(-7.90659513898706,0.264182870437372,
52.6223248131627));
#237184=CARTESIAN_POINT('Ctrl Pts',(-7.90595353200988,0.282625506951483,
52.6215824858392));
#237185=CARTESIAN_POINT('Ctrl Pts',(-7.90567917209676,0.290198648831562,
52.6212780004511));
#237186=CARTESIAN_POINT('Ctrl Pts',(-7.90515089134796,0.304223727932115,
52.6207147319171));
#237187=CARTESIAN_POINT('Ctrl Pts',(-7.90489995253835,0.310675767063107,
52.6204558524761));
#237188=CARTESIAN_POINT('Ctrl Pts',(-7.90438181296186,0.323590785070841,
52.6199381414412));
#237189=CARTESIAN_POINT('Ctrl Pts',(-7.90411458409236,0.330053757846875,
52.6196793109632));
#237190=CARTESIAN_POINT('Ctrl Pts',(-7.90347797628165,0.345005914195665,
52.619081065922));
#237191=CARTESIAN_POINT('Ctrl Pts',(-7.90310284587809,0.353494852114456,
52.6187418374667));
#237192=CARTESIAN_POINT('Ctrl Pts',(-7.90212204759867,0.374907361350196,
52.6178872178594));
#237193=CARTESIAN_POINT('Ctrl Pts',(-7.90149835139332,0.387830104258191,
52.6173724089325));
#237194=CARTESIAN_POINT('Ctrl Pts',(-7.89800117210295,0.456777265173465,
52.6146308309875));
#237195=CARTESIAN_POINT('Ctrl Pts',(-7.89456350284564,0.512772124101357,
52.6124222693121));
#237196=CARTESIAN_POINT('Ctrl Pts',(-7.88765463965521,0.608625931688615,
52.6086707946328));
#237197=CARTESIAN_POINT('Ctrl Pts',(-7.88447618195296,0.648503380186446,
52.607118765331));
#237198=CARTESIAN_POINT('Ctrl Pts',(-7.80108588307536,1.60324068771695,
52.5701585682059));
#237199=CARTESIAN_POINT('Ctrl Pts',(-7.56252295257933,2.49704936280296,
52.5409320553595));
#237200=CARTESIAN_POINT('Ctrl Pts',(-7.14668627840421,3.3931778602967,52.5051186023916));
#237201=CARTESIAN_POINT('Ctrl Pts',(-7.11650863425822,3.45602160025433,
52.502564424753));
#237202=CARTESIAN_POINT('Ctrl Pts',(-7.01475458183899,3.66093494270624,
52.4940712254409));
#237203=CARTESIAN_POINT('Ctrl Pts',(-6.93972760594997,3.80123753006522,
52.4879826079628));
#237204=CARTESIAN_POINT('Ctrl Pts',(-6.84545460471771,3.96542398621287,
52.4804634148356));
#237205=CARTESIAN_POINT('Ctrl Pts',(-6.83024115713981,3.99157134927366,
52.479254570032));
#237206=CARTESIAN_POINT('Ctrl Pts',(-6.80987565222271,4.02611619720566,
52.4776428955779));
#237207=CARTESIAN_POINT('Ctrl Pts',(-6.80485721505982,4.03459245942312,
52.4772462677514));
#237208=CARTESIAN_POINT('Ctrl Pts',(-6.79659298336621,4.04849166503751,
52.4765939828554));
#237209=CARTESIAN_POINT('Ctrl Pts',(-6.79335648938684,4.05392014613352,
52.4763387485088));
#237210=CARTESIAN_POINT('Ctrl Pts',(-6.78707359918654,4.06442961019123,
52.4758436994921));
#237211=CARTESIAN_POINT('Ctrl Pts',(-6.78402799294279,4.06951106248642,
52.475603920298));
#237212=CARTESIAN_POINT('Ctrl Pts',(-6.77698473842869,4.0812325253682,52.4750498616678));
#237213=CARTESIAN_POINT('Ctrl Pts',(-6.7729830379271,4.08787008580662,52.474735403034));
#237214=CARTESIAN_POINT('Ctrl Pts',(-6.76222473104568,4.1056555645672,52.4738909179498));
#237215=CARTESIAN_POINT('Ctrl Pts',(-6.75545032984012,4.11679265528246,
52.4733601178916));
#237216=CARTESIAN_POINT('Ctrl Pts',(-6.70742396134459,4.19531007673991,
52.4696040721258));
#237217=CARTESIAN_POINT('Ctrl Pts',(-6.66519295747925,4.26208460462532,
52.4663375849493));
#237218=CARTESIAN_POINT('Ctrl Pts',(-6.25122656140715,4.89543429045929,
52.4347230442141));
#237219=CARTESIAN_POINT('Ctrl Pts',(-5.80914108662441,5.4126731407887,52.4042669191825));
#237220=CARTESIAN_POINT('Ctrl Pts',(-5.02563446170886,6.12130554842635,
52.3587522616422));
#237221=CARTESIAN_POINT('Ctrl Pts',(-4.7268268451441,6.35488160224629,52.3428268930438));
#237222=CARTESIAN_POINT('Ctrl Pts',(-4.35455564355918,6.60504552102741,
52.3245429351046));
#237223=CARTESIAN_POINT('Ctrl Pts',(-4.29617994775286,6.6431633425181,52.3217170935278));
#237224=CARTESIAN_POINT('Ctrl Pts',(-4.21856134272978,6.6923952365298,52.3180118225116));
#237225=CARTESIAN_POINT('Ctrl Pts',(-4.19976504114966,6.70420669499665,
52.3171185393061));
#237226=CARTESIAN_POINT('Ctrl Pts',(-4.16912113100334,6.7232836571928,52.3156686985233));
#237227=CARTESIAN_POINT('Ctrl Pts',(-4.1573036904254,6.73059731131467,52.3151111463399));
#237228=CARTESIAN_POINT('Ctrl Pts',(-4.13455535827979,6.74459317698454,
52.3140408670323));
#237229=CARTESIAN_POINT('Ctrl Pts',(-4.12362738917688,6.75128004826359,
52.313528043546));
#237230=CARTESIAN_POINT('Ctrl Pts',(-4.09880695659685,6.76638503156501,
52.3123662772848));
#237231=CARTESIAN_POINT('Ctrl Pts',(-4.08490470061334,6.77478696728526,
52.3117176780363));
#237232=CARTESIAN_POINT('Ctrl Pts',(-4.04502346600183,6.79872211083111,
52.3098631110752));
#237233=CARTESIAN_POINT('Ctrl Pts',(-4.01898101152874,6.81414916370589,
52.3086594167013));
#237234=CARTESIAN_POINT('Ctrl Pts',(-3.8296951341968,6.92481588305789,52.2999633791836));
#237235=CARTESIAN_POINT('Ctrl Pts',(-3.66317036632227,7.01433007826407,
52.2925987961428));
#237236=CARTESIAN_POINT('Ctrl Pts',(-2.90958194048469,7.38525258431442,
52.2604216449909));
#237237=CARTESIAN_POINT('Ctrl Pts',(-2.29236121775071,7.59951780839213,
52.2373624417914));
#237238=CARTESIAN_POINT('Ctrl Pts',(-1.46689762266164,7.77621265400654,
52.2062514874439));
#237239=CARTESIAN_POINT('Ctrl Pts',(-1.27650168421947,7.80972537694599,
52.1990333042836));
#237240=CARTESIAN_POINT('Ctrl Pts',(-0.976792306665396,7.85122590302028,
52.18738148886));
#237241=CARTESIAN_POINT('Ctrl Pts',(-0.868211605161448,7.86397345849996,
52.1831009689399));
#237242=CARTESIAN_POINT('Ctrl Pts',(-0.746308312213926,7.87572968213505,
52.1781972640075));
#237243=CARTESIAN_POINT('Ctrl Pts',(-0.733208381019096,7.87696004750313,
52.1776690375182));
#237244=CARTESIAN_POINT('Ctrl Pts',(-0.713622888995197,7.87875026559636,
52.1768773264857));
#237245=CARTESIAN_POINT('Ctrl Pts',(-0.707139565301127,7.87933480759248,
52.1766149266276));
#237246=CARTESIAN_POINT('Ctrl Pts',(-0.696026919526955,7.88032290714134,
52.1761646011664));
#237247=CARTESIAN_POINT('Ctrl Pts',(-0.691397942095661,7.88073038994905,
52.1759768505676));
#237248=CARTESIAN_POINT('Ctrl Pts',(-0.681899812157914,7.88155806496639,
52.1755912599834));
#237249=CARTESIAN_POINT('Ctrl Pts',(-0.677030623872231,7.88197782409037,
52.1753934005481));
#237250=CARTESIAN_POINT('Ctrl Pts',(-0.665367713300532,7.88297236397686,
52.1749190227701));
#237251=CARTESIAN_POINT('Ctrl Pts',(-0.658573639667189,7.88354287397432,
52.1746423102084));
#237252=CARTESIAN_POINT('Ctrl Pts',(-0.634060227466214,7.88556939753143,
52.173642554381));
#237253=CARTESIAN_POINT('Ctrl Pts',(-0.616336827841533,7.88697445170266,
52.1729171579881));
#237254=CARTESIAN_POINT('Ctrl Pts',(-0.311729396845934,7.91008973390784,
52.1604037149726));
#237255=CARTESIAN_POINT('Ctrl Pts',(-0.02391435518396,7.91619088675665,
52.1478329046686));
#237256=CARTESIAN_POINT('Ctrl Pts',(0.977510641633306,7.88281018681442,
52.1027626971913));
#237257=CARTESIAN_POINT('Ctrl Pts',(1.68507174448236,7.76240544792788,52.0688797087307));
#237258=CARTESIAN_POINT('Ctrl Pts',(2.53646756300021,7.49545597042762,52.0298018758791));
#237259=CARTESIAN_POINT('Ctrl Pts',(2.70427238259385,7.43656128584124,52.022166253564));
#237260=CARTESIAN_POINT('Ctrl Pts',(2.95198964077305,7.34012447839218,52.0110078393031));
#237261=CARTESIAN_POINT('Ctrl Pts',(3.03348492028,7.30682147497035,52.0073554350284));
#237262=CARTESIAN_POINT('Ctrl Pts',(3.1462816874173,7.25851463621045,52.0023252688226));
#237263=CARTESIAN_POINT('Ctrl Pts',(3.17806443065659,7.24465525016644,52.0009107181923));
#237264=CARTESIAN_POINT('Ctrl Pts',(3.22560284890893,7.22355230455932,51.9987990074478));
#237265=CARTESIAN_POINT('Ctrl Pts',(3.24142729942536,7.21646524989355,51.9980967482958));
#237266=CARTESIAN_POINT('Ctrl Pts',(3.26684019746719,7.20498350935541,51.9969700465279));
#237267=CARTESIAN_POINT('Ctrl Pts',(3.27644333771793,7.20062159134022,51.996544530949));
#237268=CARTESIAN_POINT('Ctrl Pts',(3.29477899895547,7.19224893130617,51.9957325439315));
#237269=CARTESIAN_POINT('Ctrl Pts',(3.30351298769402,7.18824145968819,51.9953459659301));
#237270=CARTESIAN_POINT('Ctrl Pts',(3.31895722999937,7.18112098651579,51.9946627378169));
#237271=CARTESIAN_POINT('Ctrl Pts',(3.32567045165565,7.17801447232363,51.9943658746755));
#237272=CARTESIAN_POINT('Ctrl Pts',(3.33887941434223,7.17187957385656,51.9937819970591));
#237273=CARTESIAN_POINT('Ctrl Pts',(3.34537541624781,7.16885176929519,51.9934949638429));
#237274=CARTESIAN_POINT('Ctrl Pts',(3.36278060918614,7.16071035118143,51.9927261886038));
#237275=CARTESIAN_POINT('Ctrl Pts',(3.37368226673752,7.15558062799368,51.9922449790048));
#237276=CARTESIAN_POINT('Ctrl Pts',(3.41321054907595,7.13687036861615,51.9905012627755));
#237277=CARTESIAN_POINT('Ctrl Pts',(3.44176740661182,7.12314270936864,51.9892436298566));
#237278=CARTESIAN_POINT('Ctrl Pts',(3.92755276256321,6.88601588875911,51.9678835700672));
#237279=CARTESIAN_POINT('Ctrl Pts',(4.36227279624529,6.61917924942799,51.9493800873574));
#237280=CARTESIAN_POINT('Ctrl Pts',(4.89769438738188,6.21472233682185,51.9258878440039));
#237281=CARTESIAN_POINT('Ctrl Pts',(5.0239744011972,6.11308973187248,51.9202803036852));
#237282=CARTESIAN_POINT('Ctrl Pts',(5.18469766571331,5.97539032549101,51.9129735383617));
#237283=CARTESIAN_POINT('Ctrl Pts',(5.22204676123818,5.94277772198482,51.9112630277526));
#237284=CARTESIAN_POINT('Ctrl Pts',(5.3117648341662,5.86293849842565,51.9071187742434));
#237285=CARTESIAN_POINT('Ctrl Pts',(5.36381364818646,5.81535868234409,51.9046847813853));
#237286=CARTESIAN_POINT('Ctrl Pts',(5.47329053844085,5.71256135781169,51.8994886808603));
#237287=CARTESIAN_POINT('Ctrl Pts',(5.53053459284019,5.65715949723827,51.8967252600328));
#237288=CARTESIAN_POINT('Ctrl Pts',(5.77390838897745,5.41439277775362,51.8847351329297));
#237289=CARTESIAN_POINT('Ctrl Pts',(5.95142036700782,5.21864452628176,51.8753679638631));
#237290=CARTESIAN_POINT('Ctrl Pts',(6.18032618801816,4.93932286943376,51.8619196615312));
#237291=CARTESIAN_POINT('Ctrl Pts',(6.24046104693437,4.86312523879511,51.8582429853743));
#237292=CARTESIAN_POINT('Ctrl Pts',(6.3479983903071,4.72158344271387,51.8513661567181));
#237293=CARTESIAN_POINT('Ctrl Pts',(6.39583024176179,4.656585439111,51.8481880208492));
#237294=CARTESIAN_POINT('Ctrl Pts',(6.45071896206369,4.57955661949901,51.8444056087554));
#237295=CARTESIAN_POINT('Ctrl Pts',(6.45875024687003,4.56822276210144,51.8438486950927));
#237296=CARTESIAN_POINT('Ctrl Pts',(6.47099413354621,4.55084719267143,51.8429943997299));
#237297=CARTESIAN_POINT('Ctrl Pts',(6.47522824206945,4.54482061913332,51.8426980010337));
#237298=CARTESIAN_POINT('Ctrl Pts',(6.48259137154624,4.53430921024349,51.8421808781726));
#237299=CARTESIAN_POINT('Ctrl Pts',(6.48572417383986,4.52982702155779,51.8419603231061));
#237300=CARTESIAN_POINT('Ctrl Pts',(6.49225865331545,4.52045728196455,51.8414991721101));
#237301=CARTESIAN_POINT('Ctrl Pts',(6.49565946376103,4.51556913248198,51.8412585383494));
#237302=CARTESIAN_POINT('Ctrl Pts',(6.50503278325136,4.5020639060141,51.8405935652216));
#237303=CARTESIAN_POINT('Ctrl Pts',(6.51099367508337,4.49343880416742,51.8401687258356));
#237304=CARTESIAN_POINT('Ctrl Pts',(6.53425575421329,4.45963630486868,51.83850321145));
#237305=CARTESIAN_POINT('Ctrl Pts',(6.55142807729838,4.43437079552155,51.837257177257));
#237306=CARTESIAN_POINT('Ctrl Pts',(6.64990642672224,4.28765964077672,51.8300176659102));
#237307=CARTESIAN_POINT('Ctrl Pts',(6.72797896751328,4.16408181112704,51.823904307414));
#237308=CARTESIAN_POINT('Ctrl Pts',(6.9672158290295,3.76109508051637,51.8040607910132));
#237309=CARTESIAN_POINT('Ctrl Pts',(7.11473596704962,3.47396898476637,51.7900756821757));
#237310=CARTESIAN_POINT('Ctrl Pts',(7.44418052249601,2.72314570911304,51.7546708600605));
#237311=CARTESIAN_POINT('Ctrl Pts',(7.60064637513865,2.24979198825484,51.7334824488672));
#237312=CARTESIAN_POINT('Ctrl Pts',(7.79054781880554,1.42001356373868,51.6981947477973));
#237313=CARTESIAN_POINT('Ctrl Pts',(7.84625115385763,1.07024531693852,51.6837709687419));
#237314=CARTESIAN_POINT('Ctrl Pts',(7.88379256174759,0.65827318731429,51.6670194868207));
#237315=CARTESIAN_POINT('Ctrl Pts',(7.88855067119788,0.598562532219954,
51.6645990538531));
#237316=CARTESIAN_POINT('Ctrl Pts',(7.89467671610254,0.508825519669789,
51.6609726823818));
#237317=CARTESIAN_POINT('Ctrl Pts',(7.89655239903012,0.478836169824792,
51.6597626541195));
#237318=CARTESIAN_POINT('Ctrl Pts',(7.89949520658906,0.427051087437223,
51.6576763967149));
#237319=CARTESIAN_POINT('Ctrl Pts',(7.9006430899164,0.405260309788896,51.6567994916115));
#237320=CARTESIAN_POINT('Ctrl Pts',(7.90283589571974,0.360075236898814,
51.6549831519664));
#237321=CARTESIAN_POINT('Ctrl Pts',(7.90386713118382,0.336680481965398,
51.6540438452353));
#237322=CARTESIAN_POINT('Ctrl Pts',(7.90640606694132,0.272617432871721,
51.6514746819227));
#237323=CARTESIAN_POINT('Ctrl Pts',(7.90770385976311,0.231941468414489,
51.6498467243587));
#237324=CARTESIAN_POINT('Ctrl Pts',(7.91157557022579,0.0718421331945126,
51.6434515960189));
#237325=CARTESIAN_POINT('Ctrl Pts',(7.91175844709219,-0.047623919068554,
51.6387070502196));
#237326=CARTESIAN_POINT('Ctrl Pts',(7.90128752924617,-0.543387775044297,
51.6191102104846));
#237327=CARTESIAN_POINT('Ctrl Pts',(7.86648873491408,-0.91868269334451,
51.6045173183823));
#237328=CARTESIAN_POINT('Ctrl Pts',(7.74402111267489,-1.659624852261,51.5754834897492));
#237329=CARTESIAN_POINT('Ctrl Pts',(7.65677288121044,-2.02436018172972,
51.5610749480961));
#237330=CARTESIAN_POINT('Ctrl Pts',(7.5209905695871,-2.45448035999185,51.5432166453439));
#237331=CARTESIAN_POINT('Ctrl Pts',(7.49690482399161,-2.52709137195962,
51.5401705141228));
#237332=CARTESIAN_POINT('Ctrl Pts',(7.4653922553341,-2.6176738239576,51.5363232668059));
#237333=CARTESIAN_POINT('Ctrl Pts',(7.45894699663908,-2.63598320771407,
51.5355431878288));
#237334=CARTESIAN_POINT('Ctrl Pts',(7.44859284998366,-2.66505471852185,
51.5343005414809));
#237335=CARTESIAN_POINT('Ctrl Pts',(7.44472785746868,-2.67583243585648,
51.5338389677733));
#237336=CARTESIAN_POINT('Ctrl Pts',(7.43776005159926,-2.69513054207825,
51.5330108675046));
#237337=CARTESIAN_POINT('Ctrl Pts',(7.4346659584296,-2.70365406627205,51.5326445450864));
#237338=CARTESIAN_POINT('Ctrl Pts',(7.4273961559404,-2.72357387535458,51.5317870771952));
#237339=CARTESIAN_POINT('Ctrl Pts',(7.42320886504025,-2.73496589677564,
51.5312956552408));
#237340=CARTESIAN_POINT('Ctrl Pts',(7.41111685825313,-2.76763128935859,
51.5298834922547));
#237341=CARTESIAN_POINT('Ctrl Pts',(7.40314685501238,-2.78888018209056,
51.5289611020241));
#237342=CARTESIAN_POINT('Ctrl Pts',(7.34143011282637,-2.95129486509077,
51.5218825882311));
#237343=CARTESIAN_POINT('Ctrl Pts',(7.28374256217901,-3.090927042738,51.5156341740384));
#237344=CARTESIAN_POINT('Ctrl Pts',(7.02163824453983,-3.67719158960518,
51.488845155229));
#237345=CARTESIAN_POINT('Ctrl Pts',(6.77986210960784,-4.10592567801498,
51.4679287301087));
#237346=CARTESIAN_POINT('Ctrl Pts',(6.40063454518289,-4.65253886377285,
51.4402212244242));
#237347=CARTESIAN_POINT('Ctrl Pts',(6.29668123735791,-4.79229044014567,
51.4330262054818));
#237348=CARTESIAN_POINT('Ctrl Pts',(6.12043744610999,-5.0135812573942,51.4214460702434));
#237349=CARTESIAN_POINT('Ctrl Pts',(6.05092738978183,-5.09725708149458,
51.4170208994315));
#237350=CARTESIAN_POINT('Ctrl Pts',(5.95753905595361,-5.20507410811285,
51.411252632427));
#237351=CARTESIAN_POINT('Ctrl Pts',(5.93520051408025,-5.23053180335807,
51.4098856193712));
#237352=CARTESIAN_POINT('Ctrl Pts',(5.89835553087223,-5.27198151988611,
51.4076513758338));
#237353=CARTESIAN_POINT('Ctrl Pts',(5.88394592914525,-5.28805894644538,
51.4067826405154));
#237354=CARTESIAN_POINT('Ctrl Pts',(5.85591278059868,-5.31908031668289,
51.4051022089783));
#237355=CARTESIAN_POINT('Ctrl Pts',(5.84229739692514,-5.33403140580243,
51.4042903933297));
#237356=CARTESIAN_POINT('Ctrl Pts',(5.81067518429199,-5.36848951386144,
51.4024148543552));
#237357=CARTESIAN_POINT('Ctrl Pts',(5.79262717438009,-5.38795844293858,
51.4013517826696));
#237358=CARTESIAN_POINT('Ctrl Pts',(5.7337422832019,-5.45084147816368,51.3979068017594));
#237359=CARTESIAN_POINT('Ctrl Pts',(5.69251255569761,-5.49388517007,51.3955310038168));
#237360=CARTESIAN_POINT('Ctrl Pts',(5.34877993184729,-5.84471669441425,
51.3760094943302));
#237361=CARTESIAN_POINT('Ctrl Pts',(5.02202823518501,-6.12775747677063,
51.359168774521));
#237362=CARTESIAN_POINT('Ctrl Pts',(4.60152081278964,-6.43567854055421,
51.339091794929));
#237363=CARTESIAN_POINT('Ctrl Pts',(4.52832205492248,-6.48739174265638,
51.3356534581524));
#237364=CARTESIAN_POINT('Ctrl Pts',(4.01477254559888,-6.83727479690381,
51.3119056257524));
#237365=CARTESIAN_POINT('Ctrl Pts',(3.54622064757126,-7.09161757516245,
51.2922487525006));
#237366=CARTESIAN_POINT('Ctrl Pts',(2.83935122829312,-7.3876262975815,51.2634266808514));
#237367=CARTESIAN_POINT('Ctrl Pts',(2.61908206399757,-7.46855679499356,
51.2545316589161));
#237368=CARTESIAN_POINT('Ctrl Pts',(2.3024685659512,-7.5691544096621,51.2415801466397));
#237369=CARTESIAN_POINT('Ctrl Pts',(2.20884847374301,-7.59700254168023,
51.2377299068452));
#237370=CARTESIAN_POINT('Ctrl Pts',(2.09955003299581,-7.62732319452465,
51.2331916124215));
#237371=CARTESIAN_POINT('Ctrl Pts',(2.08434869705361,-7.63149133263188,
51.2325594542538));
#237372=CARTESIAN_POINT('Ctrl Pts',(2.06118168039161,-7.63776924120068,
51.2315944538325));
#237373=CARTESIAN_POINT('Ctrl Pts',(2.05322494974195,-7.63991205489974,
51.2312627396126));
#237374=CARTESIAN_POINT('Ctrl Pts',(2.03878084370208,-7.64377777841625,
51.2306600339215));
#237375=CARTESIAN_POINT('Ctrl Pts',(2.03229459027209,-7.64550487230856,
51.2303891883007));
#237376=CARTESIAN_POINT('Ctrl Pts',(2.01834559425839,-7.64920006459119,
51.2298062899027));
#237377=CARTESIAN_POINT('Ctrl Pts',(2.01088215753811,-7.65116550036741,
51.2294941434126));
#237378=CARTESIAN_POINT('Ctrl Pts',(1.99082946846771,-7.65641484645382,
51.2286547347505));
#237379=CARTESIAN_POINT('Ctrl Pts',(1.97823500038386,-7.65967861952292,
51.2281267493803));
#237380=CARTESIAN_POINT('Ctrl Pts',(1.92077462569151,-7.67441792425526,
51.225714153871));
#237381=CARTESIAN_POINT('Ctrl Pts',(1.87581709643743,-7.68553028374534,
51.2238161303691));
#237382=CARTESIAN_POINT('Ctrl Pts',(1.06177608986239,-7.87917245035684,
51.1892267695536));
#237383=CARTESIAN_POINT('Ctrl Pts',(0.269832480310142,-7.94579192008655,
51.1514267204623));
#237384=CARTESIAN_POINT('Ctrl Pts',(-0.90906387391072,-7.86832581836317,
51.0984082166215));
#237385=CARTESIAN_POINT('Ctrl Pts',(-1.29699672823081,-7.81375717549953,
51.0814342310139));
#237386=CARTESIAN_POINT('Ctrl Pts',(-1.73960975791977,-7.71760865638512,
51.0628256688525));
#237387=CARTESIAN_POINT('Ctrl Pts',(-1.79973014518173,-7.70381055776497,
51.0603136254667));
#237388=CARTESIAN_POINT('Ctrl Pts',(-1.87378158119324,-7.68590098525529,
51.0572383253472));
#237389=CARTESIAN_POINT('Ctrl Pts',(-1.88786988639595,-7.68245264639402,
51.0566540927801));
#237390=CARTESIAN_POINT('Ctrl Pts',(-1.91001542900665,-7.67696757355624,
51.0557370494918));
#237391=CARTESIAN_POINT('Ctrl Pts',(-1.91807904306189,-7.67495686304351,
51.0554034117045));
#237392=CARTESIAN_POINT('Ctrl Pts',(-1.93240428508631,-7.67136079192476,
51.054811181186));
#237393=CARTESIAN_POINT('Ctrl Pts',(-1.93866716185656,-7.66978046339651,
51.0545524283822));
#237394=CARTESIAN_POINT('Ctrl Pts',(-1.95312099129079,-7.66611445485102,
51.0539556441));
#237395=CARTESIAN_POINT('Ctrl Pts',(-1.96131055747216,-7.66402331280451,
51.0536177872915));
#237396=CARTESIAN_POINT('Ctrl Pts',(-1.98377329884904,-7.65824926371994,
51.0526918672706));
#237397=CARTESIAN_POINT('Ctrl Pts',(-1.99803958857213,-7.65453957413411,
51.0521046611031));
#237398=CARTESIAN_POINT('Ctrl Pts',(-2.06798410911439,-7.63614290635203,
51.049229861381));
#237399=CARTESIAN_POINT('Ctrl Pts',(-2.12351186249019,-7.62088802616805,
51.0469605243978));
#237400=CARTESIAN_POINT('Ctrl Pts',(-3.03593058252707,-7.35947666308705,
51.0098728557065));
#237401=CARTESIAN_POINT('Ctrl Pts',(-3.84521275693607,-6.9708696223835,
50.9808530086722));
#237402=CARTESIAN_POINT('Ctrl Pts',(-4.74724961333479,-6.33192697228394,
50.9425893048823));
#237403=CARTESIAN_POINT('Ctrl Pts',(-4.91671148246358,-6.201259475936,50.9350463544984));
#237404=CARTESIAN_POINT('Ctrl Pts',(-5.2124228427832,-5.95349620170652,
50.9208638412435));
#237405=CARTESIAN_POINT('Ctrl Pts',(-5.34054242286951,-5.83884140076207,
50.9143409400278));
#237406=CARTESIAN_POINT('Ctrl Pts',(-5.4836107516599,-5.70215832806318,
50.9064833612311));
#237407=CARTESIAN_POINT('Ctrl Pts',(-5.50231415306876,-5.68411254336957,
50.9054443874267));
#237408=CARTESIAN_POINT('Ctrl Pts',(-5.52609699011638,-5.66093853883887,
50.9041076843781));
#237409=CARTESIAN_POINT('Ctrl Pts',(-5.53125898143786,-5.65589490392956,
50.903816613114));
#237410=CARTESIAN_POINT('Ctrl Pts',(-5.53952835788207,-5.64779298321426,
50.9033487951516));
#237411=CARTESIAN_POINT('Ctrl Pts',(-5.54264013911168,-5.64473916998709,
50.9031724059919));
#237412=CARTESIAN_POINT('Ctrl Pts',(-5.54853717681745,-5.63894240784062,
50.9028374717575));
#237413=CARTESIAN_POINT('Ctrl Pts',(-5.55132292894481,-5.63619996273505,
50.9026789673142));
#237414=CARTESIAN_POINT('Ctrl Pts',(-5.5576342470128,-5.62997754137028,
50.902319221579));
#237415=CARTESIAN_POINT('Ctrl Pts',(-5.56115857629428,-5.6264963191132,
50.9021178788941));
#237416=CARTESIAN_POINT('Ctrl Pts',(-5.57021161430208,-5.61753719578666,
50.9015995054334));
#237417=CARTESIAN_POINT('Ctrl Pts',(-5.57573551316179,-5.61205444211983,
50.9012820757323));
#237418=CARTESIAN_POINT('Ctrl Pts',(-5.60981800342172,-5.5781258257499,
50.8993164612047));
#237419=CARTESIAN_POINT('Ctrl Pts',(-5.63816642790486,-5.54947069324606,
50.8976508544256));
#237420=CARTESIAN_POINT('Ctrl Pts',(-6.25134430504331,-4.92011052168407,
50.8609791270086));
#237421=CARTESIAN_POINT('Ctrl Pts',(-6.73724408125472,-4.23043507993487,
50.8197042175227));
#237422=CARTESIAN_POINT('Ctrl Pts',(-7.27560593288448,-3.1302872266117,
50.7647930121821));
#237423=CARTESIAN_POINT('Ctrl Pts',(-7.41976997593545,-2.77131964628872,
50.7482090714532));
#237424=CARTESIAN_POINT('Ctrl Pts',(-7.54348847028449,-2.38330429577554,
50.7317554182434));
#237425=CARTESIAN_POINT('Ctrl Pts',(-7.54975758804608,-2.36337005962162,
50.7309139765251));
#237426=CARTESIAN_POINT('Ctrl Pts',(-7.55865880549966,-2.33466953280044,
50.7297080135697));
#237427=CARTESIAN_POINT('Ctrl Pts',(-7.56135476331092,-2.32592323808961,
50.7293412386578));
#237428=CARTESIAN_POINT('Ctrl Pts',(-7.56600764361138,-2.31073465995964,
50.7287055770043));
#237429=CARTESIAN_POINT('Ctrl Pts',(-7.56797152810201,-2.30429453023421,
50.7284364449191));
#237430=CARTESIAN_POINT('Ctrl Pts',(-7.57173192344728,-2.29190647376306,
50.7279195084701));
#237431=CARTESIAN_POINT('Ctrl Pts',(-7.57352965271673,-2.28595892453885,
50.7276716613336));
#237432=CARTESIAN_POINT('Ctrl Pts',(-7.57774795541946,-2.27194363299604,
50.7270884030425));
#237433=CARTESIAN_POINT('Ctrl Pts',(-7.58016265699817,-2.26387412226327,
50.7267531987912));
#237434=CARTESIAN_POINT('Ctrl Pts',(-7.58846382173659,-2.23597089688677,
50.7255962282729));
#237435=CARTESIAN_POINT('Ctrl Pts',(-7.59428539129238,-2.21611787368668,
50.7247767449108));
#237436=CARTESIAN_POINT('Ctrl Pts',(-7.65879440192245,-1.9928864065297,
50.7156033858462));
#237437=CARTESIAN_POINT('Ctrl Pts',(-7.7093765445267,-1.7872464436281,50.707539029237));
#237438=CARTESIAN_POINT('Ctrl Pts',(-7.80701268840627,-1.30817640644099,
50.6894926242977));
#237439=CARTESIAN_POINT('Ctrl Pts',(-7.8480587307184,-1.03380809376537,
50.679706509675));
#237440=CARTESIAN_POINT('Ctrl Pts',(-7.89918585906256,-0.502552382104667,
50.6613253803921));
#237441=CARTESIAN_POINT('Ctrl Pts',(-7.91132569102394,-0.246219205752182,
50.6527051770111));
#237442=CARTESIAN_POINT('Ctrl Pts',(-7.91032769265032,0.523963540078032,
50.6266919225513));
#237443=CARTESIAN_POINT('Ctrl Pts',(-7.85962538591528,1.03633015157118,
50.6092764726127));
#237444=CARTESIAN_POINT('Ctrl Pts',(-7.75324523613621,1.57231962172495,
50.5877143879113));
#237445=CARTESIAN_POINT('Ctrl Pts',(-7.7466477853958,1.60450886891474,50.5864061596295));
#237446=CARTESIAN_POINT('Ctrl Pts',(-7.73838202077217,1.64359820378141,
50.5848002522428));
#237447=CARTESIAN_POINT('Ctrl Pts',(-7.73690461505836,1.65053880043261,
50.5845144492266));
#237448=CARTESIAN_POINT('Ctrl Pts',(-7.73445736620318,1.66196006796274,
50.5840430340289));
#237449=CARTESIAN_POINT('Ctrl Pts',(-7.73349296506658,1.666441890976,50.5838577649383));
#237450=CARTESIAN_POINT('Ctrl Pts',(-7.73174200886593,1.67454478566484,
50.5835223020355));
#237451=CARTESIAN_POINT('Ctrl Pts',(-7.73095680422824,1.67816614848497,
50.583372193434));
#237452=CARTESIAN_POINT('Ctrl Pts',(-7.72926968647717,1.68592082003794,
50.5830503661171));
#237453=CARTESIAN_POINT('Ctrl Pts',(-7.72836700197534,1.69005395782781,
50.5828785992936));
#237454=CARTESIAN_POINT('Ctrl Pts',(-7.72591061183009,1.70125795491553,
50.5824123394205));
#237455=CARTESIAN_POINT('Ctrl Pts',(-7.72435051820062,1.70832739321897,
50.582117450894));
#237456=CARTESIAN_POINT('Ctrl Pts',(-7.71653395414529,1.74351790172649,
50.5806461412921));
#237457=CARTESIAN_POINT('Ctrl Pts',(-7.71013368762364,1.77160645033107,
50.5794609390703));
#237458=CARTESIAN_POINT('Ctrl Pts',(-7.65421224601727,2.01098252167035,
50.5692717990256));
#237459=CARTESIAN_POINT('Ctrl Pts',(-7.59617324761271,2.22016964899762,
50.5597788778296));
#237460=CARTESIAN_POINT('Ctrl Pts',(-7.36614410463515,2.93391204623333,
50.5259758079177));
#237461=CARTESIAN_POINT('Ctrl Pts',(-7.15184277494405,3.42331255617383,
50.5003941302939));
#237462=CARTESIAN_POINT('Ctrl Pts',(-6.71616940725617,4.195483196243,50.4592358935602));
#237463=CARTESIAN_POINT('Ctrl Pts',(-6.52189909727086,4.49153442503722,
50.443210103376));
#237464=CARTESIAN_POINT('Ctrl Pts',(-6.17042207143741,4.95602026962088,
50.4180132197873));
#237465=CARTESIAN_POINT('Ctrl Pts',(-6.02454086189876,5.13236446589125,
50.4084264138683));
#237466=CARTESIAN_POINT('Ctrl Pts',(-5.85661189252792,5.31831671592667,
50.3982802325562));
#237467=CARTESIAN_POINT('Ctrl Pts',(-5.84194479643378,5.33442373235327,
50.3974010176935));
#237468=CARTESIAN_POINT('Ctrl Pts',(-5.82124448762606,5.35696849418104,
50.3961698295652));
#237469=CARTESIAN_POINT('Ctrl Pts',(-5.81526682006235,5.36345696771227,
50.3958154225556));
#237470=CARTESIAN_POINT('Ctrl Pts',(-5.80487224623932,5.37470197666532,
50.3952010890919));
#237471=CARTESIAN_POINT('Ctrl Pts',(-5.80046032227125,5.37946309432187,
50.3949409439696));
#237472=CARTESIAN_POINT('Ctrl Pts',(-5.79126625361084,5.38936039143677,
50.3944000802879));
#237473=CARTESIAN_POINT('Ctrl Pts',(-5.7864831229754,5.39449564990703,50.3941194055393));
#237474=CARTESIAN_POINT('Ctrl Pts',(-5.77520142776797,5.40657561943629,
50.3934590479722));
#237475=CARTESIAN_POINT('Ctrl Pts',(-5.76869715321432,5.41351499631357,
50.3930796176615));
#237476=CARTESIAN_POINT('Ctrl Pts',(-5.74738455181556,5.43617127392764,
50.3918405270949));
#237477=CARTESIAN_POINT('Ctrl Pts',(-5.7325243251148,5.45183933894015,50.3909831642796));
#237478=CARTESIAN_POINT('Ctrl Pts',(-5.44128433838478,5.75640451034283,
50.3743072158344));
#237479=CARTESIAN_POINT('Ctrl Pts',(-5.14344727488068,6.02401543239919,
50.3595204759108));
#237480=CARTESIAN_POINT('Ctrl Pts',(-4.62814530654299,6.42082155355519,
50.336419023468));
#237481=CARTESIAN_POINT('Ctrl Pts',(-4.42250903761971,6.5641523383706,50.3277523745125));
#237482=CARTESIAN_POINT('Ctrl Pts',(-3.99799616288946,6.83102501461066,
50.3104519248722));
#237483=CARTESIAN_POINT('Ctrl Pts',(-3.77934687143073,6.95438056092077,
50.3018271641067));
#237484=CARTESIAN_POINT('Ctrl Pts',(-3.25510236948542,7.21810828926355,
50.2810986754919));
#237485=CARTESIAN_POINT('Ctrl Pts',(-2.94568074263968,7.34981325299562,
50.2687920465069));
#237486=CARTESIAN_POINT('Ctrl Pts',(-2.60622576986852,7.46940972956807,
50.2544547284584));
#237487=CARTESIAN_POINT('Ctrl Pts',(-2.58360347089448,7.47726471109727,
50.2534961952832));
#237488=CARTESIAN_POINT('Ctrl Pts',(-2.55215747470383,7.48802373825333,
50.2521598443616));
#237489=CARTESIAN_POINT('Ctrl Pts',(-2.54336365864591,7.49101519016262,
50.2517857089474));
#237490=CARTESIAN_POINT('Ctrl Pts',(-2.52928229843265,7.49577768810581,
50.2511859487729));
#237491=CARTESIAN_POINT('Ctrl Pts',(-2.52399809898363,7.4975586487069,50.2509607319681));
#237492=CARTESIAN_POINT('Ctrl Pts',(-2.513668312286,7.50102799117831,50.2505201808872));
#237493=CARTESIAN_POINT('Ctrl Pts',(-2.50862289542961,7.5027168730374,50.2503048670463));
#237494=CARTESIAN_POINT('Ctrl Pts',(-2.49647650735981,7.50676908246108,
50.2497862016411));
#237495=CARTESIAN_POINT('Ctrl Pts',(-2.48937388533346,7.50912742385825,
50.249482650873));
#237496=CARTESIAN_POINT('Ctrl Pts',(-2.46779454181345,7.5162586075214,50.2485596246148));
#237497=CARTESIAN_POINT('Ctrl Pts',(-2.45330740933709,7.5209996747131,50.2479389042245));
#237498=CARTESIAN_POINT('Ctrl Pts',(-2.31130353353664,7.56701799353016,
50.2418447492537));
#237499=CARTESIAN_POINT('Ctrl Pts',(-2.18277465488257,7.60508894715016,
50.2362517768322));
#237500=CARTESIAN_POINT('Ctrl Pts',(-1.80580541054453,7.70640577991665,
50.2197201771648));
#237501=CARTESIAN_POINT('Ctrl Pts',(-1.55518467560398,7.76086443556248,
50.2085741784437));
#237502=CARTESIAN_POINT('Ctrl Pts',(-0.875789659399663,7.87425898133527,
50.1784472665762));
#237503=CARTESIAN_POINT('Ctrl Pts',(-0.444071036561553,7.91035947100023,
50.1594314781763));
#237504=CARTESIAN_POINT('Ctrl Pts',(0.339512619627885,7.91150462062581,
50.1259458845519));
#237505=CARTESIAN_POINT('Ctrl Pts',(0.690244517435434,7.88864753255679,
50.1113200870908));
#237506=CARTESIAN_POINT('Ctrl Pts',(1.07380501108117,7.83786612837951,50.0956499447213));
#237507=CARTESIAN_POINT('Ctrl Pts',(1.10926335960438,7.83292649469544,50.0942041296534));
#237508=CARTESIAN_POINT('Ctrl Pts',(1.1617684254719,7.82524843939604,50.0920672925894));
#237509=CARTESIAN_POINT('Ctrl Pts',(1.17884161369433,7.82269464220956,50.0913730977716));
#237510=CARTESIAN_POINT('Ctrl Pts',(1.2079903140451,7.81823700321695,50.0901890231708));
#237511=CARTESIAN_POINT('Ctrl Pts',(1.22007000279372,7.81636102202077,50.0896986495944));
#237512=CARTESIAN_POINT('Ctrl Pts',(1.24478919109654,7.81246342147455,50.0886958462254));
#237513=CARTESIAN_POINT('Ctrl Pts',(1.25742823206002,7.81043910958335,50.0881834665638));
#237514=CARTESIAN_POINT('Ctrl Pts',(1.28652792164341,7.80570593830926,50.0870046085689));
#237515=CARTESIAN_POINT('Ctrl Pts',(1.30298504155243,7.80297566781858,50.0863385241983));
#237516=CARTESIAN_POINT('Ctrl Pts',(1.35434261323166,7.79428833221164,50.0842617858416));
#237517=CARTESIAN_POINT('Ctrl Pts',(1.38921191795744,7.78814899648283,50.0828545323641));
#237518=CARTESIAN_POINT('Ctrl Pts',(1.46904279405581,7.77354021242246,50.0796389625636));
#237519=CARTESIAN_POINT('Ctrl Pts',(1.51397456855761,7.76491437330063,50.0778336754279));
#237520=CARTESIAN_POINT('Ctrl Pts',(1.94820642981538,7.67763972927537,50.0604295725632));
#237521=CARTESIAN_POINT('Ctrl Pts',(2.33114609284802,7.57016807343126,50.0454590821063));
#237522=CARTESIAN_POINT('Ctrl Pts',(3.04024702424708,7.31221771313176,50.0176853393892));
#237523=CARTESIAN_POINT('Ctrl Pts',(3.36741183720351,7.16743774627461,50.0048379230262));
#237524=CARTESIAN_POINT('Ctrl Pts',(3.91557611398751,6.87901567254248,49.9821106534605));
#237525=CARTESIAN_POINT('Ctrl Pts',(4.14127072079178,6.74555090909402,49.9723595492534));
#237526=CARTESIAN_POINT('Ctrl Pts',(4.3658750952618,6.5972044594386,49.9618747626815));
#237527=CARTESIAN_POINT('Ctrl Pts',(4.3718303212097,6.59325956331433,49.9615961788359));
#237528=CARTESIAN_POINT('Ctrl Pts',(4.39809625028165,6.57580909840806,49.9603648368023));
#237529=CARTESIAN_POINT('Ctrl Pts',(4.41834964992846,6.56221778673381,49.9594084116411));
#237530=CARTESIAN_POINT('Ctrl Pts',(4.46446058030299,6.53096419255763,49.9572142770302));
#237531=CARTESIAN_POINT('Ctrl Pts',(4.49027664649578,6.51324167822048,49.9559738027848));
#237532=CARTESIAN_POINT('Ctrl Pts',(4.53292881850131,6.48358721069017,49.9539031571463));
#237533=CARTESIAN_POINT('Ctrl Pts',(4.54982480756593,6.47174172857735,49.9530773339777));
#237534=CARTESIAN_POINT('Ctrl Pts',(4.57313044412891,6.45526618014219,49.951930232073));
#237535=CARTESIAN_POINT('Ctrl Pts',(4.57957987954209,6.45069233817113,49.9516119402214));
#237536=CARTESIAN_POINT('Ctrl Pts',(4.59036357911497,6.44302037834353,49.9510782996455));
#237537=CARTESIAN_POINT('Ctrl Pts',(4.59470159928951,6.43992753045374,49.9508632367408));
#237538=CARTESIAN_POINT('Ctrl Pts',(4.60318894763311,6.43386342392706,49.9504416903345));
#237539=CARTESIAN_POINT('Ctrl Pts',(4.60733853208254,6.43089252716621,49.9502352267515));
#237540=CARTESIAN_POINT('Ctrl Pts',(4.61717853573062,6.42383315986144,49.9497447644865));
#237541=CARTESIAN_POINT('Ctrl Pts',(4.62286639700492,6.41974114521041,49.9494605684063));
#237542=CARTESIAN_POINT('Ctrl Pts',(4.64131950506261,6.40642819591742,49.9485362775669));
#237543=CARTESIAN_POINT('Ctrl Pts',(4.65406259942769,6.3971767438836,49.9478944524473));
#237544=CARTESIAN_POINT('Ctrl Pts',(4.96909121374221,6.16702732253397,49.9319374506794));
#237545=CARTESIAN_POINT('Ctrl Pts',(5.25529737093517,5.92501932603227,49.9152954905421));
#237546=CARTESIAN_POINT('Ctrl Pts',(6.0141038076308,5.18503071401614,49.866980091659));
#237547=CARTESIAN_POINT('Ctrl Pts',(6.44071774748014,4.64449558108511,49.8347778215324));
#237548=CARTESIAN_POINT('Ctrl Pts',(6.91942068029469,3.84279043986989,49.7943738339742));
#237549=CARTESIAN_POINT('Ctrl Pts',(7.03648185979773,3.62399751143469,49.7839603918511));
#237550=CARTESIAN_POINT('Ctrl Pts',(7.15319544314933,3.37879714129683,49.7729410966472));
#237551=CARTESIAN_POINT('Ctrl Pts',(7.16321812964198,3.35749627089562,49.7719890155991));
#237552=CARTESIAN_POINT('Ctrl Pts',(7.17717621177664,3.32748463169668,49.7706548071203));
#237553=CARTESIAN_POINT('Ctrl Pts',(7.18119108074594,3.31881108405622,49.7702700568691));
#237554=CARTESIAN_POINT('Ctrl Pts',(7.18813635264969,3.3037352121519,49.76960276584));
#237555=CARTESIAN_POINT('Ctrl Pts',(7.19107394113495,3.29733622030934,49.7693199883963));
#237556=CARTESIAN_POINT('Ctrl Pts',(7.19717339632518,3.28400276903716,49.7687317171701));
#237557=CARTESIAN_POINT('Ctrl Pts',(7.20033379407984,3.27706764319233,49.7684262719303));
#237558=CARTESIAN_POINT('Ctrl Pts',(7.20776052589805,3.26070793313679,49.7677069879225));
#237559=CARTESIAN_POINT('Ctrl Pts',(7.21201840912271,3.25127951603576,49.7672934271915));
#237560=CARTESIAN_POINT('Ctrl Pts',(7.22591258531051,3.22035144058372,49.7659400070756));
#237561=CARTESIAN_POINT('Ctrl Pts',(7.23547136949463,3.1988169945158,49.7650026905068));
#237562=CARTESIAN_POINT('Ctrl Pts',(7.40862836498946,2.80397399893836,49.7479076508804));
#237563=CARTESIAN_POINT('Ctrl Pts',(7.54323930083466,2.4186009739306,49.7327504839495));
#237564=CARTESIAN_POINT('Ctrl Pts',(7.79928066207843,1.45142122964752,49.6970409681734));
#237565=CARTESIAN_POINT('Ctrl Pts',(7.8860908278076,0.863095349536447,49.6773337288548));
#237566=CARTESIAN_POINT('Ctrl Pts',(7.91712013831398,-0.043457692133003,
49.6449984011458));
#237567=CARTESIAN_POINT('Ctrl Pts',(7.90914648703363,-0.357892497832621,
49.6333669545769));
#237568=CARTESIAN_POINT('Ctrl Pts',(7.88076924122621,-0.69123696655325,
49.6200404118277));
#237569=CARTESIAN_POINT('Ctrl Pts',(7.87897113862675,-0.71143950147839,
49.6192293731651));
#237570=CARTESIAN_POINT('Ctrl Pts',(7.8762942947089,-0.74025955699584,49.618067759341));
#237571=CARTESIAN_POINT('Ctrl Pts',(7.87547905122072,-0.748882995955991,
49.6177195943124));
#237572=CARTESIAN_POINT('Ctrl Pts',(7.87405953616969,-0.763639575587852,
49.6171228149721));
#237573=CARTESIAN_POINT('Ctrl Pts',(7.87346225656381,-0.769773391818883,
49.6168744599458));
#237574=CARTESIAN_POINT('Ctrl Pts',(7.87225261495514,-0.782047211500224,
49.6163769188983));
#237575=CARTESIAN_POINT('Ctrl Pts',(7.87164023553197,-0.788187209220541,
49.6161277323885));
#237576=CARTESIAN_POINT('Ctrl Pts',(7.87012323044885,-0.803219288305605,
49.6155169655765));
#237577=CARTESIAN_POINT('Ctrl Pts',(7.86921071864419,-0.812110554272524,
49.6151551031322));
#237578=CARTESIAN_POINT('Ctrl Pts',(7.8659644398614,-0.843222166176726,
49.6138868343835));
#237579=CARTESIAN_POINT('Ctrl Pts',(7.86355162024573,-0.865434049971041,
49.6129776706834));
#237580=CARTESIAN_POINT('Ctrl Pts',(7.8171417592864,-1.27644744821703,49.5960891600648));
#237581=CARTESIAN_POINT('Ctrl Pts',(7.74445422984662,-1.66145453306334,
49.5792278055125));
#237582=CARTESIAN_POINT('Ctrl Pts',(7.5756321974535,-2.29416606638227,49.5509413922721));
#237583=CARTESIAN_POINT('Ctrl Pts',(7.49499028326708,-2.54529469133629,
49.5395459001544));
#237584=CARTESIAN_POINT('Ctrl Pts',(7.17778260874517,-3.38627525119422,
49.5010973471223));
#237585=CARTESIAN_POINT('Ctrl Pts',(6.88283161453795,-3.95146852869857,
49.4749551106286));
#237586=CARTESIAN_POINT('Ctrl Pts',(6.47433691152503,-4.54691360091522,
49.4456352480798));
#237587=CARTESIAN_POINT('Ctrl Pts',(6.42403646834625,-4.6177069351777,49.4421189710503));
#237588=CARTESIAN_POINT('Ctrl Pts',(6.35353751303947,-4.71354589265816,
49.4373167914929));
#237589=CARTESIAN_POINT('Ctrl Pts',(6.33433691373511,-4.73931742800615,
49.4360212169839));
#237590=CARTESIAN_POINT('Ctrl Pts',(6.30111903086722,-4.78334083237742,
49.4338007401467));
#237591=CARTESIAN_POINT('Ctrl Pts',(6.28717818388037,-4.80164982554388,
49.4328750536705));
#237592=CARTESIAN_POINT('Ctrl Pts',(6.25826854996638,-4.83927607814003,
49.4309681127715));
#237593=CARTESIAN_POINT('Ctrl Pts',(6.24328973703541,-4.85858533600675,
49.4299869785863));
#237594=CARTESIAN_POINT('Ctrl Pts',(6.20812014753273,-4.90349141679698,
49.4276992833118));
#237595=CARTESIAN_POINT('Ctrl Pts',(6.18786011692474,-4.92903347762713,
49.42639351928));
#237596=CARTESIAN_POINT('Ctrl Pts',(6.12158406150175,-5.01153583554654,
49.4221607916786));
#237597=CARTESIAN_POINT('Ctrl Pts',(6.07493478778017,-5.06798286160838,
49.4192413642065));
#237598=CARTESIAN_POINT('Ctrl Pts',(5.99205043746395,-5.16548639627903,
49.4141553483735));
#237599=CARTESIAN_POINT('Ctrl Pts',(5.95616035870386,-5.20682935974878,
49.4119848278126));
#237600=CARTESIAN_POINT('Ctrl Pts',(5.80392923001785,-5.37855562637706,
49.4029076878342));
#237601=CARTESIAN_POINT('Ctrl Pts',(5.68371296333561,-5.50543943382206,
49.3960511430872));
#237602=CARTESIAN_POINT('Ctrl Pts',(5.18398362418241,-5.99905588172231,
49.3686478983667));
#237603=CARTESIAN_POINT('Ctrl Pts',(4.7724237198176,-6.33137517358873,49.3485624053136));
#237604=CARTESIAN_POINT('Ctrl Pts',(4.22427297875216,-6.68996727406419,
49.3228349423994));
#237605=CARTESIAN_POINT('Ctrl Pts',(4.11601715674862,-6.75711077940484,
49.3177944058474));
#237606=CARTESIAN_POINT('Ctrl Pts',(3.98775570306799,-6.83243605543242,
49.3118365409727));
#237607=CARTESIAN_POINT('Ctrl Pts',(3.9692782329836,-6.84318699891152,49.310978576969));
#237608=CARTESIAN_POINT('Ctrl Pts',(3.9394676918288,-6.86037062519305,49.3095946975938));
#237609=CARTESIAN_POINT('Ctrl Pts',(3.92816187044759,-6.86685045184993,
49.3090699253161));
#237610=CARTESIAN_POINT('Ctrl Pts',(3.90796902303783,-6.87835760682458,
49.3081327244748));
#237611=CARTESIAN_POINT('Ctrl Pts',(3.89908816800399,-6.88339572520712,
49.3077205666184));
#237612=CARTESIAN_POINT('Ctrl Pts',(3.88061377750974,-6.89382904151755,
49.3068631960752));
#237613=CARTESIAN_POINT('Ctrl Pts',(3.87101868872506,-6.89922143828456,
49.3064179128951));
#237614=CARTESIAN_POINT('Ctrl Pts',(3.84605615133679,-6.91318180356323,
49.3052594465964));
#237615=CARTESIAN_POINT('Ctrl Pts',(3.83067142416883,-6.92171850085521,
49.3045454342996));
#237616=CARTESIAN_POINT('Ctrl Pts',(3.753683968429,-6.96410210704746,49.3009721450845));
#237617=CARTESIAN_POINT('Ctrl Pts',(3.69166125299304,-6.99717789300047,
49.2980929016583));
#237618=CARTESIAN_POINT('Ctrl Pts',(3.01317596259054,-7.34747173732453,
49.2666301737935));
#237619=CARTESIAN_POINT('Ctrl Pts',(2.35799642377459,-7.58317166646662,
49.236847120652));
#237620=CARTESIAN_POINT('Ctrl Pts',(1.66979020112909,-7.73277708092119,
49.2078242827824));
#237621=CARTESIAN_POINT('Ctrl Pts',(1.65909436721716,-7.73507896405873,
49.207373679671));
#237622=CARTESIAN_POINT('Ctrl Pts',(1.50187881343523,-7.76857271210901,
49.2007570896734));
#237623=CARTESIAN_POINT('Ctrl Pts',(1.35450498613362,-7.79561924610495,
49.1946411071309));
#237624=CARTESIAN_POINT('Ctrl Pts',(1.1678978778891,-7.82441417684245,49.1869961801491));
#237625=CARTESIAN_POINT('Ctrl Pts',(1.12930204155378,-7.83007787857513,
49.1854202533786));
#237626=CARTESIAN_POINT('Ctrl Pts',(1.06793728565388,-7.83861961996101,
49.1829226458428));
#237627=CARTESIAN_POINT('Ctrl Pts',(1.04519511005172,-7.8416844350422,49.1819987587911));
#237628=CARTESIAN_POINT('Ctrl Pts',(1.00268098972975,-7.84722555292625,
49.1802748066811));
#237629=CARTESIAN_POINT('Ctrl Pts',(0.982912411321682,-7.84972618886304,
49.1794744624347));
#237630=CARTESIAN_POINT('Ctrl Pts',(0.938799693025847,-7.85513699636905,
49.1776912880547));
#237631=CARTESIAN_POINT('Ctrl Pts',(0.914451029592729,-7.85800874362651,
49.1767089105883));
#237632=CARTESIAN_POINT('Ctrl Pts',(0.842875059848871,-7.86611342436338,
49.1738263708649));
#237633=CARTESIAN_POINT('Ctrl Pts',(0.795613374499294,-7.87103412298189,
49.1719297820021));
#237634=CARTESIAN_POINT('Ctrl Pts',(0.373760442075087,-7.9111173727665,
49.1550559330217));
#237635=CARTESIAN_POINT('Ctrl Pts',(-0.00286190810906917,-7.91994173535442,
49.1403425663408));
#237636=CARTESIAN_POINT('Ctrl Pts',(-0.948677347144523,-7.87461582484368,
49.1036414949084));
#237637=CARTESIAN_POINT('Ctrl Pts',(-1.51404753537399,-7.78570761869245,
49.0822651771676));
#237638=CARTESIAN_POINT('Ctrl Pts',(-2.43405743196127,-7.53694238822372,
49.046622632109));
#237639=CARTESIAN_POINT('Ctrl Pts',(-2.79544504176706,-7.41050590419739,
49.0323349507945));
#237640=CARTESIAN_POINT('Ctrl Pts',(-3.17626541325873,-7.24543504168874,
49.016064749451));
#237641=CARTESIAN_POINT('Ctrl Pts',(-3.20619573906016,-7.23224030114821,
49.014777365499));
#237642=CARTESIAN_POINT('Ctrl Pts',(-3.25151126837907,-7.21192642875092,
49.0128141209004));
#237643=CARTESIAN_POINT('Ctrl Pts',(-3.26695698304196,-7.20494277623656,
49.0121424509039));
#237644=CARTESIAN_POINT('Ctrl Pts',(-3.31236438508732,-7.18423615989473,
49.0101602344403));
#237645=CARTESIAN_POINT('Ctrl Pts',(-3.34226273619789,-7.17037563796252,
49.008845232795));
#237646=CARTESIAN_POINT('Ctrl Pts',(-3.38226084418731,-7.15152846668484,
49.0070719199289));
#237647=CARTESIAN_POINT('Ctrl Pts',(-3.39243802388179,-7.14670637990842,
49.006619484534));
#237648=CARTESIAN_POINT('Ctrl Pts',(-3.40910890443529,-7.1387638553658,
49.0058763015897));
#237649=CARTESIAN_POINT('Ctrl Pts',(-3.41560871748465,-7.13565624127435,
49.0055860260539));
#237650=CARTESIAN_POINT('Ctrl Pts',(-3.42795057044004,-7.12973477303732,
49.0050338564574));
#237651=CARTESIAN_POINT('Ctrl Pts',(-3.43379341576472,-7.12692260550121,
49.0047720257847));
#237652=CARTESIAN_POINT('Ctrl Pts',(-3.44739632784333,-7.12035489856849,
49.0041614490109));
#237653=CARTESIAN_POINT('Ctrl Pts',(-3.4551537185134,-7.11659385545897,
49.0038124931375));
#237654=CARTESIAN_POINT('Ctrl Pts',(-3.47874413845167,-7.10510876519192,
49.0027489586867));
#237655=CARTESIAN_POINT('Ctrl Pts',(-3.49455747017834,-7.09734453352809,
49.0020328132275));
#237656=CARTESIAN_POINT('Ctrl Pts',(-3.66522005895423,-7.01284179344709,
48.9942678563086));
#237657=CARTESIAN_POINT('Ctrl Pts',(-3.81751575097769,-6.93111497405427,
48.9869936551422));
#237658=CARTESIAN_POINT('Ctrl Pts',(-4.05434841994003,-6.79384779929839,
48.9751134531399));
#237659=CARTESIAN_POINT('Ctrl Pts',(-4.1406975149891,-6.74156748034654,
48.9706652642546));
#237660=CARTESIAN_POINT('Ctrl Pts',(-5.03963920542211,-6.17351361007708,
48.9232858178684));
#237661=CARTESIAN_POINT('Ctrl Pts',(-5.75291523545961,-5.51498231897554,
48.8775307954523));
#237662=CARTESIAN_POINT('Ctrl Pts',(-6.35899265573277,-4.70631580225002,
48.8361887343776));
#237663=CARTESIAN_POINT('Ctrl Pts',(-6.38725277906597,-4.66789010852951,
48.8342507130064));
#237664=CARTESIAN_POINT('Ctrl Pts',(-6.4232930267536,-4.61794550415109,
48.8317654075641));
#237665=CARTESIAN_POINT('Ctrl Pts',(-6.43139240891813,-4.60665884040604,
48.8312059664108));
#237666=CARTESIAN_POINT('Ctrl Pts',(-6.44421033575313,-4.58869708823273,
48.8303191376588));
#237667=CARTESIAN_POINT('Ctrl Pts',(-6.44894831899294,-4.58203594469263,
48.8299910115572));
#237668=CARTESIAN_POINT('Ctrl Pts',(-6.45779788168344,-4.56955340406677,
48.8293775354614));
#237669=CARTESIAN_POINT('Ctrl Pts',(-6.46191193305268,-4.56373377434584,
48.8290920918066));
#237670=CARTESIAN_POINT('Ctrl Pts',(-6.47115179674687,-4.55062576109939,
48.8284504484443));
#237671=CARTESIAN_POINT('Ctrl Pts',(-6.4762731748559,-4.5433342557451,48.8280944169137));
#237672=CARTESIAN_POINT('Ctrl Pts',(-6.49129377000335,-4.52187184686007,
48.8270490554321));
#237673=CARTESIAN_POINT('Ctrl Pts',(-6.50115890076761,-4.50767709133017,
48.8263610149082));
#237674=CARTESIAN_POINT('Ctrl Pts',(-6.57535144307397,-4.4001726203807,
48.8211751603362));
#237675=CARTESIAN_POINT('Ctrl Pts',(-6.63771500643069,-4.30552046751548,
48.8167516971204));
#237676=CARTESIAN_POINT('Ctrl Pts',(-6.86810291237869,-3.93893951383469,
48.8001313672972));
#237677=CARTESIAN_POINT('Ctrl Pts',(-7.02163131959227,-3.65825063119893,
48.7884701328979));
#237678=CARTESIAN_POINT('Ctrl Pts',(-7.45537879774512,-2.73671954071198,
48.7525506912303));
#237679=CARTESIAN_POINT('Ctrl Pts',(-7.66786858919159,-2.06783614009374,
48.7301321547401));
#237680=CARTESIAN_POINT('Ctrl Pts',(-7.79411041957937,-1.35513529185525,
48.7037779797173));
#237681=CARTESIAN_POINT('Ctrl Pts',(-7.79836362753557,-1.33044113327896,
48.7028615403327));
#237682=CARTESIAN_POINT('Ctrl Pts',(-7.81102040931224,-1.25480931528971,
48.700043608784));
#237683=CARTESIAN_POINT('Ctrl Pts',(-7.81904265379069,-1.20380981845328,
48.6981280387552));
#237684=CARTESIAN_POINT('Ctrl Pts',(-7.84210828712324,-1.0472044481388,
48.6921896832425));
#237685=CARTESIAN_POINT('Ctrl Pts',(-7.85551493416445,-0.941372934361506,
48.6880985486666));
#237686=CARTESIAN_POINT('Ctrl Pts',(-7.87078871851612,-0.797527018899254,
48.6823967410285));
#237687=CARTESIAN_POINT('Ctrl Pts',(-7.8745279592402,-0.759719505442483,
48.6808849382556));
#237688=CARTESIAN_POINT('Ctrl Pts',(-7.87870809856111,-0.714101410066124,
48.6790435066982));
#237689=CARTESIAN_POINT('Ctrl Pts',(-7.87940998446185,-0.706314676449113,
48.6787285779233));
#237690=CARTESIAN_POINT('Ctrl Pts',(-7.88053850701718,-0.69358378458703,
48.6782126763788));
#237691=CARTESIAN_POINT('Ctrl Pts',(-7.88097203785256,-0.688640229116838,
48.6780120968644));
#237692=CARTESIAN_POINT('Ctrl Pts',(-7.88173884250575,-0.679800785236281,
48.6776529961838));
#237693=CARTESIAN_POINT('Ctrl Pts',(-7.88207388037984,-0.675905047473435,
48.6774945764827));
#237694=CARTESIAN_POINT('Ctrl Pts',(-7.88271582337061,-0.668375304900736,
48.6771880762194));
#237695=CARTESIAN_POINT('Ctrl Pts',(-7.88302310419652,-0.664741332275987,
48.6770400174397));
#237696=CARTESIAN_POINT('Ctrl Pts',(-7.88368395296132,-0.656861085553477,
48.676718653775));
#237697=CARTESIAN_POINT('Ctrl Pts',(-7.88403660313302,-0.652614737967597,
48.6765452955303));
#237698=CARTESIAN_POINT('Ctrl Pts',(-7.88488459467025,-0.64230286066898,
48.6761238491736));
#237699=CARTESIAN_POINT('Ctrl Pts',(-7.88537636808917,-0.636237038868326,
48.6758755514612));
#237700=CARTESIAN_POINT('Ctrl Pts',(-7.88669645817127,-0.619717629343189,
48.6751982801246));
#237701=CARTESIAN_POINT('Ctrl Pts',(-7.8875109858695,-0.609263004909966,
48.6747684948195));
#237702=CARTESIAN_POINT('Ctrl Pts',(-7.90323768057082,-0.402089420018049,
48.6662291460158));
#237703=CARTESIAN_POINT('Ctrl Pts',(-7.91080563654813,-0.204897649807095,
48.6577000542341));
#237704=CARTESIAN_POINT('Ctrl Pts',(-7.91099630412092,-0.00764697228234312,
48.6489209116116));
#237705=CARTESIAN_POINT('',(-7.91143166941437,0.00169103298945927,44.6423315082371));
#237706=CARTESIAN_POINT('Ctrl Pts',(-7.91099626150122,-0.00769093712042951,
48.6489228683743));
#237707=CARTESIAN_POINT('Ctrl Pts',(-7.91164791772632,0.662610988365909,
48.6190895035468));
#237708=CARTESIAN_POINT('Ctrl Pts',(-7.82711173938375,1.33033400700045,
48.5868061908958));
#237709=CARTESIAN_POINT('Ctrl Pts',(-7.56272340494108,2.35334709170472,
48.5394353254642));
#237710=CARTESIAN_POINT('Ctrl Pts',(-7.43885343323155,2.71965928564517,
48.5228574067941));
#237711=CARTESIAN_POINT('Ctrl Pts',(-7.28054940035535,3.09482819938831,
48.5064056155218));
#237712=CARTESIAN_POINT('Ctrl Pts',(-7.27231631601591,3.11412532889468,
48.5055607992272));
#237713=CARTESIAN_POINT('Ctrl Pts',(-7.26037555434932,3.14180709915026,
48.5043508811569));
#237714=CARTESIAN_POINT('Ctrl Pts',(-7.25672995232899,3.15021831596243,
48.5039835051861));
#237715=CARTESIAN_POINT('Ctrl Pts',(-7.25038044184114,3.1647985426772,48.5033471375152));
#237716=CARTESIAN_POINT('Ctrl Pts',(-7.24768326417479,3.17097046180989,
48.5030778989516));
#237717=CARTESIAN_POINT('Ctrl Pts',(-7.24248427103993,3.18282596849578,
48.5025609929336));
#237718=CARTESIAN_POINT('Ctrl Pts',(-7.23998364027211,3.18851006754165,
48.5023132822061));
#237719=CARTESIAN_POINT('Ctrl Pts',(-7.2340808919189,3.20188465860019,48.5017307009548));
#237720=CARTESIAN_POINT('Ctrl Pts',(-7.23067319599463,3.20957268980701,
48.5013960361421));
#237721=CARTESIAN_POINT('Ctrl Pts',(-7.21887117103174,3.23608479888389,
48.5002426883938));
#237722=CARTESIAN_POINT('Ctrl Pts',(-7.21041550464177,3.25488157523169,
48.4994262692693));
#237723=CARTESIAN_POINT('Ctrl Pts',(-7.11550591576871,3.46367881514814,
48.4903713846731));
#237724=CARTESIAN_POINT('Ctrl Pts',(-7.02163462186226,3.65022614488148,
48.4824142806544));
#237725=CARTESIAN_POINT('Ctrl Pts',(-6.90912552480948,3.85336937889999,
48.4738349677696));
#237726=CARTESIAN_POINT('Ctrl Pts',(-6.89767092776954,3.87383619562231,
48.4729715458886));
#237727=CARTESIAN_POINT('Ctrl Pts',(-6.5165657367382,4.54773666085987,48.444569700496));
#237728=CARTESIAN_POINT('Ctrl Pts',(-6.05593026730365,5.14520197799945,
48.420740272478));
#237729=CARTESIAN_POINT('Ctrl Pts',(-5.42747543611767,5.75694397000242,
48.389967159942));
#237730=CARTESIAN_POINT('Ctrl Pts',(-5.33481663504837,5.84291221156716,
48.385453449272));
#237731=CARTESIAN_POINT('Ctrl Pts',(-5.10686044411135,6.04446425561905,
48.3742918660903));
#237732=CARTESIAN_POINT('Ctrl Pts',(-4.96965073242299,6.15777030377607,
48.3675276026204));
#237733=CARTESIAN_POINT('Ctrl Pts',(-4.81974343042241,6.27328649923102,
48.359945201152));
#237734=CARTESIAN_POINT('Ctrl Pts',(-4.81072369648317,6.28020602766404,
48.3594882579054));
#237735=CARTESIAN_POINT('Ctrl Pts',(-4.79855073843631,6.28950295375264,
48.3588705546121));
#237736=CARTESIAN_POINT('Ctrl Pts',(-4.79541056537802,6.29189749630896,
48.3587111189372));
#237737=CARTESIAN_POINT('Ctrl Pts',(-4.78951436177792,6.29638667502592,
48.3584115791611));
#237738=CARTESIAN_POINT('Ctrl Pts',(-4.78675875949195,6.29848184576806,
48.3582715183897));
#237739=CARTESIAN_POINT('Ctrl Pts',(-4.78101743996767,6.30284120693398,
48.357979556023));
#237740=CARTESIAN_POINT('Ctrl Pts',(-4.77803148816639,6.30510508549159,
48.3578276305779));
#237741=CARTESIAN_POINT('Ctrl Pts',(-4.77117625249734,6.31029489803012,
48.3574786514511));
#237742=CARTESIAN_POINT('Ctrl Pts',(-4.76730588703944,6.31321939359672,
48.3572814884621));
#237743=CARTESIAN_POINT('Ctrl Pts',(-4.75508028050654,6.32243955855908,
48.3566582778941));
#237744=CARTESIAN_POINT('Ctrl Pts',(-4.74671527130343,6.32872219146621,
48.3562312499412));
#237745=CARTESIAN_POINT('Ctrl Pts',(-4.67806032983215,6.3800735593634,48.3527216113364));
#237746=CARTESIAN_POINT('Ctrl Pts',(-4.61714431659378,6.424294879196,48.3495769969414));
#237747=CARTESIAN_POINT('Ctrl Pts',(-4.43471670617654,6.55279135583343,
48.3400937281315));
#237748=CARTESIAN_POINT('Ctrl Pts',(-4.31146699714319,6.6345334940547,48.3336019948001));
#237749=CARTESIAN_POINT('Ctrl Pts',(-4.00771767056835,6.82394808415077,
48.3175432042965));
#237750=CARTESIAN_POINT('Ctrl Pts',(-3.82507750996235,6.92797541912186,
48.3078395628417));
#237751=CARTESIAN_POINT('Ctrl Pts',(-3.49322621780812,7.09986381864569,
48.2903913324137));
#237752=CARTESIAN_POINT('Ctrl Pts',(-3.34563158485885,7.17059581106805,
48.2826917718914));
#237753=CARTESIAN_POINT('Ctrl Pts',(-2.87995336003558,7.37625375905966,
48.2587665527189));
#237754=CARTESIAN_POINT('Ctrl Pts',(-2.55513872036533,7.49496771270357,
48.2426164241586));
#237755=CARTESIAN_POINT('Ctrl Pts',(-1.92387198622441,7.67985509310382,
48.2129055711801));
#237756=CARTESIAN_POINT('Ctrl Pts',(-1.61920035885695,7.74981792725625,
48.1992684735961));
#237757=CARTESIAN_POINT('Ctrl Pts',(-1.20324504779625,7.81972491483518,
48.1816645555034));
#237758=CARTESIAN_POINT('Ctrl Pts',(-1.09495900617121,7.83562138489461,
48.1771710997982));
#237759=CARTESIAN_POINT('Ctrl Pts',(-0.969915592877777,7.85133491372611,
48.172081143961));
#237760=CARTESIAN_POINT('Ctrl Pts',(-0.953449816019706,7.85335149077491,
48.1714128576817));
#237761=CARTESIAN_POINT('Ctrl Pts',(-0.928498969036424,7.85632761390697,
48.1704031369641));
#237762=CARTESIAN_POINT('Ctrl Pts',(-0.920018538811382,7.85732523199819,
48.1700604622762));
#237763=CARTESIAN_POINT('Ctrl Pts',(-0.904758108076628,7.85909538882041,
48.1694447446672));
#237764=CARTESIAN_POINT('Ctrl Pts',(-0.89797869842171,7.85987288842498,
48.1691715405684));
#237765=CARTESIAN_POINT('Ctrl Pts',(-0.884419813309074,7.86141012363792,
48.1686257807841));
#237766=CARTESIAN_POINT('Ctrl Pts',(-0.877640344171195,7.86216986364495,
48.1683532251655));
#237767=CARTESIAN_POINT('Ctrl Pts',(-0.858733845965238,7.86426385788495,
48.1675940286768));
#237768=CARTESIAN_POINT('Ctrl Pts',(-0.846604676376769,7.86557883237744,
48.1671080138349));
#237769=CARTESIAN_POINT('Ctrl Pts',(-0.797959647548427,7.87073882099469,
48.1651629305347));
#237770=CARTESIAN_POINT('Ctrl Pts',(-0.761419986069347,7.87435767790698,
48.1637111886542));
#237771=CARTESIAN_POINT('Ctrl Pts',(-0.148815339735849,7.93072552491043,
48.1395236409995));
#237772=CARTESIAN_POINT('Ctrl Pts',(0.431333047120447,7.92039036244018,
48.1190414103495));
#237773=CARTESIAN_POINT('Ctrl Pts',(1.40121433934112,7.79614851755108,48.0852321336883));
#237774=CARTESIAN_POINT('Ctrl Pts',(1.79281738828514,7.71551123934827,48.0716489341533));
#237775=CARTESIAN_POINT('Ctrl Pts',(2.27466912532441,7.577611618939,48.0534932253593));
#237776=CARTESIAN_POINT('Ctrl Pts',(2.3721429801864,7.54766547611505,48.049742488657));
#237777=CARTESIAN_POINT('Ctrl Pts',(2.59564961580598,7.47424195990608,48.0409080683694));
#237778=CARTESIAN_POINT('Ctrl Pts',(2.7212016876782,7.42945150301658,48.0357623131637));
#237779=CARTESIAN_POINT('Ctrl Pts',(2.87083519215558,7.37176771595247,48.0293827703455));
#237780=CARTESIAN_POINT('Ctrl Pts',(2.89604598425466,7.36189999869819,48.0282998957074));
#237781=CARTESIAN_POINT('Ctrl Pts',(2.92997690475974,7.34841788575881,48.0268320155387));
#237782=CARTESIAN_POINT('Ctrl Pts',(2.93874212864078,7.3449169353033,48.0264518806728));
#237783=CARTESIAN_POINT('Ctrl Pts',(2.95256096566265,7.33936880623374,48.0258511071557));
#237784=CARTESIAN_POINT('Ctrl Pts',(2.95761878039787,7.33733206823279,48.0256309074573));
#237785=CARTESIAN_POINT('Ctrl Pts',(2.96801042737812,7.33313495171264,48.0251778558198));
#237786=CARTESIAN_POINT('Ctrl Pts',(2.97334401535499,7.3309739791643,48.0249449792933));
#237787=CARTESIAN_POINT('Ctrl Pts',(2.98546293331624,7.32604844083083,48.0244150627199));
#237788=CARTESIAN_POINT('Ctrl Pts',(2.99224678479662,7.32328026652157,48.0241178749044));
#237789=CARTESIAN_POINT('Ctrl Pts',(3.01237042260991,7.31503611566253,48.0232346662927));
#237790=CARTESIAN_POINT('Ctrl Pts',(3.02569905330234,7.30953310218356,48.0226475564617));
#237791=CARTESIAN_POINT('Ctrl Pts',(3.11585489173414,7.27202147060471,48.0186621665154));
#237792=CARTESIAN_POINT('Ctrl Pts',(3.19218638090611,7.23883923735941,48.0152183089434));
#237793=CARTESIAN_POINT('Ctrl Pts',(3.50128965375392,7.09862846713809,48.0010193650734));
#237794=CARTESIAN_POINT('Ctrl Pts',(3.72931472324528,6.98152976718042,47.9899568984898));
#237795=CARTESIAN_POINT('Ctrl Pts',(4.33540487570436,6.63210478696252,47.9594509675495));
#237796=CARTESIAN_POINT('Ctrl Pts',(4.7002752821341,6.37871321579496,47.9398839873903));
#237797=CARTESIAN_POINT('Ctrl Pts',(5.31550270848996,5.86986667640528,47.905593310329));
#237798=CARTESIAN_POINT('Ctrl Pts',(5.57349016989947,5.62548975807045,47.8907088750727));
#237799=CARTESIAN_POINT('Ctrl Pts',(5.85965286627001,5.31534392419588,47.8735155990729));
#237800=CARTESIAN_POINT('Ctrl Pts',(5.90447332132728,5.26551115058837,47.8707998545952));
#237801=CARTESIAN_POINT('Ctrl Pts',(5.96305759529284,5.19868660470533,47.8672178124476));
#237802=CARTESIAN_POINT('Ctrl Pts',(5.97739168188314,5.18219904920756,47.8663387721762));
#237803=CARTESIAN_POINT('Ctrl Pts',(6.00068108105965,5.15518559733434,47.864906287427));
#237804=CARTESIAN_POINT('Ctrl Pts',(6.00967740954633,5.14469526931984,47.8643518922996));
#237805=CARTESIAN_POINT('Ctrl Pts',(6.02697782338581,5.12441451524966,47.8632837344666));
#237806=CARTESIAN_POINT('Ctrl Pts',(6.03528565405263,5.11462734545,47.8627698849495));
#237807=CARTESIAN_POINT('Ctrl Pts',(6.05431508747019,5.09209849888594,47.8615907968072));
#237808=CARTESIAN_POINT('Ctrl Pts',(6.06502036613315,5.07934309351674,47.8609259456079));
#237809=CARTESIAN_POINT('Ctrl Pts',(6.09887349949267,5.03874725911853,47.8588185934831));
#237810=CARTESIAN_POINT('Ctrl Pts',(6.12187062922111,5.01078156875489,47.8573796978197));
#237811=CARTESIAN_POINT('Ctrl Pts',(6.34222752784816,4.73903477931616,47.8435205584969));
#237812=CARTESIAN_POINT('Ctrl Pts',(6.52512196159636,4.48387107694677,47.8314735615384));
#237813=CARTESIAN_POINT('Ctrl Pts',(6.98320898283572,3.75714588720639,47.7992953107247));
#237814=CARTESIAN_POINT('Ctrl Pts',(7.22552720475665,3.26696852218822,47.7799469547945));
#237815=CARTESIAN_POINT('Ctrl Pts',(7.5019114838266,2.52324829553692,47.7505871945972));
#237816=CARTESIAN_POINT('Ctrl Pts',(7.57733559644206,2.28679475633846,47.7412274259359));
#237817=CARTESIAN_POINT('Ctrl Pts',(7.65052373696703,2.01360801038185,47.7300284135753));
#237818=CARTESIAN_POINT('Ctrl Pts',(7.65930241548482,1.97995381891484,47.7286421611545));
#237819=CARTESIAN_POINT('Ctrl Pts',(7.67020179464787,1.93701216598482,47.7268637241967));
#237820=CARTESIAN_POINT('Ctrl Pts',(7.67252812342186,1.92777693106521,47.7264806794888));
#237821=CARTESIAN_POINT('Ctrl Pts',(7.67601634825423,1.91382278161091,47.7259010278631));
#237822=CARTESIAN_POINT('Ctrl Pts',(7.67719058741939,1.9091069384319,47.7257049808064));
#237823=CARTESIAN_POINT('Ctrl Pts',(7.67949766712264,1.89980496279101,47.7253179738754));
#237824=CARTESIAN_POINT('Ctrl Pts',(7.68063074680038,1.89521889161692,47.725127025079));
#237825=CARTESIAN_POINT('Ctrl Pts',(7.68313469287715,1.88504519627132,47.7247030967469));
#237826=CARTESIAN_POINT('Ctrl Pts',(7.6845035720382,1.87945708967914,47.724470025349));
#237827=CARTESIAN_POINT('Ctrl Pts',(7.6881695875273,1.86442053826833,47.7238422698674));
#237828=CARTESIAN_POINT('Ctrl Pts',(7.69045539647751,1.85496936459352,47.72344705524));
#237829=CARTESIAN_POINT('Ctrl Pts',(7.70075933444319,1.81201908242679,47.721648021481));
#237830=CARTESIAN_POINT('Ctrl Pts',(7.70857600681764,1.77847221666756,47.7202345300573));
#237831=CARTESIAN_POINT('Ctrl Pts',(7.8358553386864,1.21561856284086,47.6963657250822));
#237832=CARTESIAN_POINT('Ctrl Pts',(7.90075749779283,0.675494280796114,
47.6713061155912));
#237833=CARTESIAN_POINT('Ctrl Pts',(7.9181632415298,-0.359367472907174,
47.6235748808032));
#237834=CARTESIAN_POINT('Ctrl Pts',(7.88044781417404,-0.851513552323777,
47.6010161602236));
#237835=CARTESIAN_POINT('Ctrl Pts',(7.75897777392869,-1.55991840891451,
47.569917771904));
#237836=CARTESIAN_POINT('Ctrl Pts',(7.71120648062879,-1.78111952380973,
47.5603939626964));
#237837=CARTESIAN_POINT('Ctrl Pts',(7.64385662378762,-2.03887039919428,
47.5495188688549));
#237838=CARTESIAN_POINT('Ctrl Pts',(7.6333987453365,-2.07768145879723,47.5478872392832));
#237839=CARTESIAN_POINT('Ctrl Pts',(7.61922542006292,-2.12872929772349,
47.5457487453617));
#237840=CARTESIAN_POINT('Ctrl Pts',(7.61577554602076,-2.14103882712643,
47.5452336571527));
#237841=CARTESIAN_POINT('Ctrl Pts',(7.61008422704115,-2.16115827146161,
47.5443927080092));
#237842=CARTESIAN_POINT('Ctrl Pts',(7.60786056714314,-2.16897316912061,
47.5440662951332));
#237843=CARTESIAN_POINT('Ctrl Pts',(7.6035441152359,-2.18405473177788,47.5434368145077));
#237844=CARTESIAN_POINT('Ctrl Pts',(7.60145293653761,-2.19132184713629,
47.5431336969993));
#237845=CARTESIAN_POINT('Ctrl Pts',(7.59662367866529,-2.20801404286949,
47.5424379088335));
#237846=CARTESIAN_POINT('Ctrl Pts',(7.59387847075438,-2.21743705683769,
47.5420454606288));
#237847=CARTESIAN_POINT('Ctrl Pts',(7.58652246918227,-2.24251289709838,
47.5410019907324));
#237848=CARTESIAN_POINT('Ctrl Pts',(7.58188075924071,-2.25815664328931,
47.5403519334927));
#237849=CARTESIAN_POINT('Ctrl Pts',(7.55025697470046,-2.36354010844566,
47.5359789412157));
#237850=CARTESIAN_POINT('Ctrl Pts',(7.52173016133097,-2.45281029152105,
47.5323045272707));
#237851=CARTESIAN_POINT('Ctrl Pts',(7.18153029378573,-3.45560181924886,
47.4913244080797));
#237852=CARTESIAN_POINT('Ctrl Pts',(6.70684949520771,-4.30505050391386,
47.4604883065493));
#237853=CARTESIAN_POINT('Ctrl Pts',(6.02579664882594,-5.12680646109746,
47.421968628824));
#237854=CARTESIAN_POINT('Ctrl Pts',(5.95905156131876,-5.20423609343146,
47.4182276797094));
#237855=CARTESIAN_POINT('Ctrl Pts',(5.78953438319508,-5.39335167910168,
47.4087581054396));
#237856=CARTESIAN_POINT('Ctrl Pts',(5.685015814706,-5.50341220090058,47.4029404670049));
#237857=CARTESIAN_POINT('Ctrl Pts',(5.55631926246223,-5.63135154330612,
47.3957453489449));
#237858=CARTESIAN_POINT('Ctrl Pts',(5.53512836457719,-5.65218169444424,
47.3945603282218));
#237859=CARTESIAN_POINT('Ctrl Pts',(5.50664702358555,-5.6798644031683,47.3929678200024));
#237860=CARTESIAN_POINT('Ctrl Pts',(5.49946003904369,-5.68682339786983,
47.3925659833255));
#237861=CARTESIAN_POINT('Ctrl Pts',(5.48765159273853,-5.69821393008731,
47.3919058075313));
#237862=CARTESIAN_POINT('Ctrl Pts',(5.48303790423802,-5.70265353469084,
47.3916478833134));
#237863=CARTESIAN_POINT('Ctrl Pts',(5.47407735184347,-5.71125506022064,
47.3911469862032));
#237864=CARTESIAN_POINT('Ctrl Pts',(5.46973111745684,-5.71541763297707,
47.3909040464157));
#237865=CARTESIAN_POINT('Ctrl Pts',(5.45966980136849,-5.72503179397972,
47.3903416975435));
#237866=CARTESIAN_POINT('Ctrl Pts',(5.45395130169864,-5.73047978621501,
47.3900221113531));
#237867=CARTESIAN_POINT('Ctrl Pts',(5.43635448925281,-5.74719400138421,
47.3890388155757));
#237868=CARTESIAN_POINT('Ctrl Pts',(5.42444939345269,-5.75843188686159,
47.3883737446472));
#237869=CARTESIAN_POINT('Ctrl Pts',(5.32549952995165,-5.85125704755426,
47.3828480034995));
#237870=CARTESIAN_POINT('Ctrl Pts',(5.23665625844741,-5.93090078000216,
47.3778999382196));
#237871=CARTESIAN_POINT('Ctrl Pts',(5.13331565004882,-6.01940798472861,
47.3721876621747));
#237872=CARTESIAN_POINT('Ctrl Pts',(5.12054818087192,-6.03027266164513,
47.3714826526186));
#237873=CARTESIAN_POINT('Ctrl Pts',(5.1028638937583,-6.04522472376653,47.3705072298042));
#237874=CARTESIAN_POINT('Ctrl Pts',(5.09797647939127,-6.04934688164466,
47.3702377661627));
#237875=CARTESIAN_POINT('Ctrl Pts',(5.0778295247574,-6.06629753155847,47.369127464889));
#237876=CARTESIAN_POINT('Ctrl Pts',(5.06252655876757,-6.07907421084948,
47.3682852600263));
#237877=CARTESIAN_POINT('Ctrl Pts',(4.72676657057053,-6.35725825692849,
47.3498337452759));
#237878=CARTESIAN_POINT('Ctrl Pts',(4.38591508810346,-6.59702993310786,
47.331695768767));
#237879=CARTESIAN_POINT('Ctrl Pts',(3.65051488629766,-7.03205559198144,
47.2949343267975));
#237880=CARTESIAN_POINT('Ctrl Pts',(3.25533261519665,-7.22349662895991,
47.2764103480214));
#237881=CARTESIAN_POINT('Ctrl Pts',(2.54179739579593,-7.49864697020106,
47.2448001249646));
#237882=CARTESIAN_POINT('Ctrl Pts',(2.23029748456682,-7.59711921350632,
47.2314969827077));
#237883=CARTESIAN_POINT('Ctrl Pts',(1.85766486694136,-7.69001470722281,
47.2159496806692));
#237884=CARTESIAN_POINT('Ctrl Pts',(1.80157227704531,-7.7033487738541,47.2136203603499));
#237885=CARTESIAN_POINT('Ctrl Pts',(1.71646537542548,-7.72259955853075,
47.2101027701486));
#237886=CARTESIAN_POINT('Ctrl Pts',(1.68755550901289,-7.72896847820476,
47.2089107638258));
#237887=CARTESIAN_POINT('Ctrl Pts',(1.6373263615106,-7.73973883474461,47.2068446805466));
#237888=CARTESIAN_POINT('Ctrl Pts',(1.6160234249689,-7.74421481732105,47.2059699656311));
#237889=CARTESIAN_POINT('Ctrl Pts',(1.56821554746232,-7.75405392403873,
47.2040103654752));
#237890=CARTESIAN_POINT('Ctrl Pts',(1.54170101629998,-7.75936919097492,
47.2029259171615));
#237891=CARTESIAN_POINT('Ctrl Pts',(1.47065338736643,-7.7732332946957,47.2000262828967));
#237892=CARTESIAN_POINT('Ctrl Pts',(1.42607308470058,-7.78153537691466,
47.1982133825744));
#237893=CARTESIAN_POINT('Ctrl Pts',(1.22285735870231,-7.81757474965926,
47.1899782562534));
#237894=CARTESIAN_POINT('Ctrl Pts',(1.06346774005549,-7.84084769504832,
47.1835996718062));
#237895=CARTESIAN_POINT('Ctrl Pts',(0.585235132806012,-7.89582404324409,
47.164656810414));
#237896=CARTESIAN_POINT('Ctrl Pts',(0.265062059889638,-7.9130452019605,
47.1522415973748));
#237897=CARTESIAN_POINT('Ctrl Pts',(-0.424845421560862,-7.90822456977076,
47.1255668533777));
#237898=CARTESIAN_POINT('Ctrl Pts',(-0.793772353520196,-7.87974767875001,
47.1113520754224));
#237899=CARTESIAN_POINT('Ctrl Pts',(-1.24387748904195,-7.81306548385664,
47.0933639008474));
#237900=CARTESIAN_POINT('Ctrl Pts',(-1.32819992645492,-7.79917355143417,
47.0899648516399));
#237901=CARTESIAN_POINT('Ctrl Pts',(-1.43207723812229,-7.78032651164104,
47.0857309247119));
#237902=CARTESIAN_POINT('Ctrl Pts',(-1.45186091071279,-7.77665903421985,
47.0849224637683));
#237903=CARTESIAN_POINT('Ctrl Pts',(-1.48303493967257,-7.77075691907995,
47.0836450416208));
#237904=CARTESIAN_POINT('Ctrl Pts',(-1.49443477874304,-7.76857261141134,
47.0831771711006));
#237905=CARTESIAN_POINT('Ctrl Pts',(-1.51573727336818,-7.76444224444807,
47.0823014559511));
#237906=CARTESIAN_POINT('Ctrl Pts',(-1.5256410975579,-7.76250230853364,
47.081893748887));
#237907=CARTESIAN_POINT('Ctrl Pts',(-1.54770133499664,-7.75813735612915,
47.0809842890247));
#237908=CARTESIAN_POINT('Ctrl Pts',(-1.55985580622623,-7.75570270970725,
47.08048231615));
#237909=CARTESIAN_POINT('Ctrl Pts',(-1.59640447816599,-7.74829230069315,
47.0789701154108));
#237910=CARTESIAN_POINT('Ctrl Pts',(-1.62078077998999,-7.74322997723396,
47.0779577957333));
#237911=CARTESIAN_POINT('Ctrl Pts',(-1.8834225631919,-7.68739156593984,
47.0670115723598));
#237912=CARTESIAN_POINT('Ctrl Pts',(-2.11923978341215,-7.62575154262978,
47.0568413676541));
#237913=CARTESIAN_POINT('Ctrl Pts',(-2.70981564242152,-7.44186791529549,
47.0308351057076));
#237914=CARTESIAN_POINT('Ctrl Pts',(-3.05943082227927,-7.30509335568665,
47.0149493884497));
#237915=CARTESIAN_POINT('Ctrl Pts',(-3.56723494997244,-7.0635589243002,
46.9914902837725));
#237916=CARTESIAN_POINT('Ctrl Pts',(-3.73353259683494,-6.97708867872951,
46.9837365138791));
#237917=CARTESIAN_POINT('Ctrl Pts',(-3.96243897957423,-6.84753391324431,
46.9729613729912));
#237918=CARTESIAN_POINT('Ctrl Pts',(-4.02773512985558,-6.80933133599963,
46.9698753981089));
#237919=CARTESIAN_POINT('Ctrl Pts',(-4.14165889584774,-6.7404662846283,
46.9644676067707));
#237920=CARTESIAN_POINT('Ctrl Pts',(-4.19051880494137,-6.71019942766042,
46.962140475121));
#237921=CARTESIAN_POINT('Ctrl Pts',(-4.26139950981679,-6.66521539255381,
46.9587520799467));
#237922=CARTESIAN_POINT('Ctrl Pts',(-4.28368289485535,-6.65091594251652,
46.9576850178575));
#237923=CARTESIAN_POINT('Ctrl Pts',(-4.32279036419075,-6.62554225168772,
46.9558089649588));
#237924=CARTESIAN_POINT('Ctrl Pts',(-4.33964470428317,-6.61451513756861,
46.9549993274632));
#237925=CARTESIAN_POINT('Ctrl Pts',(-4.37243637290283,-6.59288158923538,
46.9534218702914));
#237926=CARTESIAN_POINT('Ctrl Pts',(-4.38837767427708,-6.58228143390373,
46.9526539703265));
#237927=CARTESIAN_POINT('Ctrl Pts',(-4.43118081515678,-6.55359491023963,
46.9505892352346));
#237928=CARTESIAN_POINT('Ctrl Pts',(-4.4579703826455,-6.53540126871248,
46.9492938854217));
#237929=CARTESIAN_POINT('Ctrl Pts',(-4.5580486311177,-6.46653328192752,
46.944442574614));
#237930=CARTESIAN_POINT('Ctrl Pts',(-4.63059159534863,-6.41478617760905,
46.9409012877639));
#237931=CARTESIAN_POINT('Ctrl Pts',(-5.26983038060739,-5.94230257982683,
46.9094336644822));
#237932=CARTESIAN_POINT('Ctrl Pts',(-5.7787648833409,-5.44867417119312,
46.8822996055486));
#237933=CARTESIAN_POINT('Ctrl Pts',(-6.41681003677691,-4.63836330232164,
46.8435641468412));
#237934=CARTESIAN_POINT('Ctrl Pts',(-6.60219645247315,-4.37045355110006,
46.8314778529121));
#237935=CARTESIAN_POINT('Ctrl Pts',(-6.88397742347322,-3.90421112663448,
46.8109531215989));
#237936=CARTESIAN_POINT('Ctrl Pts',(-6.98954822631143,-3.71190247040105,
46.8026152994368));
#237937=CARTESIAN_POINT('Ctrl Pts',(-7.12823091426804,-3.43232540823938,
46.7904336545306));
#237938=CARTESIAN_POINT('Ctrl Pts',(-7.1680041551118,-3.34846971559125,
46.7867720642286));
#237939=CARTESIAN_POINT('Ctrl Pts',(-7.21271025299846,-3.24976519090757,
46.7824361466163));
#237940=CARTESIAN_POINT('Ctrl Pts',(-7.21908655071576,-3.23557604752589,
46.781812220806));
#237941=CARTESIAN_POINT('Ctrl Pts',(-7.22875861268694,-3.21388193691375,
46.780857230924));
#237942=CARTESIAN_POINT('Ctrl Pts',(-7.23208465038839,-3.20639046187242,
46.7805272593346));
#237943=CARTESIAN_POINT('Ctrl Pts',(-7.23785002500948,-3.19335008355712,
46.7799525280505));
#237944=CARTESIAN_POINT('Ctrl Pts',(-7.24029464143683,-3.1878035142746,
46.7797079626353));
#237945=CARTESIAN_POINT('Ctrl Pts',(-7.24576104728485,-3.17536210780843,
46.7791591258388));
#237946=CARTESIAN_POINT('Ctrl Pts',(-7.24877937256675,-3.16846576081492,
46.7788547257878));
#237947=CARTESIAN_POINT('Ctrl Pts',(-7.25678380875276,-3.15010571740462,
46.7780438351657));
#237948=CARTESIAN_POINT('Ctrl Pts',(-7.26175258739268,-3.13863451761687,
46.7775366891549));
#237949=CARTESIAN_POINT('Ctrl Pts',(-7.2827125407002,-3.08992899004435,
46.7753810871942));
#237950=CARTESIAN_POINT('Ctrl Pts',(-7.29844451873437,-3.05258425654252,
46.7737225686046));
#237951=CARTESIAN_POINT('Ctrl Pts',(-7.64406237031845,-2.21420639352112,
46.7363329003107));
#237952=CARTESIAN_POINT('Ctrl Pts',(-7.84040113190449,-1.36462053495646,
46.6945171896527));
#237953=CARTESIAN_POINT('Ctrl Pts',(-7.90570422276263,-0.333951554203285,
46.6486976052779));
#237954=CARTESIAN_POINT('Ctrl Pts',(-7.9109843985096,-0.167369534641295,
46.6414201239052));
#237955=CARTESIAN_POINT('Ctrl Pts',(-7.91101914685337,0.204580413004452,
46.6254962739105));
#237956=CARTESIAN_POINT('Ctrl Pts',(-7.90304521296736,0.40983116605556,
46.616931548811));
#237957=CARTESIAN_POINT('Ctrl Pts',(-7.88553970957431,0.634495654482527,
46.6078024804637));
#237958=CARTESIAN_POINT('Ctrl Pts',(-7.88390990811863,0.654435493437473,
46.6069943435935));
#237959=CARTESIAN_POINT('Ctrl Pts',(-7.88137736095431,0.684036577842264,
46.6057977473433));
#237960=CARTESIAN_POINT('Ctrl Pts',(-7.88053245831373,0.69370261631616,
46.6054074976996));
#237961=CARTESIAN_POINT('Ctrl Pts',(-7.87905553467166,0.710248273071947,
46.6047403321912));
#237962=CARTESIAN_POINT('Ctrl Pts',(-7.87843228212967,0.717128652384837,
46.6044631445851));
#237963=CARTESIAN_POINT('Ctrl Pts',(-7.87720217828301,0.730513185691244,
46.6039244068364));
#237964=CARTESIAN_POINT('Ctrl Pts',(-7.87659628220425,0.737017421410841,
46.6036628272313));
#237965=CARTESIAN_POINT('Ctrl Pts',(-7.87512780889711,0.752572693193192,
46.6030377703939));
#237966=CARTESIAN_POINT('Ctrl Pts',(-7.87425768228362,0.761623016127559,
46.6026745281692));
#237967=CARTESIAN_POINT('Ctrl Pts',(-7.87160217877376,0.788752289338839,
46.6015869447471));
#237968=CARTESIAN_POINT('Ctrl Pts',(-7.86977012189251,0.806826666005331,
46.6008640573136));
#237969=CARTESIAN_POINT('Ctrl Pts',(-7.85327560144176,0.964152014989901,
46.594586404731));
#237970=CARTESIAN_POINT('Ctrl Pts',(-7.83498040868318,1.10300100843181,
46.5891462657306));
#237971=CARTESIAN_POINT('Ctrl Pts',(-7.77935501718813,1.45312032543868,
46.5756500914551));
#237972=CARTESIAN_POINT('Ctrl Pts',(-7.73709979674496,1.66349544685578,
46.5677487879319));
#237973=CARTESIAN_POINT('Ctrl Pts',(-7.51899058819125,2.55908857585947,
46.5346624953478));
#237974=CARTESIAN_POINT('Ctrl Pts',(-7.2602604731843,3.22066128629926,46.5119160306334));
#237975=CARTESIAN_POINT('Ctrl Pts',(-6.78241530144773,4.08163811306552,
46.4768525218232));
#237976=CARTESIAN_POINT('Ctrl Pts',(-6.63508911507151,4.31700060822855,
46.4665784875517));
#237977=CARTESIAN_POINT('Ctrl Pts',(-6.46600140977416,4.55796368165872,
46.4548228171509));
#237978=CARTESIAN_POINT('Ctrl Pts',(-6.45624040394983,4.57177941205441,
46.4541443030755));
#237979=CARTESIAN_POINT('Ctrl Pts',(-6.442756868781,4.59073471246363,46.4532070337478));
#237980=CARTESIAN_POINT('Ctrl Pts',(-6.43907229553737,4.5959013526013,46.4529509119981));
#237981=CARTESIAN_POINT('Ctrl Pts',(-6.43320054552772,4.60411400847454,
46.4525427478832));
#237982=CARTESIAN_POINT('Ctrl Pts',(-6.43101740611882,4.60716292137744,
46.4523909892367));
#237983=CARTESIAN_POINT('Ctrl Pts',(-6.42677073654578,4.61308480433933,
46.4520957810424));
#237984=CARTESIAN_POINT('Ctrl Pts',(-6.42470744569853,4.61595794491736,
46.4519523484376));
#237985=CARTESIAN_POINT('Ctrl Pts',(-6.41977611291144,4.62281513349123,
46.4516095316173));
#237986=CARTESIAN_POINT('Ctrl Pts',(-6.41690629109887,4.62679789372693,
46.4514100204948));
#237987=CARTESIAN_POINT('Ctrl Pts',(-6.40831368005967,4.63869941203079,
46.4508126314973));
#237988=CARTESIAN_POINT('Ctrl Pts',(-6.40257995358048,4.64661020477595,
46.4504139638445));
#237989=CARTESIAN_POINT('Ctrl Pts',(-6.34698984029864,4.72300934463816,
46.4465482775541));
#237990=CARTESIAN_POINT('Ctrl Pts',(-6.29605281505008,4.79070091192116,
46.4430028325326));
#237991=CARTESIAN_POINT('Ctrl Pts',(-6.08546707048257,5.0613936472923,46.4283823619154));
#237992=CARTESIAN_POINT('Ctrl Pts',(-5.91701729527572,5.25732855099089,
46.4167753595818));
#237993=CARTESIAN_POINT('Ctrl Pts',(-5.33373177489051,5.87217890901269,
46.3779072500078));
#237994=CARTESIAN_POINT('Ctrl Pts',(-4.88160528106935,6.25309762320797,
46.3499414274239));
#237995=CARTESIAN_POINT('Ctrl Pts',(-4.12016044708525,6.76125015596907,
46.3093915908466));
#237996=CARTESIAN_POINT('Ctrl Pts',(-3.83801486155599,6.92530890395117,
46.2955137683405));
#237997=CARTESIAN_POINT('Ctrl Pts',(-3.52595838988207,7.08181245173011,
46.2813933372183));
#237998=CARTESIAN_POINT('Ctrl Pts',(-3.50535082630986,7.09203537538503,
46.2804662759181));
#237999=CARTESIAN_POINT('Ctrl Pts',(-3.47678514542058,7.10605120695807,
46.2791886468821));
#238000=CARTESIAN_POINT('Ctrl Pts',(-3.46886494757564,7.109920863096,46.2788351960316));
#238001=CARTESIAN_POINT('Ctrl Pts',(-3.45525896034505,7.11654033966704,
46.2782293561906));
#238002=CARTESIAN_POINT('Ctrl Pts',(-3.44957632366842,7.11929659984846,
46.2779767257125));
#238003=CARTESIAN_POINT('Ctrl Pts',(-3.4378844952586,7.12495022453766,46.277457773404));
#238004=CARTESIAN_POINT('Ctrl Pts',(-3.43187492585763,7.12784679959228,
46.2771914812712));
#238005=CARTESIAN_POINT('Ctrl Pts',(-3.4179527872306,7.13453549524244,46.2765756068396));
#238006=CARTESIAN_POINT('Ctrl Pts',(-3.41003755145934,7.13832206382818,
46.2762262324559));
#238007=CARTESIAN_POINT('Ctrl Pts',(-3.38509523954811,7.15020326021038,
46.2751277142923));
#238008=CARTESIAN_POINT('Ctrl Pts',(-3.36804545601702,7.1582502230721,46.2743803510417));
#238009=CARTESIAN_POINT('Ctrl Pts',(-3.11999583824539,7.27423943376218,
46.2635583934711));
#238010=CARTESIAN_POINT('Ctrl Pts',(-2.88392894132317,7.37101769589469,
46.2539092775393));
#238011=CARTESIAN_POINT('Ctrl Pts',(-2.45816857229417,7.52196973683812,
46.2374324778464));
#238012=CARTESIAN_POINT('Ctrl Pts',(-2.27036081818771,7.58077092814684,
46.230467930732));
#238013=CARTESIAN_POINT('Ctrl Pts',(-1.5998579774445,7.76354365030446,46.2063476036101));
#238014=CARTESIAN_POINT('Ctrl Pts',(-1.10788731374773,7.84886694339196,
46.19005935218));
#238015=CARTESIAN_POINT('Ctrl Pts',(-0.490210998109943,7.8967293271967,
46.1685260140483));
#238016=CARTESIAN_POINT('Ctrl Pts',(-0.369051197926477,7.90331833395652,
46.1642462393734));
#238017=CARTESIAN_POINT('Ctrl Pts',(-0.0326616750813311,7.91386001225206,
46.1520963967267));
#238018=CARTESIAN_POINT('Ctrl Pts',(0.182637893657517,7.91181879906,46.1440174185811));
#238019=CARTESIAN_POINT('Ctrl Pts',(0.410882353412002,7.9003338149808,46.1348772701185));
#238020=CARTESIAN_POINT('Ctrl Pts',(0.424193995312145,7.89963025377752,
46.1343421139178));
#238021=CARTESIAN_POINT('Ctrl Pts',(0.442470771810868,7.89861794008617,
46.1336044048347));
#238022=CARTESIAN_POINT('Ctrl Pts',(0.447437560064625,7.89833814021777,
46.1334036305564));
#238023=CARTESIAN_POINT('Ctrl Pts',(0.455944787830551,7.89785084235624,
46.1330592239558));
#238024=CARTESIAN_POINT('Ctrl Pts',(0.459485340559439,7.89764564914033,
46.1329157355235));
#238025=CARTESIAN_POINT('Ctrl Pts',(0.466390677394443,7.89724079015637,
46.1326355858701));
#238026=CARTESIAN_POINT('Ctrl Pts',(0.469755474767058,7.89704135455257,
46.1324989387917));
#238027=CARTESIAN_POINT('Ctrl Pts',(0.477830560657102,7.89655755522796,
46.1321706756795));
#238028=CARTESIAN_POINT('Ctrl Pts',(0.482540719983266,7.89627112763345,
46.1319789339037));
#238029=CARTESIAN_POINT('Ctrl Pts',(0.496757000986494,7.89539385955919,
46.1313994143855));
#238030=CARTESIAN_POINT('Ctrl Pts',(0.506262282690488,7.89479006783097,
46.1310108547932));
#238031=CARTESIAN_POINT('Ctrl Pts',(0.592795251856389,7.88913642675631,
46.1274638362563));
#238032=CARTESIAN_POINT('Ctrl Pts',(0.669743771186503,7.88297673824935,
46.1242397146186));
#238033=CARTESIAN_POINT('Ctrl Pts',(1.00689969050782,7.851015574393,46.1098436161027));
#238034=CARTESIAN_POINT('Ctrl Pts',(1.26581026973013,7.81344969823005,46.0980864655485));
#238035=CARTESIAN_POINT('Ctrl Pts',(1.98903841689542,7.67162352792478,46.0641367407087));
#238036=CARTESIAN_POINT('Ctrl Pts',(2.44651220492522,7.53821461255747,46.041407712751));
#238037=CARTESIAN_POINT('Ctrl Pts',(3.31494170402759,7.1975129799865,45.998324135843));
#238038=CARTESIAN_POINT('Ctrl Pts',(3.72539586055095,6.9938938100647,45.9779972051401));
#238039=CARTESIAN_POINT('Ctrl Pts',(4.19582424969576,6.7072883231408,45.955107865128));
#238040=CARTESIAN_POINT('Ctrl Pts',(4.27478097233938,6.65724464373,45.9512779243765));
#238041=CARTESIAN_POINT('Ctrl Pts',(4.36572519529921,6.5973178527296,45.9468779184628));
#238042=CARTESIAN_POINT('Ctrl Pts',(4.37859130219193,6.58878574115383,45.9462557052739));
#238043=CARTESIAN_POINT('Ctrl Pts',(4.39905322189861,6.57513008952619,45.9452665573415));
#238044=CARTESIAN_POINT('Ctrl Pts',(4.40666521883834,6.57003094308754,45.9448986758088));
#238045=CARTESIAN_POINT('Ctrl Pts',(4.42006581944261,6.5610203443173,45.9442511880732));
#238046=CARTESIAN_POINT('Ctrl Pts',(4.42585812493511,6.55711443128995,45.943971366806));
#238047=CARTESIAN_POINT('Ctrl Pts',(4.43780448421693,6.54903562709445,45.9433943494475));
#238048=CARTESIAN_POINT('Ctrl Pts',(4.44395784547117,6.54486172147018,45.9430971933014));
#238049=CARTESIAN_POINT('Ctrl Pts',(4.4596560689931,6.53418106483038,45.9423392368472));
#238050=CARTESIAN_POINT('Ctrl Pts',(4.46919259595945,6.52766206106103,45.9418789149905));
#238051=CARTESIAN_POINT('Ctrl Pts',(4.50771455168816,6.50120513385387,45.9400199829574));
#238052=CARTESIAN_POINT('Ctrl Pts',(4.53658132250954,6.48109470829839,45.9386281199425));
#238053=CARTESIAN_POINT('Ctrl Pts',(4.72269177450918,6.34958567964282,45.9296604984897));
#238054=CARTESIAN_POINT('Ctrl Pts',(4.87595969684265,6.23266227309692,45.9223056904432));
#238055=CARTESIAN_POINT('Ctrl Pts',(5.16674075911856,5.99353631383202,45.9083098725554));
#238056=CARTESIAN_POINT('Ctrl Pts',(5.30456368744701,5.8719073179548,45.9016556888451));
#238057=CARTESIAN_POINT('Ctrl Pts',(5.85465228922296,5.35126441174039,45.8747259680411));
#238058=CARTESIAN_POINT('Ctrl Pts',(6.22712389008861,4.91282587417699,45.8557056279231));
#238059=CARTESIAN_POINT('Ctrl Pts',(6.62366873227137,4.3276662542269,45.8303253884603));
#238060=CARTESIAN_POINT('Ctrl Pts',(6.6956314675118,4.21547147514043,45.8254528399837));
#238061=CARTESIAN_POINT('Ctrl Pts',(6.84074938123687,3.97612521736984,45.8149379417926));
#238062=CARTESIAN_POINT('Ctrl Pts',(6.91326288913124,3.84866428299787,45.8092563409422));
#238063=CARTESIAN_POINT('Ctrl Pts',(6.99007950811927,3.70445549718361,45.8027195315619));
#238064=CARTESIAN_POINT('Ctrl Pts',(6.99791418982556,3.68963399900479,45.8020466369318));
#238065=CARTESIAN_POINT('Ctrl Pts',(7.00927705363812,3.66797156880741,45.8010617299988));
#238066=CARTESIAN_POINT('Ctrl Pts',(7.0128424899835,3.661150154579,45.8007513797536));
#238067=CARTESIAN_POINT('Ctrl Pts',(7.01913060688919,3.64907680369912,45.8002017310208));
#238068=CARTESIAN_POINT('Ctrl Pts',(7.02185736584784,3.64382698948614,45.7999626110031));
#238069=CARTESIAN_POINT('Ctrl Pts',(7.02749501516782,3.6329430258095,45.7994666267695));
#238070=CARTESIAN_POINT('Ctrl Pts',(7.03040502391157,3.62730842587836,45.7992097248701));
#238071=CARTESIAN_POINT('Ctrl Pts',(7.03777087237578,3.61300389845012,45.7985572037536));
#238072=CARTESIAN_POINT('Ctrl Pts',(7.04221746144918,3.60432923674784,45.7981611937507));
#238073=CARTESIAN_POINT('Ctrl Pts',(7.05991018090416,3.56965553636934,45.7965771364491));
#238074=CARTESIAN_POINT('Ctrl Pts',(7.07302836460833,3.54359170008807,45.7953838269835));
#238075=CARTESIAN_POINT('Ctrl Pts',(7.16179569425834,3.36476772815613,45.7871812659395));
#238076=CARTESIAN_POINT('Ctrl Pts',(7.2326319366691,3.20967452797392,45.7799920601974));
#238077=CARTESIAN_POINT('Ctrl Pts',(7.3735800497196,2.87266468595254,45.764351034622));
#238078=CARTESIAN_POINT('Ctrl Pts',(7.442091699172,2.6901958106158,45.7558715124615));
#238079=CARTESIAN_POINT('Ctrl Pts',(7.63710636232333,2.10611451611819,45.7289449002622));
#238080=CARTESIAN_POINT('Ctrl Pts',(7.73834115391352,1.69682317771659,45.7104284615116));
#238081=CARTESIAN_POINT('Ctrl Pts',(7.81970503848471,1.20114579350319,45.6889167994172));
#238082=CARTESIAN_POINT('Ctrl Pts',(7.83164257362626,1.1206752279207,45.6854509870675));
#238083=CARTESIAN_POINT('Ctrl Pts',(7.84605522142712,1.01199720991207,45.6808067636892));
#238084=CARTESIAN_POINT('Ctrl Pts',(7.8496230466261,0.983940510441004,45.6796110512966));
#238085=CARTESIAN_POINT('Ctrl Pts',(7.88472396204376,0.695564166980198,
45.6673545787445));
#238086=CARTESIAN_POINT('Ctrl Pts',(7.90344690351887,0.4338412695229,45.6565178200312));
#238087=CARTESIAN_POINT('Ctrl Pts',(7.90994359474025,0.134513873435497,
45.6443994715032));
#238088=CARTESIAN_POINT('Ctrl Pts',(7.91048814677211,0.0973599680355795,
45.6428999347237));
#238089=CARTESIAN_POINT('Ctrl Pts',(7.91089923204992,0.0433431444362618,
45.6407265153664));
#238090=CARTESIAN_POINT('Ctrl Pts',(7.91097364256311,0.0264823913665555,
45.6400490617653));
#238091=CARTESIAN_POINT('Ctrl Pts',(7.91100980263998,-0.00324919136649711,
45.6388561571947));
#238092=CARTESIAN_POINT('Ctrl Pts',(7.91099404652836,-0.0161199149451286,
45.6383403104487));
#238093=CARTESIAN_POINT('Ctrl Pts',(7.91089655275947,-0.0427240193872596,
45.6372751984862));
#238094=CARTESIAN_POINT('Ctrl Pts',(7.91081046290157,-0.0564573445869161,
45.6367260130036));
#238095=CARTESIAN_POINT('Ctrl Pts',(7.91050204921107,-0.0912165795131029,
45.635337629187));
#238096=CARTESIAN_POINT('Ctrl Pts',(7.91023165753433,-0.112241989610785,
45.6344993072133));
#238097=CARTESIAN_POINT('Ctrl Pts',(7.90880248143647,-0.197069300870259,
45.6311230988658));
#238098=CARTESIAN_POINT('Ctrl Pts',(7.90695557248555,-0.26085766336606,
45.6285980157543));
#238099=CARTESIAN_POINT('Ctrl Pts',(7.89003433165123,-0.672884988251195,
45.61237452518));
#238100=CARTESIAN_POINT('Ctrl Pts',(7.85273020113686,-1.019835340228,45.5991405529902));
#238101=CARTESIAN_POINT('Ctrl Pts',(7.71081289093464,-1.83109198658558,
45.5686189010716));
#238102=CARTESIAN_POINT('Ctrl Pts',(7.58699601374979,-2.290634514008,45.5516977672314));
#238103=CARTESIAN_POINT('Ctrl Pts',(7.33027569981168,-2.98703881584404,
45.5242204971208));
#238104=CARTESIAN_POINT('Ctrl Pts',(7.22519672387178,-3.23293335779673,
45.5141157504508));
#238105=CARTESIAN_POINT('Ctrl Pts',(7.10029097383133,-3.48856536984689,
45.5027540650829));
#238106=CARTESIAN_POINT('Ctrl Pts',(7.09264562335316,-3.50408309085231,
45.5020608967));
#238107=CARTESIAN_POINT('Ctrl Pts',(7.08195090117628,-3.52561170015096,
45.5010942266304));
#238108=CARTESIAN_POINT('Ctrl Pts',(7.07894461562811,-3.53164403010793,
45.5008228181208));
#238109=CARTESIAN_POINT('Ctrl Pts',(7.07375425597294,-3.54202560864643,
45.5003547725307));
#238110=CARTESIAN_POINT('Ctrl Pts',(7.07157386776715,-3.54637670288162,
45.500158317618));
#238111=CARTESIAN_POINT('Ctrl Pts',(7.06706629545426,-3.5553511453646,45.4997525130845));
#238112=CARTESIAN_POINT('Ctrl Pts',(7.06473858690384,-3.55997422598885,
45.4995431372866));
#238113=CARTESIAN_POINT('Ctrl Pts',(7.05931079486258,-3.57072811888522,
45.4990553253989));
#238114=CARTESIAN_POINT('Ctrl Pts',(7.0562072622968,-3.5768571775396,45.4987767146655));
#238115=CARTESIAN_POINT('Ctrl Pts',(7.04666549501679,-3.59564013405746,
45.4979210648263));
#238116=CARTESIAN_POINT('Ctrl Pts',(7.04020120188754,-3.60828069932307,
45.4973426836424));
#238117=CARTESIAN_POINT('Ctrl Pts',(6.97010061293252,-3.74445298009451,
45.4910837943756));
#238118=CARTESIAN_POINT('Ctrl Pts',(6.90326121295536,-3.86629122503848,
45.4852216459464));
#238119=CARTESIAN_POINT('Ctrl Pts',(6.75942538110885,-4.11285262353395,
45.4728876073449));
#238120=CARTESIAN_POINT('Ctrl Pts',(6.68209761614589,-4.23732892812539,
45.466404404723));
#238121=CARTESIAN_POINT('Ctrl Pts',(6.42420408684024,-4.62783623698831,
45.4453852478108));
#238122=CARTESIAN_POINT('Ctrl Pts',(6.2308640963602,-4.88503740364512,45.4305074192471));
#238123=CARTESIAN_POINT('Ctrl Pts',(5.72735472129881,-5.47616573367393,
45.3947180364904));
#238124=CARTESIAN_POINT('Ctrl Pts',(5.40293077719033,-5.79649772187217,
45.3739711690651));
#238125=CARTESIAN_POINT('Ctrl Pts',(5.04738372681391,-6.0916243331638,45.3539804182439));
#238126=CARTESIAN_POINT('Ctrl Pts',(5.04201908182731,-6.09606537701818,
45.3536793609821));
#238127=CARTESIAN_POINT('Ctrl Pts',(5.01527016786991,-6.11814961501412,
45.3521810927908));
#238128=CARTESIAN_POINT('Ctrl Pts',(4.99379900570893,-6.13568749836777,
45.3509874950553));
#238129=CARTESIAN_POINT('Ctrl Pts',(4.80591426104648,-6.28751428864805,
45.3406217088511));
#238130=CARTESIAN_POINT('Ctrl Pts',(4.63420465355468,-6.41512307387998,
45.3316878048027));
#238131=CARTESIAN_POINT('Ctrl Pts',(4.44033715162932,-6.54734754518713,
45.3221691602431));
#238132=CARTESIAN_POINT('Ctrl Pts',(4.4231019807628,-6.55900318445198,45.3213276669488));
#238133=CARTESIAN_POINT('Ctrl Pts',(4.39744280911085,-6.57620859568392,
45.3200818483037));
#238134=CARTESIAN_POINT('Ctrl Pts',(4.38905391772956,-6.58181042430696,
45.3196756464177));
#238135=CARTESIAN_POINT('Ctrl Pts',(4.37467526437712,-6.59137230701359,
45.3189812876583));
#238136=CARTESIAN_POINT('Ctrl Pts',(4.3686907922502,-6.59534027329059,45.3186928463632));
#238137=CARTESIAN_POINT('Ctrl Pts',(4.35703847309424,-6.60304345131603,
45.3181323000038));
#238138=CARTESIAN_POINT('Ctrl Pts',(4.35137120504217,-6.60677952653373,
45.317860164055));
#238139=CARTESIAN_POINT('Ctrl Pts',(4.33780644471185,-6.61569689935402,
45.3172099761898));
#238140=CARTESIAN_POINT('Ctrl Pts',(4.32990446010047,-6.62087136131351,
45.3168321693279));
#238141=CARTESIAN_POINT('Ctrl Pts',(4.30619259917828,-6.63633800968059,
45.3157013077879));
#238142=CARTESIAN_POINT('Ctrl Pts',(4.2903551073974,-6.64658784177486,45.3149497665221));
#238143=CARTESIAN_POINT('Ctrl Pts',(4.15228885468236,-6.73524354212397,
45.308430624798));
#238144=CARTESIAN_POINT('Ctrl Pts',(4.0279561475674,-6.81032893379145,45.3027819222614));
#238145=CARTESIAN_POINT('Ctrl Pts',(3.56926012949443,-7.07038000079558,
45.2826753791903));
#238146=CARTESIAN_POINT('Ctrl Pts',(3.22367015589914,-7.2344917770006,45.2689281102694));
#238147=CARTESIAN_POINT('Ctrl Pts',(2.52855275112702,-7.50484174369433,
45.2428137832711));
#238148=CARTESIAN_POINT('Ctrl Pts',(2.18086279749248,-7.61315069583241,
45.2304359977541));
#238149=CARTESIAN_POINT('Ctrl Pts',(1.64673179636296,-7.73992937044682,
45.2112850042528));
#238150=CARTESIAN_POINT('Ctrl Pts',(1.46506356731048,-7.77636274062096,
45.2047445353424));
#238151=CARTESIAN_POINT('Ctrl Pts',(1.03757546833957,-7.84658262609221,
45.1890153557494));
#238152=CARTESIAN_POINT('Ctrl Pts',(0.791113763081927,-7.87525001000017,
45.1796674161245));
#238153=CARTESIAN_POINT('Ctrl Pts',(0.52530832906285,-7.89356143452319,
45.1690424716581));
#238154=CARTESIAN_POINT('Ctrl Pts',(0.506909614258777,-7.89476431546944,
45.1683046517731));
#238155=CARTESIAN_POINT('Ctrl Pts',(0.480957323714662,-7.89636994244776,
45.1672607189268));
#238156=CARTESIAN_POINT('Ctrl Pts',(0.47340703412835,-7.89682619758156,
45.1669566259211));
#238157=CARTESIAN_POINT('Ctrl Pts',(0.460203647342578,-7.89760505878734,
45.1664241950331));
#238158=CARTESIAN_POINT('Ctrl Pts',(0.454550830320328,-7.89793242589721,
45.1661960332597));
#238159=CARTESIAN_POINT('Ctrl Pts',(0.442689811762091,-7.89860654752731,
45.1657168584562));
#238160=CARTESIAN_POINT('Ctrl Pts',(0.436481543543993,-7.89895205226282,
45.1654658000956));
#238161=CARTESIAN_POINT('Ctrl Pts',(0.421685784197907,-7.89975797455184,
45.1648668832787));
#238162=CARTESIAN_POINT('Ctrl Pts',(0.413097945615922,-7.90021170879171,
45.1645187863434));
#238163=CARTESIAN_POINT('Ctrl Pts',(0.385115460175408,-7.90164439805896,
45.1633830537415));
#238164=CARTESIAN_POINT('Ctrl Pts',(0.365718022450598,-7.90256593970965,
45.162593419539));
#238165=CARTESIAN_POINT('Ctrl Pts',(0.0741315556924383,-7.91534288226645,
45.1506899654776));
#238166=CARTESIAN_POINT('Ctrl Pts',(-0.198479376256622,-7.91320053288995,
45.1391311538104));
#238167=CARTESIAN_POINT('Ctrl Pts',(-1.03798266636762,-7.86319146982881,
45.1030281235171));
#238168=CARTESIAN_POINT('Ctrl Pts',(-1.60028562578764,-7.7682901021775,
45.078286348511));
#238169=CARTESIAN_POINT('Ctrl Pts',(-2.34249328756123,-7.55894653183966,
45.0458582466332));
#238170=CARTESIAN_POINT('Ctrl Pts',(-2.53525619925512,-7.49649426413489,
45.0374360336317));
#238171=CARTESIAN_POINT('Ctrl Pts',(-2.99457737418755,-7.32793515054033,
45.0172681513016));
#238172=CARTESIAN_POINT('Ctrl Pts',(-3.25817943566352,-7.21459622248732,
45.0055809705141));
#238173=CARTESIAN_POINT('Ctrl Pts',(-3.57153799931158,-7.05917939104955,
44.9914120968652));
#238174=CARTESIAN_POINT('Ctrl Pts',(-3.62769303037083,-7.03048651889441,
44.9888633056237));
#238175=CARTESIAN_POINT('Ctrl Pts',(-3.71063203770076,-6.9868498522256,
44.9850843294984));
#238176=CARTESIAN_POINT('Ctrl Pts',(-3.73768169953415,-6.97241683328406,
44.9838495330199));
#238177=CARTESIAN_POINT('Ctrl Pts',(-3.78591329980418,-6.94632033169141,
44.9816435883287));
#238178=CARTESIAN_POINT('Ctrl Pts',(-3.80712693898525,-6.93471629832611,
44.9806718822521));
#238179=CARTESIAN_POINT('Ctrl Pts',(-3.84798326401398,-6.9121235786435,
44.9787975552144));
#238180=CARTESIAN_POINT('Ctrl Pts',(-3.86763291042413,-6.90114796536284,
44.9778948141908));
#238181=CARTESIAN_POINT('Ctrl Pts',(-3.91027816743006,-6.87708845539374,
44.9759327566614));
#238182=CARTESIAN_POINT('Ctrl Pts',(-3.93325553581372,-6.86397274652391,
44.9748737772607));
#238183=CARTESIAN_POINT('Ctrl Pts',(-4.02507293746807,-6.8109500303309,
44.9706346606344));
#238184=CARTESIAN_POINT('Ctrl Pts',(-4.09337524098538,-6.77012051171215,
44.9674644089371));
#238185=CARTESIAN_POINT('Ctrl Pts',(-4.25557705942827,-6.66980792048567,
44.9598920416068));
#238186=CARTESIAN_POINT('Ctrl Pts',(-4.34886198285789,-6.60936257318151,
44.955501181235));
#238187=CARTESIAN_POINT('Ctrl Pts',(-4.70177928760292,-6.36997702317278,
44.9387291285415));
#238188=CARTESIAN_POINT('Ctrl Pts',(-4.95190290536343,-6.17753979015283,
44.9265110289741));
#238189=CARTESIAN_POINT('Ctrl Pts',(-5.45822152667925,-5.737434517197,44.9005739907985));
#238190=CARTESIAN_POINT('Ctrl Pts',(-5.71053168985345,-5.48636083463045,
44.8868933460029));
#238191=CARTESIAN_POINT('Ctrl Pts',(-6.00765592213653,-5.14791067155404,
44.8691207780525));
#238192=CARTESIAN_POINT('Ctrl Pts',(-6.06893232733867,-5.07552696022641,
44.8653541274941));
#238193=CARTESIAN_POINT('Ctrl Pts',(-6.14135536629102,-4.98678892817076,
44.860763292693));
#238194=CARTESIAN_POINT('Ctrl Pts',(-6.15376172311053,-4.97147123089405,
44.8599717804732));
#238195=CARTESIAN_POINT('Ctrl Pts',(-6.17404747217003,-4.94623284032787,
44.8586690057422));
#238196=CARTESIAN_POINT('Ctrl Pts',(-6.18196053394706,-4.93633927670484,
44.8581586555875));
#238197=CARTESIAN_POINT('Ctrl Pts',(-6.19578493978849,-4.91896948730705,
44.8572632017542));
#238198=CARTESIAN_POINT('Ctrl Pts',(-6.20170660918157,-4.91150149854571,
44.8568783866464));
#238199=CARTESIAN_POINT('Ctrl Pts',(-6.21344267413409,-4.8966457418733,
44.8561132176306));
#238200=CARTESIAN_POINT('Ctrl Pts',(-6.21925742486876,-4.88925827388927,
44.855732874729));
#238201=CARTESIAN_POINT('Ctrl Pts',(-6.23521012111914,-4.8689163416059,
44.8546859801475));
#238202=CARTESIAN_POINT('Ctrl Pts',(-6.24532078671114,-4.85594067769134,
44.8540186328727));
#238203=CARTESIAN_POINT('Ctrl Pts',(-6.28905064317848,-4.79945686536525,
44.8511154240065));
#238204=CARTESIAN_POINT('Ctrl Pts',(-6.32225586930292,-4.75563085296177,
44.8488676069389));
#238205=CARTESIAN_POINT('Ctrl Pts',(-6.41195798424915,-4.63463720616461,
44.8426797870547));
#238206=CARTESIAN_POINT('Ctrl Pts',(-6.46751630855158,-4.55678610336702,
44.8387180184373));
#238207=CARTESIAN_POINT('Ctrl Pts',(-6.65537496491862,-4.28319020282288,
44.8248919499331));
#238208=CARTESIAN_POINT('Ctrl Pts',(-6.78030859801647,-4.08254179281821,
44.8149238945223));
#238209=CARTESIAN_POINT('Ctrl Pts',(-7.13372370115756,-3.45385352866851,
44.784498602175));
#238210=CARTESIAN_POINT('Ctrl Pts',(-7.33200476137419,-3.01012614697774,
44.7641711620468));
#238211=CARTESIAN_POINT('Ctrl Pts',(-7.51194210097086,-2.48192977669456,
44.741441148462));
#238212=CARTESIAN_POINT('Ctrl Pts',(-7.53452375414921,-2.41250937540598,
44.7384799554686));
#238213=CARTESIAN_POINT('Ctrl Pts',(-7.56414407293966,-2.31697554156631,
44.7344389399165));
#238214=CARTESIAN_POINT('Ctrl Pts',(-7.57201431891645,-2.29112426063764,
44.7333488364948));
#238215=CARTESIAN_POINT('Ctrl Pts',(-7.5852391505688,-2.24687232741814,
44.7314884585909));
#238216=CARTESIAN_POINT('Ctrl Pts',(-7.59065960290408,-2.22849164736873,
44.7307173831222));
#238217=CARTESIAN_POINT('Ctrl Pts',(-7.60163615089809,-2.19076560450639,
44.7291380998129));
#238218=CARTESIAN_POINT('Ctrl Pts',(-7.60718531341491,-2.1714183647465,
44.7283299810722));
#238219=CARTESIAN_POINT('Ctrl Pts',(-7.61802338877394,-2.13307976462393,
44.7267320793164));
#238220=CARTESIAN_POINT('Ctrl Pts',(-7.62331526778823,-2.11408939373407,
44.7259422663055));
#238221=CARTESIAN_POINT('Ctrl Pts',(-7.63535777158823,-2.07024061416471,
44.7241223718093));
#238222=CARTESIAN_POINT('Ctrl Pts',(-7.64205808700295,-2.0453685979053,
44.7230928849345));
#238223=CARTESIAN_POINT('Ctrl Pts',(-7.659095115593,-1.98087349764613,44.7204303460047));
#238224=CARTESIAN_POINT('Ctrl Pts',(-7.66924589194999,-1.94120201785514,
44.7187994219176));
#238225=CARTESIAN_POINT('Ctrl Pts',(-7.83325781983586,-1.27883391880955,
44.6916758007861));
#238226=CARTESIAN_POINT('Ctrl Pts',(-7.91113768679704,-0.639744219957868,
44.6668472522222));
#238227=CARTESIAN_POINT('Ctrl Pts',(-7.91099981726586,0.00170035864730828,
44.6425804671265));
#238228=CARTESIAN_POINT('',(-7.91313519165583,0.000112501479813467,42.642361085604));
#238229=CARTESIAN_POINT('Ctrl Pts',(-7.91143166941437,0.00169103298945927,
44.6423315082371));
#238230=CARTESIAN_POINT('Ctrl Pts',(-7.91482057188058,0.894287429589468,
44.6064986371717));
#238231=CARTESIAN_POINT('Ctrl Pts',(-7.3389531910569,4.4250799800469,44.4646961888898));
#238232=CARTESIAN_POINT('Ctrl Pts',(-2.18951637767745,9.09795524730432,
44.2169241633916));
#238233=CARTESIAN_POINT('Ctrl Pts',(6.49039433236539,6.75072682562183,43.8990154317418));
#238234=CARTESIAN_POINT('Ctrl Pts',(8.71254627783232,-0.362491690837899,
43.6340914887007));
#238235=CARTESIAN_POINT('Ctrl Pts',(6.339535221574,-5.24393813728578,43.4221523342676));
#238236=CARTESIAN_POINT('Ctrl Pts',(1.9657803162333,-8.50293123149737,43.2102131798347));
#238237=CARTESIAN_POINT('Ctrl Pts',(-3.92045911912344,-7.79462844045021,
42.9982740254015));
#238238=CARTESIAN_POINT('Ctrl Pts',(-7.3291187982702,-3.69026847598658,
42.7913283977889));
#238239=CARTESIAN_POINT('Ctrl Pts',(-7.91165264643059,-1.18860184589039,
42.6903523473923));
#238240=CARTESIAN_POINT('Ctrl Pts',(-7.91313519165583,0.000112501479813467,
42.642361085604));
#238241=CARTESIAN_POINT('',(-7.91099999357494,-0.00031633835898803,38.6421995802722));
#238242=CARTESIAN_POINT('Ctrl Pts',(-7.91099999835655,0.000161253323083898,
42.6435915724384));
#238243=CARTESIAN_POINT('Ctrl Pts',(-7.91099870059755,0.0638286015180441,
42.6410668225085));
#238244=CARTESIAN_POINT('Ctrl Pts',(-7.91022881507591,0.127493277805992,
42.638529614139));
#238245=CARTESIAN_POINT('Ctrl Pts',(-7.90832539151437,0.206249592499511,
42.6353710381167));
#238246=CARTESIAN_POINT('Ctrl Pts',(-7.9079169564133,0.22135672748423,42.6347642479927));
#238247=CARTESIAN_POINT('Ctrl Pts',(-7.90714330592795,0.247228113755906,
42.6337234649721));
#238248=CARTESIAN_POINT('Ctrl Pts',(-7.90679939190703,0.257992976732809,
42.6332899181849));
#238249=CARTESIAN_POINT('Ctrl Pts',(-7.90611046252487,0.278260253947631,
42.6324727207975));
#238250=CARTESIAN_POINT('Ctrl Pts',(-7.90577029609844,0.287762817832992,
42.63208917522));
#238251=CARTESIAN_POINT('Ctrl Pts',(-7.9050362112272,0.307284959190939,
42.6313003848133));
#238252=CARTESIAN_POINT('Ctrl Pts',(-7.90464037354412,0.31730444560978,
42.6308950983097));
#238253=CARTESIAN_POINT('Ctrl Pts',(-7.9036728105286,0.340669235416282,
42.6299489135466));
#238254=CARTESIAN_POINT('Ctrl Pts',(-7.90308633337,0.354013883144208,42.6294076821203));
#238255=CARTESIAN_POINT('Ctrl Pts',(-7.90109918721431,0.396760740314834,
42.6276712079707));
#238256=CARTESIAN_POINT('Ctrl Pts',(-7.89956822106437,0.426156485313474,
42.6264728942297));
#238257=CARTESIAN_POINT('Ctrl Pts',(-7.89396496713785,0.523301666765553,
42.6224998320577));
#238258=CARTESIAN_POINT('Ctrl Pts',(-7.88918489844305,0.591006759762721,
42.6197100027726));
#238259=CARTESIAN_POINT('Ctrl Pts',(-7.84058482017965,1.17272008376745,
42.595588814592));
#238260=CARTESIAN_POINT('Ctrl Pts',(-7.74745509593689,1.68136534198015,
42.5735676573225));
#238261=CARTESIAN_POINT('Ctrl Pts',(-7.5220386691645,2.46875506434117,42.5393271557479));
#238262=CARTESIAN_POINT('Ctrl Pts',(-7.4219210303001,2.75516156289006,42.5268184404839));
#238263=CARTESIAN_POINT('Ctrl Pts',(-7.29236199789618,3.0670132149062,42.5131199356718));
#238264=CARTESIAN_POINT('Ctrl Pts',(-7.2789041760689,3.09881712585957,42.5117218180166));
#238265=CARTESIAN_POINT('Ctrl Pts',(-7.25607392047374,3.15180085256804,
42.5093905672729));
#238266=CARTESIAN_POINT('Ctrl Pts',(-7.24681597348907,3.17302940492572,
42.508455968599));
#238267=CARTESIAN_POINT('Ctrl Pts',(-7.22840792166405,3.21473841455266,
42.5066185157093));
#238268=CARTESIAN_POINT('Ctrl Pts',(-7.21926366441351,3.23522121402781,
42.5057155958044));
#238269=CARTESIAN_POINT('Ctrl Pts',(-7.20180576779138,3.273883669975,42.5040101146665));
#238270=CARTESIAN_POINT('Ctrl Pts',(-7.19351010009055,3.29207123923967,
42.5032073317));
#238271=CARTESIAN_POINT('Ctrl Pts',(-7.17456817545133,3.33318638862942,
42.5013913476605));
#238272=CARTESIAN_POINT('Ctrl Pts',(-7.16388077381466,3.35609479450021,
42.500378676122));
#238273=CARTESIAN_POINT('Ctrl Pts',(-7.13600576372836,3.41510489672469,
42.4977677206586));
#238274=CARTESIAN_POINT('Ctrl Pts',(-7.11865389642515,3.45112828501532,
42.4961715043756));
#238275=CARTESIAN_POINT('Ctrl Pts',(-6.98457416611006,3.72417073743901,
42.4840523910024));
#238276=CARTESIAN_POINT('Ctrl Pts',(-6.8563104951417,3.95534242720663,42.4736776131043));
#238277=CARTESIAN_POINT('Ctrl Pts',(-6.69361097697219,4.21680046069988,
42.4616474514794));
#238278=CARTESIAN_POINT('Ctrl Pts',(-6.67019486193765,4.25374359303614,
42.4599408199053));
#238279=CARTESIAN_POINT('Ctrl Pts',(-6.40972029917303,4.65724925413542,
42.4412270910775));
#238280=CARTESIAN_POINT('Ctrl Pts',(-6.14301203832827,5.00378929000388,
42.4245490659468));
#238281=CARTESIAN_POINT('Ctrl Pts',(-5.61542258507756,5.58313268729837,
42.3950732033718));
#238282=CARTESIAN_POINT('Ctrl Pts',(-5.3651465527745,5.82404849341945,42.3821969794744));
#238283=CARTESIAN_POINT('Ctrl Pts',(-4.92895650299121,6.19187285391271,
42.3607111520235));
#238284=CARTESIAN_POINT('Ctrl Pts',(-4.75201995878336,6.32868093484177,
42.3522170410829));
#238285=CARTESIAN_POINT('Ctrl Pts',(-4.5184609321609,6.49394689255161,42.3410525639834));
#238286=CARTESIAN_POINT('Ctrl Pts',(-4.4669619645894,6.52947823729085,42.3385934462071));
#238287=CARTESIAN_POINT('Ctrl Pts',(-4.38323240422503,6.58579264624337,
42.3345924147162));
#238288=CARTESIAN_POINT('Ctrl Pts',(-4.3512623082631,6.60695901010832,42.3330640497093));
#238289=CARTESIAN_POINT('Ctrl Pts',(-4.3117857028548,6.63268438148475,42.3311747304916));
#238290=CARTESIAN_POINT('Ctrl Pts',(-4.30442355069523,6.63746457220562,
42.3308222945574));
#238291=CARTESIAN_POINT('Ctrl Pts',(-4.29016086689439,6.646691517374,42.3301393242249));
#238292=CARTESIAN_POINT('Ctrl Pts',(-4.28326133731275,6.65113980507829,
42.3298088505483));
#238293=CARTESIAN_POINT('Ctrl Pts',(-4.2712542389336,6.65885463003269,42.3292335620636));
#238294=CARTESIAN_POINT('Ctrl Pts',(-4.26614980919285,6.66212605425707,
42.3289889427032));
#238295=CARTESIAN_POINT('Ctrl Pts',(-4.25550461176271,6.66893130024049,
42.3284786720217));
#238296=CARTESIAN_POINT('Ctrl Pts',(-4.24996319315084,6.67246409091946,
42.328212979319));
#238297=CARTESIAN_POINT('Ctrl Pts',(-4.23640167640157,6.68108614364804,
42.3275625691861));
#238298=CARTESIAN_POINT('Ctrl Pts',(-4.22837681288277,6.68616786732243,
42.327177543004));
#238299=CARTESIAN_POINT('Ctrl Pts',(-4.19765897270355,6.70554243936984,
42.3257030768762));
#238300=CARTESIAN_POINT('Ctrl Pts',(-4.17490267052612,6.71973421550902,
42.3246094136083));
#238301=CARTESIAN_POINT('Ctrl Pts',(-3.83400822828007,6.92993011537489,
42.3082004016254));
#238302=CARTESIAN_POINT('Ctrl Pts',(-3.50251849300235,7.10322450315396,
42.2916822566228));
#238303=CARTESIAN_POINT('Ctrl Pts',(-2.88859882580964,7.37072755434766,
42.2612754480296));
#238304=CARTESIAN_POINT('Ctrl Pts',(-2.61067170306401,7.47368859428964,
42.2476094290269));
#238305=CARTESIAN_POINT('Ctrl Pts',(-2.25540895700324,7.58305750969555,
42.2306489468922));
#238306=CARTESIAN_POINT('Ctrl Pts',(-2.18287539235076,7.60425446415045,
42.2272114130834));
#238307=CARTESIAN_POINT('Ctrl Pts',(-1.96843893145003,7.66359957183411,
42.2171339901846));
#238308=CARTESIAN_POINT('Ctrl Pts',(-1.82576177469744,7.69883797427789,
42.2105384219362));
#238309=CARTESIAN_POINT('Ctrl Pts',(-1.43063361459529,7.78482382225821,
42.1926305645198));
#238310=CARTESIAN_POINT('Ctrl Pts',(-1.17655050986805,7.82725612401495,
42.1815166821291));
#238311=CARTESIAN_POINT('Ctrl Pts',(-0.80939899044334,7.87028479958545,
42.166096023552));
#238312=CARTESIAN_POINT('Ctrl Pts',(-0.697695034915772,7.88097281613747,
42.1614872222848));
#238313=CARTESIAN_POINT('Ctrl Pts',(-0.568604925504825,7.8905580717715,
42.1562549250558));
#238314=CARTESIAN_POINT('Ctrl Pts',(-0.551407257854619,7.89177852490375,
42.1555597779375));
#238315=CARTESIAN_POINT('Ctrl Pts',(-0.525325112893288,7.89354380182114,
42.1545083907135));
#238316=CARTESIAN_POINT('Ctrl Pts',(-0.516443532063122,7.89412986366183,
42.1541508747595));
#238317=CARTESIAN_POINT('Ctrl Pts',(-0.501068162266608,7.89511836690642,
42.1535328328762));
#238318=CARTESIAN_POINT('Ctrl Pts',(-0.494574840011914,7.89552778847505,
42.1532720909362));
#238319=CARTESIAN_POINT('Ctrl Pts',(-0.481108193446497,7.89636021924944,
42.1527318893854));
#238320=CARTESIAN_POINT('Ctrl Pts',(-0.474134797297655,7.89678200283286,
42.1524524679748));
#238321=CARTESIAN_POINT('Ctrl Pts',(-0.45513379795647,7.89790601247448,
42.1516919459518));
#238322=CARTESIAN_POINT('Ctrl Pts',(-0.443105112664125,7.89859000180985,
42.1512114113679));
#238323=CARTESIAN_POINT('Ctrl Pts',(-0.397690237275794,7.90106836627447,
42.1494005753619));
#238324=CARTESIAN_POINT('Ctrl Pts',(-0.364294133291213,7.90267857579063,
42.1480759952152));
#238325=CARTESIAN_POINT('Ctrl Pts',(0.154392163748717,7.9243923523408,42.1276105879979));
#238326=CARTESIAN_POINT('Ctrl Pts',(0.640527675438196,7.89997628448017,
42.1099744137218));
#238327=CARTESIAN_POINT('Ctrl Pts',(1.37927812403532,7.79418870521098,42.0840395769463));
#238328=CARTESIAN_POINT('Ctrl Pts',(1.63517736337208,7.74454538581923,42.0752005077116));
#238329=CARTESIAN_POINT('Ctrl Pts',(2.27953144422728,7.58617691457483,42.052626486232));
#238330=CARTESIAN_POINT('Ctrl Pts',(2.66295556603332,7.46022598293077,42.038901452621));
#238331=CARTESIAN_POINT('Ctrl Pts',(3.14754722139484,7.25890471335881,42.019492909002));
#238332=CARTESIAN_POINT('Ctrl Pts',(3.25890930042056,7.20959492743243,42.0148818912178));
#238333=CARTESIAN_POINT('Ctrl Pts',(3.42049917552824,7.13353597706497,42.0079107646925));
#238334=CARTESIAN_POINT('Ctrl Pts',(3.47165056578738,7.10878275110357,42.0056619575579));
#238335=CARTESIAN_POINT('Ctrl Pts',(3.53076560766431,7.07938555444326,42.0030092680924));
#238336=CARTESIAN_POINT('Ctrl Pts',(3.53899435623791,7.07527558119831,42.0026387975371));
#238337=CARTESIAN_POINT('Ctrl Pts',(3.55150024029925,7.06900205248514,42.0020738823564));
#238338=CARTESIAN_POINT('Ctrl Pts',(3.55578263179744,7.06684893358418,42.0018801021677));
#238339=CARTESIAN_POINT('Ctrl Pts',(3.56354105169646,7.06293928482301,42.0015284161103));
#238340=CARTESIAN_POINT('Ctrl Pts',(3.56701774782794,7.06118407597467,42.0013705951262));
#238341=CARTESIAN_POINT('Ctrl Pts',(3.57447816624742,7.05741077037642,42.0010314540196));
#238342=CARTESIAN_POINT('Ctrl Pts',(3.57846147677908,7.05539186734896,42.0008500817292));
#238343=CARTESIAN_POINT('Ctrl Pts',(3.58912611960712,7.04997523984261,42.0003636894633));
#238344=CARTESIAN_POINT('Ctrl Pts',(3.59580432120636,7.04657139803977,42.0000582702541));
#238345=CARTESIAN_POINT('Ctrl Pts',(3.62705729328857,7.03058593637707,41.9986249740378));
#238346=CARTESIAN_POINT('Ctrl Pts',(3.65157054174572,7.01788541840043,41.9974892015698));
#238347=CARTESIAN_POINT('Ctrl Pts',(4.06845019056466,6.79912111484412,41.9779835261067));
#238348=CARTESIAN_POINT('Ctrl Pts',(4.44285243392775,6.56058896109704,41.9576218471729));
#238349=CARTESIAN_POINT('Ctrl Pts',(5.10703314298491,6.054401489337,41.9188452271468));
#238350=CARTESIAN_POINT('Ctrl Pts',(5.40071668941503,5.79394975465895,41.900530795568));
#238351=CARTESIAN_POINT('Ctrl Pts',(5.79814124642927,5.38491140359518,41.8748787660774));
#238352=CARTESIAN_POINT('Ctrl Pts',(5.91803707394898,5.25286161115937,41.8670006677436));
#238353=CARTESIAN_POINT('Ctrl Pts',(6.13349685031662,4.99880982487135,41.8526218867711));
#238354=CARTESIAN_POINT('Ctrl Pts',(6.23013733241971,4.87783516662728,41.8460793770987));
#238355=CARTESIAN_POINT('Ctrl Pts',(6.37079399765316,4.69075528225316,41.8364156828291));
#238356=CARTESIAN_POINT('Ctrl Pts',(6.41746445510188,4.62669987817769,41.833183577806));
#238357=CARTESIAN_POINT('Ctrl Pts',(6.47167544041893,4.54989623715831,41.8293971409052));
#238358=CARTESIAN_POINT('Ctrl Pts',(6.48015160032975,4.53781599616775,41.8288041511419));
#238359=CARTESIAN_POINT('Ctrl Pts',(6.49313774562894,4.51919752849987,41.8278941452395));
#238360=CARTESIAN_POINT('Ctrl Pts',(6.49767174606763,4.51267614239911,41.8275761411321));
#238361=CARTESIAN_POINT('Ctrl Pts',(6.50591270157564,4.50078476461483,41.826997619719));
#238362=CARTESIAN_POINT('Ctrl Pts',(6.50962284567701,4.49541699792591,41.82673697158));
#238363=CARTESIAN_POINT('Ctrl Pts',(6.51711626045318,4.48454693763668,41.8262101445558));
#238364=CARTESIAN_POINT('Ctrl Pts',(6.5208992145039,4.47904443187499,41.8259439787367));
#238365=CARTESIAN_POINT('Ctrl Pts',(6.53167685664295,4.46332518951311,41.8251850857048));
#238366=CARTESIAN_POINT('Ctrl Pts',(6.53865454718371,4.45309679004026,41.8246930537045));
#238367=CARTESIAN_POINT('Ctrl Pts',(6.56840559753406,4.40926487332594,41.8225920910825));
#238368=CARTESIAN_POINT('Ctrl Pts',(6.59094434609169,4.37550242949679,41.8209927214414));
#238369=CARTESIAN_POINT('Ctrl Pts',(6.93501445721856,3.85140321657824,41.7964521185822));
#238370=CARTESIAN_POINT('Ctrl Pts',(7.20133226115239,3.32695555952119,41.7759547822028));
#238371=CARTESIAN_POINT('Ctrl Pts',(7.53263720896423,2.44352334974857,41.7439858797529));
#238372=CARTESIAN_POINT('Ctrl Pts',(7.63523838939109,2.10108298526976,41.7321033063432));
#238373=CARTESIAN_POINT('Ctrl Pts',(7.78446248100036,1.44435950833828,41.7085545272018));
#238374=CARTESIAN_POINT('Ctrl Pts',(7.83599010499158,1.13192336618629,41.6970303396375));
#238375=CARTESIAN_POINT('Ctrl Pts',(7.86987714827276,0.805661861619268,
41.6838908718752));
#238376=CARTESIAN_POINT('Ctrl Pts',(7.87105781337322,0.79404424294889,41.6834215486685));
#238377=CARTESIAN_POINT('Ctrl Pts',(7.87271497859607,0.777370987452586,
41.682745855618));
#238378=CARTESIAN_POINT('Ctrl Pts',(7.87321234218713,0.772317422427499,
41.6825407751514));
#238379=CARTESIAN_POINT('Ctrl Pts',(7.87407027409981,0.763513271140609,
41.6821829985929));
#238380=CARTESIAN_POINT('Ctrl Pts',(7.87443302605777,0.759762933224345,
41.6820304400052));
#238381=CARTESIAN_POINT('Ctrl Pts',(7.87512830221276,0.752520781811202,
41.6817355416628));
#238382=CARTESIAN_POINT('Ctrl Pts',(7.87546118373133,0.749029002665477,
41.6815932238576));
#238383=CARTESIAN_POINT('Ctrl Pts',(7.87624427014324,0.740756542111757,
41.6812557407947));
#238384=CARTESIAN_POINT('Ctrl Pts',(7.87669244436285,0.735975675108506,
41.6810604519576));
#238385=CARTESIAN_POINT('Ctrl Pts',(7.87801595034233,0.721717583487722,
41.6804773021051));
#238386=CARTESIAN_POINT('Ctrl Pts',(7.8788785295607,0.712239214731559,41.6800886721552));
#238387=CARTESIAN_POINT('Ctrl Pts',(7.88665478920199,0.625047519095722,
41.6765048998713));
#238388=CARTESIAN_POINT('Ctrl Pts',(7.89243534955537,0.547239983336362,
41.6732428725542));
#238389=CARTESIAN_POINT('Ctrl Pts',(7.92032139550481,0.078054762570438,
41.653241515011));
#238390=CARTESIAN_POINT('Ctrl Pts',(7.91446008089835,-0.31440974453127,
41.6351453450269));
#238391=CARTESIAN_POINT('Ctrl Pts',(7.83315626379213,-1.22339376134746,
41.5924020090547));
#238392=CARTESIAN_POINT('Ctrl Pts',(7.73567680809133,-1.73620792553614,
41.5677256530961));
#238393=CARTESIAN_POINT('Ctrl Pts',(7.48743080959072,-2.57879933669016,
41.5284489605261));
#238394=CARTESIAN_POINT('Ctrl Pts',(7.36320480954451,-2.91463331157522,
41.5131310383426));
#238395=CARTESIAN_POINT('Ctrl Pts',(7.2053924350939,-3.26603699853198,41.4974969445848));
#238396=CARTESIAN_POINT('Ctrl Pts',(7.19399121978,-3.29107401465484,41.4963850956787));
#238397=CARTESIAN_POINT('Ctrl Pts',(7.17806155451168,-3.32557715373047,
41.4948556201981));
#238398=CARTESIAN_POINT('Ctrl Pts',(7.1736445943426,-3.33509434963568,41.49443402614));
#238399=CARTESIAN_POINT('Ctrl Pts',(7.16616169906272,-3.3511340535668,41.4937239787043));
#238400=CARTESIAN_POINT('Ctrl Pts',(7.1631057670378,-3.35766119682825,41.4934351692039));
#238401=CARTESIAN_POINT('Ctrl Pts',(7.15704573331951,-3.37055885260953,
41.4928647443787));
#238402=CARTESIAN_POINT('Ctrl Pts',(7.15404203568944,-3.37692954614723,
41.4925831150505));
#238403=CARTESIAN_POINT('Ctrl Pts',(7.14740906999548,-3.39094916852007,
41.4919636269054));
#238404=CARTESIAN_POINT('Ctrl Pts',(7.14377602061087,-3.39859630513791,
41.4916259033775));
#238405=CARTESIAN_POINT('Ctrl Pts',(7.13107999928208,-3.42520961341242,
41.4904511948363));
#238406=CARTESIAN_POINT('Ctrl Pts',(7.1219536790369,-3.44414556234178,41.4896164724179));
#238407=CARTESIAN_POINT('Ctrl Pts',(7.03091379201953,-3.63113248627902,
41.481384381308));
#238408=CARTESIAN_POINT('Ctrl Pts',(6.94314036340964,-3.79627178594612,
41.4742006783067));
#238409=CARTESIAN_POINT('Ctrl Pts',(6.78769803070729,-4.06526511745037,
41.4625704802281));
#238410=CARTESIAN_POINT('Ctrl Pts',(6.72329665144036,-4.1709121911696,41.4580213458165));
#238411=CARTESIAN_POINT('Ctrl Pts',(6.6478364102031,-4.28840829465699,41.4529618441489));
#238412=CARTESIAN_POINT('Ctrl Pts',(6.63918970967433,-4.30178272812262,
41.4523859189581));
#238413=CARTESIAN_POINT('Ctrl Pts',(6.49978840723532,-4.5159826465098,41.4431612410853));
#238414=CARTESIAN_POINT('Ctrl Pts',(6.36001271808578,-4.71079526743562,
41.4347640706728));
#238415=CARTESIAN_POINT('Ctrl Pts',(5.94762925884295,-5.23367366748182,
41.4116790647961));
#238416=CARTESIAN_POINT('Ctrl Pts',(5.65704299298588,-5.54648263022499,
41.3972455682058));
#238417=CARTESIAN_POINT('Ctrl Pts',(5.21342635695285,-5.95271591715908,
41.3755003212993));
#238418=CARTESIAN_POINT('Ctrl Pts',(5.08027153275409,-6.06675173383288,
41.3690001665635));
#238419=CARTESIAN_POINT('Ctrl Pts',(4.89991148103098,-6.21111084628582,
41.3600751269425));
#238420=CARTESIAN_POINT('Ctrl Pts',(4.85601160993663,-6.24549287430204,
41.3578928487773));
#238421=CARTESIAN_POINT('Ctrl Pts',(4.79307237772491,-6.29372163776929,
41.3547526931519));
#238422=CARTESIAN_POINT('Ctrl Pts',(4.77432808708408,-6.30795261333543,
41.3538161298554));
#238423=CARTESIAN_POINT('Ctrl Pts',(4.74130836388819,-6.33279024433729,
41.3521642232574));
#238424=CARTESIAN_POINT('Ctrl Pts',(4.72706007890023,-6.34343284695367,
41.3514507415207));
#238425=CARTESIAN_POINT('Ctrl Pts',(4.70639121606066,-6.35876292330278,
41.3504149017802));
#238426=CARTESIAN_POINT('Ctrl Pts',(4.69999920577254,-6.36348895328019,
41.3500944432749));
#238427=CARTESIAN_POINT('Ctrl Pts',(4.68880052635003,-6.37174278934834,
41.3495328147075));
#238428=CARTESIAN_POINT('Ctrl Pts',(4.68399696528157,-6.37527481592008,
41.3492918483111));
#238429=CARTESIAN_POINT('Ctrl Pts',(4.67475425839886,-6.38205483203358,
41.3488280839328));
#238430=CARTESIAN_POINT('Ctrl Pts',(4.67031570795626,-6.38530362969092,
41.3486053245037));
#238431=CARTESIAN_POINT('Ctrl Pts',(4.65985349837133,-6.39294470102254,
41.3480801420297));
#238432=CARTESIAN_POINT('Ctrl Pts',(4.65382701820704,-6.39733308971132,
41.347777537933));
#238433=CARTESIAN_POINT('Ctrl Pts',(4.6360065892842,-6.4102711407821,41.346882493395));
#238434=CARTESIAN_POINT('Ctrl Pts',(4.62419525341872,-6.41879672906169,
41.3462889530326));
#238435=CARTESIAN_POINT('Ctrl Pts',(4.51903066034954,-6.49426509022223,
41.3410019171923));
#238436=CARTESIAN_POINT('Ctrl Pts',(4.42425554580203,-6.55919801382446,
41.3362210729431));
#238437=CARTESIAN_POINT('Ctrl Pts',(3.92744505071731,-6.8839085622763,41.3111847583723));
#238438=CARTESIAN_POINT('Ctrl Pts',(3.50385539283111,-7.10886818793583,
41.2899831386461));
#238439=CARTESIAN_POINT('Ctrl Pts',(2.75467613367001,-7.42342047050458,
41.2545014273808));
#238440=CARTESIAN_POINT('Ctrl Pts',(2.43892351605282,-7.53306581064085,
41.2400869403296));
#238441=CARTESIAN_POINT('Ctrl Pts',(1.89677820470627,-7.68364994717669,
41.2163940378961));
#238442=CARTESIAN_POINT('Ctrl Pts',(1.67382248801716,-7.73528078587551,
41.2069344648335));
#238443=CARTESIAN_POINT('Ctrl Pts',(1.39850149706047,-7.78657475691858,
41.1955620038474));
#238444=CARTESIAN_POINT('Ctrl Pts',(1.34797686153379,-7.79548018567544,
41.1934873433383));
#238445=CARTESIAN_POINT('Ctrl Pts',(1.27808558524441,-7.80709935651474,
41.1906338361787));
#238446=CARTESIAN_POINT('Ctrl Pts',(1.25879034363712,-7.81023367130875,
41.1898477917781));
#238447=CARTESIAN_POINT('Ctrl Pts',(1.22632560953256,-7.81538380311779,
41.1885281828534));
#238448=CARTESIAN_POINT('Ctrl Pts',(1.2131623115111,-7.81743792414354,41.1879939372384));
#238449=CARTESIAN_POINT('Ctrl Pts',(1.18718525132024,-7.82142442930598,
41.1869412295709));
#238450=CARTESIAN_POINT('Ctrl Pts',(1.17437180631286,-7.82335860011679,
41.1864227367381));
#238451=CARTESIAN_POINT('Ctrl Pts',(1.14620406064931,-7.82753971898799,
41.1852846187976));
#238452=CARTESIAN_POINT('Ctrl Pts',(1.13084777436115,-7.82977299251159,
41.1846652457046));
#238453=CARTESIAN_POINT('Ctrl Pts',(1.07744740976148,-7.83737866167482,
41.1825152327377));
#238454=CARTESIAN_POINT('Ctrl Pts',(1.03937067696906,-7.84251910005954,
41.1809889051577));
#238455=CARTESIAN_POINT('Ctrl Pts',(0.506717972341742,-7.91048096006713,
41.159730455763));
#238456=CARTESIAN_POINT('Ctrl Pts',(0.00731260741647796,-7.92669320504271,
41.1410341984355));
#238457=CARTESIAN_POINT('Ctrl Pts',(-0.90201145808582,-7.87022465470477,
41.1076974136502));
#238458=CARTESIAN_POINT('Ctrl Pts',(-1.31105361893869,-7.81250146625802,
41.0929345420716));
#238459=CARTESIAN_POINT('Ctrl Pts',(-1.86351271515144,-7.68991452212968,
41.0717721792114));
#238460=CARTESIAN_POINT('Ctrl Pts',(-2.01230659331713,-7.65232540870932,
41.0659418603715));
#238461=CARTESIAN_POINT('Ctrl Pts',(-2.22716561755725,-7.59134653841591,
41.0572228361006));
#238462=CARTESIAN_POINT('Ctrl Pts',(-2.29416592661701,-7.57136785887135,
41.0544607076508));
#238463=CARTESIAN_POINT('Ctrl Pts',(-2.37218678289564,-7.54697230230424,
41.0511847181549));
#238464=CARTESIAN_POINT('Ctrl Pts',(-2.3834743888746,-7.54341506879274,
41.0507093013355));
#238465=CARTESIAN_POINT('Ctrl Pts',(-2.40069722003787,-7.53794486207966,
41.0499816058009));
#238466=CARTESIAN_POINT('Ctrl Pts',(-2.40663826782427,-7.53605016793063,
41.0497301680818));
#238467=CARTESIAN_POINT('Ctrl Pts',(-2.41743698034745,-7.532592215618,41.0492723738522));
#238468=CARTESIAN_POINT('Ctrl Pts',(-2.42229538866276,-7.53103127669919,
41.049066125727));
#238469=CARTESIAN_POINT('Ctrl Pts',(-2.43276060248113,-7.52765777468234,
41.0486212408881));
#238470=CARTESIAN_POINT('Ctrl Pts',(-2.4383668971224,-7.52584364682478,
41.0483825302795));
#238471=CARTESIAN_POINT('Ctrl Pts',(-2.45347245468287,-7.52093702365585,
41.0477383066767));
#238472=CARTESIAN_POINT('Ctrl Pts',(-2.46296787316416,-7.51783280301107,
41.0473322317163));
#238473=CARTESIAN_POINT('Ctrl Pts',(-2.50690719582342,-7.50337607847169,
41.0454478887469));
#238474=CARTESIAN_POINT('Ctrl Pts',(-2.54127835751409,-7.49180489411687,
41.0439588234731));
#238475=CARTESIAN_POINT('Ctrl Pts',(-3.33659015593797,-7.21795715504033,
41.0091334536547));
#238476=CARTESIAN_POINT('Ctrl Pts',(-4.05315067313634,-6.84132417149653,
40.9703917886254));
#238477=CARTESIAN_POINT('Ctrl Pts',(-4.97939950295789,-6.15708534962913,
40.9183549931759));
#238478=CARTESIAN_POINT('Ctrl Pts',(-5.24443306440607,-5.93296521418211,
40.9031176585472));
#238479=CARTESIAN_POINT('Ctrl Pts',(-5.59324502259268,-5.59630096841265,
40.8827411829602));
#238480=CARTESIAN_POINT('Ctrl Pts',(-5.69004090942325,-5.49785515395312,
40.8770448151079));
#238481=CARTESIAN_POINT('Ctrl Pts',(-5.79693849907084,-5.38328644139439,
40.8707011200634));
#238482=CARTESIAN_POINT('Ctrl Pts',(-5.80961431573372,-5.36960430390184,
40.8699480065784));
#238483=CARTESIAN_POINT('Ctrl Pts',(-5.82860683313839,-5.34895800861483,
40.8688182336109));
#238484=CARTESIAN_POINT('Ctrl Pts',(-5.83495965837832,-5.34202725368332,
40.8684401036363));
#238485=CARTESIAN_POINT('Ctrl Pts',(-5.84587360926192,-5.33007774199091,
40.8677900852868));
#238486=CARTESIAN_POINT('Ctrl Pts',(-5.85044065742265,-5.3250644226503,
40.8675179567374));
#238487=CARTESIAN_POINT('Ctrl Pts',(-5.85984123664472,-5.31471857015759,
40.8669575670575));
#238488=CARTESIAN_POINT('Ctrl Pts',(-5.86467394882794,-5.30938530085289,
40.8666693391533));
#238489=CARTESIAN_POINT('Ctrl Pts',(-5.87630393215415,-5.29651546766536,
40.8659753763027));
#238490=CARTESIAN_POINT('Ctrl Pts',(-5.88309399964106,-5.28897239495878,
40.8655699320696));
#238491=CARTESIAN_POINT('Ctrl Pts',(-5.90795268648622,-5.26124982671628,
40.8640845429697));
#238492=CARTESIAN_POINT('Ctrl Pts',(-5.92593223975613,-5.24099053542619,
40.8630081767097));
#238493=CARTESIAN_POINT('Ctrl Pts',(-6.22181759134387,-4.90411883986894,
40.8452596001976));
#238494=CARTESIAN_POINT('Ctrl Pts',(-6.47411235510459,-4.56588584959776,
40.8296579544249));
#238495=CARTESIAN_POINT('Ctrl Pts',(-7.04034076015635,-3.66480813162043,
40.7918176038611));
#238496=CARTESIAN_POINT('Ctrl Pts',(-7.31474470896616,-3.08085139283841,
40.7706197055535));
#238497=CARTESIAN_POINT('Ctrl Pts',(-7.57098143575211,-2.30125550977007,
40.7408230835879));
#238498=CARTESIAN_POINT('Ctrl Pts',(-7.62078809436649,-2.13052103914183,
40.7342001877652));
#238499=CARTESIAN_POINT('Ctrl Pts',(-7.68404135629249,-1.88294257598479,
40.7243011654923));
#238500=CARTESIAN_POINT('Ctrl Pts',(-7.70217209096954,-1.80734838724972,
40.7212374913821));
#238501=CARTESIAN_POINT('Ctrl Pts',(-7.72219683173286,-1.71807636936456,
40.7175785105827));
#238502=CARTESIAN_POINT('Ctrl Pts',(-7.72517332907833,-1.70464288098104,
40.717026843419));
#238503=CARTESIAN_POINT('Ctrl Pts',(-7.72968329499523,-1.68403414276137,
40.7161789388692));
#238504=CARTESIAN_POINT('Ctrl Pts',(-7.73124186100431,-1.67686437171393,
40.7158836613779));
#238505=CARTESIAN_POINT('Ctrl Pts',(-7.73406753038487,-1.66377794427556,
40.7153441936115));
#238506=CARTESIAN_POINT('Ctrl Pts',(-7.73533782557549,-1.6578619774857,
40.715100123017));
#238507=CARTESIAN_POINT('Ctrl Pts',(-7.73788008050035,-1.6459557590787,
40.7146085340985));
#238508=CARTESIAN_POINT('Ctrl Pts',(-7.73915187450848,-1.63996547649116,
40.7143610098755));
#238509=CARTESIAN_POINT('Ctrl Pts',(-7.74275558663714,-1.62289406768938,
40.713655058165));
#238510=CARTESIAN_POINT('Ctrl Pts',(-7.74507066474516,-1.61180942604657,
40.7131960228799));
#238511=CARTESIAN_POINT('Ctrl Pts',(-7.75486041985839,-1.56442775938644,
40.7112311692262));
#238512=CARTESIAN_POINT('Ctrl Pts',(-7.76210373800981,-1.52808371994476,
40.7097172880214));
#238513=CARTESIAN_POINT('Ctrl Pts',(-7.7699405016551,-1.4872679250133,40.7080104755257));
#238514=CARTESIAN_POINT('Ctrl Pts',(-7.77078586890594,-1.48284465118816,
40.7078254178229));
#238515=CARTESIAN_POINT('Ctrl Pts',(-7.83494860717424,-1.14555979643847,
40.6937077632809));
#238516=CARTESIAN_POINT('Ctrl Pts',(-7.87681762142771,-0.808984523196858,
40.6791532968308));
#238517=CARTESIAN_POINT('Ctrl Pts',(-7.90632403430723,-0.314033589777592,
40.6577503719093));
#238518=CARTESIAN_POINT('Ctrl Pts',(-7.91099952265989,-0.15704629847537,
40.6509581643851));
#238519=CARTESIAN_POINT('Ctrl Pts',(-7.91100234797369,0.772373789970606,
40.6108749923711));
#238520=CARTESIAN_POINT('Ctrl Pts',(-7.79788667119714,1.54064593551892,
40.578844518645));
#238521=CARTESIAN_POINT('Ctrl Pts',(-7.55062270443671,2.36205473388458,
40.5440179223328));
#238522=CARTESIAN_POINT('Ctrl Pts',(-7.52469935148756,2.44337995427355,
40.540562126901));
#238523=CARTESIAN_POINT('Ctrl Pts',(-7.48726342187173,2.55457034081584,
40.5358267958462));
#238524=CARTESIAN_POINT('Ctrl Pts',(-7.47687824320938,2.58480848789389,
40.5345379450999));
#238525=CARTESIAN_POINT('Ctrl Pts',(-7.45871756391708,2.63666093459443,
40.5323259268704));
#238526=CARTESIAN_POINT('Ctrl Pts',(-7.45103071614268,2.65830582374256,
40.5314019885384));
#238527=CARTESIAN_POINT('Ctrl Pts',(-7.43496316436037,2.70293213185022,
40.529495856555));
#238528=CARTESIAN_POINT('Ctrl Pts',(-7.42656991338957,2.72590878244444,
40.5285137882891));
#238529=CARTESIAN_POINT('Ctrl Pts',(-7.40668957857656,2.77955809941648,
40.5262191121037));
#238530=CARTESIAN_POINT('Ctrl Pts',(-7.39511829835713,2.81019912181624,
40.5249073162285));
#238531=CARTESIAN_POINT('Ctrl Pts',(-7.35675365339833,2.90991156737503,
40.5206342483615));
#238532=CARTESIAN_POINT('Ctrl Pts',(-7.3291801617614,2.97867888759196,40.5176807207594));
#238533=CARTESIAN_POINT('Ctrl Pts',(-7.04895884406455,3.65008135229361,
40.4887693267845));
#238534=CARTESIAN_POINT('Ctrl Pts',(-6.72353035685079,4.21960368041695,
40.46385531856));
#238535=CARTESIAN_POINT('Ctrl Pts',(-6.19674893016468,4.92290214617427,
40.4296839260125));
#238536=CARTESIAN_POINT('Ctrl Pts',(-6.05407085248918,5.09734090286663,
40.4208586935318));
#238537=CARTESIAN_POINT('Ctrl Pts',(-5.88616374296398,5.28561514880879,
40.4107634761776));
#238538=CARTESIAN_POINT('Ctrl Pts',(-5.86807612122627,5.3056888085986,40.4096795047913));
#238539=CARTESIAN_POINT('Ctrl Pts',(-5.84109823327695,5.33532218646695,
40.4080675396181));
#238540=CARTESIAN_POINT('Ctrl Pts',(-5.83228651665282,5.34495326363265,
40.4075417772004));
#238541=CARTESIAN_POINT('Ctrl Pts',(-5.81657685624194,5.36203858825917,
40.4066057133409));
#238542=CARTESIAN_POINT('Ctrl Pts',(-5.80968831254594,5.36950145329251,
40.4061956901212));
#238543=CARTESIAN_POINT('Ctrl Pts',(-5.79517818902847,5.38516072431975,
40.4053328871233));
#238544=CARTESIAN_POINT('Ctrl Pts',(-5.78755355013952,5.39335425988686,
40.4048800146035));
#238545=CARTESIAN_POINT('Ctrl Pts',(-5.76727022158068,5.4150584457735,40.4036765512428));
#238546=CARTESIAN_POINT('Ctrl Pts',(-5.75458154121131,5.42854078555881,
40.4029249978295));
#238547=CARTESIAN_POINT('Ctrl Pts',(-5.68454047870131,5.50244129261868,
40.3987835465537));
#238548=CARTESIAN_POINT('Ctrl Pts',(-5.62628457520848,5.56199444060645,
40.395365398516));
#238549=CARTESIAN_POINT('Ctrl Pts',(-5.44400371047081,5.74253974683037,
40.3847689166946));
#238550=CARTESIAN_POINT('Ctrl Pts',(-5.31693715025488,5.86038537166933,
40.3775195902244));
#238551=CARTESIAN_POINT('Ctrl Pts',(-4.79628416821656,6.31237380172243,
40.3485273933873));
#238552=CARTESIAN_POINT('Ctrl Pts',(-4.3742565208147,6.6118316471179,40.3266564531261));
#238553=CARTESIAN_POINT('Ctrl Pts',(-3.79644263484986,6.94213488557179,
40.2992621339574));
#238554=CARTESIAN_POINT('Ctrl Pts',(-3.66474689035937,7.01254910149011,
40.2931666450985));
#238555=CARTESIAN_POINT('Ctrl Pts',(-3.49626755928694,7.09658737874406,
40.2855436529132));
#238556=CARTESIAN_POINT('Ctrl Pts',(-3.46127141784807,7.11372191358679,
40.2839694948362));
#238557=CARTESIAN_POINT('Ctrl Pts',(-3.40547513865571,7.14053122766648,
40.2814740556934));
#238558=CARTESIAN_POINT('Ctrl Pts',(-3.38475713788507,7.15037525275031,
40.2805505748934));
#238559=CARTESIAN_POINT('Ctrl Pts',(-3.3459610811637,7.16860255018474,40.278826996598));
#238560=CARTESIAN_POINT('Ctrl Pts',(-3.32789360558772,7.17700788851833,
40.2780266210041));
#238561=CARTESIAN_POINT('Ctrl Pts',(-3.28751418085551,7.19560791417237,
40.2762428878666));
#238562=CARTESIAN_POINT('Ctrl Pts',(-3.26518616719312,7.20576727645902,
40.2752599843282));
#238563=CARTESIAN_POINT('Ctrl Pts',(-3.19941161439191,7.23532654752022,
40.2723743377453));
#238564=CARTESIAN_POINT('Ctrl Pts',(-3.15583677350629,7.25443858765414,
40.2704751798555));
#238565=CARTESIAN_POINT('Ctrl Pts',(-2.76477433797736,7.4217692765787,40.2535376005496));
#238566=CARTESIAN_POINT('Ctrl Pts',(-2.40724711869554,7.54531696811186,
40.2387646848321));
#238567=CARTESIAN_POINT('Ctrl Pts',(-1.69872307434632,7.73464329169606,
40.2103430583309));
#238568=CARTESIAN_POINT('Ctrl Pts',(-1.34938059035412,7.80317559349103,
40.1967986474047));
#238569=CARTESIAN_POINT('Ctrl Pts',(-0.497775541314349,7.9113201019901,
40.1644947463322));
#238570=CARTESIAN_POINT('Ctrl Pts',(0.00593936727166913,7.92696014748089,
40.1460161682002));
#238571=CARTESIAN_POINT('Ctrl Pts',(0.669194255993171,7.88430632434497,
40.1204784504287));
#238572=CARTESIAN_POINT('Ctrl Pts',(0.830320863652399,7.86896888133234,
40.1141705893205));
#238573=CARTESIAN_POINT('Ctrl Pts',(1.01010849946013,7.84627161771918,40.1069324370505));
#238574=CARTESIAN_POINT('Ctrl Pts',(1.02934969102803,7.84377056562541,40.1061552127109));
#238575=CARTESIAN_POINT('Ctrl Pts',(1.05737495349073,7.84002282632107,40.1050192000771));
#238576=CARTESIAN_POINT('Ctrl Pts',(1.06616650824992,7.83883209958511,40.1046622623202));
#238577=CARTESIAN_POINT('Ctrl Pts',(1.08169724998666,7.836702007757,40.1040306835718));
#238578=CARTESIAN_POINT('Ctrl Pts',(1.08843727092537,7.83576873101463,40.1037562486358));
#238579=CARTESIAN_POINT('Ctrl Pts',(1.10238863413474,7.83381856675941,40.1031874656906));
#238580=CARTESIAN_POINT('Ctrl Pts',(1.10959979136409,7.83280041493283,40.1028930744439));
#238581=CARTESIAN_POINT('Ctrl Pts',(1.1280979557436,7.8301625795568,40.1021368533298));
#238582=CARTESIAN_POINT('Ctrl Pts',(1.13938286488857,7.82852845084185,40.1016745182533));
#238583=CARTESIAN_POINT('Ctrl Pts',(1.18574710310853,7.82171223082387,40.099770787206));
#238584=CARTESIAN_POINT('Ctrl Pts',(1.2207946118134,7.81631875493454,40.0983217933654));
#238585=CARTESIAN_POINT('Ctrl Pts',(1.43957106662348,7.78114383205426,40.0892092610057));
#238586=CARTESIAN_POINT('Ctrl Pts',(1.6222076876335,7.74512698262287,40.0812696047363));
#238587=CARTESIAN_POINT('Ctrl Pts',(2.05357500590967,7.64413310936212,40.0618303084283));
#238588=CARTESIAN_POINT('Ctrl Pts',(2.30074261574574,7.57340838405021,40.0501737565286));
#238589=CARTESIAN_POINT('Ctrl Pts',(3.12962459886837,7.29190361439506,40.0101392731647));
#238590=CARTESIAN_POINT('Ctrl Pts',(3.68996569173267,7.02500741221093,39.981634394864));
#238591=CARTESIAN_POINT('Ctrl Pts',(4.36891174306192,6.5977452557836,39.947482330211));
#238592=CARTESIAN_POINT('Ctrl Pts',(4.52086260901511,6.49456999198483,39.9398489570674));
#238593=CARTESIAN_POINT('Ctrl Pts',(4.68616055607473,6.37371691234888,39.9315559304474));
#238594=CARTESIAN_POINT('Ctrl Pts',(4.70317852423507,6.36116968915161,39.9307022431757));
#238595=CARTESIAN_POINT('Ctrl Pts',(4.72794812632327,6.34275350588278,39.929459831041));
#238596=CARTESIAN_POINT('Ctrl Pts',(4.73573949836382,6.33693829274793,39.9290690440187));
#238597=CARTESIAN_POINT('Ctrl Pts',(4.74928361986323,6.32679049461528,39.9283897480596));
#238598=CARTESIAN_POINT('Ctrl Pts',(4.75504120159098,6.3224643958016,39.9281009894505));
#238599=CARTESIAN_POINT('Ctrl Pts',(4.76563212351459,6.31448399935484,39.9275698400554));
#238600=CARTESIAN_POINT('Ctrl Pts',(4.77046718520593,6.31083200139766,39.927327360621));
#238601=CARTESIAN_POINT('Ctrl Pts',(4.78346099146956,6.30099410991741,39.9266757317295));
#238602=CARTESIAN_POINT('Ctrl Pts',(4.79161194323275,6.29479791705815,39.9262669823544));
#238603=CARTESIAN_POINT('Ctrl Pts',(4.81905516219072,6.27385193398609,39.9248908127163));
#238604=CARTESIAN_POINT('Ctrl Pts',(4.83829162214233,6.25902907312811,39.9239262430707));
#238605=CARTESIAN_POINT('Ctrl Pts',(5.16869034430632,6.00200341938804,39.9073594147257));
#238606=CARTESIAN_POINT('Ctrl Pts',(5.46139734846983,5.736949378959,39.8927264229657));
#238607=CARTESIAN_POINT('Ctrl Pts',(6.01745508057288,5.15212604582466,39.8640915068873));
#238608=CARTESIAN_POINT('Ctrl Pts',(6.27794370802062,4.83131443334262,39.8501927590075));
#238609=CARTESIAN_POINT('Ctrl Pts',(6.79821587437285,4.07699817135065,39.8189553805546));
#238610=CARTESIAN_POINT('Ctrl Pts',(7.04392660354598,3.63601958059191,39.8015964760974));
#238611=CARTESIAN_POINT('Ctrl Pts',(7.25901019616077,3.14511343640741,39.7804013203069));
#238612=CARTESIAN_POINT('Ctrl Pts',(7.27181065256443,3.11540323767162,39.7791114907648));
#238613=CARTESIAN_POINT('Ctrl Pts',(7.28730603817542,3.07882220005217,39.7775138077519));
#238614=CARTESIAN_POINT('Ctrl Pts',(7.29017421320001,3.07202463761152,39.7772165189923));
#238615=CARTESIAN_POINT('Ctrl Pts',(7.29490271913841,3.06077418433231,39.7767238024391));
#238616=CARTESIAN_POINT('Ctrl Pts',(7.29676849669299,3.05632357491983,39.7765287104422));
#238617=CARTESIAN_POINT('Ctrl Pts',(7.3001335763186,3.04827589872604,39.7761756183));
#238618=CARTESIAN_POINT('Ctrl Pts',(7.30163429644865,3.04467942280767,39.7760177062426));
#238619=CARTESIAN_POINT('Ctrl Pts',(7.30483994126542,3.03698109386714,39.7756794403149));
#238620=CARTESIAN_POINT('Ctrl Pts',(7.30654406903454,3.03287891270207,39.7754990367912));
#238621=CARTESIAN_POINT('Ctrl Pts',(7.31114830290633,3.02176918531788,39.7750100400641));
#238622=CARTESIAN_POINT('Ctrl Pts',(7.31404178216675,3.01475891645706,39.7747010306974));
#238623=CARTESIAN_POINT('Ctrl Pts',(7.32895807282144,2.97847213023135,39.7730991453766));
#238624=CARTESIAN_POINT('Ctrl Pts',(7.34081498577084,2.94912833474925,39.7717957118249));
#238625=CARTESIAN_POINT('Ctrl Pts',(7.41214618164648,2.76950041500587,39.7637717178741));
#238626=CARTESIAN_POINT('Ctrl Pts',(7.46717632886497,2.61750169107085,39.7567906328849));
#238627=CARTESIAN_POINT('Ctrl Pts',(7.6425935150441,2.08230054402993,39.7318432890643));
#238628=CARTESIAN_POINT('Ctrl Pts',(7.73843080990549,1.69170914979968,39.7130258836722));
#238629=CARTESIAN_POINT('Ctrl Pts',(7.90947319428854,0.661372734536837,
39.6645049237019));
#238630=CARTESIAN_POINT('Ctrl Pts',(7.93707607450059,0.0166292319216803,
39.6354409402011));
#238631=CARTESIAN_POINT('Ctrl Pts',(7.88301626232736,-0.666127036516802,
39.6075237348211));
#238632=CARTESIAN_POINT('Ctrl Pts',(7.87938397631287,-0.707798594534086,
39.6058299266597));
#238633=CARTESIAN_POINT('Ctrl Pts',(7.87425824196206,-0.761661913541318,
39.6036534173758));
#238634=CARTESIAN_POINT('Ctrl Pts',(7.87306671358917,-0.773881293818122,
39.603160512756));
#238635=CARTESIAN_POINT('Ctrl Pts',(7.87111485122181,-0.793426902090646,
39.6023734446436));
#238636=CARTESIAN_POINT('Ctrl Pts',(7.87037272538773,-0.800754902556105,
39.6020786649584));
#238637=CARTESIAN_POINT('Ctrl Pts',(7.86896010012639,-0.814511954830978,
39.6015258399994));
#238638=CARTESIAN_POINT('Ctrl Pts',(7.86829195344806,-0.820941238776542,
39.6012677152625));
#238639=CARTESIAN_POINT('Ctrl Pts',(7.86677389097498,-0.83537678359513,
39.6006886786768));
#238640=CARTESIAN_POINT('Ctrl Pts',(7.86591963067793,-0.843382586103295,
39.600367914354));
#238641=CARTESIAN_POINT('Ctrl Pts',(7.86341024346504,-0.866564126086607,
39.5994401588033));
#238642=CARTESIAN_POINT('Ctrl Pts',(7.86172340541166,-0.88173643570895,
39.5988342432992));
#238643=CARTESIAN_POINT('Ctrl Pts',(7.84983915724431,-0.985883726085517,
39.5946838968042));
#238644=CARTESIAN_POINT('Ctrl Pts',(7.8381752333609,-1.07468657371834,39.5911894732191));
#238645=CARTESIAN_POINT('Ctrl Pts',(7.79976131148449,-1.33308578314917,
39.5811409899696));
#238646=CARTESIAN_POINT('Ctrl Pts',(7.76899527289545,-1.50203562170476,
39.5747231579468));
#238647=CARTESIAN_POINT('Ctrl Pts',(7.69079955105152,-1.86414336961229,
39.5612130823033));
#238648=CARTESIAN_POINT('Ctrl Pts',(7.64153601517832,-2.05678398142565,
39.554179662604));
#238649=CARTESIAN_POINT('Ctrl Pts',(7.35863999617281,-3.01158210706327,
39.5196356725454));
#238650=CARTESIAN_POINT('Ctrl Pts',(7.0180764893229,-3.73702445245757,39.4948757103241));
#238651=CARTESIAN_POINT('Ctrl Pts',(6.55071837234274,-4.43552897307171,
39.4619324958306));
#238652=CARTESIAN_POINT('Ctrl Pts',(6.52613167462745,-4.47162539624775,
39.4602004486837));
#238653=CARTESIAN_POINT('Ctrl Pts',(6.49678555560715,-4.51395168099094,
39.4581319095132));
#238654=CARTESIAN_POINT('Ctrl Pts',(6.49231374453956,-4.52038102105089,
39.4578166694836));
#238655=CARTESIAN_POINT('Ctrl Pts',(6.48511265210462,-4.53070165435446,
39.4573089578732));
#238656=CARTESIAN_POINT('Ctrl Pts',(6.4823894044477,-4.53459713756698,39.4571169389188));
#238657=CARTESIAN_POINT('Ctrl Pts',(6.47752182487494,-4.54154664551803,
39.4567736912171));
#238658=CARTESIAN_POINT('Ctrl Pts',(6.47537884746101,-4.54460160046006,
39.4566225646633));
#238659=CARTESIAN_POINT('Ctrl Pts',(6.47088541436579,-4.55099765345676,
39.4563056610577));
#238660=CARTESIAN_POINT('Ctrl Pts',(6.46853453141645,-4.55433844848692,
39.4561398520972));
#238661=CARTESIAN_POINT('Ctrl Pts',(6.46238463628175,-4.56306358014097,
39.4557060722785));
#238662=CARTESIAN_POINT('Ctrl Pts',(6.4585814894613,-4.56844498348352,39.4554377947126));
#238663=CARTESIAN_POINT('Ctrl Pts',(6.44200276932736,-4.59184157861496,
39.4542682334181));
#238664=CARTESIAN_POINT('Ctrl Pts',(6.42915862733806,-4.6098078146529,39.4533619183058));
#238665=CARTESIAN_POINT('Ctrl Pts',(6.33697283982645,-4.73762153613201,
39.4468569987781));
#238666=CARTESIAN_POINT('Ctrl Pts',(6.25489964491543,-4.84546272994121,
39.4410655121948));
#238667=CARTESIAN_POINT('Ctrl Pts',(6.04825966640609,-5.10297727938587,
39.4265959749351));
#238668=CARTESIAN_POINT('Ctrl Pts',(5.9208592967262,-5.25026091175052,39.4177677597876));
#238669=CARTESIAN_POINT('Ctrl Pts',(5.65165370940961,-5.53920886390032,
39.3995486536993));
#238670=CARTESIAN_POINT('Ctrl Pts',(5.50963163843938,-5.68049124530426,
39.3901556754905));
#238671=CARTESIAN_POINT('Ctrl Pts',(5.30779506440411,-5.86657906017108,
39.3772538121195));
#238672=CARTESIAN_POINT('Ctrl Pts',(5.25247838047507,-5.91615662337351,
39.3737608792202));
#238673=CARTESIAN_POINT('Ctrl Pts',(5.1346307563961,-6.01882170299738,39.3664193855873));
#238674=CARTESIAN_POINT('Ctrl Pts',(5.07195542982818,-6.07173088622744,
39.3625721246829));
#238675=CARTESIAN_POINT('Ctrl Pts',(4.98769380057236,-6.14064750997105,
39.357482595284));
#238676=CARTESIAN_POINT('Ctrl Pts',(4.96683279642721,-6.15753305064508,
39.3562291459551));
#238677=CARTESIAN_POINT('Ctrl Pts',(4.84816404091072,-6.25259176290216,
39.3491370728797));
#238678=CARTESIAN_POINT('Ctrl Pts',(4.7485956033084,-6.32854163513958,39.3433331587604));
#238679=CARTESIAN_POINT('Ctrl Pts',(4.25310540789064,-6.68821657910273,
39.3152339064891));
#238680=CARTESIAN_POINT('Ctrl Pts',(3.83332893144382,-6.93735195977141,
39.2939014058871));
#238681=CARTESIAN_POINT('Ctrl Pts',(3.36427164458332,-7.16007163635944,
39.2727834711049));
#238682=CARTESIAN_POINT('Ctrl Pts',(3.33521722870478,-7.17365148349033,
39.271485501209));
#238683=CARTESIAN_POINT('Ctrl Pts',(3.2958022348712,-7.19178257689446,39.2697381816599));
#238684=CARTESIAN_POINT('Ctrl Pts',(3.28551350961971,-7.19648872605534,
39.2692833065709));
#238685=CARTESIAN_POINT('Ctrl Pts',(3.26854048262703,-7.20420834464605,
39.2685349404013));
#238686=CARTESIAN_POINT('Ctrl Pts',(3.26186204141069,-7.20723461411041,
39.2682409944066));
#238687=CARTESIAN_POINT('Ctrl Pts',(3.24896859907966,-7.21305555768865,
39.2676744930654));
#238688=CARTESIAN_POINT('Ctrl Pts',(3.2427541770195,-7.21585149402628,39.2674018931087));
#238689=CARTESIAN_POINT('Ctrl Pts',(3.22845948657297,-7.22226063564699,
39.2667758639015));
#238690=CARTESIAN_POINT('Ctrl Pts',(3.22037674433235,-7.22586831951005,
39.2664226302322));
#238691=CARTESIAN_POINT('Ctrl Pts',(3.19519341552973,-7.23705810080611,
39.2653243750825));
#238692=CARTESIAN_POINT('Ctrl Pts',(3.1780719213602,-7.24459314151474,39.2645810140054));
#238693=CARTESIAN_POINT('Ctrl Pts',(2.98343878356135,-7.3294269522037,39.2561678659832));
#238694=CARTESIAN_POINT('Ctrl Pts',(2.8031676618595,-7.40024754997926,39.2487285214943));
#238695=CARTESIAN_POINT('Ctrl Pts',(2.30802229274416,-7.57407486475203,
39.2291011393963));
#238696=CARTESIAN_POINT('Ctrl Pts',(1.98898407430081,-7.66404182105322,
39.2173249318956));
#238697=CARTESIAN_POINT('Ctrl Pts',(1.30681986779557,-7.81092563168555,
39.1930191378243));
#238698=CARTESIAN_POINT('Ctrl Pts',(0.943482622422935,-7.86308904344701,
39.1805736772349));
#238699=CARTESIAN_POINT('Ctrl Pts',(0.359184972264966,-7.90588236407069,
39.1599403049664));
#238700=CARTESIAN_POINT('Ctrl Pts',(0.139962716899381,-7.91279922510106,
39.1520553092065));
#238701=CARTESIAN_POINT('Ctrl Pts',(-0.221047111317497,-7.90918244205259,
39.1384658144267));
#238702=CARTESIAN_POINT('Ctrl Pts',(-0.362756532939589,-7.90395047343957,
39.132964486278));
#238703=CARTESIAN_POINT('Ctrl Pts',(-0.519231561498289,-7.89395621367766,
39.1266913395954));
#238704=CARTESIAN_POINT('Ctrl Pts',(-0.534202161363723,-7.89295725090466,
39.1260892997371));
#238705=CARTESIAN_POINT('Ctrl Pts',(-0.55672519408571,-7.89138995483522,
39.1251808116274));
#238706=CARTESIAN_POINT('Ctrl Pts',(-0.564279852216511,-7.89085335112084,
39.1248756251144));
#238707=CARTESIAN_POINT('Ctrl Pts',(-0.577349614028726,-7.88990614698147,
39.1243468555256));
#238708=CARTESIAN_POINT('Ctrl Pts',(-0.582865086493773,-7.88950061003361,
39.1241234703382));
#238709=CARTESIAN_POINT('Ctrl Pts',(-0.594303099490266,-7.88864754585823,
39.123659713978));
#238710=CARTESIAN_POINT('Ctrl Pts',(-0.600225570156667,-7.88819913171024,
39.1234193087174));
#238711=CARTESIAN_POINT('Ctrl Pts',(-0.614102164234724,-7.8871327605112,
39.1228553858304));
#238712=CARTESIAN_POINT('Ctrl Pts',(-0.622055861457477,-7.88650944047409,
39.1225316646589));
#238713=CARTESIAN_POINT('Ctrl Pts',(-0.64777094388794,-7.88445504263871,
39.1214834637921));
#238714=CARTESIAN_POINT('Ctrl Pts',(-0.665528370603681,-7.88297599239676,
39.1207571980808));
#238715=CARTESIAN_POINT('Ctrl Pts',(-0.961642688585574,-7.85730438486096,
39.1086070511222));
#238716=CARTESIAN_POINT('Ctrl Pts',(-1.23851832859792,-7.81844267469711,
39.0966730025797));
#238717=CARTESIAN_POINT('Ctrl Pts',(-2.26868898926957,-7.61775005000018,
39.0511396957554));
#238718=CARTESIAN_POINT('Ctrl Pts',(-2.99919681267972,-7.36084965174593,
39.0170010411374));
#238719=CARTESIAN_POINT('Ctrl Pts',(-3.80154720339991,-6.93907036048083,
38.9795614679564));
#238720=CARTESIAN_POINT('Ctrl Pts',(-3.92040934276124,-6.87261599001586,
38.9740009093031));
#238721=CARTESIAN_POINT('Ctrl Pts',(-4.0630162838258,-6.78798203620403,
38.967300447851));
#238722=CARTESIAN_POINT('Ctrl Pts',(-4.0884479541028,-6.77269479515523,
38.9661043407375));
#238723=CARTESIAN_POINT('Ctrl Pts',(-4.1273302762464,-6.74902340832795,
38.9642738327391));
#238724=CARTESIAN_POINT('Ctrl Pts',(-4.14084268476378,-6.74074135667223,
38.9636373600786));
#238725=CARTESIAN_POINT('Ctrl Pts',(-4.16514113705716,-6.72574766766972,
38.9624922370781));
#238726=CARTESIAN_POINT('Ctrl Pts',(-4.17593606508903,-6.71905055511353,
38.961983286741));
#238727=CARTESIAN_POINT('Ctrl Pts',(-4.19893430486621,-6.70470574368689,
38.9608985301386));
#238728=CARTESIAN_POINT('Ctrl Pts',(-4.21113296480193,-6.69705066132884,
38.9603228824472));
#238729=CARTESIAN_POINT('Ctrl Pts',(-4.24399308143047,-6.67630451613915,
38.9587714914036));
#238730=CARTESIAN_POINT('Ctrl Pts',(-4.26461488405599,-6.6631508437261,
38.9577971021183));
#238731=CARTESIAN_POINT('Ctrl Pts',(-4.36662954372632,-6.59741292276161,
38.9529728854797));
#238732=CARTESIAN_POINT('Ctrl Pts',(-4.44711340348016,-6.54343134258716,
38.949154380549));
#238733=CARTESIAN_POINT('Ctrl Pts',(-5.13729534301404,-6.06189992185897,
38.9162852650773));
#238734=CARTESIAN_POINT('Ctrl Pts',(-5.68474661841976,-5.55176085948237,
38.8898898009307));
#238735=CARTESIAN_POINT('Ctrl Pts',(-6.345612358851,-4.73404902000102,38.8512052838017));
#238736=CARTESIAN_POINT('Ctrl Pts',(-6.52437542221823,-4.48447513137996,
38.8397045301339));
#238737=CARTESIAN_POINT('Ctrl Pts',(-6.69773345473422,-4.21006023195367,
38.8267469164493));
#238738=CARTESIAN_POINT('Ctrl Pts',(-6.70723004528729,-4.19491426605578,
38.8260307417187));
#238739=CARTESIAN_POINT('Ctrl Pts',(-6.72028619414195,-4.17393353813587,
38.8250371204291));
#238740=CARTESIAN_POINT('Ctrl Pts',(-6.72388969836193,-4.16812608204342,
38.8247619228636));
#238741=CARTESIAN_POINT('Ctrl Pts',(-6.73005956652532,-4.15815381665238,
38.824289074913));
#238742=CARTESIAN_POINT('Ctrl Pts',(-6.73262960495915,-4.15399127757514,
38.8240916153339));
#238743=CARTESIAN_POINT('Ctrl Pts',(-6.73763388694166,-4.14586929464999,
38.8237061550521));
#238744=CARTESIAN_POINT('Ctrl Pts',(-6.74006850512477,-4.14191008459247,
38.8235181741941));
#238745=CARTESIAN_POINT('Ctrl Pts',(-6.74590184169187,-4.13240506842805,
38.8230666818386));
#238746=CARTESIAN_POINT('Ctrl Pts',(-6.74929720889266,-4.12685721742079,
38.8228029933496));
#238747=CARTESIAN_POINT('Ctrl Pts',(-6.75952655077611,-4.11009662154917,
38.822005853868));
#238748=CARTESIAN_POINT('Ctrl Pts',(-6.76633942930401,-4.09887108278781,
38.8214712741906));
#238749=CARTESIAN_POINT('Ctrl Pts',(-6.83809994267305,-3.97996525406577,
38.8158009496879));
#238750=CARTESIAN_POINT('Ctrl Pts',(-6.90049212903592,-3.87077988264666,
38.810516976508));
#238751=CARTESIAN_POINT('Ctrl Pts',(-7.03306817711749,-3.62537485366121,
38.7985272381898));
#238752=CARTESIAN_POINT('Ctrl Pts',(-7.10195123930655,-3.48850621869802,
38.7917687265623));
#238753=CARTESIAN_POINT('Ctrl Pts',(-7.58304626281119,-2.45919381169649,
38.7408263405149));
#238754=CARTESIAN_POINT('Ctrl Pts',(-7.82978586759737,-1.49850900763372,
38.6938860509098));
#238755=CARTESIAN_POINT('Ctrl Pts',(-7.89711545381878,-0.470795646110987,
38.6514934850059));
#238756=CARTESIAN_POINT('Ctrl Pts',(-7.89974506321828,-0.424392577760123,
38.6495926731345));
#238757=CARTESIAN_POINT('Ctrl Pts',(-7.9032569944861,-0.350970695827668,
38.6466057750882));
#238758=CARTESIAN_POINT('Ctrl Pts',(-7.90440999868677,-0.323966265265489,
38.645511619673));
#238759=CARTESIAN_POINT('Ctrl Pts',(-7.90580520635408,-0.286823731104289,
38.6440126961079));
#238760=CARTESIAN_POINT('Ctrl Pts',(-7.90616634151718,-0.276690431204561,
38.6436043709949));
#238761=CARTESIAN_POINT('Ctrl Pts',(-7.90675041216298,-0.259365923096405,
38.6429073179335));
#238762=CARTESIAN_POINT('Ctrl Pts',(-7.90698302131279,-0.252175064862617,
38.6426183007084));
#238763=CARTESIAN_POINT('Ctrl Pts',(-7.90742979372104,-0.237754845543562,
38.6420393330728));
#238764=CARTESIAN_POINT('Ctrl Pts',(-7.90764385320122,-0.23052548772057,
38.6417493860273));
#238765=CARTESIAN_POINT('Ctrl Pts',(-7.90805392097528,-0.216003257010647,
38.6411675638293));
#238766=CARTESIAN_POINT('Ctrl Pts',(-7.90824975574135,-0.208710386087284,
38.6408756941452));
#238767=CARTESIAN_POINT('Ctrl Pts',(-7.90867410624758,-0.192048711219186,
38.6402095868746));
#238768=CARTESIAN_POINT('Ctrl Pts',(-7.90889606318929,-0.182679743604795,
38.6398355457794));
#238769=CARTESIAN_POINT('Ctrl Pts',(-7.90961151354725,-0.150029827977226,
38.6385338352241));
#238770=CARTESIAN_POINT('Ctrl Pts',(-7.91001886535678,-0.126747013976437,
38.63760874234));
#238771=CARTESIAN_POINT('Ctrl Pts',(-7.91077144928316,-0.069207562755391,
38.6353302278485));
#238772=CARTESIAN_POINT('Ctrl Pts',(-7.91099697586045,-0.0349497599870603,
38.6339803854939));
#238773=CARTESIAN_POINT('Ctrl Pts',(-7.91099996979002,-0.000691362661667347,
38.6326370762697));
#238774=CARTESIAN_POINT('',(-7.91099714850641,0.00671686857199988,36.6423315082371));
#238775=CARTESIAN_POINT('Ctrl Pts',(-7.91099999384339,-0.000312105552225759,
38.6423075098952));
#238776=CARTESIAN_POINT('Ctrl Pts',(-7.91100845698712,0.214204840705644,
38.633703106139));
#238777=CARTESIAN_POINT('Ctrl Pts',(-7.90228725669127,0.428551622663759,
38.6250987023827));
#238778=CARTESIAN_POINT('Ctrl Pts',(-7.88490367260169,0.642039775864754,
38.6164942986265));
#238779=CARTESIAN_POINT('Ctrl Pts',(-7.86749257111238,0.855865870816871,
38.607876274502));
#238780=CARTESIAN_POINT('Ctrl Pts',(-7.84139169850389,1.0688303849902,38.5992582503774));
#238781=CARTESIAN_POINT('Ctrl Pts',(-7.8067199407512,1.28025183720925,38.5906402262529));
#238782=CARTESIAN_POINT('Ctrl Pts',(-7.77197215411129,1.4921368983938,38.5820033043618));
#238783=CARTESIAN_POINT('Ctrl Pts',(-7.72861591878302,1.70247189396046,
38.5733663824707));
#238784=CARTESIAN_POINT('Ctrl Pts',(-7.67682144207909,1.9105846085517,38.5647294605796));
#238785=CARTESIAN_POINT('Ctrl Pts',(-7.62497517071932,2.11890543657738,
38.5560839017367));
#238786=CARTESIAN_POINT('Ctrl Pts',(-7.56467386178044,2.32499931604724,
38.5474383428938));
#238787=CARTESIAN_POINT('Ctrl Pts',(-7.49613763527628,2.5282091592656,38.538792784051));
#238788=CARTESIAN_POINT('Ctrl Pts',(-7.42750453073433,2.73170624576942,
38.5301350044481));
#238789=CARTESIAN_POINT('Ctrl Pts',(-7.35061330897551,2.93231092054215,
38.5214772248452));
#238790=CARTESIAN_POINT('Ctrl Pts',(-7.26573314758899,3.12938377768317,
38.5128194452423));
#238791=CARTESIAN_POINT('Ctrl Pts',(-7.20608463478069,3.26787435841868,
38.5067352947282));
#238792=CARTESIAN_POINT('Ctrl Pts',(-7.14249186566219,3.40462120763661,
38.5006511442142));
#238793=CARTESIAN_POINT('Ctrl Pts',(-7.0750620256049,3.53940931990685,38.4945669937001));
#238794=CARTESIAN_POINT('Ctrl Pts',(-6.9883054145714,3.7128304613219,38.4867390012391));
#238795=CARTESIAN_POINT('Ctrl Pts',(-6.89506198584002,3.88327317234364,
38.478911008778));
#238796=CARTESIAN_POINT('Ctrl Pts',(-6.79556355936849,4.05021442772887,
38.471083016317));
#238797=CARTESIAN_POINT('Ctrl Pts',(-6.69614917096623,4.2170146816804,38.4632616355119));
#238798=CARTESIAN_POINT('Ctrl Pts',(-6.59049048314436,4.38031906811435,
38.455440254707));
#238799=CARTESIAN_POINT('Ctrl Pts',(-6.47886629898294,4.53962690976947,
38.4476188739019));
#238800=CARTESIAN_POINT('Ctrl Pts',(-6.36731668231471,4.69882833016394,
38.4398027179572));
#238801=CARTESIAN_POINT('Ctrl Pts',(-6.24980970692534,4.85403823551805,
38.4319865620124));
#238802=CARTESIAN_POINT('Ctrl Pts',(-6.12666884578254,5.00478269799175,
38.4241704060676));
#238803=CARTESIAN_POINT('Ctrl Pts',(-6.00358714197187,5.15545474225958,
38.4163580050335));
#238804=CARTESIAN_POINT('Ctrl Pts',(-5.87487716579644,5.30166534453566,
38.4085456039994));
#238805=CARTESIAN_POINT('Ctrl Pts',(-5.74090433793375,5.44297146627589,
38.4007332029652));
#238806=CARTESIAN_POINT('Ctrl Pts',(-5.60697066885577,5.58423628579022,
38.3929230854101));
#238807=CARTESIAN_POINT('Ctrl Pts',(-5.4677774550567,5.72059922564389,38.3851129678549));
#238808=CARTESIAN_POINT('Ctrl Pts',(-5.32372895307522,5.85165199188987,
38.3773028502997));
#238809=CARTESIAN_POINT('Ctrl Pts',(-5.17967224363889,5.98271222513235,
38.3694922877473));
#238810=CARTESIAN_POINT('Ctrl Pts',(-5.03075994947666,6.1084614384403,38.3616817251948));
#238811=CARTESIAN_POINT('Ctrl Pts',(-4.8774319061609,6.22852944126971,38.3538711626424));
#238812=CARTESIAN_POINT('Ctrl Pts',(-4.75795500587992,6.32208931779827,
38.3477849843867));
#238813=CARTESIAN_POINT('Ctrl Pts',(-4.63579765713189,6.41220035023896,
38.341698806131));
#238814=CARTESIAN_POINT('Ctrl Pts',(-4.51118132570738,6.49870479761844,
38.3356126278753));
#238815=CARTESIAN_POINT('Ctrl Pts',(-4.33426723146526,6.6215125851782,38.326972261872));
#238816=CARTESIAN_POINT('Ctrl Pts',(-4.15248085579787,6.73699201908061,
38.3183318958687));
#238817=CARTESIAN_POINT('Ctrl Pts',(-3.96643163827274,6.84480394598041,
38.3096915298653));
#238818=CARTESIAN_POINT('Ctrl Pts',(-3.78007292961942,6.95279521700933,
38.3010367906942));
#238819=CARTESIAN_POINT('Ctrl Pts',(-3.58943740353826,7.05309337038577,
38.292382051523));
#238820=CARTESIAN_POINT('Ctrl Pts',(-3.39515819837377,7.14540564334982,
38.2837273123519));
#238821=CARTESIAN_POINT('Ctrl Pts',(-3.19487014829558,7.24057303470599,
38.2748048914935));
#238822=CARTESIAN_POINT('Ctrl Pts',(-2.99070969790356,7.32725258432475,
38.265882470635));
#238823=CARTESIAN_POINT('Ctrl Pts',(-2.78338977774932,7.40517807653,38.2569600497766));
#238824=CARTESIAN_POINT('Ctrl Pts',(-2.58161485771975,7.48101936542439,
38.2482762689134));
#238825=CARTESIAN_POINT('Ctrl Pts',(-2.37684751817603,7.54856879860471,
38.2395924880503));
#238826=CARTESIAN_POINT('Ctrl Pts',(-2.1697592267171,7.60763208219719,38.2309087071871));
#238827=CARTESIAN_POINT('Ctrl Pts',(-1.95413440900065,7.66913005327341,
38.221866966331));
#238828=CARTESIAN_POINT('Ctrl Pts',(-1.73599353148225,7.72142740611874,
38.2128252254749));
#238829=CARTESIAN_POINT('Ctrl Pts',(-1.51610670561192,7.76436355776818,
38.2037834846188));
#238830=CARTESIAN_POINT('Ctrl Pts',(-1.29621987974158,7.80729970941762,
38.1947417437627));
#238831=CARTESIAN_POINT('Ctrl Pts',(-1.07458738408571,7.84087463795251,
38.1857000029066));
#238832=CARTESIAN_POINT('Ctrl Pts',(-0.851987577295945,7.86498812256785,
38.1766582620505));
#238833=CARTESIAN_POINT('Ctrl Pts',(-0.647107318578418,7.88718210843792,
38.1683362682781));
#238834=CARTESIAN_POINT('Ctrl Pts',(-0.441233560333439,7.90137982551008,
38.1600142745056));
#238835=CARTESIAN_POINT('Ctrl Pts',(-0.235001561034966,7.90750879015073,
38.1516922807332));
#238836=CARTESIAN_POINT('Ctrl Pts',(-0.0289529880413066,7.9136323035843,
38.1433776886858));
#238837=CARTESIAN_POINT('Ctrl Pts',(0.177452899164308,7.91170137223193,
38.1350630966384));
#238838=CARTESIAN_POINT('Ctrl Pts',(0.383576684738589,7.90169538307602,
38.1267485045911));
#238839=CARTESIAN_POINT('Ctrl Pts',(0.589529710684304,7.89169768320603,
38.1184408006214));
#238840=CARTESIAN_POINT('Ctrl Pts',(0.795200810003176,7.87363828532877,
38.1101330966518));
#238841=CARTESIAN_POINT('Ctrl Pts',(0.99995067399829,7.84754863951606,38.1018253926821));
#238842=CARTESIAN_POINT('Ctrl Pts',(1.20449395460811,7.82148531698019,38.0935260708114));
#238843=CARTESIAN_POINT('Ctrl Pts',(1.40811756591243,7.78740795590163,38.0852267489406));
#238844=CARTESIAN_POINT('Ctrl Pts',(1.61018703286426,7.74539984243524,38.0769274270698));
#238845=CARTESIAN_POINT('Ctrl Pts',(1.81212739747043,7.70341856798647,38.0686334076425));
#238846=CARTESIAN_POINT('Ctrl Pts',(2.0125153127887,7.6535167074161,38.0603393882152));
#238847=CARTESIAN_POINT('Ctrl Pts',(2.21072478216942,7.59582891707692,38.0520453687879));
#238848=CARTESIAN_POINT('Ctrl Pts',(2.40878726936989,7.5381839051036,38.0437574997885));
#238849=CARTESIAN_POINT('Ctrl Pts',(2.60467425455987,7.47276456807297,38.0354696307892));
#238850=CARTESIAN_POINT('Ctrl Pts',(2.79777270488987,7.39975600217826,38.0271817617898));
#238851=CARTESIAN_POINT('Ctrl Pts',(2.8713807358158,7.37192555213036,38.0240224732685));
#238852=CARTESIAN_POINT('Ctrl Pts',(2.94458370948021,7.34299283840878,38.0208631847471));
#238853=CARTESIAN_POINT('Ctrl Pts',(3.0173482451762,7.31297002368614,38.0177038962258));
#238854=CARTESIAN_POINT('Ctrl Pts',(3.20396013851991,7.2359735274492,38.0096015863993));
#238855=CARTESIAN_POINT('Ctrl Pts',(3.3876085655808,7.15183612509522,38.0014992765729));
#238856=CARTESIAN_POINT('Ctrl Pts',(3.56773809816881,7.0608190645898,37.9933969667465));
#238857=CARTESIAN_POINT('Ctrl Pts',(3.74790738959376,6.96978191447212,37.9852928685491));
#238858=CARTESIAN_POINT('Ctrl Pts',(3.92455595283388,6.87186222152694,37.9771887703518));
#238859=CARTESIAN_POINT('Ctrl Pts',(4.09715270374799,6.76736734056683,37.9690846721544));
#238860=CARTESIAN_POINT('Ctrl Pts',(4.26980920095802,6.66283628753484,37.9609777686329));
#238861=CARTESIAN_POINT('Ctrl Pts',(4.43841081580003,6.55172567213123,37.9528708651113));
#238862=CARTESIAN_POINT('Ctrl Pts',(4.60245472775733,6.4343866435694,37.9447639615897));
#238863=CARTESIAN_POINT('Ctrl Pts',(4.76664658252704,6.31694179294026,37.9366497468665));
#238864=CARTESIAN_POINT('Ctrl Pts',(4.9262722610229,6.19325749019009,37.9285355321434));
#238865=CARTESIAN_POINT('Ctrl Pts',(5.08086030370299,6.06372654184332,37.9204213174202));
#238866=CARTESIAN_POINT('Ctrl Pts',(5.23552389854136,5.93413228754778,37.9123031370189));
#238867=CARTESIAN_POINT('Ctrl Pts',(5.38514470664768,5.79868589780636,37.9041849566175));
#238868=CARTESIAN_POINT('Ctrl Pts',(5.52928687788314,5.65781827404074,37.8960667762161));
#238869=CARTESIAN_POINT('Ctrl Pts',(5.67358406044154,5.51679916041943,37.8879398654766));
#238870=CARTESIAN_POINT('Ctrl Pts',(5.81239060997052,5.37034739094218,37.8798129547372));
#238871=CARTESIAN_POINT('Ctrl Pts',(5.94530888935037,5.21892931646056,37.8716860439978));
#238872=CARTESIAN_POINT('Ctrl Pts',(6.01583585765681,5.13858628320875,37.8673738727989));
#238873=CARTESIAN_POINT('Ctrl Pts',(6.08470572584131,5.05684558542534,37.8630617015999));
#238874=CARTESIAN_POINT('Ctrl Pts',(6.15186390298104,4.97378040520477,37.858749530401));
#238875=CARTESIAN_POINT('Ctrl Pts',(6.27642224235003,4.81971933106135,37.8507517420976));
#238876=CARTESIAN_POINT('Ctrl Pts',(6.39530611617561,4.66083294090514,37.8427539537941));
#238877=CARTESIAN_POINT('Ctrl Pts',(6.50813008396221,4.49757310226593,37.8347561654906));
#238878=CARTESIAN_POINT('Ctrl Pts',(6.62086193111673,4.33444656508584,37.8267649073716));
#238879=CARTESIAN_POINT('Ctrl Pts',(6.72754354352387,4.16695396967206,37.8187736492525));
#238880=CARTESIAN_POINT('Ctrl Pts',(6.82783007593749,3.99557973942749,37.8107823911334));
#238881=CARTESIAN_POINT('Ctrl Pts',(6.92805173036105,3.82431637567057,37.8027963027689));
#238882=CARTESIAN_POINT('Ctrl Pts',(7.02188638206704,3.64917666978696,37.7948102144045));
#238883=CARTESIAN_POINT('Ctrl Pts',(7.10903258373227,3.47067381403567,37.78682412604));
#238884=CARTESIAN_POINT('Ctrl Pts',(7.19613717947469,3.29225618031235,37.7788418504473));
#238885=CARTESIAN_POINT('Ctrl Pts',(7.27655954387214,3.11047889735802,37.7708595748546));
#238886=CARTESIAN_POINT('Ctrl Pts',(7.35004406976566,2.92587989714252,37.7628772992619));
#238887=CARTESIAN_POINT('Ctrl Pts',(7.42350596365979,2.74133775031768,37.754897482076));
#238888=CARTESIAN_POINT('Ctrl Pts',(7.49003415531645,2.55397592927376,37.7469176648901));
#238889=CARTESIAN_POINT('Ctrl Pts',(7.5494209388371,2.36435286880954,37.7389378477041));
#238890=CARTESIAN_POINT('Ctrl Pts',(7.61084854993877,2.16821340942876,37.7306838039978));
#238891=CARTESIAN_POINT('Ctrl Pts',(7.66463506173117,1.96965488086799,37.7224297602914));
#238892=CARTESIAN_POINT('Ctrl Pts',(7.71060635131985,1.7693136225627,37.7141757165851));
#238893=CARTESIAN_POINT('Ctrl Pts',(7.7550563337884,1.57560216702007,37.7061948202185));
#238894=CARTESIAN_POINT('Ctrl Pts',(7.79220000586526,1.38022442966616,37.698213923852));
#238895=CARTESIAN_POINT('Ctrl Pts',(7.82193174012489,1.18376722915736,37.6902330274855));
#238896=CARTESIAN_POINT('Ctrl Pts',(7.85167007520916,0.987266412641513,
37.6822503592581));
#238897=CARTESIAN_POINT('Ctrl Pts',(7.87399314149391,0.789685986156863,
37.6742676910307));
#238898=CARTESIAN_POINT('Ctrl Pts',(7.88884701985376,0.591619554565615,
37.6662850228033));
#238899=CARTESIAN_POINT('Ctrl Pts',(7.90370647925503,0.393478703558105,
37.6582993552513));
#238900=CARTESIAN_POINT('Ctrl Pts',(7.91109113082668,0.19485181704736,37.6503136876993));
#238901=CARTESIAN_POINT('Ctrl Pts',(7.91099915083615,-0.00366544263280774,
37.6423280201474));
#238902=CARTESIAN_POINT('Ctrl Pts',(7.9109071221447,-0.202287811830585,
37.6343381244005));
#238903=CARTESIAN_POINT('Ctrl Pts',(7.90333056992725,-0.40080010423743,
37.6263482286537));
#238904=CARTESIAN_POINT('Ctrl Pts',(7.88831971041271,-0.59860934365767,
37.6183583329068));
#238905=CARTESIAN_POINT('Ctrl Pts',(7.87329106929592,-0.796652904451298,
37.6103589724689));
#238906=CARTESIAN_POINT('Ctrl Pts',(7.85081055391816,-0.993991414902722,
37.602359612031));
#238907=CARTESIAN_POINT('Ctrl Pts',(7.82098008880441,-1.19003842396997,
37.594360251593));
#238908=CARTESIAN_POINT('Ctrl Pts',(7.79112877051456,-1.38622248094407,
37.5863552991514));
#238909=CARTESIAN_POINT('Ctrl Pts',(7.75391731762823,-1.58111290822961,
37.5783503467097));
#238910=CARTESIAN_POINT('Ctrl Pts',(7.70949829634302,-1.77413556942082,
37.570345394268));
#238911=CARTESIAN_POINT('Ctrl Pts',(7.66502130461008,-1.96741014093707,
37.5623299947102));
#238912=CARTESIAN_POINT('Ctrl Pts',(7.61331804226879,-2.1588117554832,37.5543145951523));
#238913=CARTESIAN_POINT('Ctrl Pts',(7.55459058646191,-2.34778237299396,
37.5462991955945));
#238914=CARTESIAN_POINT('Ctrl Pts',(7.54125967442368,-2.39067799387917,
37.5444797299801));
#238915=CARTESIAN_POINT('Ctrl Pts',(7.52756701912597,-2.43344843754376,
37.5426602643658));
#238916=CARTESIAN_POINT('Ctrl Pts',(7.51351532345902,-2.47608733370747,
37.5408407987515));
#238917=CARTESIAN_POINT('Ctrl Pts',(7.45357883045174,-2.65796046577115,
37.5330799995815));
#238918=CARTESIAN_POINT('Ctrl Pts',(7.38692818315501,-2.83797895846785,
37.5253192004114));
#238919=CARTESIAN_POINT('Ctrl Pts',(7.31369244998865,-3.01559674807144,
37.5175584012414));
#238920=CARTESIAN_POINT('Ctrl Pts',(7.24054562427867,-3.19299891143357,
37.5098070236049));
#238921=CARTESIAN_POINT('Ctrl Pts',(7.16082975950019,-3.36800584520122,
37.5020556459683));
#238922=CARTESIAN_POINT('Ctrl Pts',(7.07472422788984,-3.54008447629553,
37.4943042683318));
#238923=CARTESIAN_POINT('Ctrl Pts',(6.98870574909145,-3.71198913565495,
37.4865607273488));
#238924=CARTESIAN_POINT('Ctrl Pts',(6.89631062222946,-3.88097106769996,
37.4788171863659));
#238925=CARTESIAN_POINT('Ctrl Pts',(6.79776707992659,-4.04651501011258,
37.4710736453829));
#238926=CARTESIAN_POINT('Ctrl Pts',(6.69930319182685,-4.21192514090741,
37.4633363636186));
#238927=CARTESIAN_POINT('Ctrl Pts',(6.59470096549073,-4.37390250821271,
37.4555990818544));
#238928=CARTESIAN_POINT('Ctrl Pts',(6.4842355806927,-4.53195431729831,37.4478618000902));
#238929=CARTESIAN_POINT('Ctrl Pts',(6.37383712052952,-4.68991037186651,
37.4401292059008));
#238930=CARTESIAN_POINT('Ctrl Pts',(6.25758278008694,-4.84394531068987,
37.4323966117113));
#238931=CARTESIAN_POINT('Ctrl Pts',(6.13579232178727,-4.99359325374988,
37.4246640175219));
#238932=CARTESIAN_POINT('Ctrl Pts',(6.01405100795465,-5.14318081138638,
37.4169345435623));
#238933=CARTESIAN_POINT('Ctrl Pts',(5.88677825172797,-5.28838462093796,
37.4092050696027));
#238934=CARTESIAN_POINT('Ctrl Pts',(5.75433560554668,-5.42876991027781,
37.4014755956432));
#238935=CARTESIAN_POINT('Ctrl Pts',(5.62189509522726,-5.56915293566722,
37.3937462463344));
#238936=CARTESIAN_POINT('Ctrl Pts',(5.4842850992924,-5.70471732690519,37.3860168970257));
#238937=CARTESIAN_POINT('Ctrl Pts',(5.34190599268322,-5.83506309865927,
37.378287547717));
#238938=CARTESIAN_POINT('Ctrl Pts',(5.19952112985637,-5.96541414013762,
37.3705578859198));
#238939=CARTESIAN_POINT('Ctrl Pts',(5.05236703677377,-6.09054589860268,
37.3628282241227));
#238940=CARTESIAN_POINT('Ctrl Pts',(4.90087920027377,-6.21009694484103,
37.3550985623256));
#238941=CARTESIAN_POINT('Ctrl Pts',(4.74935748158953,-6.32967473019368,
37.3473671716911));
#238942=CARTESIAN_POINT('Ctrl Pts',(4.59350037119699,-6.44366909505734,
37.3396357810567));
#238943=CARTESIAN_POINT('Ctrl Pts',(4.43377454944196,-6.55176039280442,
37.3319043904223));
#238944=CARTESIAN_POINT('Ctrl Pts',(4.2739837266316,-6.65989567873293,37.3241698534678));
#238945=CARTESIAN_POINT('Ctrl Pts',(4.11032135462739,-6.7621229128854,37.3164353165133));
#238946=CARTESIAN_POINT('Ctrl Pts',(3.94328108648753,-6.85816704907002,
37.3087007795589));
#238947=CARTESIAN_POINT('Ctrl Pts',(3.77604410282847,-6.95432429194637,
37.3009571340016));
#238948=CARTESIAN_POINT('Ctrl Pts',(3.60542158991372,-7.04428371568233,
37.2932134884444));
#238949=CARTESIAN_POINT('Ctrl Pts',(3.43193060864663,-7.1278168675573,37.2854698428871));
#238950=CARTESIAN_POINT('Ctrl Pts',(3.25832846911384,-7.21140354037165,
37.2777212358604));
#238951=CARTESIAN_POINT('Ctrl Pts',(3.08185452803681,-7.28855559639948,
37.2699726288336));
#238952=CARTESIAN_POINT('Ctrl Pts',(2.90304347049441,-7.35909366759384,
37.2622240218069));
#238953=CARTESIAN_POINT('Ctrl Pts',(2.72396147978784,-7.42973861754103,
37.2544636741493));
#238954=CARTESIAN_POINT('Ctrl Pts',(2.54253563730978,-7.4937494487335,37.2467033264917));
#238955=CARTESIAN_POINT('Ctrl Pts',(2.35931450721544,-7.55099702397258,
37.2389429788341));
#238956=CARTESIAN_POINT('Ctrl Pts',(2.23330909823,-7.5903675055743,37.2336060082567));
#238957=CARTESIAN_POINT('Ctrl Pts',(2.10645482339439,-7.62654028306821,
37.2282690376794));
#238958=CARTESIAN_POINT('Ctrl Pts',(1.97893192261877,-7.65948754458419,
37.222932067102));
#238959=CARTESIAN_POINT('Ctrl Pts',(1.78983049186541,-7.70834444992577,
37.2150179688034));
#238960=CARTESIAN_POINT('Ctrl Pts',(1.59865148808939,-7.75026327553616,
37.2071038705047));
#238961=CARTESIAN_POINT('Ctrl Pts',(1.40594636116218,-7.78506492134361,
37.199189772206));
#238962=CARTESIAN_POINT('Ctrl Pts',(1.21346251425868,-7.81982660501237,
37.191284761532));
#238963=CARTESIAN_POINT('Ctrl Pts',(1.0194563706773,-7.84748732618165,37.183379750858));
#238964=CARTESIAN_POINT('Ctrl Pts',(0.82449426457881,-7.86791778094285,
37.175474740184));
#238965=CARTESIAN_POINT('Ctrl Pts',(0.629719818694653,-7.8883285704286,
37.1675773384552));
#238966=CARTESIAN_POINT('Ctrl Pts',(0.433991583861733,-7.9015229212864,
37.1596799367265));
#238967=CARTESIAN_POINT('Ctrl Pts',(0.237886089320525,-7.90742253888761,
37.1517825349978));
#238968=CARTESIAN_POINT('Ctrl Pts',(0.0419329444939414,-7.91331757321563,
37.1438912685734));
#238969=CARTESIAN_POINT('Ctrl Pts',(-0.154396533022881,-7.91192915444299,
37.136000002149));
#238970=CARTESIAN_POINT('Ctrl Pts',(-0.350520402733202,-7.90323076009221,
37.1281087357247));
#238971=CARTESIAN_POINT('Ctrl Pts',(-0.546528313749996,-7.8945375086873,
37.1202221350299));
#238972=CARTESIAN_POINT('Ctrl Pts',(-0.742330515623083,-7.87854290891249,
37.1123355343352));
#238973=CARTESIAN_POINT('Ctrl Pts',(-0.937344491595128,-7.85527251621968,
37.1044489336404));
#238974=CARTESIAN_POINT('Ctrl Pts',(-1.13227935775763,-7.83201156344688,
37.0965655322419));
#238975=CARTESIAN_POINT('Ctrl Pts',(-1.3264262933321,-7.8014807407568,37.0886821308434));
#238976=CARTESIAN_POINT('Ctrl Pts',(-1.51920704762722,-7.76375752754037,
37.0807987294449));
#238977=CARTESIAN_POINT('Ctrl Pts',(-1.71197237255739,-7.72603733353209,
37.0729159590008));
#238978=CARTESIAN_POINT('Ctrl Pts',(-1.90337139443323,-7.68112595550735,
37.0650331885567));
#238979=CARTESIAN_POINT('Ctrl Pts',(-2.09283469600871,-7.62915224223387,
37.0571504181127));
#238980=CARTESIAN_POINT('Ctrl Pts',(-2.28229847681395,-7.57717839749774,
37.0492676277299));
#238981=CARTESIAN_POINT('Ctrl Pts',(-2.46982619466817,-7.51814227264755,
37.0413848373471));
#238982=CARTESIAN_POINT('Ctrl Pts',(-2.65486217690922,-7.45222301206941,
37.0335020469643));
#238983=CARTESIAN_POINT('Ctrl Pts',(-2.83992974387146,-7.38629249940159,
37.0256179110284));
#238984=CARTESIAN_POINT('Ctrl Pts',(-3.02250440274074,-7.31347662573346,
37.0177337750925));
#238985=CARTESIAN_POINT('Ctrl Pts',(-3.20204886462847,-7.23400332240258,
37.0098496391567));
#238986=CARTESIAN_POINT('Ctrl Pts',(-3.38165416722836,-7.15450308862604,
37.0019628315904));
#238987=CARTESIAN_POINT('Ctrl Pts',(-3.55822691168626,-7.06834106985719,
36.9940760240241));
#238988=CARTESIAN_POINT('Ctrl Pts',(-3.73125266538508,-6.9757920372569,
36.9861892164578));
#238989=CARTESIAN_POINT('Ctrl Pts',(-3.90444749073451,-6.88315257061791,
36.9782947023187));
#238990=CARTESIAN_POINT('Ctrl Pts',(-4.07408809812436,-6.78411378700904,
36.9704001881795));
#238991=CARTESIAN_POINT('Ctrl Pts',(-4.23968649499488,-6.67899539033813,
36.9625056740404));
#238992=CARTESIAN_POINT('Ctrl Pts',(-4.40537750050749,-6.57381820763935,
36.9546067450021));
#238993=CARTESIAN_POINT('Ctrl Pts',(-4.56702150496516,-6.46255482837822,
36.9467078159637));
#238994=CARTESIAN_POINT('Ctrl Pts',(-4.72416186895681,-6.3455666126749,
36.9388088869254));
#238995=CARTESIAN_POINT('Ctrl Pts',(-4.88149411744783,-6.22843554236294,
36.9309003124846));
#238996=CARTESIAN_POINT('Ctrl Pts',(-5.03431147256526,-6.10556588780956,
36.9229917380439));
#238997=CARTESIAN_POINT('Ctrl Pts',(-5.18219174192037,-5.97735809116137,
36.9150831636031));
#238998=CARTESIAN_POINT('Ctrl Pts',(-5.24489373318827,-5.92299732903288,
36.9117298875529));
#238999=CARTESIAN_POINT('Ctrl Pts',(-5.3067085985598,-5.86767731612106,
36.9083766115027));
#239000=CARTESIAN_POINT('Ctrl Pts',(-5.36760627154116,-5.81143045331457,
36.9050233354525));
#239001=CARTESIAN_POINT('Ctrl Pts',(-5.52367396083747,-5.66728179411931,
36.8964296073328));
#239002=CARTESIAN_POINT('Ctrl Pts',(-5.6740275740787,-5.51675480152332,
36.887835879213));
#239003=CARTESIAN_POINT('Ctrl Pts',(-5.81816424798464,-5.36030650088904,
36.8792421510933));
#239004=CARTESIAN_POINT('Ctrl Pts',(-5.96209281342726,-5.20408408458074,
36.8706608308327));
#239005=CARTESIAN_POINT('Ctrl Pts',(-6.0998221849825,-5.04195760390072,
36.8620795105721));
#239006=CARTESIAN_POINT('Ctrl Pts',(-6.23088592796903,-4.87442115052008,
36.8534981903116));
#239007=CARTESIAN_POINT('Ctrl Pts',(-6.36761776080882,-4.69963927861393,
36.8445457552546));
#239008=CARTESIAN_POINT('Ctrl Pts',(-6.49709444095225,-4.51896928210813,
36.8355933201976));
#239009=CARTESIAN_POINT('Ctrl Pts',(-6.61882955468969,-4.33301469256294,
36.8266408851406));
#239010=CARTESIAN_POINT('Ctrl Pts',(-6.73505851645895,-4.15547094026742,
36.8180933740731));
#239011=CARTESIAN_POINT('Ctrl Pts',(-6.84423051064621,-3.97311029123179,
36.8095458630055));
#239012=CARTESIAN_POINT('Ctrl Pts',(-6.94596260802212,-3.78649236734456,
36.800998351938));
#239013=CARTESIAN_POINT('Ctrl Pts',(-7.0475383006116,-3.60016135326535,
36.7924639819702));
#239014=CARTESIAN_POINT('Ctrl Pts',(-7.1416967961109,-3.40958633864797,
36.7839296120024));
#239015=CARTESIAN_POINT('Ctrl Pts',(-7.22809886420539,-3.21535500517016,
36.7753952420347));
#239016=CARTESIAN_POINT('Ctrl Pts',(-7.31431281523246,-3.02154655773731,
36.7668794533426));
#239017=CARTESIAN_POINT('Ctrl Pts',(-7.39280393547199,-2.82409790275373,
36.7583636646506));
#239018=CARTESIAN_POINT('Ctrl Pts',(-7.46327923506166,-2.62362041071063,
36.7498478759585));
#239019=CARTESIAN_POINT('Ctrl Pts',(-7.47370377569695,-2.59396625138911,
36.7485882405149));
#239020=CARTESIAN_POINT('Ctrl Pts',(-7.48395301401652,-2.56424586810514,
36.7473286050713));
#239021=CARTESIAN_POINT('Ctrl Pts',(-7.49402608667908,-2.53446128638286,
36.7460689696277));
#239022=CARTESIAN_POINT('Ctrl Pts',(-7.55402569557346,-2.35705134263631,
36.7385660321927));
#239023=CARTESIAN_POINT('Ctrl Pts',(-7.60773975115643,-2.17745488740816,
36.7310630947577));
#239024=CARTESIAN_POINT('Ctrl Pts',(-7.65500905793486,-1.99618569350029,
36.7235601573226));
#239025=CARTESIAN_POINT('Ctrl Pts',(-7.70229117428998,-1.81486737719569,
36.7160551866559));
#239026=CARTESIAN_POINT('Ctrl Pts',(-7.74312495255439,-1.63187578218918,
36.7085502159892));
#239027=CARTESIAN_POINT('Ctrl Pts',(-7.77740159634273,-1.44773803196767,
36.7010452453225));
#239028=CARTESIAN_POINT('Ctrl Pts',(-7.81168274059985,-1.26357610475252,
36.693539289265));
#239029=CARTESIAN_POINT('Ctrl Pts',(-7.83940497754203,-1.07826809693323,
36.6860333332076));
#239030=CARTESIAN_POINT('Ctrl Pts',(-7.86051110285172,-0.892348699749605,
36.6785273771502));
#239031=CARTESIAN_POINT('Ctrl Pts',(-7.88163270239363,-0.706292993324796,
36.6710159180028));
#239032=CARTESIAN_POINT('Ctrl Pts',(-7.89612847385921,-0.519625379766348,
36.6635044588554));
#239033=CARTESIAN_POINT('Ctrl Pts',(-7.90399327063924,-0.332883429580984,
36.655992999708));
#239034=CARTESIAN_POINT('Ctrl Pts',(-7.90876131246361,-0.219670913892321,
36.6514391692177));
#239035=CARTESIAN_POINT('Ctrl Pts',(-7.911093217297,-0.106431084262574,
36.6468853387274));
#239036=CARTESIAN_POINT('Ctrl Pts',(-7.91099714850641,0.00671686857199988,
36.6423315082371));
#239037=CARTESIAN_POINT('',(-7.91099848652071,-0.00489349231630381,32.6423315082371));
#239038=CARTESIAN_POINT('Ctrl Pts',(-7.91099706278514,0.00681708184264343,
36.6450777990978));
#239039=CARTESIAN_POINT('Ctrl Pts',(-7.91070528407644,0.345416582456211,
36.6327147129114));
#239040=CARTESIAN_POINT('Ctrl Pts',(-7.88867503774943,0.68363518933523,
36.6202189618414));
#239041=CARTESIAN_POINT('Ctrl Pts',(-7.8393101641919,1.06354126535353,36.6051583824506));
#239042=CARTESIAN_POINT('Ctrl Pts',(-7.83319959704548,1.10764969224287,
36.6033937543779));
#239043=CARTESIAN_POINT('Ctrl Pts',(-7.82516509291598,1.16225036545417,
36.6011870502451));
#239044=CARTESIAN_POINT('Ctrl Pts',(-7.82359181834253,1.17279397243764,
36.6007598934203));
#239045=CARTESIAN_POINT('Ctrl Pts',(-7.82099482329918,1.18996045492925,
36.6000626940279));
#239046=CARTESIAN_POINT('Ctrl Pts',(-7.81998398707249,1.19658528818443,
36.5997932137383));
#239047=CARTESIAN_POINT('Ctrl Pts',(-7.81819033045375,1.2082412349205,36.5993183313836));
#239048=CARTESIAN_POINT('Ctrl Pts',(-7.81741106757056,1.21327289816011,
36.5991130871169));
#239049=CARTESIAN_POINT('Ctrl Pts',(-7.81582923860537,1.22342189954141,
36.598698601407));
#239050=CARTESIAN_POINT('Ctrl Pts',(-7.81502650307395,1.22853920872915,
36.5984893524356));
#239051=CARTESIAN_POINT('Ctrl Pts',(-7.81346128021241,1.23845363919506,
36.5980834414047));
#239052=CARTESIAN_POINT('Ctrl Pts',(-7.8126993992683,1.24325085575843,36.5978868069372));
#239053=CARTESIAN_POINT('Ctrl Pts',(-7.81087524324058,1.2546688398177,36.5974182393464));
#239054=CARTESIAN_POINT('Ctrl Pts',(-7.80980896897679,1.26128895607668,
36.5971461226603));
#239055=CARTESIAN_POINT('Ctrl Pts',(-7.80657916940378,1.28118050400872,
36.5963271396894));
#239056=CARTESIAN_POINT('Ctrl Pts',(-7.80439023056759,1.29444773456824,
36.5957790884124));
#239057=CARTESIAN_POINT('Ctrl Pts',(-7.77729701338445,1.45609361835273,
36.5890790050618));
#239058=CARTESIAN_POINT('Ctrl Pts',(-7.74820146872424,1.60372137993247,
36.5827132490778));
#239059=CARTESIAN_POINT('Ctrl Pts',(-7.67739188676139,1.91581287388975,
36.5688300730985));
#239060=CARTESIAN_POINT('Ctrl Pts',(-7.63455793024819,2.07995331249798,
36.5612754489659));
#239061=CARTESIAN_POINT('Ctrl Pts',(-7.56721709163401,2.30776211892767,
36.5505357530121));
#239062=CARTESIAN_POINT('Ctrl Pts',(-7.54711106335815,2.37268938563442,
36.5474452977945));
#239063=CARTESIAN_POINT('Ctrl Pts',(-7.5062612801121,2.49882744872548,36.5413918441512));
#239064=CARTESIAN_POINT('Ctrl Pts',(-7.48559901490657,2.56005943389883,
36.5384302709666));
#239065=CARTESIAN_POINT('Ctrl Pts',(-7.42557493208854,2.73099640628764,
36.5301077137671));
#239066=CARTESIAN_POINT('Ctrl Pts',(-7.38453563148447,2.84009467163069,
36.5247320885914));
#239067=CARTESIAN_POINT('Ctrl Pts',(-7.25264348142139,3.16850473520379,
36.5084111899047));
#239068=CARTESIAN_POINT('Ctrl Pts',(-7.15431598157754,3.38467532582889,
36.4974800345152));
#239069=CARTESIAN_POINT('Ctrl Pts',(-6.87964711060265,3.92287798540189,
36.4700808805751));
#239070=CARTESIAN_POINT('Ctrl Pts',(-6.69033849445937,4.23767954039783,
36.4538959396896));
#239071=CARTESIAN_POINT('Ctrl Pts',(-6.39792012662386,4.65520511985469,
36.4324424525915));
#239072=CARTESIAN_POINT('Ctrl Pts',(-6.31283878358843,4.76994610465057,
36.4265445986849));
#239073=CARTESIAN_POINT('Ctrl Pts',(-6.21309531438781,4.89711352397218,
36.4200011498997));
#239074=CARTESIAN_POINT('Ctrl Pts',(-6.20144313842409,4.9118608754035,36.4192422007314));
#239075=CARTESIAN_POINT('Ctrl Pts',(-6.18386521261576,4.93394578195421,
36.4181054288256));
#239076=CARTESIAN_POINT('Ctrl Pts',(-6.17797875491938,4.94131444573236,
36.417726108244));
#239077=CARTESIAN_POINT('Ctrl Pts',(-6.16783426400353,4.95396684888715,
36.4170747292975));
#239078=CARTESIAN_POINT('Ctrl Pts',(-6.16358259018361,4.95925566011073,
36.4168024279444));
#239079=CARTESIAN_POINT('Ctrl Pts',(-6.1548146619227,4.97013371181017,36.4162423150181));
#239080=CARTESIAN_POINT('Ctrl Pts',(-6.15029758631067,4.97572228284742,
36.4159545354244));
#239081=CARTESIAN_POINT('Ctrl Pts',(-6.1394086947008,4.98915664571703,36.4152626836935));
#239082=CARTESIAN_POINT('Ctrl Pts',(-6.13302943749608,4.99699640542645,
36.4148588983926));
#239083=CARTESIAN_POINT('Ctrl Pts',(-6.11342090119484,5.02100011653531,
36.413622432649));
#239084=CARTESIAN_POINT('Ctrl Pts',(-6.10014256949035,5.03712397360805,
36.4127916476173));
#239085=CARTESIAN_POINT('Ctrl Pts',(-5.94818684316513,5.22016147029716,
36.4033576641535));
#239086=CARTESIAN_POINT('Ctrl Pts',(-5.80275700278186,5.38135967587272,
36.3950247822911));
#239087=CARTESIAN_POINT('Ctrl Pts',(-5.14588127976912,6.05181976761474,
36.3599861980014));
#239088=CARTESIAN_POINT('Ctrl Pts',(-4.57277788374726,6.49571303085079,
36.3360812566952));
#239089=CARTESIAN_POINT('Ctrl Pts',(-3.73086370745845,6.98047578459952,
36.3019010940387));
#239090=CARTESIAN_POINT('Ctrl Pts',(-3.50849286935078,7.09484685526336,
36.2929146763334));
#239091=CARTESIAN_POINT('Ctrl Pts',(-3.2003601929441,7.23529459093938,36.2801137688988));
#239092=CARTESIAN_POINT('Ctrl Pts',(-3.11901344209155,7.27073230674187,
36.2767019812494));
#239093=CARTESIAN_POINT('Ctrl Pts',(-2.98953510491732,7.32456503420561,
36.2712015553313));
#239094=CARTESIAN_POINT('Ctrl Pts',(-2.94179175885726,7.34387051648252,
36.2691594814894));
#239095=CARTESIAN_POINT('Ctrl Pts',(-2.88252742754584,7.36716397294914,
36.2666104156077));
#239096=CARTESIAN_POINT('Ctrl Pts',(-2.87118049793392,7.37159358083965,
36.2661217223737));
#239097=CARTESIAN_POINT('Ctrl Pts',(-2.8543899213502,7.37810362748676,36.2653976770858));
#239098=CARTESIAN_POINT('Ctrl Pts',(-2.84895410211927,7.38020429831263,
36.2651631332968));
#239099=CARTESIAN_POINT('Ctrl Pts',(-2.8383888159033,7.38427383821025,36.2647069990688));
#239100=CARTESIAN_POINT('Ctrl Pts',(-2.83325960788966,7.38624337414168,
36.2644854349616));
#239101=CARTESIAN_POINT('Ctrl Pts',(-2.8226585010605,7.39030136664032,36.264027258876));
#239102=CARTESIAN_POINT('Ctrl Pts',(-2.8171863278237,7.39238909267262,36.2637906188887));
#239103=CARTESIAN_POINT('Ctrl Pts',(-2.80237120210787,7.39802247280592,
36.2631495946696));
#239104=CARTESIAN_POINT('Ctrl Pts',(-2.79302385720518,7.40155649809921,
36.2627447695621));
#239105=CARTESIAN_POINT('Ctrl Pts',(-2.75822707562884,7.41463709231251,
36.2612363913187));
#239106=CARTESIAN_POINT('Ctrl Pts',(-2.73273533494119,7.42407013571564,
36.2601286659647));
#239107=CARTESIAN_POINT('Ctrl Pts',(-2.56275942017937,7.4859744892282,36.2527266183532));
#239108=CARTESIAN_POINT('Ctrl Pts',(-2.4168244902327,7.53435508431277,36.2462962288376));
#239109=CARTESIAN_POINT('Ctrl Pts',(-2.2501326870075,7.58427556946827,36.2389246507686));
#239110=CARTESIAN_POINT('Ctrl Pts',(-2.23066531977546,7.59002406117988,
36.2380633286273));
#239111=CARTESIAN_POINT('Ctrl Pts',(-1.94716049245495,7.67255487476962,
36.2255152194321));
#239112=CARTESIAN_POINT('Ctrl Pts',(-1.67932009705048,7.73559391449341,
36.2136125196681));
#239113=CARTESIAN_POINT('Ctrl Pts',(-0.674306896117623,7.91746777695069,
36.1694908955377));
#239114=CARTESIAN_POINT('Ctrl Pts',(0.0752945901321078,7.94578121850872,
36.1381661598143));
#239115=CARTESIAN_POINT('Ctrl Pts',(0.975269774363557,7.85225137429399,
36.1012586174437));
#239116=CARTESIAN_POINT('Ctrl Pts',(1.13226772742942,7.8311540247008,36.0948222850803));
#239117=CARTESIAN_POINT('Ctrl Pts',(1.32016409661107,7.8001356336022,36.0871263490344));
#239118=CARTESIAN_POINT('Ctrl Pts',(1.35176862144557,7.79472069715811,36.0858320936758));
#239119=CARTESIAN_POINT('Ctrl Pts',(1.41261387819294,7.78391463573031,36.0833407779462));
#239120=CARTESIAN_POINT('Ctrl Pts',(1.44185885594751,7.77855051223805,36.0821435149027));
#239121=CARTESIAN_POINT('Ctrl Pts',(1.49247569249424,7.76897108963063,36.0800715763413));
#239122=CARTESIAN_POINT('Ctrl Pts',(1.51386164165528,7.76483215638587,36.0791962517859));
#239123=CARTESIAN_POINT('Ctrl Pts',(1.56167570972921,7.75537340872317,36.0772393869506));
#239124=CARTESIAN_POINT('Ctrl Pts',(1.58809429921554,7.75000672471615,36.0761582748788));
#239125=CARTESIAN_POINT('Ctrl Pts',(1.65850041301441,7.73532927117364,36.0732773020853));
#239126=CARTESIAN_POINT('Ctrl Pts',(1.70243694458549,7.72577834448097,36.0714796743983));
#239127=CARTESIAN_POINT('Ctrl Pts',(1.899000171306,7.68129119029673,36.0634376442952));
#239128=CARTESIAN_POINT('Ctrl Pts',(2.05065227578138,7.64220271131309,36.0572342714464));
#239129=CARTESIAN_POINT('Ctrl Pts',(2.56530279672973,7.49312740778367,36.0361407028324));
#239130=CARTESIAN_POINT('Ctrl Pts',(2.92150369899722,7.36155956161799,36.0214892748173));
#239131=CARTESIAN_POINT('Ctrl Pts',(3.44337623176874,7.12493015787836,35.9993411171139));
#239132=CARTESIAN_POINT('Ctrl Pts',(3.61685585972647,7.03845311696228,35.9918522997115));
#239133=CARTESIAN_POINT('Ctrl Pts',(3.906508794791,6.88052637567865,35.9789929104648));
#239134=CARTESIAN_POINT('Ctrl Pts',(4.02433036437457,6.81228437072018,35.9736566171887));
#239135=CARTESIAN_POINT('Ctrl Pts',(4.20271328177182,6.7027219634552,35.9653632212593));
#239136=CARTESIAN_POINT('Ctrl Pts',(4.26456040402482,6.66354297607204,35.9624468443415));
#239137=CARTESIAN_POINT('Ctrl Pts',(4.34186872616721,6.61305245898055,35.9587424974102));
#239138=CARTESIAN_POINT('Ctrl Pts',(4.35784524034377,6.60253524922748,35.9579737402198));
#239139=CARTESIAN_POINT('Ctrl Pts',(4.3818320997843,6.5866199032509,35.9568145392717));
#239140=CARTESIAN_POINT('Ctrl Pts',(4.389870993509,6.58126484502446,35.9564251979859));
#239141=CARTESIAN_POINT('Ctrl Pts',(4.40605915405835,6.5704383474748,35.9556394289025));
#239142=CARTESIAN_POINT('Ctrl Pts',(4.41420808517499,6.56496643762655,35.9552429891663));
#239143=CARTESIAN_POINT('Ctrl Pts',(4.43090275727621,6.55371102765095,35.9544289441032));
#239144=CARTESIAN_POINT('Ctrl Pts',(4.43944740730779,6.54792594608191,35.954011296441));
#239145=CARTESIAN_POINT('Ctrl Pts',(4.46354320839489,6.53154324601246,35.9528306526604));
#239146=CARTESIAN_POINT('Ctrl Pts',(4.47906777983703,6.52090691279368,35.9520665571161));
#239147=CARTESIAN_POINT('Ctrl Pts',(4.55966056972187,6.46526686856762,35.9480820921412));
#239148=CARTESIAN_POINT('Ctrl Pts',(4.62408819050632,6.41934484934875,35.9448365230807));
#239149=CARTESIAN_POINT('Ctrl Pts',(5.18428084240982,6.00724689531925,35.9161265688413));
#239150=CARTESIAN_POINT('Ctrl Pts',(5.63637242781823,5.58525948795938,35.8897185944934));
#239151=CARTESIAN_POINT('Ctrl Pts',(6.17641289500448,4.94810567346979,35.855077630033));
#239152=CARTESIAN_POINT('Ctrl Pts',(6.31094296593637,4.77533545081489,35.8461002761938));
#239153=CARTESIAN_POINT('Ctrl Pts',(6.4622622475926,4.56342097878544,35.8355491808253));
#239154=CARTESIAN_POINT('Ctrl Pts',(6.4861202828166,4.52944677518939,35.8338710112579));
#239155=CARTESIAN_POINT('Ctrl Pts',(6.52345037012987,4.47538836240697,35.8312214288481));
#239156=CARTESIAN_POINT('Ctrl Pts',(6.53709958358123,4.45542756257335,35.8302474870463));
#239157=CARTESIAN_POINT('Ctrl Pts',(6.56181905548895,4.41891932849473,35.8284740468403));
#239158=CARTESIAN_POINT('Ctrl Pts',(6.57291876927047,4.40239210022035,35.8276741390254));
#239159=CARTESIAN_POINT('Ctrl Pts',(6.5968268705265,4.3665014857691,35.8259433001152));
#239160=CARTESIAN_POINT('Ctrl Pts',(6.60961265409561,4.34712325015933,35.8250126878944));
#239161=CARTESIAN_POINT('Ctrl Pts',(6.64432298040021,4.29400884067751,35.8224724342672));
#239162=CARTESIAN_POINT('Ctrl Pts',(6.66607579817694,4.26016117844394,35.8208651307021));
#239163=CARTESIAN_POINT('Ctrl Pts',(6.78169813048691,4.07719735040688,35.812236493039));
#239164=CARTESIAN_POINT('Ctrl Pts',(6.87082502759339,3.92514109825721,35.8052782890374));
#239165=CARTESIAN_POINT('Ctrl Pts',(6.96672573649211,3.74823686309907,35.7973769699102));
#239166=CARTESIAN_POINT('Ctrl Pts',(6.97854604194942,3.72618333053912,35.7963952999387));
#239167=CARTESIAN_POINT('Ctrl Pts',(6.99169551014139,3.70136789216168,35.7952942750104));
#239168=CARTESIAN_POINT('Ctrl Pts',(6.99312791429543,3.69866088658637,35.7951742168448));
#239169=CARTESIAN_POINT('Ctrl Pts',(6.99607776725517,3.69307831571942,35.794926722603));
#239170=CARTESIAN_POINT('Ctrl Pts',(6.99759501600783,3.69020264531196,35.7947992878969));
#239171=CARTESIAN_POINT('Ctrl Pts',(7.00325608427099,3.67945706929135,35.7943232986429));
#239172=CARTESIAN_POINT('Ctrl Pts',(7.00738840503139,3.67158111006522,35.79397482051));
#239173=CARTESIAN_POINT('Ctrl Pts',(7.35164865905182,3.01274318125731,35.764856695746));
#239174=CARTESIAN_POINT('Ctrl Pts',(7.59949128928855,2.31757308743826,35.7371318304023));
#239175=CARTESIAN_POINT('Ctrl Pts',(7.83832611160117,1.15974337726697,35.6929232434117));
#239176=CARTESIAN_POINT('Ctrl Pts',(7.89138348015633,0.714408154638406,
35.6762316585544));
#239177=CARTESIAN_POINT('Ctrl Pts',(7.90742710246973,0.239341158786664,
35.6573115373116));
#239178=CARTESIAN_POINT('Ctrl Pts',(7.90821631719195,0.211665376319118,
35.6562051248054));
#239179=CARTESIAN_POINT('Ctrl Pts',(7.90910095356235,0.17363825722812,35.6546785923203));
#239180=CARTESIAN_POINT('Ctrl Pts',(7.90932137131331,0.163289871669249,
35.6542625337007));
#239181=CARTESIAN_POINT('Ctrl Pts',(7.90964343604327,0.146633932053922,
35.653591814127));
#239182=CARTESIAN_POINT('Ctrl Pts',(7.90975784931207,0.140326620285303,
35.6533375787019));
#239183=CARTESIAN_POINT('Ctrl Pts',(7.9099799510671,0.127218088190425,35.6528086788881));
#239184=CARTESIAN_POINT('Ctrl Pts',(7.91008641224594,0.120416853968545,
35.6525339732033));
#239185=CARTESIAN_POINT('Ctrl Pts',(7.91031128864618,0.104760419078613,
35.6519009170061));
#239186=CARTESIAN_POINT('Ctrl Pts',(7.91042360625605,0.095905148632572,
35.6515423571482));
#239187=CARTESIAN_POINT('Ctrl Pts',(7.91073366554095,0.0677289495780813,
35.6503998266645));
#239188=CARTESIAN_POINT('Ctrl Pts',(7.91087549124689,0.0484075584678235,
35.6496138939339));
#239189=CARTESIAN_POINT('Ctrl Pts',(7.91160936912533,-0.151196350409517,
35.6414677988726));
#239190=CARTESIAN_POINT('Ctrl Pts',(7.90611006295592,-0.331417862464458,
35.6338584674401));
#239191=CARTESIAN_POINT('Ctrl Pts',(7.84630317469573,-1.25483571835492,
35.5935749927134));
#239192=CARTESIAN_POINT('Ctrl Pts',(7.69335173637718,-1.98785632586977,
35.5580675828169));
#239193=CARTESIAN_POINT('Ctrl Pts',(7.35805813766003,-2.91567333815961,
35.5145506942186));
#239194=CARTESIAN_POINT('Ctrl Pts',(7.26568348756958,-3.13879380260562,
35.50416552714));
#239195=CARTESIAN_POINT('Ctrl Pts',(7.11749019147832,-3.45497880394309,
35.489617319248));
#239196=CARTESIAN_POINT('Ctrl Pts',(7.06974234676012,-3.55166010471907,
35.4851916942741));
#239197=CARTESIAN_POINT('Ctrl Pts',(7.01216272956621,-3.66248360727265,
35.480143991968));
#239198=CARTESIAN_POINT('Ctrl Pts',(7.00424452537631,-3.67760396901163,
35.479455848788));
#239199=CARTESIAN_POINT('Ctrl Pts',(6.99213954654262,-3.70053835876744,
35.4784128970207));
#239200=CARTESIAN_POINT('Ctrl Pts',(6.98798849329457,-3.70837112507276,
35.4780568434847));
#239201=CARTESIAN_POINT('Ctrl Pts',(6.98044705879823,-3.72254369302833,
35.4774128617745));
#239202=CARTESIAN_POINT('Ctrl Pts',(6.97706118731049,-3.72888587597723,
35.4771247762576));
#239203=CARTESIAN_POINT('Ctrl Pts',(6.97028074790042,-3.7415449645188,35.4765499401766));
#239204=CARTESIAN_POINT('Ctrl Pts',(6.96688622689929,-3.74786188751085,
35.4762631883492));
#239205=CARTESIAN_POINT('Ctrl Pts',(6.95732777245099,-3.76559152195833,
35.4754586240659));
#239206=CARTESIAN_POINT('Ctrl Pts',(6.95114434046665,-3.77699372565035,
35.47494149789));
#239207=CARTESIAN_POINT('Ctrl Pts',(6.92574442066891,-3.82355735052294,
35.4728308975617));
#239208=CARTESIAN_POINT('Ctrl Pts',(6.90628881316048,-3.85858801661332,
35.4712458812878));
#239209=CARTESIAN_POINT('Ctrl Pts',(6.58648689813112,-4.42423709558592,
35.4456945362196));
#239210=CARTESIAN_POINT('Ctrl Pts',(6.22605544251963,-4.91853791413004,
35.424191484825));
#239211=CARTESIAN_POINT('Ctrl Pts',(5.54496019890987,-5.65621281444071,
35.3898913364315));
#239212=CARTESIAN_POINT('Ctrl Pts',(5.25627045360818,-5.92544755955108,
35.3766914946964));
#239213=CARTESIAN_POINT('Ctrl Pts',(4.82439392239379,-6.2717255844288,35.3571269544986));
#239214=CARTESIAN_POINT('Ctrl Pts',(4.69707942914819,-6.36763375925413,
35.351375686854));
#239215=CARTESIAN_POINT('Ctrl Pts',(4.48115496048411,-6.52029247833874,
35.3415069429887));
#239216=CARTESIAN_POINT('Ctrl Pts',(4.39415213054745,-6.57923926471133,
35.3375010048448));
#239217=CARTESIAN_POINT('Ctrl Pts',(4.26270862701209,-6.66452547611605,
35.3313681142168));
#239218=CARTESIAN_POINT('Ctrl Pts',(4.21914015245588,-6.69219252665309,
35.3293223994837));
#239219=CARTESIAN_POINT('Ctrl Pts',(4.16769075057763,-6.72416204219813,
35.3268881070584));
#239220=CARTESIAN_POINT('Ctrl Pts',(4.16006849619777,-6.72888040225786,
35.3265269918238));
#239221=CARTESIAN_POINT('Ctrl Pts',(4.14840051546367,-6.73607576165551,
35.3259734572116));
#239222=CARTESIAN_POINT('Ctrl Pts',(4.14436053258067,-6.73856210769509,
35.325781661779));
#239223=CARTESIAN_POINT('Ctrl Pts',(4.13732260994436,-6.74288476699529,
35.3254472992998));
#239224=CARTESIAN_POINT('Ctrl Pts',(4.13432567424517,-6.74472272068568,
35.3253048425462));
#239225=CARTESIAN_POINT('Ctrl Pts',(4.12806855145587,-6.74855433689502,
35.3250072545488));
#239226=CARTESIAN_POINT('Ctrl Pts',(4.12480814373666,-6.75054763562258,
35.3248520988065));
#239227=CARTESIAN_POINT('Ctrl Pts',(4.11681640767235,-6.75542555077468,
35.3244715632216));
#239228=CARTESIAN_POINT('Ctrl Pts',(4.11208349665493,-6.75830755609491,
35.32424600627));
#239229=CARTESIAN_POINT('Ctrl Pts',(4.09363584923845,-6.76951430529142,
35.3233660747703));
#239230=CARTESIAN_POINT('Ctrl Pts',(4.07989911165069,-6.7778021230506,35.3227091690026));
#239231=CARTESIAN_POINT('Ctrl Pts',(3.85069589391009,-6.91513857648727,
35.3117215202549));
#239232=CARTESIAN_POINT('Ctrl Pts',(3.62924570567944,-7.03388618953717,
35.3007156549931));
#239233=CARTESIAN_POINT('Ctrl Pts',(2.86975921874841,-7.39572128763022,
35.2627369797264));
#239234=CARTESIAN_POINT('Ctrl Pts',(2.31023670295025,-7.58914336350543,
35.2345505280346));
#239235=CARTESIAN_POINT('Ctrl Pts',(1.43371657745948,-7.78609867108479,
35.1940773289123));
#239236=CARTESIAN_POINT('Ctrl Pts',(1.12935733332025,-7.83603576734698,
35.1806263670723));
#239237=CARTESIAN_POINT('Ctrl Pts',(0.71295788331513,-7.87958229016834,
35.1631645077018));
#239238=CARTESIAN_POINT('Ctrl Pts',(0.602849329554254,-7.88877050614783,
35.1586335269741));
#239239=CARTESIAN_POINT('Ctrl Pts',(0.476506946563828,-7.89665255111096,
35.1535312231086));
#239240=CARTESIAN_POINT('Ctrl Pts',(0.460429731994517,-7.89760627337691,
35.1528837340511));
#239241=CARTESIAN_POINT('Ctrl Pts',(0.43613530425295,-7.89897301460196,
35.1519079858912));
#239242=CARTESIAN_POINT('Ctrl Pts',(0.427920225573886,-7.89942231876122,
35.1515785024877));
#239243=CARTESIAN_POINT('Ctrl Pts',(0.413734661019399,-7.90017597077229,
35.1510103554901));
#239244=CARTESIAN_POINT('Ctrl Pts',(0.407764512162655,-7.90048636741614,
35.1507714879162));
#239245=CARTESIAN_POINT('Ctrl Pts',(0.395416977482603,-7.90111430024951,
35.1502779606968));
#239246=CARTESIAN_POINT('Ctrl Pts',(0.389039546091621,-7.90143088329806,
35.1500233333827));
#239247=CARTESIAN_POINT('Ctrl Pts',(0.371748224690901,-7.90226825926077,
35.1493337023921));
#239248=CARTESIAN_POINT('Ctrl Pts',(0.36083360822879,-7.90277416432851,
35.1488992014654));
#239249=CARTESIAN_POINT('Ctrl Pts',(0.320132635023746,-7.90457620622215,
35.1472819259567));
#239250=CARTESIAN_POINT('Ctrl Pts',(0.290339890298518,-7.90572657498813,
35.1461040724566));
#239251=CARTESIAN_POINT('Ctrl Pts',(-0.183792432772987,-7.92135013940513,
35.1274526735648));
#239252=CARTESIAN_POINT('Ctrl Pts',(-0.62859310451462,-7.89851235134479,
35.1113297268909));
#239253=CARTESIAN_POINT('Ctrl Pts',(-1.53153963099389,-7.77535110596137,
35.0797562554624));
#239254=CARTESIAN_POINT('Ctrl Pts',(-1.98741790875059,-7.67149589729444,
35.0644355819677));
#239255=CARTESIAN_POINT('Ctrl Pts',(-2.66568863962111,-7.45242264858109,
35.0397943035602));
#239256=CARTESIAN_POINT('Ctrl Pts',(-2.896230849264,-7.36588976150276,35.0310584726172));
#239257=CARTESIAN_POINT('Ctrl Pts',(-3.19666779003233,-7.23683483120016,
35.0187311737756));
#239258=CARTESIAN_POINT('Ctrl Pts',(-3.27048979546408,-7.20377394393731,
35.015623727536));
#239259=CARTESIAN_POINT('Ctrl Pts',(-3.3808162050088,-7.15231934167255,
35.010841528461));
#239260=CARTESIAN_POINT('Ctrl Pts',(-3.41770783065832,-7.13476441387362,
35.0092188377385));
#239261=CARTESIAN_POINT('Ctrl Pts',(-3.46163540585171,-7.11344255007217,
35.0072563825009));
#239262=CARTESIAN_POINT('Ctrl Pts',(-3.46880436200363,-7.10994942973714,
35.0069351417212));
#239263=CARTESIAN_POINT('Ctrl Pts',(-3.47988827015735,-7.10452796972739,
35.0064369522124));
#239264=CARTESIAN_POINT('Ctrl Pts',(-3.48380693615512,-7.10260721683944,
35.0062605247722));
#239265=CARTESIAN_POINT('Ctrl Pts',(-3.49071452737688,-7.09921433605655,
35.0059490113607));
#239266=CARTESIAN_POINT('Ctrl Pts',(-3.49370412388529,-7.09774355662329,
35.0058140176421));
#239267=CARTESIAN_POINT('Ctrl Pts',(-3.5000311779489,-7.09462589600445,
35.0055279618301));
#239268=CARTESIAN_POINT('Ctrl Pts',(-3.50336840323916,-7.09297854797006,
35.0053768679942));
#239269=CARTESIAN_POINT('Ctrl Pts',(-3.51280987839659,-7.08830968212789,
35.004948802898));
#239270=CARTESIAN_POINT('Ctrl Pts',(-3.51891137666305,-7.08528264179443,
35.0046714584796));
#239271=CARTESIAN_POINT('Ctrl Pts',(-3.54437500734256,-7.07260876633628,
35.003511064577));
#239272=CARTESIAN_POINT('Ctrl Pts',(-3.56370126849847,-7.06289049927954,
35.002623245603));
#239273=CARTESIAN_POINT('Ctrl Pts',(-3.88852100881482,-6.89788133903762,
34.9875847775401));
#239274=CARTESIAN_POINT('Ctrl Pts',(-4.18361746525914,-6.72299483106897,
34.9721887483753));
#239275=CARTESIAN_POINT('Ctrl Pts',(-5.03521647966954,-6.14047506005405,
34.9244906823409));
#239276=CARTESIAN_POINT('Ctrl Pts',(-5.55084173935188,-5.67866308281204,
34.8913218951509));
#239277=CARTESIAN_POINT('Ctrl Pts',(-6.20353054142754,-4.91910317391241,
34.847114686122));
#239278=CARTESIAN_POINT('Ctrl Pts',(-6.39279887307541,-4.67049468715187,
34.8338783030197));
#239279=CARTESIAN_POINT('Ctrl Pts',(-6.57808754008093,-4.39466588035967,
34.8204355997297));
#239280=CARTESIAN_POINT('Ctrl Pts',(-6.58921667738758,-4.37796156577782,
34.81962606533));
#239281=CARTESIAN_POINT('Ctrl Pts',(-6.60537072762976,-4.35351395425731,
34.8184478692966));
#239282=CARTESIAN_POINT('Ctrl Pts',(-6.6104458093076,-4.34580399952919,
34.8180772592681));
#239283=CARTESIAN_POINT('Ctrl Pts',(-6.61933032260097,-4.33225526518893,
34.8174276507688));
#239284=CARTESIAN_POINT('Ctrl Pts',(-6.62314554631107,-4.326420307271,34.8171484283016));
#239285=CARTESIAN_POINT('Ctrl Pts',(-6.63053911450104,-4.31507997197211,
34.8166068014018));
#239286=CARTESIAN_POINT('Ctrl Pts',(-6.63411832660669,-4.30957516958262,
34.8163443636169));
#239287=CARTESIAN_POINT('Ctrl Pts',(-6.64264709592539,-4.29642218032096,
34.815718440098));
#239288=CARTESIAN_POINT('Ctrl Pts',(-6.64759030920783,-4.28876987891027,
34.8153551985196));
#239289=CARTESIAN_POINT('Ctrl Pts',(-6.66249373418397,-4.26561108142173,
34.8142586447625));
#239290=CARTESIAN_POINT('Ctrl Pts',(-6.67241302042754,-4.2500782518517,
34.8135269006031));
#239291=CARTESIAN_POINT('Ctrl Pts',(-6.7730894822763,-4.09120556713317,
34.8060801099556));
#239292=CARTESIAN_POINT('Ctrl Pts',(-6.85927046892438,-3.94501166973401,
34.7995407344318));
#239293=CARTESIAN_POINT('Ctrl Pts',(-7.02716418806364,-3.63804363252641,
34.7863751107902));
#239294=CARTESIAN_POINT('Ctrl Pts',(-7.10821555084118,-3.47702080470081,
34.779772836855));
#239295=CARTESIAN_POINT('Ctrl Pts',(-7.45230308949078,-2.73100539348885,
34.7502718727135));
#239296=CARTESIAN_POINT('Ctrl Pts',(-7.64907637125781,-2.11819648010552,
34.7292064240524));
#239297=CARTESIAN_POINT('Ctrl Pts',(-7.81330498254887,-1.26089029544188,
34.6976758137546));
#239298=CARTESIAN_POINT('Ctrl Pts',(-7.84687314368932,-1.03158298422918,
34.6890136934493));
#239299=CARTESIAN_POINT('Ctrl Pts',(-7.87413990191499,-0.763712073946177,
34.6783598892406));
#239300=CARTESIAN_POINT('Ctrl Pts',(-7.87768143455745,-0.72627162633861,
34.6768601797615));
#239301=CARTESIAN_POINT('Ctrl Pts',(-7.8818854217051,-0.67817194338873,
34.6749208881759));
#239302=CARTESIAN_POINT('Ctrl Pts',(-7.88279347792796,-0.66753424522885,
34.6744912039117));
#239303=CARTESIAN_POINT('Ctrl Pts',(-7.8842200882024,-0.650412874666579,
34.6737983821548));
#239304=CARTESIAN_POINT('Ctrl Pts',(-7.88475218675746,-0.643930322195523,
34.6735357764512));
#239305=CARTESIAN_POINT('Ctrl Pts',(-7.88574915055482,-0.63159779361437,
34.6730356519341));
#239306=CARTESIAN_POINT('Ctrl Pts',(-7.8862155026584,-0.625747939483491,
34.6727981907134));
#239307=CARTESIAN_POINT('Ctrl Pts',(-7.8872621224248,-0.612432271626754,
34.6722571543863));
#239308=CARTESIAN_POINT('Ctrl Pts',(-7.88783829920551,-0.604966148034549,
34.6719534237771));
#239309=CARTESIAN_POINT('Ctrl Pts',(-7.88951901594675,-0.582776709622307,
34.6710496490344));
#239310=CARTESIAN_POINT('Ctrl Pts',(-7.89059293587748,-0.568051153424212,
34.670448461855));
#239311=CARTESIAN_POINT('Ctrl Pts',(-7.89775524617057,-0.465900514353901,
34.6662685496937));
#239312=CARTESIAN_POINT('Ctrl Pts',(-7.90243164160236,-0.378384321028612,
34.6626392711476));
#239313=CARTESIAN_POINT('Ctrl Pts',(-7.90918039501917,-0.19492018992749,
34.6549496850105));
#239314=CARTESIAN_POINT('Ctrl Pts',(-7.91096274880416,-0.0989752959457913,
34.6508818064442));
#239315=CARTESIAN_POINT('Ctrl Pts',(-7.91107275700221,0.188848524910494,
34.6385730740983));
#239316=CARTESIAN_POINT('Ctrl Pts',(-7.90416559975877,0.380656400235834,
34.6302310135188));
#239317=CARTESIAN_POINT('Ctrl Pts',(-7.8685506472537,0.871920452914543,
34.6087034270501));
#239318=CARTESIAN_POINT('Ctrl Pts',(-7.82972775036714,1.17034252646841,
34.5954787338032));
#239319=CARTESIAN_POINT('Ctrl Pts',(-7.74820065132595,1.60272043721625,
34.5763743909714));
#239320=CARTESIAN_POINT('Ctrl Pts',(-7.71877779695645,1.73890671062302,
34.5703635255649));
#239321=CARTESIAN_POINT('Ctrl Pts',(-7.60083664326615,2.22255112026571,
34.5490690659233));
#239322=CARTESIAN_POINT('Ctrl Pts',(-7.49231808227196,2.56469210752963,
34.534123361522));
#239323=CARTESIAN_POINT('Ctrl Pts',(-7.34633320136737,2.93545624937585,
34.5179843385539));
#239324=CARTESIAN_POINT('Ctrl Pts',(-7.33142549257565,2.97249309148422,
34.5163724530777));
#239325=CARTESIAN_POINT('Ctrl Pts',(-7.31022006699589,3.02404593784191,
34.5141291068849));
#239326=CARTESIAN_POINT('Ctrl Pts',(-7.30415823708213,3.03865820912228,
34.5134932865611));
#239327=CARTESIAN_POINT('Ctrl Pts',(-7.29302207540162,3.06527647961835,
34.5123351295118));
#239328=CARTESIAN_POINT('Ctrl Pts',(-7.287961828526,3.0772882991266,34.5118125258578));
#239329=CARTESIAN_POINT('Ctrl Pts',(-7.27770391914602,3.10147091021826,
34.5107604621578));
#239330=CARTESIAN_POINT('Ctrl Pts',(-7.27250535570819,3.11364127576453,
34.5102310215708));
#239331=CARTESIAN_POINT('Ctrl Pts',(-7.25972318197535,3.14335898981476,
34.5089383044952));
#239332=CARTESIAN_POINT('Ctrl Pts',(-7.25210645253976,3.16089202957714,
34.5081756843678));
#239333=CARTESIAN_POINT('Ctrl Pts',(-7.22449779041522,3.22381962951235,
34.5054388026399));
#239334=CARTESIAN_POINT('Ctrl Pts',(-7.20414246775042,3.2690537927787,34.5034718910792));
#239335=CARTESIAN_POINT('Ctrl Pts',(-7.08754882379454,3.52177278577797,
34.4924847062207));
#239336=CARTESIAN_POINT('Ctrl Pts',(-6.98277127782974,3.72520383142453,
34.483651956027));
#239337=CARTESIAN_POINT('Ctrl Pts',(-6.70768292456216,4.20679388393263,
34.4626499021831));
#239338=CARTESIAN_POINT('Ctrl Pts',(-6.52870899158561,4.47951930306538,
34.4506872206033));
#239339=CARTESIAN_POINT('Ctrl Pts',(-6.00972063840075,5.17290993479888,
34.4191427874257));
#239340=CARTESIAN_POINT('Ctrl Pts',(-5.64260555892777,5.57105305774826,
34.3998725866302));
#239341=CARTESIAN_POINT('Ctrl Pts',(-5.2164350660965,5.94756608199953,34.3772962545697));
#239342=CARTESIAN_POINT('Ctrl Pts',(-5.19492398685463,5.96636420611167,
34.3761559116807));
#239343=CARTESIAN_POINT('Ctrl Pts',(-5.16633446096287,5.99107622159623,
34.3746385933119));
#239344=CARTESIAN_POINT('Ctrl Pts',(-5.15934664326809,5.99709498582975,
34.3742675961681));
#239345=CARTESIAN_POINT('Ctrl Pts',(-5.14848061043203,6.00642109604818,
34.373690458721));
#239346=CARTESIAN_POINT('Ctrl Pts',(-5.14460968183564,6.00973694935427,
34.3734848118043));
#239347=CARTESIAN_POINT('Ctrl Pts',(-5.13689091832819,6.01633595123726,
34.3730746457925));
#239348=CARTESIAN_POINT('Ctrl Pts',(-5.13304313382562,6.01961915498458,
34.3728701301292));
#239349=CARTESIAN_POINT('Ctrl Pts',(-5.12441730400735,6.02696504300323,
34.3724115379909));
#239350=CARTESIAN_POINT('Ctrl Pts',(-5.11963757457088,6.03102573696138,
34.3721573441653));
#239351=CARTESIAN_POINT('Ctrl Pts',(-5.10569518660571,6.04284219286316,
34.3714156173279));
#239352=CARTESIAN_POINT('Ctrl Pts',(-5.09651972614669,6.05058276407319,
34.3709271769505));
#239353=CARTESIAN_POINT('Ctrl Pts',(-5.02677329272439,6.10915080374051,
34.367211687322));
#239354=CARTESIAN_POINT('Ctrl Pts',(-4.96546639655223,6.15908397527802,
34.3639277919866));
#239355=CARTESIAN_POINT('Ctrl Pts',(-4.82260776964509,6.27192001731401,
34.3562424610373));
#239356=CARTESIAN_POINT('Ctrl Pts',(-4.74055700436013,6.33416484679106,
34.3518065623045));
#239357=CARTESIAN_POINT('Ctrl Pts',(-4.55310333349143,6.47068715544381,
34.3416626361279));
#239358=CARTESIAN_POINT('Ctrl Pts',(-4.44705247423557,6.54402510220171,
34.3359172604791));
#239359=CARTESIAN_POINT('Ctrl Pts',(-3.76030904391294,6.99452808568198,
34.2988753894218));
#239360=CARTESIAN_POINT('Ctrl Pts',(-3.1339110057794,7.29671921277099,34.2661012541298));
#239361=CARTESIAN_POINT('Ctrl Pts',(-2.4009978845483,7.53826223019135,34.2322486332985));
#239362=CARTESIAN_POINT('Ctrl Pts',(-2.32544074441799,7.56191206343619,
34.2288048065048));
#239363=CARTESIAN_POINT('Ctrl Pts',(-2.02737730355157,7.65031767360384,
34.2154046424973));
#239364=CARTESIAN_POINT('Ctrl Pts',(-1.80241675960301,7.7064209923196,34.2056975034139));
#239365=CARTESIAN_POINT('Ctrl Pts',(-1.55263291173244,7.75717650079496,
34.1953564828679));
#239366=CARTESIAN_POINT('Ctrl Pts',(-1.52994111845616,7.76168386424671,
34.1944209241997));
#239367=CARTESIAN_POINT('Ctrl Pts',(-1.49791701752003,7.76789904687555,
34.1931060205783));
#239368=CARTESIAN_POINT('Ctrl Pts',(-1.488601014569,7.76968969869472,34.192724152463));
#239369=CARTESIAN_POINT('Ctrl Pts',(-1.47238266917604,7.77277682671952,
34.1920604714581));
#239370=CARTESIAN_POINT('Ctrl Pts',(-1.46548178808664,7.77408087503589,
34.1917784281484));
#239371=CARTESIAN_POINT('Ctrl Pts',(-1.45107502149182,7.77678343377511,
34.1911903466519));
#239372=CARTESIAN_POINT('Ctrl Pts',(-1.44356882723896,7.77818027145643,
34.1908843596391));
#239373=CARTESIAN_POINT('Ctrl Pts',(-1.42581032641579,7.78145838269297,
34.190161417822));
#239374=CARTESIAN_POINT('Ctrl Pts',(-1.41555628975377,7.78333026667,34.1897447490815));
#239375=CARTESIAN_POINT('Ctrl Pts',(-1.38168199248268,7.78944489595657,
34.1883708063087));
#239376=CARTESIAN_POINT('Ctrl Pts',(-1.3580460252912,7.79360044659157,34.1874161840546));
#239377=CARTESIAN_POINT('Ctrl Pts',(-0.994047170786951,7.85589062829521,
34.1727763021128));
#239378=CARTESIAN_POINT('Ctrl Pts',(-0.650240750991511,7.89179093117464,
34.1597969559625));
#239379=CARTESIAN_POINT('Ctrl Pts',(0.190528588098214,7.92424735389335,
34.1293710571656));
#239380=CARTESIAN_POINT('Ctrl Pts',(0.686931845273835,7.8967163559241,34.1125470744031));
#239381=CARTESIAN_POINT('Ctrl Pts',(1.63259166383128,7.75437875179024,34.0793509219251));
#239382=CARTESIAN_POINT('Ctrl Pts',(2.08086441694054,7.64628993356028,34.0630341684548));
#239383=CARTESIAN_POINT('Ctrl Pts',(2.54498181759764,7.49051720398846,34.0436254849891));
#239384=CARTESIAN_POINT('Ctrl Pts',(2.5727220039266,7.48103481448433,34.04245655637));
#239385=CARTESIAN_POINT('Ctrl Pts',(2.61015496918314,7.46800632938839,34.0408677353606));
#239386=CARTESIAN_POINT('Ctrl Pts',(2.61989466946123,7.46459506059157,34.0404532873622));
#239387=CARTESIAN_POINT('Ctrl Pts',(2.63520953950674,7.45919745755351,34.0397999743238));
#239388=CARTESIAN_POINT('Ctrl Pts',(2.64078922238311,7.45722390106425,34.0395616115591));
#239389=CARTESIAN_POINT('Ctrl Pts',(2.65152407730603,7.45341338030751,34.0391023718561));
#239390=CARTESIAN_POINT('Ctrl Pts',(2.65667956932722,7.45157732403126,34.0388815301399));
#239391=CARTESIAN_POINT('Ctrl Pts',(2.66882880136625,7.44723633411519,34.0383604289886));
#239392=CARTESIAN_POINT('Ctrl Pts',(2.6758209202681,7.44472689823923,34.0380599980318));
#239393=CARTESIAN_POINT('Ctrl Pts',(2.6961601773935,7.43739488674601,34.0371845637561));
#239394=CARTESIAN_POINT('Ctrl Pts',(2.7094978508953,7.43254625256531,34.0366085872982));
#239395=CARTESIAN_POINT('Ctrl Pts',(2.80456618666071,7.39769622873416,34.0324898830865));
#239396=CARTESIAN_POINT('Ctrl Pts',(2.88580824261921,7.36638385988909,34.0289002688795));
#239397=CARTESIAN_POINT('Ctrl Pts',(3.15499382992904,7.25749761817918,34.0168049709042));
#239398=CARTESIAN_POINT('Ctrl Pts',(3.34045900833821,7.17402168633489,34.0081420734133));
#239399=CARTESIAN_POINT('Ctrl Pts',(3.8280737800776,6.93153953925002,33.984745234026));
#239400=CARTESIAN_POINT('Ctrl Pts',(4.12349815824072,6.75996718491266,33.9699218826192));
#239401=CARTESIAN_POINT('Ctrl Pts',(4.96362336634729,6.19642852570688,33.9265330512412));
#239402=CARTESIAN_POINT('Ctrl Pts',(5.4706192272667,5.75375277790836,33.8988970267875));
#239403=CARTESIAN_POINT('Ctrl Pts',(5.97341324591713,5.18746622838379,33.868147655446));
#239404=CARTESIAN_POINT('Ctrl Pts',(6.03003200365184,5.12154135587622,33.864628982967));
#239405=CARTESIAN_POINT('Ctrl Pts',(6.10796387820317,5.02771602740295,33.8597058539575));
#239406=CARTESIAN_POINT('Ctrl Pts',(6.13019465424269,5.00058643576555,33.8582920184751));
#239407=CARTESIAN_POINT('Ctrl Pts',(6.16645993343334,4.95572438913711,33.855969874392));
#239408=CARTESIAN_POINT('Ctrl Pts',(6.18060009993573,4.93807804104071,33.8550604379545));
#239409=CARTESIAN_POINT('Ctrl Pts',(6.2100350099089,4.90101998598743,33.8531588436651));
#239410=CARTESIAN_POINT('Ctrl Pts',(6.22531485121378,4.88159674027004,33.8521668582874));
#239411=CARTESIAN_POINT('Ctrl Pts',(6.26154222050212,4.8350989468069,33.8498032345234));
#239412=CARTESIAN_POINT('Ctrl Pts',(6.28240554564411,4.80795937748013,33.8484325571041));
#239413=CARTESIAN_POINT('Ctrl Pts',(6.3531651268356,4.71466644131793,33.8437508988213));
#239414=CARTESIAN_POINT('Ctrl Pts',(6.40219810248842,4.64786471352681,33.8404499471088));
#239415=CARTESIAN_POINT('Ctrl Pts',(6.67390184188345,4.26524036482616,33.8218216826655));
#239416=CARTESIAN_POINT('Ctrl Pts',(6.87424867518735,3.93420342718045,33.8067889470348));
#239417=CARTESIAN_POINT('Ctrl Pts',(7.16543486055353,3.36238324148139,33.7819609615455));
#239418=CARTESIAN_POINT('Ctrl Pts',(7.27018813362744,3.12944738746237,33.7721276616706));
#239419=CARTESIAN_POINT('Ctrl Pts',(7.4453491631003,2.68343728213385,33.7534916224684));
#239420=CARTESIAN_POINT('Ctrl Pts',(7.51831423271007,2.47164040696927,33.744717833383));
#239421=CARTESIAN_POINT('Ctrl Pts',(7.5898989491045,2.23116201769167,33.734677095712));
#239422=CARTESIAN_POINT('Ctrl Pts',(7.5974696294702,2.20524493515027,33.7335939392209));
#239423=CARTESIAN_POINT('Ctrl Pts',(7.60850237886289,2.16674475890125,33.7319829535654));
#239424=CARTESIAN_POINT('Ctrl Pts',(7.61206625219226,2.15419095490056,33.7314573518577));
#239425=CARTESIAN_POINT('Ctrl Pts',(7.61834831644763,2.13185202713648,33.7305214688025));
#239426=CARTESIAN_POINT('Ctrl Pts',(7.62107876122559,2.12207036895957,33.7301114652925));
#239427=CARTESIAN_POINT('Ctrl Pts',(7.62677935013026,2.10149543439788,33.7292485964937));
#239428=CARTESIAN_POINT('Ctrl Pts',(7.62974543424081,2.09070106042789,33.7287956382194));
#239429=CARTESIAN_POINT('Ctrl Pts',(7.63755898236424,2.06202739017408,33.7275916640917));
#239430=CARTESIAN_POINT('Ctrl Pts',(7.64236653881737,2.04413743381336,33.7268396841063));
#239431=CARTESIAN_POINT('Ctrl Pts',(7.66848931408079,1.94554857884579,33.7226912053715));
#239432=CARTESIAN_POINT('Ctrl Pts',(7.68858892867833,1.8645341408897,33.7192663447152));
#239433=CARTESIAN_POINT('Ctrl Pts',(7.74657487058553,1.61390801926714,33.7086411952719));
#239434=CARTESIAN_POINT('Ctrl Pts',(7.78015706553231,1.44335566140471,33.7013695011496));
#239435=CARTESIAN_POINT('Ctrl Pts',(7.89433954600021,0.74236463259594,33.6715033267744));
#239436=CARTESIAN_POINT('Ctrl Pts',(7.92650776288397,0.205465166371491,
33.6487805333601));
#239437=CARTESIAN_POINT('Ctrl Pts',(7.89859463168227,-0.461981566028062,
33.6213452956789));
#239438=CARTESIAN_POINT('Ctrl Pts',(7.88982110678699,-0.593251939845101,
33.6159822584154));
#239439=CARTESIAN_POINT('Ctrl Pts',(7.87468374746445,-0.757904671680177,
33.6092899609492));
#239440=CARTESIAN_POINT('Ctrl Pts',(7.87137343804469,-0.791545214675656,
33.6079244379071));
#239441=CARTESIAN_POINT('Ctrl Pts',(7.86544596437889,-0.848063048106572,
33.6056330656535));
#239442=CARTESIAN_POINT('Ctrl Pts',(7.86294435175595,-0.870951937648596,
33.6047058599445));
#239443=CARTESIAN_POINT('Ctrl Pts',(7.85831997680068,-0.911618717420446,
33.6030597617128));
#239444=CARTESIAN_POINT('Ctrl Pts',(7.85623672504698,-0.929400917681355,
33.6023404116204));
#239445=CARTESIAN_POINT('Ctrl Pts',(7.85135358338842,-0.969892497417391,
33.6007033172868));
#239446=CARTESIAN_POINT('Ctrl Pts',(7.84851549640411,-0.992597126123971,
33.5997860230528));
#239447=CARTESIAN_POINT('Ctrl Pts',(7.84047361374117,-1.05474023500931,
33.5972770295948));
#239448=CARTESIAN_POINT('Ctrl Pts',(7.83507077710528,-1.09415236137217,
33.5956876252606));
#239449=CARTESIAN_POINT('Ctrl Pts',(7.80263041955931,-1.31822172075325,
33.586659953005));
#239450=CARTESIAN_POINT('Ctrl Pts',(7.76936231264552,-1.50191907340749,
33.5792934349324));
#239451=CARTESIAN_POINT('Ctrl Pts',(7.64068251027363,-2.09246990461497,
33.5555742754769));
#239452=CARTESIAN_POINT('Ctrl Pts',(7.51953730779798,-2.49299799263316,
33.5393798474998));
#239453=CARTESIAN_POINT('Ctrl Pts',(7.10139902132887,-3.56186232690879,
33.4957149213162));
#239454=CARTESIAN_POINT('Ctrl Pts',(6.74269472370014,-4.20150497822946,
33.4694002469612));
#239455=CARTESIAN_POINT('Ctrl Pts',(6.27066974870917,-4.82340275239621,
33.4388608412441));
#239456=CARTESIAN_POINT('Ctrl Pts',(6.23949773618388,-4.86365922976025,
33.4368571473716));
#239457=CARTESIAN_POINT('Ctrl Pts',(6.20040904514496,-4.91314525266786,
33.4343576677292));
#239458=CARTESIAN_POINT('Ctrl Pts',(6.19285651983289,-4.92266154880706,
33.4338753244391));
#239459=CARTESIAN_POINT('Ctrl Pts',(6.16692716522239,-4.95517881529396,
33.4322212567101));
#239460=CARTESIAN_POINT('Ctrl Pts',(6.14844398118256,-4.97809444857104,
33.4310454658514));
#239461=CARTESIAN_POINT('Ctrl Pts',(6.12289995151748,-5.00940490325771,
33.4294243208895));
#239462=CARTESIAN_POINT('Ctrl Pts',(6.115948810461,-5.01788914261537,33.4289835516718));
#239463=CARTESIAN_POINT('Ctrl Pts',(6.10486905471203,-5.03135535318596,
33.4282815566676));
#239464=CARTESIAN_POINT('Ctrl Pts',(6.10075192059565,-5.036346778003,33.4280208258888));
#239465=CARTESIAN_POINT('Ctrl Pts',(6.09274305434589,-5.04603212953442,
33.4275138692608));
#239466=CARTESIAN_POINT('Ctrl Pts',(6.08885200972897,-5.05072661920389,
33.4272676736596));
#239467=CARTESIAN_POINT('Ctrl Pts',(6.07955262351533,-5.06191983159958,
33.4266795201582));
#239468=CARTESIAN_POINT('Ctrl Pts',(6.07413928928858,-5.06841438492518,
33.4263373394146));
#239469=CARTESIAN_POINT('Ctrl Pts',(6.05794192546089,-5.08778367091741,
33.4253140352011));
#239470=CARTESIAN_POINT('Ctrl Pts',(6.0471273354793,-5.10063270953619,33.4246315154351));
#239471=CARTESIAN_POINT('Ctrl Pts',(5.95231133520476,-5.21256017194947,
33.4186530173416));
#239472=CARTESIAN_POINT('Ctrl Pts',(5.86593281889663,-5.30957862845449,
33.4132380705982));
#239473=CARTESIAN_POINT('Ctrl Pts',(5.73162163410296,-5.45315366801678,
33.4048292385462));
#239474=CARTESIAN_POINT('Ctrl Pts',(5.68543353193467,-5.50129227403439,
33.4019425125504));
#239475=CARTESIAN_POINT('Ctrl Pts',(5.35132360401761,-5.84080947781086,
33.3811305794373));
#239476=CARTESIAN_POINT('Ctrl Pts',(5.04177128796185,-6.1100113505011,33.3622403092658));
#239477=CARTESIAN_POINT('Ctrl Pts',(4.30504545794233,-6.65644130039882,
33.3202099944185));
#239478=CARTESIAN_POINT('Ctrl Pts',(3.8691073434636,-6.91894037269793,33.2972827902246));
#239479=CARTESIAN_POINT('Ctrl Pts',(3.26826795600276,-7.20606439880843,
33.2691241546764));
#239480=CARTESIAN_POINT('Ctrl Pts',(3.12353557052244,-7.26997034578886,
33.2625742465813));
#239481=CARTESIAN_POINT('Ctrl Pts',(2.95971212467584,-7.33650955533215,
33.2554156861002));
#239482=CARTESIAN_POINT('Ctrl Pts',(2.94242077799682,-7.34346160116359,
33.2546632260482));
#239483=CARTESIAN_POINT('Ctrl Pts',(2.91640742958189,-7.35381372700929,
33.2535358687255));
#239484=CARTESIAN_POINT('Ctrl Pts',(2.90770375475078,-7.35725951032207,
33.2531594524301));
#239485=CARTESIAN_POINT('Ctrl Pts',(2.89265050535234,-7.36318820451808,
33.2525097744516));
#239486=CARTESIAN_POINT('Ctrl Pts',(2.88630380784358,-7.36567836729344,
33.2522362718966));
#239487=CARTESIAN_POINT('Ctrl Pts',(2.87354018498532,-7.3706672171093,33.2516870672129));
#239488=CARTESIAN_POINT('Ctrl Pts',(2.8671231998896,-7.37316573644356,33.2514113708138));
#239489=CARTESIAN_POINT('Ctrl Pts',(2.85198900607451,-7.37903564599636,
33.2507621383588));
#239490=CARTESIAN_POINT('Ctrl Pts',(2.84326906030105,-7.38239997610226,
33.2503888370053));
#239491=CARTESIAN_POINT('Ctrl Pts',(2.8162721661635,-7.39276099202303,33.2492354725393));
#239492=CARTESIAN_POINT('Ctrl Pts',(2.79797513955904,-7.39970534038252,
33.2484571469723));
#239493=CARTESIAN_POINT('Ctrl Pts',(2.75574074133208,-7.41555569515303,
33.2466682485789));
#239494=CARTESIAN_POINT('Ctrl Pts',(2.73178557906378,-7.42441383994552,
33.2456592630205));
#239495=CARTESIAN_POINT('Ctrl Pts',(2.65222499606333,-7.45339657343536,
33.2423267522719));
#239496=CARTESIAN_POINT('Ctrl Pts',(2.59643629125748,-7.47301389554289,
33.2400199377527));
#239497=CARTESIAN_POINT('Ctrl Pts',(2.37704236793153,-7.54740725644711,
33.231061504581));
#239498=CARTESIAN_POINT('Ctrl Pts',(2.21187921263003,-7.59745228526428,
33.2245639999587));
#239499=CARTESIAN_POINT('Ctrl Pts',(1.82205695413581,-7.70177844077924,
33.2097171392192));
#239500=CARTESIAN_POINT('Ctrl Pts',(1.59639371773892,-7.75169767255701,
33.2014954827003));
#239501=CARTESIAN_POINT('Ctrl Pts',(0.565705906051421,-7.9327716704868,
33.1650180842437));
#239502=CARTESIAN_POINT('Ctrl Pts',(-0.254295056719606,-7.94882421314376,
33.1393353748658));
#239503=CARTESIAN_POINT('Ctrl Pts',(-1.10698695403444,-7.8332976042954,
33.1055569888184));
#239504=CARTESIAN_POINT('Ctrl Pts',(-1.15180529946786,-7.82683306810016,
33.1037594655331));
#239505=CARTESIAN_POINT('Ctrl Pts',(-1.20477604327292,-7.81872781773682,
33.1016064147208));
#239506=CARTESIAN_POINT('Ctrl Pts',(-1.21298522435998,-7.81745846467005,
33.1012719307997));
#239507=CARTESIAN_POINT('Ctrl Pts',(-1.22618854464113,-7.81539558974431,
33.1007326316085));
#239508=CARTESIAN_POINT('Ctrl Pts',(-1.23118396476856,-7.8146102024239,
33.1005282839324));
#239509=CARTESIAN_POINT('Ctrl Pts',(-1.24006366485248,-7.81320539717708,
33.100164492716));
#239510=CARTESIAN_POINT('Ctrl Pts',(-1.24394824663736,-7.81258787028632,
33.1000051588568));
#239511=CARTESIAN_POINT('Ctrl Pts',(-1.25204194133461,-7.81129503666675,
33.099672787477));
#239512=CARTESIAN_POINT('Ctrl Pts',(-1.25625097096794,-7.81061922452501,
33.0994997204936));
#239513=CARTESIAN_POINT('Ctrl Pts',(-1.26715663428347,-7.80885914105427,
33.0990507235426));
#239514=CARTESIAN_POINT('Ctrl Pts',(-1.27385241069877,-7.80776965950133,
33.0987744872436));
#239515=CARTESIAN_POINT('Ctrl Pts',(-1.30292340751619,-7.8030010753022,
33.0975726729861));
#239516=CARTESIAN_POINT('Ctrl Pts',(-1.32528370329718,-7.79923446590876,
33.0966418547931));
#239517=CARTESIAN_POINT('Ctrl Pts',(-1.48784462420015,-7.77113170041769,
33.0898295792521));
#239518=CARTESIAN_POINT('Ctrl Pts',(-1.62737531321939,-7.7431140196866,
33.0837382771522));
#239519=CARTESIAN_POINT('Ctrl Pts',(-1.90170194822282,-7.6802872753975,
33.0713916472817));
#239520=CARTESIAN_POINT('Ctrl Pts',(-2.03648968708364,-7.64565169904366,
33.0651449976961));
#239521=CARTESIAN_POINT('Ctrl Pts',(-2.51367454224812,-7.5095187469555,
33.0425606024695));
#239522=CARTESIAN_POINT('Ctrl Pts',(-2.8500298662681,-7.38842059827652,
33.0257893660323));
#239523=CARTESIAN_POINT('Ctrl Pts',(-3.35377556121985,-7.16752030909823,
33.0003370067336));
#239524=CARTESIAN_POINT('Ctrl Pts',(-3.52760930456423,-7.08358206223383,
32.9914835664204));
#239525=CARTESIAN_POINT('Ctrl Pts',(-4.01859904418437,-6.82393887190937,
32.966454707792));
#239526=CARTESIAN_POINT('Ctrl Pts',(-4.32699442876898,-6.63268024582356,
32.9507292024945));
#239527=CARTESIAN_POINT('Ctrl Pts',(-4.67033730848178,-6.38557225903462,
32.9333674822912));
#239528=CARTESIAN_POINT('Ctrl Pts',(-4.71905137201568,-6.34965652838012,
32.9309069465731));
#239529=CARTESIAN_POINT('Ctrl Pts',(-4.77768189135187,-6.30538217618281,
32.9279483816718));
#239530=CARTESIAN_POINT('Ctrl Pts',(-4.78799534936075,-6.29755422202991,
32.9274280596859));
#239531=CARTESIAN_POINT('Ctrl Pts',(-4.80490077869327,-6.28465740135022,
32.9265753338291));
#239532=CARTESIAN_POINT('Ctrl Pts',(-4.81150403756006,-6.27960341443356,
32.9262423010124));
#239533=CARTESIAN_POINT('Ctrl Pts',(-4.8230891819454,-6.27070740211041,
32.9256580791199));
#239534=CARTESIAN_POINT('Ctrl Pts',(-4.82807446967707,-6.2668698323316,
32.9254067013155));
#239535=CARTESIAN_POINT('Ctrl Pts',(-4.83874047572135,-6.25863908361579,
32.9248689268498));
#239536=CARTESIAN_POINT('Ctrl Pts',(-4.84441980298106,-6.25424410646158,
32.9245826070497));
#239537=CARTESIAN_POINT('Ctrl Pts',(-4.85919300959943,-6.24277958701514,
32.9238378969922));
#239538=CARTESIAN_POINT('Ctrl Pts',(-4.86827746307664,-6.2356978936318,
32.9233800254965));
#239539=CARTESIAN_POINT('Ctrl Pts',(-4.88808292797253,-6.22018908423993,
32.922381941198));
#239540=CARTESIAN_POINT('Ctrl Pts',(-4.89879769230012,-6.21175402981377,
32.92184206974));
#239541=CARTESIAN_POINT('Ctrl Pts',(-4.92998613446486,-6.18707046143443,
32.9202708581929));
#239542=CARTESIAN_POINT('Ctrl Pts',(-4.95040125335474,-6.17074806076066,
32.9192426907221));
#239543=CARTESIAN_POINT('Ctrl Pts',(-5.01960032552379,-6.11485723849423,
32.9157583943229));
#239544=CARTESIAN_POINT('Ctrl Pts',(-5.06799432180668,-6.07480866113479,
32.9133230221243));
#239545=CARTESIAN_POINT('Ctrl Pts',(-5.25347026708293,-5.91755837522489,
32.9039893140947));
#239546=CARTESIAN_POINT('Ctrl Pts',(-5.38700932170671,-5.79625590262394,
32.8972712509505));
#239547=CARTESIAN_POINT('Ctrl Pts',(-5.77102749514541,-5.42268040001609,
32.8778186098568));
#239548=CARTESIAN_POINT('Ctrl Pts',(-6.00878352578486,-5.15798010686436,
32.8656141319729));
#239549=CARTESIAN_POINT('Ctrl Pts',(-6.61625359361432,-4.38242722531574,
32.832262283388));
#239550=CARTESIAN_POINT('Ctrl Pts',(-6.94392670045103,-3.84215250971736,
32.811695866637));
#239551=CARTESIAN_POINT('Ctrl Pts',(-7.22018416563913,-3.23332405583869,
32.7854154625734));
#239552=CARTESIAN_POINT('Ctrl Pts',(-7.23604542286125,-3.19766952160274,
32.7838652966413));
#239553=CARTESIAN_POINT('Ctrl Pts',(-7.25465465695654,-3.15499027336271,
32.7819947604547));
#239554=CARTESIAN_POINT('Ctrl Pts',(-7.25765746243578,-3.14807655146799,
32.7816912813118));
#239555=CARTESIAN_POINT('Ctrl Pts',(-7.26252341858543,-3.13682910709141,
32.7811967981714));
#239556=CARTESIAN_POINT('Ctrl Pts',(-7.26439257762675,-3.13249800165178,
32.7810061981507));
#239557=CARTESIAN_POINT('Ctrl Pts',(-7.26772792946892,-3.12475048040685,
32.7806649176362));
#239558=CARTESIAN_POINT('Ctrl Pts',(-7.26919558695255,-3.12133470491688,
32.7805143362191));
#239559=CARTESIAN_POINT('Ctrl Pts',(-7.2722949430002,-3.11410732840079,
32.7801954815238));
#239560=CARTESIAN_POINT('Ctrl Pts',(-7.27392605338335,-3.11029547801546,
32.7800271693351));
#239561=CARTESIAN_POINT('Ctrl Pts',(-7.27824888268384,-3.10017117176651,
32.7795797564026));
#239562=CARTESIAN_POINT('Ctrl Pts',(-7.280935380527,-3.09385650548485,32.7793003128052));
#239563=CARTESIAN_POINT('Ctrl Pts',(-7.29325459756733,-3.06479503107134,
32.7780125054566));
#239564=CARTESIAN_POINT('Ctrl Pts',(-7.30278885919563,-3.04200691288834,
32.7769977724746));
#239565=CARTESIAN_POINT('Ctrl Pts',(-7.3742873870809,-2.86884281070689,
32.76925187874));
#239566=CARTESIAN_POINT('Ctrl Pts',(-7.43170412403889,-2.7166414463969,
32.762244000626));
#239567=CARTESIAN_POINT('Ctrl Pts',(-7.76625893670682,-1.73960537619222,
32.7165088511698));
#239568=CARTESIAN_POINT('Ctrl Pts',(-7.91041738305944,-0.875554323490879,
32.6734984947441));
#239569=CARTESIAN_POINT('Ctrl Pts',(-7.91099823792547,-0.00528010797013839,
32.6351117714718));
#239570=CARTESIAN_POINT('',(-7.90633320911253,0.0091686610735674,30.6423296657176));
#239571=CARTESIAN_POINT('Ctrl Pts',(-7.91099848652071,-0.00489349231630381,
32.6423315082371));
#239572=CARTESIAN_POINT('Ctrl Pts',(-7.91112000549778,0.191558526308438,
32.6344573356086));
#239573=CARTESIAN_POINT('Ctrl Pts',(-7.90391953153266,0.3880566740996,32.6265831629801));
#239574=CARTESIAN_POINT('Ctrl Pts',(-7.88941347252823,0.584017173968438,
32.6187089903516));
#239575=CARTESIAN_POINT('Ctrl Pts',(-7.87490737418884,0.779978205208178,
32.6108347963714));
#239576=CARTESIAN_POINT('Ctrl Pts',(-7.85309567576184,0.975401241513716,
32.6029606023911));
#239577=CARTESIAN_POINT('Ctrl Pts',(-7.82404679708957,1.16970625242088,
32.5950864084109));
#239578=CARTESIAN_POINT('Ctrl Pts',(-7.79499295893251,1.36404443682007,
32.5872108700777));
#239579=CARTESIAN_POINT('Ctrl Pts',(-7.75869952909333,1.55726387423657,
32.5793353317445));
#239580=CARTESIAN_POINT('Ctrl Pts',(-7.7152863595527,1.74879312387145,32.5714597934113));
#239581=CARTESIAN_POINT('Ctrl Pts',(-7.67185848387765,1.94038725370098,
32.5635815872534));
#239582=CARTESIAN_POINT('Ctrl Pts',(-7.62130613881505,2.1302897186296,32.5557033810955));
#239583=CARTESIAN_POINT('Ctrl Pts',(-7.56379956637718,2.31794243234649,
32.5478251749376));
#239584=CARTESIAN_POINT('Ctrl Pts',(-7.50623084948155,2.50579793290405,
32.539938455199));
#239585=CARTESIAN_POINT('Ctrl Pts',(-7.44169299101388,2.69139849450419,
32.5320517354603));
#239586=CARTESIAN_POINT('Ctrl Pts',(-7.37040551932443,2.87420310359445,
32.5241650157217));
#239587=CARTESIAN_POINT('Ctrl Pts',(-7.29907845676179,3.05710923675234,
32.516273915941));
#239588=CARTESIAN_POINT('Ctrl Pts',(-7.22099444403144,3.23721600540227,
32.5083828161603));
#239589=CARTESIAN_POINT('Ctrl Pts',(-7.13641997995962,3.41400510685517,
32.5004917163797));
#239590=CARTESIAN_POINT('Ctrl Pts',(-7.0517210203732,3.59105444584432,32.4925890007225));
#239591=CARTESIAN_POINT('Ctrl Pts',(-6.960512674969,3.76477605187092,32.4846862850654));
#239592=CARTESIAN_POINT('Ctrl Pts',(-6.86310673043122,3.93467749716667,
32.4767835694082));
#239593=CARTESIAN_POINT('Ctrl Pts',(-6.77073650364176,4.09579533353997,
32.4692894103919));
#239594=CARTESIAN_POINT('Ctrl Pts',(-6.67279342162344,4.25347781647384,
32.4617952513755));
#239595=CARTESIAN_POINT('Ctrl Pts',(-6.56957742872845,4.4073317787457,32.4543010923592));
#239596=CARTESIAN_POINT('Ctrl Pts',(-6.45121722598701,4.58375973003807,
32.4457073642394));
#239597=CARTESIAN_POINT('Ctrl Pts',(-6.32567389938808,4.75552543575751,
32.4371136361197));
#239598=CARTESIAN_POINT('Ctrl Pts',(-6.19332147061131,4.92206157637884,
32.4285199079999));
#239599=CARTESIAN_POINT('Ctrl Pts',(-6.06116013588264,5.08835726757617,
32.4199385877393));
#239600=CARTESIAN_POINT('Ctrl Pts',(-5.92220947264522,5.24943826804819,
32.4113572674787));
#239601=CARTESIAN_POINT('Ctrl Pts',(-5.77688574263718,5.40476753584419,
32.4027759472181));
#239602=CARTESIAN_POINT('Ctrl Pts',(-5.62527722371201,5.56681430023003,
32.3938235121611));
#239603=CARTESIAN_POINT('Ctrl Pts',(-5.46673230395977,5.72260058575925,
32.3848710771042));
#239604=CARTESIAN_POINT('Ctrl Pts',(-5.30177229556195,5.87155273552165,
32.3759186420472));
#239605=CARTESIAN_POINT('Ctrl Pts',(-5.14427352695691,6.01376769050683,
32.3673711309796));
#239606=CARTESIAN_POINT('Ctrl Pts',(-4.98092733305738,6.14975280576015,
32.358823619912));
#239607=CARTESIAN_POINT('Ctrl Pts',(-4.812227598083,6.27904344181885,32.3502761088444));
#239608=CARTESIAN_POINT('Ctrl Pts',(-4.64378722517104,6.40813530408562,
32.3417417388769));
#239609=CARTESIAN_POINT('Ctrl Pts',(-4.47000992688538,6.5305530686014,32.3332073689094));
#239610=CARTESIAN_POINT('Ctrl Pts',(-4.2914240497278,6.64587094558854,32.3246729989419));
#239611=CARTESIAN_POINT('Ctrl Pts',(-4.11322699487409,6.76093774917994,
32.3161572102499));
#239612=CARTESIAN_POINT('Ctrl Pts',(-3.93024246014209,6.86893537581798,
32.3076414215579));
#239613=CARTESIAN_POINT('Ctrl Pts',(-3.74302932750089,6.96948007052666,
32.299125632866));
#239614=CARTESIAN_POINT('Ctrl Pts',(-3.71533720103348,6.98435240540092,
32.2978659974221));
#239615=CARTESIAN_POINT('Ctrl Pts',(-3.68755261220178,6.99906174571603,
32.2966063619783));
#239616=CARTESIAN_POINT('Ctrl Pts',(-3.65967742918494,7.01360692613396,
32.2953467265344));
#239617=CARTESIAN_POINT('Ctrl Pts',(-3.48497466296167,7.10476626498729,
32.2874521847716));
#239618=CARTESIAN_POINT('Ctrl Pts',(-3.30687280924795,7.18938953503818,
32.2795576430088));
#239619=CARTESIAN_POINT('Ctrl Pts',(-3.12590476337168,7.2672305873923,32.271663101246));
#239620=CARTESIAN_POINT('Ctrl Pts',(-2.94489593494597,7.34508918182989,
32.2637667803871));
#239621=CARTESIAN_POINT('Ctrl Pts',(-2.76101994164748,7.41616237708621,
32.2558704595283));
#239622=CARTESIAN_POINT('Ctrl Pts',(-2.57482919663688,7.48025237596609,
32.2479741386694));
#239623=CARTESIAN_POINT('Ctrl Pts',(-2.38856579612657,7.54436738409599,
32.2400747365019));
#239624=CARTESIAN_POINT('Ctrl Pts',(-2.19998616738562,7.60149365387825,
32.2321753343345));
#239625=CARTESIAN_POINT('Ctrl Pts',(-2.00965766347297,7.65148332518894,
32.224275932167));
#239626=CARTESIAN_POINT('Ctrl Pts',(-1.81911972483716,7.70152800440836,
32.2163678376121));
#239627=CARTESIAN_POINT('Ctrl Pts',(-1.62682939779038,7.74442030912966,
32.2084597430572));
#239628=CARTESIAN_POINT('Ctrl Pts',(-1.43336521450231,7.78006331348626,
32.2005516485022));
#239629=CARTESIAN_POINT('Ctrl Pts',(-1.2397857683471,7.81572755337496,32.192638842431));
#239630=CARTESIAN_POINT('Ctrl Pts',(-1.04503140962768,7.84413383167741,
32.1847260363598));
#239631=CARTESIAN_POINT('Ctrl Pts',(-0.849685900793989,7.8652371146706,
32.1768132302886));
#239632=CARTESIAN_POINT('Ctrl Pts',(-0.654066647658819,7.88636997041156,
32.1688893357332));
#239633=CARTESIAN_POINT('Ctrl Pts',(-0.45785493019226,7.90017935774268,
32.1609654411779));
#239634=CARTESIAN_POINT('Ctrl Pts',(-0.261636014943777,7.90667234654911,
32.1530415466225));
#239635=CARTESIAN_POINT('Ctrl Pts',(-0.124208424811838,7.91121989897692,
32.1474918179849));
#239636=CARTESIAN_POINT('Ctrl Pts',(0.0132227108735123,7.91217962945228,
32.1419420893473));
#239637=CARTESIAN_POINT('Ctrl Pts',(0.150457961287746,7.90956910342688,
32.1363923607096));
#239638=CARTESIAN_POINT('Ctrl Pts',(0.351362711009467,7.90574743897704,
32.1282678676249));
#239639=CARTESIAN_POINT('Ctrl Pts',(0.552289511266152,7.89426372287408,
32.1201433745403));
#239640=CARTESIAN_POINT('Ctrl Pts',(0.75262882604898,7.87511719596605,32.1120188814556));
#239641=CARTESIAN_POINT('Ctrl Pts',(0.95279114157448,7.85598758496415,32.1039015663391));
#239642=CARTESIAN_POINT('Ctrl Pts',(1.15236668873377,7.82920869128804,32.0957842512227));
#239643=CARTESIAN_POINT('Ctrl Pts',(1.35074749380469,7.79483176264763,32.0876669361062));
#239644=CARTESIAN_POINT('Ctrl Pts',(1.54898127630582,7.76048031119182,32.0795556368366));
#239645=CARTESIAN_POINT('Ctrl Pts',(1.74602176733017,7.7185421071342,32.0714443375669));
#239646=CARTESIAN_POINT('Ctrl Pts',(1.9412670915232,7.66912009811876,32.0633330382973));
#239647=CARTESIAN_POINT('Ctrl Pts',(2.13639547986959,7.61972768881072,32.0552265970269));
#239648=CARTESIAN_POINT('Ctrl Pts',(2.32973053525365,7.56286049108492,32.0471201557565));
#239649=CARTESIAN_POINT('Ctrl Pts',(2.52068097188842,7.49867244503716,32.0390137144862));
#239650=CARTESIAN_POINT('Ctrl Pts',(2.71154416765701,7.43451372503252,32.0309109768626));
#239651=CARTESIAN_POINT('Ctrl Pts',(2.90002461400492,7.36304092931086,32.0228082392389));
#239652=CARTESIAN_POINT('Ctrl Pts',(3.08554602564457,7.28445788810869,32.0147055016153));
#239653=CARTESIAN_POINT('Ctrl Pts',(3.27274283328488,7.20516518373727,32.0065295902588));
#239654=CARTESIAN_POINT('Ctrl Pts',(3.45692658085326,7.11863327249783,31.9983536789023));
#239655=CARTESIAN_POINT('Ctrl Pts',(3.63752461481758,7.02512175528626,31.9901777675459));
#239656=CARTESIAN_POINT('Ctrl Pts',(3.81643807878664,6.93248248841233,31.9820781188964));
#239657=CARTESIAN_POINT('Ctrl Pts',(3.99183215466595,6.83299343225187,31.973978470247));
#239658=CARTESIAN_POINT('Ctrl Pts',(4.16317336433251,6.72695388259146,31.9658788215976));
#239659=CARTESIAN_POINT('Ctrl Pts',(4.3345134095745,6.62091505356946,31.9577792279929));
#239660=CARTESIAN_POINT('Ctrl Pts',(4.501800370889,6.50832598870004,31.9496796343882));
#239661=CARTESIAN_POINT('Ctrl Pts',(4.66452819305336,6.38953032203545,31.9415800407835));
#239662=CARTESIAN_POINT('Ctrl Pts',(4.82727591879314,6.27072012522794,31.9334794565008));
#239663=CARTESIAN_POINT('Ctrl Pts',(4.9854631345689,6.14570200217393,31.9253788722181));
#239664=CARTESIAN_POINT('Ctrl Pts',(5.13861498424679,6.01486134866585,31.9172782879354));
#239665=CARTESIAN_POINT('Ctrl Pts',(5.29426820851848,5.88188372138169,31.9090453996958));
#239666=CARTESIAN_POINT('Ctrl Pts',(5.44471989471052,5.74289193843662,31.9008125114562));
#239667=CARTESIAN_POINT('Ctrl Pts',(5.58950865835294,5.59833135480543,31.8925796232166));
#239668=CARTESIAN_POINT('Ctrl Pts',(5.73210667912259,5.45595806154336,31.8844713036298));
#239669=CARTESIAN_POINT('Ctrl Pts',(5.86921173082491,5.30818354979302,31.876362984043));
#239670=CARTESIAN_POINT('Ctrl Pts',(6.00042193345515,5.15546871006995,31.8682546644563));
#239671=CARTESIAN_POINT('Ctrl Pts',(6.13465582268388,4.99923461799452,31.8599594918903));
#239672=CARTESIAN_POINT('Ctrl Pts',(6.26271967295164,4.83783003424346,31.8516643193242));
#239673=CARTESIAN_POINT('Ctrl Pts',(6.38422822998997,4.671782412249,31.8433691467582));
#239674=CARTESIAN_POINT('Ctrl Pts',(6.50573678702833,4.50573479025451,31.8350739741922));
#239675=CARTESIAN_POINT('Ctrl Pts',(6.62068987352878,4.3350444414627,31.8267788016262));
#239676=CARTESIAN_POINT('Ctrl Pts',(6.72875067701665,4.16026866038096,31.8184836290601));
#239677=CARTESIAN_POINT('Ctrl Pts',(6.83072554834154,3.99533616671763,31.8106556365991));
#239678=CARTESIAN_POINT('Ctrl Pts',(6.92675804387642,3.82644917922782,31.802827644138));
#239679=CARTESIAN_POINT('Ctrl Pts',(7.01652494160159,3.65407973967219,31.794999651677));
#239680=CARTESIAN_POINT('Ctrl Pts',(7.10621602067271,3.4818558862874,31.787178270872));
#239681=CARTESIAN_POINT('Ctrl Pts',(7.18965187749445,3.30615574759313,31.779356890067));
#239682=CARTESIAN_POINT('Ctrl Pts',(7.26655298979631,3.12747959969082,31.771535509262));
#239683=CARTESIAN_POINT('Ctrl Pts',(7.34340273040609,2.9489228115192,31.7637193533173));
#239684=CARTESIAN_POINT('Ctrl Pts',(7.41372628156807,2.76739429547649,31.7559031973726));
#239685=CARTESIAN_POINT('Ctrl Pts',(7.47729035038828,2.58341828126812,31.7480870414278));
#239686=CARTESIAN_POINT('Ctrl Pts',(7.54082388279168,2.39953064982624,31.7402746403937));
#239687=CARTESIAN_POINT('Ctrl Pts',(7.59760428629726,2.21319819435234,31.7324622393596));
#239688=CARTESIAN_POINT('Ctrl Pts',(7.64744658960323,2.02496460689217,31.7246498383254));
#239689=CARTESIAN_POINT('Ctrl Pts',(7.69727432455182,1.83678603804048,31.7168397207703));
#239690=CARTESIAN_POINT('Ctrl Pts',(7.74016790974515,1.64670778446427,31.7090296032151));
#239691=CARTESIAN_POINT('Ctrl Pts',(7.77599234082576,1.45528832724622,31.7012194856599));
#239692=CARTESIAN_POINT('Ctrl Pts',(7.81181881307571,1.26385796351785,31.6934089231075));
#239693=CARTESIAN_POINT('Ctrl Pts',(7.84057525530673,1.07108658848957,31.6855983605551));
#239694=CARTESIAN_POINT('Ctrl Pts',(7.86217777683998,0.877542936478608,
31.6777877980026));
#239695=CARTESIAN_POINT('Ctrl Pts',(7.87901098135532,0.726729066351007,
31.6717016197469));
#239696=CARTESIAN_POINT('Ctrl Pts',(7.89150141216044,0.575446532133352,
31.6656154414912));
#239697=CARTESIAN_POINT('Ctrl Pts',(7.89963121182758,0.423966646234818,
31.6595292632355));
#239698=CARTESIAN_POINT('Ctrl Pts',(7.91117284628295,0.208915163791779,
31.6508888972321));
#239699=CARTESIAN_POINT('Ctrl Pts',(7.91391921597654,-0.00643163438786562,
31.6422485312288));
#239700=CARTESIAN_POINT('Ctrl Pts',(7.90790194795712,-0.221377012121736,
31.6336081652254));
#239701=CARTESIAN_POINT('Ctrl Pts',(7.90187467026881,-0.436679949474773,
31.6249534260543));
#239702=CARTESIAN_POINT('Ctrl Pts',(7.88705462113972,-0.651579901821391,
31.6162986868832));
#239703=CARTESIAN_POINT('Ctrl Pts',(7.86352535064658,-0.865384342207935,
31.6076439477121));
#239704=CARTESIAN_POINT('Ctrl Pts',(7.83926834535949,-1.08580152183831,
31.5987215268536));
#239705=CARTESIAN_POINT('Ctrl Pts',(7.80575485188671,-1.3050540693302,31.5897991059952));
#239706=CARTESIAN_POINT('Ctrl Pts',(7.76313293069965,-1.52239551375017,
31.5808766851367));
#239707=CARTESIAN_POINT('Ctrl Pts',(7.72165097984496,-1.73392392131651,
31.5721929042736));
#239708=CARTESIAN_POINT('Ctrl Pts',(7.67154163656631,-1.94364192956361,
31.5635091234104));
#239709=CARTESIAN_POINT('Ctrl Pts',(7.61299237196658,-2.150876134132,31.5548253425472));
#239710=CARTESIAN_POINT('Ctrl Pts',(7.55202960860712,-2.36665287974031,
31.5457836016911));
#239711=CARTESIAN_POINT('Ctrl Pts',(7.4819165041512,-2.57973645053514,31.536741860835));
#239712=CARTESIAN_POINT('Ctrl Pts',(7.40292104009272,-2.7893872219813,31.5277001199789));
#239713=CARTESIAN_POINT('Ctrl Pts',(7.32392557603425,-2.99903799342743,
31.5186583791228));
#239714=CARTESIAN_POINT('Ctrl Pts',(7.23604788008165,-3.20525571698875,
31.5096166382667));
#239715=CARTESIAN_POINT('Ctrl Pts',(7.13961162634878,-3.40732546506866,
31.5005748974106));
#239716=CARTESIAN_POINT('Ctrl Pts',(7.05085195984431,-3.59330991340587,
31.4922529036381));
#239717=CARTESIAN_POINT('Ctrl Pts',(6.95476663062083,-3.77593846816199,
31.4839309098656));
#239718=CARTESIAN_POINT('Ctrl Pts',(6.85162772868264,-3.9546325325556,31.4756089160932));
#239719=CARTESIAN_POINT('Ctrl Pts',(6.74858056026681,-4.13316766335924,
31.4672943240458));
#239720=CARTESIAN_POINT('Ctrl Pts',(6.63849247985562,-4.30777503239189,
31.4589797319984));
#239721=CARTESIAN_POINT('Ctrl Pts',(6.52168189619684,-4.47789975823694,
31.4506651399511));
#239722=CARTESIAN_POINT('Ctrl Pts',(6.40496808221328,-4.6478835472426,31.4423574359814));
#239723=CARTESIAN_POINT('Ctrl Pts',(6.28154304031016,-4.81339186116776,
31.4340497320117));
#239724=CARTESIAN_POINT('Ctrl Pts',(6.1517694211802,-4.97389726357836,31.425742028042));
#239725=CARTESIAN_POINT('Ctrl Pts',(6.02212673778417,-5.1342407232705,31.4174427061712));
#239726=CARTESIAN_POINT('Ctrl Pts',(5.88614844625316,-5.28959112027977,
31.4091433843005));
#239727=CARTESIAN_POINT('Ctrl Pts',(5.74423876278191,-5.43945236546417,
31.4008440624297));
#239728=CARTESIAN_POINT('Ctrl Pts',(5.60241974552068,-5.58921786417942,
31.3925500430023));
#239729=CARTESIAN_POINT('Ctrl Pts',(5.4546770957743,-5.73350099465784,31.3842560235749));
#239730=CARTESIAN_POINT('Ctrl Pts',(5.3014542838967,-5.87183987143326,31.3759620041475));
#239731=CARTESIAN_POINT('Ctrl Pts',(5.14834509435641,-6.01007616304967,
31.3676741351482));
#239732=CARTESIAN_POINT('Ctrl Pts',(4.9897640699021,-6.14237680291009,31.3593862661488));
#239733=CARTESIAN_POINT('Ctrl Pts',(4.82619078682655,-6.26831743685261,
31.3510983971494));
#239734=CARTESIAN_POINT('Ctrl Pts',(4.76383758172261,-6.31632529016147,
31.3479391086282));
#239735=CARTESIAN_POINT('Ctrl Pts',(4.70075932402139,-6.36340937113779,
31.344779820107));
#239736=CARTESIAN_POINT('Ctrl Pts',(4.63698390055644,-6.40954766781404,
31.3416205315859));
#239737=CARTESIAN_POINT('Ctrl Pts',(4.47342548012091,-6.52787392134491,
31.3335182217594));
#239738=CARTESIAN_POINT('Ctrl Pts',(4.30534816810133,-6.63992687499192,
31.325415911933));
#239739=CARTESIAN_POINT('Ctrl Pts',(4.13326606970902,-6.74537119786541,
31.3173136021066));
#239740=CARTESIAN_POINT('Ctrl Pts',(3.96114598873752,-6.85083879478879,
31.3092095039092));
#239741=CARTESIAN_POINT('Ctrl Pts',(3.78501963037437,-6.94969468511056,
31.3011054057118));
#239742=CARTESIAN_POINT('Ctrl Pts',(3.60542753985813,-7.04164847566481,
31.2930013075145));
#239743=CARTESIAN_POINT('Ctrl Pts',(3.42577328152959,-7.1336340970529,31.2848944039928));
#239744=CARTESIAN_POINT('Ctrl Pts',(3.24265118208867,-7.21871270823087,
31.2767875004711));
#239745=CARTESIAN_POINT('Ctrl Pts',(3.05662419990538,-7.29664097380108,
31.2686805969494));
#239746=CARTESIAN_POINT('Ctrl Pts',(2.87042944950575,-7.37463951888646,
31.2605663822263));
#239747=CARTESIAN_POINT('Ctrl Pts',(2.68132487568337,-7.44547470887926,
31.2524521675032));
#239748=CARTESIAN_POINT('Ctrl Pts',(2.48989240424191,-7.5089517787304,31.24433795278));
#239749=CARTESIAN_POINT('Ctrl Pts',(2.29836637358184,-7.57245987187143,
31.2362197723787));
#239750=CARTESIAN_POINT('Ctrl Pts',(2.10451048050494,-7.62860257782504,
31.2281015919773));
#239751=CARTESIAN_POINT('Ctrl Pts',(1.90892035503056,-7.67723544501209,
31.2199834115759));
#239752=CARTESIAN_POINT('Ctrl Pts',(1.71311989080711,-7.72592061226503,
31.2118565008365));
#239753=CARTESIAN_POINT('Ctrl Pts',(1.5155817785933,-7.76707973273538,31.2037295900971));
#239754=CARTESIAN_POINT('Ctrl Pts',(1.31691173377675,-7.80061949369671,
31.1956026793576));
#239755=CARTESIAN_POINT('Ctrl Pts',(1.21149661691418,-7.81841582441454,
31.1912905081588));
#239756=CARTESIAN_POINT('Ctrl Pts',(1.10576292376352,-7.83406787061175,
31.18697833696));
#239757=CARTESIAN_POINT('Ctrl Pts',(0.999801603749123,-7.84756763291281,
31.1826661657612));
#239758=CARTESIAN_POINT('Ctrl Pts',(0.803275035865438,-7.87260565576786,
31.1746683774577));
#239759=CARTESIAN_POINT('Ctrl Pts',(0.605624164434566,-7.89028031150178,
31.1666705891542));
#239760=CARTESIAN_POINT('Ctrl Pts',(0.407435973534077,-7.90050105546923,
31.1586728008507));
#239761=CARTESIAN_POINT('Ctrl Pts',(0.209409603049642,-7.91071345421169,
31.1506815427317));
#239762=CARTESIAN_POINT('Ctrl Pts',(0.0108471198679824,-7.91348405289138,
31.1426902846126));
#239763=CARTESIAN_POINT('Ctrl Pts',(-0.187658120185684,-7.90877395238531,
31.1346990264935));
#239764=CARTESIAN_POINT('Ctrl Pts',(-0.386034941989788,-7.90406689896688,
31.126712938129));
#239765=CARTESIAN_POINT('Ctrl Pts',(-0.584354261112515,-7.89188879974217,
31.1187268497645));
#239766=CARTESIAN_POINT('Ctrl Pts',(-0.78202104470825,-7.8722527960955,
31.1107407614));
#239767=CARTESIAN_POINT('Ctrl Pts',(-0.979593456904803,-7.85262616720115,
31.1027584858073));
#239768=CARTESIAN_POINT('Ctrl Pts',(-1.17651362232059,-7.82554876433088,
31.0947762102146));
#239769=CARTESIAN_POINT('Ctrl Pts',(-1.37218954246306,-7.7910857304714,
31.0867939346219));
#239770=CARTESIAN_POINT('Ctrl Pts',(-1.56780519770736,-7.75663331064774,
31.0788141174361));
#239771=CARTESIAN_POINT('Ctrl Pts',(-1.76217704252591,-7.71479985261514,
31.0708343002502));
#239772=CARTESIAN_POINT('Ctrl Pts',(-1.95472080065425,-7.66570202861353,
31.0628544830644));
#239773=CARTESIAN_POINT('Ctrl Pts',(-2.15388132751438,-7.61491695725678,
31.054600439358));
#239774=CARTESIAN_POINT('Ctrl Pts',(-2.35108552174003,-7.55635943088405,
31.0463463956517));
#239775=CARTESIAN_POINT('Ctrl Pts',(-2.54570046579419,-7.49021562696664,
31.0380923519453));
#239776=CARTESIAN_POINT('Ctrl Pts',(-2.73387510541626,-7.42626069007378,
31.0301114555788));
#239777=CARTESIAN_POINT('Ctrl Pts',(-2.91962879532448,-7.3552136682197,
31.0221305592123));
#239778=CARTESIAN_POINT('Ctrl Pts',(-3.10240674042604,-7.27729300062593,
31.0141496628458));
#239779=CARTESIAN_POINT('Ctrl Pts',(-3.28522526456568,-7.19935503364881,
31.0061669946183));
#239780=CARTESIAN_POINT('Ctrl Pts',(-3.46506641872656,-7.11454050960702,
30.9981843263909));
#239781=CARTESIAN_POINT('Ctrl Pts',(-3.64139680113664,-7.02311542954207,
30.9902016581635));
#239782=CARTESIAN_POINT('Ctrl Pts',(-3.81779343608521,-6.93165599837124,
30.9822159906116));
#239783=CARTESIAN_POINT('Ctrl Pts',(-3.99067637246239,-6.83358121347228,
30.9742303230596));
#239784=CARTESIAN_POINT('Ctrl Pts',(-4.15953782867062,-6.72920248260209,
30.9662446555077));
#239785=CARTESIAN_POINT('Ctrl Pts',(-4.32848869245094,-6.62476848601813,
30.9582547597609));
#239786=CARTESIAN_POINT('Ctrl Pts',(-4.49341354679249,-6.51402406493902,
30.9502648640141));
#239787=CARTESIAN_POINT('Ctrl Pts',(-4.65383423728175,-6.39732349439233,
30.9422749682673));
#239788=CARTESIAN_POINT('Ctrl Pts',(-4.81444495932278,-6.28048468238537,
30.9342756078293));
#239789=CARTESIAN_POINT('Ctrl Pts',(-4.97054058840902,-6.15767582334372,
30.9262762473914));
#239790=CARTESIAN_POINT('Ctrl Pts',(-5.12167568950783,-6.02929176035664,
30.9182768869534));
#239791=CARTESIAN_POINT('Ctrl Pts',(-5.27291644255949,-5.90081794967448,
30.9102719345117));
#239792=CARTESIAN_POINT('Ctrl Pts',(-5.4191895056411,-5.76676138739371,
30.9022669820701));
#239793=CARTESIAN_POINT('Ctrl Pts',(-5.56008652872081,-5.62755353534175,
30.8942620296284));
#239794=CARTESIAN_POINT('Ctrl Pts',(-5.70116743391328,-5.48816400568305,
30.8862466300705));
#239795=CARTESIAN_POINT('Ctrl Pts',(-5.83685805631752,-5.34361000062216,
30.8782312305126));
#239796=CARTESIAN_POINT('Ctrl Pts',(-5.96678975451033,-5.19435665173952,
30.8702158309548));
#239797=CARTESIAN_POINT('Ctrl Pts',(-5.99628376231048,-5.16047670175525,
30.8683963653404));
#239798=CARTESIAN_POINT('Ctrl Pts',(-6.02548120320849,-5.12635472781571,
30.866576899726));
#239799=CARTESIAN_POINT('Ctrl Pts',(-6.05437807709909,-5.09199637662302,
30.8647574341116));
#239800=CARTESIAN_POINT('Ctrl Pts',(-6.17670551434893,-4.94654918861768,
30.8570551973017));
#239801=CARTESIAN_POINT('Ctrl Pts',(-6.29402186928434,-4.79641363535212,
30.8493529604917));
#239802=CARTESIAN_POINT('Ctrl Pts',(-6.40593152587227,-4.64197827287416,
30.8416507236818));
#239803=CARTESIAN_POINT('Ctrl Pts',(-6.51769924070127,-4.48773879006967,
30.8339582560828));
#239804=CARTESIAN_POINT('Ctrl Pts',(-6.62407369436811,-4.3292106427767,
30.8262657884838));
#239805=CARTESIAN_POINT('Ctrl Pts',(-6.72469650293035,-4.16681868377739,
30.8185733208848));
#239806=CARTESIAN_POINT('Ctrl Pts',(-6.82518779454681,-4.00463897580518,
30.8108909075653));
#239807=CARTESIAN_POINT('Ctrl Pts',(-6.91994222679607,-3.83860582307059,
30.8032084942458));
#239808=CARTESIAN_POINT('Ctrl Pts',(-7.00864229111484,-3.66917623387001,
30.7955260809263));
#239809=CARTESIAN_POINT('Ctrl Pts',(-7.09727541642188,-3.49987450758978,
30.7878494652707));
#239810=CARTESIAN_POINT('Ctrl Pts',(-7.17986309738958,-3.32718176537128,
30.780172849615));
#239811=CARTESIAN_POINT('Ctrl Pts',(-7.25613136580334,-3.15158350709686,
30.7724962339594));
#239812=CARTESIAN_POINT('Ctrl Pts',(-7.33235639994112,-2.97608479039744,
30.7648239699552));
#239813=CARTESIAN_POINT('Ctrl Pts',(-7.4022690064745,-2.79768416835301,
30.757151705951));
#239814=CARTESIAN_POINT('Ctrl Pts',(-7.46564138949943,-2.61689121734033,
30.7494794419468));
#239815=CARTESIAN_POINT('Ctrl Pts',(-7.52898973886491,-2.43616683115052,
30.7418100876104));
#239816=CARTESIAN_POINT('Ctrl Pts',(-7.58580268248014,-2.25305226534913,
30.7341407332739));
#239817=CARTESIAN_POINT('Ctrl Pts',(-7.63590076839302,-2.06807651097701,
30.7264713789375));
#239818=CARTESIAN_POINT('Ctrl Pts',(-7.68599815158814,-1.88310335122995,
30.7188021321778));
#239819=CARTESIAN_POINT('Ctrl Pts',(-7.72938075927012,-1.69626940359867,
30.7111328854182));
#239820=CARTESIAN_POINT('Ctrl Pts',(-7.76591910683258,-1.50811850533461,
30.7034636386586));
#239821=CARTESIAN_POINT('Ctrl Pts',(-7.80245646267677,-1.31997271383357,
30.6957946000564));
#239822=CARTESIAN_POINT('Ctrl Pts',(-7.8321498640609,-1.13051040154314,
30.6881255614543));
#239823=CARTESIAN_POINT('Ctrl Pts',(-7.85492108572722,-0.940284923306739,
30.6804565228522));
#239824=CARTESIAN_POINT('Ctrl Pts',(-7.87770307273813,-0.749969513890778,
30.6727838586281));
#239825=CARTESIAN_POINT('Ctrl Pts',(-7.89355630427478,-0.558890580240167,
30.6651111944039));
#239826=CARTESIAN_POINT('Ctrl Pts',(-7.90245446202203,-0.367606414073757,
30.6574385301797));
#239827=CARTESIAN_POINT('Ctrl Pts',(-7.90829444408519,-0.242064011802341,
30.6524028561988));
#239828=CARTESIAN_POINT('Ctrl Pts',(-7.91113961314385,-0.11643327993427,
30.6473671822179));
#239829=CARTESIAN_POINT('Ctrl Pts',(-7.91099473374487,0.00912812472498083,
30.642331508237));
#239830=CARTESIAN_POINT('',(-7.92501410677892,-0.00343255291858106,28.642331508237));
#239831=CARTESIAN_POINT('Ctrl Pts',(-7.90633320911253,0.0091686610735674,
30.6423296657176));
#239832=CARTESIAN_POINT('Ctrl Pts',(-7.91336746977763,0.802296278954325,
30.6105026779658));
#239833=CARTESIAN_POINT('Ctrl Pts',(-7.44150124210029,4.22685934970188,
30.4727061129974));
#239834=CARTESIAN_POINT('Ctrl Pts',(-3.57838467684135,7.95204539560988,
30.2819247594207));
#239835=CARTESIAN_POINT('Ctrl Pts',(1.84890739308732,8.01686568835012,30.0699856049879));
#239836=CARTESIAN_POINT('Ctrl Pts',(6.72176570595038,5.56614746243324,29.8580464505547));
#239837=CARTESIAN_POINT('Ctrl Pts',(8.72502379230441,-0.0138583237335466,
29.6461072961218));
#239838=CARTESIAN_POINT('Ctrl Pts',(6.53049753724295,-5.01776157217315,
29.4341681416887));
#239839=CARTESIAN_POINT('Ctrl Pts',(3.34789267773502,-7.54374501772842,
29.2752137758639));
#239840=CARTESIAN_POINT('Ctrl Pts',(-0.668896594127559,-8.20840108341964,
29.1162594100393));
#239841=CARTESIAN_POINT('Ctrl Pts',(-5.81251715635164,-6.4871340805156,
28.9052986541635));
#239842=CARTESIAN_POINT('Ctrl Pts',(-7.92294825320361,-2.5984269134878,
28.7473226868962));
#239843=CARTESIAN_POINT('Ctrl Pts',(-7.92501410677892,-0.00343255291858106,
28.642331508237));
#239844=CARTESIAN_POINT('',(-7.911,-2.20934381900406E-13,24.642331508237));
#239845=CARTESIAN_POINT('Ctrl Pts',(-7.91099939187997,-0.00310188245014101,
28.6503955877365));
#239846=CARTESIAN_POINT('Ctrl Pts',(-7.91100069750583,0.000227968239218608,
28.6502613150879));
#239847=CARTESIAN_POINT('Ctrl Pts',(-7.91099990075837,0.0035578146403876,
28.6501269234759));
#239848=CARTESIAN_POINT('Ctrl Pts',(-7.91099372550141,0.0106505683740582,
28.6498404065745));
#239849=CARTESIAN_POINT('Ctrl Pts',(-7.91098776457367,0.0144134729226244,
28.649688248172));
#239850=CARTESIAN_POINT('Ctrl Pts',(-7.91097028956923,0.0220191955620909,
28.6493803880486));
#239851=CARTESIAN_POINT('Ctrl Pts',(-7.91095866021637,0.0258620120489566,
28.6492246797667));
#239852=CARTESIAN_POINT('Ctrl Pts',(-7.91092980626999,0.0335463549286024,
28.6489129912032));
#239853=CARTESIAN_POINT('Ctrl Pts',(-7.91091258351208,0.0373878802412497,
28.6487570110713));
#239854=CARTESIAN_POINT('Ctrl Pts',(-7.91086330887346,0.0468424567040657,
28.6483727184439));
#239855=CARTESIAN_POINT('Ctrl Pts',(-7.91082808115321,0.0524554816042823,
28.6481442216884));
#239856=CARTESIAN_POINT('Ctrl Pts',(-7.91066499237011,0.0746734089642306,
28.6472383724012));
#239857=CARTESIAN_POINT('Ctrl Pts',(-7.91049082701998,0.0912775885031617,
28.6465582915197));
#239858=CARTESIAN_POINT('Ctrl Pts',(-7.90633603099997,0.395923944287139,
28.6340247013134));
#239859=CARTESIAN_POINT('Ctrl Pts',(-7.88667765437492,0.68351374242021,
28.6212865391246));
#239860=CARTESIAN_POINT('Ctrl Pts',(-7.79356480844529,1.43768529788987,
28.5867060414319));
#239861=CARTESIAN_POINT('Ctrl Pts',(-7.69395872348861,1.89989813937944,
28.564366966351));
#239862=CARTESIAN_POINT('Ctrl Pts',(-7.47299284271564,2.61001391222413,
28.530404667836));
#239863=CARTESIAN_POINT('Ctrl Pts',(-7.37891251455699,2.86521594782051,
28.5182597392054));
#239864=CARTESIAN_POINT('Ctrl Pts',(-7.19952949890077,3.28396891102393,
28.4986198111455));
#239865=CARTESIAN_POINT('Ctrl Pts',(-7.12131958148455,3.45028848752972,
28.4908970527732));
#239866=CARTESIAN_POINT('Ctrl Pts',(-7.01483659852659,3.65765294324576,
28.4813718555403));
#239867=CARTESIAN_POINT('Ctrl Pts',(-6.99187752568665,3.70135196213072,
28.4793704019216));
#239868=CARTESIAN_POINT('Ctrl Pts',(-6.96249123284194,3.75603494812408,
28.476872918965));
#239869=CARTESIAN_POINT('Ctrl Pts',(-6.95644479396315,3.76722159284334,
28.4763623751625));
#239870=CARTESIAN_POINT('Ctrl Pts',(-6.94679207522196,3.78497781054658,
28.4755525886451));
#239871=CARTESIAN_POINT('Ctrl Pts',(-6.9432034003835,3.79155689711105,28.4752526719134));
#239872=CARTESIAN_POINT('Ctrl Pts',(-6.93643485370573,3.80392378079822,
28.4746891485306));
#239873=CARTESIAN_POINT('Ctrl Pts',(-6.93325707452281,3.80971271209514,
28.47442546189));
#239874=CARTESIAN_POINT('Ctrl Pts',(-6.92610911208688,3.82269552560342,
28.4738343116019));
#239875=CARTESIAN_POINT('Ctrl Pts',(-6.92213495926728,3.82988722030503,
28.4735070010147));
#239876=CARTESIAN_POINT('Ctrl Pts',(-6.91202366550362,3.84811763914778,
28.4726776711487));
#239877=CARTESIAN_POINT('Ctrl Pts',(-6.90587126957856,3.85914790170746,
28.4721762402867));
#239878=CARTESIAN_POINT('Ctrl Pts',(-6.87205461697762,3.91943592520712,
28.4694374658705));
#239879=CARTESIAN_POINT('Ctrl Pts',(-6.84388939434853,3.96841161772681,
28.4672195356385));
#239880=CARTESIAN_POINT('Ctrl Pts',(-6.31375551053387,4.86781301471811,
28.4266031238632));
#239881=CARTESIAN_POINT('Ctrl Pts',(-5.65763198849656,5.6169207411592,28.3961955078519));
#239882=CARTESIAN_POINT('Ctrl Pts',(-4.77148256975636,6.31158599312026,
28.3560885092999));
#239883=CARTESIAN_POINT('Ctrl Pts',(-4.66008259963891,6.39427798120392,
28.351033313477));
#239884=CARTESIAN_POINT('Ctrl Pts',(-4.47982046028401,6.5208728543024,28.34273272976));
#239885=CARTESIAN_POINT('Ctrl Pts',(-4.41235100523158,6.5667139369484,28.3396001284843));
#239886=CARTESIAN_POINT('Ctrl Pts',(-4.32160497183233,6.62633998329858,
28.3353352864027));
#239887=CARTESIAN_POINT('Ctrl Pts',(-4.29894738683064,6.64106184566675,
28.3342662304549));
#239888=CARTESIAN_POINT('Ctrl Pts',(-4.26619511427759,6.66210492949661,
28.3327141437806));
#239889=CARTESIAN_POINT('Ctrl Pts',(-4.25616066497755,6.66852001838038,
28.332237719767));
#239890=CARTESIAN_POINT('Ctrl Pts',(-4.24060053424063,6.67841828388974,
28.331497479866));
#239891=CARTESIAN_POINT('Ctrl Pts',(-4.23508492323408,6.68191734145765,
28.3312348027027));
#239892=CARTESIAN_POINT('Ctrl Pts',(-4.22477576473722,6.68843949326119,
28.3307432938459));
#239893=CARTESIAN_POINT('Ctrl Pts',(-4.21998328506552,6.69146427855042,
28.3305145844437));
#239894=CARTESIAN_POINT('Ctrl Pts',(-4.21225805610636,6.69632847559487,
28.3301455592729));
#239895=CARTESIAN_POINT('Ctrl Pts',(-4.20932736072825,6.69817110519297,
28.3300054810382));
#239896=CARTESIAN_POINT('Ctrl Pts',(-4.20321049616838,6.70201138966755,
28.3297129436406));
#239897=CARTESIAN_POINT('Ctrl Pts',(-4.20002411095955,6.70400869701049,
28.3295604594732));
#239898=CARTESIAN_POINT('Ctrl Pts',(-4.19265385197047,6.70862124597143,
28.3292075365407));
#239899=CARTESIAN_POINT('Ctrl Pts',(-4.18846895727958,6.71123484449945,
28.3290069803148));
#239900=CARTESIAN_POINT('Ctrl Pts',(-4.17502757636155,6.71961194097316,
28.3283623000814));
#239901=CARTESIAN_POINT('Ctrl Pts',(-4.16576165487082,6.72536019355585,
28.3279170975541));
#239902=CARTESIAN_POINT('Ctrl Pts',(-4.08255166408519,6.77674281183797,
28.3239122518502));
#239903=CARTESIAN_POINT('Ctrl Pts',(-4.00787495439204,6.82117353949541,
28.3202698307919));
#239904=CARTESIAN_POINT('Ctrl Pts',(-3.68396626654726,7.00673566293631,
28.3043184548576));
#239905=CARTESIAN_POINT('Ctrl Pts',(-3.42791732057716,7.13549647419334,
28.2913323050295));
#239906=CARTESIAN_POINT('Ctrl Pts',(-3.02332581642951,7.31214607335183,
28.2708728029163));
#239907=CARTESIAN_POINT('Ctrl Pts',(-2.87938443717211,7.37001513697177,
28.2636040263249));
#239908=CARTESIAN_POINT('Ctrl Pts',(-2.69194493070265,7.43904203987247,
28.2542205246128));
#239909=CARTESIAN_POINT('Ctrl Pts',(-2.64992268633678,7.45411455049617,
28.2521219780601));
#239910=CARTESIAN_POINT('Ctrl Pts',(-2.55986721172178,7.48555781691231,
28.247638093769));
#239911=CARTESIAN_POINT('Ctrl Pts',(-2.51179939178841,7.50182376477952,
28.2452528610037));
#239912=CARTESIAN_POINT('Ctrl Pts',(-2.40804899529163,7.53582349122296,
28.2401251985732));
#239913=CARTESIAN_POINT('Ctrl Pts',(-2.35231952535368,7.55340509646899,
28.2373835780121));
#239914=CARTESIAN_POINT('Ctrl Pts',(-2.23080304102068,7.590265984888,28.2314377861457));
#239915=CARTESIAN_POINT('Ctrl Pts',(-2.16494959868516,7.60931096031932,
28.2282359341819));
#239916=CARTESIAN_POINT('Ctrl Pts',(-2.01905068141353,7.64945792625273,
28.2211938629336));
#239917=CARTESIAN_POINT('Ctrl Pts',(-1.93890422734654,7.6701644660312,28.2173594750244));
#239918=CARTESIAN_POINT('Ctrl Pts',(-1.57656917404609,7.75773462790546,
28.2001981828266));
#239919=CARTESIAN_POINT('Ctrl Pts',(-1.29114372364367,7.81031283063245,
28.1871621729531));
#239920=CARTESIAN_POINT('Ctrl Pts',(-0.845272370409721,7.86732907906118,
28.1677053388765));
#239921=CARTESIAN_POINT('Ctrl Pts',(-0.686507738654565,7.88277003708533,
28.1609501978895));
#239922=CARTESIAN_POINT('Ctrl Pts',(-0.445220905622621,7.89889101406481,
28.1509437282521));
#239923=CARTESIAN_POINT('Ctrl Pts',(-0.362981612354909,7.90309722944765,
28.1475785115249));
#239924=CARTESIAN_POINT('Ctrl Pts',(-0.265322876925592,7.90656443802844,
28.1436342470231));
#239925=CARTESIAN_POINT('Ctrl Pts',(-0.249954281716337,7.90706521424777,
28.1430150582266));
#239926=CARTESIAN_POINT('Ctrl Pts',(-0.226305744770819,7.90776677097254,
28.1420645967093));
#239927=CARTESIAN_POINT('Ctrl Pts',(-0.218026827105749,7.90799936124399,
28.1417322949427));
#239928=CARTESIAN_POINT('Ctrl Pts',(-0.202942505682139,7.90839943860257,
28.1411276282901));
#239929=CARTESIAN_POINT('Ctrl Pts',(-0.196137227451665,7.90857114334941,
28.1408551273204));
#239930=CARTESIAN_POINT('Ctrl Pts',(-0.181315439582044,7.90892597063747,
28.1402622615986));
#239931=CARTESIAN_POINT('Ctrl Pts',(-0.173298851774147,7.90910568940206,
28.1399420070591));
#239932=CARTESIAN_POINT('Ctrl Pts',(-0.151489154864978,7.90956145189505,
28.1390718297102));
#239933=CARTESIAN_POINT('Ctrl Pts',(-0.137695544958028,7.90981360493365,
28.1385226779377));
#239934=CARTESIAN_POINT('Ctrl Pts',(-0.0720454124986548,7.91084193694461,
28.1359146394308));
#239935=CARTESIAN_POINT('Ctrl Pts',(-0.0201821841223189,7.91114426013311,
28.1338710242911));
#239936=CARTESIAN_POINT('Ctrl Pts',(0.889310074192833,7.90750201682776,
28.0983136759724));
#239937=CARTESIAN_POINT('Ctrl Pts',(1.74055375587961,7.76465212691922,28.0702090047863));
#239938=CARTESIAN_POINT('Ctrl Pts',(2.87982968575234,7.37633129990284,28.0277447212724));
#239939=CARTESIAN_POINT('Ctrl Pts',(3.19971383537684,7.24330910870905,28.0150769246642));
#239940=CARTESIAN_POINT('Ctrl Pts',(3.52884280033714,7.08036987832201,28.000421018349));
#239941=CARTESIAN_POINT('Ctrl Pts',(3.5477762884037,7.07090181794877,27.9995727016386));
#239942=CARTESIAN_POINT('Ctrl Pts',(3.57431102841773,7.05749919770662,27.9983766604006));
#239943=CARTESIAN_POINT('Ctrl Pts',(3.58194434888166,7.05362806889196,27.9980317579995));
#239944=CARTESIAN_POINT('Ctrl Pts',(3.59495913966229,7.04700123019173,27.9974422916614));
#239945=CARTESIAN_POINT('Ctrl Pts',(3.60034377055346,7.0442517195044,27.997197998491));
#239946=CARTESIAN_POINT('Ctrl Pts',(3.61058757890795,7.0390061924101,27.9967324720837));
#239947=CARTESIAN_POINT('Ctrl Pts',(3.61544733526907,7.03651130941019,27.9965112877436));
#239948=CARTESIAN_POINT('Ctrl Pts',(3.62754904745606,7.03028273220812,27.9959596693016));
#239949=CARTESIAN_POINT('Ctrl Pts',(3.63478781743424,7.02654288452659,27.9956289734115));
#239950=CARTESIAN_POINT('Ctrl Pts',(3.65842088096235,7.01428677469717,27.9945469285674));
#239951=CARTESIAN_POINT('Ctrl Pts',(3.67479105506096,7.00572430192148,27.9937936496346));
#239952=CARTESIAN_POINT('Ctrl Pts',(3.88328972352501,6.89573653676422,27.9841525100428));
#239953=CARTESIAN_POINT('Ctrl Pts',(4.07118341144484,6.78649975393642,27.9749558601663));
#239954=CARTESIAN_POINT('Ctrl Pts',(4.30261350486665,6.63887921920449,27.9631400393756));
#239955=CARTESIAN_POINT('Ctrl Pts',(4.35055670117626,6.60756056031079,27.960664578983));
#239956=CARTESIAN_POINT('Ctrl Pts',(4.55366275659396,6.47171362983408,27.9500676087089));
#239957=CARTESIAN_POINT('Ctrl Pts',(4.70543037963849,6.36222017369908,27.9418736171299));
#239958=CARTESIAN_POINT('Ctrl Pts',(4.99867963181355,6.13441700950387,27.9256026940386));
#239959=CARTESIAN_POINT('Ctrl Pts',(5.14019499050633,6.01633331953407,27.9175307793291));
#239960=CARTESIAN_POINT('Ctrl Pts',(5.38352493741036,5.79843526414609,27.9033205736802));
#239961=CARTESIAN_POINT('Ctrl Pts',(5.48700882673113,5.70060764310326,27.8971619471324));
#239962=CARTESIAN_POINT('Ctrl Pts',(5.83170193321483,5.35666803760051,27.8762779111186));
#239963=CARTESIAN_POINT('Ctrl Pts',(6.05945537562609,5.09761339391123,27.8618454937884));
#239964=CARTESIAN_POINT('Ctrl Pts',(6.30974284918697,4.77235775333514,27.8451284060405));
#239965=CARTESIAN_POINT('Ctrl Pts',(6.34923124628318,4.71969448759089,27.8424616701445));
#239966=CARTESIAN_POINT('Ctrl Pts',(6.40085069594386,4.64903233855344,27.8389346455726));
#239967=CARTESIAN_POINT('Ctrl Pts',(6.41357127967324,4.63146788422882,27.8380620939076));
#239968=CARTESIAN_POINT('Ctrl Pts',(6.4342586784555,4.6026542625308,27.8366375130033));
#239969=CARTESIAN_POINT('Ctrl Pts',(6.44226857953668,4.59143621889701,27.8360845528981));
#239970=CARTESIAN_POINT('Ctrl Pts',(6.45768930546228,4.56971935430552,27.8350173152911));
#239971=CARTESIAN_POINT('Ctrl Pts',(6.46510394679604,4.55922330022064,27.8345029554047));
#239972=CARTESIAN_POINT('Ctrl Pts',(6.48211518649803,4.53501750364098,27.8333200830842));
#239973=CARTESIAN_POINT('Ctrl Pts',(6.49169393295344,4.52129527157791,27.8326519664111));
#239974=CARTESIAN_POINT('Ctrl Pts',(6.52133881547096,4.47853845602889,27.8305777998808));
#239975=CARTESIAN_POINT('Ctrl Pts',(6.54125431669742,4.44939980640473,27.8291751185168));
#239976=CARTESIAN_POINT('Ctrl Pts',(6.72601630461986,4.17515018047701,27.8160741977128));
#239977=CARTESIAN_POINT('Ctrl Pts',(6.87721269275172,3.92111378965817,27.8047042179514));
#239978=CARTESIAN_POINT('Ctrl Pts',(7.23137641049123,3.24226353805426,27.7759364261887));
#239979=CARTESIAN_POINT('Ctrl Pts',(7.41128504969639,2.80676536531833,27.7590609056798));
#239980=CARTESIAN_POINT('Ctrl Pts',(7.6103324652913,2.16928357363508,27.7346436666831));
#239981=CARTESIAN_POINT('Ctrl Pts',(7.66212917370045,1.97856616625083,27.727360824489));
#239982=CARTESIAN_POINT('Ctrl Pts',(7.73347120397359,1.67073959523631,27.7154092046737));
#239983=CARTESIAN_POINT('Ctrl Pts',(7.75761585171015,1.55478050873955,27.710862680265));
#239984=CARTESIAN_POINT('Ctrl Pts',(7.7896233363017,1.38166895679634,27.7039578000215));
#239985=CARTESIAN_POINT('Ctrl Pts',(7.7994795879539,1.3248995266088,27.7016747728488));
#239986=CARTESIAN_POINT('Ctrl Pts',(7.81051183161563,1.25696127301639,27.6989152843981));
#239987=CARTESIAN_POINT('Ctrl Pts',(7.81228546354891,1.24589026315899,27.6984647424382));
#239988=CARTESIAN_POINT('Ctrl Pts',(7.8149880761139,1.22878786235243,27.6977673663296));
#239989=CARTESIAN_POINT('Ctrl Pts',(7.81593362837821,1.22275907559367,27.6975212683163));
#239990=CARTESIAN_POINT('Ctrl Pts',(7.81757444252269,1.21221767136442,27.6970904906555));
#239991=CARTESIAN_POINT('Ctrl Pts',(7.81827277608412,1.20770552940837,27.6969059493699));
#239992=CARTESIAN_POINT('Ctrl Pts',(7.81982717575409,1.19760423881393,27.6964924752013));
#239993=CARTESIAN_POINT('Ctrl Pts',(7.82068115612301,1.19201477570479,27.6962634476173));
#239994=CARTESIAN_POINT('Ctrl Pts',(7.82292447625388,1.17722563820278,27.6956568316467));
#239995=CARTESIAN_POINT('Ctrl Pts',(7.82430357745864,1.16802443940177,27.6952787723308));
#239996=CARTESIAN_POINT('Ctrl Pts',(7.8301579471061,1.12848912754554,27.6936514842474));
#239997=CARTESIAN_POINT('Ctrl Pts',(7.83447303613741,1.09813177915668,27.6923947362356));
#239998=CARTESIAN_POINT('Ctrl Pts',(7.90005308046722,0.616692937639541,
27.6723391194829));
#239999=CARTESIAN_POINT('Ctrl Pts',(7.92244177925405,0.161212538544038,
27.6516666678638));
#240000=CARTESIAN_POINT('Ctrl Pts',(7.88794912182902,-0.767502434094909,
27.6089087074514));
#240001=CARTESIAN_POINT('Ctrl Pts',(7.82777272970739,-1.23888115495861,
27.586914023236));
#240002=CARTESIAN_POINT('Ctrl Pts',(7.70578328661029,-1.79260254353746,
27.561801987866));
#240003=CARTESIAN_POINT('Ctrl Pts',(7.6842413581143,-1.88280517663804,27.5577321030192));
#240004=CARTESIAN_POINT('Ctrl Pts',(7.61629433043974,-2.14669424541121,
27.5458953573642));
#240005=CARTESIAN_POINT('Ctrl Pts',(7.56554840994925,-2.31920633322945,
27.5382481571461));
#240006=CARTESIAN_POINT('Ctrl Pts',(7.47872827294973,-2.58104149531858,
27.5267894275504));
#240007=CARTESIAN_POINT('Ctrl Pts',(7.44683034956438,-2.67167931200832,
27.5228503468896));
#240008=CARTESIAN_POINT('Ctrl Pts',(7.40734466260113,-2.77767095780826,
27.518274687283));
#240009=CARTESIAN_POINT('Ctrl Pts',(7.40134923865544,-2.79360705046267,
27.5175875461814));
#240010=CARTESIAN_POINT('Ctrl Pts',(7.39208419796691,-2.81799473472111,
27.5165372208217));
#240011=CARTESIAN_POINT('Ctrl Pts',(7.38885144732317,-2.82646022523184,
27.5161728590177));
#240012=CARTESIAN_POINT('Ctrl Pts',(7.38292997659567,-2.84188698729883,
27.5155092913804));
#240013=CARTESIAN_POINT('Ctrl Pts',(7.38024594061698,-2.84885003892416,
27.5152099360156));
#240014=CARTESIAN_POINT('Ctrl Pts',(7.37442223215794,-2.86389471028146,
27.514563465398));
#240015=CARTESIAN_POINT('Ctrl Pts',(7.37127911684671,-2.87197499150922,
27.5142164610236));
#240016=CARTESIAN_POINT('Ctrl Pts',(7.36272382273786,-2.89386226936205,
27.5132770731304));
#240017=CARTESIAN_POINT('Ctrl Pts',(7.35728608196858,-2.90765927078222,
27.5126855112933));
#240018=CARTESIAN_POINT('Ctrl Pts',(7.33154433578997,-2.97243840514617,
27.5099107843658));
#240019=CARTESIAN_POINT('Ctrl Pts',(7.31074879325445,-3.02322421407497,
27.5077434782227));
#240020=CARTESIAN_POINT('Ctrl Pts',(6.9476543563465,-3.88429474074423,27.4711220894172));
#240021=CARTESIAN_POINT('Ctrl Pts',(6.47315210377507,-4.63205170740908,
27.4420193411361));
#240022=CARTESIAN_POINT('Ctrl Pts',(5.61792701522823,-5.58417432911609,
27.397134420406));
#240023=CARTESIAN_POINT('Ctrl Pts',(5.32826474102179,-5.86120416465559,
27.3826192214403));
#240024=CARTESIAN_POINT('Ctrl Pts',(5.00548171015029,-6.12612227622994,
27.3659543503292));
#240025=CARTESIAN_POINT('Ctrl Pts',(4.99205054272018,-6.1370719945937,27.3652605393221));
#240026=CARTESIAN_POINT('Ctrl Pts',(4.97232073780811,-6.15304903479525,
27.3642409358957));
#240027=CARTESIAN_POINT('Ctrl Pts',(4.96605016825652,-6.15811104722852,
27.3639168207194));
#240028=CARTESIAN_POINT('Ctrl Pts',(4.95508593623094,-6.16693445263731,
27.3633500037873));
#240029=CARTESIAN_POINT('Ctrl Pts',(4.95039569180073,-6.17070009584951,
27.3631075026071));
#240030=CARTESIAN_POINT('Ctrl Pts',(4.94070029229818,-6.17846604553034,
27.3626061636518));
#240031=CARTESIAN_POINT('Ctrl Pts',(4.93569456348985,-6.18246562705647,
27.3623472926453));
#240032=CARTESIAN_POINT('Ctrl Pts',(4.92304151301149,-6.19255026388212,
27.3616928757877));
#240033=CARTESIAN_POINT('Ctrl Pts',(4.91538777538602,-6.19862722916318,
27.3612969639971));
#240034=CARTESIAN_POINT('Ctrl Pts',(4.88651731079452,-6.22146289674119,
27.3598033866403));
#240035=CARTESIAN_POINT('Ctrl Pts',(4.86522610182895,-6.23812687928477,
27.3587015707564));
#240036=CARTESIAN_POINT('Ctrl Pts',(4.7235934993176,-6.3478122585053,27.3513719085748));
#240037=CARTESIAN_POINT('Ctrl Pts',(4.60067922769253,-6.43745322224898,
27.3450107756092));
#240038=CARTESIAN_POINT('Ctrl Pts',(3.9360669171789,-6.89339211330293,27.3108767433396));
#240039=CARTESIAN_POINT('Ctrl Pts',(3.35307889087473,-7.19502786354673,
27.2821516336935));
#240040=CARTESIAN_POINT('Ctrl Pts',(2.26597366979905,-7.59632626646408,
27.2333002017464));
#240041=CARTESIAN_POINT('Ctrl Pts',(1.77669114644166,-7.72542560950767,
27.2126610815678));
#240042=CARTESIAN_POINT('Ctrl Pts',(1.21024481498384,-7.8181841746075,27.1893957300751));
#240043=CARTESIAN_POINT('Ctrl Pts',(1.14190591260103,-7.82845752778553,
27.1866013212568));
#240044=CARTESIAN_POINT('Ctrl Pts',(1.04195581519104,-7.84214632516268,
27.1825324351451));
#240045=CARTESIAN_POINT('Ctrl Pts',(1.0104449481947,-7.84626866229335,27.1812522692178));
#240046=CARTESIAN_POINT('Ctrl Pts',(0.954781625108807,-7.85320980754346,
27.1789954539141));
#240047=CARTESIAN_POINT('Ctrl Pts',(0.930639433645672,-7.85610733641379,
27.1780181473124));
#240048=CARTESIAN_POINT('Ctrl Pts',(0.883385639279105,-7.86155782626504,
27.1761081845053));
#240049=CARTESIAN_POINT('Ctrl Pts',(0.860275379822527,-7.86412028885816,
27.1751754544352));
#240050=CARTESIAN_POINT('Ctrl Pts',(0.79753688709894,-7.87079686016875,
27.1726469927131));
#240051=CARTESIAN_POINT('Ctrl Pts',(0.757888261979526,-7.87471356304108,
27.171053053983));
#240052=CARTESIAN_POINT('Ctrl Pts',(0.605608998775533,-7.88859578560043,
27.1649459215727));
#240053=CARTESIAN_POINT('Ctrl Pts',(0.492798413333528,-7.89644577318701,
27.1604527576214));
#240054=CARTESIAN_POINT('Ctrl Pts',(0.302136363620833,-7.90561124475939,
27.1529038368206));
#240055=CARTESIAN_POINT('Ctrl Pts',(0.224363953506112,-7.90820058383713,
27.1498371403737));
#240056=CARTESIAN_POINT('Ctrl Pts',(-0.513661300400068,-7.92187618780069,
27.1208349444013));
#240057=CARTESIAN_POINT('Ctrl Pts',(-1.17280383165529,-7.85139858238789,
27.0958899741146));
#240058=CARTESIAN_POINT('Ctrl Pts',(-1.90840247602796,-7.67795765219672,
27.066060416114));
#240059=CARTESIAN_POINT('Ctrl Pts',(-2.00091005091787,-7.65437079275459,
27.0622678420703));
#240060=CARTESIAN_POINT('Ctrl Pts',(-2.11304730774199,-7.62360712828126,
27.0576056288537));
#240061=CARTESIAN_POINT('Ctrl Pts',(-2.13310584498613,-7.61801903512717,
27.056769127253));
#240062=CARTESIAN_POINT('Ctrl Pts',(-2.16445974210661,-7.60915063350176,
27.0554573841175));
#240063=CARTESIAN_POINT('Ctrl Pts',(-2.17577028932236,-7.60592420324783,
27.0549833328181));
#240064=CARTESIAN_POINT('Ctrl Pts',(-2.19676285101964,-7.59988523779251,
27.0541018532935));
#240065=CARTESIAN_POINT('Ctrl Pts',(-2.20644677106315,-7.59707939256954,
27.0536945783104));
#240066=CARTESIAN_POINT('Ctrl Pts',(-2.22784103102108,-7.59083620477417,
27.0527933419118));
#240067=CARTESIAN_POINT('Ctrl Pts',(-2.23954882583235,-7.5873902629724,
27.0522991798805));
#240068=CARTESIAN_POINT('Ctrl Pts',(-2.27333823279566,-7.57736004352931,
27.0508701217227));
#240069=CARTESIAN_POINT('Ctrl Pts',(-2.29539894767959,-7.57070641398238,
27.04993351194));
#240070=CARTESIAN_POINT('Ctrl Pts',(-2.47229480477882,-7.51650940813083,
27.0423951007361));
#240071=CARTESIAN_POINT('Ctrl Pts',(-2.62566279256396,-7.46431832394128,
27.0356873226902));
#240072=CARTESIAN_POINT('Ctrl Pts',(-3.22788148345043,-7.23852530562619,
27.0088253168393));
#240073=CARTESIAN_POINT('Ctrl Pts',(-3.66209650357547,-7.02883565103473,
26.9883448860614));
#240074=CARTESIAN_POINT('Ctrl Pts',(-4.22296367476717,-6.69182120773536,
26.9610970086187));
#240075=CARTESIAN_POINT('Ctrl Pts',(-4.36839439778994,-6.59780459234992,
26.9539441038624));
#240076=CARTESIAN_POINT('Ctrl Pts',(-4.59960920893525,-6.43733239431023,
26.9424241406506));
#240077=CARTESIAN_POINT('Ctrl Pts',(-4.68731619086642,-6.37375247603161,
26.9380175595952));
#240078=CARTESIAN_POINT('Ctrl Pts',(-4.80065776835905,-6.28798454442269,
26.9322697292135));
#240079=CARTESIAN_POINT('Ctrl Pts',(-4.82749367379495,-6.26740532304475,
26.9309047760873));
#240080=CARTESIAN_POINT('Ctrl Pts',(-4.87123570090996,-6.23341394281793,
26.9286730362737));
#240081=CARTESIAN_POINT('Ctrl Pts',(-4.8882203086831,-6.22010360474032,
26.9278047513385));
#240082=CARTESIAN_POINT('Ctrl Pts',(-4.92101901566706,-6.19418291149676,
26.9261245897198));
#240083=CARTESIAN_POINT('Ctrl Pts',(-4.93683962822205,-6.18158107459217,
26.9253125950674));
#240084=CARTESIAN_POINT('Ctrl Pts',(-4.97333466322978,-6.15228165452778,
26.9234357721402));
#240085=CARTESIAN_POINT('Ctrl Pts',(-4.99397364343534,-6.13554027647342,
26.922371598295));
#240086=CARTESIAN_POINT('Ctrl Pts',(-5.06074754575701,-6.08081625645618,
26.9189192799987));
#240087=CARTESIAN_POINT('Ctrl Pts',(-5.10653670357011,-6.04241466888241,
26.9165372834474));
#240088=CARTESIAN_POINT('Ctrl Pts',(-5.48073507461986,-5.72129727413463,
26.8969392517743));
#240089=CARTESIAN_POINT('Ctrl Pts',(-5.78585522984609,-5.41254083981036,
26.8800300446694));
#240090=CARTESIAN_POINT('Ctrl Pts',(-6.11997531801542,-5.01371911638406,
26.859991588568));
#240091=CARTESIAN_POINT('Ctrl Pts',(-6.17469694995096,-4.94616973211665,
26.8566566265284));
#240092=CARTESIAN_POINT('Ctrl Pts',(-6.55640491701762,-4.45877318992151,
26.8329965411742));
#240093=CARTESIAN_POINT('Ctrl Pts',(-6.84140072411021,-4.00778435727092,
26.8133260798258));
#240094=CARTESIAN_POINT('Ctrl Pts',(-7.18377333489709,-3.32151283187578,
26.7844826260153));
#240095=CARTESIAN_POINT('Ctrl Pts',(-7.27917941520453,-3.1068613735164,
26.7755791547357));
#240096=CARTESIAN_POINT('Ctrl Pts',(-7.40058591975522,-2.79728532262134,
26.7626154389189));
#240097=CARTESIAN_POINT('Ctrl Pts',(-7.43458566182813,-2.70562606258487,
26.7587617960729));
#240098=CARTESIAN_POINT('Ctrl Pts',(-7.47208565803646,-2.59848138100245,
26.7542198530485));
#240099=CARTESIAN_POINT('Ctrl Pts',(-7.47724938449326,-2.58358495248393,
26.7535875511159));
#240100=CARTESIAN_POINT('Ctrl Pts',(-7.48504434582995,-2.56087876614334,
26.7526223759556));
#240101=CARTESIAN_POINT('Ctrl Pts',(-7.48770797918858,-2.553080126387,26.7522906313868));
#240102=CARTESIAN_POINT('Ctrl Pts',(-7.49251902831954,-2.53892194944552,
26.7516878934578));
#240103=CARTESIAN_POINT('Ctrl Pts',(-7.49467054710605,-2.53256380869944,
26.751417046023));
#240104=CARTESIAN_POINT('Ctrl Pts',(-7.49927832456228,-2.51888966964696,
26.7508341692596));
#240105=CARTESIAN_POINT('Ctrl Pts',(-7.50173197396476,-2.51157280352617,
26.7505220462804));
#240106=CARTESIAN_POINT('Ctrl Pts',(-7.50829264793326,-2.49191326541878,
26.7496827613901));
#240107=CARTESIAN_POINT('Ctrl Pts',(-7.51237993343311,-2.47956406304294,
26.7491548766488));
#240108=CARTESIAN_POINT('Ctrl Pts',(-7.53087234844916,-2.42322619320042,
26.7467433192638));
#240109=CARTESIAN_POINT('Ctrl Pts',(-7.5449215185686,-2.37912224858076,
26.7448462473919));
#240110=CARTESIAN_POINT('Ctrl Pts',(-7.79195640446019,-1.57941559712661,
26.7102474342051));
#240111=CARTESIAN_POINT('Ctrl Pts',(-7.91071778081479,-0.793331051394151,
26.6724337110449));
#240112=CARTESIAN_POINT('Ctrl Pts',(-7.91115323352253,0.428571442726039,
26.6176012636813));
#240113=CARTESIAN_POINT('Ctrl Pts',(-7.87602182063576,0.859285952645077,
26.5989630286065));
#240114=CARTESIAN_POINT('Ctrl Pts',(-7.8013956521794,1.31260341219004,26.5803038022687));
#240115=CARTESIAN_POINT('Ctrl Pts',(-7.796710534783,1.3401517441448,26.5791734450176));
#240116=CARTESIAN_POINT('Ctrl Pts',(-7.79014045727208,1.37758260871179,
26.577642393961));
#240117=CARTESIAN_POINT('Ctrl Pts',(-7.7883824932134,1.38748705514272,26.5772377261131));
#240118=CARTESIAN_POINT('Ctrl Pts',(-7.78536810985002,1.40428397343252,
26.5765522244372));
#240119=CARTESIAN_POINT('Ctrl Pts',(-7.78412141900727,1.41117816678409,
26.57627108558));
#240120=CARTESIAN_POINT('Ctrl Pts',(-7.78170024028225,1.4244664382731,26.5757296268643));
#240121=CARTESIAN_POINT('Ctrl Pts',(-7.78052702603791,1.4308607412084,26.5754692672213));
#240122=CARTESIAN_POINT('Ctrl Pts',(-7.77773672550261,1.44596365213746,
26.5748547619746));
#240123=CARTESIAN_POINT('Ctrl Pts',(-7.77611289134087,1.45467101308581,
26.5745008290344));
#240124=CARTESIAN_POINT('Ctrl Pts',(-7.77132358543822,1.48011515408911,
26.5734676074171));
#240125=CARTESIAN_POINT('Ctrl Pts',(-7.76811866960463,1.49684450712406,
26.5727895627329));
#240126=CARTESIAN_POINT('Ctrl Pts',(-7.74440299081455,1.6185103149424,26.5678677109966));
#240127=CARTESIAN_POINT('Ctrl Pts',(-7.7218202765575,1.72303396548536,26.5636898858591));
#240128=CARTESIAN_POINT('Ctrl Pts',(-7.64260808230237,2.05674095974465,
26.5504972332984));
#240129=CARTESIAN_POINT('Ctrl Pts',(-7.57783716017767,2.28386416534251,
26.541744589189));
#240130=CARTESIAN_POINT('Ctrl Pts',(-7.29347674395331,3.13464536068801,
26.509439043966));
#240131=CARTESIAN_POINT('Ctrl Pts',(-7.0062335019558,3.73275205311661,26.4879507496564));
#240132=CARTESIAN_POINT('Ctrl Pts',(-6.49866984652717,4.51963317915568,
26.4551303542329));
#240133=CARTESIAN_POINT('Ctrl Pts',(-6.33738410007175,4.74313564605484,
26.4451699102142));
#240134=CARTESIAN_POINT('Ctrl Pts',(-6.1203941954405,5.0129545588054,26.431761006296));
#240135=CARTESIAN_POINT('Ctrl Pts',(-6.07526472610776,5.06755330212035,
26.4289716620884));
#240136=CARTESIAN_POINT('Ctrl Pts',(-6.02252159938466,5.12964597027968,
26.4257022383939));
#240137=CARTESIAN_POINT('Ctrl Pts',(-6.0156174334469,5.13774085448112,26.4252740818744));
#240138=CARTESIAN_POINT('Ctrl Pts',(-6.00542409335878,5.14964346107971,
26.4246416419693));
#240139=CARTESIAN_POINT('Ctrl Pts',(-6.00214755812901,5.15346204095446,
26.4244383046035));
#240140=CARTESIAN_POINT('Ctrl Pts',(-5.99630559980613,5.16025731876955,
26.4240756726765));
#240141=CARTESIAN_POINT('Ctrl Pts',(-5.99374159486631,5.16323523927039,
26.4239164853653));
#240142=CARTESIAN_POINT('Ctrl Pts',(-5.98838367736504,5.16944873343351,
26.4235837713961));
#240143=CARTESIAN_POINT('Ctrl Pts',(-5.98558935970127,5.17268395437235,
26.4234102138374));
#240144=CARTESIAN_POINT('Ctrl Pts',(-5.97831889980753,5.18108780884048,
26.4229585384681));
#240145=CARTESIAN_POINT('Ctrl Pts',(-5.97383868510563,5.18625289727279,
26.4226801073904));
#240146=CARTESIAN_POINT('Ctrl Pts',(-5.95413400648279,5.20891034676229,
26.4214550601818));
#240147=CARTESIAN_POINT('Ctrl Pts',(-5.93883967053494,5.22634117666884,
26.4205029479036));
#240148=CARTESIAN_POINT('Ctrl Pts',(-5.82563916825739,5.35421636913377,
26.4134484972194));
#240149=CARTESIAN_POINT('Ctrl Pts',(-5.72474082912931,5.46196321994297,
26.4071206215268));
#240150=CARTESIAN_POINT('Ctrl Pts',(-5.35545475970595,5.83483650152617,
26.384051665594));
#240151=CARTESIAN_POINT('Ctrl Pts',(-5.07119699638799,6.08351455379554,
26.366480565096));
#240152=CARTESIAN_POINT('Ctrl Pts',(-4.62748775459407,6.41890386143699,
26.3406119496773));
#240153=CARTESIAN_POINT('Ctrl Pts',(-4.48104928751347,6.52197583467332,
26.3322947385368));
#240154=CARTESIAN_POINT('Ctrl Pts',(-4.13640591247933,6.74746441238821,
26.3133645062173));
#240155=CARTESIAN_POINT('Ctrl Pts',(-3.9360333499996,6.86627854841027,26.3028240628792));
#240156=CARTESIAN_POINT('Ctrl Pts',(-3.64585238949148,7.02146280099603,
26.28832383032));
#240157=CARTESIAN_POINT('Ctrl Pts',(-3.56017993803925,7.06528832928464,
26.2841321990931));
#240158=CARTESIAN_POINT('Ctrl Pts',(-3.28468301116491,7.19993421645528,
26.2709448387543));
#240159=CARTESIAN_POINT('Ctrl Pts',(-3.09201949013388,7.28475259347493,
26.2621591220722));
#240160=CARTESIAN_POINT('Ctrl Pts',(-2.87698347807668,7.36934957183451,
26.2528226897495));
#240161=CARTESIAN_POINT('Ctrl Pts',(-2.85774597391413,7.37683095933883,
26.2519914478159));
#240162=CARTESIAN_POINT('Ctrl Pts',(-2.83062494197478,7.38725620541511,
26.2508251683409));
#240163=CARTESIAN_POINT('Ctrl Pts',(-2.82276574945083,7.39026287292216,
26.2504878620272));
#240164=CARTESIAN_POINT('Ctrl Pts',(-2.80909707415674,7.39546707157249,
26.2499023648688));
#240165=CARTESIAN_POINT('Ctrl Pts',(-2.80328978017355,7.39767030810257,
26.2496539682316));
#240166=CARTESIAN_POINT('Ctrl Pts',(-2.79118048021438,7.4022481639531,26.2491367599536));
#240167=CARTESIAN_POINT('Ctrl Pts',(-2.78487802287419,7.40462158060136,
26.2488679918123));
#240168=CARTESIAN_POINT('Ctrl Pts',(-2.76999458486316,7.41020478363784,
26.2482342770542));
#240169=CARTESIAN_POINT('Ctrl Pts',(-2.7614110349545,7.41340772063927,26.2478695773413));
#240170=CARTESIAN_POINT('Ctrl Pts',(-2.7331826597784,7.42388526217052,26.2466727410348));
#240171=CARTESIAN_POINT('Ctrl Pts',(-2.71351442084337,7.43109677872282,
26.245842873794));
#240172=CARTESIAN_POINT('Ctrl Pts',(-2.33321914023445,7.56882391637849,
26.2298740519594));
#240173=CARTESIAN_POINT('Ctrl Pts',(-1.96358772280067,7.6730289495587,26.2157282373308));
#240174=CARTESIAN_POINT('Ctrl Pts',(-1.10543592251756,7.84884663629935,
26.1848831318124));
#240175=CARTESIAN_POINT('Ctrl Pts',(-0.614898182543244,7.90242192526621,
26.1686941642928));
#240176=CARTESIAN_POINT('Ctrl Pts',(0.270674092557271,7.9161436271238,26.1383674843764));
#240177=CARTESIAN_POINT('Ctrl Pts',(0.663780681655991,7.89290336375354,
26.1244810596426));
#240178=CARTESIAN_POINT('Ctrl Pts',(1.07782696147844,7.83727079501794,26.1079073636825));
#240179=CARTESIAN_POINT('Ctrl Pts',(1.10215822685561,7.83388611670848,26.1069261417326));
#240180=CARTESIAN_POINT('Ctrl Pts',(1.13347515830392,7.82938088928804,26.1056533618288));
#240181=CARTESIAN_POINT('Ctrl Pts',(1.14047587960559,7.82836418490359,26.1053682049606));
#240182=CARTESIAN_POINT('Ctrl Pts',(1.15119111929889,7.82679334795556,26.1049307621782));
#240183=CARTESIAN_POINT('Ctrl Pts',(1.15490663674343,7.82624595607969,26.1047788973489));
#240184=CARTESIAN_POINT('Ctrl Pts',(1.16191463398962,7.82520839748316,26.1044921185943));
#240185=CARTESIAN_POINT('Ctrl Pts',(1.16520719882351,7.82471879778873,26.1043572398327));
#240186=CARTESIAN_POINT('Ctrl Pts',(1.17276523294139,7.82359005260197,26.1040473041234));
#240187=CARTESIAN_POINT('Ctrl Pts',(1.17703048652175,7.82294949724309,26.1038721603524));
#240188=CARTESIAN_POINT('Ctrl Pts',(1.18882107218922,7.82116892725666,26.1033873544864));
#240189=CARTESIAN_POINT('Ctrl Pts',(1.19634526829126,7.82002154271879,26.1030772420138));
#240190=CARTESIAN_POINT('Ctrl Pts',(1.23699814748896,7.81376223249415,26.1013978062007));
#240191=CARTESIAN_POINT('Ctrl Pts',(1.27009527117754,7.80845071555044,26.1000164646679));
#240192=CARTESIAN_POINT('Ctrl Pts',(1.77675059669189,7.7238348624857,26.0786661570943));
#240193=CARTESIAN_POINT('Ctrl Pts',(2.2421162159693,7.60179529812355,26.0563598131128));
#240194=CARTESIAN_POINT('Ctrl Pts',(3.09447293763029,7.29314924779506,26.0138061286022));
#240195=CARTESIAN_POINT('Ctrl Pts',(3.48308121579645,7.11575536627994,25.9936815251743));
#240196=CARTESIAN_POINT('Ctrl Pts',(4.01138527105143,6.8208926187245,25.9663143425586));
#240197=CARTESIAN_POINT('Ctrl Pts',(4.16427924726478,6.72863816026076,25.9583855005607));
#240198=CARTESIAN_POINT('Ctrl Pts',(4.51625888036789,6.49966074398804,25.9401587881319));
#240199=CARTESIAN_POINT('Ctrl Pts',(4.71247010742161,6.3588382451958,25.9300219980779));
#240200=CARTESIAN_POINT('Ctrl Pts',(4.91928730015014,6.19556466398832,25.9193502384425));
#240201=CARTESIAN_POINT('Ctrl Pts',(4.93656956896215,6.18180313085005,25.9184585274147));
#240202=CARTESIAN_POINT('Ctrl Pts',(4.96071364762451,6.16241185512859,25.9172127881281));
#240203=CARTESIAN_POINT('Ctrl Pts',(4.96762389100698,6.15684274966645,25.9168562490253));
#240204=CARTESIAN_POINT('Ctrl Pts',(4.97958242596478,6.14717188405658,25.9162392386036));
#240205=CARTESIAN_POINT('Ctrl Pts',(4.98463505079739,6.14307550985348,25.9159785439694));
#240206=CARTESIAN_POINT('Ctrl Pts',(4.99512108339739,6.13455258989415,25.9154375048495));
#240207=CARTESIAN_POINT('Ctrl Pts',(5.00055367419677,6.1301250450378,25.9151572022822));
#240208=CARTESIAN_POINT('Ctrl Pts',(5.01330222177585,6.11970679400144,25.9144994146451));
#240209=CARTESIAN_POINT('Ctrl Pts',(5.02061334293253,6.11371017247318,25.9141221764823));
#240210=CARTESIAN_POINT('Ctrl Pts',(5.04434985878454,6.09417006001401,25.912897392132));
#240211=CARTESIAN_POINT('Ctrl Pts',(5.06073140497371,6.08057331788893,25.9120520698406));
#240212=CARTESIAN_POINT('Ctrl Pts',(5.38637643554274,5.80805921374848,25.895246213873));
#240213=CARTESIAN_POINT('Ctrl Pts',(5.6754623561066,5.5259184381252,25.8803370786886));
#240214=CARTESIAN_POINT('Ctrl Pts',(6.27011228381404,4.84942489064089,25.8483637678578));
#240215=CARTESIAN_POINT('Ctrl Pts',(6.56247372882423,4.44580122646084,25.8316935546056));
#240216=CARTESIAN_POINT('Ctrl Pts',(6.91781220683121,3.84301683863817,25.8069848401363));
#240217=CARTESIAN_POINT('Ctrl Pts',(7.01388183108026,3.66474540948979,25.7996869988365));
#240218=CARTESIAN_POINT('Ctrl Pts',(7.13427751659233,3.41921785981841,25.7894099858113));
#240219=CARTESIAN_POINT('Ctrl Pts',(7.16468960440114,3.35502442328154,25.7867027369443));
#240220=CARTESIAN_POINT('Ctrl Pts',(7.22672273303816,3.21939457384322,25.7809237749373));
#240221=CARTESIAN_POINT('Ctrl Pts',(7.25815764873642,3.14788332052009,25.777841874611));
#240222=CARTESIAN_POINT('Ctrl Pts',(7.29359559588401,3.06391158548436,25.774190479926));
#240223=CARTESIAN_POINT('Ctrl Pts',(7.2986342281089,3.05188946745068,25.7736669462404));
#240224=CARTESIAN_POINT('Ctrl Pts',(7.30662467730634,3.03269138425578,25.772829743969));
#240225=CARTESIAN_POINT('Ctrl Pts',(7.30959570315216,3.02552340315881,25.7725168978054));
#240226=CARTESIAN_POINT('Ctrl Pts',(7.31481714431917,3.01287342281304,25.7719643433128));
#240227=CARTESIAN_POINT('Ctrl Pts',(7.31707195767473,3.00739323712137,25.7717248196948));
#240228=CARTESIAN_POINT('Ctrl Pts',(7.32171729765526,2.99606687270199,25.7712294772718));
#240229=CARTESIAN_POINT('Ctrl Pts',(7.32410698440346,2.99022035529244,25.7709736240022));
#240230=CARTESIAN_POINT('Ctrl Pts',(7.3301988727343,2.97526505751482,25.7703187452598));
#240231=CARTESIAN_POINT('Ctrl Pts',(7.33389109293483,2.9661522402239,25.7699193147646));
#240232=CARTESIAN_POINT('Ctrl Pts',(7.34799805010092,2.93114730523009,25.7683835500981));
#240233=CARTESIAN_POINT('Ctrl Pts',(7.35829266765072,2.90520719786508,25.7672424692423));
#240234=CARTESIAN_POINT('Ctrl Pts',(7.42680005071799,2.72988389094158,25.7595119491278));
#240235=CARTESIAN_POINT('Ctrl Pts',(7.48059552369722,2.57881991545966,25.7527627603881));
#240236=CARTESIAN_POINT('Ctrl Pts',(7.57801063966181,2.27649401736567,25.7391903386938));
#240237=CARTESIAN_POINT('Ctrl Pts',(7.62178083557579,2.12535300142618,25.732373834178));
#240238=CARTESIAN_POINT('Ctrl Pts',(7.75338882681451,1.61433155697979,25.7093683059126));
#240239=CARTESIAN_POINT('Ctrl Pts',(7.82046110818994,1.24960009383117,25.6930391849767));
#240240=CARTESIAN_POINT('Ctrl Pts',(7.91356405651987,0.41926592395969,25.6568611486482));
#240241=CARTESIAN_POINT('Ctrl Pts',(7.92452867562839,-0.0466752222971706,
25.6372781353941));
#240242=CARTESIAN_POINT('Ctrl Pts',(7.89186314670459,-0.551421332796872,
25.6167844943394));
#240243=CARTESIAN_POINT('Ctrl Pts',(7.8889292064818,-0.591916736334149,
25.6151447841897));
#240244=CARTESIAN_POINT('Ctrl Pts',(7.88437398432118,-0.648718964333772,
25.6128509140851));
#240245=CARTESIAN_POINT('Ctrl Pts',(7.88301359124601,-0.665045969766149,
25.6121922921765));
#240246=CARTESIAN_POINT('Ctrl Pts',(7.88056957172468,-0.693316700811977,
25.6110531187557));
#240247=CARTESIAN_POINT('Ctrl Pts',(7.87950948889312,-0.705262389321949,
25.6105721526273));
#240248=CARTESIAN_POINT('Ctrl Pts',(7.87732643998743,-0.729242932820919,
25.6096074094877));
#240249=CARTESIAN_POINT('Ctrl Pts',(7.87620304738806,-0.74127771750638,
25.6091236414423));
#240250=CARTESIAN_POINT('Ctrl Pts',(7.87346876379282,-0.769861738101626,
25.6079755734287));
#240251=CARTESIAN_POINT('Ctrl Pts',(7.8718332691595,-0.786408580381014,
25.6073117219543));
#240252=CARTESIAN_POINT('Ctrl Pts',(7.86655258293882,-0.838167419799401,
25.6052375182829));
#240253=CARTESIAN_POINT('Ctrl Pts',(7.86272318943543,-0.873360312132879,
25.6038305727208));
#240254=CARTESIAN_POINT('Ctrl Pts',(7.85335165086542,-0.954423125706396,
25.6005975743449));
#240255=CARTESIAN_POINT('Ctrl Pts',(7.84764361275078,-1.00027268178144,
25.5987747009162));
#240256=CARTESIAN_POINT('Ctrl Pts',(7.78810478296598,-1.44658680221168,
25.5810845557414));
#240257=CARTESIAN_POINT('Ctrl Pts',(7.70406824708064,-1.84243034530877,
25.5658698828461));
#240258=CARTESIAN_POINT('Ctrl Pts',(7.40337791033981,-2.86581218369819,
25.5266429365841));
#240259=CARTESIAN_POINT('Ctrl Pts',(7.13751549315792,-3.47542187534271,
25.5035403828359));
#240260=CARTESIAN_POINT('Ctrl Pts',(6.78327536612906,-4.07087513869016,
25.4760585818342));
#240261=CARTESIAN_POINT('Ctrl Pts',(6.76754866782858,-4.09696644855851,
25.4748432087378));
#240262=CARTESIAN_POINT('Ctrl Pts',(6.74674109882409,-4.13104043233352,
25.4732404550622));
#240263=CARTESIAN_POINT('Ctrl Pts',(6.74179592184971,-4.13910597292978,
25.4728599251289));
#240264=CARTESIAN_POINT('Ctrl Pts',(6.7341391328884,-4.15154400318084,25.4722712997907));
#240265=CARTESIAN_POINT('Ctrl Pts',(6.73143769275227,-4.155922768755,25.4720637305759));
#240266=CARTESIAN_POINT('Ctrl Pts',(6.7263168678056,-4.16420502432065,25.4716704614654));
#240267=CARTESIAN_POINT('Ctrl Pts',(6.72389835107848,-4.16810905026834,
25.4714848070942));
#240268=CARTESIAN_POINT('Ctrl Pts',(6.7183144432621,-4.17710521666728,25.4710563512632));
#240269=CARTESIAN_POINT('Ctrl Pts',(6.71514666252388,-4.18219586463287,
25.4708134231343));
#240270=CARTESIAN_POINT('Ctrl Pts',(6.70629777858811,-4.19638011548431,
25.4701351954627));
#240271=CARTESIAN_POINT('Ctrl Pts',(6.70060398527656,-4.20546575297769,
25.4696992129861));
#240272=CARTESIAN_POINT('Ctrl Pts',(6.66786980790264,-4.25746473442685,
25.4671949545672));
#240273=CARTESIAN_POINT('Ctrl Pts',(6.64043742628702,-4.30012608767705,
25.4651044659931));
#240274=CARTESIAN_POINT('Ctrl Pts',(6.55823600476274,-4.42529868456959,
25.4588618965666));
#240275=CARTESIAN_POINT('Ctrl Pts',(6.50232854621353,-4.50704449709793,
25.4546462635495));
#240276=CARTESIAN_POINT('Ctrl Pts',(6.39493788545992,-4.65790875222603,
25.4466322764198));
#240277=CARTESIAN_POINT('Ctrl Pts',(6.3438302323843,-4.72727847542925,25.4428513684603));
#240278=CARTESIAN_POINT('Ctrl Pts',(6.04035596901734,-5.12540596672461,
25.4206450382768));
#240279=CARTESIAN_POINT('Ctrl Pts',(5.76360505415213,-5.43475171000619,
25.4013764489329));
#240280=CARTESIAN_POINT('Ctrl Pts',(5.01942047650561,-6.1454956440562,25.3540120357548));
#240281=CARTESIAN_POINT('Ctrl Pts',(4.52692046934216,-6.51681590509685,
25.3264482449478));
#240282=CARTESIAN_POINT('Ctrl Pts',(3.94139570983323,-6.85954613464755,
25.2985278931954));
#240283=CARTESIAN_POINT('Ctrl Pts',(3.88607054964027,-6.8910397790384,25.2959311305616));
#240284=CARTESIAN_POINT('Ctrl Pts',(3.81788358005277,-6.92877259244427,
25.2927803022379));
#240285=CARTESIAN_POINT('Ctrl Pts',(3.80537799203041,-6.93564870859802,
25.292204457958));
#240286=CARTESIAN_POINT('Ctrl Pts',(3.78469697854054,-6.9469472556835,25.2912554804291));
#240287=CARTESIAN_POINT('Ctrl Pts',(3.77653226797111,-6.95138917212442,
25.2908816827509));
#240288=CARTESIAN_POINT('Ctrl Pts',(3.76178497541852,-6.95937861546379,
25.290208051278));
#240289=CARTESIAN_POINT('Ctrl Pts',(3.75520516225295,-6.9629312149718,25.2899080449809));
#240290=CARTESIAN_POINT('Ctrl Pts',(3.74114027095115,-6.97049945301062,
25.2892679245558));
#240291=CARTESIAN_POINT('Ctrl Pts',(3.73365373916137,-6.97451237779075,
25.2889279028926));
#240292=CARTESIAN_POINT('Ctrl Pts',(3.71342776775083,-6.9853119876847,25.288011179519));
#240293=CARTESIAN_POINT('Ctrl Pts',(3.70067616664857,-6.99207589088613,
25.2874352509688));
#240294=CARTESIAN_POINT('Ctrl Pts',(3.63807612165887,-7.02506196361125,
25.2846177705243));
#240295=CARTESIAN_POINT('Ctrl Pts',(3.58796657139059,-7.05078644554548,
25.2823930629384));
#240296=CARTESIAN_POINT('Ctrl Pts',(3.17202403732779,-7.2587341389627,25.2641713853836));
#240297=CARTESIAN_POINT('Ctrl Pts',(2.79283639816729,-7.41289855684044,
25.2491540744402));
#240298=CARTESIAN_POINT('Ctrl Pts',(2.06802766020124,-7.64402357077033,
25.2222185966223));
#240299=CARTESIAN_POINT('Ctrl Pts',(1.72588399181924,-7.7284644605348,25.210178402911));
#240300=CARTESIAN_POINT('Ctrl Pts',(0.892907146292186,-7.87595001267056,
25.1809104913779));
#240301=CARTESIAN_POINT('Ctrl Pts',(0.399564734553673,-7.91632554801724,
25.1635904060704));
#240302=CARTESIAN_POINT('Ctrl Pts',(-0.128326483362468,-7.91003230056521,
25.1427104788361));
#240303=CARTESIAN_POINT('Ctrl Pts',(-0.162345484888009,-7.90940722041612,
25.1413556328557));
#240304=CARTESIAN_POINT('Ctrl Pts',(-0.207319566408222,-7.90829057411755,
25.1395530951377));
#240305=CARTESIAN_POINT('Ctrl Pts',(-0.2182794854113,-7.90799565452776,
25.1391129322763));
#240306=CARTESIAN_POINT('Ctrl Pts',(-0.235283884072636,-7.90750270746726,
25.1384286609986));
#240307=CARTESIAN_POINT('Ctrl Pts',(-0.241328833869524,-7.90732053026867,
25.1381851413681));
#240308=CARTESIAN_POINT('Ctrl Pts',(-0.25282129510099,-7.90696099014185,
25.1377216713262));
#240309=CARTESIAN_POINT('Ctrl Pts',(-0.258268845628237,-7.90678492878626,
25.1375017685695));
#240310=CARTESIAN_POINT('Ctrl Pts',(-0.2709042296182,-7.90636348921582,
25.136991224677));
#240311=CARTESIAN_POINT('Ctrl Pts',(-0.278091913268336,-7.90611393875588,
25.1367004336836));
#240312=CARTESIAN_POINT('Ctrl Pts',(-0.298356904620666,-7.90538268559308,
25.1358795602324));
#240313=CARTESIAN_POINT('Ctrl Pts',(-0.31143334100732,-7.90487833682059,
25.1353486805052));
#240314=CARTESIAN_POINT('Ctrl Pts',(-0.389438147581476,-7.9016758921437,
25.1321749217301));
#240315=CARTESIAN_POINT('Ctrl Pts',(-0.454331603766616,-7.89821033573475,
25.1295061030923));
#240316=CARTESIAN_POINT('Ctrl Pts',(-0.767204610793201,-7.87763310944881,
25.1165213591357));
#240317=CARTESIAN_POINT('Ctrl Pts',(-1.01432200024726,-7.8496401047812,
25.1059149459615));
#240318=CARTESIAN_POINT('Ctrl Pts',(-1.42060480679042,-7.78410984820686,
25.0882062682119));
#240319=CARTESIAN_POINT('Ctrl Pts',(-1.58066643160403,-7.75319143955675,
25.0811573547996));
#240320=CARTESIAN_POINT('Ctrl Pts',(-2.41718768415652,-7.56462143454308,
25.0441163516376));
#240321=CARTESIAN_POINT('Ctrl Pts',(-3.07169686577322,-7.32332428500461,
25.0148602313158));
#240322=CARTESIAN_POINT('Ctrl Pts',(-3.85920077119008,-6.90859483200105,
24.9784786209216));
#240323=CARTESIAN_POINT('Ctrl Pts',(-4.02868505155801,-6.81115347557454,
24.9705249472782));
#240324=CARTESIAN_POINT('Ctrl Pts',(-4.23443943109837,-6.68249019055684,
24.960712382342));
#240325=CARTESIAN_POINT('Ctrl Pts',(-4.27426643629504,-6.65708636716249,
24.9588055484855));
#240326=CARTESIAN_POINT('Ctrl Pts',(-4.33708197457112,-6.6162231048759,
24.9557861183175));
#240327=CARTESIAN_POINT('Ctrl Pts',(-4.36022087023407,-6.60099706073905,
24.9546712660697));
#240328=CARTESIAN_POINT('Ctrl Pts',(-4.40311666151133,-6.57244646316064,
24.9525996083202));
#240329=CARTESIAN_POINT('Ctrl Pts',(-4.42289423302735,-6.55915356223814,
24.9516424911782));
#240330=CARTESIAN_POINT('Ctrl Pts',(-4.46667809829981,-6.52943747718006,
24.9495192162957));
#240331=CARTESIAN_POINT('Ctrl Pts',(-4.49065450569651,-6.51297083667225,
24.9483535355956));
#240332=CARTESIAN_POINT('Ctrl Pts',(-4.56012943768581,-6.46469045543939,
24.9449670642311));
#240333=CARTESIAN_POINT('Ctrl Pts',(-4.60538467697536,-6.43252945560772,
24.9427501575247));
#240334=CARTESIAN_POINT('Ctrl Pts',(-4.70686112012858,-6.35879454162698,
24.9377532698846));
#240335=CARTESIAN_POINT('Ctrl Pts',(-4.76287733930216,-6.31694619033517,
24.9349766274018));
#240336=CARTESIAN_POINT('Ctrl Pts',(-4.94234353897597,-6.17912693867589,
24.9260174705253));
#240337=CARTESIAN_POINT('Ctrl Pts',(-5.06350578203972,-6.08023679844488,
24.9198707185008));
#240338=CARTESIAN_POINT('Ctrl Pts',(-5.42453302331702,-5.76729328858461,
24.901192208494));
#240339=CARTESIAN_POINT('Ctrl Pts',(-5.65435206053312,-5.54215984406977,
24.8887963742496));
#240340=CARTESIAN_POINT('Ctrl Pts',(-6.01740140029522,-5.14035484515502,
24.8678586022022));
#240341=CARTESIAN_POINT('Ctrl Pts',(-6.15808236656568,-4.97095432613832,
24.8593393837935));
#240342=CARTESIAN_POINT('Ctrl Pts',(-6.37749611203214,-4.68311645786316,
24.8451500723635));
#240343=CARTESIAN_POINT('Ctrl Pts',(-6.46042724311262,-4.56803184101864,
24.8395461789172));
#240344=CARTESIAN_POINT('Ctrl Pts',(-6.55272448061564,-4.43240532886357,
24.8329766340643));
#240345=CARTESIAN_POINT('Ctrl Pts',(-6.56515298355492,-4.41397569249168,
24.8320846448784));
#240346=CARTESIAN_POINT('Ctrl Pts',(-6.58488513591073,-4.38444811181062,
24.8306564116691));
#240347=CARTESIAN_POINT('Ctrl Pts',(-6.59223881665402,-4.37338368782955,
24.8301214305637));
#240348=CARTESIAN_POINT('Ctrl Pts',(-6.60520032851953,-4.35377469291024,
24.8291736001751));
#240349=CARTESIAN_POINT('Ctrl Pts',(-6.61081954406833,-4.34523767031747,
24.8287610482132));
#240350=CARTESIAN_POINT('Ctrl Pts',(-6.62156871649564,-4.32883782013141,
24.8279686833773));
#240351=CARTESIAN_POINT('Ctrl Pts',(-6.62670125268815,-4.32097670062247,
24.8275889401349));
#240352=CARTESIAN_POINT('Ctrl Pts',(-6.63763962354227,-4.30415789391444,
24.8267766057991));
#240353=CARTESIAN_POINT('Ctrl Pts',(-6.64344134329728,-4.29519755832799,
24.8263439036952));
#240354=CARTESIAN_POINT('Ctrl Pts',(-6.65731368971747,-4.2736773768335,
24.8253048131739));
#240355=CARTESIAN_POINT('Ctrl Pts',(-6.66536691698014,-4.26110639900326,
24.8246979384826));
#240356=CARTESIAN_POINT('Ctrl Pts',(-6.74569384203709,-4.13493225572388,
24.8186082185335));
#240357=CARTESIAN_POINT('Ctrl Pts',(-6.8150904613982,-4.019526196529,24.8130502646201));
#240358=CARTESIAN_POINT('Ctrl Pts',(-7.07042589224615,-3.56926764338862,
24.7915061307935));
#240359=CARTESIAN_POINT('Ctrl Pts',(-7.23490359258804,-3.22285014961678,
24.7752459526445));
#240360=CARTESIAN_POINT('Ctrl Pts',(-7.42031007689021,-2.74581747595993,
24.7537405127815));
#240361=CARTESIAN_POINT('Ctrl Pts',(-7.46403738280445,-2.62462601690647,
24.7483469613483));
#240362=CARTESIAN_POINT('Ctrl Pts',(-7.58670156865326,-2.25675471832648,
24.7321983807278));
#240363=CARTESIAN_POINT('Ctrl Pts',(-7.65650666553869,-2.00721060201868,
24.7215461312734));
#240364=CARTESIAN_POINT('Ctrl Pts',(-7.72318865482372,-1.71406349184627,
24.7093574827083));
#240365=CARTESIAN_POINT('Ctrl Pts',(-7.73210823394862,-1.67336754392676,
24.7076723989871));
#240366=CARTESIAN_POINT('Ctrl Pts',(-7.74597837700718,-1.60760464455309,
24.7049602313704));
#240367=CARTESIAN_POINT('Ctrl Pts',(-7.75112967470828,-1.58258095594426,
24.703930739403));
#240368=CARTESIAN_POINT('Ctrl Pts',(-7.76011158640798,-1.53785307219791,
24.7020949857497));
#240369=CARTESIAN_POINT('Ctrl Pts',(-7.76398859115839,-1.51815844509082,
24.7012881782103));
#240370=CARTESIAN_POINT('Ctrl Pts',(-7.77133790987195,-1.48006041193939,
24.6997303124276));
#240371=CARTESIAN_POINT('Ctrl Pts',(-7.77481991163523,-1.46165901506856,
24.6989791453062));
#240372=CARTESIAN_POINT('Ctrl Pts',(-7.78220196596491,-1.42187412134314,
24.6973577825686));
#240373=CARTESIAN_POINT('Ctrl Pts',(-7.78607930032468,-1.40048655422635,
24.6964878552548));
#240374=CARTESIAN_POINT('Ctrl Pts',(-7.79529299447324,-1.34844222269386,
24.6943749478352));
#240375=CARTESIAN_POINT('Ctrl Pts',(-7.80053672141716,-1.31776939005816,
24.6931330267593));
#240376=CARTESIAN_POINT('Ctrl Pts',(-7.82558409321283,-1.16586599309891,
24.6869982566981));
#240377=CARTESIAN_POINT('Ctrl Pts',(-7.84274340238029,-1.04421566810183,
24.6821349300275));
#240378=CARTESIAN_POINT('Ctrl Pts',(-7.89298455370822,-0.616172009389288,
24.6651523667399));
#240379=CARTESIAN_POINT('Ctrl Pts',(-7.9109944847476,-0.308287032974473,
24.6531273941981));
#240380=CARTESIAN_POINT('Ctrl Pts',(-7.91099999873345,-0.000141560223926238,
24.6412306241627));
#240381=CARTESIAN_POINT('',(-7.911,-2.22599716437344E-13,22.642331508237));
#240382=CARTESIAN_POINT('Ctrl Pts',(-7.911,-2.20934381900406E-13,24.642331508237));
#240383=CARTESIAN_POINT('Ctrl Pts',(-7.91100000000006,2.2016758966665,24.5537440725043));
#240384=CARTESIAN_POINT('Ctrl Pts',(-6.94214576672388,4.38610418338655,
24.4651566367716));
#240385=CARTESIAN_POINT('Ctrl Pts',(-3.67820201488323,7.34180684107613,
24.2879817653061));
#240386=CARTESIAN_POINT('Ctrl Pts',(-1.4086817587179,8.08992666571327,24.1993943295734));
#240387=CARTESIAN_POINT('Ctrl Pts',(2.97309270521222,7.65454228025276,24.022219458108));
#240388=CARTESIAN_POINT('Ctrl Pts',(5.05102072675554,6.47444880834262,23.9336320223752));
#240389=CARTESIAN_POINT('Ctrl Pts',(7.66951518847845,2.93425195367772,23.7564571509098));
#240390=CARTESIAN_POINT('Ctrl Pts',(8.18956872247065,0.601881960099923,
23.6678697151771));
#240391=CARTESIAN_POINT('Ctrl Pts',(7.3230668976138,-3.71537198232373,23.4906948437116));
#240392=CARTESIAN_POINT('Ctrl Pts',(5.94329958850263,-5.66643518936444,
23.4021074079789));
#240393=CARTESIAN_POINT('Ctrl Pts',(2.16154501637943,-7.9220591323297,23.2249325365135));
#240394=CARTESIAN_POINT('Ctrl Pts',(-0.210816529299319,-8.20894963713004,
23.1363451007807));
#240395=CARTESIAN_POINT('Ctrl Pts',(-4.42123908576341,-6.91982244717892,
22.9591702293153));
#240396=CARTESIAN_POINT('Ctrl Pts',(-6.22631625634109,-5.3539035880361,
22.8705827935826));
#240397=CARTESIAN_POINT('Ctrl Pts',(-7.65317280859467,-2.31334857514605,
22.7354407413122));
#240398=CARTESIAN_POINT('Ctrl Pts',(-7.91099999999997,-1.15702837836574,
22.6888861247746));
#240399=CARTESIAN_POINT('Ctrl Pts',(-7.911,-2.22599716437344E-13,22.642331508237));
#240400=CARTESIAN_POINT('',(-7.911,-5.77315972805081E-14,18.642331508237));
#240401=CARTESIAN_POINT('Ctrl Pts',(-7.91099999997837,1.85007747019461E-5,
22.6428089873088));
#240402=CARTESIAN_POINT('Ctrl Pts',(-7.91099947188172,0.225834589107863,
22.6340593417855));
#240403=CARTESIAN_POINT('Ctrl Pts',(-7.90133019881069,0.451545623192688,
22.625271724421));
#240404=CARTESIAN_POINT('Ctrl Pts',(-7.87628419288177,0.743347599373823,
22.6136725448826));
#240405=CARTESIAN_POINT('Ctrl Pts',(-7.86969985014172,0.810087925509054,
22.6110031635888));
#240406=CARTESIAN_POINT('Ctrl Pts',(-7.86039549709614,0.893526189294941,
22.6076401591403));
#240407=CARTESIAN_POINT('Ctrl Pts',(-7.85846939797451,0.910310463447805,
22.6069623552187));
#240408=CARTESIAN_POINT('Ctrl Pts',(-7.85514325884769,0.938497395190295,
22.6058217621311));
#240409=CARTESIAN_POINT('Ctrl Pts',(-7.85377211620916,0.949903428503671,
22.605359576643));
#240410=CARTESIAN_POINT('Ctrl Pts',(-7.85121277146412,0.970809288817946,
22.6045112405228));
#240411=CARTESIAN_POINT('Ctrl Pts',(-7.85003215939754,0.980310029480703,
22.6041252539591));
#240412=CARTESIAN_POINT('Ctrl Pts',(-7.84757168723977,0.999820709126633,
22.6033316286725));
#240413=CARTESIAN_POINT('Ctrl Pts',(-7.84628991462983,1.00983038756246,
22.6029239483633));
#240414=CARTESIAN_POINT('Ctrl Pts',(-7.84339225134556,1.03212034556546,
22.602014913668));
#240415=CARTESIAN_POINT('Ctrl Pts',(-7.84176666681656,1.04439932883301,
22.6015133401986));
#240416=CARTESIAN_POINT('Ctrl Pts',(-7.83679430839989,1.08129228993849,
22.6000038185238));
#240417=CARTESIAN_POINT('Ctrl Pts',(-7.83336045860627,1.10589418857624,
22.5989937899261));
#240418=CARTESIAN_POINT('Ctrl Pts',(-7.79597594242603,1.36482300994179,
22.5883289695019));
#240419=CARTESIAN_POINT('Ctrl Pts',(-7.75163812332933,1.59752424659365,
22.5784506834872));
#240420=CARTESIAN_POINT('Ctrl Pts',(-7.66769492256991,1.95099672648986,
22.5631819610048));
#240421=CARTESIAN_POINT('Ctrl Pts',(-7.63550721297095,2.07339409088313,
22.557844577228));
#240422=CARTESIAN_POINT('Ctrl Pts',(-7.57845711590641,2.27093855724286,
22.5491703269968));
#240423=CARTESIAN_POINT('Ctrl Pts',(-7.55537867926464,2.34657776940649,
22.5458344051522));
#240424=CARTESIAN_POINT('Ctrl Pts',(-7.46888534036507,2.61554315244939,
22.5339289701738));
#240425=CARTESIAN_POINT('Ctrl Pts',(-7.39915136782156,2.80675526995091,
22.5253867440962));
#240426=CARTESIAN_POINT('Ctrl Pts',(-7.22505167866806,3.23238142449122,
22.5062460365987));
#240427=CARTESIAN_POINT('Ctrl Pts',(-7.1164986088984,3.4648398212024,22.4957044439306));
#240428=CARTESIAN_POINT('Ctrl Pts',(-6.98210501527786,3.71956025029167,
22.4840320954564));
#240429=CARTESIAN_POINT('Ctrl Pts',(-6.96719668165485,3.7474110143701,22.4827540877373));
#240430=CARTESIAN_POINT('Ctrl Pts',(-6.94165181214019,3.7944528591276,22.4805922490391));
#240431=CARTESIAN_POINT('Ctrl Pts',(-6.93110154893593,3.8136902998665,22.479707266701));
#240432=CARTESIAN_POINT('Ctrl Pts',(-6.91143514245836,3.84919902275244,
22.478071984102));
#240433=CARTESIAN_POINT('Ctrl Pts',(-6.90234123007919,3.8654824266882,22.4773213916176));
#240434=CARTESIAN_POINT('Ctrl Pts',(-6.88338295794391,3.89914856235341,
22.4757680361489));
#240435=CARTESIAN_POINT('Ctrl Pts',(-6.87351013381267,3.91652638191039,
22.4749653924566));
#240436=CARTESIAN_POINT('Ctrl Pts',(-6.85101900454776,3.95576753807374,
22.4731509608421));
#240437=CARTESIAN_POINT('Ctrl Pts',(-6.83836168591077,3.97760828566071,
22.4721396988799));
#240438=CARTESIAN_POINT('Ctrl Pts',(-6.80544566493161,4.03378477728129,
22.4695348352247));
#240439=CARTESIAN_POINT('Ctrl Pts',(-6.78503152774331,4.06802870150093,
22.4679432850186));
#240440=CARTESIAN_POINT('Ctrl Pts',(-6.62875464993973,4.32572807193166,
22.4559356229943));
#240441=CARTESIAN_POINT('Ctrl Pts',(-6.4821440984346,4.54247980283908,22.4456648460621));
#240442=CARTESIAN_POINT('Ctrl Pts',(-6.28058366354077,4.81078733198935,
22.4325530690247));
#240443=CARTESIAN_POINT('Ctrl Pts',(-6.23527154137811,4.86937314146339,
22.4296652489258));
#240444=CARTESIAN_POINT('Ctrl Pts',(-6.15435604600134,4.97101017366863,
22.4246125997869));
#240445=CARTESIAN_POINT('Ctrl Pts',(-6.11910688717685,5.0143365892881,22.4224447028392));
#240446=CARTESIAN_POINT('Ctrl Pts',(-5.95684678751198,5.20951901160713,
22.4126145385632));
#240447=CARTESIAN_POINT('Ctrl Pts',(-5.82462080235687,5.35694936395049,
22.4050135008768));
#240448=CARTESIAN_POINT('Ctrl Pts',(-5.4896007793828,5.70340642148044,22.3866671704931));
#240449=CARTESIAN_POINT('Ctrl Pts',(-5.28134977784322,5.89677110331032,
22.3760093399635));
#240450=CARTESIAN_POINT('Ctrl Pts',(-4.8877576665812,6.22461666329464,22.3568458554157));
#240451=CARTESIAN_POINT('Ctrl Pts',(-4.70612459444823,6.36305095458173,
22.3483344491076));
#240452=CARTESIAN_POINT('Ctrl Pts',(-4.3415918921577,6.61672811096935,22.3315952822459));
#240453=CARTESIAN_POINT('Ctrl Pts',(-4.15945478890625,6.73271429524361,
22.3233836074929));
#240454=CARTESIAN_POINT('Ctrl Pts',(-3.92005662246139,6.87173911146183,
22.3125749451155));
#240455=CARTESIAN_POINT('Ctrl Pts',(-3.86695199250248,6.90176241592576,
22.3101761715765));
#240456=CARTESIAN_POINT('Ctrl Pts',(-3.78062839310874,6.94925737892598,
22.3062684962585));
#240457=CARTESIAN_POINT('Ctrl Pts',(-3.74762264836752,6.96711228571304,
22.3047724465327));
#240458=CARTESIAN_POINT('Ctrl Pts',(-3.7067609966152,6.98884257757154,22.3029167076623));
#240459=CARTESIAN_POINT('Ctrl Pts',(-3.69902377467732,6.99294078151754,
22.3025651617896));
#240460=CARTESIAN_POINT('Ctrl Pts',(-3.68403311561726,7.00084910081391,
22.3018837199889));
#240461=CARTESIAN_POINT('Ctrl Pts',(-3.67678052949254,7.00466081025467,
22.3015538839924));
#240462=CARTESIAN_POINT('Ctrl Pts',(-3.66357803353426,7.01157343321013,
22.3009531647719));
#240463=CARTESIAN_POINT('Ctrl Pts',(-3.65763007008554,7.01467806012467,
22.3006824227379));
#240464=CARTESIAN_POINT('Ctrl Pts',(-3.64569438681568,7.02088875702022,
22.3001389028311));
#240465=CARTESIAN_POINT('Ctrl Pts',(-3.63970663004246,7.02399474283716,
22.2998661220643));
#240466=CARTESIAN_POINT('Ctrl Pts',(-3.6227321961501,7.03277223491493,22.2990924885493));
#240467=CARTESIAN_POINT('Ctrl Pts',(-3.6117362111439,7.03842563449197,22.2985909293477));
#240468=CARTESIAN_POINT('Ctrl Pts',(-3.56563632572705,7.06199063316919,
22.2964863463025));
#240469=CARTESIAN_POINT('Ctrl Pts',(-3.53041244659525,7.07966538728848,
22.2948738448653));
#240470=CARTESIAN_POINT('Ctrl Pts',(-3.12823238779529,7.27772481163952,
22.2763988287588));
#240471=CARTESIAN_POINT('Ctrl Pts',(-2.74802911571958,7.42962425631084,
22.2580950489523));
#240472=CARTESIAN_POINT('Ctrl Pts',(-2.07436532959066,7.63997019556098,
22.2258840418904));
#240473=CARTESIAN_POINT('Ctrl Pts',(-1.78608933201022,7.71245905865922,
22.2121852835603));
#240474=CARTESIAN_POINT('Ctrl Pts',(-1.4540998467207,7.77632307354195,22.1968332689011));
#240475=CARTESIAN_POINT('Ctrl Pts',(-1.41371932530258,7.78376545192754,
22.194972807624));
#240476=CARTESIAN_POINT('Ctrl Pts',(-1.32481652063159,7.79943614115764,
22.1908930085562));
#240477=CARTESIAN_POINT('Ctrl Pts',(-1.27627155825407,7.80752674731903,
22.1886758531657));
#240478=CARTESIAN_POINT('Ctrl Pts',(-1.16778080995629,7.82456914009742,
22.1837463996782));
#240479=CARTESIAN_POINT('Ctrl Pts',(-1.1078010156543,7.83328611152453,22.1810384719679));
#240480=CARTESIAN_POINT('Ctrl Pts',(-0.927566984344306,7.857368295966,22.1729575392434));
#240481=CARTESIAN_POINT('Ctrl Pts',(-0.8070518028975,7.87065980948529,22.167629173485));
#240482=CARTESIAN_POINT('Ctrl Pts',(-0.510681921319957,7.8964670567616,
22.1547289874667));
#240483=CARTESIAN_POINT('Ctrl Pts',(-0.334619928280042,7.90588530861514,
22.1472410774888));
#240484=CARTESIAN_POINT('Ctrl Pts',(-0.0656134310241799,7.91127205124591,
22.1360805822652));
#240485=CARTESIAN_POINT('Ctrl Pts',(0.0271832380362279,7.91149748277865,
22.1322811667856));
#240486=CARTESIAN_POINT('Ctrl Pts',(0.136364745785925,7.9098416346343,22.1278692412764));
#240487=CARTESIAN_POINT('Ctrl Pts',(0.152764209294816,7.90954190389132,
22.1272080993915));
#240488=CARTESIAN_POINT('Ctrl Pts',(0.177884482337895,7.90900462861615,
22.1261977317544));
#240489=CARTESIAN_POINT('Ctrl Pts',(0.186605981675171,7.90880365875589,
22.1258473769466));
#240490=CARTESIAN_POINT('Ctrl Pts',(0.201811108095771,7.90842812093658,
22.1252373202608));
#240491=CARTESIAN_POINT('Ctrl Pts',(0.208294878119738,7.90826000529718,
22.124977419095));
#240492=CARTESIAN_POINT('Ctrl Pts',(0.222870067641702,7.9078641525774,22.1243937104413));
#240493=CARTESIAN_POINT('Ctrl Pts',(0.230961364495052,7.90763196989324,
22.1240700408404));
#240494=CARTESIAN_POINT('Ctrl Pts',(0.252581737747672,7.90697835323765,
22.1232061672142));
#240495=CARTESIAN_POINT('Ctrl Pts',(0.266110139623721,7.90653461440098,
22.1226666547609));
#240496=CARTESIAN_POINT('Ctrl Pts',(0.324218775260846,7.90447931068766,
22.1203536956783));
#240497=CARTESIAN_POINT('Ctrl Pts',(0.368786477951271,7.90252539401648,
22.1185908841695));
#240498=CARTESIAN_POINT('Ctrl Pts',(1.08739624247348,7.86492795316929,22.0903422464757));
#240499=CARTESIAN_POINT('Ctrl Pts',(1.75415916349144,7.74354869690067,22.0669395413601));
#240500=CARTESIAN_POINT('Ctrl Pts',(2.72994846730285,7.43323781131119,22.0320968713692));
#240501=CARTESIAN_POINT('Ctrl Pts',(3.05505821906778,7.30563109655708,22.0203113192068));
#240502=CARTESIAN_POINT('Ctrl Pts',(3.53012980368479,7.08189040513239,22.0016192066847));
#240503=CARTESIAN_POINT('Ctrl Pts',(3.68702782460995,7.00148615918928,21.9951859512676));
#240504=CARTESIAN_POINT('Ctrl Pts',(3.90745831682518,6.87905893891138,21.9856038899837));
#240505=CARTESIAN_POINT('Ctrl Pts',(3.97327889362922,6.84125256043448,21.9826708224208));
#240506=CARTESIAN_POINT('Ctrl Pts',(4.07265036097292,6.78225724436087,21.978117974155));
#240507=CARTESIAN_POINT('Ctrl Pts',(4.10660392991548,6.76175260951729,21.9765397832609));
#240508=CARTESIAN_POINT('Ctrl Pts',(4.14747804407004,6.73664722596892,21.9746108816709));
#240509=CARTESIAN_POINT('Ctrl Pts',(4.15454790129882,6.73228948486491,21.9742761885484));
#240510=CARTESIAN_POINT('Ctrl Pts',(4.16552421250567,6.72549999694147,21.9737548962195));
#240511=CARTESIAN_POINT('Ctrl Pts',(4.16943544558883,6.72307595068726,21.9735688129392));
#240512=CARTESIAN_POINT('Ctrl Pts',(4.17632080872631,6.71880032270922,21.9732406469143));
#240513=CARTESIAN_POINT('Ctrl Pts',(4.17929583225755,6.71695017253029,21.9730986609444));
#240514=CARTESIAN_POINT('Ctrl Pts',(4.18607532265463,6.7127277983333,21.9727746625463));
#240515=CARTESIAN_POINT('Ctrl Pts',(4.18987900084942,6.71035431698915,21.9725925645437));
#240516=CARTESIAN_POINT('Ctrl Pts',(4.20010062288934,6.70396398281072,21.9721023559091));
#240517=CARTESIAN_POINT('Ctrl Pts',(4.20651480684571,6.69994115677308,21.9717938351828));
#240518=CARTESIAN_POINT('Ctrl Pts',(4.23695296205756,6.680790118873,21.970325400161));
#240519=CARTESIAN_POINT('Ctrl Pts',(4.26090078451377,6.66554209851233,21.9691571149886));
#240520=CARTESIAN_POINT('Ctrl Pts',(4.66035652620445,6.40816893017067,21.9494599959016));
#240521=CARTESIAN_POINT('Ctrl Pts',(5.0147402093208,6.1348074521758,21.9289125924497));
#240522=CARTESIAN_POINT('Ctrl Pts',(5.54324189633102,5.65060343332933,21.8956222157966));
#240523=CARTESIAN_POINT('Ctrl Pts',(5.73289344247054,5.45809382295399,21.8830181441089));
#240524=CARTESIAN_POINT('Ctrl Pts',(6.10438682706551,5.04023178486727,21.8573830384152));
#240525=CARTESIAN_POINT('Ctrl Pts',(6.28446923994954,4.81382821691317,21.8444055708804));
#240526=CARTESIAN_POINT('Ctrl Pts',(6.54119723364208,4.45202674585738,21.8252230986467));
#240527=CARTESIAN_POINT('Ctrl Pts',(6.62691928739897,4.32339541815724,21.818678789976));
#240528=CARTESIAN_POINT('Ctrl Pts',(6.75415067617889,4.11979199745794,21.8087454503479));
#240529=CARTESIAN_POINT('Ctrl Pts',(6.79830100027159,4.04652216335594,21.8052528562462));
#240530=CARTESIAN_POINT('Ctrl Pts',(6.84882584814265,3.9595116851916,21.8011995931593));
#240531=CARTESIAN_POINT('Ctrl Pts',(6.85635904392977,3.94645270434103,21.8005937224651));
#240532=CARTESIAN_POINT('Ctrl Pts',(6.86783791703805,3.92642171947991,21.7996681380012));
#240533=CARTESIAN_POINT('Ctrl Pts',(6.87181038928772,3.91946516097647,21.7993473824943));
#240534=CARTESIAN_POINT('Ctrl Pts',(6.87871617792437,3.90732903342419,21.7987890055021));
#240535=CARTESIAN_POINT('Ctrl Pts',(6.88165422405628,3.9021521718947,21.7985512005224));
#240536=CARTESIAN_POINT('Ctrl Pts',(6.8877813985314,3.89132759775534,21.7980547530893));
#240537=CARTESIAN_POINT('Ctrl Pts',(6.89096943075404,3.88567926773465,21.7977961532129));
#240538=CARTESIAN_POINT('Ctrl Pts',(6.89975692693925,3.87006537608898,21.7970825340427));
#240539=CARTESIAN_POINT('Ctrl Pts',(6.90534175404857,3.86009156981522,21.7966280813417));
#240540=CARTESIAN_POINT('Ctrl Pts',(6.92709495946532,3.82104476219223,21.7948543410736));
#240541=CARTESIAN_POINT('Ctrl Pts',(6.94310162327903,3.79188179376777,21.793541295473));
#240542=CARTESIAN_POINT('Ctrl Pts',(7.20123219617396,3.31447196654534,21.7722341279695));
#240543=CARTESIAN_POINT('Ctrl Pts',(7.39969815673857,2.84394314497516,21.7540460092325));
#240544=CARTESIAN_POINT('Ctrl Pts',(7.64136847332154,2.06984492742794,21.7262883056658));
#240545=CARTESIAN_POINT('Ctrl Pts',(7.71467518660256,1.77723268559261,21.7162270292646));
#240546=CARTESIAN_POINT('Ctrl Pts',(7.8225374645392,1.21131559017786,21.69663899123));
#240547=CARTESIAN_POINT('Ctrl Pts',(7.85987595156819,0.93899572923286,21.6871537086428));
#240548=CARTESIAN_POINT('Ctrl Pts',(7.89638970338853,0.506354469200814,
21.6712640996314));
#240549=CARTESIAN_POINT('Ctrl Pts',(7.90499325211327,0.347046390675704,
21.665237634515));
#240550=CARTESIAN_POINT('Ctrl Pts',(7.90950277392658,0.156932182869372,
21.6577204511803));
#240551=CARTESIAN_POINT('Ctrl Pts',(7.91005177978121,0.126264129222067,
21.656497733352));
#240552=CARTESIAN_POINT('Ctrl Pts',(7.91051053026259,0.0883024688019221,
21.6549708614013));
#240553=CARTESIAN_POINT('Ctrl Pts',(7.91058856414158,0.0810107618625305,
21.6546769684268));
#240554=CARTESIAN_POINT('Ctrl Pts',(7.91069583887694,0.0694992955269612,
21.6542120194351));
#240555=CARTESIAN_POINT('Ctrl Pts',(7.91073178551788,0.0652795888302459,
21.6540413775776));
#240556=CARTESIAN_POINT('Ctrl Pts',(7.91079296536326,0.0573532802561827,
21.6537204561918));
#240557=CARTESIAN_POINT('Ctrl Pts',(7.91081896980937,0.0536466812177394,
21.6535702238721));
#240558=CARTESIAN_POINT('Ctrl Pts',(7.91087138337838,0.0453440202853812,
21.6532333542403));
#240559=CARTESIAN_POINT('Ctrl Pts',(7.9108963922299,0.0407479542872487,
21.6530466317827));
#240560=CARTESIAN_POINT('Ctrl Pts',(7.91094955548323,0.0291145307100258,
21.6525733949361));
#240561=CARTESIAN_POINT('Ctrl Pts',(7.9109723247733,0.0220771669155261,
21.6522865559681));
#240562=CARTESIAN_POINT('Ctrl Pts',(7.91104465223491,-0.0159673076060156,
21.650732863045));
#240563=CARTESIAN_POINT('Ctrl Pts',(7.91092130081699,-0.0469740685472476,
21.6494557316463));
#240564=CARTESIAN_POINT('Ctrl Pts',(7.90594116408264,-0.552187211951711,
21.6284789904422));
#240565=CARTESIAN_POINT('Ctrl Pts',(7.85863612941356,-1.02497058752852,
21.6064852780704));
#240566=CARTESIAN_POINT('Ctrl Pts',(7.67751068385218,-1.96902258567539,
21.5613785362503));
#240567=CARTESIAN_POINT('Ctrl Pts',(7.54172299689951,-2.43797134772273,
21.5383768620033));
#240568=CARTESIAN_POINT('Ctrl Pts',(7.22822485254222,-3.23635152834974,
21.5000003508207));
#240569=CARTESIAN_POINT('Ctrl Pts',(7.06872916756617,-3.57131980832494,
21.4841453801161));
#240570=CARTESIAN_POINT('Ctrl Pts',(6.87625230642662,-3.91171235823119,
21.4683228537066));
#240571=CARTESIAN_POINT('Ctrl Pts',(6.86611562341367,-3.92947777822749,
21.4674978269409));
#240572=CARTESIAN_POINT('Ctrl Pts',(6.85126888633146,-3.95526512048715,
21.466301332907));
#240573=CARTESIAN_POINT('Ctrl Pts',(6.84661344438168,-3.96331829029176,
21.4659278304604));
#240574=CARTESIAN_POINT('Ctrl Pts',(6.83843837022138,-3.97740247107555,
21.4652748740868));
#240575=CARTESIAN_POINT('Ctrl Pts',(6.83492494136836,-3.98343705942763,
21.4649951889962));
#240576=CARTESIAN_POINT('Ctrl Pts',(6.82810266970285,-3.99511924421489,
21.464453915443));
#240577=CARTESIAN_POINT('Ctrl Pts',(6.82479479969096,-4.00076739962065,
21.4641922910071));
#240578=CARTESIAN_POINT('Ctrl Pts',(6.81690574877656,-4.01419962020725,
21.4635702769125));
#240579=CARTESIAN_POINT('Ctrl Pts',(6.81231823452317,-4.02197996649668,
21.4632101244152));
#240580=CARTESIAN_POINT('Ctrl Pts',(6.79599666540415,-4.04955303239049,
21.4619342402075));
#240581=CARTESIAN_POINT('Ctrl Pts',(6.78418954091072,-4.06930248606056,
21.4610212451497));
#240582=CARTESIAN_POINT('Ctrl Pts',(6.62266647098264,-4.33682071272996,
21.4486652021049));
#240583=CARTESIAN_POINT('Ctrl Pts',(6.45954090847352,-4.57625125008697,
21.4377470820495));
#240584=CARTESIAN_POINT('Ctrl Pts',(6.13496480416999,-5.00060190909944,
21.4183060161173));
#240585=CARTESIAN_POINT('Ctrl Pts',(5.97734070090344,-5.1879877640431,21.4096817891106));
#240586=CARTESIAN_POINT('Ctrl Pts',(5.50390402895874,-5.70054194215602,
21.3854245849952));
#240587=CARTESIAN_POINT('Ctrl Pts',(5.16852816703237,-6.00628181767911,
21.3701489956794));
#240588=CARTESIAN_POINT('Ctrl Pts',(4.62554652830653,-6.42195708805594,
21.3454416127073));
#240589=CARTESIAN_POINT('Ctrl Pts',(4.4361893134968,-6.55419258023866,21.3368069465427));
#240590=CARTESIAN_POINT('Ctrl Pts',(4.22056204148704,-6.69114201294729,
21.326699399606));
#240591=CARTESIAN_POINT('Ctrl Pts',(4.19974845360624,-6.7042254057345,21.3257216406511));
#240592=CARTESIAN_POINT('Ctrl Pts',(4.16310891011882,-6.72701939555684,
21.323997103028));
#240593=CARTESIAN_POINT('Ctrl Pts',(4.14730904376409,-6.73677173677074,
21.3232523632811));
#240594=CARTESIAN_POINT('Ctrl Pts',(4.12455559772059,-6.75070573765319,
21.3221784515565));
#240595=CARTESIAN_POINT('Ctrl Pts',(4.11762961466437,-6.75493250823952,
21.3218513737654));
#240596=CARTESIAN_POINT('Ctrl Pts',(4.10560263412475,-6.76224693163935,
21.3212830922317));
#240597=CARTESIAN_POINT('Ctrl Pts',(4.10050461781171,-6.76533949132353,
21.321042111575));
#240598=CARTESIAN_POINT('Ctrl Pts',(4.09069745398288,-6.77127355748216,
21.320578352336));
#240599=CARTESIAN_POINT('Ctrl Pts',(4.08598882880483,-6.77411592320258,
21.3203556123759));
#240600=CARTESIAN_POINT('Ctrl Pts',(4.07489255655459,-6.78079841915755,
21.3198305256301));
#240601=CARTESIAN_POINT('Ctrl Pts',(4.06850244610479,-6.78463443335356,
21.3195279979531));
#240602=CARTESIAN_POINT('Ctrl Pts',(4.04961328853411,-6.79593740371535,
21.3186333273905));
#240603=CARTESIAN_POINT('Ctrl Pts',(4.0370990743449,-6.80337886952804,21.3180400858648));
#240604=CARTESIAN_POINT('Ctrl Pts',(3.92584616496902,-6.86911937608084,
21.3127619211503));
#240605=CARTESIAN_POINT('Ctrl Pts',(3.82587388177438,-6.92529831198529,
21.3079899667837));
#240606=CARTESIAN_POINT('Ctrl Pts',(3.32852948085659,-7.1907221540629,21.2842108497175));
#240607=CARTESIAN_POINT('Ctrl Pts',(2.91506385306577,-7.3680378635069,21.264368070567));
#240608=CARTESIAN_POINT('Ctrl Pts',(1.90821527390292,-7.70173633795492,
21.2179821260291));
#240609=CARTESIAN_POINT('Ctrl Pts',(1.30722648202128,-7.82619369685106,
21.1918798392884));
#240610=CARTESIAN_POINT('Ctrl Pts',(0.659868975158418,-7.88352391502151,
21.1655687150648));
#240611=CARTESIAN_POINT('Ctrl Pts',(0.621844084298277,-7.88661437812317,
21.1640288870407));
#240612=CARTESIAN_POINT('Ctrl Pts',(0.566609848015124,-7.89070157449081,
21.1618002867522));
#240613=CARTESIAN_POINT('Ctrl Pts',(0.54941733552787,-7.89191729883797,
21.1611077483324));
#240614=CARTESIAN_POINT('Ctrl Pts',(0.519366456113566,-7.89394359452179,
21.1598992689248));
#240615=CARTESIAN_POINT('Ctrl Pts',(0.506509844379948,-7.89477895624264,
21.1593828905884));
#240616=CARTESIAN_POINT('Ctrl Pts',(0.481625998817894,-7.89633475535607,
21.1583846913591));
#240617=CARTESIAN_POINT('Ctrl Pts',(0.469599049334774,-7.89705913015734,
21.1579028011264));
#240618=CARTESIAN_POINT('Ctrl Pts',(0.440994627876495,-7.89871637793553,
21.15675803145));
#240619=CARTESIAN_POINT('Ctrl Pts',(0.424415764088776,-7.89962454440719,
21.156095602503));
#240620=CARTESIAN_POINT('Ctrl Pts',(0.374570164154309,-7.90219764570721,
21.1541071703505));
#240621=CARTESIAN_POINT('Ctrl Pts',(0.341295539876163,-7.90370468924481,
21.1527840834318));
#240622=CARTESIAN_POINT('Ctrl Pts',(-0.0430653294796413,-7.9186810113998,
21.137550164931));
#240623=CARTESIAN_POINT('Ctrl Pts',(-0.394673749012077,-7.90895805574895,
21.1241172264983));
#240624=CARTESIAN_POINT('Ctrl Pts',(-1.22661763511753,-7.83031644154327,
21.0929999943611));
#240625=CARTESIAN_POINT('Ctrl Pts',(-1.70352733113975,-7.74057019691383,
21.0757346401214));
#240626=CARTESIAN_POINT('Ctrl Pts',(-2.35957022404099,-7.55351072474762,
21.0505783273413));
#240627=CARTESIAN_POINT('Ctrl Pts',(-2.54780071400087,-7.49211599380507,
21.0431770401856));
#240628=CARTESIAN_POINT('Ctrl Pts',(-2.82831680165654,-7.38882596620705,
21.0316340986691));
#240629=CARTESIAN_POINT('Ctrl Pts',(-2.92243036539303,-7.3521102206016,
21.0276713870739));
#240630=CARTESIAN_POINT('Ctrl Pts',(-3.02777372924851,-7.30867119591772,
21.0231082142334));
#240631=CARTESIAN_POINT('Ctrl Pts',(-3.03972304191331,-7.30370948430901,
21.0225887320002));
#240632=CARTESIAN_POINT('Ctrl Pts',(-3.05762491173799,-7.29622455096867,
21.0218075861669));
#240633=CARTESIAN_POINT('Ctrl Pts',(-3.06358667334252,-7.29372329428451,
21.0215469649109));
#240634=CARTESIAN_POINT('Ctrl Pts',(-3.07382205823133,-7.28941427593686,
21.0210986838954));
#240635=CARTESIAN_POINT('Ctrl Pts',(-3.07809717625586,-7.28761005442125,
21.0209111948495));
#240636=CARTESIAN_POINT('Ctrl Pts',(-3.08688651943401,-7.28389158752044,
21.0205252096201));
#240637=CARTESIAN_POINT('Ctrl Pts',(-3.09140055723503,-7.28197690446732,
21.0203266921194));
#240638=CARTESIAN_POINT('Ctrl Pts',(-3.10224204459045,-7.27736646051384,
21.0198492208686));
#240639=CARTESIAN_POINT('Ctrl Pts',(-3.10856775602569,-7.27466664593997,
21.0195700671702));
#240640=CARTESIAN_POINT('Ctrl Pts',(-3.12788425322536,-7.26639256658187,
21.0187158886257));
#240641=CARTESIAN_POINT('Ctrl Pts',(-3.14086357467296,-7.26079174983371,
21.0181395319606));
#240642=CARTESIAN_POINT('Ctrl Pts',(-3.32727219984936,-7.17975962895686,
21.0098263157074));
#240643=CARTESIAN_POINT('Ctrl Pts',(-3.49793586214657,-7.0981770012961,
21.0017503046371));
#240644=CARTESIAN_POINT('Ctrl Pts',(-4.3628255608543,-6.64596714814462,
20.9588999972478));
#240645=CARTESIAN_POINT('Ctrl Pts',(-5.00188316938379,-6.17936010600693,
20.921150105005));
#240646=CARTESIAN_POINT('Ctrl Pts',(-5.79638767176517,-5.39396087513738,
20.8719180164918));
#240647=CARTESIAN_POINT('Ctrl Pts',(-6.0164388465983,-5.14737023493961,
20.8578863960726));
#240648=CARTESIAN_POINT('Ctrl Pts',(-6.23627549657994,-4.86759127089052,
20.843439056477));
#240649=CARTESIAN_POINT('Ctrl Pts',(-6.25200031230084,-4.84737753430764,
20.8424029459769));
#240650=CARTESIAN_POINT('Ctrl Pts',(-6.27415780221411,-4.81860762444148,
20.8409390696484));
#240651=CARTESIAN_POINT('Ctrl Pts',(-6.28067161431032,-4.81011430630571,
20.8405082368316));
#240652=CARTESIAN_POINT('Ctrl Pts',(-6.29183353018156,-4.79549902624557,
20.8397691288665));
#240653=CARTESIAN_POINT('Ctrl Pts',(-6.29648997761467,-4.78938347226887,
20.8394605394564));
#240654=CARTESIAN_POINT('Ctrl Pts',(-6.30534908190281,-4.77771310077262,
20.838872946654));
#240655=CARTESIAN_POINT('Ctrl Pts',(-6.30955332805746,-4.77215950263993,
20.838593883651));
#240656=CARTESIAN_POINT('Ctrl Pts',(-6.31932595889826,-4.75921485744452,
20.8379447176215));
#240657=CARTESIAN_POINT('Ctrl Pts',(-6.32488872616406,-4.75181957112347,
20.8375748253926));
#240658=CARTESIAN_POINT('Ctrl Pts',(-6.34381227697357,-4.72657001203405,
20.8363152275862));
#240659=CARTESIAN_POINT('Ctrl Pts',(-6.35711059236594,-4.70866894255109,
20.8354278577297));
#240660=CARTESIAN_POINT('Ctrl Pts',(-6.48670944749926,-4.53266412410689,
20.8267578671421));
#240661=CARTESIAN_POINT('Ctrl Pts',(-6.59716769700055,-4.37033501285362,
20.8191948236975));
#240662=CARTESIAN_POINT('Ctrl Pts',(-6.79249251988921,-4.05897749541245,
20.8053948962966));
#240663=CARTESIAN_POINT('Ctrl Pts',(-6.87877337749367,-3.91097596847907,
20.7991151281128));
#240664=CARTESIAN_POINT('Ctrl Pts',(-7.27285164837035,-3.18154810208835,
20.7692686341362));
#240665=CARTESIAN_POINT('Ctrl Pts',(-7.51209847467027,-2.56611210108341,
20.7475807677498));
#240666=CARTESIAN_POINT('Ctrl Pts',(-7.69850281660668,-1.82439868890262,
20.7201608877691));
#240667=CARTESIAN_POINT('Ctrl Pts',(-7.72247993861398,-1.72008104818995,
20.7162714700308));
#240668=CARTESIAN_POINT('Ctrl Pts',(-7.77886662927705,-1.44974476356953,
20.7060467822104));
#240669=CARTESIAN_POINT('Ctrl Pts',(-7.80808139873681,-1.28311773366718,
20.6995979093381));
#240670=CARTESIAN_POINT('Ctrl Pts',(-7.83641435877223,-1.08422341681566,
20.6916404810625));
#240671=CARTESIAN_POINT('Ctrl Pts',(-7.84070546545657,-1.05274317164936,
20.6903741640498));
#240672=CARTESIAN_POINT('Ctrl Pts',(-7.8461316237566,-1.0110612587017,20.6886891386515));
#240673=CARTESIAN_POINT('Ctrl Pts',(-7.84743665606868,-1.00088173822597,
20.688276965953));
#240674=CARTESIAN_POINT('Ctrl Pts',(-7.84954405022219,-0.984186113947172,
20.6875999053313));
#240675=CARTESIAN_POINT('Ctrl Pts',(-7.85035811775608,-0.977671481597511,
20.6873354546936));
#240676=CARTESIAN_POINT('Ctrl Pts',(-7.85191795538473,-0.96506120789022,
20.6868230643658));
#240677=CARTESIAN_POINT('Ctrl Pts',(-7.85266473937148,-0.958965694821149,
20.6865751620137));
#240678=CARTESIAN_POINT('Ctrl Pts',(-7.85436999721802,-0.944911218397947,
20.6860030619439));
#240679=CARTESIAN_POINT('Ctrl Pts',(-7.85532347176574,-0.936951662157876,
20.685678684521));
#240680=CARTESIAN_POINT('Ctrl Pts',(-7.85825297630143,-0.912177502636292,
20.6846679122884));
#240681=CARTESIAN_POINT('Ctrl Pts',(-7.86018712173715,-0.895358052431021,
20.6839800459206));
#240682=CARTESIAN_POINT('Ctrl Pts',(-7.87669600195275,-0.747618598424283,
20.677924197034));
#240683=CARTESIAN_POINT('Ctrl Pts',(-7.88805225089174,-0.616362931133154,
20.6724497875655));
#240684=CARTESIAN_POINT('Ctrl Pts',(-7.89678816775971,-0.474103779083254,
20.6664506830004));
#240685=CARTESIAN_POINT('Ctrl Pts',(-7.89742837317041,-0.463317223575977,
20.6659953998199));
#240686=CARTESIAN_POINT('Ctrl Pts',(-7.89965501296814,-0.424455429701931,
20.6643536841128));
#240687=CARTESIAN_POINT('Ctrl Pts',(-7.90111384649708,-0.396373191349824,
20.6631646787213));
#240688=CARTESIAN_POINT('Ctrl Pts',(-7.90320411514384,-0.351521415326295,
20.6612618393129));
#240689=CARTESIAN_POINT('Ctrl Pts',(-7.90393197432876,-0.334756528885346,
20.6605497382605));
#240690=CARTESIAN_POINT('Ctrl Pts',(-7.90652966255593,-0.270183001643106,
20.6578038828691));
#240691=CARTESIAN_POINT('Ctrl Pts',(-7.90801909469223,-0.222360306165593,
20.6557638993645));
#240692=CARTESIAN_POINT('Ctrl Pts',(-7.91035932368518,-0.116307885784508,
20.6512286090017));
#240693=CARTESIAN_POINT('Ctrl Pts',(-7.91100115241832,-0.058076311635061,
20.6487307575025));
#240694=CARTESIAN_POINT('Ctrl Pts',(-7.91098990207056,0.509701392572241,
20.6243222131824));
#240695=CARTESIAN_POINT('Ctrl Pts',(-7.86174935620109,1.01808176974271,
20.6021719372389));
#240696=CARTESIAN_POINT('Ctrl Pts',(-7.72218697327911,1.73179727208443,
20.5714613976149));
#240697=CARTESIAN_POINT('Ctrl Pts',(-7.67161952798435,1.94359224450184,
20.5623790039317));
#240698=CARTESIAN_POINT('Ctrl Pts',(-7.52853977103367,2.44947207946064,
20.5406577788275));
#240699=CARTESIAN_POINT('Ctrl Pts',(-7.42745184572128,2.74076434054692,
20.5280969872044));
#240700=CARTESIAN_POINT('Ctrl Pts',(-7.28674470831208,3.0807231404329,20.5131880115792));
#240701=CARTESIAN_POINT('Ctrl Pts',(-7.26322761146261,3.13576597123713,
20.5107675700267));
#240702=CARTESIAN_POINT('Ctrl Pts',(-7.22683103870119,3.21834705753255,
20.5071262829839));
#240703=CARTESIAN_POINT('Ctrl Pts',(-7.21441384196527,3.24608650047917,
20.5059014531776));
#240704=CARTESIAN_POINT('Ctrl Pts',(-7.19249609564274,3.29430272263465,
20.5037694715243));
#240705=CARTESIAN_POINT('Ctrl Pts',(-7.18306718945709,3.31481164908821,
20.5028616727524));
#240706=CARTESIAN_POINT('Ctrl Pts',(-7.16311649284448,3.35772178959058,
20.5009602886571));
#240707=CARTESIAN_POINT('Ctrl Pts',(-7.15257709330927,3.38011455939787,
20.4999668817465));
#240708=CARTESIAN_POINT('Ctrl Pts',(-7.12712478262492,3.43354026409209,
20.4975939258901));
#240709=CARTESIAN_POINT('Ctrl Pts',(-7.11211400439904,3.46452605875132,
20.4962153582619));
#240710=CARTESIAN_POINT('Ctrl Pts',(-7.05974677432867,3.57084971029093,
20.4914767851592));
#240711=CARTESIAN_POINT('Ctrl Pts',(-7.02139152913762,3.64568969192213,
20.488127152778));
#240712=CARTESIAN_POINT('Ctrl Pts',(-6.794709943032,4.07114602618178,20.4689938297933));
#240713=CARTESIAN_POINT('Ctrl Pts',(-6.58132920444999,4.4077692635504,20.4535252145148));
#240714=CARTESIAN_POINT('Ctrl Pts',(-6.07770338931803,5.0836360648932,20.4209235739589));
#240715=CARTESIAN_POINT('Ctrl Pts',(-5.78227693877506,5.4172948688147,20.4038682580775));
#240716=CARTESIAN_POINT('Ctrl Pts',(-5.43067096644422,5.75268811631658,
20.3844964289683));
#240717=CARTESIAN_POINT('Ctrl Pts',(-5.40073321443414,5.78080344028513,
20.3828533478669));
#240718=CARTESIAN_POINT('Ctrl Pts',(-5.36003351456923,5.81843346260337,
20.3806268234898));
#240719=CARTESIAN_POINT('Ctrl Pts',(-5.34946244625771,5.82815397619461,
20.3800491689768));
#240720=CARTESIAN_POINT('Ctrl Pts',(-5.33155952207037,5.84452667620866,
20.3790718879354));
#240721=CARTESIAN_POINT('Ctrl Pts',(-5.32424152873898,5.85119399347706,
20.3786727015414));
#240722=CARTESIAN_POINT('Ctrl Pts',(-5.31015726583092,5.86397766060507,
20.3779049480101));
#240723=CARTESIAN_POINT('Ctrl Pts',(-5.30339289395329,5.87009608130744,
20.3775364432053));
#240724=CARTESIAN_POINT('Ctrl Pts',(-5.28745394057272,5.88446293520925,
20.3766686488264));
#240725=CARTESIAN_POINT('Ctrl Pts',(-5.27827062417996,5.89270162371462,
20.3761690657088));
#240726=CARTESIAN_POINT('Ctrl Pts',(-5.25074663988041,5.91727843165131,
20.3746728468169));
#240727=CARTESIAN_POINT('Ctrl Pts',(-5.23234925248312,5.93355252751604,
20.3736741869352));
#240728=CARTESIAN_POINT('Ctrl Pts',(-5.20041874966383,5.96153386469735,
20.3719435995793));
#240729=CARTESIAN_POINT('Ctrl Pts',(-5.18692108728663,5.97328141160708,
20.371212872831));
#240730=CARTESIAN_POINT('Ctrl Pts',(-4.92616107393042,6.19868081592559,
20.3571131048857));
#240731=CARTESIAN_POINT('Ctrl Pts',(-4.6659401344634,6.39685080528621,20.3433501424095));
#240732=CARTESIAN_POINT('Ctrl Pts',(-4.22688785360173,6.69012952596437,
20.3210782471044));
#240733=CARTESIAN_POINT('Ctrl Pts',(-4.05535217828034,6.79547891472674,
20.3125871545781));
#240734=CARTESIAN_POINT('Ctrl Pts',(-3.66934621425892,7.01271999203399,
20.2940113076679));
#240735=CARTESIAN_POINT('Ctrl Pts',(-3.45338060462254,7.1215525131337,20.2839607745937));
#240736=CARTESIAN_POINT('Ctrl Pts',(-3.11605419996019,7.27258412732115,
20.2687891367996));
#240737=CARTESIAN_POINT('Ctrl Pts',(-2.99808990153073,7.32200323538005,
20.2635769678611));
#240738=CARTESIAN_POINT('Ctrl Pts',(-2.84418133791662,7.38213716835213,
20.2568896004129));
#240739=CARTESIAN_POINT('Ctrl Pts',(-2.80928855997919,7.39548608686989,
20.2553808606657));
#240740=CARTESIAN_POINT('Ctrl Pts',(-2.75336477497699,7.41642793229259,
20.2529741741643));
#240741=CARTESIAN_POINT('Ctrl Pts',(-2.73239394819534,7.42417969710052,
20.252074243437));
#240742=CARTESIAN_POINT('Ctrl Pts',(-2.6944823315391,7.43801115243769,20.2504518366645));
#240743=CARTESIAN_POINT('Ctrl Pts',(-2.67755313412428,7.44412212116101,
20.2497289782724));
#240744=CARTESIAN_POINT('Ctrl Pts',(-2.63761052865143,7.45838640624921,
20.2480272157248));
#240745=CARTESIAN_POINT('Ctrl Pts',(-2.61457991838856,7.46649107286388,
20.2470489118075));
#240746=CARTESIAN_POINT('Ctrl Pts',(-2.54709021940113,7.48989071556468,
20.2441903745017));
#240747=CARTESIAN_POINT('Ctrl Pts',(-2.50253174316113,7.50489616354739,
20.2423136242906));
#240748=CARTESIAN_POINT('Ctrl Pts',(-2.11147629759914,7.63271743287569,
20.2259297004352));
#240749=CARTESIAN_POINT('Ctrl Pts',(-1.75769280324902,7.72186717236216,
20.2116741168259));
#240750=CARTESIAN_POINT('Ctrl Pts',(-1.05124290684691,7.84880033087584,
20.183826940435));
#240751=CARTESIAN_POINT('Ctrl Pts',(-0.699659541783445,7.88791894207995,
20.1703455207084));
#240752=CARTESIAN_POINT('Ctrl Pts',(0.129790875696725,7.92429752897928,
20.1390689469837));
#240753=CARTESIAN_POINT('Ctrl Pts',(0.60711348199341,7.90207113504019,20.1215101104165));
#240754=CARTESIAN_POINT('Ctrl Pts',(1.2804445546505,7.80932282080689,20.0955806383408));
#240755=CARTESIAN_POINT('Ctrl Pts',(1.48023232260705,7.77392870705506,20.0877260389873));
#240756=CARTESIAN_POINT('Ctrl Pts',(1.69832461855102,7.72657937933853,20.078815728932));
#240757=CARTESIAN_POINT('Ctrl Pts',(1.7182015154207,7.72218356162564,20.0780005242406));
#240758=CARTESIAN_POINT('Ctrl Pts',(1.74688754589496,7.71572334644354,20.0768192951148));
#240759=CARTESIAN_POINT('Ctrl Pts',(1.75571053092691,7.71372046341466,20.0764553349855));
#240760=CARTESIAN_POINT('Ctrl Pts',(1.77119188624082,7.7101781435857,20.0758155446941));
#240761=CARTESIAN_POINT('Ctrl Pts',(1.77785174240546,7.70864520427608,20.0755399378421));
#240762=CARTESIAN_POINT('Ctrl Pts',(1.79153785927188,7.70547630867441,20.0749727708743));
#240763=CARTESIAN_POINT('Ctrl Pts',(1.79856388391593,7.70383936747289,20.0746811765623));
#240764=CARTESIAN_POINT('Ctrl Pts',(1.81638704340427,7.69966117077797,20.0739403733921));
#240765=CARTESIAN_POINT('Ctrl Pts',(1.82718107198305,7.69710681782101,20.0734906990327));
#240766=CARTESIAN_POINT('Ctrl Pts',(1.87004883197118,7.68686712228251,20.0717006473563));
#240767=CARTESIAN_POINT('Ctrl Pts',(1.90207947157292,7.67900400001702,20.070353777417));
#240768=CARTESIAN_POINT('Ctrl Pts',(2.46169666275869,7.53790878499424,20.046646234895));
#240769=CARTESIAN_POINT('Ctrl Pts',(2.97408131709752,7.35082264186398,20.021718839324));
#240770=CARTESIAN_POINT('Ctrl Pts',(3.63914852300124,7.02700920951749,19.9877996600801));
#240771=CARTESIAN_POINT('Ctrl Pts',(3.81195453103858,6.93478660606003,19.9788308465271));
#240772=CARTESIAN_POINT('Ctrl Pts',(4.40715840068742,6.58816312596132,19.9476401985171));
#240773=CARTESIAN_POINT('Ctrl Pts',(4.80907306980818,6.3007827118657,19.9261110866259));
#240774=CARTESIAN_POINT('Ctrl Pts',(5.20597165233274,5.95674536766719,19.9047430027069));
#240775=CARTESIAN_POINT('Ctrl Pts',(5.23015543593674,5.93552275436501,19.9034401261152));
#240776=CARTESIAN_POINT('Ctrl Pts',(5.26289629957581,5.90643535197804,19.9016749546935));
#240777=CARTESIAN_POINT('Ctrl Pts',(5.27156634752686,5.89869852359713,19.9012073983207));
#240778=CARTESIAN_POINT('Ctrl Pts',(5.28588804470872,5.88586157922251,19.9004348482886));
#240779=CARTESIAN_POINT('Ctrl Pts',(5.29154942121424,5.88077237055003,19.9001294034453));
#240780=CARTESIAN_POINT('Ctrl Pts',(5.30250135960793,5.87089867161536,19.8995384106328));
#240781=CARTESIAN_POINT('Ctrl Pts',(5.30779281242425,5.86611518312908,19.8992528214901));
#240782=CARTESIAN_POINT('Ctrl Pts',(5.32000810743495,5.85504246188589,19.8985934229701));
#240783=CARTESIAN_POINT('Ctrl Pts',(5.32692728560109,5.84874808727013,19.8982198288159));
#240784=CARTESIAN_POINT('Ctrl Pts',(5.34867987139071,5.82888914455127,19.897045036568));
#240785=CARTESIAN_POINT('Ctrl Pts',(5.36347280722148,5.81528025806648,19.8962456988135));
#240786=CARTESIAN_POINT('Ctrl Pts',(5.55471542991089,5.63799450291346,19.8859061386516));
#240787=CARTESIAN_POINT('Ctrl Pts',(5.72366545121628,5.4663983630254,19.8767136597119));
#240788=CARTESIAN_POINT('Ctrl Pts',(6.01433522197778,5.14289878850957,19.8606421727424));
#240789=CARTESIAN_POINT('Ctrl Pts',(6.13877234309855,4.99370752062864,19.8536635454289));
#240790=CARTESIAN_POINT('Ctrl Pts',(6.68840670977723,4.28310191560628,19.8220239499397));
#240791=CARTESIAN_POINT('Ctrl Pts',(7.04287989768205,3.67116140114844,19.7994587090832));
#240792=CARTESIAN_POINT('Ctrl Pts',(7.38858744289925,2.83430188987769,19.7663505689866));
#240793=CARTESIAN_POINT('Ctrl Pts',(7.45834846080899,2.64528243095303,19.7587173697232));
#240794=CARTESIAN_POINT('Ctrl Pts',(7.52510778228723,2.44066901551668,19.7501031695655));
#240795=CARTESIAN_POINT('Ctrl Pts',(7.529364245289,2.42750621741429,19.7495474851352));
#240796=CARTESIAN_POINT('Ctrl Pts',(7.5351873985636,2.40933588313313,19.7487782106013));
#240797=CARTESIAN_POINT('Ctrl Pts',(7.53678368682007,2.40433778555811,19.7485663786761));
#240798=CARTESIAN_POINT('Ctrl Pts',(7.53950948225137,2.39577372866259,19.7482030162123));
#240799=CARTESIAN_POINT('Ctrl Pts',(7.54064143641804,2.39220854425085,19.7480516322639));
#240800=CARTESIAN_POINT('Ctrl Pts',(7.54283997961578,2.38526698285068,19.7477566505204));
#240801=CARTESIAN_POINT('Ctrl Pts',(7.54390683117187,2.38189069020287,19.7476130686374));
#240802=CARTESIAN_POINT('Ctrl Pts',(7.5464548006046,2.37380818194039,19.7472690912954));
#240803=CARTESIAN_POINT('Ctrl Pts',(7.54793378186227,2.36910129936091,19.7470685665204));
#240804=CARTESIAN_POINT('Ctrl Pts',(7.55236531638669,2.3549515945079,19.7464651211991));
#240805=CARTESIAN_POINT('Ctrl Pts',(7.55530451978847,2.34550474263469,19.7460613899193));
#240806=CARTESIAN_POINT('Ctrl Pts',(7.58491040271362,2.24971580938813,19.7419589228398));
#240807=CARTESIAN_POINT('Ctrl Pts',(7.61011251564614,2.16293164540803,19.7381708867654));
#240808=CARTESIAN_POINT('Ctrl Pts',(7.70610953898764,1.80988899206583,19.7225352516025));
#240809=CARTESIAN_POINT('Ctrl Pts',(7.76445621658028,1.54046147382365,19.7100927972623));
#240810=CARTESIAN_POINT('Ctrl Pts',(7.85179929363146,1.00282120593915,19.6850298083011));
#240811=CARTESIAN_POINT('Ctrl Pts',(7.88137679948177,0.735052137332435,
19.6724368488032));
#240812=CARTESIAN_POINT('Ctrl Pts',(7.9327023936629,-0.134201643794408,
19.6320814850932));
#240813=CARTESIAN_POINT('Ctrl Pts',(7.8995584229053,-0.736869550851738,
19.6051076769524));
#240814=CARTESIAN_POINT('Ctrl Pts',(7.79288191539919,-1.36234608977134,
19.5792690619989));
#240815=CARTESIAN_POINT('Ctrl Pts',(7.78717026582562,-1.3946234987114,19.5779411194538));
#240816=CARTESIAN_POINT('Ctrl Pts',(7.77844040197462,-1.44223090068032,
19.575990409465));
#240817=CARTESIAN_POINT('Ctrl Pts',(7.77557715980859,-1.45758872585251,
19.5753623448484));
#240818=CARTESIAN_POINT('Ctrl Pts',(7.77115432439072,-1.48092795160832,
19.5744097190642));
#240819=CARTESIAN_POINT('Ctrl Pts',(7.76962789451794,-1.4889155491938,19.574084021512));
#240820=CARTESIAN_POINT('Ctrl Pts',(7.76686189660701,-1.50326955208913,
19.5734993185415));
#240821=CARTESIAN_POINT('Ctrl Pts',(7.76562681162257,-1.50963680734525,
19.5732401595628));
#240822=CARTESIAN_POINT('Ctrl Pts',(7.76319898613434,-1.52207119880334,
19.5727344614775));
#240823=CARTESIAN_POINT('Ctrl Pts',(7.76200696038873,-1.52813846874612,
19.5724878980501));
#240824=CARTESIAN_POINT('Ctrl Pts',(7.7586895288115,-1.54491977237181,19.571806453356));
#240825=CARTESIAN_POINT('Ctrl Pts',(7.75654904106625,-1.55563083101748,
19.5713720905621));
#240826=CARTESIAN_POINT('Ctrl Pts',(7.74794361033847,-1.59823329491209,
19.5696467546712));
#240827=CARTESIAN_POINT('Ctrl Pts',(7.741304066329,-1.63008933534529,19.5683617908376));
#240828=CARTESIAN_POINT('Ctrl Pts',(7.69805515450783,-1.83136893724368,
19.5602746442576));
#240829=CARTESIAN_POINT('Ctrl Pts',(7.65608133562765,-1.99959713998963,
19.5536597971191));
#240830=CARTESIAN_POINT('Ctrl Pts',(7.55758499850289,-2.34553917490843,
19.5402900474365));
#240831=CARTESIAN_POINT('Ctrl Pts',(7.50023952415913,-2.52290640362542,
19.5335663882337));
#240832=CARTESIAN_POINT('Ctrl Pts',(7.2970620125559,-3.08291992399194,19.5125484767092));
#240833=CARTESIAN_POINT('Ctrl Pts',(7.12777901090042,-3.4563393659593,19.4988903193199));
#240834=CARTESIAN_POINT('Ctrl Pts',(6.72646949039652,-4.18536610419681,
19.4707186353078));
#240835=CARTESIAN_POINT('Ctrl Pts',(6.49323210775315,-4.53878300446091,
19.4562236048039));
#240836=CARTESIAN_POINT('Ctrl Pts',(6.18342529954361,-4.93514221662879,
19.436907695107));
#240837=CARTESIAN_POINT('Ctrl Pts',(6.13298329429413,-4.99768868428522,
19.4337601095561));
#240838=CARTESIAN_POINT('Ctrl Pts',(6.07555114854313,-5.06672366219893,
19.4301593403808));
#240839=CARTESIAN_POINT('Ctrl Pts',(6.06949019508079,-5.07398257761095,
19.4297791355549));
#240840=CARTESIAN_POINT('Ctrl Pts',(6.06036919511765,-5.08486663782468,
19.4292066322581));
#240841=CARTESIAN_POINT('Ctrl Pts',(6.05731886417883,-5.08849994430902,
19.4290151129272));
#240842=CARTESIAN_POINT('Ctrl Pts',(6.05202012415163,-5.09479985699783,
19.4286823220164));
#240843=CARTESIAN_POINT('Ctrl Pts',(6.04977322970132,-5.09746770809901,
19.4285411729235));
#240844=CARTESIAN_POINT('Ctrl Pts',(6.04508707958194,-5.10302434791125,
19.4282467270026));
#240845=CARTESIAN_POINT('Ctrl Pts',(6.04264751654127,-5.10591287487736,
19.4280934055184));
#240846=CARTESIAN_POINT('Ctrl Pts',(6.03688645936826,-5.11272425403975,
19.4277312528581));
#240847=CARTESIAN_POINT('Ctrl Pts',(6.03356321438374,-5.11664561592186,
19.4275222821108));
#240848=CARTESIAN_POINT('Ctrl Pts',(6.02264114149838,-5.12950800419541,
19.4268352830302));
#240849=CARTESIAN_POINT('Ctrl Pts',(6.01502627570537,-5.1384353244905,19.4263559866161));
#240850=CARTESIAN_POINT('Ctrl Pts',(5.72222632904747,-5.48015784994654,
19.4079154140099));
#240851=CARTESIAN_POINT('Ctrl Pts',(5.40992645708177,-5.78866253848166,
19.3878720113857));
#240852=CARTESIAN_POINT('Ctrl Pts',(4.80768315451328,-6.29208633658248,
19.3512012394283));
#240853=CARTESIAN_POINT('Ctrl Pts',(4.52728564901074,-6.49675774905601,
19.3347707410609));
#240854=CARTESIAN_POINT('Ctrl Pts',(3.76992160943709,-6.97667045242813,
19.2932178707207));
#240855=CARTESIAN_POINT('Ctrl Pts',(3.27601230682214,-7.22178302922347,
19.2688527421055));
#240856=CARTESIAN_POINT('Ctrl Pts',(2.72690199471424,-7.42625204076528,
19.2449859721987));
#240857=CARTESIAN_POINT('Ctrl Pts',(2.69312042686586,-7.43856950458513,
19.24352938245));
#240858=CARTESIAN_POINT('Ctrl Pts',(2.64808853795734,-7.4546420898588,19.241603020218));
#240859=CARTESIAN_POINT('Ctrl Pts',(2.63691235046668,-7.45860274115461,
19.2411261774669));
#240860=CARTESIAN_POINT('Ctrl Pts',(2.61869056275803,-7.46501415817808,
19.2403507503374));
#240861=CARTESIAN_POINT('Ctrl Pts',(2.61165034658844,-7.46748010461694,
19.2400516453995));
#240862=CARTESIAN_POINT('Ctrl Pts',(2.59820613460645,-7.47216781323428,
19.2394813990162));
#240863=CARTESIAN_POINT('Ctrl Pts',(2.59180275285883,-7.47439130883709,
19.2392101984106));
#240864=CARTESIAN_POINT('Ctrl Pts',(2.57728878662772,-7.47941021109845,
19.238596403636));
#240865=CARTESIAN_POINT('Ctrl Pts',(2.56917649076423,-7.48220066260464,
19.2382539789761));
#240866=CARTESIAN_POINT('Ctrl Pts',(2.54462077387564,-7.49060264541635,
19.2372194063836));
#240867=CARTESIAN_POINT('Ctrl Pts',(2.52816333949308,-7.49617322427117,
19.2365286543539));
#240868=CARTESIAN_POINT('Ctrl Pts',(2.38525232641287,-7.544022154678,19.2305529327192));
#240869=CARTESIAN_POINT('Ctrl Pts',(2.25776368119933,-7.58315265857015,
19.2253755122488));
#240870=CARTESIAN_POINT('Ctrl Pts',(1.79856115802301,-7.71148892177604,
19.2072180163425));
#240871=CARTESIAN_POINT('Ctrl Pts',(1.46209740235628,-7.78229900855084,
19.1948372757722));
#240872=CARTESIAN_POINT('Ctrl Pts',(0.884241338001069,-7.86509801106841,
19.174360975963));
#240873=CARTESIAN_POINT('Ctrl Pts',(0.644971956958332,-7.8883244275455,
19.1661003967226));
#240874=CARTESIAN_POINT('Ctrl Pts',(-0.108863998888231,-7.92696893060566,
19.1400487451691));
#240875=CARTESIAN_POINT('Ctrl Pts',(-0.62409799557544,-7.9031135359761,
19.1222036195459));
#240876=CARTESIAN_POINT('Ctrl Pts',(-1.16636529533192,-7.82461662109957,
19.1004847108101));
#240877=CARTESIAN_POINT('Ctrl Pts',(-1.19934108394442,-7.81963005435704,
19.0991536354783));
#240878=CARTESIAN_POINT('Ctrl Pts',(-1.24279745333352,-7.8127772764407,
19.0973865960682));
#240879=CARTESIAN_POINT('Ctrl Pts',(-1.25330751389175,-7.81109816577966,
19.0969582339062));
#240880=CARTESIAN_POINT('Ctrl Pts',(-1.26958487790401,-7.80846395980715,
19.0962932922865));
#240881=CARTESIAN_POINT('Ctrl Pts',(-1.27535458897554,-7.80752366925352,
19.0960572996053));
#240882=CARTESIAN_POINT('Ctrl Pts',(-1.28688445695356,-7.80563152345428,
19.0955851191524));
#240883=CARTESIAN_POINT('Ctrl Pts',(-1.29264461309927,-7.80467968525813,
19.0953489321676));
#240884=CARTESIAN_POINT('Ctrl Pts',(-1.30547020447907,-7.80254572963671,
19.0948223921611));
#240885=CARTESIAN_POINT('Ctrl Pts',(-1.3125350937906,-7.80136039066242,
19.0945319151144));
#240886=CARTESIAN_POINT('Ctrl Pts',(-1.33309320821116,-7.79788245753654,
19.0936854021472));
#240887=CARTESIAN_POINT('Ctrl Pts',(-1.34658206838306,-7.79556444739808,
19.0931284037695));
#240888=CARTESIAN_POINT('Ctrl Pts',(-1.44242276225144,-7.77883840907748,
19.0891599073342));
#240889=CARTESIAN_POINT('Ctrl Pts',(-1.52454603434658,-7.76316103261057,
19.0857020721842));
#240890=CARTESIAN_POINT('Ctrl Pts',(-1.78714767343735,-7.70870271666713,
19.0744866456546));
#240891=CARTESIAN_POINT('Ctrl Pts',(-1.96651938767471,-7.66490650605838,
19.0665852701679));
#240892=CARTESIAN_POINT('Ctrl Pts',(-2.88209025194624,-7.40710109747689,
19.025403022942));
#240893=CARTESIAN_POINT('Ctrl Pts',(-3.58598658390007,-7.09313081695239,
18.9913388361158));
#240894=CARTESIAN_POINT('Ctrl Pts',(-4.36463843130316,-6.59983967931645,
18.9531377967241));
#240895=CARTESIAN_POINT('Ctrl Pts',(-4.49312749330956,-6.51304535230898,
18.9467948813139));
#240896=CARTESIAN_POINT('Ctrl Pts',(-4.64271044466376,-6.40546756260444,
18.9393474295766));
#240897=CARTESIAN_POINT('Ctrl Pts',(-4.66634028449643,-6.38827389307354,
18.9381689667992));
#240898=CARTESIAN_POINT('Ctrl Pts',(-4.70326282439339,-6.36109394598825,
18.9363244843165));
#240899=CARTESIAN_POINT('Ctrl Pts',(-4.71662019470146,-6.35119605479172,
18.9356565719948));
#240900=CARTESIAN_POINT('Ctrl Pts',(-4.74023279045556,-6.33358340709557,
18.9344747359603));
#240901=CARTESIAN_POINT('Ctrl Pts',(-4.75050061873216,-6.32588567355723,
18.933960439506));
#240902=CARTESIAN_POINT('Ctrl Pts',(-4.7717976364832,-6.30983832387473,
18.9328929208718));
#240903=CARTESIAN_POINT('Ctrl Pts',(-4.78282375079526,-6.30148469229766,
18.932339791111));
#240904=CARTESIAN_POINT('Ctrl Pts',(-4.81125227344537,-6.27982900612894,
18.9309125160287));
#240905=CARTESIAN_POINT('Ctrl Pts',(-4.8286214787523,-6.26648349600445,
18.9300393679856));
#240906=CARTESIAN_POINT('Ctrl Pts',(-4.90184838607415,-6.20973488010401,
18.9263535163539));
#240907=CARTESIAN_POINT('Ctrl Pts',(-4.95717850641239,-6.16565538576281,
18.9235568028503));
#240908=CARTESIAN_POINT('Ctrl Pts',(-5.32964480475741,-5.86066979694523,
18.9046463678356));
#240909=CARTESIAN_POINT('Ctrl Pts',(-5.62664578650971,-5.57615010463298,
18.8891988399541));
#240910=CARTESIAN_POINT('Ctrl Pts',(-6.30534442883819,-4.81626458508839,
18.8517593036166));
#240911=CARTESIAN_POINT('Ctrl Pts',(-6.65676723491854,-4.31753312438085,
18.8304109926013));
#240912=CARTESIAN_POINT('Ctrl Pts',(-6.95766242595286,-3.76500990253246,
18.805876122935));
#240913=CARTESIAN_POINT('Ctrl Pts',(-6.96767718657558,-3.74644372882379,
18.805050503328));
#240914=CARTESIAN_POINT('Ctrl Pts',(-6.99035917066659,-3.70398849964009,
18.803159395557));
#240915=CARTESIAN_POINT('Ctrl Pts',(-7.00297837366307,-3.68007418613781,
18.8020918923767));
#240916=CARTESIAN_POINT('Ctrl Pts',(-7.02484851386608,-3.63810881640134,
18.8002138855589));
#240917=CARTESIAN_POINT('Ctrl Pts',(-7.03415313349208,-3.62008592259415,
18.7994058204276));
#240918=CARTESIAN_POINT('Ctrl Pts',(-7.05008114190442,-3.58894036751498,
18.7980064651438));
#240919=CARTESIAN_POINT('Ctrl Pts',(-7.0567374837265,-3.57583460896057,
18.7974167391941));
#240920=CARTESIAN_POINT('Ctrl Pts',(-7.06639187030768,-3.55669401855285,
18.7965540609624));
#240921=CARTESIAN_POINT('Ctrl Pts',(-7.06941881737628,-3.55067373754263,
18.7962825217044));
#240922=CARTESIAN_POINT('Ctrl Pts',(-7.0747561871207,-3.5400243868076,18.7958018244254));
#240923=CARTESIAN_POINT('Ctrl Pts',(-7.0770697703803,-3.53539689870533,
18.7955928232146));
#240924=CARTESIAN_POINT('Ctrl Pts',(-7.08185201221599,-3.52580824557546,
18.795159489854));
#240925=CARTESIAN_POINT('Ctrl Pts',(-7.08432000015436,-3.52084675080762,
18.7949351243002));
#240926=CARTESIAN_POINT('Ctrl Pts',(-7.09064142553778,-3.50810498078884,
18.7943585444258));
#240927=CARTESIAN_POINT('Ctrl Pts',(-7.09448726444883,-3.50032096177427,
18.7940059456127));
#240928=CARTESIAN_POINT('Ctrl Pts',(-7.11024318364745,-3.4682981760712,
18.7925538329663));
#240929=CARTESIAN_POINT('Ctrl Pts',(-7.12204181289879,-3.44400504570947,
18.7914485824966));
#240930=CARTESIAN_POINT('Ctrl Pts',(-7.20093438722308,-3.27942772639249,
18.7839332811853));
#240931=CARTESIAN_POINT('Ctrl Pts',(-7.26399947844926,-3.13726111848784,
18.7773026052747));
#240932=CARTESIAN_POINT('Ctrl Pts',(-7.71112719486996,-2.04341882552673,
18.7256981864378));
#240933=CARTESIAN_POINT('Ctrl Pts',(-7.91094841064365,-1.02695608467868,
18.6757941483577));
#240934=CARTESIAN_POINT('Ctrl Pts',(-7.91099999001413,-0.000397487684091757,
18.632833427413));
#240935=CARTESIAN_POINT('',(-7.91112653880827,0.00440551095844195,16.642331508237));
#240936=CARTESIAN_POINT('Ctrl Pts',(-7.911,-5.77315972805081E-14,18.642331508237));
#240937=CARTESIAN_POINT('Ctrl Pts',(-7.91100000000002,2.20167589666668,
18.5537440725043));
#240938=CARTESIAN_POINT('Ctrl Pts',(-6.94214576672377,4.38610418338673,
18.4651566367716));
#240939=CARTESIAN_POINT('Ctrl Pts',(-3.67820201488301,7.34180684107624,
18.2879817653061));
#240940=CARTESIAN_POINT('Ctrl Pts',(-1.40868175871763,8.08992666571332,
18.1993943295734));
#240941=CARTESIAN_POINT('Ctrl Pts',(2.9730927052125,7.65454228025265,18.022219458108));
#240942=CARTESIAN_POINT('Ctrl Pts',(5.0510207267558,6.47444880834242,17.9336320223752));
#240943=CARTESIAN_POINT('Ctrl Pts',(7.66951518847859,2.93425195367738,17.7564571509098));
#240944=CARTESIAN_POINT('Ctrl Pts',(8.18956872247068,0.60188196009954,17.6678697151771));
#240945=CARTESIAN_POINT('Ctrl Pts',(7.32306689761362,-3.71537198232411,
17.4906948437116));
#240946=CARTESIAN_POINT('Ctrl Pts',(5.94329958850233,-5.66643518936477,
17.4021074079789));
#240947=CARTESIAN_POINT('Ctrl Pts',(2.16154501637897,-7.92205913232984,
17.2249325365134));
#240948=CARTESIAN_POINT('Ctrl Pts',(-0.210816529299819,-8.20894963713003,
17.1363451007807));
#240949=CARTESIAN_POINT('Ctrl Pts',(-4.42123908576386,-6.91982244717863,
16.9591702293153));
#240950=CARTESIAN_POINT('Ctrl Pts',(-6.22631625634146,-5.35390358803568,
16.8705827935825));
#240951=CARTESIAN_POINT('Ctrl Pts',(-7.6531728085948,-2.3133485751456,16.7354407413122));
#240952=CARTESIAN_POINT('Ctrl Pts',(-7.91100000000001,-1.15702837836537,
16.6888861247746));
#240953=CARTESIAN_POINT('Ctrl Pts',(-7.911,5.32907051820075E-14,16.642331508237));
#240954=CARTESIAN_POINT('',(-7.91918800173243,0.000313487325539099,14.6423316599192));
#240955=CARTESIAN_POINT('Ctrl Pts',(-7.91117084713064,0.00594812703317959,
16.642331508237));
#240956=CARTESIAN_POINT('Ctrl Pts',(-7.91495777771905,0.699069697383863,
16.6145091754524));
#240957=CARTESIAN_POINT('Ctrl Pts',(-7.5015571643441,4.02599103967887,16.4807172654514));
#240958=CARTESIAN_POINT('Ctrl Pts',(-3.89567832531485,7.80704314161589,
16.2939405668419));
#240959=CARTESIAN_POINT('Ctrl Pts',(1.56115343882902,8.08629267461694,16.0820014124088));
#240960=CARTESIAN_POINT('Ctrl Pts',(5.24511136736693,6.37222732002422,15.9230470465842));
#240961=CARTESIAN_POINT('Ctrl Pts',(7.6385445361554,3.07862117984459,15.7640926807593));
#240962=CARTESIAN_POINT('Ctrl Pts',(8.40705311350932,-2.31605264250739,
15.5521535263265));
#240963=CARTESIAN_POINT('Ctrl Pts',(4.12950229334074,-8.39726041388267,
15.287229583285));
#240964=CARTESIAN_POINT('Ctrl Pts',(-4.85377709130171,-8.00864403078137,
14.9693208516356));
#240965=CARTESIAN_POINT('Ctrl Pts',(-7.87757738652791,-2.77203907481525,
14.7543548828771));
#240966=CARTESIAN_POINT('Ctrl Pts',(-7.92006828996515,-0.0745985010899101,
14.6453584913352));
#240967=CARTESIAN_POINT('Ctrl Pts',(-7.92011057934193,0.000313101301251344,
14.6423316770099));
#240968=CARTESIAN_POINT('',(-7.90467196448321,-0.00677022214583101,12.642331508237));
#240969=CARTESIAN_POINT('Ctrl Pts',(-7.91099999365225,0.000316913346238894,
14.642331508237));
#240970=CARTESIAN_POINT('Ctrl Pts',(-7.91099160947722,0.209608220964732,
14.6338653232035));
#240971=CARTESIAN_POINT('Ctrl Pts',(-7.9026734681258,0.419065023665548,
14.62539913817));
#240972=CARTESIAN_POINT('Ctrl Pts',(-7.88603207588891,0.62802794368667,
14.6169329531365));
#240973=CARTESIAN_POINT('Ctrl Pts',(-7.86941516844141,0.836683412683476,
14.6084792245583));
#240974=CARTESIAN_POINT('Ctrl Pts',(-7.84449946276681,1.0448461810492,14.60002549598));
#240975=CARTESIAN_POINT('Ctrl Pts',(-7.81132342387363,1.25185756683547,
14.5915717674017));
#240976=CARTESIAN_POINT('Ctrl Pts',(-7.77822011466537,1.45841513494589,
14.583136571386));
#240977=CARTESIAN_POINT('Ctrl Pts',(-7.73689265527382,1.66382609268568,
14.5747013753703));
#240978=CARTESIAN_POINT('Ctrl Pts',(-7.68743107903436,1.86743792536636,
14.5662661793546));
#240979=CARTESIAN_POINT('Ctrl Pts',(-7.63803532221137,2.07077880808887,
14.5578422082072));
#240980=CARTESIAN_POINT('Ctrl Pts',(-7.5805271015822,2.27232508058972,14.5494182370598));
#240981=CARTESIAN_POINT('Ctrl Pts',(-7.51504765843897,2.47143272038529,
14.5409942659124));
#240982=CARTESIAN_POINT('Ctrl Pts',(-7.44970173420307,2.67013436047726,
14.5325874720556));
#240983=CARTESIAN_POINT('Ctrl Pts',(-7.37641710833143,2.86640703628315,
14.5241806781988));
#240984=CARTESIAN_POINT('Ctrl Pts',(-7.29538505604854,3.05962054575133,
14.515773884342));
#240985=CARTESIAN_POINT('Ctrl Pts',(-7.2204712854315,3.23824557277003,14.5080018409484));
#240986=CARTESIAN_POINT('Ctrl Pts',(-7.13893640916405,3.41425589335646,
14.5002297975548));
#240987=CARTESIAN_POINT('Ctrl Pts',(-7.05096979243143,3.58716405900532,
14.4924577541612));
#240988=CARTESIAN_POINT('Ctrl Pts',(-6.96161669767182,3.76279750137008,
14.4845632123951));
#240989=CARTESIAN_POINT('Ctrl Pts',(-6.86570200825127,3.93508139648814,
14.476668670629));
#240990=CARTESIAN_POINT('Ctrl Pts',(-6.76351680122221,4.10350599848287,
14.4687741288628));
#240991=CARTESIAN_POINT('Ctrl Pts',(-6.66130856596594,4.27196855626507,
14.4608778080006));
#240992=CARTESIAN_POINT('Ctrl Pts',(-6.55282717441282,4.43656979476182,
14.4529814871384));
#240993=CARTESIAN_POINT('Ctrl Pts',(-6.43840766156614,4.59682801325941,
14.4450851662761));
#240994=CARTESIAN_POINT('Ctrl Pts',(-6.3239434998463,4.75714876784627,14.4371857641053));
#240995=CARTESIAN_POINT('Ctrl Pts',(-6.20353679781398,4.91312284650394,
14.4292863619345));
#240996=CARTESIAN_POINT('Ctrl Pts',(-6.07756374070671,5.06430054179717,
14.4213869597637));
#240997=CARTESIAN_POINT('Ctrl Pts',(-5.95145206467407,5.21564459083414,
14.4134788652053));
#240998=CARTESIAN_POINT('Ctrl Pts',(-5.81976201597311,5.36218144894817,
14.4055707706468));
#240999=CARTESIAN_POINT('Ctrl Pts',(-5.68290844638268,5.50349639684014,
14.3976626760884));
#241000=CARTESIAN_POINT('Ctrl Pts',(-5.54597334162283,5.64489553791941,
14.3897498700137));
#241001=CARTESIAN_POINT('Ctrl Pts',(-5.40386882865687,5.78106632889452,
14.3818370639389));
#241002=CARTESIAN_POINT('Ctrl Pts',(-5.25704413753824,5.91163327143817,
14.3739242578641));
#241003=CARTESIAN_POINT('Ctrl Pts',(-5.11001369598899,6.04238318187674,
14.3660003633052));
#241004=CARTESIAN_POINT('Ctrl Pts',(-4.95825012312907,6.16751333505882,
14.3580764687463));
#241005=CARTESIAN_POINT('Ctrl Pts',(-4.80223411572721,6.28668978857282,
14.3501525741874));
#241006=CARTESIAN_POINT('Ctrl Pts',(-4.69296379485831,6.3701584629246,14.3446028455705));
#241007=CARTESIAN_POINT('Ctrl Pts',(-4.58160814846415,6.45070756604176,
14.3390531169535));
#241008=CARTESIAN_POINT('Ctrl Pts',(-4.4683397720312,6.5282356484493,14.3335033883366));
#241009=CARTESIAN_POINT('Ctrl Pts',(-4.30252118821672,6.64173243577439,
14.3253788952627));
#241010=CARTESIAN_POINT('Ctrl Pts',(-4.13223745152282,6.74900267259293,
14.3172544021888));
#241011=CARTESIAN_POINT('Ctrl Pts',(-3.95798447766342,6.84969195472143,
14.3091299091149));
#241012=CARTESIAN_POINT('Ctrl Pts',(-3.7838854558489,6.95029227813353,14.3010125940094));
#241013=CARTESIAN_POINT('Ctrl Pts',(-3.60582446489278,7.04432307928305,
14.2928952789038));
#241014=CARTESIAN_POINT('Ctrl Pts',(-3.4243263340565,7.13147321090721,14.2847779637982));
#241015=CARTESIAN_POINT('Ctrl Pts',(-3.24296271382359,7.21855875444589,
14.2766666645394));
#241016=CARTESIAN_POINT('Ctrl Pts',(-3.05816732094315,7.2987736578556,14.2685553652807));
#241017=CARTESIAN_POINT('Ctrl Pts',(-2.87049002626376,7.37185241368276,
14.2604440660219));
#241018=CARTESIAN_POINT('Ctrl Pts',(-2.68292513480602,7.44488740136202,
14.2523376247624));
#241019=CARTESIAN_POINT('Ctrl Pts',(-2.49248208156313,7.51079464820408,
14.244231183503));
#241020=CARTESIAN_POINT('Ctrl Pts',(-2.29973171106852,7.56935631722446,
14.2361247422435));
#241021=CARTESIAN_POINT('Ctrl Pts',(-2.10706940378885,7.627891230764,14.2280220046308));
#241022=CARTESIAN_POINT('Ctrl Pts',(-1.91210218797431,7.67908716653114,
14.2199192670181));
#241023=CARTESIAN_POINT('Ctrl Pts',(-1.71541765013888,7.72277562056493,
14.2118165294053));
#241024=CARTESIAN_POINT('Ctrl Pts',(-1.51695690455812,7.76685861385071,
14.2036406180421));
#241025=CARTESIAN_POINT('Ctrl Pts',(-1.31674797921391,7.80329775242719,
14.1954647066788));
#241026=CARTESIAN_POINT('Ctrl Pts',(-1.11540787354316,7.83197205534072,
14.1872887953156));
#241027=CARTESIAN_POINT('Ctrl Pts',(-0.915945814777616,7.86037889199031,
14.1791891466769));
#241028=CARTESIAN_POINT('Ctrl Pts',(-0.715373913618147,7.88116510167342,
14.1710894980383));
#241029=CARTESIAN_POINT('Ctrl Pts',(-0.514300307894198,7.89426476584742,
14.1629898493996));
#241030=CARTESIAN_POINT('Ctrl Pts',(-0.313228068651659,7.90736434099706,
14.1548902558056));
#241031=CARTESIAN_POINT('Ctrl Pts',(-0.111654451680012,7.91277745408288,
14.1467906622115));
#241032=CARTESIAN_POINT('Ctrl Pts',(0.0898090014107483,7.91049020878388,
14.1386910686175));
#241033=CARTESIAN_POINT('Ctrl Pts',(0.291297095913608,7.90820268372717,
14.1305904843454));
#241034=CARTESIAN_POINT('Ctrl Pts',(0.492674678992804,7.89821292611473,
14.1224899000733));
#241035=CARTESIAN_POINT('Ctrl Pts',(0.693331375740398,7.88055915550502,
14.1143893158012));
#241036=CARTESIAN_POINT('Ctrl Pts',(0.897265327583533,7.86261705208298,
14.1061564275417));
#241037=CARTESIAN_POINT('Ctrl Pts',(1.10045429902011,7.83675844239101,14.0979235392822));
#241038=CARTESIAN_POINT('Ctrl Pts',(1.30226408393771,7.80307819105293,14.0896906510227));
#241039=CARTESIAN_POINT('Ctrl Pts',(1.50102036219682,7.76990754271434,14.0815823314461));
#241040=CARTESIAN_POINT('Ctrl Pts',(1.69843858236954,7.72915036219104,14.0734740118696));
#241041=CARTESIAN_POINT('Ctrl Pts',(1.89392397681129,7.68094870247545,14.065365692293));
#241042=CARTESIAN_POINT('Ctrl Pts',(2.09391425501415,7.63163625453585,14.057070519692));
#241043=CARTESIAN_POINT('Ctrl Pts',(2.29188120657217,7.57453217548862,14.048775347091));
#241044=CARTESIAN_POINT('Ctrl Pts',(2.48720496812253,7.50984237161784,14.04048017449));
#241045=CARTESIAN_POINT('Ctrl Pts',(2.68252872967288,7.44515256774706,14.032185001889));
#241046=CARTESIAN_POINT('Ctrl Pts',(2.87520897606093,7.37287718975586,14.023889829288));
#241047=CARTESIAN_POINT('Ctrl Pts',(3.06464797065199,7.2932745605783,14.015594656687));
#241048=CARTESIAN_POINT('Ctrl Pts',(3.24341785300369,7.21815511284434,14.0077666641812));
#241049=CARTESIAN_POINT('Ctrl Pts',(3.41964401130501,7.13636638325002,13.9999386716753));
#241050=CARTESIAN_POINT('Ctrl Pts',(3.5927892581542,7.04810516000519,13.9921106791695));
#241051=CARTESIAN_POINT('Ctrl Pts',(3.76578826356659,6.95991848369906,13.9842892983201));
#241052=CARTESIAN_POINT('Ctrl Pts',(3.93571122723641,6.86527035761309,13.9764679174706));
#241053=CARTESIAN_POINT('Ctrl Pts',(4.10204015953403,6.76440592584227,13.9686465366211));
#241054=CARTESIAN_POINT('Ctrl Pts',(4.26825798031597,6.66360887380953,13.9608303806322));
#241055=CARTESIAN_POINT('Ctrl Pts',(4.43088625131069,6.5566039679859,13.9530142246434));
#241056=CARTESIAN_POINT('Ctrl Pts',(4.58943072520149,6.44368269071162,13.9451980686545));
#241057=CARTESIAN_POINT('Ctrl Pts',(4.74789903371938,6.33081566125173,13.9373856675769));
#241058=CARTESIAN_POINT('Ctrl Pts',(4.90228716674321,6.21203812559488,13.9295732664993));
#241059=CARTESIAN_POINT('Ctrl Pts',(5.05212892981133,6.087685461369,13.9217608654217));
#241060=CARTESIAN_POINT('Ctrl Pts',(5.20192689577287,5.96336914406521,13.9139507478234));
#241061=CARTESIAN_POINT('Ctrl Pts',(5.34718086868082,5.83348116963574,13.9061406302251));
#241062=CARTESIAN_POINT('Ctrl Pts',(5.48745675924078,5.69839796043262,13.8983305126268));
#241063=CARTESIAN_POINT('Ctrl Pts',(5.62774064229124,5.56330705460207,13.8905199500319));
#241064=CARTESIAN_POINT('Ctrl Pts',(5.76304561808925,5.42302056223409,13.882709387437));
#241065=CARTESIAN_POINT('Ctrl Pts',(5.89297326897815,5.27795292240363,13.8748988248421));
#241066=CARTESIAN_POINT('Ctrl Pts',(5.99421601557345,5.16491273274382,13.8688126468488));
#241067=CARTESIAN_POINT('Ctrl Pts',(6.09219438355787,5.04897027525893,13.8627264688555));
#241068=CARTESIAN_POINT('Ctrl Pts',(6.18673635657413,4.93033611980399,13.8566402908622));
#241069=CARTESIAN_POINT('Ctrl Pts',(6.32095478386334,4.76191473763961,13.8479999249761));
#241070=CARTESIAN_POINT('Ctrl Pts',(6.44818247280803,4.58814793997287,13.8393595590899));
#241071=CARTESIAN_POINT('Ctrl Pts',(6.56804077931242,4.40962144875148,13.8307191932037));
#241072=CARTESIAN_POINT('Ctrl Pts',(6.68809846894754,4.23079798044293,13.8220644541526));
#241073=CARTESIAN_POINT('Ctrl Pts',(6.80076214391928,4.04719918287814,13.8134097151016));
#241074=CARTESIAN_POINT('Ctrl Pts',(6.90569788511941,3.85943748744002,13.8047549760505));
#241075=CARTESIAN_POINT('Ctrl Pts',(7.01387917710065,3.66586852261663,13.7958325551328));
#241076=CARTESIAN_POINT('Ctrl Pts',(7.11384676695315,3.46787530176986,13.786910134215));
#241077=CARTESIAN_POINT('Ctrl Pts',(7.20528795746181,3.26615162692362,13.7779877132972));
#241078=CARTESIAN_POINT('Ctrl Pts',(7.29428345054031,3.06982327852086,13.7693039325567));
#241079=CARTESIAN_POINT('Ctrl Pts',(7.37520271079234,2.86996167315181,13.7606201518162));
#241080=CARTESIAN_POINT('Ctrl Pts',(7.44780754301474,2.66722398800941,13.7519363710757));
#241081=CARTESIAN_POINT('Ctrl Pts',(7.52340527036207,2.45612910940026,13.7428946300693));
#241082=CARTESIAN_POINT('Ctrl Pts',(7.58998853841794,2.24191630478465,13.7338528890629));
#241083=CARTESIAN_POINT('Ctrl Pts',(7.64734627763182,2.02534340544778,13.7248111480566));
#241084=CARTESIAN_POINT('Ctrl Pts',(7.7047040168457,1.80877050611091,13.7157694070502));
#241085=CARTESIAN_POINT('Ctrl Pts',(7.75283618695792,1.58983778856473,13.7067276660438));
#241086=CARTESIAN_POINT('Ctrl Pts',(7.79159140450717,1.36931529795366,13.6976859250375));
#241087=CARTESIAN_POINT('Ctrl Pts',(7.82726160143207,1.16634699680898,13.6893639311838));
#241088=CARTESIAN_POINT('Ctrl Pts',(7.85501855400681,0.961859510919619,
13.6810419373302));
#241089=CARTESIAN_POINT('Ctrl Pts',(7.87474800181552,0.756481928338384,
13.6727199434766));
#241090=CARTESIAN_POINT('Ctrl Pts',(7.89445990191067,0.551287012146152,
13.6644053513488));
#241091=CARTESIAN_POINT('Ctrl Pts',(7.90615851249631,0.345203868562909,
13.6560907592211));
#241092=CARTESIAN_POINT('Ctrl Pts',(7.90978105619522,0.13886915804202,13.6477761670933));
#241093=CARTESIAN_POINT('Ctrl Pts',(7.91340059886103,-0.0672946180895682,
13.6394684630443));
#241094=CARTESIAN_POINT('Ctrl Pts',(7.90895741685068,-0.273709253870452,
13.6311607589952));
#241095=CARTESIAN_POINT('Ctrl Pts',(7.89644068938977,-0.479734758954975,
13.6228530549462));
#241096=CARTESIAN_POINT('Ctrl Pts',(7.88393659074577,-0.685552393540713,
13.6145537329981));
#241097=CARTESIAN_POINT('Ctrl Pts',(7.8633752240688,-0.890981390013255,
13.60625441105));
#241098=CARTESIAN_POINT('Ctrl Pts',(7.83479781068352,-1.095383159314,13.5979550891019));
#241099=CARTESIAN_POINT('Ctrl Pts',(7.80623865543539,-1.29965433612594,
13.5896610695987));
#241100=CARTESIAN_POINT('Ctrl Pts',(7.76967370946852,-1.50289930603503,
13.5813670500955));
#241101=CARTESIAN_POINT('Ctrl Pts',(7.72519601193587,-1.70448454882117,
13.5730730305923));
#241102=CARTESIAN_POINT('Ctrl Pts',(7.68075129684107,-1.90592030606487,
13.5647851615194));
#241103=CARTESIAN_POINT('Ctrl Pts',(7.6284056039201,-2.10569850763858,13.5564972924466));
#241104=CARTESIAN_POINT('Ctrl Pts',(7.56830315791786,-2.30319523919501,
13.5482094233737));
#241105=CARTESIAN_POINT('Ctrl Pts',(7.54539245095782,-2.37847985809532,
13.5450501353201));
#241106=CARTESIAN_POINT('Ctrl Pts',(7.52135514613833,-2.45343306631481,
13.5418908472664));
#241107=CARTESIAN_POINT('Ctrl Pts',(7.49620117606039,-2.52802075308548,
13.5387315592127));
#241108=CARTESIAN_POINT('Ctrl Pts',(7.43169130684809,-2.71930832731386,
13.530629249378));
#241109=CARTESIAN_POINT('Ctrl Pts',(7.3598604819201,-2.90811028686713,13.5225269395432));
#241110=CARTESIAN_POINT('Ctrl Pts',(7.28093271431342,-3.09385516946747,
13.5144246297084));
#241111=CARTESIAN_POINT('Ctrl Pts',(7.20198752547956,-3.27964105036152,
13.5063205315021));
#241112=CARTESIAN_POINT('Ctrl Pts',(7.11594239453415,-3.46236821501396,
13.4982164332957));
#241113=CARTESIAN_POINT('Ctrl Pts',(7.02306894780017,-3.64148644847747,
13.4901123350893));
#241114=CARTESIAN_POINT('Ctrl Pts',(6.93016335187538,-3.82066668573718,
13.4820054315579));
#241115=CARTESIAN_POINT('Ctrl Pts',(6.83042487268483,-3.99623521722305,
13.4738985280265));
#241116=CARTESIAN_POINT('Ctrl Pts',(6.72417070117546,-4.16766713899437,
13.4657916244951));
#241117=CARTESIAN_POINT('Ctrl Pts',(6.61782070445251,-4.33925366646526,
13.4576774097613));
#241118=CARTESIAN_POINT('Ctrl Pts',(6.50494344117653,-4.50669585802107,
13.4495631950274));
#241119=CARTESIAN_POINT('Ctrl Pts',(6.38589973895333,-4.66949735239628,
13.4414489802936));
#241120=CARTESIAN_POINT('Ctrl Pts',(6.26679785622839,-4.83237841311937,
13.4333307998809));
#241121=CARTESIAN_POINT('Ctrl Pts',(6.14152371665662,-4.99061399937773,
13.4252126194683));
#241122=CARTESIAN_POINT('Ctrl Pts',(6.01047851030768,-5.14374076690588,
13.4170944390557));
#241123=CARTESIAN_POINT('Ctrl Pts',(5.87929237717569,-5.29703220785743,
13.4089675283042));
#241124=CARTESIAN_POINT('Ctrl Pts',(5.74232298845278,-5.44520361406672,
13.4008406175528));
#241125=CARTESIAN_POINT('Ctrl Pts',(5.60000942884617,-5.58782743083875,
13.3927137068013));
#241126=CARTESIAN_POINT('Ctrl Pts',(5.52449728862179,-5.66350419474794,
13.3884015356635));
#241127=CARTESIAN_POINT('Ctrl Pts',(5.44748114347228,-5.73761973610153,
13.3840893645257));
#241128=CARTESIAN_POINT('Ctrl Pts',(5.36903041219186,-5.81011475213347,
13.3797771933879));
#241129=CARTESIAN_POINT('Ctrl Pts',(5.22352776130406,-5.94457133190829,
13.3717794052043));
#241130=CARTESIAN_POINT('Ctrl Pts',(5.07283573485256,-6.07368435372215,
13.3637816170206));
#241131=CARTESIAN_POINT('Ctrl Pts',(4.91737977091784,-6.19703938897987,
13.355783828837));
#241132=CARTESIAN_POINT('Ctrl Pts',(4.76205073661163,-6.32029370498307,
13.3477925708389));
#241133=CARTESIAN_POINT('Ctrl Pts',(4.60196577737757,-6.43779919678073,
13.3398013128408));
#241134=CARTESIAN_POINT('Ctrl Pts',(4.437585495946,-6.54917979339166,13.3318100548426));
#241135=CARTESIAN_POINT('Ctrl Pts',(4.273311556453,-6.66048833495768,13.3238239666));
#241136=CARTESIAN_POINT('Ctrl Pts',(4.10474810912281,-6.76567969161241,
13.3158378783574));
#241137=CARTESIAN_POINT('Ctrl Pts',(3.93238732758968,-6.86441919653893,
13.3078517901148));
#241138=CARTESIAN_POINT('Ctrl Pts',(3.76010883571297,-6.96311156057955,
13.2998695146447));
#241139=CARTESIAN_POINT('Ctrl Pts',(3.58403691314571,-7.05535804693963,
13.2918872391747));
#241140=CARTESIAN_POINT('Ctrl Pts',(3.40469144528709,-7.14086809585424,
13.2839049637046));
#241141=CARTESIAN_POINT('Ctrl Pts',(3.22540121283494,-7.22635180910302,
13.275925146642));
#241142=CARTESIAN_POINT('Ctrl Pts',(3.04283974672231,-7.30510307728589,
13.2679453295794));
#241143=CARTESIAN_POINT('Ctrl Pts',(2.85755055253053,-7.37687778397694,
13.2599655125168));
#241144=CARTESIAN_POINT('Ctrl Pts',(2.66589388806462,-7.45111903121981,
13.2517114687343));
#241145=CARTESIAN_POINT('Ctrl Pts',(2.47131902410358,-7.51789553407416,
13.2434574249519));
#241146=CARTESIAN_POINT('Ctrl Pts',(2.27444941787763,-7.57699154318626,
13.2352033811695));
#241147=CARTESIAN_POINT('Ctrl Pts',(2.08409473330921,-7.63413191335023,
13.2272224849268));
#241148=CARTESIAN_POINT('Ctrl Pts',(1.89159509497252,-7.68409190491757,
13.2192415886842));
#241149=CARTESIAN_POINT('Ctrl Pts',(1.69752906883348,-7.72672738359943,
13.2112606924416));
#241150=CARTESIAN_POINT('Ctrl Pts',(1.50341995755849,-7.769372327902,13.203278024338));
#241151=CARTESIAN_POINT('Ctrl Pts',(1.30774409210163,-7.80468944529393,
13.1952953562345));
#241152=CARTESIAN_POINT('Ctrl Pts',(1.11109022321741,-7.83258574902763,
13.187312688131));
#241153=CARTESIAN_POINT('Ctrl Pts',(0.914362465654845,-7.86049253422821,
13.1793270207028));
#241154=CARTESIAN_POINT('Ctrl Pts',(0.716656303351637,-7.88097290013038,
13.1713413532747));
#241155=CARTESIAN_POINT('Ctrl Pts',(0.518565978983622,-7.89398570593086,
13.1633556858465));
#241156=CARTESIAN_POINT('Ctrl Pts',(0.320370771139717,-7.90700540166051,
13.1553657902231));
#241157=CARTESIAN_POINT('Ctrl Pts',(0.121791329243065,-7.91254963283518,
13.1473758945998));
#241158=CARTESIAN_POINT('Ctrl Pts',(-0.0765773490314934,-7.91062936242214,
13.1393859989764));
#241159=CARTESIAN_POINT('Ctrl Pts',(-0.275181011409237,-7.90870681729001,
13.131386638661));
#241160=CARTESIAN_POINT('Ctrl Pts',(-0.473573076801867,-7.89930211007153,
13.1233872783456));
#241161=CARTESIAN_POINT('Ctrl Pts',(-0.671161645071544,-7.88247822998484,
13.1153879180301));
#241162=CARTESIAN_POINT('Ctrl Pts',(-0.868888338898598,-7.86564258905674,
13.1073829657105));
#241163=CARTESIAN_POINT('Ctrl Pts',(-1.06581008426671,-7.84137747212006,
13.0993780133909));
#241164=CARTESIAN_POINT('Ctrl Pts',(-1.26134392584015,-7.80979721252391,
13.0913730610712));
#241165=CARTESIAN_POINT('Ctrl Pts',(-1.45713295507633,-7.77817573810493,
13.0833576616338));
#241166=CARTESIAN_POINT('Ctrl Pts',(-1.65153013554003,-7.73922011694579,
13.0753422621964));
#241167=CARTESIAN_POINT('Ctrl Pts',(-1.84396530479523,-7.69309514790448,
13.067326862759));
#241168=CARTESIAN_POINT('Ctrl Pts',(-1.88764740001141,-7.68262494488855,
13.0655073957521));
#241169=CARTESIAN_POINT('Ctrl Pts',(-1.93122847039918,-7.6717855238411,
13.0636879287453));
#241170=CARTESIAN_POINT('Ctrl Pts',(-1.97470198113393,-7.6605791612453,
13.0618684617384));
#241171=CARTESIAN_POINT('Ctrl Pts',(-2.16013496408955,-7.61277926634147,
13.0541076623741));
#241172=CARTESIAN_POINT('Ctrl Pts',(-2.34416056971887,-7.55815743266138,
13.0463468630099));
#241173=CARTESIAN_POINT('Ctrl Pts',(-2.52622540524093,-7.49680640018904,
13.0385860636456));
#241174=CARTESIAN_POINT('Ctrl Pts',(-2.70806921584986,-7.43552984726451,
13.0308346858152));
#241175=CARTESIAN_POINT('Ctrl Pts',(-2.8879566586254,-7.36754046866688,
13.0230833079847));
#241176=CARTESIAN_POINT('Ctrl Pts',(-3.06534398242874,-7.29298205601714,
13.0153319301543));
#241177=CARTESIAN_POINT('Ctrl Pts',(-3.24255196739692,-7.21849902202799,
13.0075883889778));
#241178=CARTESIAN_POINT('Ctrl Pts',(-3.4172645371924,-7.13746031240183,
12.9998448478013));
#241179=CARTESIAN_POINT('Ctrl Pts',(-3.58895248720248,-7.05005964830108,
12.9921013066248));
#241180=CARTESIAN_POINT('Ctrl Pts',(-3.76050165929437,-6.96272963145433,
12.9843640246675));
#241181=CARTESIAN_POINT('Ctrl Pts',(-3.92903076112556,-6.869048060348,12.9766267427103));
#241182=CARTESIAN_POINT('Ctrl Pts',(-4.09402990757578,-6.76925698403267,
12.9688894607531));
#241183=CARTESIAN_POINT('Ctrl Pts',(-4.2589290905073,-6.66952636540659,
12.9611568663712));
#241184=CARTESIAN_POINT('Ctrl Pts',(-4.4203022703938,-6.56369379713786,
12.9534242719893));
#241185=CARTESIAN_POINT('Ctrl Pts',(-4.57766347511734,-6.45204759038374,
12.9456916776074));
#241186=CARTESIAN_POINT('Ctrl Pts',(-4.73496118197615,-6.34044643473193,
12.937962203456));
#241187=CARTESIAN_POINT('Ctrl Pts',(-4.88824984562933,-6.22303652024753,
12.9302327293046));
#241188=CARTESIAN_POINT('Ctrl Pts',(-5.03707177534301,-6.10014991045653,
12.9225032551532));
#241189=CARTESIAN_POINT('Ctrl Pts',(-5.1858913050233,-5.97726528244313,
12.9147739056541));
#241190=CARTESIAN_POINT('Ctrl Pts',(-5.33024396038324,-5.84890435506099,
12.907044556155));
#241191=CARTESIAN_POINT('Ctrl Pts',(-5.46970419884377,-5.71544022601504,
12.8993152066559));
#241192=CARTESIAN_POINT('Ctrl Pts',(-5.60917007550081,-5.58197070118749,
12.8915855446693));
#241193=CARTESIAN_POINT('Ctrl Pts',(-5.74374288107121,-5.44339781157549,
12.8838558826826));
#241194=CARTESIAN_POINT('Ctrl Pts',(-5.87303322717905,-5.30013223537403,
12.876126220696));
#241195=CARTESIAN_POINT('Ctrl Pts',(-6.00235249070338,-5.15683461601961,
12.8683948298729));
#241196=CARTESIAN_POINT('Ctrl Pts',(-6.12638670121882,-5.00884248660251,
12.8606634390499));
#241197=CARTESIAN_POINT('Ctrl Pts',(-6.24478610264365,-4.85660040895159,
12.8529320482268));
#241198=CARTESIAN_POINT('Ctrl Pts',(-6.36323368715811,-4.7042963758044,
12.8451975110847));
#241199=CARTESIAN_POINT('Ctrl Pts',(-6.47604167612806,-4.54773923373394,
12.8374629739425));
#241200=CARTESIAN_POINT('Ctrl Pts',(-6.582903036094,-4.38740340262716,12.8297284368004));
#241201=CARTESIAN_POINT('Ctrl Pts',(-6.68989024165548,-4.22687875155628,
12.8219847910578));
#241202=CARTESIAN_POINT('Ctrl Pts',(-6.79091663303328,-4.06256682320184,
12.8142411453152));
#241203=CARTESIAN_POINT('Ctrl Pts',(-6.88572012340353,-3.89496846998222,
12.8064974995726));
#241204=CARTESIAN_POINT('Ctrl Pts',(-6.98058435577491,-3.72726273401415,
12.7987488923614));
#241205=CARTESIAN_POINT('Ctrl Pts',(-7.06921758044806,-3.55626669639221,
12.7910002851502));
#241206=CARTESIAN_POINT('Ctrl Pts',(-7.15140552479671,-3.38250203546237,
12.783251677939));
#241207=CARTESIAN_POINT('Ctrl Pts',(-7.23371799966124,-3.20847408770819,
12.7754913301002));
#241208=CARTESIAN_POINT('Ctrl Pts',(-7.30956554881387,-3.03166946694644,
12.7677309822614));
#241209=CARTESIAN_POINT('Ctrl Pts',(-7.37878310472328,-2.8526270161818,
12.7599706344225));
#241210=CARTESIAN_POINT('Ctrl Pts',(-7.42638559578358,-2.72949544139617,
12.7546336663113));
#241211=CARTESIAN_POINT('Ctrl Pts',(-7.47085339602555,-2.60530576544274,
12.7492966982001));
#241212=CARTESIAN_POINT('Ctrl Pts',(-7.51214685623806,-2.48023599891473,
12.7439597300889));
#241213=CARTESIAN_POINT('Ctrl Pts',(-7.58953553677097,-2.24584091174236,
12.7339576397326));
#241214=CARTESIAN_POINT('Ctrl Pts',(-7.65597446903994,-2.00774751142973,
12.7239555493762));
#241215=CARTESIAN_POINT('Ctrl Pts',(-7.71116937423448,-1.76685819517815,
12.7139534590199));
#241216=CARTESIAN_POINT('Ctrl Pts',(-7.76593347273457,-1.52784906568836,
12.7040294368742));
#241217=CARTESIAN_POINT('Ctrl Pts',(-7.80962837999544,-1.28608735383261,
12.6941054147285));
#241218=CARTESIAN_POINT('Ctrl Pts',(-7.84201276806946,-1.04247625653326,
12.6841813925827));
#241219=CARTESIAN_POINT('Ctrl Pts',(-7.87386998810044,-0.802830773317237,
12.6744189182582));
#241220=CARTESIAN_POINT('Ctrl Pts',(-7.89478191907505,-0.561395526168362,
12.6646564439336));
#241221=CARTESIAN_POINT('Ctrl Pts',(-7.90456362223255,-0.319053196313435,
12.6548939696091));
#241222=CARTESIAN_POINT('Ctrl Pts',(-7.90875934364808,-0.215103926243778,
12.6507064961259));
#241223=CARTESIAN_POINT('Ctrl Pts',(-7.91090782873707,-0.110988063861366,
12.6465190226428));
#241224=CARTESIAN_POINT('Ctrl Pts',(-7.91099709751604,-0.00677665793934715,
12.6423315491596));
#241225=CARTESIAN_POINT('',(-7.90222559779306,0.00578867911134829,10.6423315007885));
#241226=CARTESIAN_POINT('Ctrl Pts',(-7.90467196448321,-0.00677022214583101,
12.642331508237));
#241227=CARTESIAN_POINT('Ctrl Pts',(-7.88763856955293,1.78596353784846,
12.5702380049711));
#241228=CARTESIAN_POINT('Ctrl Pts',(-6.82905835000328,4.91048047638214,
12.4451597130971));
#241229=CARTESIAN_POINT('Ctrl Pts',(-3.14753813267382,7.60142069635078,
12.2670966326146));
#241230=CARTESIAN_POINT('Ctrl Pts',(2.24296169861674,8.43405333923742,12.0551574781816));
#241231=CARTESIAN_POINT('Ctrl Pts',(7.112990747597,5.05288013614879,11.8432183237487));
#241232=CARTESIAN_POINT('Ctrl Pts',(8.23030514357243,-0.295633148393404,
11.6312791693155));
#241233=CARTESIAN_POINT('Ctrl Pts',(7.10478066087843,-4.19983146691073,
11.4723248034909));
#241234=CARTESIAN_POINT('Ctrl Pts',(4.21961160578687,-7.07249030027441,
11.313370437666));
#241235=CARTESIAN_POINT('Ctrl Pts',(-0.992041909284247,-8.66363251511341,
11.1014312832332));
#241236=CARTESIAN_POINT('Ctrl Pts',(-6.62199532390963,-5.88691039012652,
10.87775164009));
#241237=CARTESIAN_POINT('Ctrl Pts',(-7.89102930427202,-1.61035822570545,
10.7070567855553));
#241238=CARTESIAN_POINT('Ctrl Pts',(-7.90039148196552,0.00578714936241065,
10.642331508237));
#241239=CARTESIAN_POINT('Ctrl Pts',(-7.91099787678106,0.00579599565279081,
10.6423314651635));
#241240=CARTESIAN_POINT('Ctrl Pts',(-7.91084011201517,0.22113030623056,
10.6337190262862));
#241241=CARTESIAN_POINT('Ctrl Pts',(-7.90188645289187,0.436110537192641,
10.625106587409));
#241242=CARTESIAN_POINT('Ctrl Pts',(-7.88424739306299,0.650049263501995,
10.6164941485317));
#241243=CARTESIAN_POINT('Ctrl Pts',(-7.86650936761889,0.865188313290822,
10.6078333887507));
#241244=CARTESIAN_POINT('Ctrl Pts',(-7.83998829271854,1.07927392276559,
10.5991726289697));
#241245=CARTESIAN_POINT('Ctrl Pts',(-7.80484642310435,1.29162429202741,
10.5905118691887));
#241246=CARTESIAN_POINT('Ctrl Pts',(-7.76960354634283,1.50458501313636,
10.581826216064));
#241247=CARTESIAN_POINT('Ctrl Pts',(-7.72569036399297,1.71580030444112,
10.5731405629392));
#241248=CARTESIAN_POINT('Ctrl Pts',(-7.67331901160124,1.92460290610788,
10.5644549098145));
#241249=CARTESIAN_POINT('Ctrl Pts',(-7.62072078907441,2.13431003042467,
10.5557316308656));
#241250=CARTESIAN_POINT('Ctrl Pts',(-7.55959107197527,2.34158331837183,
10.5470083519167));
#241251=CARTESIAN_POINT('Ctrl Pts',(-7.49019186016789,2.54577039378547,
10.5382850729678));
#241252=CARTESIAN_POINT('Ctrl Pts',(-7.43798576035897,2.69937171808185,
10.5317229181592));
#241253=CARTESIAN_POINT('Ctrl Pts',(-7.38110100282061,2.8512270490789,10.5251607633507));
#241254=CARTESIAN_POINT('Ctrl Pts',(-7.31966593697622,3.00106840493015,
10.5185986085422));
#241255=CARTESIAN_POINT('Ctrl Pts',(-7.24557212977723,3.1817846844406,10.510684316818));
#241256=CARTESIAN_POINT('Ctrl Pts',(-7.16467709171961,3.3600106342992,10.5027700250937));
#241257=CARTESIAN_POINT('Ctrl Pts',(-7.0771675753867,3.53519732262503,10.4948557333695));
#241258=CARTESIAN_POINT('Ctrl Pts',(-6.98975853982763,3.71018285689646,
10.4869505290472));
#241259=CARTESIAN_POINT('Ctrl Pts',(-6.89575030608029,3.88213577507176,
10.479045324725));
#241260=CARTESIAN_POINT('Ctrl Pts',(-6.79537842180121,4.05052504059888,
10.4711401204028));
#241261=CARTESIAN_POINT('Ctrl Pts',(-6.69510314731133,4.21875222835326,
10.4632425249855));
#241262=CARTESIAN_POINT('Ctrl Pts',(-6.58847659906755,4.38342230214607,
10.4553449295682));
#241263=CARTESIAN_POINT('Ctrl Pts',(-6.47578128375428,4.54402660258254,
10.4474473341509));
#241264=CARTESIAN_POINT('Ctrl Pts',(-6.3631735186266,4.70450613353527,10.4395558741789));
#241265=CARTESIAN_POINT('Ctrl Pts',(-6.24450657656139,4.86092590298295,
10.4316644142069));
#241266=CARTESIAN_POINT('Ctrl Pts',(-6.12010767000815,5.0128039167224,10.4237729542349));
#241267=CARTESIAN_POINT('Ctrl Pts',(-5.99578231786302,5.16459212824641,
10.4158861603141));
#241268=CARTESIAN_POINT('Ctrl Pts',(-5.86573197233401,5.31184366896547,
10.4079993663934));
#241269=CARTESIAN_POINT('Ctrl Pts',(-5.73032590167918,5.45410726522175,
10.4001125724726));
#241270=CARTESIAN_POINT('Ctrl Pts',(-5.59497476743434,5.59631314286015,
10.3922289783503));
#241271=CARTESIAN_POINT('Ctrl Pts',(-5.45427247593998,5.73353485970938,
10.384345384228));
#241272=CARTESIAN_POINT('Ctrl Pts',(-5.30862732871614,5.86535564862082,
10.3764617901058));
#241273=CARTESIAN_POINT('Ctrl Pts',(-5.16299386279386,5.99716586499746,
10.3685788282781));
#241274=CARTESIAN_POINT('Ctrl Pts',(-5.01241858207212,6.12357578017002,
10.3606958664505));
#241275=CARTESIAN_POINT('Ctrl Pts',(-4.85734564250934,6.24420645952674,
10.3528129046228));
#241276=CARTESIAN_POINT('Ctrl Pts',(-4.70227232770731,6.36483743078073,
10.3449299237203));
#241277=CARTESIAN_POINT('Ctrl Pts',(-4.54270160435299,6.47968892606496,
10.3370469428177));
#241278=CARTESIAN_POINT('Ctrl Pts',(-4.37910968259495,6.58842313363396,
10.3291639619152));
#241279=CARTESIAN_POINT('Ctrl Pts',(-4.21548985849375,6.69717588697919,
10.3212796364864));
#241280=CARTESIAN_POINT('Ctrl Pts',(-4.0478477567119,6.79980908269741,10.3133953110575));
#241281=CARTESIAN_POINT('Ctrl Pts',(-3.87668765577041,6.89602884416802,
10.3055109856287));
#241282=CARTESIAN_POINT('Ctrl Pts',(-3.70546958249056,6.99228119550355,
10.2976239897599));
#241283=CARTESIAN_POINT('Ctrl Pts',(-3.53073143644949,7.08211561553676,
10.2897369938911));
#241284=CARTESIAN_POINT('Ctrl Pts',(-3.35300132737368,7.16528457904013,
10.2818499980222));
#241285=CARTESIAN_POINT('Ctrl Pts',(-3.17509761438337,7.24853478065056,
10.2739552982626));
#241286=CARTESIAN_POINT('Ctrl Pts',(-2.99419641350989,7.32510637492556,
10.2660605985029));
#241287=CARTESIAN_POINT('Ctrl Pts',(-2.81084599246224,7.39479991660755,
10.2581658987433));
#241288=CARTESIAN_POINT('Ctrl Pts',(-2.62739306749653,7.46453242117299,
10.2502667853714));
#241289=CARTESIAN_POINT('Ctrl Pts',(-2.44148851844214,7.52737909640816,
10.2423676719995));
#241290=CARTESIAN_POINT('Ctrl Pts',(-2.25369520558157,7.58319055017996,
10.2344685586277));
#241291=CARTESIAN_POINT('Ctrl Pts',(-2.06567266421524,7.63907012978627,
10.226559803262));
#241292=CARTESIAN_POINT('Ctrl Pts',(-1.87575708710941,7.68789724919696,
10.2186510478964));
#241293=CARTESIAN_POINT('Ctrl Pts',(-1.68452201279013,7.72957350624376,
10.2107422925307));
#241294=CARTESIAN_POINT('Ctrl Pts',(-1.60349896248135,7.74723102792698,
10.2073914873181));
#241295=CARTESIAN_POINT('Ctrl Pts',(-1.52223912846249,7.7636055542267,10.2040406821054));
#241296=CARTESIAN_POINT('Ctrl Pts',(-1.44078636577397,7.77869241249452,
10.2006898768928));
#241297=CARTESIAN_POINT('Ctrl Pts',(-1.23193470200725,7.8173763729428,10.1920981334022));
#241298=CARTESIAN_POINT('Ctrl Pts',(-1.02139613098446,7.84766857101163,
10.1835063899116));
#241299=CARTESIAN_POINT('Ctrl Pts',(-0.809837471830828,7.86943989552107,
10.174914646421));
#241300=CARTESIAN_POINT('Ctrl Pts',(-0.59858373311001,7.89117984092403,
10.1663352862483));
#241301=CARTESIAN_POINT('Ctrl Pts',(-0.386313087132472,7.90442339618755,
10.1577559260757));
#241302=CARTESIAN_POINT('Ctrl Pts',(-0.173700237161343,7.90909281950908,
10.149176565903));
#241303=CARTESIAN_POINT('Ctrl Pts',(0.0481825568613072,7.91396583020996,
10.1402231446668));
#241304=CARTESIAN_POINT('Ctrl Pts',(0.270437816712338,7.90950025771785,
10.1312697234305));
#241305=CARTESIAN_POINT('Ctrl Pts',(0.492290480755137,7.89566786805004,
10.1223163021943));
#241306=CARTESIAN_POINT('Ctrl Pts',(0.704039497636602,7.88246543513847,
10.1137706390052));
#241307=CARTESIAN_POINT('Ctrl Pts',(0.915421462210409,7.86073030452146,
10.1052249758162));
#241308=CARTESIAN_POINT('Ctrl Pts',(1.12575916832216,7.83049087190188,10.0966793126271));
#241309=CARTESIAN_POINT('Ctrl Pts',(1.33577481171214,7.80029774098518,10.0881467342986));
#241310=CARTESIAN_POINT('Ctrl Pts',(1.54474914109195,7.76162631997591,10.07961415597));
#241311=CARTESIAN_POINT('Ctrl Pts',(1.75200864203953,7.71455680633818,10.0710815776415));
#241312=CARTESIAN_POINT('Ctrl Pts',(1.95881897803677,7.66758929996989,10.062567490794));
#241313=CARTESIAN_POINT('Ctrl Pts',(2.16392165896475,7.61226007246776,10.0540534039464));
#241314=CARTESIAN_POINT('Ctrl Pts',(2.36665188143885,7.54870054195303,10.0455393170989));
#241315=CARTESIAN_POINT('Ctrl Pts',(2.39684288358654,7.53923512580117,10.0442713817552));
#241316=CARTESIAN_POINT('Ctrl Pts',(2.42698128175428,7.52958727327394,10.0430034464116));
#241317=CARTESIAN_POINT('Ctrl Pts',(2.45706489385209,7.51975751652935,10.0417355110679));
#241318=CARTESIAN_POINT('Ctrl Pts',(2.64442867903153,7.45853679525852,10.0338386812399));
#241319=CARTESIAN_POINT('Ctrl Pts',(2.82949288590725,7.39031267098654,10.0259418514119));
#241320=CARTESIAN_POINT('Ctrl Pts',(3.0117087418066,7.31529435187168,10.0180450215839));
#241321=CARTESIAN_POINT('Ctrl Pts',(3.1939660984105,7.24025894690509,10.0101463932077));
#241322=CARTESIAN_POINT('Ctrl Pts',(3.37337349464752,7.15842639333845,10.0022477648315));
#241323=CARTESIAN_POINT('Ctrl Pts',(3.54940309944911,7.07005365167911,9.99434913645532));
#241324=CARTESIAN_POINT('Ctrl Pts',(3.72550175846788,6.98164624249607,9.98644740954578));
#241325=CARTESIAN_POINT('Ctrl Pts',(3.89821967970184,6.8866936855725,9.97854568263623));
#241326=CARTESIAN_POINT('Ctrl Pts',(4.06705430413475,6.78549852901163,9.97064395572668));
#241327=CARTESIAN_POINT('Ctrl Pts',(4.23607502340706,6.68419183196272,9.96273351928492));
#241328=CARTESIAN_POINT('Ctrl Pts',(4.40120360083051,6.57662896464247,9.95482308284316));
#241329=CARTESIAN_POINT('Ctrl Pts',(4.56196608780908,6.46315607220497,9.9469126464014));
#241330=CARTESIAN_POINT('Ctrl Pts',(4.72282455024674,6.34961543627114,9.93899748741657));
#241331=CARTESIAN_POINT('Ctrl Pts',(4.87931145338171,6.23015794712718,9.93108232843174));
#241332=CARTESIAN_POINT('Ctrl Pts',(5.03098630054118,6.10516976371394,9.92316716944691));
#241333=CARTESIAN_POINT('Ctrl Pts',(5.18287371041121,5.98000641726247,9.9152409178671));
#241334=CARTESIAN_POINT('Ctrl Pts',(5.32993533367976,5.84929711584608,9.90731466628729));
#241335=CARTESIAN_POINT('Ctrl Pts',(5.47176687964138,5.71346551707978,9.89938841470748));
#241336=CARTESIAN_POINT('Ctrl Pts',(5.57082314764714,5.61859965941869,9.8938526582194));
#241337=CARTESIAN_POINT('Ctrl Pts',(5.66732911631661,5.52123603491172,9.88831690173133));
#241338=CARTESIAN_POINT('Ctrl Pts',(5.76115891386824,5.42152828722275,9.88278114524325));
#241339=CARTESIAN_POINT('Ctrl Pts',(5.89885173923236,5.27520972053894,9.87465756434186));
#241340=CARTESIAN_POINT('Ctrl Pts',(6.03108242737734,5.12352022575209,9.86653398344048));
#241341=CARTESIAN_POINT('Ctrl Pts',(6.15742438184121,4.96689500411549,9.8584104025391));
#241342=CARTESIAN_POINT('Ctrl Pts',(6.28365463989171,4.81040825172748,9.85029400353429));
#241343=CARTESIAN_POINT('Ctrl Pts',(6.40400634340106,4.64899472080601,9.84217760452949));
#241344=CARTESIAN_POINT('Ctrl Pts',(6.51809117228047,4.48312485548187,9.83406120552468));
#241345=CARTESIAN_POINT('Ctrl Pts',(6.63209141237905,4.31737797521915,9.82595082446549));
#241346=CARTESIAN_POINT('Ctrl Pts',(6.73983386163787,4.14718161220173,9.81784044340631));
#241347=CARTESIAN_POINT('Ctrl Pts',(6.84097142903509,3.9730379946743,9.80973006234712));
#241348=CARTESIAN_POINT('Ctrl Pts',(6.94204841315618,3.79899869239925,9.80162453955641));
#241349=CARTESIAN_POINT('Ctrl Pts',(7.03652824432652,3.62101712740149,9.79351901676571));
#241350=CARTESIAN_POINT('Ctrl Pts',(7.12410769532924,3.4396236051857,9.78541349397499));
#241351=CARTESIAN_POINT('Ctrl Pts',(7.21164714563034,3.25831293194962,9.77731167326959));
#241352=CARTESIAN_POINT('Ctrl Pts',(7.29229236202178,3.07359369784467,9.76920985256418));
#241353=CARTESIAN_POINT('Ctrl Pts',(7.36578627721016,2.88602036002218,9.76110803185878));
#241354=CARTESIAN_POINT('Ctrl Pts',(7.43995748519188,2.69671841555783,9.7529315477644));
#241355=CARTESIAN_POINT('Ctrl Pts',(7.50684476678568,2.50450979065043,9.74475506367002));
#241356=CARTESIAN_POINT('Ctrl Pts',(7.5662333607541,2.30998565593202,9.73657857957565));
#241357=CARTESIAN_POINT('Ctrl Pts',(7.6250573061041,2.11731099729274,9.72847983499552));
#241358=CARTESIAN_POINT('Ctrl Pts',(7.67652445379345,1.92236498446628,9.7203810904154));
#241359=CARTESIAN_POINT('Ctrl Pts',(7.72047593411518,1.72573820458037,9.71228234583528));
#241360=CARTESIAN_POINT('Ctrl Pts',(7.76442715590926,1.52911258127578,9.7041836488929));
#241361=CARTESIAN_POINT('Ctrl Pts',(7.80086272862794,1.33080652374314,9.69608495195053));
#241362=CARTESIAN_POINT('Ctrl Pts',(7.82967465811501,1.13142200264603,9.68798625500815));
#241363=CARTESIAN_POINT('Ctrl Pts',(7.8584901442091,0.932012869091566,9.67988655834507));
#241364=CARTESIAN_POINT('Ctrl Pts',(7.87968006490698,0.73152532405803,9.671786861682));
#241365=CARTESIAN_POINT('Ctrl Pts',(7.8931880989192,0.530568219063547,9.66368716501892));
#241366=CARTESIAN_POINT('Ctrl Pts',(7.90692105171448,0.326265029253143,
9.65545260240015));
#241367=CARTESIAN_POINT('Ctrl Pts',(7.91271401193322,0.121476846567367,
9.64721803978139));
#241368=CARTESIAN_POINT('Ctrl Pts',(7.91056295792561,-0.0831546071802162,
9.63898347716262));
#241369=CARTESIAN_POINT('Ctrl Pts',(7.90844510494008,-0.284627621674178,
9.63087601311709));
#241370=CARTESIAN_POINT('Ctrl Pts',(7.89862673624289,-0.485948387733569,
9.62276854907157));
#241371=CARTESIAN_POINT('Ctrl Pts',(7.88115654522144,-0.686507472438068,
9.61466108502604));
#241372=CARTESIAN_POINT('Ctrl Pts',(7.86327554084196,-0.891782724868992,
9.60636297312065));
#241373=CARTESIAN_POINT('Ctrl Pts',(7.83737846417857,-1.09625967758778,
9.59806486121527));
#241374=CARTESIAN_POINT('Ctrl Pts',(7.80357339207048,-1.29929339048948,
9.58976674930988));
#241375=CARTESIAN_POINT('Ctrl Pts',(7.76976831996239,-1.50232710339118,
9.58146863740449));
#241376=CARTESIAN_POINT('Ctrl Pts',(7.72805535156513,-1.70391723110227,
9.5731705254991));
#241377=CARTESIAN_POINT('Ctrl Pts',(7.67859786229843,-1.90343265420819,
9.56487241359372));
#241378=CARTESIAN_POINT('Ctrl Pts',(7.63195627071978,-2.09158852334186,
9.5570467606521));
#241379=CARTESIAN_POINT('Ctrl Pts',(7.57833708343701,-2.27826124570093,
9.54922110771048));
#241380=CARTESIAN_POINT('Ctrl Pts',(7.51785168359855,-2.46288998199562,
9.54139545476887));
#241381=CARTESIAN_POINT('Ctrl Pts',(7.45741739758756,-2.64736269582211,
9.53357641497812));
#241382=CARTESIAN_POINT('Ctrl Pts',(7.39012856107222,-2.82979453024159,
9.52575737518737));
#241383=CARTESIAN_POINT('Ctrl Pts',(7.31614729843773,-3.00963614205476,
9.51793833539662));
#241384=CARTESIAN_POINT('Ctrl Pts',(7.24221547118042,-3.18935758103504,
9.51012452040425));
#241385=CARTESIAN_POINT('Ctrl Pts',(7.16160025724386,-3.36649191982711,
9.50231070541188));
#241386=CARTESIAN_POINT('Ctrl Pts',(7.07451323002585,-3.54050611610674,
9.49449689041951));
#241387=CARTESIAN_POINT('Ctrl Pts',(6.98746798788579,-3.71443681893174,
9.48668682456038));
#241388=CARTESIAN_POINT('Ctrl Pts',(6.89395727496761,-3.88525004675205,
9.47887675870126));
#241389=CARTESIAN_POINT('Ctrl Pts',(6.7942403649099,-4.05243369641367,9.47106669284213));
#241390=CARTESIAN_POINT('Ctrl Pts',(6.69455257874541,-4.21956851745878,
9.46325890803567));
#241391=CARTESIAN_POINT('Ctrl Pts',(6.58866238726719,-4.38307557008177,
9.45545112322922));
#241392=CARTESIAN_POINT('Ctrl Pts',(6.47687457155242,-4.54246813795954,
9.44764333842276));
#241393=CARTESIAN_POINT('Ctrl Pts',(6.36508021315268,-4.70187003471947,
9.43983509664453));
#241394=CARTESIAN_POINT('Ctrl Pts',(6.2473877379407,-4.8571566733063,9.4320268548663));
#241395=CARTESIAN_POINT('Ctrl Pts',(6.12414499222924,-5.00787071659738,
9.42421861308807));
#241396=CARTESIAN_POINT('Ctrl Pts',(6.0278616042375,-5.12561605424163,9.41811842464837));
#241397=CARTESIAN_POINT('Ctrl Pts',(5.92819149177514,-5.24057104731698,
9.41201823620866));
#241398=CARTESIAN_POINT('Ctrl Pts',(5.82531752358805,-5.35253180741395,
9.40591804776896));
#241399=CARTESIAN_POINT('Ctrl Pts',(5.67928539102838,-5.51146286497972,
9.39725867997588));
#241400=CARTESIAN_POINT('Ctrl Pts',(5.52686841486363,-5.66428149419263,
9.38859931218279));
#241401=CARTESIAN_POINT('Ctrl Pts',(5.36858988646197,-5.81052180367463,
9.37993994438971));
#241402=CARTESIAN_POINT('Ctrl Pts',(5.21003743637605,-5.95701520112935,
9.37126559042867));
#241403=CARTESIAN_POINT('Ctrl Pts',(5.04560332164886,-6.09690736730511,
9.36259123646763));
#241404=CARTESIAN_POINT('Ctrl Pts',(4.87584411823539,-6.22977247856367,
9.35391688250659));
#241405=CARTESIAN_POINT('Ctrl Pts',(4.70141911963666,-6.3662893588217,9.34500411579305));
#241406=CARTESIAN_POINT('Ctrl Pts',(4.52137238261631,-6.49538727664552,
9.33609134907952));
#241407=CARTESIAN_POINT('Ctrl Pts',(4.33633789484381,-6.61665282916835,
9.32717858236599));
#241408=CARTESIAN_POINT('Ctrl Pts',(4.15563539520363,-6.73507933832845,
9.31847447945397));
#241409=CARTESIAN_POINT('Ctrl Pts',(3.97017627356648,-6.8460360228435,9.30977037654195));
#241410=CARTESIAN_POINT('Ctrl Pts',(3.7805760327062,-6.94918454647216,9.30106627362992));
#241411=CARTESIAN_POINT('Ctrl Pts',(3.584157850797,-7.05604224552271,9.29204917501564));
#241412=CARTESIAN_POINT('Ctrl Pts',(3.38329546915963,-7.15451973244231,
9.28303207640135));
#241413=CARTESIAN_POINT('Ctrl Pts',(3.17869751905459,-7.24429451929974,
9.27401497778706));
#241414=CARTESIAN_POINT('Ctrl Pts',(2.97409956894955,-7.33406930615716,
9.26499787917277));
#241415=CARTESIAN_POINT('Ctrl Pts',(2.76576630604029,-7.41514131334428,
9.25598078055848));
#241416=CARTESIAN_POINT('Ctrl Pts',(2.55442732361032,-7.48724395544803,
9.2469636819442));
#241417=CARTESIAN_POINT('Ctrl Pts',(2.36035336384111,-7.55345627984745,
9.23868322173954));
#241418=CARTESIAN_POINT('Ctrl Pts',(2.16357684847049,-7.61216197823561,
9.23040276153488));
#241419=CARTESIAN_POINT('Ctrl Pts',(1.96469543193453,-7.66315162708762,
9.22212230133022));
#241420=CARTESIAN_POINT('Ctrl Pts',(1.76598859761605,-7.71409651617212,
9.21384910988465));
#241421=CARTESIAN_POINT('Ctrl Pts',(1.56518083565212,-7.75733879224521,
9.20557591843909));
#241422=CARTESIAN_POINT('Ctrl Pts',(1.36288538465213,-7.792718680172,9.19730272699352));
#241423=CARTESIAN_POINT('Ctrl Pts',(1.16075177834765,-7.82807026273077,
9.18903615444197));
#241424=CARTESIAN_POINT('Ctrl Pts',(0.957133150287012,-7.85557195343149,
9.18076958189042));
#241425=CARTESIAN_POINT('Ctrl Pts',(0.752654151315554,-7.87511477557676,
9.17250300933887));
#241426=CARTESIAN_POINT('Ctrl Pts',(0.548365589235476,-7.8946393969566,
9.16424413567271));
#241427=CARTESIAN_POINT('Ctrl Pts',(0.343218551836084,-7.90621991579081,
9.15598526200656));
#241428=CARTESIAN_POINT('Ctrl Pts',(0.137844450573246,-7.90979898021727,
9.14772638834041));
#241429=CARTESIAN_POINT('Ctrl Pts',(-0.0674099135277758,-7.9133759579784,
9.1394723297609));
#241430=CARTESIAN_POINT('Ctrl Pts',(-0.272890779820393,-7.90896078059047,
9.13121827118139));
#241431=CARTESIAN_POINT('Ctrl Pts',(-0.477963770675786,-7.89654808342996,
9.12296421260188));
#241432=CARTESIAN_POINT('Ctrl Pts',(-0.682906975524917,-7.88414324198163,
9.1147153778273));
#241433=CARTESIAN_POINT('Ctrl Pts',(-0.887442522784967,-7.86375099972519,
9.10646654305271));
#241434=CARTESIAN_POINT('Ctrl Pts',(-1.09093763596683,-7.83541805358406,
9.09821770827812));
#241435=CARTESIAN_POINT('Ctrl Pts',(-1.17488314562582,-7.82373018763599,
9.09481491089189));
#241436=CARTESIAN_POINT('Ctrl Pts',(-1.25865163316916,-7.8106916524491,
9.09141211350566));
#241437=CARTESIAN_POINT('Ctrl Pts',(-1.34219888083408,-7.79630830356828,
9.08800931611943));
#241438=CARTESIAN_POINT('Ctrl Pts',(-1.54246652179313,-7.76183057473867,
9.07985261168873));
#241439=CARTESIAN_POINT('Ctrl Pts',(-1.74137495677086,-7.71963717112491,
9.07169590725802));
#241440=CARTESIAN_POINT('Ctrl Pts',(-1.9383181463002,-7.66986595474285,
9.06353920282732));
#241441=CARTESIAN_POINT('Ctrl Pts',(-2.1353203067587,-7.62007983530735,
9.05538005602508));
#241442=CARTESIAN_POINT('Ctrl Pts',(-2.33035574563551,-7.56271145302439,
9.04722090922285));
#241443=CARTESIAN_POINT('Ctrl Pts',(-2.52283233455093,-7.4979489203211,
9.03906176242061));
#241444=CARTESIAN_POINT('Ctrl Pts',(-2.71538770680269,-7.4331598794153,
9.03089927596647));
#241445=CARTESIAN_POINT('Ctrl Pts',(-2.9053818443482,-7.36097074974645,
9.02273678951233));
#241446=CARTESIAN_POINT('Ctrl Pts',(-3.0922407765744,-7.28161850001018,
9.01457430305819));
#241447=CARTESIAN_POINT('Ctrl Pts',(-3.27927779040433,-7.20219062543906,
9.00640403753424));
#241448=CARTESIAN_POINT('Ctrl Pts',(-3.46317334050545,-7.11558611008798,
8.99823377201029));
#241449=CARTESIAN_POINT('Ctrl Pts',(-3.64337500980557,-7.02208939973882,
8.99006350648634));
#241450=CARTESIAN_POINT('Ctrl Pts',(-3.82366938334809,-6.92854459026975,
8.98188903779225));
#241451=CARTESIAN_POINT('Ctrl Pts',(-4.00026581133523,-6.82810066111308,
8.97371456909816));
#241452=CARTESIAN_POINT('Ctrl Pts',(-4.17263830753271,-6.72108700691417,
8.96554010040408));
#241453=CARTESIAN_POINT('Ctrl Pts',(-4.34519482194472,-6.61395910907426,
8.95735690496316));
#241454=CARTESIAN_POINT('Ctrl Pts',(-4.51351813219441,-6.50024764074212,
8.94917370952225));
#241455=CARTESIAN_POINT('Ctrl Pts',(-4.67711175205704,-6.3803249649818,
8.94099051408134));
#241456=CARTESIAN_POINT('Ctrl Pts',(-4.75664800408561,-6.32202073422253,
8.93701199281911));
#241457=CARTESIAN_POINT('Ctrl Pts',(-4.83506677825874,-6.26224895531807,
8.93303347155689));
#241458=CARTESIAN_POINT('Ctrl Pts',(-4.91231393835858,-6.20105577873704,
8.92905495029467));
#241459=CARTESIAN_POINT('Ctrl Pts',(-5.06467539118251,-6.08035902723515,
8.92120775851674));
#241460=CARTESIAN_POINT('Ctrl Pts',(-5.21276933187155,-5.95389820078589,
8.91336056673882));
#241461=CARTESIAN_POINT('Ctrl Pts',(-5.35612987218644,-5.82200942907791,
8.9055133749609));
#241462=CARTESIAN_POINT('Ctrl Pts',(-5.49936350951701,-5.69023740552595,
8.89767312952995));
#241463=CARTESIAN_POINT('Ctrl Pts',(-5.63787183538287,-5.55304724188308,
8.889832884099));
#241464=CARTESIAN_POINT('Ctrl Pts',(-5.77122058026558,-5.41081639070474,
8.88199263866805));
#241465=CARTESIAN_POINT('Ctrl Pts',(-5.90447698927311,-5.26868402571862,
8.87415782212902));
#241466=CARTESIAN_POINT('Ctrl Pts',(-6.03258069520401,-5.12151818025878,
8.86632300558998));
#241467=CARTESIAN_POINT('Ctrl Pts',(-6.15513282804547,-4.96973448678267,
8.85848818905095));
#241468=CARTESIAN_POINT('Ctrl Pts',(-6.27762371764066,-4.81802664450478,
8.85065728782198));
#241469=CARTESIAN_POINT('Ctrl Pts',(-6.39456834165947,-4.66170582363914,
8.84282638659301));
#241470=CARTESIAN_POINT('Ctrl Pts',(-6.5056066906416,-4.50122234361725,
8.83499548536405));
#241471=CARTESIAN_POINT('Ctrl Pts',(-6.61943505737918,-4.33670645710859,
8.82696782010112));
#241472=CARTESIAN_POINT('Ctrl Pts',(-6.72705619161308,-4.16781625990227,
8.81894015483819));
#241473=CARTESIAN_POINT('Ctrl Pts',(-6.82812775317153,-3.99507101143006,
8.81091248957526));
#241474=CARTESIAN_POINT('Ctrl Pts',(-6.92669905157804,-3.82659905776764,
8.8030834091105));
#241475=CARTESIAN_POINT('Ctrl Pts',(-7.01904081241868,-3.65446084903053,
8.79525432864574));
#241476=CARTESIAN_POINT('Ctrl Pts',(-7.10488071172684,-3.47916528381909,
8.78742524818098));
#241477=CARTESIAN_POINT('Ctrl Pts',(-7.19073027564623,-3.30384998229036,
8.77959528624945));
#241478=CARTESIAN_POINT('Ctrl Pts',(-7.27007636510633,-3.12537693073728,
8.77176532431792));
#241479=CARTESIAN_POINT('Ctrl Pts',(-7.34269374456673,-2.94427742807987,
8.76393536238639));
#241480=CARTESIAN_POINT('Ctrl Pts',(-7.41533197604286,-2.76312592286182,
8.75610315208827));
#241481=CARTESIAN_POINT('Ctrl Pts',(-7.48123751801491,-2.57934678931001,
8.74827094179016));
#241482=CARTESIAN_POINT('Ctrl Pts',(-7.54023412577994,-2.39348915360477,
8.74043873149204));
#241483=CARTESIAN_POINT('Ctrl Pts',(-7.60181734548886,-2.19948288701055,
8.73226313045552));
#241484=CARTESIAN_POINT('Ctrl Pts',(-7.65587202929742,-2.00321216380559,
8.72408752941899));
#241485=CARTESIAN_POINT('Ctrl Pts',(-7.70225654814461,-1.80531578028985,
8.71591192838247));
#241486=CARTESIAN_POINT('Ctrl Pts',(-7.74676446764627,-1.61542577978758,
8.70806709131495));
#241487=CARTESIAN_POINT('Ctrl Pts',(-7.78421063099003,-1.42403942123451,
8.70022225424743));
#241488=CARTESIAN_POINT('Ctrl Pts',(-7.81452279807668,-1.23172823233851,
8.69237741717991));
#241489=CARTESIAN_POINT('Ctrl Pts',(-7.84485569390023,-1.03928553294957,
8.68452721548231));
#241490=CARTESIAN_POINT('Ctrl Pts',(-7.86804482960821,-0.845917089121394,
8.6766770137847));
#241491=CARTESIAN_POINT('Ctrl Pts',(-7.88406999468733,-0.652197300570159,
8.6688268120871));
#241492=CARTESIAN_POINT('Ctrl Pts',(-7.90011556588749,-0.458230833158753,
8.66096661410145));
#241493=CARTESIAN_POINT('Ctrl Pts',(-7.9089789397769,-0.263912475701678,
8.65310641611579));
#241494=CARTESIAN_POINT('Ctrl Pts',(-7.91069193117117,-0.0698152569529835,
8.64524621813014));
#241495=CARTESIAN_POINT('Ctrl Pts',(-7.91090366690793,-0.0458237075776071,
8.64427465177134));
#241496=CARTESIAN_POINT('Ctrl Pts',(-7.91100622103527,-0.0218355284886099,
8.64330308541254));
#241497=CARTESIAN_POINT('Ctrl Pts',(-7.91099970833086,0.00214820601359551,
8.64233151905374));
#241498=CARTESIAN_POINT('Origin',(0.,0.,4.30282021618968));
#241499=CARTESIAN_POINT('',(-6.76699855375495,-0.00289230543239241,137.30282021619));
#241500=CARTESIAN_POINT('Ctrl Pts',(3.09910619832119,6.01563211736948,136.651395695404));
#241501=CARTESIAN_POINT('Ctrl Pts',(2.93375330764808,6.10081787314662,136.660145143307));
#241502=CARTESIAN_POINT('Ctrl Pts',(2.76488627843049,6.17918207037049,136.668894591209));
#241503=CARTESIAN_POINT('Ctrl Pts',(2.59307866646677,6.25045854554007,136.677644039111));
#241504=CARTESIAN_POINT('Ctrl Pts',(2.42127244185344,6.3217344451505,136.686393416362));
#241505=CARTESIAN_POINT('Ctrl Pts',(2.24652594672423,6.38592262741853,136.695142793612));
#241506=CARTESIAN_POINT('Ctrl Pts',(2.06943269687071,6.44280508110578,136.703892170862));
#241507=CARTESIAN_POINT('Ctrl Pts',(1.89234081822012,6.49968709436186,136.712641480368));
#241508=CARTESIAN_POINT('Ctrl Pts',(1.71290249405508,6.54926340459566,136.721390789873));
#241509=CARTESIAN_POINT('Ctrl Pts',(1.53172716624962,6.59136563150406,136.730140099378));
#241510=CARTESIAN_POINT('Ctrl Pts',(1.35055318107239,6.63346754640729,136.738889344046));
#241511=CARTESIAN_POINT('Ctrl Pts',(1.16764249714326,6.66809542395792,136.747638588713));
#241512=CARTESIAN_POINT('Ctrl Pts',(0.983616340613428,6.69513165624682,
136.75638783338));
#241513=CARTESIAN_POINT('Ctrl Pts',(0.799591486713008,6.7221676971597,136.765137016116));
#241514=CARTESIAN_POINT('Ctrl Pts',(0.614451459525972,6.74161215869377,
136.773886198851));
#241515=CARTESIAN_POINT('Ctrl Pts',(0.428825047909639,6.75339900185716,
136.782635381587));
#241516=CARTESIAN_POINT('Ctrl Pts',(0.243199888596407,6.76518576550223,
136.791384505298));
#241517=CARTESIAN_POINT('Ctrl Pts',(0.0570886373912859,6.76931499599835,
136.800133629008));
#241518=CARTESIAN_POINT('Ctrl Pts',(-0.128876626811774,6.76577266947846,
136.808882752719));
#241519=CARTESIAN_POINT('Ctrl Pts',(-0.314840698188627,6.7622303656799,
136.81763182031));
#241520=CARTESIAN_POINT('Ctrl Pts',(-0.500658497951566,6.7510166087922,
136.826380887902));
#241521=CARTESIAN_POINT('Ctrl Pts',(-0.685698951926375,6.73216948296217,
136.835129955493));
#241522=CARTESIAN_POINT('Ctrl Pts',(-0.870738280460203,6.71332247176289,
136.843878969872));
#241523=CARTESIAN_POINT('Ctrl Pts',(-1.05499998761305,6.68684221356179,
136.85262798425));
#241524=CARTESIAN_POINT('Ctrl Pts',(-1.23785829161493,6.65281863948509,
136.861376998629));
#241525=CARTESIAN_POINT('Ctrl Pts',(-1.43007412917463,6.61705395368848,
136.870573732328));
#241526=CARTESIAN_POINT('Ctrl Pts',(-1.62073882535838,6.57295372727778,
136.879770466027));
#241527=CARTESIAN_POINT('Ctrl Pts',(-1.80913696091546,6.5206834347827,136.888967199726));
#241528=CARTESIAN_POINT('Ctrl Pts',(-1.98838356186147,6.47095219815188,
136.89771719744));
#241529=CARTESIAN_POINT('Ctrl Pts',(-2.16557827572571,6.41382586850878,
136.906467195154));
#241530=CARTESIAN_POINT('Ctrl Pts',(-2.3401191862174,6.34949849943263,136.915217192868));
#241531=CARTESIAN_POINT('Ctrl Pts',(-2.51465655691146,6.28517243495532,
136.923967013126));
#241532=CARTESIAN_POINT('Ctrl Pts',(-2.68653996295384,6.21364572242351,
136.932716833384));
#241533=CARTESIAN_POINT('Ctrl Pts',(-2.85518555380051,6.13516132252192,
136.941466653642));
#241534=CARTESIAN_POINT('Ctrl Pts',(-3.02382794858743,6.05667841000479,
136.95021630808));
#241535=CARTESIAN_POINT('Ctrl Pts',(-3.18923239109328,5.97123819492056,
136.958965962517));
#241536=CARTESIAN_POINT('Ctrl Pts',(-3.35083705967737,5.87913088810691,
136.967715616955));
#241537=CARTESIAN_POINT('Ctrl Pts',(-3.51243888042425,5.78702520443087,
136.976465117204));
#241538=CARTESIAN_POINT('Ctrl Pts',(-3.67024081223702,5.68825280605775,
136.985214617453));
#241539=CARTESIAN_POINT('Ctrl Pts',(-3.82370687544401,5.58314917682505,
136.993964117702));
#241540=CARTESIAN_POINT('Ctrl Pts',(-3.97717043817814,5.47804726008022,
137.002713475392));
#241541=CARTESIAN_POINT('Ctrl Pts',(-4.12629803722458,5.36661448084237,
137.011462833083));
#241542=CARTESIAN_POINT('Ctrl Pts',(-4.27058317206905,5.24922931204579,
137.020212190773));
#241543=CARTESIAN_POINT('Ctrl Pts',(-4.41486614774839,5.13184589986788,
137.028961417533));
#241544=CARTESIAN_POINT('Ctrl Pts',(-4.55430658194423,5.00851045723026,
137.037710644293));
#241545=CARTESIAN_POINT('Ctrl Pts',(-4.6884308900186,4.87964187103105,137.046459871053));
#241546=CARTESIAN_POINT('Ctrl Pts',(-4.8225533691786,4.75077504207937,137.055208978509));
#241547=CARTESIAN_POINT('Ctrl Pts',(-4.95135966065167,4.61637541908059,
137.063958085965));
#241548=CARTESIAN_POINT('Ctrl Pts',(-5.07441230869284,4.476899454018,137.072707193421));
#241549=CARTESIAN_POINT('Ctrl Pts',(-5.19746344226446,4.3374252055548,137.081456193198));
#241550=CARTESIAN_POINT('Ctrl Pts',(-5.31476088454787,4.1928749549131,137.090205192974));
#241551=CARTESIAN_POINT('Ctrl Pts',(-5.42590627628865,4.0437396158669,137.09895419275));
#241552=CARTESIAN_POINT('Ctrl Pts',(-5.53706380672674,3.89458798906724,
137.107704148045));
#241553=CARTESIAN_POINT('Ctrl Pts',(-5.64206777071866,3.7408505015528,137.11645410334));
#241554=CARTESIAN_POINT('Ctrl Pts',(-5.74056148164006,3.58304938223163,
137.125204058634));
#241555=CARTESIAN_POINT('Ctrl Pts',(-5.83905138951881,3.42525435593287,
137.133953676075));
#241556=CARTESIAN_POINT('Ctrl Pts',(-5.93103139557648,3.26339625497191,
137.142703293517));
#241557=CARTESIAN_POINT('Ctrl Pts',(-6.01618907820841,3.09802485065015,
137.151452910958));
#241558=CARTESIAN_POINT('Ctrl Pts',(-6.10134392544986,2.93265895249636,
137.160202237074));
#241559=CARTESIAN_POINT('Ctrl Pts',(-6.17967677261841,2.76378023986016,
137.168951563189));
#241560=CARTESIAN_POINT('Ctrl Pts',(-6.25092157009239,2.59196229227081,
137.177700889305));
#241561=CARTESIAN_POINT('Ctrl Pts',(-6.3221643740777,2.42014915229049,137.186449970608));
#241562=CARTESIAN_POINT('Ctrl Pts',(-6.38631941548939,2.24539720662801,
137.19519905191));
#241563=CARTESIAN_POINT('Ctrl Pts',(-6.44316881037556,2.06829994947628,
137.203948133213));
#241564=CARTESIAN_POINT('Ctrl Pts',(-6.50002334524592,1.89118668024382,
137.212698005555));
#241565=CARTESIAN_POINT('Ctrl Pts',(-6.54957082411117,1.71172794807624,
137.221447877897));
#241566=CARTESIAN_POINT('Ctrl Pts',(-6.59164294296104,1.53053334250251,
137.23019775024));
#241567=CARTESIAN_POINT('Ctrl Pts',(-6.6337121408215,1.34935131693519,137.238947015095));
#241568=CARTESIAN_POINT('Ctrl Pts',(-6.66830695239702,1.16643393829691,
137.24769627995));
#241569=CARTESIAN_POINT('Ctrl Pts',(-6.69530988153998,0.982402458340346,
137.256445544804));
#241570=CARTESIAN_POINT('Ctrl Pts',(-6.72231419690491,0.798361530946396,
137.265195258811));
#241571=CARTESIAN_POINT('Ctrl Pts',(-6.74172580829284,0.613206671361794,
137.273944972819));
#241572=CARTESIAN_POINT('Ctrl Pts',(-6.75347878028184,0.427566795112697,
137.282694686826));
#241573=CARTESIAN_POINT('Ctrl Pts',(-6.76248992368205,0.285234494206634,
137.289403196614));
#241574=CARTESIAN_POINT('Ctrl Pts',(-6.76699999999985,0.142617266095565,
137.296111706402));
#241575=CARTESIAN_POINT('Ctrl Pts',(-6.767,6.94095400683209E-12,137.30282021619));
#241576=CARTESIAN_POINT('',(3.93014697525799,-5.50874157615607,137.999994970183));
#241577=CARTESIAN_POINT('Ctrl Pts',(-6.76699661606879,-0.00676743035154104,
137.30282021619));
#241578=CARTESIAN_POINT('Ctrl Pts',(-6.76675997058177,-0.243397750383354,
137.313965237425));
#241579=CARTESIAN_POINT('Ctrl Pts',(-6.75410846046182,-0.479452755848537,
137.32511025866));
#241580=CARTESIAN_POINT('Ctrl Pts',(-6.72924119810341,-0.713864061112333,
137.336255279896));
#241581=CARTESIAN_POINT('Ctrl Pts',(-6.7034162722948,-0.957302783070773,
137.347829507182));
#241582=CARTESIAN_POINT('Ctrl Pts',(-6.66441646993814,-1.19896933863425,
137.359403734469));
#241583=CARTESIAN_POINT('Ctrl Pts',(-6.61251193072666,-1.43769780065132,
137.370977961756));
#241584=CARTESIAN_POINT('Ctrl Pts',(-6.58579060248779,-1.56059922103628,
137.376936568289));
#241585=CARTESIAN_POINT('Ctrl Pts',(-6.55564981007044,-1.68272237431578,
137.382895174822));
#241586=CARTESIAN_POINT('Ctrl Pts',(-6.52213127688092,-1.80391036560347,
137.388853781355));
#241587=CARTESIAN_POINT('Ctrl Pts',(-6.476833696767,-1.96768611059689,137.396906354995));
#241588=CARTESIAN_POINT('Ctrl Pts',(-6.42527716931142,-2.13006556088003,
137.404958928634));
#241589=CARTESIAN_POINT('Ctrl Pts',(-6.36755898385533,-2.29051993816323,
137.413011502274));
#241590=CARTESIAN_POINT('Ctrl Pts',(-6.30991413540764,-2.45077044133083,
137.421053844274));
#241591=CARTESIAN_POINT('Ctrl Pts',(-6.24612333029497,-2.60910039008183,
137.429096186274));
#241592=CARTESIAN_POINT('Ctrl Pts',(-6.17633473175018,-2.76499155177306,
137.437138528274));
#241593=CARTESIAN_POINT('Ctrl Pts',(-6.10661936852886,-2.92071912313737,
137.445172430737));
#241594=CARTESIAN_POINT('Ctrl Pts',(-6.03091888762117,-3.07401266096776,
137.453206333199));
#241595=CARTESIAN_POINT('Ctrl Pts',(-5.94943105221846,-3.22436957480043,
137.461240235661));
#241596=CARTESIAN_POINT('Ctrl Pts',(-5.86801073572888,-3.37460190641353,
137.46926748142));
#241597=CARTESIAN_POINT('Ctrl Pts',(-5.78081278558136,-3.52190212884627,
137.477294727179));
#241598=CARTESIAN_POINT('Ctrl Pts',(-5.6880827714529,-3.66578823516862,
137.485321972938));
#241599=CARTESIAN_POINT('Ctrl Pts',(-5.59540914186583,-3.80958685145666,
137.493344337725));
#241600=CARTESIAN_POINT('Ctrl Pts',(-5.49721034636524,-3.94997516976006,
137.501366702512));
#241601=CARTESIAN_POINT('Ctrl Pts',(-5.39377746694698,-4.08649649908758,
137.509389067299));
#241602=CARTESIAN_POINT('Ctrl Pts',(-5.28774626359827,-4.22644736299833,
137.51761296087));
#241603=CARTESIAN_POINT('Ctrl Pts',(-5.17621473704244,-4.36233404085406,
137.525836854441));
#241604=CARTESIAN_POINT('Ctrl Pts',(-5.05954349078207,-4.49369654793076,
137.534060748012));
#241605=CARTESIAN_POINT('Ctrl Pts',(-4.94577196478572,-4.62179420153317,
137.542080246828));
#241606=CARTESIAN_POINT('Ctrl Pts',(-4.82711344885099,-4.74558962290845,
137.550099745643));
#241607=CARTESIAN_POINT('Ctrl Pts',(-4.70394248253506,-4.86469054730123,
137.558119244459));
#241608=CARTESIAN_POINT('Ctrl Pts',(-4.58075989890919,-4.9838027051234,
137.566139499663));
#241609=CARTESIAN_POINT('Ctrl Pts',(-4.45306428714298,-5.09821922345179,
137.574159754866));
#241610=CARTESIAN_POINT('Ctrl Pts',(-4.32126605820613,-5.20758568380739,
137.582180010069));
#241611=CARTESIAN_POINT('Ctrl Pts',(-4.18942909599465,-5.31698428511949,
137.59020262229));
#241612=CARTESIAN_POINT('Ctrl Pts',(-4.05348740551106,-5.42132963515267,
137.598225234511));
#241613=CARTESIAN_POINT('Ctrl Pts',(-3.91388323497627,-5.52030859852705,
137.606247846732));
#241614=CARTESIAN_POINT('Ctrl Pts',(-3.7681257785839,-5.62365022422875,
137.614624068922));
#241615=CARTESIAN_POINT('Ctrl Pts',(-3.61837602773323,-5.72114139189279,
137.623000291111));
#241616=CARTESIAN_POINT('Ctrl Pts',(-3.46516838418653,-5.81247770483759,
137.6313765133));
#241617=CARTESIAN_POINT('Ctrl Pts',(-3.31817049754964,-5.90011200731284,
137.639413233475));
#241618=CARTESIAN_POINT('Ctrl Pts',(-3.16798987172157,-5.98208046317299,
137.64744995365));
#241619=CARTESIAN_POINT('Ctrl Pts',(-3.01512071593136,-6.05816276344253,
137.655486673825));
#241620=CARTESIAN_POINT('Ctrl Pts',(-2.86213645315186,-6.13430235194969,
137.663529445467));
#241621=CARTESIAN_POINT('Ctrl Pts',(-2.70645996954239,-6.20454680768543,
137.671572217109));
#241622=CARTESIAN_POINT('Ctrl Pts',(-2.54860298262317,-6.26872489721509,
137.679614988751));
#241623=CARTESIAN_POINT('Ctrl Pts',(-2.39052228006946,-6.33299394022295,
137.687669158645));
#241624=CARTESIAN_POINT('Ctrl Pts',(-2.23025525810373,-6.39117933781976,
137.695723328539));
#241625=CARTESIAN_POINT('Ctrl Pts',(-2.06832677251032,-6.44316019994203,
137.703777498433));
#241626=CARTESIAN_POINT('Ctrl Pts',(-2.04832227399967,-6.44958186858851,
137.70477250329));
#241627=CARTESIAN_POINT('Ctrl Pts',(-2.02829242796762,-6.45590890876347,
137.705767508147));
#241628=CARTESIAN_POINT('Ctrl Pts',(-2.00823823124795,-6.46214114721693,
137.706762513004));
#241629=CARTESIAN_POINT('Ctrl Pts',(-1.84137858411901,-6.51399608430093,
137.715041386581));
#241630=CARTESIAN_POINT('Ctrl Pts',(-1.67227889322659,-6.55945574328369,
137.723320260158));
#241631=CARTESIAN_POINT('Ctrl Pts',(-1.50146737897553,-6.59832438652969,
137.731599133736));
#241632=CARTESIAN_POINT('Ctrl Pts',(-1.33086001777546,-6.63714657417144,
137.739868112445));
#241633=CARTESIAN_POINT('Ctrl Pts',(-1.15854525003179,-6.66939335785156,
137.748137091155));
#241634=CARTESIAN_POINT('Ctrl Pts',(-0.985068047904076,-6.69491821764825,
137.756406069864));
#241635=CARTESIAN_POINT('Ctrl Pts',(-0.811764623609784,-6.72041750835126,
137.764666765265));
#241636=CARTESIAN_POINT('Ctrl Pts',(-0.637301432280176,-6.73920823695477,
137.772927460666));
#241637=CARTESIAN_POINT('Ctrl Pts',(-0.462235428407887,-6.75119451717432,
137.781188156067));
#241638=CARTESIAN_POINT('Ctrl Pts',(-0.287310939905778,-6.76317110823181,
137.789442173899));
#241639=CARTESIAN_POINT('Ctrl Pts',(-0.111784961143709,-6.76835418502657,
137.797696191731));
#241640=CARTESIAN_POINT('Ctrl Pts',(0.06377845566846,-6.76669943980022,
137.805950209562));
#241641=CARTESIAN_POINT('Ctrl Pts',(0.239228010772019,-6.7650457677594,
137.814198874248));
#241642=CARTESIAN_POINT('Ctrl Pts',(0.414714602696616,-6.75656311526461,
137.822447538934));
#241643=CARTESIAN_POINT('Ctrl Pts',(0.589672091611263,-6.74125921652437,
137.83069620362));
#241644=CARTESIAN_POINT('Ctrl Pts',(0.764567338287138,-6.7259607622434,
137.838941933791));
#241645=CARTESIAN_POINT('Ctrl Pts',(0.938933504922963,-6.70384592580967,
137.847187663962));
#241646=CARTESIAN_POINT('Ctrl Pts',(1.11220716957069,-6.67497447275685,
137.855433394133));
#241647=CARTESIAN_POINT('Ctrl Pts',(1.285449543949,-6.64610823339617,137.863677635265));
#241648=CARTESIAN_POINT('Ctrl Pts',(1.45759946058247,-6.61048786635831,
137.871921876398));
#241649=CARTESIAN_POINT('Ctrl Pts',(1.62810119702784,-6.56822468344655,
137.880166117531));
#241650=CARTESIAN_POINT('Ctrl Pts',(1.79860200943978,-6.52596172957993,
137.888410313984));
#241651=CARTESIAN_POINT('Ctrl Pts',(1.9674543163267,-6.47705611755172,137.896654510437));
#241652=CARTESIAN_POINT('Ctrl Pts',(2.13411500467748,-6.4216697319942,137.90489870689));
#241653=CARTESIAN_POINT('Ctrl Pts',(2.30086722539536,-6.3662529274637,137.91314743117));
#241654=CARTESIAN_POINT('Ctrl Pts',(2.46542508579837,-6.30434834740739,
137.921396155451));
#241655=CARTESIAN_POINT('Ctrl Pts',(2.62726227747752,-6.23616724642177,
137.929644879731));
#241656=CARTESIAN_POINT('Ctrl Pts',(2.78914341309458,-6.16796763210162,
137.937895843802));
#241657=CARTESIAN_POINT('Ctrl Pts',(2.94830208456367,-6.09348824471639,
137.946146807873));
#241658=CARTESIAN_POINT('Ctrl Pts',(3.10423415084922,-6.01298755500969,
137.954397771944));
#241659=CARTESIAN_POINT('Ctrl Pts',(3.26031933642722,-5.93240781672149,
137.962656838144));
#241660=CARTESIAN_POINT('Ctrl Pts',(3.41317127472098,-5.8457951308704,137.970915904345));
#241661=CARTESIAN_POINT('Ctrl Pts',(3.56231163725544,-5.75345329337733,
137.979174970545));
#241662=CARTESIAN_POINT('Ctrl Pts',(3.68763259641482,-5.67585949215202,
137.986114970424));
#241663=CARTESIAN_POINT('Ctrl Pts',(3.81033325902537,-5.59422126474488,
137.993054970304));
#241664=CARTESIAN_POINT('Ctrl Pts',(3.93014697525799,-5.50874157615607,
137.999994970183));
#241665=CARTESIAN_POINT('',(-3.92888236737319,-5.50964357679733,138.));
#241666=CARTESIAN_POINT('Origin',(0.,0.,138.));
#241667=CARTESIAN_POINT('',(-6.767,6.64344400075779E-12,137.69717978381));
#241668=CARTESIAN_POINT('Ctrl Pts',(-6.76699999999825,4.86320023540543E-6,
137.697286552978));
#241669=CARTESIAN_POINT('Ctrl Pts',(-6.76700012425513,-0.17289492391004,
137.705426224725));
#241670=CARTESIAN_POINT('Ctrl Pts',(-6.76036941594973,-0.345936048758181,
137.713565896472));
#241671=CARTESIAN_POINT('Ctrl Pts',(-6.74710141855822,-0.518566724433509,
137.721705568218));
#241672=CARTESIAN_POINT('Ctrl Pts',(-6.73384006786635,-0.691110919518242,
137.729841162338));
#241673=CARTESIAN_POINT('Ctrl Pts',(-6.71394807658885,-0.863244710707634,
137.737976756457));
#241674=CARTESIAN_POINT('Ctrl Pts',(-6.68747105695194,-1.03441764410229,
137.746112350576));
#241675=CARTESIAN_POINT('Ctrl Pts',(-6.66099847292775,-1.20556190142803,
137.754246581764));
#241676=CARTESIAN_POINT('Ctrl Pts',(-6.62794310576004,-1.37574525885523,
137.762380812953));
#241677=CARTESIAN_POINT('Ctrl Pts',(-6.58840230936357,-1.54442352027313,
137.770515044141));
#241678=CARTESIAN_POINT('Ctrl Pts',(-6.54886654853085,-1.71308030032959,
137.778648239426));
#241679=CARTESIAN_POINT('Ctrl Pts',(-6.50284709023229,-1.88023201037332,
137.786781434712));
#241680=CARTESIAN_POINT('Ctrl Pts',(-6.4504921137362,-2.04534605644792,
137.794914629997));
#241681=CARTESIAN_POINT('Ctrl Pts',(-6.39811630240641,-2.21052581019584,
137.803051061913));
#241682=CARTESIAN_POINT('Ctrl Pts',(-6.33940004546313,-2.3736659301633,
137.81118749383));
#241683=CARTESIAN_POINT('Ctrl Pts',(-6.27454113990482,-2.53424988579301,
137.819323925747));
#241684=CARTESIAN_POINT('Ctrl Pts',(-6.21682352896187,-2.67715273305712,
137.826564495223));
#241685=CARTESIAN_POINT('Ctrl Pts',(-6.15424223112599,-2.81803139624315,
137.833805064699));
#241686=CARTESIAN_POINT('Ctrl Pts',(-6.08696823580425,-2.95653626669962,
137.841045634175));
#241687=CARTESIAN_POINT('Ctrl Pts',(-6.00343429352145,-3.12851739847668,
137.850036230167));
#241688=CARTESIAN_POINT('Ctrl Pts',(-5.91263302428386,-3.29690429134303,
137.859026826159));
#241689=CARTESIAN_POINT('Ctrl Pts',(-5.8148925622811,-3.46111448656758,
137.868017422151));
#241690=CARTESIAN_POINT('Ctrl Pts',(-5.71710988895613,-3.62539559949928,
137.877011900926));
#241691=CARTESIAN_POINT('Ctrl Pts',(-5.61238216277252,-3.78549620326186,
137.8860063797));
#241692=CARTESIAN_POINT('Ctrl Pts',(-5.50108187272786,-3.9408612294199,
137.895000858475));
#241693=CARTESIAN_POINT('Ctrl Pts',(-5.38973960828518,-4.0962848479989,
137.903998729314));
#241694=CARTESIAN_POINT('Ctrl Pts',(-5.27181996794762,-4.24696912163422,
137.912996600154));
#241695=CARTESIAN_POINT('Ctrl Pts',(-5.14773770480197,-4.39238950032442,
137.921994470993));
#241696=CARTESIAN_POINT('Ctrl Pts',(-5.02366300552272,-4.53780101440907,
137.930991793336));
#241697=CARTESIAN_POINT('Ctrl Pts',(-4.89342659445217,-4.67794909155439,
137.939989115679));
#241698=CARTESIAN_POINT('Ctrl Pts',(-4.75748267824785,-4.81234325107548,
137.948986438022));
#241699=CARTESIAN_POINT('Ctrl Pts',(-4.62157878878662,-4.94669784015717,
137.957981111232));
#241700=CARTESIAN_POINT('Ctrl Pts',(-4.47997092572928,-5.07530172645476,
137.966975784442));
#241701=CARTESIAN_POINT('Ctrl Pts',(-4.33314991941424,-5.19770148968565,
137.975970457652));
#241702=CARTESIAN_POINT('Ctrl Pts',(-4.20240432861014,-5.30669971657128,
137.983980305102));
#241703=CARTESIAN_POINT('Ctrl Pts',(-4.06752526370029,-5.4107784463858,
137.991990152551));
#241704=CARTESIAN_POINT('Ctrl Pts',(-3.92888236737319,-5.50964357679733,
138.));
#241705=CARTESIAN_POINT('Ctrl Pts',(3.0991061983214,6.01563211736937,137.045755263024));
#241706=CARTESIAN_POINT('Ctrl Pts',(2.9337533076482,6.10081787314656,137.054504710927));
#241707=CARTESIAN_POINT('Ctrl Pts',(2.76488627843052,6.17918207037047,137.063254158829));
#241708=CARTESIAN_POINT('Ctrl Pts',(2.59307866646672,6.2504585455401,137.072003606731));
#241709=CARTESIAN_POINT('Ctrl Pts',(2.42127244185352,6.32173444515046,137.080752983982));
#241710=CARTESIAN_POINT('Ctrl Pts',(2.24652594672447,6.38592262741844,137.089502361232));
#241711=CARTESIAN_POINT('Ctrl Pts',(2.0694326968711,6.44280508110565,137.098251738482));
#241712=CARTESIAN_POINT('Ctrl Pts',(1.89234081822066,6.4996870943617,137.107001047988));
#241713=CARTESIAN_POINT('Ctrl Pts',(1.71290249405578,6.54926340459548,137.115750357493));
#241714=CARTESIAN_POINT('Ctrl Pts',(1.53172716625048,6.59136563150386,137.124499666998));
#241715=CARTESIAN_POINT('Ctrl Pts',(1.35055318107328,6.63346754640711,137.133248911666));
#241716=CARTESIAN_POINT('Ctrl Pts',(1.16764249714418,6.66809542395776,137.141998156333));
#241717=CARTESIAN_POINT('Ctrl Pts',(0.983616340614383,6.69513165624668,
137.150747401));
#241718=CARTESIAN_POINT('Ctrl Pts',(0.799591486713868,6.7221676971596,137.159496583736));
#241719=CARTESIAN_POINT('Ctrl Pts',(0.614451459526737,6.74161215869371,
137.168245766471));
#241720=CARTESIAN_POINT('Ctrl Pts',(0.428825047910307,6.75339900185712,
137.176994949207));
#241721=CARTESIAN_POINT('Ctrl Pts',(0.243199888596977,6.76518576550221,
137.185744072918));
#241722=CARTESIAN_POINT('Ctrl Pts',(0.0570886373917548,6.76931499599835,
137.194493196628));
#241723=CARTESIAN_POINT('Ctrl Pts',(-0.128876626811405,6.76577266947846,
137.203242320339));
#241724=CARTESIAN_POINT('Ctrl Pts',(-0.314840698188485,6.76223036567992,
137.21199138793));
#241725=CARTESIAN_POINT('Ctrl Pts',(-0.500658497951649,6.7510166087922,
137.220740455522));
#241726=CARTESIAN_POINT('Ctrl Pts',(-0.685698951926683,6.73216948296214,
137.229489523113));
#241727=CARTESIAN_POINT('Ctrl Pts',(-0.870738280460354,6.71332247176287,
137.238238537492));
#241728=CARTESIAN_POINT('Ctrl Pts',(-1.05499998761304,6.68684221356178,
137.24698755187));
#241729=CARTESIAN_POINT('Ctrl Pts',(-1.23785829161477,6.65281863948512,
137.255736566249));
#241730=CARTESIAN_POINT('Ctrl Pts',(-1.43007412917444,6.61705395368852,
137.264933299948));
#241731=CARTESIAN_POINT('Ctrl Pts',(-1.62073882535816,6.57295372727783,
137.274130033647));
#241732=CARTESIAN_POINT('Ctrl Pts',(-1.80913696091522,6.52068343478277,
137.283326767346));
#241733=CARTESIAN_POINT('Ctrl Pts',(-1.9883835618612,6.47095219815196,137.29207676506));
#241734=CARTESIAN_POINT('Ctrl Pts',(-2.16557827572541,6.41382586850888,
137.300826762774));
#241735=CARTESIAN_POINT('Ctrl Pts',(-2.34011918621708,6.34949849943275,
137.309576760487));
#241736=CARTESIAN_POINT('Ctrl Pts',(-2.514656556911,6.2851724349555,137.318326580746));
#241737=CARTESIAN_POINT('Ctrl Pts',(-2.68653996295324,6.21364572242376,
137.327076401004));
#241738=CARTESIAN_POINT('Ctrl Pts',(-2.85518555379978,6.13516132252226,
137.335826221262));
#241739=CARTESIAN_POINT('Ctrl Pts',(-3.02382794858668,6.05667841000517,
137.3445758757));
#241740=CARTESIAN_POINT('Ctrl Pts',(-3.18923239109251,5.97123819492097,
137.353325530137));
#241741=CARTESIAN_POINT('Ctrl Pts',(-3.35083705967659,5.87913088810735,
137.362075184575));
#241742=CARTESIAN_POINT('Ctrl Pts',(-3.51243888042357,5.78702520443129,
137.370824684824));
#241743=CARTESIAN_POINT('Ctrl Pts',(-3.67024081223644,5.68825280605813,
137.379574185073));
#241744=CARTESIAN_POINT('Ctrl Pts',(-3.82370687544351,5.58314917682539,
137.388323685322));
#241745=CARTESIAN_POINT('Ctrl Pts',(-3.97717043817763,5.47804726008059,
137.397073043012));
#241746=CARTESIAN_POINT('Ctrl Pts',(-4.12629803722406,5.36661448084277,
137.405822400703));
#241747=CARTESIAN_POINT('Ctrl Pts',(-4.27058317206852,5.24922931204622,
137.414571758393));
#241748=CARTESIAN_POINT('Ctrl Pts',(-4.41486614774784,5.13184589986834,
137.423320985153));
#241749=CARTESIAN_POINT('Ctrl Pts',(-4.55430658194368,5.00851045723076,
137.432070211913));
#241750=CARTESIAN_POINT('Ctrl Pts',(-4.68843089001804,4.87964187103159,
137.440819438673));
#241751=CARTESIAN_POINT('Ctrl Pts',(-4.82255336917822,4.75077504207976,
137.449568546129));
#241752=CARTESIAN_POINT('Ctrl Pts',(-4.95135966065145,4.61637541908083,
137.458317653585));
#241753=CARTESIAN_POINT('Ctrl Pts',(-5.07441230869278,4.47689945401807,
137.467066761041));
#241754=CARTESIAN_POINT('Ctrl Pts',(-5.1974634422643,4.33742520555499,137.475815760818));
#241755=CARTESIAN_POINT('Ctrl Pts',(-5.31476088454762,4.19287495491342,
137.484564760594));
#241756=CARTESIAN_POINT('Ctrl Pts',(-5.42590627628832,4.04373961586736,
137.49331376037));
#241757=CARTESIAN_POINT('Ctrl Pts',(-5.53706380672648,3.89458798906763,
137.502063715665));
#241758=CARTESIAN_POINT('Ctrl Pts',(-5.64206777071847,3.7408505015531,137.51081367096));
#241759=CARTESIAN_POINT('Ctrl Pts',(-5.74056148163992,3.58304938223186,
137.519563626254));
#241760=CARTESIAN_POINT('Ctrl Pts',(-5.83905138951873,3.42525435593301,
137.528313243695));
#241761=CARTESIAN_POINT('Ctrl Pts',(-5.93103139557645,3.26339625497197,
137.537062861137));
#241762=CARTESIAN_POINT('Ctrl Pts',(-6.01618907820842,3.09802485065013,
137.545812478578));
#241763=CARTESIAN_POINT('Ctrl Pts',(-6.10134392544986,2.93265895249636,
137.554561804694));
#241764=CARTESIAN_POINT('Ctrl Pts',(-6.1796767726184,2.76378023986018,137.563311130809));
#241765=CARTESIAN_POINT('Ctrl Pts',(-6.25092157009236,2.59196229227086,
137.572060456925));
#241766=CARTESIAN_POINT('Ctrl Pts',(-6.32216437407767,2.42014915229057,
137.580809538228));
#241767=CARTESIAN_POINT('Ctrl Pts',(-6.38631941548935,2.24539720662811,
137.58955861953));
#241768=CARTESIAN_POINT('Ctrl Pts',(-6.44316881037552,2.06829994947642,
137.598307700833));
#241769=CARTESIAN_POINT('Ctrl Pts',(-6.50002334524583,1.8911866802441,137.607057573175));
#241770=CARTESIAN_POINT('Ctrl Pts',(-6.54957082411105,1.71172794807668,
137.615807445517));
#241771=CARTESIAN_POINT('Ctrl Pts',(-6.5916429429609,1.53053334250311,137.62455731786));
#241772=CARTESIAN_POINT('Ctrl Pts',(-6.63371214082143,1.34935131693556,
137.633306582715));
#241773=CARTESIAN_POINT('Ctrl Pts',(-6.668306952397,1.16643393829707,137.642055847569));
#241774=CARTESIAN_POINT('Ctrl Pts',(-6.69530988153999,0.98240245834028,
137.650805112424));
#241775=CARTESIAN_POINT('Ctrl Pts',(-6.72231419690491,0.798361530946359,
137.659554826431));
#241776=CARTESIAN_POINT('Ctrl Pts',(-6.74172580829284,0.613206671361785,
137.668304540438));
#241777=CARTESIAN_POINT('Ctrl Pts',(-6.75347878028184,0.427566795112718,
137.677054254445));
#241778=CARTESIAN_POINT('Ctrl Pts',(-6.76248992368206,0.285234494206549,
137.683762764234));
#241779=CARTESIAN_POINT('Ctrl Pts',(-6.76699999999986,0.142617266095373,
137.690471274022));
#241780=CARTESIAN_POINT('Ctrl Pts',(-6.767,6.64344399020961E-12,137.69717978381));
#241781=CARTESIAN_POINT('Origin',(-1.11022302462516E-15,0.,-22.));
#241782=CARTESIAN_POINT('',(6.,0.,-24.));
#241783=CARTESIAN_POINT('',(5.65685424949238,-2.,-22.));
#241784=CARTESIAN_POINT('Ctrl Pts',(6.,9.71445146547012E-16,-24.));
#241785=CARTESIAN_POINT('Ctrl Pts',(6.,-0.253174643734702,-24.));
#241786=CARTESIAN_POINT('Ctrl Pts',(5.98240475886912,-0.521932274441712,
-23.9490088416061));
#241787=CARTESIAN_POINT('Ctrl Pts',(5.9188739106068,-1.01415562391481,-23.7442869722332));
#241788=CARTESIAN_POINT('Ctrl Pts',(5.87374622031366,-1.23776803829002,
-23.5906590864562));
#241789=CARTESIAN_POINT('Ctrl Pts',(5.78813771212597,-1.59074095999941,
-23.2376861647468));
#241790=CARTESIAN_POINT('Ctrl Pts',(5.74186082552466,-1.7443058152527,-23.0141063599154));
#241791=CARTESIAN_POINT('Ctrl Pts',(5.67565356574251,-1.94898067853762,
-22.522003946927));
#241792=CARTESIAN_POINT('Ctrl Pts',(5.65685424949238,-2.,-22.2532921208158));
#241793=CARTESIAN_POINT('Ctrl Pts',(5.65685424949238,-2.,-22.));
#241794=CARTESIAN_POINT('',(6.,0.,-20.));
#241795=CARTESIAN_POINT('Ctrl Pts',(6.,-3.46944695195361E-16,-20.));
#241796=CARTESIAN_POINT('Ctrl Pts',(6.,0.253174643734703,-20.));
#241797=CARTESIAN_POINT('Ctrl Pts',(5.98240475886912,0.521932274441713,
-20.0509911583939));
#241798=CARTESIAN_POINT('Ctrl Pts',(5.9188739106068,1.01415562391481,-20.2557130277668));
#241799=CARTESIAN_POINT('Ctrl Pts',(5.87374622031365,1.23776803829002,-20.4093409135438));
#241800=CARTESIAN_POINT('Ctrl Pts',(5.78813771212597,1.59074095999941,-20.7623138352532));
#241801=CARTESIAN_POINT('Ctrl Pts',(5.74186082552466,1.7443058152527,-20.9858936400846));
#241802=CARTESIAN_POINT('Ctrl Pts',(5.67565356574251,1.94898067853762,-21.477996053073));
#241803=CARTESIAN_POINT('Ctrl Pts',(5.65685424949238,2.,-21.7467078791842));
#241804=CARTESIAN_POINT('Ctrl Pts',(5.65685424949238,2.,-22.2532921208158));
#241805=CARTESIAN_POINT('Ctrl Pts',(5.67565356574251,1.94898067853762,-22.5220039469271));
#241806=CARTESIAN_POINT('Ctrl Pts',(5.74186082552466,1.7443058152527,-23.0141063599154));
#241807=CARTESIAN_POINT('Ctrl Pts',(5.78813771212597,1.59074095999941,-23.2376861647468));
#241808=CARTESIAN_POINT('Ctrl Pts',(5.87374622031365,1.23776803829002,-23.5906590864562));
#241809=CARTESIAN_POINT('Ctrl Pts',(5.9188739106068,1.01415562391481,-23.7442869722332));
#241810=CARTESIAN_POINT('Ctrl Pts',(5.98240475886912,0.521932274441715,
-23.9490088416061));
#241811=CARTESIAN_POINT('Ctrl Pts',(6.,0.253174643734703,-24.));
#241812=CARTESIAN_POINT('Ctrl Pts',(6.,7.11236625150491E-16,-24.));
#241813=CARTESIAN_POINT('Ctrl Pts',(5.65685424949238,-2.,-22.));
#241814=CARTESIAN_POINT('Ctrl Pts',(5.65685424949238,-2.,-21.7467078791842));
#241815=CARTESIAN_POINT('Ctrl Pts',(5.67565356574251,-1.94898067853762,
-21.477996053073));
#241816=CARTESIAN_POINT('Ctrl Pts',(5.74186082552466,-1.7443058152527,-20.9858936400846));
#241817=CARTESIAN_POINT('Ctrl Pts',(5.78813771212597,-1.59074095999941,
-20.7623138352532));
#241818=CARTESIAN_POINT('Ctrl Pts',(5.87374622031365,-1.23776803829002,
-20.4093409135438));
#241819=CARTESIAN_POINT('Ctrl Pts',(5.9188739106068,-1.01415562391481,-20.2557130277668));
#241820=CARTESIAN_POINT('Ctrl Pts',(5.98240475886912,-0.521932274441714,
-20.0509911583939));
#241821=CARTESIAN_POINT('Ctrl Pts',(6.,-0.253174643734704,-20.));
#241822=CARTESIAN_POINT('Ctrl Pts',(6.,-1.04083408558608E-16,-20.));
#241823=CARTESIAN_POINT('',(-5.65685424949238,-2.,-22.));
#241824=CARTESIAN_POINT('',(-1.11022302462516E-15,-2.,-22.));
#241825=CARTESIAN_POINT('',(-6.,0.,-20.));
#241826=CARTESIAN_POINT('Ctrl Pts',(-6.,-1.38777878078145E-16,-20.));
#241827=CARTESIAN_POINT('Ctrl Pts',(-6.,-0.253174643734703,-20.));
#241828=CARTESIAN_POINT('Ctrl Pts',(-5.98240475886912,-0.521932274441714,
-20.0509911583939));
#241829=CARTESIAN_POINT('Ctrl Pts',(-5.9188739106068,-1.01415562391481,
-20.2557130277668));
#241830=CARTESIAN_POINT('Ctrl Pts',(-5.87374622031365,-1.23776803829002,
-20.4093409135438));
#241831=CARTESIAN_POINT('Ctrl Pts',(-5.78813771212597,-1.59074095999941,
-20.7623138352532));
#241832=CARTESIAN_POINT('Ctrl Pts',(-5.74186082552466,-1.7443058152527,
-20.9858936400846));
#241833=CARTESIAN_POINT('Ctrl Pts',(-5.67565356574251,-1.94898067853762,
-21.477996053073));
#241834=CARTESIAN_POINT('Ctrl Pts',(-5.65685424949238,-2.,-21.7467078791842));
#241835=CARTESIAN_POINT('Ctrl Pts',(-5.65685424949238,-2.,-22.));
#241836=CARTESIAN_POINT('',(-6.,0.,-24.));
#241837=CARTESIAN_POINT('Ctrl Pts',(-6.,6.24500451351651E-16,-24.));
#241838=CARTESIAN_POINT('Ctrl Pts',(-6.,0.253174643734704,-24.));
#241839=CARTESIAN_POINT('Ctrl Pts',(-5.98240475886912,0.521932274441715,
-23.9490088416061));
#241840=CARTESIAN_POINT('Ctrl Pts',(-5.9188739106068,1.01415562391481,-23.7442869722332));
#241841=CARTESIAN_POINT('Ctrl Pts',(-5.87374622031365,1.23776803829002,
-23.5906590864562));
#241842=CARTESIAN_POINT('Ctrl Pts',(-5.78813771212597,1.59074095999941,
-23.2376861647468));
#241843=CARTESIAN_POINT('Ctrl Pts',(-5.74186082552466,1.7443058152527,-23.0141063599154));
#241844=CARTESIAN_POINT('Ctrl Pts',(-5.67565356574251,1.94898067853762,
-22.522003946927));
#241845=CARTESIAN_POINT('Ctrl Pts',(-5.65685424949238,2.,-22.2532921208158));
#241846=CARTESIAN_POINT('Ctrl Pts',(-5.65685424949238,2.,-21.7467078791842));
#241847=CARTESIAN_POINT('Ctrl Pts',(-5.67565356574251,1.94898067853762,
-21.477996053073));
#241848=CARTESIAN_POINT('Ctrl Pts',(-5.74186082552466,1.7443058152527,-20.9858936400846));
#241849=CARTESIAN_POINT('Ctrl Pts',(-5.78813771212597,1.59074095999941,
-20.7623138352532));
#241850=CARTESIAN_POINT('Ctrl Pts',(-5.87374622031365,1.23776803829002,
-20.4093409135438));
#241851=CARTESIAN_POINT('Ctrl Pts',(-5.9188739106068,1.01415562391481,-20.2557130277668));
#241852=CARTESIAN_POINT('Ctrl Pts',(-5.98240475886912,0.521932274441713,
-20.0509911583939));
#241853=CARTESIAN_POINT('Ctrl Pts',(-6.,0.253174643734703,-20.));
#241854=CARTESIAN_POINT('Ctrl Pts',(-6.,-2.94902990916057E-16,-20.));
#241855=CARTESIAN_POINT('Ctrl Pts',(-5.65685424949238,-2.,-22.));
#241856=CARTESIAN_POINT('Ctrl Pts',(-5.65685424949238,-2.,-22.2532921208158));
#241857=CARTESIAN_POINT('Ctrl Pts',(-5.67565356574251,-1.94898067853762,
-22.522003946927));
#241858=CARTESIAN_POINT('Ctrl Pts',(-5.74186082552466,-1.7443058152527,
-23.0141063599154));
#241859=CARTESIAN_POINT('Ctrl Pts',(-5.78813771212597,-1.59074095999941,
-23.2376861647468));
#241860=CARTESIAN_POINT('Ctrl Pts',(-5.87374622031365,-1.23776803829002,
-23.5906590864562));
#241861=CARTESIAN_POINT('Ctrl Pts',(-5.9188739106068,-1.01415562391481,
-23.7442869722332));
#241862=CARTESIAN_POINT('Ctrl Pts',(-5.98240475886912,-0.521932274441713,
-23.9490088416061));
#241863=CARTESIAN_POINT('Ctrl Pts',(-6.,-0.253174643734702,-24.));
#241864=CARTESIAN_POINT('Ctrl Pts',(-6.,1.05818132034585E-15,-24.));
#241865=CARTESIAN_POINT('Ctrl Pts',(-2.92234961580469,6.09539287100994,
7.33528614149682));
#241866=CARTESIAN_POINT('Ctrl Pts',(-3.93714486470952,5.60886538126811,
7.38828008561611));
#241867=CARTESIAN_POINT('Ctrl Pts',(-5.71537785310802,4.12322732536813,
7.49425881834364));
#241868=CARTESIAN_POINT('Ctrl Pts',(-6.99675326026537,0.871633769604885,
7.65322233967944));
#241869=CARTESIAN_POINT('Ctrl Pts',(-6.55091532659029,-2.56655158848262,
7.81217670550419));
#241870=CARTESIAN_POINT('Ctrl Pts',(-3.86326988828824,-6.37353479344272,
8.02411585993721));
#241871=CARTESIAN_POINT('Ctrl Pts',(2.36377026589466,-7.63953912008178,
8.28903980297847));
#241872=CARTESIAN_POINT('Ctrl Pts',(7.71195073098936,-2.1230738351773,8.606948534628));
#241873=CARTESIAN_POINT('Ctrl Pts',(6.24580147088772,4.06257053960132,8.87187247766926));
#241874=CARTESIAN_POINT('Ctrl Pts',(2.36304990153233,6.62817509056407,9.08381163210228));
#241875=CARTESIAN_POINT('Ctrl Pts',(-1.10032041202936,6.96614410245639,
9.24276599792703));
#241876=CARTESIAN_POINT('Ctrl Pts',(-4.28427191756992,5.58239383986575,
9.40172036375181));
#241877=CARTESIAN_POINT('Ctrl Pts',(-7.19973962574471,1.93580196426138,
9.61365951818479));
#241878=CARTESIAN_POINT('Ctrl Pts',(-6.77647567883404,-3.11256971208317,
9.82559867261786));
#241879=CARTESIAN_POINT('Ctrl Pts',(-3.29440639851251,-6.21029458306668,
10.0375378270508));
#241880=CARTESIAN_POINT('Ctrl Pts',(1.20026516117126,-7.35377856012818,
10.2494769814839));
#241881=CARTESIAN_POINT('Ctrl Pts',(6.76952833401824,-4.26652457372789,
10.5144009245251));
#241882=CARTESIAN_POINT('Ctrl Pts',(7.2358798186972,3.40243708410996,10.8323096561747));
#241883=CARTESIAN_POINT('Ctrl Pts',(2.10440537187899,7.14786414098517,11.0972335992159));
#241884=CARTESIAN_POINT('Ctrl Pts',(-2.51597475780455,6.57195704382539,
11.3091727536489));
#241885=CARTESIAN_POINT('Ctrl Pts',(-5.36562902415266,4.57639845624688,
11.4681271194737));
#241886=CARTESIAN_POINT('Ctrl Pts',(-6.88511019966572,1.4546699720389,11.6270814852985));
#241887=CARTESIAN_POINT('Ctrl Pts',(-6.72813106585684,-3.21150195768999,
11.8390206397315));
#241888=CARTESIAN_POINT('Ctrl Pts',(-3.12381767200652,-6.77133116212613,
12.0509597941645));
#241889=CARTESIAN_POINT('Ctrl Pts',(1.53599132603708,-6.86015371718211,
12.2628989485975));
#241890=CARTESIAN_POINT('Ctrl Pts',(5.69401924554645,-4.80588969870767,
12.4748381030305));
#241891=CARTESIAN_POINT('Ctrl Pts',(7.91717704197876,1.16114852504975,12.7397620460718));
#241892=CARTESIAN_POINT('Ctrl Pts',(3.2842236423008,7.29029237713238,13.0576707777213));
#241893=CARTESIAN_POINT('Ctrl Pts',(-3.04967515282414,6.79852489801197,
13.3225947207625));
#241894=CARTESIAN_POINT('Ctrl Pts',(-6.18512036033732,3.35634566664468,
13.5345338751956));
#241895=CARTESIAN_POINT('Ctrl Pts',(-7.05217846098628,-0.0127773233050138,
13.6934882410203));
#241896=CARTESIAN_POINT('Ctrl Pts',(-6.176389907705,-3.37239090485859,13.8524426068451));
#241897=CARTESIAN_POINT('Ctrl Pts',(-3.02267724704907,-6.81505045200992,
14.0643817612781));
#241898=CARTESIAN_POINT('Ctrl Pts',(2.0303998283825,-7.17541903106724,14.2763209157112));
#241899=CARTESIAN_POINT('Ctrl Pts',(5.62807325196858,-4.21257292617558,
14.4882600701441));
#241900=CARTESIAN_POINT('Ctrl Pts',(7.45088764127239,0.0519955308776357,
14.7001992245772));
#241901=CARTESIAN_POINT('Ctrl Pts',(5.25932460636586,6.03071000917909,14.9651231676184));
#241902=CARTESIAN_POINT('Ctrl Pts',(-2.24603046352291,7.67397127462124,
15.283031899268));
#241903=CARTESIAN_POINT('Ctrl Pts',(-6.73789351069379,3.1813912437732,15.5479558423092));
#241904=CARTESIAN_POINT('Ctrl Pts',(-6.88130840713808,-1.47253684735641,
15.7598949967422));
#241905=CARTESIAN_POINT('Ctrl Pts',(-5.34900987301425,-4.59581088177074,
15.918849362567));
#241906=CARTESIAN_POINT('Ctrl Pts',(-2.49890939824775,-6.57846977125929,
16.0778037283918));
#241907=CARTESIAN_POINT('Ctrl Pts',(2.1356643282549,-7.14285855133397,16.2897428828248));
#241908=CARTESIAN_POINT('Ctrl Pts',(6.20868011891633,-4.13055116299326,
16.5016820372578));
#241909=CARTESIAN_POINT('Ctrl Pts',(7.01495057508644,0.459834338936403,
16.7136211916908));
#241910=CARTESIAN_POINT('Ctrl Pts',(5.62639274700488,4.88488841563443,16.9255603461238));
#241911=CARTESIAN_POINT('Ctrl Pts',(0.0735112942413086,8.00153451654928,
17.1904842891651));
#241912=CARTESIAN_POINT('Ctrl Pts',(-6.69670162250066,4.36905886279388,
17.5083930208146));
#241913=CARTESIAN_POINT('Ctrl Pts',(-7.18745818769423,-1.96491832076134,
17.7733169638558));
#241914=CARTESIAN_POINT('Ctrl Pts',(-4.26990858085605,-5.5936259145728,
17.9852561182889));
#241915=CARTESIAN_POINT('Ctrl Pts',(-1.07477207623318,-6.96980984437503,
18.1442104841136));
#241916=CARTESIAN_POINT('Ctrl Pts',(2.37970350210302,-6.62252398667525,
18.3031648499384));
#241917=CARTESIAN_POINT('Ctrl Pts',(6.26747184736106,-4.0373613969903,18.5151040043714));
#241918=CARTESIAN_POINT('Ctrl Pts',(7.40267982884013,0.899718334147306,
18.7270431588044));
#241919=CARTESIAN_POINT('Ctrl Pts',(5.03000323061986,4.91121641654369,18.9389823132374));
#241920=CARTESIAN_POINT('Ctrl Pts',(1.09750105770811,7.36979793515926,19.1509214676704));
#241921=CARTESIAN_POINT('Ctrl Pts',(-5.14763615074514,6.12632031397724,
19.4158454107117));
#241922=CARTESIAN_POINT('Ctrl Pts',(-7.92851849591846,-1.03589691921599,
19.7337541423612));
#241923=CARTESIAN_POINT('Ctrl Pts',(-4.18228023263746,-6.16676505655972,
19.9986780854025));
#241924=CARTESIAN_POINT('Ctrl Pts',(0.393876779249377,-7.02606797887813,
20.2106172398355));
#241925=CARTESIAN_POINT('Ctrl Pts',(3.7160685048052,-5.99368160233694,20.3695716056603));
#241926=CARTESIAN_POINT('Ctrl Pts',(6.11448183316621,-3.48337833487705,
20.528525971485));
#241927=CARTESIAN_POINT('Ctrl Pts',(7.38673979810175,1.00874454769807,20.7404651259181));
#241928=CARTESIAN_POINT('Ctrl Pts',(5.03848790433384,5.49752684095302,20.952404280351));
#241929=CARTESIAN_POINT('Ctrl Pts',(0.627321250835717,7.00196024256239,
21.1643434347841));
#241930=CARTESIAN_POINT('Ctrl Pts',(-3.95891838810468,6.31232091809937,
21.3762825892171));
#241931=CARTESIAN_POINT('Ctrl Pts',(-7.8945072103994,1.30641281180972,21.6412065322584));
#241932=CARTESIAN_POINT('Ctrl Pts',(-5.34939273263063,-5.9429357525924,
21.9591152639079));
#241933=CARTESIAN_POINT('Ctrl Pts',(0.833163582985019,-7.40447821599224,
22.2240392069491));
#241934=CARTESIAN_POINT('Ctrl Pts',(4.86834028654934,-5.08134165505618,
22.4359783613822));
#241935=CARTESIAN_POINT('Ctrl Pts',(6.72073378548061,-2.13661453409292,
22.5949327272069));
#241936=CARTESIAN_POINT('Ctrl Pts',(6.91025718008171,1.33009714575273,22.7538870930317));
#241937=CARTESIAN_POINT('Ctrl Pts',(4.95547789167846,5.5699846743467,22.9658262474647));
#241938=CARTESIAN_POINT('Ctrl Pts',(0.252483078837816,7.4528795793316,23.1777654018977));
#241939=CARTESIAN_POINT('Ctrl Pts',(-4.07689061791219,5.72712336865149,
23.3897045563307));
#241940=CARTESIAN_POINT('Ctrl Pts',(-7.11243366736574,2.22074705990363,
23.6016437107637));
#241941=CARTESIAN_POINT('Ctrl Pts',(-6.84678358765764,-4.14143852226377,
23.866567653805));
#241942=CARTESIAN_POINT('Ctrl Pts',(-0.199013732592527,-7.99342739390318,
24.1844763854546));
#241943=CARTESIAN_POINT('Ctrl Pts',(5.4481367907149,-5.08313532347652,24.4494003284958));
#241944=CARTESIAN_POINT('Ctrl Pts',(7.0027744961245,-0.694204233260489,
24.6613394829288));
#241945=CARTESIAN_POINT('Ctrl Pts',(6.4949934177085,2.74744331816343,24.8202938487536));
#241946=CARTESIAN_POINT('Ctrl Pts',(4.38453006323543,5.50424461998147,24.9792482145783));
#241947=CARTESIAN_POINT('Ctrl Pts',(0.142302896148915,7.45394125903327,
25.1911873690113));
#241948=CARTESIAN_POINT('Ctrl Pts',(-4.65488093005226,5.82591153864809,
25.4031265234444));
#241949=CARTESIAN_POINT('Ctrl Pts',(-6.82149347660548,1.69947225302547,
25.6150656778774));
#241950=CARTESIAN_POINT('Ctrl Pts',(-6.84726779860935,-2.93825694432527,
25.8270048323104));
#241951=CARTESIAN_POINT('Ctrl Pts',(-2.5080668857004,-7.59865508012841,
26.0919287753516));
#241952=CARTESIAN_POINT('Ctrl Pts',(5.04702373367946,-6.20177711620133,
26.4098375070012));
#241953=CARTESIAN_POINT('Ctrl Pts',(7.44439418198704,-0.318519183587702,
26.6747614500424));
#241954=CARTESIAN_POINT('Ctrl Pts',(5.77123662450275,4.0266112284459,26.8867006044755));
#241955=CARTESIAN_POINT('Ctrl Pts',(3.14735236276397,6.31090781006993,27.0456549703002));
#241956=CARTESIAN_POINT('Ctrl Pts',(-0.248676851823201,7.03270734037595,
27.204609336125));
#241957=CARTESIAN_POINT('Ctrl Pts',(-4.73927178521599,5.75506675488882,
27.416548490558));
#241958=CARTESIAN_POINT('Ctrl Pts',(-7.32481757918334,1.39864547359366,
27.628487644991));
#241959=CARTESIAN_POINT('Ctrl Pts',(-6.28725926764394,-3.14505168345447,
27.840426799424));
#241960=CARTESIAN_POINT('Ctrl Pts',(-3.29087610852275,-6.68495060678104,
28.052365953857));
#241961=CARTESIAN_POINT('Ctrl Pts',(3.03618386846919,-7.4034820217757,28.3172898968983));
#241962=CARTESIAN_POINT('Ctrl Pts',(7.86714544468835,-1.42916427309168,
28.6351986285478));
#241963=CARTESIAN_POINT('Ctrl Pts',(5.86240940769175,4.59919722818268,28.9001225715891));
#241964=CARTESIAN_POINT('Ctrl Pts',(1.76568091712064,6.81198510420894,29.1120617260221));
#241965=CARTESIAN_POINT('Ctrl Pts',(-1.71310338992859,6.8409546890776,29.2710160918468));
#241966=CARTESIAN_POINT('Ctrl Pts',(-4.76235409461543,5.18081037961341,
29.4299704576716));
#241967=CARTESIAN_POINT('Ctrl Pts',(-7.34285557553195,1.28994666721163,
29.6419096121046));
#241968=CARTESIAN_POINT('Ctrl Pts',(-6.47398806841075,-3.7008972181341,
29.8538487665376));
#241969=CARTESIAN_POINT('Ctrl Pts',(-2.73097441663356,-6.47786677277848,
30.0657879209707));
#241970=CARTESIAN_POINT('Ctrl Pts',(1.84731678194465,-7.21843825795398,
30.2777270754036));
#241971=CARTESIAN_POINT('Ctrl Pts',(7.12105446691572,-3.64973174481743,
30.542651018445));
#241972=CARTESIAN_POINT('Ctrl Pts',(6.90582425186084,4.03039444344759,30.8605597500945));
#241973=CARTESIAN_POINT('Ctrl Pts',(1.46258344691281,7.30625135537594,31.1254836931357));
#241974=CARTESIAN_POINT('Ctrl Pts',(-3.08857164243337,6.32309223170156,
31.3374228475688));
#241975=CARTESIAN_POINT('Ctrl Pts',(-5.75013434350845,4.08281022265331,
31.4963772133934));
#241976=CARTESIAN_POINT('Ctrl Pts',(-6.98694564257054,0.838691421069132,
31.6553315792183));
#241977=CARTESIAN_POINT('Ctrl Pts',(-6.41700301498727,-3.79520259182766,
31.8672707336512));
#241978=CARTESIAN_POINT('Ctrl Pts',(-2.51135435712696,-7.02155688021231,
32.0792098880843));
#241979=CARTESIAN_POINT('Ctrl Pts',(2.13798780902864,-6.6970133133076,32.2911490425173));
#241980=CARTESIAN_POINT('Ctrl Pts',(6.09757350988195,-4.28229231467612,
32.5030881969503));
#241981=CARTESIAN_POINT('Ctrl Pts',(7.78310022106858,1.85830823027581,32.7680121399916));
#241982=CARTESIAN_POINT('Ctrl Pts',(2.625131338256,7.55269312393059,33.085920871641));
#241983=CARTESIAN_POINT('Ctrl Pts',(-3.64025173563295,6.50146341282771,
33.3508448146825));
#241984=CARTESIAN_POINT('Ctrl Pts',(-6.45826320049278,2.79492515001907,
33.5627839691153));
#241985=CARTESIAN_POINT('Ctrl Pts',(-7.02329053943438,-0.637788586672086,
33.7217383349402));
#241986=CARTESIAN_POINT('Ctrl Pts',(-5.85317344787643,-3.90655517061833,
33.8806927007649));
#241987=CARTESIAN_POINT('Ctrl Pts',(-2.40673684018765,-7.05613975127012,
34.092631855198));
#241988=CARTESIAN_POINT('Ctrl Pts',(2.65839357106603,-6.96721647076019,
34.3045710096309));
#241989=CARTESIAN_POINT('Ctrl Pts',(5.97929916872158,-3.69715575018147,
34.516510164064));
#241990=CARTESIAN_POINT('Ctrl Pts',(7.41695445299038,0.712191560617269,
34.728449318497));
#241991=CARTESIAN_POINT('Ctrl Pts',(4.70410047050428,6.47312886425953,34.9933732615382));
#241992=CARTESIAN_POINT('Ctrl Pts',(-2.91736413645297,7.44469438343174,
35.3112819931877));
#241993=CARTESIAN_POINT('Ctrl Pts',(-6.99335390629178,2.57166489816807,
35.576205936229));
#241994=CARTESIAN_POINT('Ctrl Pts',(-6.72370891457839,-2.07665803469601,
35.7881450906621));
#241995=CARTESIAN_POINT('Ctrl Pts',(-4.9206133586103,-5.05182624975003,
35.9470994564868));
#241996=CARTESIAN_POINT('Ctrl Pts',(-1.90599944753247,-6.77406663814406,
36.1060538223116));
#241997=CARTESIAN_POINT('Ctrl Pts',(2.76035781957077,-6.92545414505831,
36.3179929767445));
#241998=CARTESIAN_POINT('Ctrl Pts',(6.55035102549848,-3.56399539447913,
36.5299321311776));
#241999=CARTESIAN_POINT('Ctrl Pts',(6.94658480072917,1.07978645872825,36.7418712856106));
#242000=CARTESIAN_POINT('Ctrl Pts',(5.17128248312963,5.3643515597344,36.9538104400436));
#242001=CARTESIAN_POINT('Ctrl Pts',(-0.635984634104433,7.97655828506829,
37.2187343830848));
#242002=CARTESIAN_POINT('Ctrl Pts',(-7.05759166159136,3.75830918174626,
37.5366431147344));
#242003=CARTESIAN_POINT('Ctrl Pts',(-6.98501212133915,-2.59423685731685,
37.8015670577756));
#242004=CARTESIAN_POINT('Ctrl Pts',(-3.75731894680806,-5.95006928472314,
38.0135062122087));
#242005=CARTESIAN_POINT('Ctrl Pts',(-0.452781167209595,-7.03763976750855,
38.1724605780334));
#242006=CARTESIAN_POINT('Ctrl Pts',(2.95731728034348,-6.38553734742756,
38.3314149438582));
#242007=CARTESIAN_POINT('Ctrl Pts',(6.60065160063017,-3.46596146176918,
38.5433540982912));
#242008=CARTESIAN_POINT('Ctrl Pts',(7.29379945881797,1.55230511938344,38.7552932527242));
#242009=CARTESIAN_POINT('Ctrl Pts',(4.57490663890595,5.3377156570455,38.9672324071572));
#242010=CARTESIAN_POINT('Ctrl Pts',(0.439968219370932,7.43806817276445,
39.1791715615902));
#242011=CARTESIAN_POINT('Ctrl Pts',(-5.67037568507045,5.6459541372624,39.4440955046315));
#242012=CARTESIAN_POINT('Ctrl Pts',(-7.80549854202645,-1.73455483562362,
39.762004236281));
#242013=CARTESIAN_POINT('Ctrl Pts',(-3.61923596515816,-6.51318587448737,
40.0269281793224));
#242014=CARTESIAN_POINT('Ctrl Pts',(1.01507386770645,-6.9635045202935,40.2388673337553));
#242015=CARTESIAN_POINT('Ctrl Pts',(4.23268601565952,-5.64072277065963,
40.3978216995801));
#242016=CARTESIAN_POINT('Ctrl Pts',(6.39916207500406,-2.92771881331523,
40.5567760654049));
#242017=CARTESIAN_POINT('Ctrl Pts',(7.26825875330756,1.65948941013164,40.7687152198378));
#242018=CARTESIAN_POINT('Ctrl Pts',(4.53139098387666,5.92247055546574,40.9806543742709));
#242019=CARTESIAN_POINT('Ctrl Pts',(0.00424177129030791,7.03000435259828,
41.1925935287039));
#242020=CARTESIAN_POINT('Ctrl Pts',(-4.50282233051353,5.93658329652475,
41.4045326831369));
#242021=CARTESIAN_POINT('Ctrl Pts',(-7.97922898576225,0.601550764840454,
41.6694566261781));
#242022=CARTESIAN_POINT('Ctrl Pts',(-4.80159388164659,-6.39368314534717,
41.9873653578277));
#242023=CARTESIAN_POINT('Ctrl Pts',(1.48617170717807,-7.30148977017016,
42.2522893008689));
#242024=CARTESIAN_POINT('Ctrl Pts',(5.29955859651241,-4.62984328494818,
42.464228455302));
#242025=CARTESIAN_POINT('Ctrl Pts',(6.88365916119135,-1.53252107168022,
42.6231828211267));
#242026=CARTESIAN_POINT('Ctrl Pts',(6.76516872873376,1.93734477669137,42.7821371869515));
#242027=CARTESIAN_POINT('Ctrl Pts',(4.44228546067889,5.98728572002473,42.9940763413845));
#242028=CARTESIAN_POINT('Ctrl Pts',(-0.409087847200969,7.44592565517477,
43.2060154958175));
#242029=CARTESIAN_POINT('Ctrl Pts',(-4.56846195731471,5.34323259223688,
43.4179546502505));
#242030=CARTESIAN_POINT('Ctrl Pts',(-7.28127440862704,1.5816046165276,43.6298938046836));
#242031=CARTESIAN_POINT('Ctrl Pts',(-6.45276501179143,-4.73199558669585,
43.8948177477248));
#242032=CARTESIAN_POINT('Ctrl Pts',(0.510257573223466,-7.97960683093662,
44.2127264793743));
#242033=CARTESIAN_POINT('Ctrl Pts',(5.87723216227991,-4.5802403122302,44.4776504224156));
#242034=CARTESIAN_POINT('Ctrl Pts',(7.03674349602929,-0.0707893504553004,
44.6895895768486));
#242035=CARTESIAN_POINT('Ctrl Pts',(6.22591451695742,3.31230625246769,44.8485439426733));
#242036=CARTESIAN_POINT('Ctrl Pts',(3.87941151685467,5.87119911048039,45.0074983084981));
#242037=CARTESIAN_POINT('Ctrl Pts',(-0.518928492009235,7.43721746539336,
45.2194374629312));
#242038=CARTESIAN_POINT('Ctrl Pts',(-5.15293343338446,5.39040246736978,
45.4313766173641));
#242039=CARTESIAN_POINT('Ctrl Pts',(-6.94527669779923,1.08816854447353,
45.6433157717972));
#242040=CARTESIAN_POINT('Ctrl Pts',(-6.55988990217875,-3.53359231491712,
45.8552549262302));
#242041=CARTESIAN_POINT('Ctrl Pts',(-1.82469796774667,-7.79104844397787,
46.1201788692715));
#242042=CARTESIAN_POINT('Ctrl Pts',(5.57684727553539,-5.73003162580412,
46.4380876009209));
#242043=CARTESIAN_POINT('Ctrl Pts',(7.44332668653606,0.34255954900659,46.7030115439622));
#242044=CARTESIAN_POINT('Ctrl Pts',(5.39162868515475,4.52229038015749,46.9149506983953));
#242045=CARTESIAN_POINT('Ctrl Pts',(2.57560536052975,6.56503170665673,47.07390506422));
#242046=CARTESIAN_POINT('Ctrl Pts',(-0.871033878891199,6.98298737603286,
47.2328594300447));
#242047=CARTESIAN_POINT('Ctrl Pts',(-5.2307129054187,5.31235662474358,47.4447985844778));
#242048=CARTESIAN_POINT('Ctrl Pts',(-7.41995642837388,0.743914195422315,
47.6567377389107));
#242049=CARTESIAN_POINT('Ctrl Pts',(-5.98375640066137,-3.68993746935074,
47.8686768933438));
#242050=CARTESIAN_POINT('Ctrl Pts',(-2.68541139296351,-6.95032343328639,
48.0806160477768));
#242051=CARTESIAN_POINT('Ctrl Pts',(3.6804332198673,-7.10523538273054,48.3455399908181));
#242052=CARTESIAN_POINT('Ctrl Pts',(7.96285483987609,-0.726244288393699,
48.6634487224676));
#242053=CARTESIAN_POINT('Ctrl Pts',(5.43169215040701,5.10070383283746,48.9283726655089));
#242054=CARTESIAN_POINT('Ctrl Pts',(1.15495939305906,6.94167407484916,49.140311819942));
#242055=CARTESIAN_POINT('Ctrl Pts',(-2.3127010697674,6.66219168476068,49.2992661857666));
#242056=CARTESIAN_POINT('Ctrl Pts',(-5.20280583031192,4.73831448978248,
49.4582205515914));
#242057=CARTESIAN_POINT('Ctrl Pts',(-7.42828904121764,0.634044420759983,
49.6701597060245));
#242058=CARTESIAN_POINT('Ctrl Pts',(-6.12048357297907,-4.26014583811528,
49.8820988604574));
#242059=CARTESIAN_POINT('Ctrl Pts',(-2.14606795096395,-6.69442839531649,
50.0940380148904));
#242060=CARTESIAN_POINT('Ctrl Pts',(2.47984404763027,-7.02629373682747,
50.3059771693235));
#242061=CARTESIAN_POINT('Ctrl Pts',(7.41651765727688,-3.00420111996666,
50.5709011123647));
#242062=CARTESIAN_POINT('Ctrl Pts',(6.52141556975414,4.62662154643429,50.8888098440143));
#242063=CARTESIAN_POINT('Ctrl Pts',(0.809246122055264,7.40713034319324,
51.1537337870554));
#242064=CARTESIAN_POINT('Ctrl Pts',(-3.63685573074989,6.02445437817901,
51.3656729414886));
#242065=CARTESIAN_POINT('Ctrl Pts',(-6.0893784968316,3.55708501513851,51.5246273073133));
#242066=CARTESIAN_POINT('Ctrl Pts',(-7.03378339253583,0.216110848634113,
51.6835816731381));
#242067=CARTESIAN_POINT('Ctrl Pts',(-6.05536415093935,-4.34902924879671,
51.895520827571));
#242068=CARTESIAN_POINT('Ctrl Pts',(-1.8791229213296,-7.2165129235422,52.1074599820041));
#242069=CARTESIAN_POINT('Ctrl Pts',(2.72315518706222,-6.48115769113438,
52.3193991364371));
#242070=CARTESIAN_POINT('Ctrl Pts',(6.45313109988518,-3.72498713882919,
52.5313382908701));
#242071=CARTESIAN_POINT('Ctrl Pts',(7.58775913309835,2.54084038616979,52.7962622339114));
#242072=CARTESIAN_POINT('Ctrl Pts',(1.94537547108583,7.75564325145627,53.1141709655609));
#242073=CARTESIAN_POINT('Ctrl Pts',(-4.20217428426094,6.1532260231371,53.3790949086021));
#242074=CARTESIAN_POINT('Ctrl Pts',(-6.68057017534676,2.21150453160647,
53.5910340630352));
#242075=CARTESIAN_POINT('Ctrl Pts',(-6.9391191756799,-1.25777953088348,
53.7499884288599));
#242076=CARTESIAN_POINT('Ctrl Pts',(-5.48388405553002,-4.40996920369223,
53.9089427946847));
#242077=CARTESIAN_POINT('Ctrl Pts',(-1.77185193776174,-7.24168703535447,
54.1208819491178));
#242078=CARTESIAN_POINT('Ctrl Pts',(3.26546191579567,-6.70417185084077,
54.3328211035507));
#242079=CARTESIAN_POINT('Ctrl Pts',(6.28345936197013,-3.15263661665029,
54.5447602579837));
#242080=CARTESIAN_POINT('Ctrl Pts',(7.32463911719643,1.36678161371311,54.7566994124168));
#242081=CARTESIAN_POINT('Ctrl Pts',(4.11184826737424,6.86459484281479,55.0216233554581));
#242082=CARTESIAN_POINT('Ctrl Pts',(-3.56573393857394,7.15681699127929,
55.3395320871076));
#242083=CARTESIAN_POINT('Ctrl Pts',(-7.19376650262481,1.94169583427197,
55.6044560301488));
#242084=CARTESIAN_POINT('Ctrl Pts',(-6.51318411840115,-2.66443292294169,
55.8163951845819));
#242085=CARTESIAN_POINT('Ctrl Pts',(-4.4534845077477,-5.4680764462331,55.9753495504066));
#242086=CARTESIAN_POINT('Ctrl Pts',(-1.29808652736431,-6.91634181337834,
56.1343039162313));
#242087=CARTESIAN_POINT('Ctrl Pts',(3.36332330666462,-6.65353640872412,
56.3462430706644));
#242088=CARTESIAN_POINT('Ctrl Pts',(6.84046120552639,-2.96938583293011,
56.5581822250974));
#242089=CARTESIAN_POINT('Ctrl Pts',(6.82353936752462,1.6912390990088,56.7701213795304));
#242090=CARTESIAN_POINT('Ctrl Pts',(4.67546675461387,5.80158950661353,56.9820605339634));
#242091=CARTESIAN_POINT('Ctrl Pts',(-1.34047444450577,7.88879501530715,
57.2469844770046));
#242092=CARTESIAN_POINT('Ctrl Pts',(-7.36292825745679,3.11797617741172,
57.5648932086542));
#242093=CARTESIAN_POINT('Ctrl Pts',(-6.72758391760391,-3.20313500163717,
57.8298171516955));
#242094=CARTESIAN_POINT('Ctrl Pts',(-3.21515378405285,-6.25967701290882,
58.0417563061285));
#242095=CARTESIAN_POINT('Ctrl Pts',(0.172773783780828,-7.05007329764989,
58.2007106719533));
#242096=CARTESIAN_POINT('Ctrl Pts',(3.51165269883899,-6.09828730339489,
58.359665037778));
#242097=CARTESIAN_POINT('Ctrl Pts',(6.88187468914349,-2.86727940220291,
58.5716041922111));
#242098=CARTESIAN_POINT('Ctrl Pts',(7.12750634893194,2.19267302055105,58.783543346644));
#242099=CARTESIAN_POINT('Ctrl Pts',(4.08379892209254,5.7221993633646,58.995482501077));
#242100=CARTESIAN_POINT('Ctrl Pts',(-0.221027804521507,7.44779006728682,
59.2074216555101));
#242101=CARTESIAN_POINT('Ctrl Pts',(-6.14848117016335,5.1211461441805,59.4723455985513));
#242102=CARTESIAN_POINT('Ctrl Pts',(-7.62103803718001,-2.41955929938033,
59.7902543302009));
#242103=CARTESIAN_POINT('Ctrl Pts',(-3.02770308154028,-6.80833850929487,
60.0551782732421));
#242104=CARTESIAN_POINT('Ctrl Pts',(1.62828085824023,-6.84612822022322,
60.2671174276751));
#242105=CARTESIAN_POINT('Ctrl Pts',(4.71598617216184,-5.24336330102886,
60.4260717934999));
#242106=CARTESIAN_POINT('Ctrl Pts',(6.63347166576597,-2.34901391470771,
60.5850261593247));
#242107=CARTESIAN_POINT('Ctrl Pts',(7.0925660109032,2.29717169326795,60.7969653137576));
#242108=CARTESIAN_POINT('Ctrl Pts',(3.98862546939676,6.30079586988792,61.0089044681907));
#242109=CARTESIAN_POINT('Ctrl Pts',(-0.618871097123766,7.00271217138896,
61.2208436226237));
#242110=CARTESIAN_POINT('Ctrl Pts',(-5.01128255547801,5.51411618719717,
61.4327827770568));
#242111=CARTESIAN_POINT('Ctrl Pts',(-8.00114270057177,-0.108046355772149,
61.6977067200978));
#242112=CARTESIAN_POINT('Ctrl Pts',(-4.21599954944376,-6.79410301411839,
62.0156154517476));
#242113=CARTESIAN_POINT('Ctrl Pts',(2.12748151280638,-7.14102805062289,
62.2805393947886));
#242114=CARTESIAN_POINT('Ctrl Pts',(5.68906172348862,-4.14190135896367,
62.4924785492218));
#242115=CARTESIAN_POINT('Ctrl Pts',(6.99240019375371,-0.916364454238048,
62.6514329150465));
#242116=CARTESIAN_POINT('Ctrl Pts',(6.56682862513636,2.52934270515092,62.8103872808712));
#242117=CARTESIAN_POINT('Ctrl Pts',(3.89412582486431,6.35745817662179,63.0223264353044));
#242118=CARTESIAN_POINT('Ctrl Pts',(-1.06743866082989,7.38036153819596,
63.2342655897372));
#242119=CARTESIAN_POINT('Ctrl Pts',(-5.02407290057349,4.91728285538854,
63.4462047441704));
#242120=CARTESIAN_POINT('Ctrl Pts',(-7.39280100026574,0.93001265970799,
63.6581438986033));
#242121=CARTESIAN_POINT('Ctrl Pts',(-6.00795385229093,-5.28530500904657,
63.9230678416446));
#242122=CARTESIAN_POINT('Ctrl Pts',(1.21551241471566,-7.90297523322938,
64.2409765732942));
#242123=CARTESIAN_POINT('Ctrl Pts',(6.26006522526891,-4.04129219216908,
64.5059005163353));
#242124=CARTESIAN_POINT('Ctrl Pts',(7.01532315789409,0.553182746814791,
64.7178396707685));
#242125=CARTESIAN_POINT('Ctrl Pts',(5.90782867371946,3.85109655092691,64.8767940365932));
#242126=CARTESIAN_POINT('Ctrl Pts',(3.34375639684328,6.19193878123707,65.0357484024179));
#242127=CARTESIAN_POINT('Ctrl Pts',(-1.17607516319154,7.36195202496903,
65.247687556851));
#242128=CARTESIAN_POINT('Ctrl Pts',(-5.61042490559491,4.91246314058462,
65.4596267112839));
#242129=CARTESIAN_POINT('Ctrl Pts',(-7.01439055682164,0.468299377290018,
65.671565865717));
#242130=CARTESIAN_POINT('Ctrl Pts',(-6.22087619441535,-4.10111320864855,
65.88350502015));
#242131=CARTESIAN_POINT('Ctrl Pts',(-1.12696604053075,-7.92211499999566,
66.1484289631913));
#242132=CARTESIAN_POINT('Ctrl Pts',(6.06277297200943,-5.2131825077762,66.4663376948408));
#242133=CARTESIAN_POINT('Ctrl Pts',(7.38366945566897,1.00094184309718,66.7312616378821));
#242134=CARTESIAN_POINT('Ctrl Pts',(4.96958083852046,4.98237257263741,66.943200792315));
#242135=CARTESIAN_POINT('Ctrl Pts',(1.98358462215674,6.76747931875516,67.1021551581399));
#242136=CARTESIAN_POINT('Ctrl Pts',(-1.48653460954908,6.87830121153664,
67.2611095239646));
#242137=CARTESIAN_POINT('Ctrl Pts',(-5.68098076067773,4.82783057365139,
67.4730486783976));
#242138=CARTESIAN_POINT('Ctrl Pts',(-7.45668949435264,0.0833272357797441,
67.6849878328307));
#242139=CARTESIAN_POINT('Ctrl Pts',(-5.63315273213393,-4.20577811385,67.8969269872636));
#242140=CARTESIAN_POINT('Ctrl Pts',(-2.05880859419072,-7.16098717781453,
68.1088661416967));
#242141=CARTESIAN_POINT('Ctrl Pts',(4.29571221098905,-6.75106026423516,
68.3737900847379));
#242142=CARTESIAN_POINT('Ctrl Pts',(7.99588512145278,-0.0176077317945067,
68.6916988163875));
#242143=CARTESIAN_POINT('Ctrl Pts',(4.9582195286531,5.56206056255386,68.9566227594286));
#242144=CARTESIAN_POINT('Ctrl Pts',(0.535146807666416,7.01672199441423,
69.1685619138617));
#242145=CARTESIAN_POINT('Ctrl Pts',(-2.89409475134154,6.43098770826065,
69.3275162796864));
#242146=CARTESIAN_POINT('Ctrl Pts',(-5.60230340683511,4.25852102893992,
69.4864706455113));
#242147=CARTESIAN_POINT('Ctrl Pts',(-7.45525241801838,-0.0268482377574512,
69.6984097999442));
#242148=CARTESIAN_POINT('Ctrl Pts',(-5.71879957776433,-4.78586178669096,
69.9103489543773));
#242149=CARTESIAN_POINT('Ctrl Pts',(-1.54427169558857,-6.85829422219245,
70.1222881088102));
#242150=CARTESIAN_POINT('Ctrl Pts',(3.09285805960138,-6.7788444056032,70.3342272632433));
#242151=CARTESIAN_POINT('Ctrl Pts',(7.65358787062285,-2.33501825228283,
70.5991512062845));
#242152=CARTESIAN_POINT('Ctrl Pts',(6.08569908081881,5.18642192048741,70.9170599379341));
#242153=CARTESIAN_POINT('Ctrl Pts',(0.149496258939197,7.44971896383081,
71.1819838809753));
#242154=CARTESIAN_POINT('Ctrl Pts',(-4.1564535195748,5.67837535520366,71.3939230354084));
#242155=CARTESIAN_POINT('Ctrl Pts',(-6.38081912316377,3.00340405698944,
71.5528774012331));
#242156=CARTESIAN_POINT('Ctrl Pts',(-7.02501524399713,-0.408252188217427,
71.7118317670579));
#242157=CARTESIAN_POINT('Ctrl Pts',(-5.64660810487616,-4.86843712768816,
71.9237709214909));
#242158=CARTESIAN_POINT('Ctrl Pts',(-1.23105069577916,-7.35502050892989,
72.1357100759239));
#242159=CARTESIAN_POINT('Ctrl Pts',(3.28566072525786,-6.21387000785308,
72.3476492303569));
#242160=CARTESIAN_POINT('Ctrl Pts',(6.76075871342928,-3.13933136936446,
72.5595883847899));
#242161=CARTESIAN_POINT('Ctrl Pts',(7.32662904256254,3.20541028052231,72.8245123278312));
#242162=CARTESIAN_POINT('Ctrl Pts',(1.26079203493607,7.89410385780598,73.1424210594807));
#242163=CARTESIAN_POINT('Ctrl Pts',(-5.94922018012124,5.33486142538932,
73.4603297911302));
#242164=CARTESIAN_POINT('Ctrl Pts',(-7.7092089677762,-2.11567753454102,
73.7782385227798));
#242165=CARTESIAN_POINT('Ctrl Pts',(-2.39279777489314,-7.62420395766902,
74.0961472544292));
#242166=CARTESIAN_POINT('Ctrl Pts',(5.11354927904136,-6.14476086141691,
74.4140559860789));
#242167=CARTESIAN_POINT('Ctrl Pts',(7.9364501518555,0.983314385591691,74.7319647177282));
#242168=CARTESIAN_POINT('Ctrl Pts',(4.2113156217051,6.1504536875151,74.9968886607696));
#242169=CARTESIAN_POINT('Ctrl Pts',(-0.346322503067723,7.02052758700276,
75.2088278152026));
#242170=CARTESIAN_POINT('Ctrl Pts',(-4.8128110953465,5.69637269346616,75.4207669696356));
#242171=CARTESIAN_POINT('Ctrl Pts',(-7.34061996470585,1.3042858927657,75.6327061240687));
#242172=CARTESIAN_POINT('Ctrl Pts',(-6.2493396542438,-3.23469672666109,
75.8446452785016));
#242173=CARTESIAN_POINT('Ctrl Pts',(-3.95397872191655,-5.839635337819,76.0035996443264));
#242174=CARTESIAN_POINT('Ctrl Pts',(-0.675821523237244,-7.00452124014909,
76.1625540101512));
#242175=CARTESIAN_POINT('Ctrl Pts',(3.93109667452361,-6.32986103378635,
76.3744931645842));
#242176=CARTESIAN_POINT('Ctrl Pts',(7.88051160939144,-1.35360349210481,
76.6394171076255));
#242177=CARTESIAN_POINT('Ctrl Pts',(5.38962152202552,5.91453272720326,76.9573258392749));
#242178=CARTESIAN_POINT('Ctrl Pts',(-0.800496012063925,7.4079490135184,
77.2222497823163));
#242179=CARTESIAN_POINT('Ctrl Pts',(-4.82861356016322,5.1093508192883,77.4341889367493));
#242180=CARTESIAN_POINT('Ctrl Pts',(-7.36055018309903,1.19642912620305,
77.6461280911822));
#242181=CARTESIAN_POINT('Ctrl Pts',(-6.42463045389124,-3.78227880717078,
77.8580672456154));
#242182=CARTESIAN_POINT('Ctrl Pts',(-2.64387061986552,-6.52156062316159,
78.0700064000482));
#242183=CARTESIAN_POINT('Ctrl Pts',(0.793861069575679,-7.00736554888885,
78.2289607658731));
#242184=CARTESIAN_POINT('Ctrl Pts',(4.04171201133761,-5.76067128640936,
78.3879151316978));
#242185=CARTESIAN_POINT('Ctrl Pts',(7.10270483729022,-2.25211957723571,
78.5998542861308));
#242186=CARTESIAN_POINT('Ctrl Pts',(6.86684019138204,4.09646124035234,78.864778229172));
#242187=CARTESIAN_POINT('Ctrl Pts',(0.248045042783987,7.9980267408734,79.1826869608217));
#242188=CARTESIAN_POINT('Ctrl Pts',(-5.42557734563471,5.10700897344742,
79.4476109038628));
#242189=CARTESIAN_POINT('Ctrl Pts',(-6.99080999885538,0.741319638476606,
79.659550058296));
#242190=CARTESIAN_POINT('Ctrl Pts',(-6.3696296295627,-3.87775450816691,
79.8714892127287));
#242191=CARTESIAN_POINT('Ctrl Pts',(-2.4209356389253,-7.05128081154447,
80.083428367162));
#242192=CARTESIAN_POINT('Ctrl Pts',(2.23257239746651,-6.67356225655268,
80.2953675215949));
#242193=CARTESIAN_POINT('Ctrl Pts',(5.16003344080966,-4.80701978077493,
80.4543218874197));
#242194=CARTESIAN_POINT('Ctrl Pts',(6.8165859479432,-1.74783471113904,80.6132762532443));
#242195=CARTESIAN_POINT('Ctrl Pts',(6.86027898238168,2.90809757190748,80.8252154076776));
#242196=CARTESIAN_POINT('Ctrl Pts',(2.55255244952595,7.57753020198079,81.0901393507185));
#242197=CARTESIAN_POINT('Ctrl Pts',(-5.01276718579973,6.23715669761748,
81.4080480823685));
#242198=CARTESIAN_POINT('Ctrl Pts',(-7.44278175877897,0.351325870925839,
81.6729720254094));
#242199=CARTESIAN_POINT('Ctrl Pts',(-5.79278720436264,-3.98303848780944,
81.8849111798426));
#242200=CARTESIAN_POINT('Ctrl Pts',(-2.31706440085395,-7.08804446171282,
82.0968503342754));
#242201=CARTESIAN_POINT('Ctrl Pts',(2.74641161828516,-6.9309965827701,82.3087894887087));
#242202=CARTESIAN_POINT('Ctrl Pts',(6.03590165419069,-3.61783138536833,
82.5207286431415));
#242203=CARTESIAN_POINT('Ctrl Pts',(7.0459703068444,-0.296119431394292,
82.6796830089663));
#242204=CARTESIAN_POINT('Ctrl Pts',(6.31498177687263,3.10512082193679,82.8386373747911));
#242205=CARTESIAN_POINT('Ctrl Pts',(3.32037324809578,6.67050078333239,83.050576529224));
#242206=CARTESIAN_POINT('Ctrl Pts',(-2.98865185291137,7.41636353406801,
83.3155004722653));
#242207=CARTESIAN_POINT('Ctrl Pts',(-7.86412952468985,1.47831841928965,
83.633409203915));
#242208=CARTESIAN_POINT('Ctrl Pts',(-5.88251902724038,-4.57322643993298,
83.8983331469561));
#242209=CARTESIAN_POINT('Ctrl Pts',(-1.81038802006712,-6.79289882207679,
84.1102723013891));
#242210=CARTESIAN_POINT('Ctrl Pts',(2.84922712524779,-6.89137624265787,
84.3222114558222));
#242211=CARTESIAN_POINT('Ctrl Pts',(6.59366141269033,-3.47924123655858,
84.5341506102552));
#242212=CARTESIAN_POINT('Ctrl Pts',(6.93799848399193,1.17685587398636,84.7460897646883));
#242213=CARTESIAN_POINT('Ctrl Pts',(5.54517247875604,4.35711446526757,84.905044130513));
#242214=CARTESIAN_POINT('Ctrl Pts',(2.77800178948208,6.46556078145453,85.0639984963377));
#242215=CARTESIAN_POINT('Ctrl Pts',(-1.8155118597288,7.22664347358443,85.2759376507708));
#242216=CARTESIAN_POINT('Ctrl Pts',(-7.09332286364526,3.69042798594542,
85.540861593812));
#242217=CARTESIAN_POINT('Ctrl Pts',(-6.93549859986734,-3.99109229424056,
85.8587703254616));
#242218=CARTESIAN_POINT('Ctrl Pts',(-1.49474916635836,-7.29959965384536,
86.1236942685027));
#242219=CARTESIAN_POINT('Ctrl Pts',(3.04219705054772,-6.33766647085607,
86.3356334229359));
#242220=CARTESIAN_POINT('Ctrl Pts',(6.64600161752001,-3.38228092107058,
86.5475725773687));
#242221=CARTESIAN_POINT('Ctrl Pts',(7.2715845009025,1.6448553898765,86.7595117318021));
#242222=CARTESIAN_POINT('Ctrl Pts',(4.50525864164091,5.40587248128648,86.9714508862347));
#242223=CARTESIAN_POINT('Ctrl Pts',(1.37901740415747,6.91604621743004,87.1304052520598));
#242224=CARTESIAN_POINT('Ctrl Pts',(-2.09425987377605,6.71824722246359,
87.2893596178843));
#242225=CARTESIAN_POINT('Ctrl Pts',(-6.07874824292151,4.3092086287733,87.5012987723175));
#242226=CARTESIAN_POINT('Ctrl Pts',(-7.78849857574283,-1.80935842303686,
87.7662227153585));
#242227=CARTESIAN_POINT('Ctrl Pts',(-2.67323260379538,-7.54213404653577,
88.0841314470083));
#242228=CARTESIAN_POINT('Ctrl Pts',(3.61149077593769,-6.51732802243875,
88.3490553900493));
#242229=CARTESIAN_POINT('Ctrl Pts',(6.43251165346284,-2.83615461818277,
88.5609945444826));
#242230=CARTESIAN_POINT('Ctrl Pts',(7.2482914225384,1.75255047946504,88.7729336989153));
#242231=CARTESIAN_POINT('Ctrl Pts',(4.45432858118756,5.97833148112297,88.9848728533486));
#242232=CARTESIAN_POINT('Ctrl Pts',(-0.0929907162208757,7.0364881467041,
89.1968120077815));
#242233=CARTESIAN_POINT('Ctrl Pts',(-3.44997981742828,6.15069293185211,
89.3557663736062));
#242234=CARTESIAN_POINT('Ctrl Pts',(-5.95988905589371,3.74172321297108,
89.5147207394312));
#242235=CARTESIAN_POINT('Ctrl Pts',(-7.42015744381375,-0.679501814664077,
89.7266598938637));
#242236=CARTESIAN_POINT('Ctrl Pts',(-4.74003399571024,-6.43945383451685,
89.9915838369055));
#242237=CARTESIAN_POINT('Ctrl Pts',(2.87395643469399,-7.46795373187258,
90.3094925685547));
#242238=CARTESIAN_POINT('Ctrl Pts',(6.98182202518171,-2.60242029377199,
90.5744165115962));
#242239=CARTESIAN_POINT('Ctrl Pts',(6.73095821900039,2.0285908025635,90.7863556660291));
#242240=CARTESIAN_POINT('Ctrl Pts',(4.36659833218498,6.04499633866525,90.9982948204622));
#242241=CARTESIAN_POINT('Ctrl Pts',(-0.50395667669231,7.43824697596069,
91.2102339748951));
#242242=CARTESIAN_POINT('Ctrl Pts',(-4.64654291086805,5.28492683861115,
91.4221731293282));
#242243=CARTESIAN_POINT('Ctrl Pts',(-6.62070062977333,2.42893133981105,
91.5811274951529));
#242244=CARTESIAN_POINT('Ctrl Pts',(-6.96082222641317,-1.0333073566566,
91.7400818609777));
#242245=CARTESIAN_POINT('Ctrl Pts',(-5.19497417370953,-5.3416011215372,
91.9520210154106));
#242246=CARTESIAN_POINT('Ctrl Pts',(0.586787841480146,-7.97434436154179,
92.216944958452));
#242247=CARTESIAN_POINT('Ctrl Pts',(7.03974198416446,-3.80420705618134,
92.5348536901015));
#242248=CARTESIAN_POINT('Ctrl Pts',(6.99625226324018,2.56337364538507,92.7997776331427));
#242249=CARTESIAN_POINT('Ctrl Pts',(3.79408463287575,5.91826841134726,93.0117167875758));
#242250=CARTESIAN_POINT('Ctrl Pts',(-0.613955443182657,7.43183829499158,
93.2236559420087));
#242251=CARTESIAN_POINT('Ctrl Pts',(-5.22000878757889,5.3228750375121,93.4355950964418));
#242252=CARTESIAN_POINT('Ctrl Pts',(-6.96667552007488,0.993098640619434,
93.6475342508748));
#242253=CARTESIAN_POINT('Ctrl Pts',(-6.60909799444585,-2.46032680398553,
93.8064886166995));
#242254=CARTESIAN_POINT('Ctrl Pts',(-4.61594820447646,-5.31166568362871,
93.9654429825243));
#242255=CARTESIAN_POINT('Ctrl Pts',(-0.472760899151676,-7.4361923280231,
94.1773821369574));
#242256=CARTESIAN_POINT('Ctrl Pts',(5.63156268528228,-5.67626547028052,
94.4423060799985));
#242257=CARTESIAN_POINT('Ctrl Pts',(7.82178656201855,1.68807982872061,94.7602148116482));
#242258=CARTESIAN_POINT('Ctrl Pts',(3.64784541378302,6.4970496391739,95.0251387546894));
#242259=CARTESIAN_POINT('Ctrl Pts',(-0.966463691743675,6.96325549744629,
95.2370779091224));
#242260=CARTESIAN_POINT('Ctrl Pts',(-5.29940377398743,5.24647323154949,
95.4490170635554));
#242261=CARTESIAN_POINT('Ctrl Pts',(-7.42699769040191,0.648995927672792,
95.6609562179884));
#242262=CARTESIAN_POINT('Ctrl Pts',(-5.93818747723761,-3.77607497240045,
95.8728953724214));
#242263=CARTESIAN_POINT('Ctrl Pts',(-3.42074886478076,-6.16699776931195,
96.0318497382463));
#242264=CARTESIAN_POINT('Ctrl Pts',(-0.0523603294637201,-7.03690475684776,
96.1908041040708));
#242265=CARTESIAN_POINT('Ctrl Pts',(4.47669087758938,-5.95648369372606,
96.4027432585041));
#242266=CARTESIAN_POINT('Ctrl Pts',(7.96945573777992,-0.649817829033016,
96.6676672015452));
#242267=CARTESIAN_POINT('Ctrl Pts',(4.84419055635731,6.3689698055185,96.9855759331948));
#242268=CARTESIAN_POINT('Ctrl Pts',(-1.45394444495315,7.30783659695112,
97.2504998762359));
#242269=CARTESIAN_POINT('Ctrl Pts',(-5.26246902619562,4.66126580860892,
97.4624390306691));
#242270=CARTESIAN_POINT('Ctrl Pts',(-7.43762669290687,0.53932449052114,
97.6743781851019));
#242271=CARTESIAN_POINT('Ctrl Pts',(-6.06410627124071,-4.33683127853385,
97.8863173395352));
#242272=CARTESIAN_POINT('Ctrl Pts',(-2.05543456090541,-6.73023041788661,
98.098256493968));
#242273=CARTESIAN_POINT('Ctrl Pts',(1.41182644723664,-6.90942330194649,
98.2572108597928));
#242274=CARTESIAN_POINT('Ctrl Pts',(4.53639519977446,-5.37976660762449,
98.4161652256177));
#242275=CARTESIAN_POINT('Ctrl Pts',(7.27436459572607,-1.61371587820268,
98.6281043800504));
#242276=CARTESIAN_POINT('Ctrl Pts',(6.47672915079787,4.68897296586018,98.8930283230921));
#242277=CARTESIAN_POINT('Ctrl Pts',(-0.461826873943633,7.98853393736367,
99.2109370547412));
#242278=CARTESIAN_POINT('Ctrl Pts',(-5.85687752741677,4.60601951858521,
99.4758609977827));
#242279=CARTESIAN_POINT('Ctrl Pts',(-7.02900210216742,0.118779787425345,
99.6878001522157));
#242280=CARTESIAN_POINT('Ctrl Pts',(-6.00086032543074,-4.42705738428912,
99.8997393066486));
#242281=CARTESIAN_POINT('Ctrl Pts',(-1.78642551855117,-7.23810571033889,
100.111678461082));
#242282=CARTESIAN_POINT('Ctrl Pts',(2.81528895915896,-6.44941553851574,
100.323617615515));
#242283=CARTESIAN_POINT('Ctrl Pts',(5.56578953098327,-4.33074718488558,
100.48257198134));
#242284=CARTESIAN_POINT('Ctrl Pts',(6.94467503324845,-1.13677563468953,
100.641526347164));
#242285=CARTESIAN_POINT('Ctrl Pts',(6.57552301821642,3.50470487259935,100.853465501597));
#242286=CARTESIAN_POINT('Ctrl Pts',(1.87088082740638,7.77394963303761,101.118389444639));
#242287=CARTESIAN_POINT('Ctrl Pts',(-5.54586137949077,5.76830825193848,
101.436298176288));
#242288=CARTESIAN_POINT('Ctrl Pts',(-7.44462839157768,-0.309739064478167,
101.701222119329));
#242289=CARTESIAN_POINT('Ctrl Pts',(-5.41695646656369,-4.48079924003838,
101.913161273763));
#242290=CARTESIAN_POINT('Ctrl Pts',(-1.67970458774967,-7.26551816644961,
102.125100428195));
#242291=CARTESIAN_POINT('Ctrl Pts',(3.34992324121293,-6.66029313809475,
102.337039582629));
#242292=CARTESIAN_POINT('Ctrl Pts',(6.33280825391566,-3.06860755574061,
102.548978737061));
#242293=CARTESIAN_POINT('Ctrl Pts',(7.04448552145472,0.329557310058005,
102.707933102886));
#242294=CARTESIAN_POINT('Ctrl Pts',(6.01490902677195,3.65262091664403,102.866887468711));
#242295=CARTESIAN_POINT('Ctrl Pts',(2.71607318310361,6.93854492463233,103.078826623144));
#242296=CARTESIAN_POINT('Ctrl Pts',(-3.63423001483137,7.12227914130449,
103.343750566185));
#242297=CARTESIAN_POINT('Ctrl Pts',(-7.96420750968263,0.775472290042344,
103.661659297835));
#242298=CARTESIAN_POINT('Ctrl Pts',(-5.45402451437071,-5.07661765089621,
103.926583240876));
#242299=CARTESIAN_POINT('Ctrl Pts',(-1.20118223144524,-6.92662547255407,
104.138522395309));
#242300=CARTESIAN_POINT('Ctrl Pts',(3.44882239259403,-6.61171580102016,
104.350461549742));
#242301=CARTESIAN_POINT('Ctrl Pts',(6.87608904987469,-2.88112647857823,
104.562400704175));
#242302=CARTESIAN_POINT('Ctrl Pts',(6.80638321060322,1.78716543790136,104.774339858608));
#242303=CARTESIAN_POINT('Ctrl Pts',(5.13716049914964,4.83145591810317,104.933294224433));
#242304=CARTESIAN_POINT('Ctrl Pts',(2.19400096420631,6.68633905288312,105.092248590258));
#242305=CARTESIAN_POINT('Ctrl Pts',(-2.44889156040358,7.03728565090971,
105.304187744691));
#242306=CARTESIAN_POINT('Ctrl Pts',(-7.3925022614039,3.04719515005204,105.569111687732));
#242307=CARTESIAN_POINT('Ctrl Pts',(-6.55445662757077,-4.59010423053793,
105.887020419382));
#242308=CARTESIAN_POINT('Ctrl Pts',(-0.84187481190605,-7.40335579165466,
106.151944362423));
#242309=CARTESIAN_POINT('Ctrl Pts',(3.59195542694403,-6.04308161462527,
106.363883516856));
#242310=CARTESIAN_POINT('Ctrl Pts',(6.91962929457424,-2.7799086594323,106.575822671289));
#242311=CARTESIAN_POINT('Ctrl Pts',(7.09717573846594,2.28289004218361,106.787761825722));
#242312=CARTESIAN_POINT('Ctrl Pts',(4.00838403999365,5.78391477287955,106.999700980155));
#242313=CARTESIAN_POINT('Ctrl Pts',(0.760594345871106,7.01105416635946,
107.15865534598));
#242314=CARTESIAN_POINT('Ctrl Pts',(-2.68148139540731,6.50618380366963,
107.317609711804));
#242315=CARTESIAN_POINT('Ctrl Pts',(-6.436765619817,3.75346607319929,107.529548866237));
#242316=CARTESIAN_POINT('Ctrl Pts',(-7.59747484998492,-2.49256170860609,
107.794472809279));
#242317=CARTESIAN_POINT('Ctrl Pts',(-1.99422331481243,-7.74938913080039,
108.112381540928));
#242318=CARTESIAN_POINT('Ctrl Pts',(4.1749326607475,-6.17157738791076,108.377305483969));
#242319=CARTESIAN_POINT('Ctrl Pts',(6.65857430471428,-2.25485419013588,
108.589244638402));
#242320=CARTESIAN_POINT('Ctrl Pts',(7.06442890749218,2.38809671916914,108.801183792835));
#242321=CARTESIAN_POINT('Ctrl Pts',(3.90691519543565,6.34960660695168,109.013122947268));
#242322=CARTESIAN_POINT('Ctrl Pts',(-0.716295588026219,7.00055235982021,
109.225062101702));
#242323=CARTESIAN_POINT('Ctrl Pts',(-3.98156109415913,5.82070060526018,
109.384016467526));
#242324=CARTESIAN_POINT('Ctrl Pts',(-6.26807582664584,3.19874906681764,
109.542970833351));
#242325=CARTESIAN_POINT('Ctrl Pts',(-7.3307269191519,-1.33450441885264,
109.754909987784));
#242326=CARTESIAN_POINT('Ctrl Pts',(-4.15062511488581,-6.83423727441782,
110.019833930825));
#242327=CARTESIAN_POINT('Ctrl Pts',(3.52455864249324,-7.18383218801323,
110.337742662475));
#242328=CARTESIAN_POINT('Ctrl Pts',(7.18500597614252,-1.9733522999061,110.602666605516));
#242329=CARTESIAN_POINT('Ctrl Pts',(6.52466527420378,2.61719740366944,110.814605759949));
#242330=CARTESIAN_POINT('Ctrl Pts',(3.81362146703718,6.40823322260278,111.026544914382));
#242331=CARTESIAN_POINT('Ctrl Pts',(-1.16125352223572,7.36430449292163,
111.238484068815));
#242332=CARTESIAN_POINT('Ctrl Pts',(-5.09667868721811,4.85228596346781,
111.450423223248));
#242333=CARTESIAN_POINT('Ctrl Pts',(-6.80992886475379,1.83255372079252,
111.609377589073));
#242334=CARTESIAN_POINT('Ctrl Pts',(-6.84184037924238,-1.64620484327354,
111.768331954898));
#242335=CARTESIAN_POINT('Ctrl Pts',(-4.70108165962939,-5.78102849297703,
111.98027110933));
#242336=CARTESIAN_POINT('Ctrl Pts',(1.2912750482904,-7.89095030506626,112.245195052372));
#242337=CARTESIAN_POINT('Ctrl Pts',(7.34921693556565,-3.16527549573553,
112.563103784021));
#242338=CARTESIAN_POINT('Ctrl Pts',(6.74151534594509,3.17338951550774,112.828027727063));
#242339=CARTESIAN_POINT('Ctrl Pts',(3.25459340362493,6.23125998231941,113.039966881496));
#242340=CARTESIAN_POINT('Ctrl Pts',(-1.27025133821028,7.34817142334694,
113.251906035929));
#242341=CARTESIAN_POINT('Ctrl Pts',(-5.67125105544294,4.83925633475936,
113.463845190362));
#242342=CARTESIAN_POINT('Ctrl Pts',(-7.02727875005749,0.371706982716854,
113.675784344795));
#242343=CARTESIAN_POINT('Ctrl Pts',(-6.36501824456443,-3.03643327424791,
113.83473871062));
#242344=CARTESIAN_POINT('Ctrl Pts',(-4.12698786823344,-5.69988958634311,
113.993693076444));
#242345=CARTESIAN_POINT('Ctrl Pts',(0.188197924330976,-7.4488281459833,
114.205632230877));
#242346=CARTESIAN_POINT('Ctrl Pts',(6.11250753694742,-5.15477832482867,
114.470556173918));
#242347=CARTESIAN_POINT('Ctrl Pts',(7.64138120966544,2.37471087471314,114.788464905568));
#242348=CARTESIAN_POINT('Ctrl Pts',(3.0576301475705,6.79480154658071,115.053388848609));
#242349=CARTESIAN_POINT('Ctrl Pts',(-1.57983992658859,6.85018868327952,
115.265328003042));
#242350=CARTESIAN_POINT('Ctrl Pts',(-5.74356178094228,4.75611814378246,
115.477267157475));
#242351=CARTESIAN_POINT('Ctrl Pts',(-7.45529008054121,-0.0118415520598074,
115.689206311908));
#242352=CARTESIAN_POINT('Ctrl Pts',(-5.58012845229728,-4.28753765789555,
115.901145466341));
#242353=CARTESIAN_POINT('Ctrl Pts',(-2.86068114714526,-6.44592023352485,
116.060099832166));
#242354=CARTESIAN_POINT('Ctrl Pts',(0.571553529458742,-7.01385034941665,
116.219054197991));
#242355=CARTESIAN_POINT('Ctrl Pts',(4.98701779701701,-5.53625439257915,
116.430993352424));
#242356=CARTESIAN_POINT('Ctrl Pts',(7.99568601189068,0.0591030169962317,
116.695917295465));
#242357=CARTESIAN_POINT('Ctrl Pts',(4.26061901329965,6.77326244533743,117.013826027115));
#242358=CARTESIAN_POINT('Ctrl Pts',(-2.09594363167219,7.15020632356861,
117.278749970156));
#242359=CARTESIAN_POINT('Ctrl Pts',(-5.65490322588073,4.17648760277076,
117.490689124589));
#242360=CARTESIAN_POINT('Ctrl Pts',(-7.45615665129927,-0.122023442024885,
117.702628279022));
#242361=CARTESIAN_POINT('Ctrl Pts',(-5.65584968870064,-4.85724764719652,
117.914567433455));
#242362=CARTESIAN_POINT('Ctrl Pts',(-1.45081887747908,-6.88592312596942,
118.126506587888));
#242363=CARTESIAN_POINT('Ctrl Pts',(2.018678504524,-6.75709415192438,118.285460953713));
#242364=CARTESIAN_POINT('Ctrl Pts',(4.9953704984076,-4.95651528240232,118.444415319538));
#242365=CARTESIAN_POINT('Ctrl Pts',(7.38876452641094,-0.962609983517036,
118.65635447397));
#242366=CARTESIAN_POINT('Ctrl Pts',(6.03563693453518,5.24457574660108,118.921278417012));
#242367=CARTESIAN_POINT('Ctrl Pts',(-1.16806356881025,7.91615980315751,
119.239187148661));
#242368=CARTESIAN_POINT('Ctrl Pts',(-6.24207561025776,4.06877404786426,
119.504111091703));
#242369=CARTESIAN_POINT('Ctrl Pts',(-7.01186580799012,-0.504695037535718,
119.716050246136));
#242370=CARTESIAN_POINT('Ctrl Pts',(-5.58485557652853,-4.94151291796711,
119.927989400569));
#242371=CARTESIAN_POINT('Ctrl Pts',(-1.13785365035902,-7.36795626193152,
120.139928555001));
#242372=CARTESIAN_POINT('Ctrl Pts',(3.37584513009584,-6.17450260098888,
120.351867709435));
#242373=CARTESIAN_POINT('Ctrl Pts',(5.92773481558134,-3.82038535212645,
120.510822075259));
#242374=CARTESIAN_POINT('Ctrl Pts',(7.01809949255712,-0.516768491317174,
120.669776441084));
#242375=CARTESIAN_POINT('Ctrl Pts',(6.23900818738519,4.07372508214002,120.881715595517));
#242376=CARTESIAN_POINT('Ctrl Pts',(1.17448267020993,7.90917684874589,121.146639538559));
#242377=CARTESIAN_POINT('Ctrl Pts',(-6.03530163148667,5.25405488616963,
121.464548270208));
#242378=CARTESIAN_POINT('Ctrl Pts',(-7.38787504286815,-0.968365905902512,
121.729472213249));
#242379=CARTESIAN_POINT('Ctrl Pts',(-4.99848645493423,-4.94328962837636,
121.941411367682));
#242380=CARTESIAN_POINT('Ctrl Pts',(-1.02912307268412,-7.38580174594381,
122.153350522115));
#242381=CARTESIAN_POINT('Ctrl Pts',(3.92706612823956,-6.33716356359886,
122.365289676548));
#242382=CARTESIAN_POINT('Ctrl Pts',(6.57986650300704,-2.49522935110501,
122.577228830981));
#242383=CARTESIAN_POINT('Ctrl Pts',(6.98755045709731,0.952639959332536,
122.736183196806));
#242384=CARTESIAN_POINT('Ctrl Pts',(5.66749025225642,4.1713696074104,122.895137562631));
#242385=CARTESIAN_POINT('Ctrl Pts',(2.09039369796188,7.15197269252594,123.107076717064));
#242386=CARTESIAN_POINT('Ctrl Pts',(-4.2512015357783,6.77213212138965,123.372000660105));
#242387=CARTESIAN_POINT('Ctrl Pts',(-8.00159567484203,0.0665220734654481,
123.689909391754));
#242388=CARTESIAN_POINT('Ctrl Pts',(-4.98259894856729,-5.54004854622093,
123.954833334796));
#242389=CARTESIAN_POINT('Ctrl Pts',(-0.582521403186913,-7.00582957293448,
124.166772489229));
#242390=CARTESIAN_POINT('Ctrl Pts',(4.02127044483243,-6.28001160338379,
124.378711643662));
#242391=CARTESIAN_POINT('Ctrl Pts',(7.1043919316239,-2.26033309254376,124.590650798095));
#242392=CARTESIAN_POINT('Ctrl Pts',(6.62119186744593,2.38340742771311,124.802589952528));
#242393=CARTESIAN_POINT('Ctrl Pts',(4.68871164421649,5.26776683234803,124.961544318353));
#242394=CARTESIAN_POINT('Ctrl Pts',(1.5927301814374,6.85448617550486,125.120498684177));
#242395=CARTESIAN_POINT('Ctrl Pts',(-3.06299494632564,6.79253422265207,
125.33243783861));
#242396=CARTESIAN_POINT('Ctrl Pts',(-7.63349198563593,2.37997648572275,
125.597361781652));
#242397=CARTESIAN_POINT('Ctrl Pts',(-6.12182161169902,-5.15298541473229,
125.915270513301));
#242398=CARTESIAN_POINT('Ctrl Pts',(-0.182373686338716,-7.44883682297308,
126.180194456342));
#242399=CARTESIAN_POINT('Ctrl Pts',(4.11343992445248,-5.70092897500878,
126.392133610776));
#242400=CARTESIAN_POINT('Ctrl Pts',(7.13878949156039,-2.15565450021674,
126.604072765208));
#242401=CARTESIAN_POINT('Ctrl Pts',(6.86690194892787,2.90295505152627,126.816011919642));
#242402=CARTESIAN_POINT('Ctrl Pts',(3.4799576646154,6.11642929857729,127.027951074075));
#242403=CARTESIAN_POINT('Ctrl Pts',(0.136184311171292,7.05087498938877,
127.186905439899));
#242404=CARTESIAN_POINT('Ctrl Pts',(-3.24759578423723,6.24290731816938,
127.345859805724));
#242405=CARTESIAN_POINT('Ctrl Pts',(-6.74411635140901,3.16817831660003,
127.557798960157));
#242406=CARTESIAN_POINT('Ctrl Pts',(-7.34664802028274,-3.15614493226094,
127.822722903198));
#242407=CARTESIAN_POINT('Ctrl Pts',(-1.29951660707707,-7.89564532624417,
128.140631634848));
#242408=CARTESIAN_POINT('Ctrl Pts',(4.70551179355111,-5.77724752260976,
128.405555577889));
#242409=CARTESIAN_POINT('Ctrl Pts',(6.83222435584126,-1.65580480178665,
128.617494732322));
#242410=CARTESIAN_POINT('Ctrl Pts',(6.82495913021777,3.00484518735816,128.829433886755));
#242411=CARTESIAN_POINT('Ctrl Pts',(3.32874874236082,6.67090115483483,129.041373041188));
#242412=CARTESIAN_POINT('Ctrl Pts',(-1.3339621786439,6.90951211142804,129.253312195621));
#242413=CARTESIAN_POINT('Ctrl Pts',(-4.4818017325012,5.44489095512069,129.412266561446));
#242414=CARTESIAN_POINT('Ctrl Pts',(-6.52692378448263,2.63059614394271,
129.571220927271));
#242415=CARTESIAN_POINT('Ctrl Pts',(-7.18359298217773,-1.97900254517614,
129.783160081704));
#242416=CARTESIAN_POINT('Ctrl Pts',(-3.528544817525,-7.17522539280143,130.048084024745));
#242417=CARTESIAN_POINT('Ctrl Pts',(4.14741748141174,-6.84316350563237,
130.365992756394));
#242418=CARTESIAN_POINT('Ctrl Pts',(7.33163354923769,-1.32875117226272,
130.630916699436));
#242419=CARTESIAN_POINT('Ctrl Pts',(6.26701378668714,3.18520287977783,130.842855853869));
#242420=CARTESIAN_POINT('Ctrl Pts',(3.23062589135893,6.72102805265527,131.054795008302));
#242421=CARTESIAN_POINT('Ctrl Pts',(-1.809409625499,7.23239429306926,131.266734162735));
#242422=CARTESIAN_POINT('Ctrl Pts',(-5.50669623769313,4.38145058775621,
131.478673317168));
#242423=CARTESIAN_POINT('Ctrl Pts',(-6.94555312241035,1.22175125511097,
131.637627682993));
#242424=CARTESIAN_POINT('Ctrl Pts',(-6.66900335975431,-2.24614431714648,
131.796582048817));
#242425=CARTESIAN_POINT('Ctrl Pts',(-4.17018484809034,-6.17495082242762,
132.00852120325));
#242426=CARTESIAN_POINT('Ctrl Pts',(1.98559807003753,-7.74544305904998,
132.273445146292));
#242427=CARTESIAN_POINT('Ctrl Pts',(7.60084290492707,-2.50142866096168,
132.591353877941));
#242428=CARTESIAN_POINT('Ctrl Pts',(6.43371300725464,3.75842625377709,132.856277820982));
#242429=CARTESIAN_POINT('Ctrl Pts',(2.68948376270878,6.49520249623938,133.068216975416));
#242430=CARTESIAN_POINT('Ctrl Pts',(-1.91654836717798,7.20666392385459,
133.280156129848));
#242431=CARTESIAN_POINT('Ctrl Pts',(-6.0778526942598,4.31754549373526,133.492095284281));
#242432=CARTESIAN_POINT('Ctrl Pts',(-7.03256675939648,-0.252610300115997,
133.704034438715));
#242433=CARTESIAN_POINT('Ctrl Pts',(-6.07083740358252,-3.58863913962263,
133.862988804539));
#242434=CARTESIAN_POINT('Ctrl Pts',(-3.60554071796445,-6.04324618883724,
134.021943170364));
#242435=CARTESIAN_POINT('Ctrl Pts',(0.847672210623471,-7.40283294222638,
134.233882324797));
#242436=CARTESIAN_POINT('Ctrl Pts',(6.54534463423149,-4.59271145197401,
134.498806267838));
#242437=CARTESIAN_POINT('Ctrl Pts',(7.40081577286274,3.04264222337198,134.816714999488));
#242438=CARTESIAN_POINT('Ctrl Pts',(2.44336599080527,7.0390807783047,135.081638942529));
#242439=CARTESIAN_POINT('Ctrl Pts',(-2.18080593719544,6.68318470426492,
135.293578096962));
#242440=CARTESIAN_POINT('Ctrl Pts',(-6.14244425541415,4.22836746363605,
135.505517251395));
#242441=CARTESIAN_POINT('Ctrl Pts',(-7.42503155180524,-0.672671077163957,
135.717456405828));
#242442=CARTESIAN_POINT('Ctrl Pts',(-5.17798142336632,-4.76514587670965,
135.929395560261));
#242443=CARTESIAN_POINT('Ctrl Pts',(-2.27843768804545,-6.67432321415518,
136.088349926086));
#242444=CARTESIAN_POINT('Ctrl Pts',(1.19159215245574,-6.93518694849042,
136.247304291911));
#242445=CARTESIAN_POINT('Ctrl Pts',(5.45674202613881,-5.07331073985723,
136.459243446344));
#242446=CARTESIAN_POINT('Ctrl Pts',(7.96176695298124,0.769346198559143,
136.724167389385));
#242447=CARTESIAN_POINT('Ctrl Pts',(3.63863730986622,7.12111552809232,137.042076121035));
#242448=CARTESIAN_POINT('Ctrl Pts',(-2.7132561331389,6.94154457948401,137.307000064076));
#242449=CARTESIAN_POINT('Ctrl Pts',(-6.01384419569356,3.65176076193676,
137.518939218509));
#242450=CARTESIAN_POINT('Ctrl Pts',(-7.04258940770208,0.340934081417236,
137.677893584334));
#242451=CARTESIAN_POINT('Ctrl Pts',(-6.33771717830036,-3.08215861357682,
137.83685466469));
#242452=CARTESIAN_POINT('Ctrl Pts',(-4.84060268287388,-4.85066217551467,
137.942830956438));
#242453=CARTESIAN_POINT('Ctrl Pts',(-3.92431279643241,-5.50397225712299,
137.995822459578));
#242454=CARTESIAN_POINT('Ctrl Pts',(-3.09240756406622,6.45009718150145,
7.56239467184173));
#242455=CARTESIAN_POINT('Ctrl Pts',(-4.16625597930013,5.93525758761204,
7.61538861596101));
#242456=CARTESIAN_POINT('Ctrl Pts',(-6.04796825433211,4.36316698740353,
7.72136734868855));
#242457=CARTESIAN_POINT('Ctrl Pts',(-7.40390971324263,0.922356054745332,
7.88033087002435));
#242458=CARTESIAN_POINT('Ctrl Pts',(-6.93212749013402,-2.71590486739369,
8.03928523584911));
#242459=CARTESIAN_POINT('Ctrl Pts',(-4.08808205560294,-6.74442479383243,
8.25122439028213));
#242460=CARTESIAN_POINT('Ctrl Pts',(2.50132325387603,-8.0841006952593,8.51614833332338));
#242461=CARTESIAN_POINT('Ctrl Pts',(8.16072609698623,-2.24662016873822,
8.8340570649729));
#242462=CARTESIAN_POINT('Ctrl Pts',(6.60925838844497,4.29898044993359,9.09898100801417));
#242463=CARTESIAN_POINT('Ctrl Pts',(2.50056096992704,7.01388316961167,9.31092016244718));
#242464=CARTESIAN_POINT('Ctrl Pts',(-1.16435047560862,7.37151934125338,
9.46987452827195));
#242465=CARTESIAN_POINT('Ctrl Pts',(-4.53358311844593,5.90724560902383,
9.6288288940967));
#242466=CARTESIAN_POINT('Ctrl Pts',(-7.61870830154839,2.04845053597936,
9.84076804852971));
#242467=CARTESIAN_POINT('Ctrl Pts',(-7.17081369511765,-3.29369698590258,
10.0527072029627));
#242468=CARTESIAN_POINT('Ctrl Pts',(-3.48611514884083,-6.57168527676829,
10.2646463573957));
#242469=CARTESIAN_POINT('Ctrl Pts',(1.2701112294088,-7.78171110014282,10.4765855118288));
#242470=CARTESIAN_POINT('Ctrl Pts',(7.16346206903531,-4.51480301765152,
10.74150945487));
#242471=CARTESIAN_POINT('Ctrl Pts',(7.65695157177441,3.60043237751478,11.0594181865195));
#242472=CARTESIAN_POINT('Ctrl Pts',(2.22686534652227,7.5638140682943,11.3243421295608));
#242473=CARTESIAN_POINT('Ctrl Pts',(-2.66238485975687,6.95439367115044,
11.5362812839938));
#242474=CARTESIAN_POINT('Ctrl Pts',(-5.67786677217702,4.84270914258127,
11.6952356498186));
#242475=CARTESIAN_POINT('Ctrl Pts',(-7.285769897525,1.53932041547079,11.8541900156433));
#242476=CARTESIAN_POINT('Ctrl Pts',(-7.11965580283671,-3.39838631636118,
12.0661291700763));
#242477=CARTESIAN_POINT('Ctrl Pts',(-3.30559948933912,-7.16536980767384,
12.2780683245094));
#242478=CARTESIAN_POINT('Ctrl Pts',(1.62537403782534,-7.25936114246434,
12.4900074789424));
#242479=CARTESIAN_POINT('Ctrl Pts',(6.02536674244457,-5.08555498492485,
12.7019466333754));
#242480=CARTESIAN_POINT('Ctrl Pts',(8.37789497815503,1.22871831024241,12.9668705764166));
#242481=CARTESIAN_POINT('Ctrl Pts',(3.47533983566063,7.71453051659892,13.2847793080662));
#242482=CARTESIAN_POINT('Ctrl Pts',(-3.22714245398094,7.19414600682971,
13.5497032511075));
#242483=CARTESIAN_POINT('Ctrl Pts',(-6.54504611067856,3.55165879914496,
13.7616424055404));
#242484=CARTESIAN_POINT('Ctrl Pts',(-7.46256022823305,-0.0135208638365823,
13.9205967713652));
#242485=CARTESIAN_POINT('Ctrl Pts',(-6.53580761381524,-3.56863774504305,
14.07955113719));
#242486=CARTESIAN_POINT('Ctrl Pts',(-3.19857348071929,-7.21163321914283,
14.291490291623));
#242487=CARTESIAN_POINT('Ctrl Pts',(2.14855325776632,-7.59297243800312,
14.503429446056));
#242488=CARTESIAN_POINT('Ctrl Pts',(5.95558320653318,-4.45771180512786,
14.715368600489));
#242489=CARTESIAN_POINT('Ctrl Pts',(7.88447117219099,0.0550212651201416,
14.927307754922));
#242490=CARTESIAN_POINT('Ctrl Pts',(5.56537626663262,6.38165028175068,15.1922316979633));
#242491=CARTESIAN_POINT('Ctrl Pts',(-2.37673191358021,8.12053653256265,
15.5101404296128));
#242492=CARTESIAN_POINT('Ctrl Pts',(-7.12998634579964,3.36652339380924,
15.7750643726541));
#242493=CARTESIAN_POINT('Ctrl Pts',(-7.2817468703326,-1.55822700354007,
15.9870035270871));
#242494=CARTESIAN_POINT('Ctrl Pts',(-5.66028051609993,-4.86325121982078,
16.1459578929119));
#242495=CARTESIAN_POINT('Ctrl Pts',(-2.64432642941238,-6.96128538851076,
16.3049122587366));
#242496=CARTESIAN_POINT('Ctrl Pts',(2.25994333028622,-7.55851719237741,
16.5168514131696));
#242497=CARTESIAN_POINT('Ctrl Pts',(6.56997686340006,-4.37091701523981,
16.7287905676027));
#242498=CARTESIAN_POINT('Ctrl Pts',(7.42316596981569,0.486593109960187,
16.9407297220357));
#242499=CARTESIAN_POINT('Ctrl Pts',(5.95380490929089,5.16915081085088,17.1526688764687));
#242500=CARTESIAN_POINT('Ctrl Pts',(0.0777890780505113,8.4671613996115,
17.4175928195099));
#242501=CARTESIAN_POINT('Ctrl Pts',(-7.08639741108168,4.62330400239646,
17.7355015511595));
#242502=CARTESIAN_POINT('Ctrl Pts',(-7.60571217961958,-2.07926123727055,
18.0004254942007));
#242503=CARTESIAN_POINT('Ctrl Pts',(-4.5183839475935,-5.91913130284974,
18.2123646486338));
#242504=CARTESIAN_POINT('Ctrl Pts',(-1.13731542598947,-7.37539840075269,
18.3713190144585));
#242505=CARTESIAN_POINT('Ctrl Pts',(2.51818368012486,-7.0079032155646,18.5302733802833));
#242506=CARTESIAN_POINT('Ctrl Pts',(6.63218981176315,-4.27230433189676,
18.7422125347163));
#242507=CARTESIAN_POINT('Ctrl Pts',(7.8334580411794,0.952074921836845,18.9541516891493));
#242508=CARTESIAN_POINT('Ctrl Pts',(5.32271017592142,5.19701089600908,19.1660908435823));
#242509=CARTESIAN_POINT('Ctrl Pts',(1.16136705686085,7.79866267782204,19.3780299980154));
#242510=CARTESIAN_POINT('Ctrl Pts',(-5.44718841425855,6.4828243603618,19.6429539410565));
#242511=CARTESIAN_POINT('Ctrl Pts',(-8.38989641623108,-1.09617803812816,
19.9608626727062));
#242512=CARTESIAN_POINT('Ctrl Pts',(-4.42565631316116,-6.52562267142425,
20.2257866157473));
#242513=CARTESIAN_POINT('Ctrl Pts',(0.416797334882363,-7.43493031977308,
20.4377257701804));
#242514=CARTESIAN_POINT('Ctrl Pts',(3.93231470002717,-6.34246711051537,
20.5966801360051));
#242515=CARTESIAN_POINT('Ctrl Pts',(6.4702969723287,-3.68608377759403,20.7556345018299));
#242516=CARTESIAN_POINT('Ctrl Pts',(7.81659042501185,1.06744561042331,20.9675736562629));
#242517=CARTESIAN_POINT('Ctrl Pts',(5.33168859145039,5.81744001288424,21.1795128106959));
#242518=CARTESIAN_POINT('Ctrl Pts',(0.663826453443777,7.40941970128585,
21.391451965129));
#242519=CARTESIAN_POINT('Ctrl Pts',(-4.18929655188581,6.67964874851767,
21.603391119562));
#242520=CARTESIAN_POINT('Ctrl Pts',(-8.35390593924179,1.38243584517833,
21.8683150626032));
#242521=CARTESIAN_POINT('Ctrl Pts',(-5.66068565515894,-6.28876824822158,
22.1862237942527));
#242522=CARTESIAN_POINT('Ctrl Pts',(0.88164720339901,-7.83536108043323,
22.4511477372941));
#242523=CARTESIAN_POINT('Ctrl Pts',(5.151639709757,-5.37703609613148,22.663086891727));
#242524=CARTESIAN_POINT('Ctrl Pts',(7.11182805845451,-2.26094883068994,
22.8220412575518));
#242525=CARTESIAN_POINT('Ctrl Pts',(7.31238023601108,1.40749842257895,22.9809956233766));
#242526=CARTESIAN_POINT('Ctrl Pts',(5.24384804368006,5.89411432688507,23.1929347778096));
#242527=CARTESIAN_POINT('Ctrl Pts',(0.267175624221262,7.8865790255047,23.4048739322426));
#242528=CARTESIAN_POINT('Ctrl Pts',(-4.31413384508076,6.06039726724439,
23.6168130866756));
#242529=CARTESIAN_POINT('Ctrl Pts',(-7.52632181752917,2.34997721312367,
23.8287522411086));
#242530=CARTESIAN_POINT('Ctrl Pts',(-7.24521297571152,-4.38243793388043,
24.0936761841499));
#242531=CARTESIAN_POINT('Ctrl Pts',(-0.210594779177801,-8.45858250567698,
24.4115849157994));
#242532=CARTESIAN_POINT('Ctrl Pts',(5.76517584705003,-5.37893414206013,
24.6765088588406));
#242533=CARTESIAN_POINT('Ctrl Pts',(7.4102813380527,-0.73460150364279,24.8884480132737));
#242534=CARTESIAN_POINT('Ctrl Pts',(6.87295136244285,2.90732308447373,25.0474023790985));
#242535=CARTESIAN_POINT('Ctrl Pts',(4.63967550600167,5.82454871424181,25.2063567449232));
#242536=CARTESIAN_POINT('Ctrl Pts',(0.150583814495755,7.88770248668208,
25.4182958993562));
#242537=CARTESIAN_POINT('Ctrl Pts',(-4.92575868406381,6.16493413801628,
25.6302350537893));
#242538=CARTESIAN_POINT('Ctrl Pts',(-7.21845117750304,1.79836827932979,
25.8421742082222));
#242539=CARTESIAN_POINT('Ctrl Pts',(-7.24572536396301,-3.10924057500208,
26.0541133626553));
#242540=CARTESIAN_POINT('Ctrl Pts',(-2.65401681119048,-8.04083752314715,
26.3190373056965));
#242541=CARTESIAN_POINT('Ctrl Pts',(5.3407211394704,-6.56267215978184,26.6369460373461));
#242542=CARTESIAN_POINT('Ctrl Pts',(7.87759984423547,-0.337054515071836,
26.9018699803873));
#242543=CARTESIAN_POINT('Ctrl Pts',(6.10707757042656,4.26092858741369,27.1138091348203));
#242544=CARTESIAN_POINT('Ctrl Pts',(3.33050371548742,6.67815340862603,27.2727635006451));
#242545=CARTESIAN_POINT('Ctrl Pts',(-0.263147904490414,7.4419560403116,
27.4317178664699));
#242546=CARTESIAN_POINT('Ctrl Pts',(-5.01506042860352,6.08996674055397,
27.6436570209029));
#242547=CARTESIAN_POINT('Ctrl Pts',(-7.75106481605285,1.48003572830395,
27.8555961753358));
#242548=CARTESIAN_POINT('Ctrl Pts',(-6.65312870553,-3.32806915459214,28.0675353297689));
#242549=CARTESIAN_POINT('Ctrl Pts',(-3.482379423516,-7.07396257792533,28.2794744842018));
#242550=CARTESIAN_POINT('Ctrl Pts',(3.21286608213192,-7.8343069154852,28.5443984272432));
#242551=CARTESIAN_POINT('Ctrl Pts',(8.32495193223544,-1.51233048383331,
28.8623071588927));
#242552=CARTESIAN_POINT('Ctrl Pts',(6.20355589829181,4.86683462517456,29.1272311019339));
#242553=CARTESIAN_POINT('Ctrl Pts',(1.86842977113328,7.20838949201477,29.339170256367));
#242554=CARTESIAN_POINT('Ctrl Pts',(-1.81279264205507,7.23904488070974,
29.4981246221917));
#242555=CARTESIAN_POINT('Ctrl Pts',(-5.03948594832806,5.48229312442995,
29.6570789880165));
#242556=CARTESIAN_POINT('Ctrl Pts',(-7.7701524830614,1.36501149942906,29.8690181424494));
#242557=CARTESIAN_POINT('Ctrl Pts',(-6.85072366569395,-3.9162605628341,
30.0809572968826));
#242558=CARTESIAN_POINT('Ctrl Pts',(-2.88989582135995,-6.85482808039567,
30.2928964513155));
#242559=CARTESIAN_POINT('Ctrl Pts',(1.95481620639003,-7.63849504827036,
30.5048356057486));
#242560=CARTESIAN_POINT('Ctrl Pts',(7.53544428035591,-3.86211765814873,
30.7697595487898));
#242561=CARTESIAN_POINT('Ctrl Pts',(7.3076893459521,4.26493195601293,31.0876682804394));
#242562=CARTESIAN_POINT('Ctrl Pts',(1.54769439284355,7.73141818286851,31.3525922234805));
#242563=CARTESIAN_POINT('Ctrl Pts',(-3.26830241582556,6.6910468685367,31.5645313779137));
#242564=CARTESIAN_POINT('Ctrl Pts',(-6.08474730131315,4.32039792463397,
31.7234857437383));
#242565=CARTESIAN_POINT('Ctrl Pts',(-7.39353136871431,0.887496718532063,
31.8824401095632));
#242566=CARTESIAN_POINT('Ctrl Pts',(-6.79042252674316,-4.01605377353168,
32.0943792639961));
#242567=CARTESIAN_POINT('Ctrl Pts',(-2.65749558780613,-7.43015671035946,
32.3063184184292));
#242568=CARTESIAN_POINT('Ctrl Pts',(2.26240201951379,-7.08672723986146,
32.5182575728622));
#242569=CARTESIAN_POINT('Ctrl Pts',(6.45240471654349,-4.53148831810734,
32.7301967272952));
#242570=CARTESIAN_POINT('Ctrl Pts',(8.23601593229881,1.9664472712618,32.9951206703364));
#242571=CARTESIAN_POINT('Ctrl Pts',(2.77789350157973,7.99220093968132,33.313029401986));
#242572=CARTESIAN_POINT('Ctrl Pts',(-3.85208598639099,6.87979786080079,
33.5779533450272));
#242573=CARTESIAN_POINT('Ctrl Pts',(-6.8340837331447,2.95756798850223,33.7898924994603));
#242574=CARTESIAN_POINT('Ctrl Pts',(-7.43199125502254,-0.674902906563349,
33.948846865285));
#242575=CARTESIAN_POINT('Ctrl Pts',(-6.19378247767171,-4.13388620366533,
34.1078012311098));
#242576=CARTESIAN_POINT('Ctrl Pts',(-2.54679014757844,-7.46675203470667,
34.3197403855428));
#242577=CARTESIAN_POINT('Ctrl Pts',(2.81309133683725,-7.37265411302604,
34.5316795399758));
#242578=CARTESIAN_POINT('Ctrl Pts',(6.32724773147186,-3.91230137063581,
34.7436186944088));
#242579=CARTESIAN_POINT('Ctrl Pts',(7.84856333708846,0.753635553120347,
34.9555578488418));
#242580=CARTESIAN_POINT('Ctrl Pts',(4.97784241777191,6.84981446256493,35.2204817918832));
#242581=CARTESIAN_POINT('Ctrl Pts',(-3.08713196871166,7.87791751506195,
35.5383905235326));
#242582=CARTESIAN_POINT('Ctrl Pts',(-7.40031254338871,2.72131573180937,
35.8033144665739));
#242583=CARTESIAN_POINT('Ctrl Pts',(-7.11497631685437,-2.19750333079328,
36.0152536210069));
#242584=CARTESIAN_POINT('Ctrl Pts',(-5.206954666791,-5.34580312450827,36.1742079868317));
#242585=CARTESIAN_POINT('Ctrl Pts',(-2.01691374528798,-7.16826446705451,
36.3331623526564));
#242586=CARTESIAN_POINT('Ctrl Pts',(2.92098910910757,-7.32846154578664,
36.5451015070894));
#242587=CARTESIAN_POINT('Ctrl Pts',(6.93153035112154,-3.77139212111251,
36.7570406615225));
#242588=CARTESIAN_POINT('Ctrl Pts',(7.35082184076201,1.14262160642573,36.9689798159554));
#242589=CARTESIAN_POINT('Ctrl Pts',(5.47221077870483,5.67651496929609,37.1809189703885));
#242590=CARTESIAN_POINT('Ctrl Pts',(-0.67299397803026,8.44073174631607,
37.4458429134297));
#242591=CARTESIAN_POINT('Ctrl Pts',(-7.46828843488125,3.97701345481512,
37.7637516450793));
#242592=CARTESIAN_POINT('Ctrl Pts',(-7.39148533163188,-2.74520120288113,
38.0286755881206));
#242593=CARTESIAN_POINT('Ctrl Pts',(-3.97596559592911,-6.29631689626835,
38.2406147425535));
#242594=CARTESIAN_POINT('Ctrl Pts',(-0.479129498664982,-7.4471754962219,
38.3995691083783));
#242595=CARTESIAN_POINT('Ctrl Pts',(3.12941007387295,-6.7571258028181,38.558523474203));
#242596=CARTESIAN_POINT('Ctrl Pts',(6.98475802729447,-3.66765337835299,
38.7704626286361));
#242597=CARTESIAN_POINT('Ctrl Pts',(7.71824168307701,1.64263716666871,38.9824017830691));
#242598=CARTESIAN_POINT('Ctrl Pts',(4.84113051310985,5.64832906487674,39.1943409375021));
#242599=CARTESIAN_POINT('Ctrl Pts',(0.46557093722521,7.87090571062995,39.4062800919351));
#242600=CARTESIAN_POINT('Ctrl Pts',(-6.00034731120954,5.97450461984868,
39.6712040349764));
#242601=CARTESIAN_POINT('Ctrl Pts',(-8.25971766079083,-1.83549239453124,
39.9891127666259));
#242602=CARTESIAN_POINT('Ctrl Pts',(-3.82984726203311,-6.89220247827404,
40.2540367096672));
#242603=CARTESIAN_POINT('Ctrl Pts',(1.07414324747652,-7.36872615600191,
40.4659758641002));
#242604=CARTESIAN_POINT('Ctrl Pts',(4.47899531950356,-5.96896882852342,
40.624930229925));
#242605=CARTESIAN_POINT('Ctrl Pts',(6.77154338324349,-3.09808920698211,
40.7838845957497));
#242606=CARTESIAN_POINT('Ctrl Pts',(7.69121470776753,1.75605874691569,40.9958237501828));
#242607=CARTESIAN_POINT('Ctrl Pts',(4.79508258645515,6.26711213628601,41.2077629046157));
#242608=CARTESIAN_POINT('Ctrl Pts',(0.00448860928583322,7.43909575973327,
41.4197020590487));
#242609=CARTESIAN_POINT('Ctrl Pts',(-4.76485146035186,6.28204612877034,
41.6316412134818));
#242610=CARTESIAN_POINT('Ctrl Pts',(-8.4435578609544,0.636556326217869,
41.896565156523));
#242611=CARTESIAN_POINT('Ctrl Pts',(-5.08100918482557,-6.7657456226258,
42.2144738881726));
#242612=CARTESIAN_POINT('Ctrl Pts',(1.57265530582791,-7.72637951055219,
42.4793978312138));
#242613=CARTESIAN_POINT('Ctrl Pts',(5.60795156111167,-4.89926404335092,
42.6913369856469));
#242614=CARTESIAN_POINT('Ctrl Pts',(7.28423441993201,-1.62170184173807,
42.8502913514716));
#242615=CARTESIAN_POINT('Ctrl Pts',(7.15884876873537,2.05008312805698,43.0092457172964));
#242616=CARTESIAN_POINT('Ctrl Pts',(4.70079181698436,6.335699037752,43.2211848717293));
#242617=CARTESIAN_POINT('Ctrl Pts',(-0.43289356831613,7.87922043721453,
43.4331240261624));
#242618=CARTESIAN_POINT('Ctrl Pts',(-4.83431080133031,5.6541670426541,43.6450631805954));
#242619=CARTESIAN_POINT('Ctrl Pts',(-7.70498777268218,1.67364166595904,
43.8570023350284));
#242620=CARTESIAN_POINT('Ctrl Pts',(-6.82826559275586,-5.00736081209647,
44.1219262780697));
#242621=CARTESIAN_POINT('Ctrl Pts',(0.539950583094435,-8.44395769377002,
44.4398350097192));
#242622=CARTESIAN_POINT('Ctrl Pts',(6.21924122155443,-4.84677456460966,
44.7047589527604));
#242623=CARTESIAN_POINT('Ctrl Pts',(7.44622706873499,-0.0749087383720799,
44.9166981071936));
#242624=CARTESIAN_POINT('Ctrl Pts',(6.58821416894859,3.50505663464716,45.0756524730181));
#242625=CARTESIAN_POINT('Ctrl Pts',(4.10516300101935,6.21285709320837,45.2346068388431));
#242626=CARTESIAN_POINT('Ctrl Pts',(-0.549126081705336,7.87000549872679,
45.4465459932759));
#242627=CARTESIAN_POINT('Ctrl Pts',(-5.45279395741946,5.70408183651311,
45.6584851477091));
#242628=CARTESIAN_POINT('Ctrl Pts',(-7.34943761644713,1.1514914641658,45.8704243021421));
#242629=CARTESIAN_POINT('Ctrl Pts',(-6.94162431600446,-3.73921981951735,
46.082363456575));
#242630=CARTESIAN_POINT('Ctrl Pts',(-1.93088115367067,-8.24442667977177,
46.3472873996164));
#242631=CARTESIAN_POINT('Ctrl Pts',(5.90137627792282,-6.06347476227379,
46.6651961312657));
#242632=CARTESIAN_POINT('Ctrl Pts',(7.87647022887751,0.362493842202579,
46.9301200743072));
#242633=CARTESIAN_POINT('Ctrl Pts',(5.7053794106066,4.78545239860063,47.1420592287401));
#242634=CARTESIAN_POINT('Ctrl Pts',(2.7254854983381,6.94706533338848,47.3010135945649));
#242635=CARTESIAN_POINT('Ctrl Pts',(-0.921721255073133,7.38934276194536,
47.4599679603896));
#242636=CARTESIAN_POINT('Ctrl Pts',(-5.53509958791175,5.62149433473857,
47.6719071148227));
#242637=CARTESIAN_POINT('Ctrl Pts',(-7.85174000401877,0.78720419777877,
47.8838462692556));
#242638=CARTESIAN_POINT('Ctrl Pts',(-6.331964339536,-3.90466304217649,48.0957854236888));
#242639=CARTESIAN_POINT('Ctrl Pts',(-2.84168138518263,-7.35477803256649,
48.3077245781216));
#242640=CARTESIAN_POINT('Ctrl Pts',(3.89460571952277,-7.51870464888691,
48.572648521163));
#242641=CARTESIAN_POINT('Ctrl Pts',(8.42623086752431,-0.768506040016876,
48.8905572528124));
#242642=CARTESIAN_POINT('Ctrl Pts',(5.74777425697222,5.39752500160179,49.1554811958538));
#242643=CARTESIAN_POINT('Ctrl Pts',(1.22216901905492,7.34562534894807,49.3674203502868));
#242644=CARTESIAN_POINT('Ctrl Pts',(-2.44728222896209,7.04987926420199,
49.5263747161115));
#242645=CARTESIAN_POINT('Ctrl Pts',(-5.50556853875714,5.01404742604368,
49.6853290819364));
#242646=CARTESIAN_POINT('Ctrl Pts',(-7.86055750992125,0.670940859405257,
49.8972682363692));
#242647=CARTESIAN_POINT('Ctrl Pts',(-6.47664796657427,-4.50805308939218,
50.1092073908024));
#242648=CARTESIAN_POINT('Ctrl Pts',(-2.27095236266987,-7.08399189981036,
50.3211465452353));
#242649=CARTESIAN_POINT('Ctrl Pts',(2.62415162413245,-7.43516921507365,
50.5330856996684));
#242650=CARTESIAN_POINT('Ctrl Pts',(7.84810112327243,-3.17902218718639,
50.7980096427096));
#242651=CARTESIAN_POINT('Ctrl Pts',(6.90091107759898,4.89585482479138,51.1159183743592));
#242652=CARTESIAN_POINT('Ctrl Pts',(0.856337932839807,7.83816754074625,
51.3808423174003));
#242653=CARTESIAN_POINT('Ctrl Pts',(-3.84849236051841,6.3750306218306,51.5927814718335));
#242654=CARTESIAN_POINT('Ctrl Pts',(-6.44373281766883,3.76407961160719,
51.7517358376581));
#242655=CARTESIAN_POINT('Ctrl Pts',(-7.44309471031215,0.228686813986007,
51.910690203483));
#242656=CARTESIAN_POINT('Ctrl Pts',(-6.40773910221589,-4.60210882113104,
52.122629357916));
#242657=CARTESIAN_POINT('Ctrl Pts',(-1.98847321494345,-7.63645767441696,
52.334568512349));
#242658=CARTESIAN_POINT('Ctrl Pts',(2.88162157363182,-6.85831050452472,
52.546507666782));
#242659=CARTESIAN_POINT('Ctrl Pts',(6.82865298432106,-3.94175232896983,
52.7584468212151));
#242660=CARTESIAN_POINT('Ctrl Pts',(8.02930751700683,2.68869747369813,53.0233707642562));
#242661=CARTESIAN_POINT('Ctrl Pts',(2.05858114621105,8.20696118126715,53.3412794959059));
#242662=CARTESIAN_POINT('Ctrl Pts',(-4.44670804338187,6.51129577188378,
53.606203438947));
#242663=CARTESIAN_POINT('Ctrl Pts',(-7.06932723955645,2.34019684178733,
53.8181425933801));
#242664=CARTESIAN_POINT('Ctrl Pts',(-7.34292177457965,-1.33097248672672,
53.9770969592048));
#242665=CARTESIAN_POINT('Ctrl Pts',(-5.80300332378635,-4.66659500596445,
54.1360513250296));
#242666=CARTESIAN_POINT('Ctrl Pts',(-1.87495989703104,-7.66309672313511,
54.3479904794625));
#242667=CARTESIAN_POINT('Ctrl Pts',(3.45548632304764,-7.09430234843002,
54.5599296338957));
#242668=CARTESIAN_POINT('Ctrl Pts',(6.64910767499218,-3.33609547172361,
54.7718687883286));
#242669=CARTESIAN_POINT('Ctrl Pts',(7.75087596897043,1.44631764037241,54.9838079427617));
#242670=CARTESIAN_POINT('Ctrl Pts',(4.35112575701066,7.26406070696073,55.2487318858029));
#242671=CARTESIAN_POINT('Ctrl Pts',(-3.77323183491082,7.57328790462749,
55.5666406174525));
#242672=CARTESIAN_POINT('Ctrl Pts',(-7.61238758926359,2.05468738324218,
55.8315645604936));
#242673=CARTESIAN_POINT('Ctrl Pts',(-6.89220061999691,-2.81948213187466,
56.0435037149268));
#242674=CARTESIAN_POINT('Ctrl Pts',(-4.71264256122068,-5.78627583495556,
56.2024580807514));
#242675=CARTESIAN_POINT('Ctrl Pts',(-1.37362503593767,-7.31881894749509,
56.3614124465763));
#242676=CARTESIAN_POINT('Ctrl Pts',(3.55904248337716,-7.04072031862616,
56.5733516010092));
#242677=CARTESIAN_POINT('Ctrl Pts',(7.23852268026616,-3.14218092206377,
56.7852907554423));
#242678=CARTESIAN_POINT('Ctrl Pts',(7.220616123312,1.78965601998303,56.9972299098752));
#242679=CARTESIAN_POINT('Ctrl Pts',(4.9475424430092,6.13919675347174,57.2091690643084));
#242680=CARTESIAN_POINT('Ctrl Pts',(-1.41847959915863,8.34786133896,57.4740930073495));
#242681=CARTESIAN_POINT('Ctrl Pts',(-7.79139323847274,3.29941806533262,
57.7920017389992));
#242682=CARTESIAN_POINT('Ctrl Pts',(-7.1190768148242,-3.38953246874281,
58.0569256820402));
#242683=CARTESIAN_POINT('Ctrl Pts',(-3.40225065052701,-6.62394137875892,
58.2688648364734));
#242684=CARTESIAN_POINT('Ctrl Pts',(0.182827870063121,-7.4603325608144,
58.4278192022981));
#242685=CARTESIAN_POINT('Ctrl Pts',(3.71600348895036,-6.45316004726959,
58.5867735681229));
#242686=CARTESIAN_POINT('Ctrl Pts',(7.28234610553302,-3.0341326936749,58.7987127225559));
#242687=CARTESIAN_POINT('Ctrl Pts',(7.54227161156929,2.32026948370767,59.0106518769889));
#242688=CARTESIAN_POINT('Ctrl Pts',(4.32144415866702,6.05518672326604,59.2225910314219));
#242689=CARTESIAN_POINT('Ctrl Pts',(-0.233889898346162,7.88119334356588,
59.434530185855));
#242690=CARTESIAN_POINT('Ctrl Pts',(-6.50627480548557,5.41915689597893,
59.6994541288961));
#242691=CARTESIAN_POINT('Ctrl Pts',(-8.06452299367309,-2.56035877385966,
60.0173628605457));
#242692=CARTESIAN_POINT('Ctrl Pts',(-3.20389177956769,-7.20453069372653,
60.282286803587));
#242693=CARTESIAN_POINT('Ctrl Pts',(1.72303410078483,-7.24451947100556,
60.49422595802));
#242694=CARTESIAN_POINT('Ctrl Pts',(4.99041977453763,-5.54848613785086,
60.6531803238448));
#242695=CARTESIAN_POINT('Ctrl Pts',(7.01948796416786,-2.48570819817419,
60.8121346896695));
#242696=CARTESIAN_POINT('Ctrl Pts',(7.50529801846231,2.43084916390639,61.0240738441026));
#242697=CARTESIAN_POINT('Ctrl Pts',(4.22073235354174,6.66745303241609,61.2360129985355));
#242698=CARTESIAN_POINT('Ctrl Pts',(-0.654884566712431,7.41021538650372,
61.4479521529686));
#242699=CARTESIAN_POINT('Ctrl Pts',(-5.30290010354056,5.8349947296536,61.6598913074015));
#242700=CARTESIAN_POINT('Ctrl Pts',(-8.46674678300096,-0.114333810730216,
61.9248152504429));
#242701=CARTESIAN_POINT('Ctrl Pts',(-4.46133783113658,-7.18946680379233,
62.2427239820923));
#242702=CARTESIAN_POINT('Ctrl Pts',(2.25128433881871,-7.556580170806,62.5076479251336));
#242703=CARTESIAN_POINT('Ctrl Pts',(6.02012073128016,-4.38292770406461,
62.7195870795667));
#242704=CARTESIAN_POINT('Ctrl Pts',(7.39930333222143,-0.969689716247477,
62.8785414453915));
#242705=CARTESIAN_POINT('Ctrl Pts',(6.94896681850422,2.67653071734569,63.0374958112161));
#242706=CARTESIAN_POINT('Ctrl Pts',(4.1207335669581,6.72741264333794,63.2494349656491));
#242707=CARTESIAN_POINT('Ctrl Pts',(-1.12955526302388,7.80984100014096,
63.4613741200822));
#242708=CARTESIAN_POINT('Ctrl Pts',(-5.31643474693376,5.20343035426541,
63.6733132745152));
#242709=CARTESIAN_POINT('Ctrl Pts',(-7.82300434185401,0.984132140796148,
63.8852524289482));
#242710=CARTESIAN_POINT('Ctrl Pts',(-6.35756989406835,-5.59286852605801,
64.1501763719894));
#242711=CARTESIAN_POINT('Ctrl Pts',(1.28624575415458,-8.36286673493512,
64.468085103639));
#242712=CARTESIAN_POINT('Ctrl Pts',(6.62435218204968,-4.27646386868794,
64.7330090466803));
#242713=CARTESIAN_POINT('Ctrl Pts',(7.42356023403596,0.585373666898152,
64.9449482011133));
#242714=CARTESIAN_POINT('Ctrl Pts',(6.25161821125358,4.07520032498098,65.1039025669381));
#242715=CARTESIAN_POINT('Ctrl Pts',(3.53833693205918,6.55226131047918,65.2628569327628));
#242716=CARTESIAN_POINT('Ctrl Pts',(-1.24451356227045,7.79036019687026,
65.4747960871958));
#242717=CARTESIAN_POINT('Ctrl Pts',(-5.93690786408821,5.19833016966197,
65.6867352416289));
#242718=CARTESIAN_POINT('Ctrl Pts',(-7.42257336285703,0.495550747503218,
65.8986743960618));
#242719=CARTESIAN_POINT('Ctrl Pts',(-6.58288265534216,-4.33976600161993,
66.110613550495));
#242720=CARTESIAN_POINT('Ctrl Pts',(-1.19254667180593,-8.38312028680404,
66.375537493536));
#242721=CARTESIAN_POINT('Ctrl Pts',(6.4155790588712,-5.51654905789318,66.6934462251858));
#242722=CARTESIAN_POINT('Ctrl Pts',(7.81334141260345,1.05918884928924,66.9583701682268));
#242723=CARTESIAN_POINT('Ctrl Pts',(5.25877167200093,5.27230778524644,67.17030932266));
#242724=CARTESIAN_POINT('Ctrl Pts',(2.09901377177692,7.16129381706967,67.3292636884847));
#242725=CARTESIAN_POINT('Ctrl Pts',(-1.57303932628563,7.27856467940848,
67.4882180543094));
#242726=CARTESIAN_POINT('Ctrl Pts',(-6.01156951947919,5.10877264761354,
67.7001572087426));
#242727=CARTESIAN_POINT('Ctrl Pts',(-7.89061064785605,0.0881762308052003,
67.9120963631754));
#242728=CARTESIAN_POINT('Ctrl Pts',(-5.96095827281491,-4.45052158773688,
68.1240355176085));
#242729=CARTESIAN_POINT('Ctrl Pts',(-2.17861519210624,-7.57770076348474,
68.3359746720415));
#242730=CARTESIAN_POINT('Ctrl Pts',(4.54568914768806,-7.14391930167323,
68.6008986150827));
#242731=CARTESIAN_POINT('Ctrl Pts',(8.46118325379544,-0.0186323644137214,
68.9188073467324));
#242732=CARTESIAN_POINT('Ctrl Pts',(5.2467492225371,5.88572909360765,69.1837312897735));
#242733=CARTESIAN_POINT('Ctrl Pts',(0.566288176802008,7.42504047192828,
69.3956704442066));
#242734=CARTESIAN_POINT('Ctrl Pts',(-3.06250848692811,6.80522102006031,
69.5546248100314));
#242735=CARTESIAN_POINT('Ctrl Pts',(-5.92831375746228,4.50633372899844,
69.7135791758561));
#242736=CARTESIAN_POINT('Ctrl Pts',(-7.88908994489078,-0.0284105957327118,
69.9255183302893));
#242737=CARTESIAN_POINT('Ctrl Pts',(-6.05158909666752,-5.06436160468178,
70.137457484722));
#242738=CARTESIAN_POINT('Ctrl Pts',(-1.63413626028271,-7.25739343937373,
70.3493966391552));
#242739=CARTESIAN_POINT('Ctrl Pts',(3.2728382690313,-7.17332026330462,70.5613357935883));
#242740=CARTESIAN_POINT('Ctrl Pts',(8.09896697347761,-2.47089809738648,
70.8262597366294));
#242741=CARTESIAN_POINT('Ctrl Pts',(6.43983928834939,5.48823121320375,71.1441684682791));
#242742=CARTESIAN_POINT('Ctrl Pts',(0.158195774879766,7.88323448684002,
71.4090924113202));
#242743=CARTESIAN_POINT('Ctrl Pts',(-4.39832668689196,6.00881249973269,
71.6210315657532));
#242744=CARTESIAN_POINT('Ctrl Pts',(-6.75213301471285,3.17817874136241,
71.779985931578));
#242745=CARTESIAN_POINT('Ctrl Pts',(-7.43381632393515,-0.43200928049931,
71.9389402974028));
#242746=CARTESIAN_POINT('Ctrl Pts',(-5.97519664327555,-5.15174218629462,
72.1508794518358));
#242747=CARTESIAN_POINT('Ctrl Pts',(-1.30268824194961,-7.78302532067559,
72.3628186062687));
#242748=CARTESIAN_POINT('Ctrl Pts',(3.47686054563489,-6.57546876338237,
72.5747577607018));
#242749=CARTESIAN_POINT('Ctrl Pts',(7.15418212494621,-3.32201596284964,
72.7866969151348));
#242750=CARTESIAN_POINT('Ctrl Pts',(7.75298169246792,3.39194015110797,73.051620858176));
#242751=CARTESIAN_POINT('Ctrl Pts',(1.33416029501156,8.35347911467427,73.3695295898257));
#242752=CARTESIAN_POINT('Ctrl Pts',(-6.29541838040319,5.6453087392055,73.6874383214751));
#242753=CARTESIAN_POINT('Ctrl Pts',(-8.1578247845443,-2.23879346110978,
74.0053470531247));
#242754=CARTESIAN_POINT('Ctrl Pts',(-2.53203993743254,-8.06787314603517,
74.3232557847741));
#242755=CARTESIAN_POINT('Ctrl Pts',(5.41111795255811,-6.50233800379432,
74.6411645164237));
#242756=CARTESIAN_POINT('Ctrl Pts',(8.39828963266304,1.04053561128162,74.9590732480732));
#242757=CARTESIAN_POINT('Ctrl Pts',(4.4563813353463,6.50836210795808,75.2239971911145));
#242758=CARTESIAN_POINT('Ctrl Pts',(-0.366475770832498,7.42906752031522,
75.4359363455475));
#242759=CARTESIAN_POINT('Ctrl Pts',(-5.09287915284989,6.02785714267165,
75.6478754999804));
#242760=CARTESIAN_POINT('Ctrl Pts',(-7.76778677712684,1.38018515603965,
75.8598146544136));
#242761=CARTESIAN_POINT('Ctrl Pts',(-6.6130024664685,-3.42293083992707,
76.0717538088464));
#242762=CARTESIAN_POINT('Ctrl Pts',(-4.18406943566272,-6.17945655523008,
76.2307081746713));
#242763=CARTESIAN_POINT('Ctrl Pts',(-0.715149063313115,-7.41212972895188,
76.3896625404961));
#242764=CARTESIAN_POINT('Ctrl Pts',(4.15985583163179,-6.69820956209441,
76.601601694929));
#242765=CARTESIAN_POINT('Ctrl Pts',(8.33909590344503,-1.43237265489772,
76.8665256379704));
#242766=CARTESIAN_POINT('Ctrl Pts',(5.70325544624252,6.25871238834748,77.1844343696198));
#242767=CARTESIAN_POINT('Ctrl Pts',(-0.847078634713838,7.8390338512972,
77.4493583126611));
#242768=CARTESIAN_POINT('Ctrl Pts',(-5.10960119783234,5.40667517520201,
77.6612974670941));
#242769=CARTESIAN_POINT('Ctrl Pts',(-7.78887677874035,1.26605196713225,
77.8732366215271));
#242770=CARTESIAN_POINT('Ctrl Pts',(-6.79849382308411,-4.00237792543563,
78.0851757759601));
#242771=CARTESIAN_POINT('Ctrl Pts',(-2.79772326318019,-6.90106457198351,
78.2971149303932));
#242772=CARTESIAN_POINT('Ctrl Pts',(0.840057590336768,-7.4151395542697,
78.4560692962179));
#242773=CARTESIAN_POINT('Ctrl Pts',(4.27690811805749,-6.09589741208402,
78.6150236620428));
#242774=CARTESIAN_POINT('Ctrl Pts',(7.51602684544494,-2.38317536620462,
78.8269628164757));
#242775=CARTESIAN_POINT('Ctrl Pts',(7.2664367172965,4.33484332506232,79.0918867595171));
#242776=CARTESIAN_POINT('Ctrl Pts',(0.262479329093425,8.463449498758,79.4097954911665));
#242777=CARTESIAN_POINT('Ctrl Pts',(-5.74130361826883,5.40419705220362,
79.6747194342077));
#242778=CARTESIAN_POINT('Ctrl Pts',(-7.39762060038627,0.784458657860876,
79.8866585886409));
#242779=CARTESIAN_POINT('Ctrl Pts',(-6.74029237988116,-4.10340956735422,
80.0985977430736));
#242780=CARTESIAN_POINT('Ctrl Pts',(-2.56181520562744,-7.46161034259711,
80.3105368975069));
#242781=CARTESIAN_POINT('Ctrl Pts',(2.36249069307547,-7.06191151456218,
80.5224760519397));
#242782=CARTESIAN_POINT('Ctrl Pts',(5.46030712988442,-5.08675082895186,
80.6814304177646));
#242783=CARTESIAN_POINT('Ctrl Pts',(7.21325806895984,-1.84954505519482,
80.8403847835894));
#242784=CARTESIAN_POINT('Ctrl Pts',(7.25949369712115,3.07732616240482,81.0523239380222));
#242785=CARTESIAN_POINT('Ctrl Pts',(2.70109108776638,8.01848334190188,81.3172478810638));
#242786=CARTESIAN_POINT('Ctrl Pts',(-5.30447112776438,6.60011055681453,
81.635156612713));
#242787=CARTESIAN_POINT('Ctrl Pts',(-7.87589359057637,0.371770295664173,
81.9000805557545));
#242788=CARTESIAN_POINT('Ctrl Pts',(-6.12988222590252,-4.21482025321488,
82.1120197101873));
#242789=CARTESIAN_POINT('Ctrl Pts',(-2.45189947187555,-7.50051335038523,
82.3239588646206));
#242790=CARTESIAN_POINT('Ctrl Pts',(2.90623134771161,-7.33432651013266,
82.5358980190533));
#242791=CARTESIAN_POINT('Ctrl Pts',(6.38714403999805,-3.82836094665771,
82.7478371734866));
#242792=CARTESIAN_POINT('Ctrl Pts',(7.45599080795447,-0.313351272057573,
82.906791539311));
#242793=CARTESIAN_POINT('Ctrl Pts',(6.6824644485123,3.28581462846386,83.0657459051361));
#242794=CARTESIAN_POINT('Ctrl Pts',(3.51359306648352,7.05867188748558,83.2776850595689));
#242795=CARTESIAN_POINT('Ctrl Pts',(-3.16256807410052,7.84793803129486,
83.5426090026103));
#242796=CARTESIAN_POINT('Ctrl Pts',(-8.32176050922241,1.5643450178527,83.8605177342598));
#242797=CARTESIAN_POINT('Ctrl Pts',(-6.22483574080837,-4.83935253966577,
84.1254416773011));
#242798=CARTESIAN_POINT('Ctrl Pts',(-1.91573847867857,-7.18819253716854,
84.337380831734));
#242799=CARTESIAN_POINT('Ctrl Pts',(3.01502991504078,-7.29240057533304,
84.5493199861671));
#242800=CARTESIAN_POINT('Ctrl Pts',(6.97736106495208,-3.68170593242992,
84.7612591406));
#242801=CARTESIAN_POINT('Ctrl Pts',(7.34173586737877,1.2453397043426,84.9731982950332));
#242802=CARTESIAN_POINT('Ctrl Pts',(5.86785825508849,4.61066453412179,85.1321526608577));
#242803=CARTESIAN_POINT('Ctrl Pts',(2.93965982041344,6.84180597638467,85.2911070266827));
#242804=CARTESIAN_POINT('Ctrl Pts',(-1.92116048583458,7.64717774343563,
85.5030461811155));
#242805=CARTESIAN_POINT('Ctrl Pts',(-7.50609891412956,3.90518210300933,
85.7679701241569));
#242806=CARTESIAN_POINT('Ctrl Pts',(-7.33909050950137,-4.22334272834674,
86.0858788558065));
#242807=CARTESIAN_POINT('Ctrl Pts',(-1.58173190621261,-7.72437940420364,
86.3508027988476));
#242808=CARTESIAN_POINT('Ctrl Pts',(3.21922918449413,-6.70646921470574,
86.5627419532807));
#242809=CARTESIAN_POINT('Ctrl Pts',(7.03274706135878,-3.57910328303859,
86.7746811077136));
#242810=CARTESIAN_POINT('Ctrl Pts',(7.69473398792592,1.74057314085235,86.9866202621468));
#242811=CARTESIAN_POINT('Ctrl Pts',(4.76742954577874,5.72045208454751,87.1985594165797));
#242812=CARTESIAN_POINT('Ctrl Pts',(1.45926545835945,7.31850615016874,87.3575137824045));
#242813=CARTESIAN_POINT('Ctrl Pts',(-2.21612945958299,7.10919679686913,
87.5164681482293));
#242814=CARTESIAN_POINT('Ctrl Pts',(-6.43248396591558,4.5599709516912,87.7284073026623));
#242815=CARTESIAN_POINT('Ctrl Pts',(-8.24172842909861,-1.91464896713466,
87.9933312457035));
#242816=CARTESIAN_POINT('Ctrl Pts',(-2.82879388550048,-7.98102740636118,
88.3112399773531));
#242817=CARTESIAN_POINT('Ctrl Pts',(3.82165136322666,-6.89658566691984,
88.5761639203943));
#242818=CARTESIAN_POINT('Ctrl Pts',(6.80683364698421,-3.00119669005193,
88.7881030748274));
#242819=CARTESIAN_POINT('Ctrl Pts',(7.67008543412729,1.85453524444709,89.0000422292602));
#242820=CARTESIAN_POINT('Ctrl Pts',(4.71353575314952,6.3262237320047,89.2119813836935));
#242821=CARTESIAN_POINT('Ctrl Pts',(-0.098402050417027,7.44595686007123,
89.4239205381264));
#242822=CARTESIAN_POINT('Ctrl Pts',(-3.65074172699665,6.50861527444854,
89.582874903951));
#242823=CARTESIAN_POINT('Ctrl Pts',(-6.30670810150985,3.95946231205651,
89.7418292697761));
#242824=CARTESIAN_POINT('Ctrl Pts',(-7.85195271698889,-0.719043518989206,
89.9537684242088));
#242825=CARTESIAN_POINT('Ctrl Pts',(-5.01586699380124,-6.81417980881466,
90.2186923672503));
#242826=CARTESIAN_POINT('Ctrl Pts',(3.04119827736541,-7.90253037611894,
90.5366010988996));
#242827=CARTESIAN_POINT('Ctrl Pts',(7.38810959676663,-2.75386085149218,
90.8015250419411));
#242828=CARTESIAN_POINT('Ctrl Pts',(7.12264747423663,2.14663896075815,91.0134641963739));
#242829=CARTESIAN_POINT('Ctrl Pts',(4.62070028810255,6.3967679641548,91.2254033508071));
#242830=CARTESIAN_POINT('Ctrl Pts',(-0.533283023543019,7.87109491877717,
91.43734250524));
#242831=CARTESIAN_POINT('Ctrl Pts',(-4.91693545721402,5.59246834905301,
91.649281659673));
#242832=CARTESIAN_POINT('Ctrl Pts',(-7.00597375351663,2.57027619392447,
91.8082360254978));
#242833=CARTESIAN_POINT('Ctrl Pts',(-7.36588777354428,-1.09343778323085,
91.9671903913226));
#242834=CARTESIAN_POINT('Ctrl Pts',(-5.49728114084035,-5.65244063308855,
92.1791295457554));
#242835=CARTESIAN_POINT('Ctrl Pts',(0.620934315895268,-8.43838898971278,
92.4440534887969));
#242836=CARTESIAN_POINT('Ctrl Pts',(7.44940004548645,-4.02558222745956,
92.7619622204463));
#242837=CARTESIAN_POINT('Ctrl Pts',(7.40337956209903,2.71254199280134,93.0268861634876));
#242838=CARTESIAN_POINT('Ctrl Pts',(4.01487075809005,6.26266546016378,93.2388253179207));
#242839=CARTESIAN_POINT('Ctrl Pts',(-0.649682860062558,7.86431330257443,
93.4507644723536));
#242840=CARTESIAN_POINT('Ctrl Pts',(-5.52377257392429,5.63262483706841,
93.6627036267866));
#242841=CARTESIAN_POINT('Ctrl Pts',(-7.3720816832314,1.05088923361697,93.8746427812198));
#242842=CARTESIAN_POINT('Ctrl Pts',(-6.9936959353334,-2.60349862917581,
94.0335971470443));
#242843=CARTESIAN_POINT('Ctrl Pts',(-4.8845603776014,-5.62076318624192,
94.1925515128693));
#242844=CARTESIAN_POINT('Ctrl Pts',(-0.500271895129622,-7.86892070635947,
94.4044906673021));
#242845=CARTESIAN_POINT('Ctrl Pts',(5.95927569764219,-6.00657983596767,
94.6694146103437));
#242846=CARTESIAN_POINT('Ctrl Pts',(8.27695351647176,1.78631290481188,94.9873233419929));
#242847=CARTESIAN_POINT('Ctrl Pts',(3.86012155736479,6.87512723995585,95.2522472850343));
#242848=CARTESIAN_POINT('Ctrl Pts',(-1.02270433851611,7.36846264196782,
95.4641864394672));
#242849=CARTESIAN_POINT('Ctrl Pts',(-5.60778772912366,5.55177704206492,
95.6761255939003));
#242850=CARTESIAN_POINT('Ctrl Pts',(-7.85919101256279,0.686762427372801,
95.8880647483333));
#242851=CARTESIAN_POINT('Ctrl Pts',(-6.28374366028536,-3.99581307588229,
96.1000039027662));
#242852=CARTESIAN_POINT('Ctrl Pts',(-3.61980976095626,-6.52586892624304,
96.2589582685911));
#242853=CARTESIAN_POINT('Ctrl Pts',(-0.0554072921370151,-7.44639771367499,
96.4179126344158));
#242854=CARTESIAN_POINT('Ctrl Pts',(4.73719936073806,-6.30310457383125,
96.6298517888488));
#242855=CARTESIAN_POINT('Ctrl Pts',(8.43321588618773,-0.687632156979905,
96.8947757318901));
#242856=CARTESIAN_POINT('Ctrl Pts',(5.12608465367676,6.73959415922588,97.2126844635397));
#242857=CARTESIAN_POINT('Ctrl Pts',(-1.53855266836986,7.73309567313556,
97.4776084065809));
#242858=CARTESIAN_POINT('Ctrl Pts',(-5.5687036671652,4.93251511273872,97.689547561014));
#242859=CARTESIAN_POINT('Ctrl Pts',(-7.87043854008896,0.570708968205702,
97.9014867154469));
#242860=CARTESIAN_POINT('Ctrl Pts',(-6.41698994571513,-4.58920102416412,
98.11342586988));
#242861=CARTESIAN_POINT('Ctrl Pts',(-2.17504481640704,-7.12187732077639,
98.325365024313));
#242862=CARTESIAN_POINT('Ctrl Pts',(1.49398373177941,-7.31149783267407,
98.4843193901377));
#242863=CARTESIAN_POINT('Ctrl Pts',(4.80037800867734,-5.69282705270879,
98.6432737559625));
#242864=CARTESIAN_POINT('Ctrl Pts',(7.69767586257887,-1.70762155254026,
98.8552129103956));
#242865=CARTESIAN_POINT('Ctrl Pts',(6.85362425769077,4.96183461037897,99.1201368534366));
#242866=CARTESIAN_POINT('Ctrl Pts',(-0.48870159495969,8.45340428814426,
99.4380455850865));
#242867=CARTESIAN_POINT('Ctrl Pts',(-6.1977021057436,4.87405391965216,99.7029695281274));
#242868=CARTESIAN_POINT('Ctrl Pts',(-7.43803518614661,0.125691844365409,
99.9149086825606));
#242869=CARTESIAN_POINT('Ctrl Pts',(-6.35006357928672,-4.68467758535475,
100.126847836994));
#242870=CARTESIAN_POINT('Ctrl Pts',(-1.89038154652329,-7.65930699294415,
100.338786991427));
#242871=CARTESIAN_POINT('Ctrl Pts',(2.97911681246191,-6.82472120626732,
100.55072614586));
#242872=CARTESIAN_POINT('Ctrl Pts',(5.88967505890723,-4.58276288373128,
100.709680511685));
#242873=CARTESIAN_POINT('Ctrl Pts',(7.34880093971353,-1.20292710781303,
100.868634877509));
#242874=CARTESIAN_POINT('Ctrl Pts',(6.9581671574302,3.70865135342868,101.080574031942));
#242875=CARTESIAN_POINT('Ctrl Pts',(1.97975149545645,8.22633285143508,101.345497974984));
#242876=CARTESIAN_POINT('Ctrl Pts',(-5.86858724447197,6.10397878942532,
101.663406706633));
#242877=CARTESIAN_POINT('Ctrl Pts',(-7.87784768299701,-0.327763461531114,
101.928330649674));
#242878=CARTESIAN_POINT('Ctrl Pts',(-5.73218107129307,-4.7415467978292,
102.140269804107));
#242879=CARTESIAN_POINT('Ctrl Pts',(-1.7774502901569,-7.68831464013599,
102.35220895854));
#242880=CARTESIAN_POINT('Ctrl Pts',(3.54486263865986,-7.04787023693198,
102.564148112973));
#242881=CARTESIAN_POINT('Ctrl Pts',(6.70132828744226,-3.2471765750409,102.776087267406));
#242882=CARTESIAN_POINT('Ctrl Pts',(7.45441961963896,0.348734974387096,
102.935041633231));
#242883=CARTESIAN_POINT('Ctrl Pts',(6.36492980544189,3.86517495723589,103.093995999056));
#242884=CARTESIAN_POINT('Ctrl Pts',(2.87412745229389,7.34231410660148,103.305935153489));
#242885=CARTESIAN_POINT('Ctrl Pts',(-3.84571384841862,7.5367402212391,103.57085909653));
#242886=CARTESIAN_POINT('Ctrl Pts',(-8.42766225216046,0.820598727297953,
103.88876782818));
#242887=CARTESIAN_POINT('Ctrl Pts',(-5.77140619028756,-5.37203719178541,
104.153691771221));
#242888=CARTESIAN_POINT('Ctrl Pts',(-1.27108166601713,-7.32970103540452,
104.365630925654));
#242889=CARTESIAN_POINT('Ctrl Pts',(3.64951694906699,-6.99646607782685,
104.577570080087));
#242890=CARTESIAN_POINT('Ctrl Pts',(7.27622378719676,-3.04878556186414,
104.78950923452));
#242891=CARTESIAN_POINT('Ctrl Pts',(7.20246161190543,1.89116452340786,105.001448388953));
#242892=CARTESIAN_POINT('Ctrl Pts',(5.4361031614677,5.11260895882911,105.160402754778));
#242893=CARTESIAN_POINT('Ctrl Pts',(2.32167470332257,7.07543182075821,105.319357120603));
#242894=CARTESIAN_POINT('Ctrl Pts',(-2.59139794363207,7.44680077279955,
105.531296275036));
#242895=CARTESIAN_POINT('Ctrl Pts',(-7.82268821872125,3.22451813439498,
105.796220218077));
#242896=CARTESIAN_POINT('Ctrl Pts',(-6.93587486720317,-4.85721248600803,
106.114128949726));
#242897=CARTESIAN_POINT('Ctrl Pts',(-0.890865357879725,-7.83417333975615,
106.379052892768));
#242898=CARTESIAN_POINT('Ctrl Pts',(3.80097920933104,-6.39474181811339,
106.590992047201));
#242899=CARTESIAN_POINT('Ctrl Pts',(7.32229773444863,-2.94167765531786,
106.802931201634));
#242900=CARTESIAN_POINT('Ctrl Pts',(7.51017599620535,2.41573643215052,107.014870356067));
#242901=CARTESIAN_POINT('Ctrl Pts',(4.2416407187964,6.12049348812788,107.2268095105));
#242902=CARTESIAN_POINT('Ctrl Pts',(0.804855002849698,7.41904282049959,
107.385763876324));
#242903=CARTESIAN_POINT('Ctrl Pts',(-2.83752269243022,6.88479294156259,
107.544718242149));
#242904=CARTESIAN_POINT('Ctrl Pts',(-6.81133516099195,3.97188851513535,
107.756657396582));
#242905=CARTESIAN_POINT('Ctrl Pts',(-8.03958861281681,-2.63760935375736,
108.021581339624));
#242906=CARTESIAN_POINT('Ctrl Pts',(-2.11027155334492,-8.20034311958203,
108.339490071273));
#242907=CARTESIAN_POINT('Ctrl Pts',(4.41788116991169,-6.5307150429149,108.604414014314));
#242908=CARTESIAN_POINT('Ctrl Pts',(7.04605138085898,-2.3860691122409,108.816353168747));
#242909=CARTESIAN_POINT('Ctrl Pts',(7.47552355515081,2.52706531694266,109.02829232318));
#242910=CARTESIAN_POINT('Ctrl Pts',(4.13426717911749,6.71910417356882,109.240231477613));
#242911=CARTESIAN_POINT('Ctrl Pts',(-0.757978402905966,7.40792989075192,
109.452170632047));
#242912=CARTESIAN_POINT('Ctrl Pts',(-4.21325688678036,6.15941996895951,
109.611124997871));
#242913=CARTESIAN_POINT('Ctrl Pts',(-6.63282893793018,3.38489130673388,
109.770079363696));
#242914=CARTESIAN_POINT('Ctrl Pts',(-7.75731803350436,-1.41216216458898,
109.982018518129));
#242915=CARTESIAN_POINT('Ctrl Pts',(-4.39215911452095,-7.23193656492455,
110.24694246117));
#242916=CARTESIAN_POINT('Ctrl Pts',(3.72966045783671,-7.60187517504613,
110.56485119282));
#242917=CARTESIAN_POINT('Ctrl Pts',(7.60311726848728,-2.08818600820106,
110.829775135861));
#242918=CARTESIAN_POINT('Ctrl Pts',(6.9043498894944,2.76949787389946,111.041714290294));
#242919=CARTESIAN_POINT('Ctrl Pts',(4.03554448357857,6.78114240086186,111.253653444727));
#242920=CARTESIAN_POINT('Ctrl Pts',(-1.22882941744544,7.79284956010438,
111.46559259916));
#242921=CARTESIAN_POINT('Ctrl Pts',(-5.39326562391045,5.134651150323,111.677531753593));
#242922=CARTESIAN_POINT('Ctrl Pts',(-7.20621359546558,1.93919405025541,
111.836486119418));
#242923=CARTESIAN_POINT('Ctrl Pts',(-7.2399821111322,-1.742001121909,111.995440485243));
#242924=CARTESIAN_POINT('Ctrl Pts',(-4.97464793565611,-6.11743924925306,
112.207379639676));
#242925=CARTESIAN_POINT('Ctrl Pts',(1.36641718192386,-8.3501420497681,112.472303582717));
#242926=CARTESIAN_POINT('Ctrl Pts',(7.77688402461956,-3.34946983496645,
112.790212314366));
#242927=CARTESIAN_POINT('Ctrl Pts',(7.13381894360561,3.35805602738686,113.055136257408));
#242928=CARTESIAN_POINT('Ctrl Pts',(3.44398534826098,6.59387069869117,113.26707541184));
#242929=CARTESIAN_POINT('Ctrl Pts',(-1.34417005593833,7.77577767174627,
113.479014566274));
#242930=CARTESIAN_POINT('Ctrl Pts',(-6.00127362130826,5.12086329887732,
113.690953720707));
#242931=CARTESIAN_POINT('Ctrl Pts',(-7.43621154838904,0.393337429153544,
113.90289287514));
#242932=CARTESIAN_POINT('Ctrl Pts',(-6.73541264825281,-3.21313000138109,
114.061847240965));
#242933=CARTESIAN_POINT('Ctrl Pts',(-4.36714636452488,-6.03157869127675,
114.220801606789));
#242934=CARTESIAN_POINT('Ctrl Pts',(0.199149575258351,-7.88229183034368,
114.432740761222));
#242935=CARTESIAN_POINT('Ctrl Pts',(6.46820778747301,-5.45474620715169,
114.697664704263));
#242936=CARTESIAN_POINT('Ctrl Pts',(8.08604998008524,2.5129005207721,115.015573435913));
#242937=CARTESIAN_POINT('Ctrl Pts',(3.23556036735803,7.1902059853941,115.280497378954));
#242938=CARTESIAN_POINT('Ctrl Pts',(-1.67177428483406,7.24881622133312,
115.492436533387));
#242939=CARTESIAN_POINT('Ctrl Pts',(-6.07779226688301,5.03288711380715,
115.70437568782));
#242940=CARTESIAN_POINT('Ctrl Pts',(-7.88912979907862,-0.012530638005558,
115.916314842253));
#242941=CARTESIAN_POINT('Ctrl Pts',(-5.90484839357282,-4.5370388993801,
116.128253996686));
#242942=CARTESIAN_POINT('Ctrl Pts',(-3.02715047165072,-6.82102250179571,
116.287208362511));
#242943=CARTESIAN_POINT('Ctrl Pts',(0.604813485768121,-7.42200171959558,
116.446162728336));
#242944=CARTESIAN_POINT('Ctrl Pts',(5.2772233254442,-5.85842120587252,116.658101882769));
#242945=CARTESIAN_POINT('Ctrl Pts',(8.46097255761023,0.0625423514801803,
116.92302582581));
#242946=CARTESIAN_POINT('Ctrl Pts',(4.50855379967994,7.16741347650078,117.24093455746));
#242947=CARTESIAN_POINT('Ctrl Pts',(-2.21791119905249,7.56629254763077,
117.505858500501));
#242948=CARTESIAN_POINT('Ctrl Pts',(-5.98397447560684,4.41952659742876,
117.717797654934));
#242949=CARTESIAN_POINT('Ctrl Pts',(-7.89004679749403,-0.1291242543574,
117.929736809367));
#242950=CARTESIAN_POINT('Ctrl Pts',(-5.98497601517829,-5.13990156533564,
118.1416759638));
#242951=CARTESIAN_POINT('Ctrl Pts',(-1.53524521725277,-7.28663012979732,
118.353615118233));
#242952=CARTESIAN_POINT('Ctrl Pts',(2.13614984430581,-7.15030431455134,
118.512569484058));
#242953=CARTESIAN_POINT('Ctrl Pts',(5.28606208889017,-5.24494580245065,
118.671523849883));
#242954=CARTESIAN_POINT('Ctrl Pts',(7.81873297671236,-1.01862637453541,
118.883463004315));
#242955=CARTESIAN_POINT('Ctrl Pts',(6.38686391572332,5.54976913829684,119.148386947357));
#242956=CARTESIAN_POINT('Ctrl Pts',(-1.23603575560048,8.37681854397064,
119.466295679006));
#242957=CARTESIAN_POINT('Ctrl Pts',(-6.60531571179499,4.3055449539786,119.731219622048));
#242958=CARTESIAN_POINT('Ctrl Pts',(-7.41990169334089,-0.534064351226985,
119.943158776481));
#242959=CARTESIAN_POINT('Ctrl Pts',(-5.90985059955452,-5.22907041745032,
120.155097930914));
#242960=CARTESIAN_POINT('Ctrl Pts',(-1.20406785558409,-7.79671383358068,
120.367037085347));
#242961=CARTESIAN_POINT('Ctrl Pts',(3.57229297924018,-6.53381048057249,
120.57897623978));
#242962=CARTESIAN_POINT('Ctrl Pts',(6.27268273526995,-4.04270197401007,
120.737930605604));
#242963=CARTESIAN_POINT('Ctrl Pts',(7.42649812971622,-0.546840385823883,
120.896884971429));
#242964=CARTESIAN_POINT('Ctrl Pts',(6.60206978884195,4.31078409982334,121.108824125862));
#242965=CARTESIAN_POINT('Ctrl Pts',(1.2428283986206,8.36942923609148,121.373748068903));
#242966=CARTESIAN_POINT('Ctrl Pts',(-6.38650910065396,5.55979988983391,
121.691656800553));
#242967=CARTESIAN_POINT('Ctrl Pts',(-7.81779173216678,-1.02471724669847,
121.956580743594));
#242968=CARTESIAN_POINT('Ctrl Pts',(-5.28935936977621,-5.23095051854392,
122.168519898027));
#242969=CARTESIAN_POINT('Ctrl Pts',(-1.08901000657497,-7.81559778553687,
122.38045905246));
#242970=CARTESIAN_POINT('Ctrl Pts',(4.15559073899923,-6.70593704216965,
122.592398206893));
#242971=CARTESIAN_POINT('Ctrl Pts',(6.96276339914931,-2.64043223223665,
122.804337361326));
#242972=CARTESIAN_POINT('Ctrl Pts',(7.39417137872784,1.00807617272766,122.963291727151));
#242973=CARTESIAN_POINT('Ctrl Pts',(5.99729396871652,4.41411077466833,123.122246092976));
#242974=CARTESIAN_POINT('Ctrl Pts',(2.21203830249847,7.56816170548093,123.334185247409));
#242975=CARTESIAN_POINT('Ctrl Pts',(-4.49858829844026,7.1662173765172,123.59910919045));
#242976=CARTESIAN_POINT('Ctrl Pts',(-8.46722611683975,0.0703931391534947,
123.917017922099));
#242977=CARTESIAN_POINT('Ctrl Pts',(-5.27254733448871,-5.86243614965592,
124.181941865141));
#242978=CARTESIAN_POINT('Ctrl Pts',(-0.616419604178061,-7.41351419649813,
124.393881019574));
#242979=CARTESIAN_POINT('Ctrl Pts',(4.25527701186128,-6.64545928375415,
124.605820174007));
#242980=CARTESIAN_POINT('Ctrl Pts',(7.51781211550661,-2.39186684402398,
124.81775932844));
#242981=CARTESIAN_POINT('Ctrl Pts',(7.00649357738897,2.52210314530843,125.029698482873));
#242982=CARTESIAN_POINT('Ctrl Pts',(4.9615580818537,5.57430976430365,125.188652848697));
#242983=CARTESIAN_POINT('Ctrl Pts',(1.68541465194798,7.25336379407827,125.347607214523));
#242984=CARTESIAN_POINT('Ctrl Pts',(-3.24123735554682,7.18780672090154,
125.559546368955));
#242985=CARTESIAN_POINT('Ctrl Pts',(-8.07770166476711,2.51847254926066,
125.824470311997));
#242986=CARTESIAN_POINT('Ctrl Pts',(-6.47806386870863,-5.45284896367621,
126.142379043646));
#242987=CARTESIAN_POINT('Ctrl Pts',(-0.192986412053176,-7.88230101226661,
126.407302986687));
#242988=CARTESIAN_POINT('Ctrl Pts',(4.35281003611391,-6.03267856425323,
126.619242141121));
#242989=CARTESIAN_POINT('Ctrl Pts',(7.55421134507096,-2.28109677429749,
126.831181295553));
#242990=CARTESIAN_POINT('Ctrl Pts',(7.26650206864976,3.07188438745797,127.043120449986));
#242991=CARTESIAN_POINT('Ctrl Pts',(3.6824640510103,6.47235776503311,127.25505960442));
#242992=CARTESIAN_POINT('Ctrl Pts',(0.144109175608007,7.46118090475793,
127.414013970244));
#242993=CARTESIAN_POINT('Ctrl Pts',(-3.4365805220192,6.60619581861787,127.572968336069));
#242994=CARTESIAN_POINT('Ctrl Pts',(-7.13657130729556,3.35254157735825,
127.784907490502));
#242995=CARTESIAN_POINT('Ctrl Pts',(-7.7741656185088,-3.33980794393267,
128.049831433543));
#242996=CARTESIAN_POINT('Ctrl Pts',(-1.37513833513254,-8.35511028454946,
128.367740165193));
#242997=CARTESIAN_POINT('Ctrl Pts',(4.97933586881002,-6.11343825590796,
128.632664108234));
#242998=CARTESIAN_POINT('Ctrl Pts',(7.22980651019096,-1.75215972311049,
128.844603262667));
#242999=CARTESIAN_POINT('Ctrl Pts',(7.22211850511719,3.17970373427608,129.0565424171));
#243000=CARTESIAN_POINT('Ctrl Pts',(3.52245594917145,7.05909555748589,129.268481571533));
#243001=CARTESIAN_POINT('Ctrl Pts',(-1.41158837023047,7.31159181017459,
129.480420725966));
#243002=CARTESIAN_POINT('Ctrl Pts',(-4.74260762753219,5.7617411291468,129.639375091791));
#243003=CARTESIAN_POINT('Ctrl Pts',(-6.90673982745152,2.78367631632252,
129.798329457616));
#243004=CARTESIAN_POINT('Ctrl Pts',(-7.6016220492973,-2.094165053665,130.010268612049));
#243005=CARTESIAN_POINT('Ctrl Pts',(-3.7338785971554,-7.5927675315013,130.27519255509));
#243006=CARTESIAN_POINT('Ctrl Pts',(4.38876482180459,-7.24138223315527,
130.59310128674));
#243007=CARTESIAN_POINT('Ctrl Pts',(7.75827742238802,-1.40607412393191,
130.858025229781));
#243008=CARTESIAN_POINT('Ctrl Pts',(6.63170509553124,3.37055683729277,131.069964384214));
#243009=CARTESIAN_POINT('Ctrl Pts',(3.4186231137691,7.11213944968299,131.281903538646));
#243010=CARTESIAN_POINT('Ctrl Pts',(-1.91470314918058,7.65326321574815,
131.49384269308));
#243011=CARTESIAN_POINT('Ctrl Pts',(-5.82714299697742,4.6364168290748,131.705781847513));
#243012=CARTESIAN_POINT('Ctrl Pts',(-7.34973012681403,1.29284764638627,
131.864736213338));
#243013=CARTESIAN_POINT('Ctrl Pts',(-7.05708732553743,-2.37685239259637,
132.023690579162));
#243014=CARTESIAN_POINT('Ctrl Pts',(-4.41285707159829,-6.53428478500254,
132.235629733595));
#243015=CARTESIAN_POINT('Ctrl Pts',(2.10114438661684,-8.19616741724167,
132.500553676637));
#243016=CARTESIAN_POINT('Ctrl Pts',(8.04315266228028,-2.6469922935616,132.818462408286));
#243017=CARTESIAN_POINT('Ctrl Pts',(6.80810491019363,3.9771373395256,133.083386351327));
#243018=CARTESIAN_POINT('Ctrl Pts',(2.84599073507557,6.87317260771338,133.29532550576));
#243019=CARTESIAN_POINT('Ctrl Pts',(-2.02807652975791,7.62603553978654,
133.507264660194));
#243020=CARTESIAN_POINT('Ctrl Pts',(-6.43153630330859,4.56879295715197,
133.719203814626));
#243021=CARTESIAN_POINT('Ctrl Pts',(-7.4418072786159,-0.267310248786153,
133.93114296906));
#243022=CARTESIAN_POINT('Ctrl Pts',(-6.42411277744482,-3.79746993996031,
134.090097334884));
#243023=CARTESIAN_POINT('Ctrl Pts',(-3.81535505829936,-6.39491596926097,
134.249051700709));
#243024=CARTESIAN_POINT('Ctrl Pts',(0.897000119973648,-7.83362006457017,
134.460990855142));
#243025=CARTESIAN_POINT('Ctrl Pts',(6.92623262694139,-4.85997142739007,
134.725914798183));
#243026=CARTESIAN_POINT('Ctrl Pts',(7.83148551168685,3.21970026290371,135.043823529833));
#243027=CARTESIAN_POINT('Ctrl Pts',(2.58555082899131,7.44870036260414,135.308747472874));
#243028=CARTESIAN_POINT('Ctrl Pts',(-2.30771182868448,7.07209391365953,
135.520686627307));
#243029=CARTESIAN_POINT('Ctrl Pts',(-6.49988658939628,4.47442546144379,
135.73262578174));
#243030=CARTESIAN_POINT('Ctrl Pts',(-7.85711046003902,-0.711815285858144,
135.944564936173));
#243031=CARTESIAN_POINT('Ctrl Pts',(-5.47929954500003,-5.04244019035943,
136.156504090606));
#243032=CARTESIAN_POINT('Ctrl Pts',(-2.41102498573675,-7.06271675396063,
136.315458456431));
#243033=CARTESIAN_POINT('Ctrl Pts',(1.26093351925047,-7.33876072244591,
136.474412822256));
#243034=CARTESIAN_POINT('Ctrl Pts',(5.77428184003987,-5.36853784432293,
136.686351976689));
#243035=CARTESIAN_POINT('Ctrl Pts',(8.42507967409952,0.814116145085501,
136.95127591973));
#243036=CARTESIAN_POINT('Ctrl Pts',(3.85037761363912,7.53550889481658,137.269184651379));
#243037=CARTESIAN_POINT('Ctrl Pts',(-2.87114647199993,7.34548831796273,
137.534108594421));
#243038=CARTESIAN_POINT('Ctrl Pts',(-6.3638030095027,3.86426474823463,137.746047748854));
#243039=CARTESIAN_POINT('Ctrl Pts',(-7.45241316685895,0.360773785080116,
137.905002114679));
#243040=CARTESIAN_POINT('Ctrl Pts',(-6.70652287292767,-3.26151619872227,
138.063963195035));
#243041=CARTESIAN_POINT('Ctrl Pts',(-5.12228799394831,-5.13293287057993,
138.169939486783));
#243042=CARTESIAN_POINT('Ctrl Pts',(-4.15267718476094,-5.82426050198983,
138.222930989923));
#243043=CARTESIAN_POINT('Ctrl Pts',(-3.26246551232774,6.80480149199297,
7.78950320218665));
#243044=CARTESIAN_POINT('Ctrl Pts',(-4.39536709389074,6.26164979395597,
7.84249714630593));
#243045=CARTESIAN_POINT('Ctrl Pts',(-6.38055865555621,4.60310664943894,
7.94847587903347));
#243046=CARTESIAN_POINT('Ctrl Pts',(-7.81106616621988,0.973078339885786,
8.10743940036926));
#243047=CARTESIAN_POINT('Ctrl Pts',(-7.31333965367775,-2.86525814630475,
8.26639376619402));
#243048=CARTESIAN_POINT('Ctrl Pts',(-4.31289422291763,-7.11531479422214,
8.47833292062704));
#243049=CARTESIAN_POINT('Ctrl Pts',(2.63887624185738,-8.52866227043683,
8.74325686366829));
#243050=CARTESIAN_POINT('Ctrl Pts',(8.60950146298311,-2.37016650229916,
9.06116559531783));
#243051=CARTESIAN_POINT('Ctrl Pts',(6.97271530600223,4.53539036026586,9.32608953835907));
#243052=CARTESIAN_POINT('Ctrl Pts',(2.63807203832175,7.39959124865925,9.53802869279212));
#243053=CARTESIAN_POINT('Ctrl Pts',(-1.22838053918788,7.77689458005039,
9.69698305861685));
#243054=CARTESIAN_POINT('Ctrl Pts',(-4.78289431932195,6.23209737818189,
9.85593742444163));
#243055=CARTESIAN_POINT('Ctrl Pts',(-8.03767697735206,2.16109910769733,
10.0678765788747));
#243056=CARTESIAN_POINT('Ctrl Pts',(-7.56515171140129,-3.47482425972199,
10.2798157333077));
#243057=CARTESIAN_POINT('Ctrl Pts',(-3.67782389916916,-6.93307597046991,
10.4917548877407));
#243058=CARTESIAN_POINT('Ctrl Pts',(1.33995729764632,-8.20964364015745,
10.7036940421737));
#243059=CARTESIAN_POINT('Ctrl Pts',(7.55739580405241,-4.76308146157516,
10.968617985215));
#243060=CARTESIAN_POINT('Ctrl Pts',(8.07802332485162,3.7984276709196,11.2865267168645));
#243061=CARTESIAN_POINT('Ctrl Pts',(2.34932532116556,7.97976399560343,11.5514506599058));
#243062=CARTESIAN_POINT('Ctrl Pts',(-2.80879496170917,7.33683029847549,
11.7633898143388));
#243063=CARTESIAN_POINT('Ctrl Pts',(-5.9901045202014,5.10901982891564,11.9223441801636));
#243064=CARTESIAN_POINT('Ctrl Pts',(-7.68642959538423,1.62397085890266,
12.0812985459883));
#243065=CARTESIAN_POINT('Ctrl Pts',(-7.51118053981663,-3.58527067503237,
12.2932377004213));
#243066=CARTESIAN_POINT('Ctrl Pts',(-3.48738130667171,-7.55940845322157,
12.5051768548543));
#243067=CARTESIAN_POINT('Ctrl Pts',(1.7147567496136,-7.65856856774657,12.7171160092874));
#243068=CARTESIAN_POINT('Ctrl Pts',(6.35671423934268,-5.36522027114204,
12.9290551637204));
#243069=CARTESIAN_POINT('Ctrl Pts',(8.83861291433131,1.29628809543511,13.1939791067616));
#243070=CARTESIAN_POINT('Ctrl Pts',(3.66645602902048,8.13876865606542,13.5118878384111));
#243071=CARTESIAN_POINT('Ctrl Pts',(-3.40460975513775,7.58976711564749,
13.7768117814524));
#243072=CARTESIAN_POINT('Ctrl Pts',(-6.90497186101978,3.7469719316452,13.9887509358854));
#243073=CARTESIAN_POINT('Ctrl Pts',(-7.87294199547984,-0.0142644043681365,
14.1477053017102));
#243074=CARTESIAN_POINT('Ctrl Pts',(-6.89522531992549,-3.7648845852275,
14.3066596675349));
#243075=CARTESIAN_POINT('Ctrl Pts',(-3.37446971438952,-7.60821598627574,
14.518598821968));
#243076=CARTESIAN_POINT('Ctrl Pts',(2.26670668715013,-8.01052584493903,
14.730537976401));
#243077=CARTESIAN_POINT('Ctrl Pts',(6.28309316109777,-4.70285068408011,
14.942477130834));
#243078=CARTESIAN_POINT('Ctrl Pts',(8.31805470310959,0.0580469993626351,
15.154416285267));
#243079=CARTESIAN_POINT('Ctrl Pts',(5.87142792689939,6.73259055432228,15.4193402283083));
#243080=CARTESIAN_POINT('Ctrl Pts',(-2.50743336363754,8.56710179050404,
15.7372489599578));
#243081=CARTESIAN_POINT('Ctrl Pts',(-7.52207918090548,3.5516555438453,16.002172902999));
#243082=CARTESIAN_POINT('Ctrl Pts',(-7.68218533352712,-1.64391715972375,
16.2141120574321));
#243083=CARTESIAN_POINT('Ctrl Pts',(-5.97155115918559,-5.13069155787081,
16.3730664232568));
#243084=CARTESIAN_POINT('Ctrl Pts',(-2.78974346057701,-7.34410100576223,
16.5320207890816));
#243085=CARTESIAN_POINT('Ctrl Pts',(2.38422233231754,-7.97417583342083,
16.7439599435146));
#243086=CARTESIAN_POINT('Ctrl Pts',(6.93127360788379,-4.61128286748637,
16.9558990979476));
#243087=CARTESIAN_POINT('Ctrl Pts',(7.83138136454493,0.513351880983981,
17.1678382523807));
#243088=CARTESIAN_POINT('Ctrl Pts',(6.28121707157689,5.45341320606732,17.3797774068136));
#243089=CARTESIAN_POINT('Ctrl Pts',(0.082066861859703,8.93278828267373,
17.6447013498549));
#243090=CARTESIAN_POINT('Ctrl Pts',(-7.47609319966269,4.87754914199904,
17.9626100815045));
#243091=CARTESIAN_POINT('Ctrl Pts',(-8.02396617154493,-2.19360415377977,
18.2275340245457));
#243092=CARTESIAN_POINT('Ctrl Pts',(-4.76685931433096,-6.24463669112668,
18.4394731789787));
#243093=CARTESIAN_POINT('Ctrl Pts',(-1.19985877574573,-7.78098695713035,
18.5984275448035));
#243094=CARTESIAN_POINT('Ctrl Pts',(2.6566638581467,-7.39328244445395,18.7573819106283));
#243095=CARTESIAN_POINT('Ctrl Pts',(6.99690777616525,-4.50724726680322,
18.9693210650612));
#243096=CARTESIAN_POINT('Ctrl Pts',(8.26423625351865,1.00443150952637,19.1812602194943));
#243097=CARTESIAN_POINT('Ctrl Pts',(5.61541712122299,5.48280537547449,19.3931993739273));
#243098=CARTESIAN_POINT('Ctrl Pts',(1.22523305601358,8.2275274204848,19.6051385283603));
#243099=CARTESIAN_POINT('Ctrl Pts',(-5.74674067777189,6.83932840674638,
19.8700624714015));
#243100=CARTESIAN_POINT('Ctrl Pts',(-8.85127433654376,-1.15645915704036,
20.1879712030511));
#243101=CARTESIAN_POINT('Ctrl Pts',(-4.66903239368483,-6.88448028628875,
20.4528951460923));
#243102=CARTESIAN_POINT('Ctrl Pts',(0.43971789051534,-7.84379266066805,
20.6648343005254));
#243103=CARTESIAN_POINT('Ctrl Pts',(4.14856089524914,-6.69125261869378,
20.8237886663501));
#243104=CARTESIAN_POINT('Ctrl Pts',(6.82611211149119,-3.88878922031102,
20.9827430321749));
#243105=CARTESIAN_POINT('Ctrl Pts',(8.24644105192192,1.12614667314857,21.1946821866079));
#243106=CARTESIAN_POINT('Ctrl Pts',(5.62488927856695,6.13735318481544,21.4066213410409));
#243107=CARTESIAN_POINT('Ctrl Pts',(0.700331656051833,7.8168791600093,21.6185604954739));
#243108=CARTESIAN_POINT('Ctrl Pts',(-4.41967471566694,7.04697657893599,
21.830499649907));
#243109=CARTESIAN_POINT('Ctrl Pts',(-8.81330466808416,1.45845887854694,
22.0954235929482));
#243110=CARTESIAN_POINT('Ctrl Pts',(-5.97197857768723,-6.63460074385073,
22.4133323245977));
#243111=CARTESIAN_POINT('Ctrl Pts',(0.930130823812995,-8.26624394487423,
22.678256267639));
#243112=CARTESIAN_POINT('Ctrl Pts',(5.43493913296469,-5.67273053720678,
22.890195422072));
#243113=CARTESIAN_POINT('Ctrl Pts',(7.50292233142839,-2.38528312728696,
23.0491497878967));
#243114=CARTESIAN_POINT('Ctrl Pts',(7.71450329194046,1.4848996994052,23.2081041537216));
#243115=CARTESIAN_POINT('Ctrl Pts',(5.53221819568165,6.21824397942342,23.4200433081545));
#243116=CARTESIAN_POINT('Ctrl Pts',(0.281868169604722,8.32027847167783,
23.6319824625876));
#243117=CARTESIAN_POINT('Ctrl Pts',(-4.55137707224933,6.39367116583729,
23.8439216170206));
#243118=CARTESIAN_POINT('Ctrl Pts',(-7.9402099676926,2.47920736634371,24.0558607714536));
#243119=CARTESIAN_POINT('Ctrl Pts',(-7.6436423637654,-4.6234373454971,24.3207847144949));
#243120=CARTESIAN_POINT('Ctrl Pts',(-0.222175825763065,-8.9237376174508,
24.6386934461444));
#243121=CARTESIAN_POINT('Ctrl Pts',(6.08221490338514,-5.67473296064375,
24.9036173891856));
#243122=CARTESIAN_POINT('Ctrl Pts',(7.81778817998088,-0.774998774025085,
25.1155565436187));
#243123=CARTESIAN_POINT('Ctrl Pts',(7.25090930717722,3.06720285078402,25.2745109094434));
#243124=CARTESIAN_POINT('Ctrl Pts',(4.8948209487679,6.14485280850215,25.4334652752682));
#243125=CARTESIAN_POINT('Ctrl Pts',(0.158864732842611,8.32146371433087,
25.6454044297012));
#243126=CARTESIAN_POINT('Ctrl Pts',(-5.19663643807538,6.50395673738447,
25.8573435841342));
#243127=CARTESIAN_POINT('Ctrl Pts',(-7.6154088784006,1.89726430563413,26.0692827385672));
#243128=CARTESIAN_POINT('Ctrl Pts',(-7.64418292931668,-3.28022420567889,
26.2812218930003));
#243129=CARTESIAN_POINT('Ctrl Pts',(-2.79996673668053,-8.48301996616586,
26.5461458360415));
#243130=CARTESIAN_POINT('Ctrl Pts',(5.63441854526134,-6.92356720336237,
26.8640545676911));
#243131=CARTESIAN_POINT('Ctrl Pts',(8.31080550648391,-0.355589846555956,
27.1289785107322));
#243132=CARTESIAN_POINT('Ctrl Pts',(6.44291851635036,4.49524594638147,27.3409176651653));
#243133=CARTESIAN_POINT('Ctrl Pts',(3.51365506821086,7.04539900718213,27.49987203099));
#243134=CARTESIAN_POINT('Ctrl Pts',(-0.277618957157626,7.85120474024724,
27.6588263968148));
#243135=CARTESIAN_POINT('Ctrl Pts',(-5.29084907199106,6.42486672621914,
27.8707655512479));
#243136=CARTESIAN_POINT('Ctrl Pts',(-8.17731205292236,1.56142598301422,
28.0827047056808));
#243137=CARTESIAN_POINT('Ctrl Pts',(-7.01899814341604,-3.51108662572979,
28.2946438601139));
#243138=CARTESIAN_POINT('Ctrl Pts',(-3.67388273850926,-7.46297454906964,
28.5065830145468));
#243139=CARTESIAN_POINT('Ctrl Pts',(3.38954829579464,-8.26513180919469,
28.7715069575882));
#243140=CARTESIAN_POINT('Ctrl Pts',(8.78275841978252,-1.59549669457496,
29.0894156892376));
#243141=CARTESIAN_POINT('Ctrl Pts',(6.54470238889186,5.13447202216646,29.3543396322789));
#243142=CARTESIAN_POINT('Ctrl Pts',(1.97117862514593,7.6047938798206,29.566278786712));
#243143=CARTESIAN_POINT('Ctrl Pts',(-1.91248189418154,7.6371350723419,29.7252331525367));
#243144=CARTESIAN_POINT('Ctrl Pts',(-5.3166178020407,5.78377586924648,29.8841875183615));
#243145=CARTESIAN_POINT('Ctrl Pts',(-8.19744939059084,1.4400763316465,30.0961266727944));
#243146=CARTESIAN_POINT('Ctrl Pts',(-7.22745926297717,-4.13162390753411,
30.3080658272275));
#243147=CARTESIAN_POINT('Ctrl Pts',(-3.04881722608634,-7.23178938801285,
30.5200049816605));
#243148=CARTESIAN_POINT('Ctrl Pts',(2.0623156308354,-8.05855183858673,30.7319441360935));
#243149=CARTESIAN_POINT('Ctrl Pts',(7.9498340937961,-4.07450357148001,30.9968680791348));
#243150=CARTESIAN_POINT('Ctrl Pts',(7.70955444004336,4.49946946857826,31.3147768107843));
#243151=CARTESIAN_POINT('Ctrl Pts',(1.63280533877429,8.15658501036109,31.5797007538256));
#243152=CARTESIAN_POINT('Ctrl Pts',(-3.44803318921775,7.05900150537185,
31.7916399082586));
#243153=CARTESIAN_POINT('Ctrl Pts',(-6.41936025911783,4.55798562661464,
31.9505942740834));
#243154=CARTESIAN_POINT('Ctrl Pts',(-7.8001170948581,0.936302015994993,
32.1095486399081));
#243155=CARTESIAN_POINT('Ctrl Pts',(-7.16384203849904,-4.23690495523571,
32.3214877943411));
#243156=CARTESIAN_POINT('Ctrl Pts',(-2.80363681848531,-7.83875654050661,
32.5334269487741));
#243157=CARTESIAN_POINT('Ctrl Pts',(2.38681622999895,-7.47644116641532,
32.7453661032072));
#243158=CARTESIAN_POINT('Ctrl Pts',(6.80723592320504,-4.78068432153856,
32.9573052576402));
#243159=CARTESIAN_POINT('Ctrl Pts',(8.68893164352905,2.07458631224778,33.2222292006814));
#243160=CARTESIAN_POINT('Ctrl Pts',(2.93065566490345,8.43170875543204,33.540137932331));
#243161=CARTESIAN_POINT('Ctrl Pts',(-4.06392023714902,7.25813230877389,
33.8050618753722));
#243162=CARTESIAN_POINT('Ctrl Pts',(-7.20990426579662,3.12021082698539,
34.0170010298053));
#243163=CARTESIAN_POINT('Ctrl Pts',(-7.84069197061069,-0.712017226454603,
34.17595539563));
#243164=CARTESIAN_POINT('Ctrl Pts',(-6.53439150746701,-4.36121723671235,
34.3349097614548));
#243165=CARTESIAN_POINT('Ctrl Pts',(-2.68684345496923,-7.8773643181432,
34.5468489158878));
#243166=CARTESIAN_POINT('Ctrl Pts',(2.96778910260848,-7.7780917552919,34.7587880703208));
#243167=CARTESIAN_POINT('Ctrl Pts',(6.67519629422216,-4.12744699109014,
34.9707272247538));
#243168=CARTESIAN_POINT('Ctrl Pts',(8.28017222118654,0.795079545623429,
35.1826663791868));
#243169=CARTESIAN_POINT('Ctrl Pts',(5.25158436503955,7.2265000608703,35.4475903222281));
#243170=CARTESIAN_POINT('Ctrl Pts',(-3.25689980097036,8.31114064669219,
35.7654990538776));
#243171=CARTESIAN_POINT('Ctrl Pts',(-7.80727118048563,2.87096656545065,
36.0304229969189));
#243172=CARTESIAN_POINT('Ctrl Pts',(-7.50624371913036,-2.31834862689053,
36.2423621513519));
#243173=CARTESIAN_POINT('Ctrl Pts',(-5.49329597497169,-5.63977999926653,
36.4013165171766));
#243174=CARTESIAN_POINT('Ctrl Pts',(-2.12782804304351,-7.56246229596497,
36.5602708830014));
#243175=CARTESIAN_POINT('Ctrl Pts',(3.08162039864436,-7.73146894651498,
36.7722100374344));
#243176=CARTESIAN_POINT('Ctrl Pts',(7.31270967674463,-3.97878884774588,
36.9841491918675));
#243177=CARTESIAN_POINT('Ctrl Pts',(7.75505888079484,1.20545675412319,37.1960883463004));
#243178=CARTESIAN_POINT('Ctrl Pts',(5.77313907428006,5.9886783788578,37.4080275007335));
#243179=CARTESIAN_POINT('Ctrl Pts',(-0.710003321956093,8.90490520756383,
37.6729514437747));
#243180=CARTESIAN_POINT('Ctrl Pts',(-7.87898520817115,4.19571772788399,
37.9908601754243));
#243181=CARTESIAN_POINT('Ctrl Pts',(-7.7979585419246,-2.89616554844543,
38.2557841184655));
#243182=CARTESIAN_POINT('Ctrl Pts',(-4.19461224505018,-6.64256450781354,
38.4677232728986));
#243183=CARTESIAN_POINT('Ctrl Pts',(-0.505477830120367,-7.85671122493527,
38.6266776387233));
#243184=CARTESIAN_POINT('Ctrl Pts',(3.30150286740242,-7.12871425820865,
38.7856320045481));
#243185=CARTESIAN_POINT('Ctrl Pts',(7.36886445395877,-3.86934529493679,
38.9975711589811));
#243186=CARTESIAN_POINT('Ctrl Pts',(8.14268390733605,1.73296921395396,39.209510313414));
#243187=CARTESIAN_POINT('Ctrl Pts',(5.10735438731375,5.95894247270799,39.4214494678471));
#243188=CARTESIAN_POINT('Ctrl Pts',(0.491173655079499,8.30374324849543,
39.6333886222801));
#243189=CARTESIAN_POINT('Ctrl Pts',(-6.33031893734865,6.30305510243496,
39.8983125653214));
#243190=CARTESIAN_POINT('Ctrl Pts',(-8.71393677955521,-1.93642995343888,
40.2162212969708));
#243191=CARTESIAN_POINT('Ctrl Pts',(-4.04045855890807,-7.2712190820607,
40.4811452400122));
#243192=CARTESIAN_POINT('Ctrl Pts',(1.13321262724659,-7.77394779171034,
40.6930843944451));
#243193=CARTESIAN_POINT('Ctrl Pts',(4.72530462334761,-6.29721488638721,
40.85203876027));
#243194=CARTESIAN_POINT('Ctrl Pts',(7.14392469148291,-3.26845960064897,
41.0109931260947));
#243195=CARTESIAN_POINT('Ctrl Pts',(8.11417066222751,1.85262808369974,41.2229322805278));
#243196=CARTESIAN_POINT('Ctrl Pts',(5.05877418903363,6.61175371710629,41.4348714349606));
#243197=CARTESIAN_POINT('Ctrl Pts',(0.00473544728136623,7.84818716686823,
41.6468105893938));
#243198=CARTESIAN_POINT('Ctrl Pts',(-5.02688059019021,6.62750896101593,
41.8587497438267));
#243199=CARTESIAN_POINT('Ctrl Pts',(-8.90788673614655,0.671561887595279,
42.123673686868));
#243200=CARTESIAN_POINT('Ctrl Pts',(-5.36042448800456,-7.13780809990443,
42.4415824185176));
#243201=CARTESIAN_POINT('Ctrl Pts',(1.65913890447776,-8.15126925093418,
42.7065063615587));
#243202=CARTESIAN_POINT('Ctrl Pts',(5.91634452571092,-5.16868480175369,
42.9184455159919));
#243203=CARTESIAN_POINT('Ctrl Pts',(7.68480967867267,-1.71088261179591,
43.0773998818165));
#243204=CARTESIAN_POINT('Ctrl Pts',(7.55252880873698,2.16282147942261,43.2363542476413));
#243205=CARTESIAN_POINT('Ctrl Pts',(4.95929817328987,6.68411235547928,43.4482934020744));
#243206=CARTESIAN_POINT('Ctrl Pts',(-0.456699289431316,8.3125152192543,
43.6602325565073));
#243207=CARTESIAN_POINT('Ctrl Pts',(-5.10015964534588,5.96510149307131,
43.8721717109404));
#243208=CARTESIAN_POINT('Ctrl Pts',(-8.12870113673735,1.76567871539049,
44.0841108653733));
#243209=CARTESIAN_POINT('Ctrl Pts',(-7.20376617372028,-5.2827260374971,
44.3490348084147));
#243210=CARTESIAN_POINT('Ctrl Pts',(0.569643592965396,-8.9083085566034,
44.6669435400641));
#243211=CARTESIAN_POINT('Ctrl Pts',(6.56125028082896,-5.11330881698911,
44.9318674831055));
#243212=CARTESIAN_POINT('Ctrl Pts',(7.85571064144068,-0.079028126288852,
45.1438066375384));
#243213=CARTESIAN_POINT('Ctrl Pts',(6.95051382093977,3.69780701682662,45.3027610033632));
#243214=CARTESIAN_POINT('Ctrl Pts',(4.33091448518403,6.55451507593636,45.461715369188));
#243215=CARTESIAN_POINT('Ctrl Pts',(-0.579323671401443,8.30279353206021,
45.673654523621));
#243216=CARTESIAN_POINT('Ctrl Pts',(-5.75265448145445,6.01776120565647,
45.8855936780539));
#243217=CARTESIAN_POINT('Ctrl Pts',(-7.75359853509504,1.21481438385805,
46.0975328324871));
#243218=CARTESIAN_POINT('Ctrl Pts',(-7.32335872983018,-3.94484732411758,
46.3094719869199));
#243219=CARTESIAN_POINT('Ctrl Pts',(-2.03706433959468,-8.69780491556567,
46.5743959299614));
#243220=CARTESIAN_POINT('Ctrl Pts',(6.22590528031026,-6.39691789874345,
46.8923046616107));
#243221=CARTESIAN_POINT('Ctrl Pts',(8.30961377121896,0.382428135398561,
47.1572286046521));
#243222=CARTESIAN_POINT('Ctrl Pts',(6.01913013605845,5.04861441704378,47.3691677590852));
#243223=CARTESIAN_POINT('Ctrl Pts',(2.87536563614646,7.32909896012022,47.5281221249098));
#243224=CARTESIAN_POINT('Ctrl Pts',(-0.972408631255065,7.79569814785787,
47.6870764907346));
#243225=CARTESIAN_POINT('Ctrl Pts',(-5.83948627040479,5.93063204473356,
47.8990156451677));
#243226=CARTESIAN_POINT('Ctrl Pts',(-8.28352357966365,0.830494200135225,
48.1109547996006));
#243227=CARTESIAN_POINT('Ctrl Pts',(-6.68017227841064,-4.11938861500226,
48.3228939540337));
#243228=CARTESIAN_POINT('Ctrl Pts',(-2.99795137740172,-7.75923263184659,
48.5348331084667));
#243229=CARTESIAN_POINT('Ctrl Pts',(4.10877821917824,-7.93217391504327,
48.799757051508));
#243230=CARTESIAN_POINT('Ctrl Pts',(8.88960689517256,-0.810767791640073,
49.1176657831574));
#243231=CARTESIAN_POINT('Ctrl Pts',(6.06385636353744,5.69434617036614,49.3825897261988));
#243232=CARTESIAN_POINT('Ctrl Pts',(1.28937864505078,7.74957662304695,49.5945288806317));
#243233=CARTESIAN_POINT('Ctrl Pts',(-2.5818633881568,7.43756684364333,49.7534832464565));
#243234=CARTESIAN_POINT('Ctrl Pts',(-5.80833124720238,5.28978036230487,
49.9124376122813));
#243235=CARTESIAN_POINT('Ctrl Pts',(-8.29282597862484,0.707837298050547,
50.1243767667142));
#243236=CARTESIAN_POINT('Ctrl Pts',(-6.83281236016946,-4.75596034066911,
50.3363159211473));
#243237=CARTESIAN_POINT('Ctrl Pts',(-2.3958367743758,-7.47355540430421,
50.5482550755803));
#243238=CARTESIAN_POINT('Ctrl Pts',(2.76845920063465,-7.84404469331985,
50.7601942300133));
#243239=CARTESIAN_POINT('Ctrl Pts',(8.27968458926794,-3.35384325440609,
51.0251181730547));
#243240=CARTESIAN_POINT('Ctrl Pts',(7.28040658544384,5.16508810314844,51.3430269047041));
#243241=CARTESIAN_POINT('Ctrl Pts',(0.903429743624333,8.26920473829927,
51.6079508477454));
#243242=CARTESIAN_POINT('Ctrl Pts',(-4.06012899028692,6.72560686548218,
51.8198900021784));
#243243=CARTESIAN_POINT('Ctrl Pts',(-6.79808713850607,3.97107420807589,
51.9788443680031));
#243244=CARTESIAN_POINT('Ctrl Pts',(-7.85240602808846,0.241262779337893,
52.1377987338279));
#243245=CARTESIAN_POINT('Ctrl Pts',(-6.76011405349243,-4.85518839346535,
52.3497378882609));
#243246=CARTESIAN_POINT('Ctrl Pts',(-2.09782350855731,-8.05640242529173,
52.561677042694));
#243247=CARTESIAN_POINT('Ctrl Pts',(3.04008796020144,-7.23546331791505,
52.7736161971269));
#243248=CARTESIAN_POINT('Ctrl Pts',(7.20417486875693,-4.15851751911049,
52.98555535156));
#243249=CARTESIAN_POINT('Ctrl Pts',(8.47085590091533,2.83655456122647,53.2504792946012));
#243250=CARTESIAN_POINT('Ctrl Pts',(2.17178682133626,8.658279111078,53.5683880262508));
#243251=CARTESIAN_POINT('Ctrl Pts',(-4.69124180250278,6.86936552063046,
53.8333119692919));
#243252=CARTESIAN_POINT('Ctrl Pts',(-7.45808430376615,2.4688891519682,54.0452511237251));
#243253=CARTESIAN_POINT('Ctrl Pts',(-7.74672437347938,-1.40416544256998,
54.2042054895497));
#243254=CARTESIAN_POINT('Ctrl Pts',(-6.12212259204269,-4.92322080823666,
54.3631598553746));
#243255=CARTESIAN_POINT('Ctrl Pts',(-1.97806785630035,-8.08450641091576,
54.5750990098075));
#243256=CARTESIAN_POINT('Ctrl Pts',(3.64551073029963,-7.48443284601927,
54.7870381642407));
#243257=CARTESIAN_POINT('Ctrl Pts',(7.01475598801421,-3.51955432679692,
54.9989773186736));
#243258=CARTESIAN_POINT('Ctrl Pts',(8.17711282074447,1.52585366703169,55.2109164731066));
#243259=CARTESIAN_POINT('Ctrl Pts',(4.59040324664707,7.66352657110666,55.475840416148));
#243260=CARTESIAN_POINT('Ctrl Pts',(-3.98072973124768,7.98975881797569,
55.7937491477973));
#243261=CARTESIAN_POINT('Ctrl Pts',(-8.03100867590238,2.16767893221239,
56.0586730908387));
#243262=CARTESIAN_POINT('Ctrl Pts',(-7.27121712159267,-2.97453134080762,
56.2706122452717));
#243263=CARTESIAN_POINT('Ctrl Pts',(-4.97180061469368,-6.10447522367803,
56.4295666110964));
#243264=CARTESIAN_POINT('Ctrl Pts',(-1.44916354451103,-7.72129608161182,
56.5885209769212));
#243265=CARTESIAN_POINT('Ctrl Pts',(3.75476166008969,-7.42790422852821,
56.8004601313542));
#243266=CARTESIAN_POINT('Ctrl Pts',(7.63658415500593,-3.31497601119741,
57.0123992857873));
#243267=CARTESIAN_POINT('Ctrl Pts',(7.61769287909937,1.88807294095723,57.2243384402202));
#243268=CARTESIAN_POINT('Ctrl Pts',(5.21961813140454,6.47680400032997,57.4362775946533));
#243269=CARTESIAN_POINT('Ctrl Pts',(-1.49648475381148,8.80692766261284,
57.7012015376945));
#243270=CARTESIAN_POINT('Ctrl Pts',(-8.21985821948872,3.48085995325354,
58.0191102693441));
#243271=CARTESIAN_POINT('Ctrl Pts',(-7.51056971204447,-3.57592993584844,
58.2840342123853));
#243272=CARTESIAN_POINT('Ctrl Pts',(-3.58934751700118,-6.98820574460903,
58.4959733668183));
#243273=CARTESIAN_POINT('Ctrl Pts',(0.192881956345414,-7.87059182397891,
58.6549277326431));
#243274=CARTESIAN_POINT('Ctrl Pts',(3.92035427906174,-6.8080327911443,58.8138820984678));
#243275=CARTESIAN_POINT('Ctrl Pts',(7.68281752192254,-3.20098598514689,
59.0258212529009));
#243276=CARTESIAN_POINT('Ctrl Pts',(7.95703687420663,2.44786594686428,59.2377604073338));
#243277=CARTESIAN_POINT('Ctrl Pts',(4.55908939524148,6.3881740831675,59.4496995617669));
#243278=CARTESIAN_POINT('Ctrl Pts',(-0.246751992170809,8.31459661984495,
59.6616387161999));
#243279=CARTESIAN_POINT('Ctrl Pts',(-6.86406844080779,5.71716764777737,
59.9265626592412));
#243280=CARTESIAN_POINT('Ctrl Pts',(-8.50800795016616,-2.70115824833899,
60.2444713908907));
#243281=CARTESIAN_POINT('Ctrl Pts',(-3.38008047759511,-7.60072287815818,
60.509395333932));
#243282=CARTESIAN_POINT('Ctrl Pts',(1.81778734332943,-7.64291072178791,
60.721334488365));
#243283=CARTESIAN_POINT('Ctrl Pts',(5.26485337691342,-5.85360897467286,
60.8802888541898));
#243284=CARTESIAN_POINT('Ctrl Pts',(7.40550426256974,-2.62240248164066,
61.0392432200145));
#243285=CARTESIAN_POINT('Ctrl Pts',(7.91803002602142,2.56452663454484,61.2511823744476));
#243286=CARTESIAN_POINT('Ctrl Pts',(4.45283923768672,7.03411019494427,61.4631215288804));
#243287=CARTESIAN_POINT('Ctrl Pts',(-0.690898036301095,7.81771860161846,
61.6750606833136));
#243288=CARTESIAN_POINT('Ctrl Pts',(-5.59451765160311,6.15587327211004,
61.8869998377465));
#243289=CARTESIAN_POINT('Ctrl Pts',(-8.93235086543013,-0.120621265688294,
62.1519237807879));
#243290=CARTESIAN_POINT('Ctrl Pts',(-4.70667611282939,-7.58483059346624,
62.4698325124373));
#243291=CARTESIAN_POINT('Ctrl Pts',(2.37508716483103,-7.97213229098914,
62.7347564554786));
#243292=CARTESIAN_POINT('Ctrl Pts',(6.35117973907172,-4.62395404916552,
62.9466956099116));
#243293=CARTESIAN_POINT('Ctrl Pts',(7.80620647068915,-1.02301497825693,
63.1056499757364));
#243294=CARTESIAN_POINT('Ctrl Pts',(7.33110501187211,2.82371872954047,63.2646043415611));
#243295=CARTESIAN_POINT('Ctrl Pts',(4.34734130905187,7.09736711005406,63.4765434959941));
#243296=CARTESIAN_POINT('Ctrl Pts',(-1.19167186521786,8.23932046208598,
63.6884826504273));
#243297=CARTESIAN_POINT('Ctrl Pts',(-5.60879659329404,5.48957785314227,
63.9004218048601));
#243298=CARTESIAN_POINT('Ctrl Pts',(-8.2532076834423,1.03825162188433,64.1123609592932));
#243299=CARTESIAN_POINT('Ctrl Pts',(-6.70718593584579,-5.90043204306947,
64.3772849023344));
#243300=CARTESIAN_POINT('Ctrl Pts',(1.3569790935935,-8.82275823664084,64.695193633984));
#243301=CARTESIAN_POINT('Ctrl Pts',(6.98863913883046,-4.51163554520679,
64.9601175770253));
#243302=CARTESIAN_POINT('Ctrl Pts',(7.83179731017781,0.617564586981519,
65.1720567314582));
#243303=CARTESIAN_POINT('Ctrl Pts',(6.5954077487877,4.29930409903505,65.3310110972831));
#243304=CARTESIAN_POINT('Ctrl Pts',(3.73291746727506,6.91258383972131,65.4899654631077));
#243305=CARTESIAN_POINT('Ctrl Pts',(-1.31295196134937,8.21876836877148,
65.7019046175408));
#243306=CARTESIAN_POINT('Ctrl Pts',(-6.2633908225815,5.48419719873932,65.9138437719738));
#243307=CARTESIAN_POINT('Ctrl Pts',(-7.83075616889244,0.522802117716418,
66.1257829264069));
#243308=CARTESIAN_POINT('Ctrl Pts',(-6.94488911626896,-4.5784187945913,
66.3377220808398));
#243309=CARTESIAN_POINT('Ctrl Pts',(-1.25812730308113,-8.84412557361244,
66.6026460238811));
#243310=CARTESIAN_POINT('Ctrl Pts',(6.768385145733,-5.81991560801015,66.9205547555308));
#243311=CARTESIAN_POINT('Ctrl Pts',(8.24301336953791,1.11743585548131,67.1854786985716));
#243312=CARTESIAN_POINT('Ctrl Pts',(5.54796250548142,5.56224299785549,67.397417853005));
#243313=CARTESIAN_POINT('Ctrl Pts',(2.21444292139709,7.55510831538417,67.5563722188296));
#243314=CARTESIAN_POINT('Ctrl Pts',(-1.65954404302216,7.67882814728032,
67.7153265846545));
#243315=CARTESIAN_POINT('Ctrl Pts',(-6.34215827828067,5.38971472157569,
67.9272657390875));
#243316=CARTESIAN_POINT('Ctrl Pts',(-8.32453180135945,0.0930252258306557,
68.1392048935204));
#243317=CARTESIAN_POINT('Ctrl Pts',(-6.28876381349589,-4.69526506162374,
68.3511440479535));
#243318=CARTESIAN_POINT('Ctrl Pts',(-2.29842179002175,-7.99441434915497,
68.5630832023865));
#243319=CARTESIAN_POINT('Ctrl Pts',(4.79566608438709,-7.5367783391113,68.8280071454277));
#243320=CARTESIAN_POINT('Ctrl Pts',(8.92648138613808,-0.0196569970329377,
69.1459158770774));
#243321=CARTESIAN_POINT('Ctrl Pts',(5.53527891642114,6.20939762466144,69.4108398201185));
#243322=CARTESIAN_POINT('Ctrl Pts',(0.5974295459376,7.83335894944233,69.6227789745516));
#243323=CARTESIAN_POINT('Ctrl Pts',(-3.23092222251469,7.17945433185997,
69.7817333403763));
#243324=CARTESIAN_POINT('Ctrl Pts',(-6.25432410808943,4.75414642905697,
69.9406877062012));
#243325=CARTESIAN_POINT('Ctrl Pts',(-8.32292747176321,-0.0299729537079767,
70.152626860634));
#243326=CARTESIAN_POINT('Ctrl Pts',(-6.38437861557071,-5.3428614226726,
70.3645660150671));
#243327=CARTESIAN_POINT('Ctrl Pts',(-1.72400082497685,-7.65649265655503,
70.5765051695001));
#243328=CARTESIAN_POINT('Ctrl Pts',(3.45281847846123,-7.56779612100605,
70.7884443239331));
#243329=CARTESIAN_POINT('Ctrl Pts',(8.54434607633237,-2.60677794249014,
71.0533682669744));
#243330=CARTESIAN_POINT('Ctrl Pts',(6.79397949587998,5.7900405059201,71.371276998624));
#243331=CARTESIAN_POINT('Ctrl Pts',(0.166895290820339,8.31675000984924,
71.6362009416652));
#243332=CARTESIAN_POINT('Ctrl Pts',(-4.64019985420912,6.3392496442617,71.8481400960982));
#243333=CARTESIAN_POINT('Ctrl Pts',(-7.12344690626189,3.3529534257354,72.0070944619229));
#243334=CARTESIAN_POINT('Ctrl Pts',(-7.84261740387319,-0.455766372781194,
72.1660488277477));
#243335=CARTESIAN_POINT('Ctrl Pts',(-6.30378518167492,-5.43504724490109,
72.3779879821807));
#243336=CARTESIAN_POINT('Ctrl Pts',(-1.37432578812005,-8.21103013242127,
72.5899271366136));
#243337=CARTESIAN_POINT('Ctrl Pts',(3.66806036601191,-6.93706751891167,
72.8018662910468));
#243338=CARTESIAN_POINT('Ctrl Pts',(7.54760553646316,-3.50470055633481,
73.0138054454797));
#243339=CARTESIAN_POINT('Ctrl Pts',(8.17933434237327,3.57847002169365,73.2787293885211));
#243340=CARTESIAN_POINT('Ctrl Pts',(1.40752855508706,8.81285437154256,73.5966381201706));
#243341=CARTESIAN_POINT('Ctrl Pts',(-6.64161658068516,5.95575605302166,
73.9145468518201));
#243342=CARTESIAN_POINT('Ctrl Pts',(-8.60644060131243,-2.36190938767852,
74.2324555834696));
#243343=CARTESIAN_POINT('Ctrl Pts',(-2.67128209997195,-8.51154233440134,
74.5503643151191));
#243344=CARTESIAN_POINT('Ctrl Pts',(5.70868662607485,-6.85991514617173,
74.8682730467687));
#243345=CARTESIAN_POINT('Ctrl Pts',(8.8601291134706,1.09775683697152,75.1861817784181));
#243346=CARTESIAN_POINT('Ctrl Pts',(4.7014470489875,6.86627052840108,75.4511057214595));
#243347=CARTESIAN_POINT('Ctrl Pts',(-0.386629038597262,7.83760745362767,
75.6630448758923));
#243348=CARTESIAN_POINT('Ctrl Pts',(-5.37294721035328,6.35934159187716,
75.8749840303256));
#243349=CARTESIAN_POINT('Ctrl Pts',(-8.19495358954785,1.45608441931355,
76.0869231847584));
#243350=CARTESIAN_POINT('Ctrl Pts',(-6.97666527869318,-3.61116495319303,
76.2988623391915));
#243351=CARTESIAN_POINT('Ctrl Pts',(-4.41416014940891,-6.51927777264119,
76.4578167050163));
#243352=CARTESIAN_POINT('Ctrl Pts',(-0.754476603388974,-7.81973821775469,
76.616771070841));
#243353=CARTESIAN_POINT('Ctrl Pts',(4.38861498873997,-7.06655809040249,
76.828710225274));
#243354=CARTESIAN_POINT('Ctrl Pts',(8.79768019749863,-1.51114181769062,
77.0936341683152));
#243355=CARTESIAN_POINT('Ctrl Pts',(6.01688937045951,6.60289204949171,77.4115428999649));
#243356=CARTESIAN_POINT('Ctrl Pts',(-0.893661257363742,8.27011868907599,
77.6764668430059));
#243357=CARTESIAN_POINT('Ctrl Pts',(-5.39058883550149,5.70399953111573,
77.8884059974392));
#243358=CARTESIAN_POINT('Ctrl Pts',(-8.21720337438167,1.33567480806146,
78.100345151872));
#243359=CARTESIAN_POINT('Ctrl Pts',(-7.172357192277,-4.22247704370048,78.3122843063052));
#243360=CARTESIAN_POINT('Ctrl Pts',(-2.95157590649486,-7.28056852080544,
78.5242234607381));
#243361=CARTESIAN_POINT('Ctrl Pts',(0.886254111097857,-7.82291355965053,
78.6831778265629));
#243362=CARTESIAN_POINT('Ctrl Pts',(4.51210422477735,-6.4311235377587,78.8421321923876));
#243363=CARTESIAN_POINT('Ctrl Pts',(7.92934885359968,-2.51423115517351,
79.0540713468206));
#243364=CARTESIAN_POINT('Ctrl Pts',(7.66603324321095,4.57322540977227,79.318995289862));
#243365=CARTESIAN_POINT('Ctrl Pts',(0.276913615402863,8.92887225664263,
79.6369040215116));
#243366=CARTESIAN_POINT('Ctrl Pts',(-6.05702989090295,5.7013851309598,79.9018279645525));
#243367=CARTESIAN_POINT('Ctrl Pts',(-7.80443120191717,0.827597677245151,
80.113767118986));
#243368=CARTESIAN_POINT('Ctrl Pts',(-7.11095513019963,-4.32906462654154,
80.3257062734185));
#243369=CARTESIAN_POINT('Ctrl Pts',(-2.70269477232959,-7.87193987364972,
80.537645427852));
#243370=CARTESIAN_POINT('Ctrl Pts',(2.49240898868442,-7.45026077257168,
80.7495845822845));
#243371=CARTESIAN_POINT('Ctrl Pts',(5.7605808189592,-5.3664818771288,80.9085389481096));
#243372=CARTESIAN_POINT('Ctrl Pts',(7.60993018997647,-1.95125539925059,
81.0674933139342));
#243373=CARTESIAN_POINT('Ctrl Pts',(7.65870841186064,3.24655475290215,81.2794324683674));
#243374=CARTESIAN_POINT('Ctrl Pts',(2.8496297260068,8.45943648182299,81.5443564114084));
#243375=CARTESIAN_POINT('Ctrl Pts',(-5.59617506972902,6.96306441601157,
81.8622651430582));
#243376=CARTESIAN_POINT('Ctrl Pts',(-8.30900542237379,0.392214720402506,
82.1271890860993));
#243377=CARTESIAN_POINT('Ctrl Pts',(-6.46697724744239,-4.44660201862032,
82.3391282405323));
#243378=CARTESIAN_POINT('Ctrl Pts',(-2.58673454289715,-7.91298223905764,
82.5510673949653));
#243379=CARTESIAN_POINT('Ctrl Pts',(3.06605107713806,-7.73765643749523,
82.7630065493983));
#243380=CARTESIAN_POINT('Ctrl Pts',(6.73838642580539,-4.03889050794708,
82.9749457038315));
#243381=CARTESIAN_POINT('Ctrl Pts',(7.86601130906456,-0.330583112720854,
83.1339000696561));
#243382=CARTESIAN_POINT('Ctrl Pts',(7.04994712015195,3.46650843499095,83.292854435481));
#243383=CARTESIAN_POINT('Ctrl Pts',(3.70681288487125,7.44684299163876,83.5047935899139));
#243384=CARTESIAN_POINT('Ctrl Pts',(-3.33648429528967,8.27951252852172,
83.7697175329551));
#243385=CARTESIAN_POINT('Ctrl Pts',(-8.77939149375497,1.65037161641574,
84.0876262646048));
#243386=CARTESIAN_POINT('Ctrl Pts',(-6.56715245437637,-5.10547863939855,
84.352550207646));
#243387=CARTESIAN_POINT('Ctrl Pts',(-2.02108893729002,-7.58348625226029,
84.564489362079));
#243388=CARTESIAN_POINT('Ctrl Pts',(3.18083270483377,-7.6934249080082,84.776428516512));
#243389=CARTESIAN_POINT('Ctrl Pts',(7.36106071721383,-3.88417062830127,
84.988367670945));
#243390=CARTESIAN_POINT('Ctrl Pts',(7.74547325076561,1.31382353469886,85.2003068253781));
#243391=CARTESIAN_POINT('Ctrl Pts',(6.19054403142093,4.86421460297602,85.3592611912026));
#243392=CARTESIAN_POINT('Ctrl Pts',(3.10131785134482,7.21805117131482,85.5182155570277));
#243393=CARTESIAN_POINT('Ctrl Pts',(-2.02680911194038,8.06771201328684,
85.7301547114604));
#243394=CARTESIAN_POINT('Ctrl Pts',(-7.91887496461385,4.11993622007326,
85.9950786545018));
#243395=CARTESIAN_POINT('Ctrl Pts',(-7.7426824191354,-4.45559316245293,
86.3129873861515));
#243396=CARTESIAN_POINT('Ctrl Pts',(-1.66871464606686,-8.1491591545619,
86.5779113291926));
#243397=CARTESIAN_POINT('Ctrl Pts',(3.39626131844057,-7.07527195855542,
86.7898504836257));
#243398=CARTESIAN_POINT('Ctrl Pts',(7.41949250519753,-3.77592564500659,
87.0017896380585));
#243399=CARTESIAN_POINT('Ctrl Pts',(8.11788347494936,1.83629089182822,87.2137287924919));
#243400=CARTESIAN_POINT('Ctrl Pts',(5.02960044991658,6.03503168780853,87.4256679469244));
#243401=CARTESIAN_POINT('Ctrl Pts',(1.53951351256144,7.72096608290747,87.5846223127496));
#243402=CARTESIAN_POINT('Ctrl Pts',(-2.33799904538993,7.50014637127467,
87.7435766785741));
#243403=CARTESIAN_POINT('Ctrl Pts',(-6.78621968890966,4.8107332746091,87.9555158330073));
#243404=CARTESIAN_POINT('Ctrl Pts',(-8.69495828245439,-2.01993951123245,
88.2204397760485));
#243405=CARTESIAN_POINT('Ctrl Pts',(-2.98435516720558,-8.41992076618659,
88.538348507698));
#243406=CARTESIAN_POINT('Ctrl Pts',(4.03181195051564,-7.2758433114009,88.8032724507394));
#243407=CARTESIAN_POINT('Ctrl Pts',(7.18115564050557,-3.16623876192109,
89.0152116051722));
#243408=CARTESIAN_POINT('Ctrl Pts',(8.0918794457162,1.95652000942912,89.2271507596054));
#243409=CARTESIAN_POINT('Ctrl Pts',(4.97274292511143,6.67411598288644,89.4390899140382));
#243410=CARTESIAN_POINT('Ctrl Pts',(-0.103813384613165,7.85542557343836,
89.6510290684714));
#243411=CARTESIAN_POINT('Ctrl Pts',(-3.85150363656501,6.86653761704497,
89.809983434296));
#243412=CARTESIAN_POINT('Ctrl Pts',(-6.653527147126,4.17720141114196,89.9689378001209));
#243413=CARTESIAN_POINT('Ctrl Pts',(-8.28374799016402,-0.758585223314343,
90.1808769545537));
#243414=CARTESIAN_POINT('Ctrl Pts',(-5.29169999189226,-7.18890578311246,
90.4458008975953));
#243415=CARTESIAN_POINT('Ctrl Pts',(3.20844012003686,-8.3371070203653,90.7637096292446));
#243416=CARTESIAN_POINT('Ctrl Pts',(7.79439716835156,-2.90530140921238,
91.0286335722861));
#243417=CARTESIAN_POINT('Ctrl Pts',(7.51433672947288,2.2646871189528,91.2405727267189));
#243418=CARTESIAN_POINT('Ctrl Pts',(4.87480224402012,6.74853958964436,91.452511881152));
#243419=CARTESIAN_POINT('Ctrl Pts',(-0.562609370393717,8.30394286159366,
91.664451035585));
#243420=CARTESIAN_POINT('Ctrl Pts',(-5.18732800355999,5.90000985949486,
91.876390190018));
#243421=CARTESIAN_POINT('Ctrl Pts',(-7.39124687725992,2.7116210480379,92.0353445558428));
#243422=CARTESIAN_POINT('Ctrl Pts',(-7.7709533206754,-1.15356820980508,
92.1942989216675));
#243423=CARTESIAN_POINT('Ctrl Pts',(-5.79958810797117,-5.96328014463993,
92.4062380761006));
#243424=CARTESIAN_POINT('Ctrl Pts',(0.65508079031038,-8.90243361788374,
92.6711620191416));
#243425=CARTESIAN_POINT('Ctrl Pts',(7.85905810680846,-4.24695739873778,
92.9890707507916));
#243426=CARTESIAN_POINT('Ctrl Pts',(7.81050686095784,2.8617103402176,93.2539946938323));
#243427=CARTESIAN_POINT('Ctrl Pts',(4.23565688330435,6.60706250898031,93.4659338482658));
#243428=CARTESIAN_POINT('Ctrl Pts',(-0.685410276942486,8.29678831015729,
93.6778730026984));
#243429=CARTESIAN_POINT('Ctrl Pts',(-5.82753636026967,5.94237463662472,
93.8898121571318));
#243430=CARTESIAN_POINT('Ctrl Pts',(-7.77748784638796,1.1086798266145,94.1017513115646));
#243431=CARTESIAN_POINT('Ctrl Pts',(-7.37829387622094,-2.74667045436609,
94.2607056773893));
#243432=CARTESIAN_POINT('Ctrl Pts',(-5.15317255072635,-5.92986068885513,
94.4196600432142));
#243433=CARTESIAN_POINT('Ctrl Pts',(-0.527782891107564,-8.30164908469586,
94.6315991976472));
#243434=CARTESIAN_POINT('Ctrl Pts',(6.28698871000212,-6.33689420165481,
94.8965231406882));
#243435=CARTESIAN_POINT('Ctrl Pts',(8.73212047092496,1.88454598090315,95.2144318723381));
#243436=CARTESIAN_POINT('Ctrl Pts',(4.07239770094658,7.25320484073779,95.4793558153791));
#243437=CARTESIAN_POINT('Ctrl Pts',(-1.07894498528856,7.77366978648934,
95.6912949698123));
#243438=CARTESIAN_POINT('Ctrl Pts',(-5.91617168425987,5.85708085258035,
95.903234124245));
#243439=CARTESIAN_POINT('Ctrl Pts',(-8.29138433472371,0.724528927072806,
96.1151732786783));
#243440=CARTESIAN_POINT('Ctrl Pts',(-6.62929984333307,-4.21555117936412,
96.3271124331113));
#243441=CARTESIAN_POINT('Ctrl Pts',(-3.81887065713178,-6.88474008317412,
96.4860667989358));
#243442=CARTESIAN_POINT('Ctrl Pts',(-0.0584542548102956,-7.85589067050221,
96.6450211647609));
#243443=CARTESIAN_POINT('Ctrl Pts',(4.99770784388671,-6.64972545393648,
96.8569603191938));
#243444=CARTESIAN_POINT('Ctrl Pts',(8.89697603459555,-0.725446484926773,
97.1218842622352));
#243445=CARTESIAN_POINT('Ctrl Pts',(5.40797875099621,7.11021851293324,97.4397929938846));
#243446=CARTESIAN_POINT('Ctrl Pts',(-1.62316089178656,8.15835474932004,
97.7047169369258));
#243447=CARTESIAN_POINT('Ctrl Pts',(-5.87493830813479,5.20376441686851,
97.916656091359));
#243448=CARTESIAN_POINT('Ctrl Pts',(-8.30325038727105,0.602093445890282,
98.1285952457918));
#243449=CARTESIAN_POINT('Ctrl Pts',(-6.76987362018956,-4.84157076979441,
98.340534400225));
#243450=CARTESIAN_POINT('Ctrl Pts',(-2.29465507190867,-7.51352422366614,
98.5524735546578));
#243451=CARTESIAN_POINT('Ctrl Pts',(1.57614101632218,-7.71357236340167,
98.7114279204827));
#243452=CARTESIAN_POINT('Ctrl Pts',(5.06436081758022,-6.00588749779308,
98.8703822863075));
#243453=CARTESIAN_POINT('Ctrl Pts',(8.12098712943168,-1.80152722687786,
99.0823214407404));
#243454=CARTESIAN_POINT('Ctrl Pts',(7.23051936458366,5.23469625489779,99.3472453837818));
#243455=CARTESIAN_POINT('Ctrl Pts',(-0.515576315975734,8.91827463892484,
99.6651541154311));
#243456=CARTESIAN_POINT('Ctrl Pts',(-6.53852668407044,5.14208832071911,
99.9300780584726));
#243457=CARTESIAN_POINT('Ctrl Pts',(-7.8470682701258,0.132603901305477,
100.142017212906));
#243458=CARTESIAN_POINT('Ctrl Pts',(-6.69926683314272,-4.94229778642039,
100.353956367339));
#243459=CARTESIAN_POINT('Ctrl Pts',(-1.99433757449542,-8.08050827554942,
100.565895521772));
#243460=CARTESIAN_POINT('Ctrl Pts',(3.14294466576488,-7.2000268740189,100.777834676205));
#243461=CARTESIAN_POINT('Ctrl Pts',(6.21356058683115,-4.83477858257698,
100.93678904203));
#243462=CARTESIAN_POINT('Ctrl Pts',(7.75292684617862,-1.26907858093652,
101.095743407854));
#243463=CARTESIAN_POINT('Ctrl Pts',(7.34081129664397,3.912597834258,101.307682562287));
#243464=CARTESIAN_POINT('Ctrl Pts',(2.08862216350653,8.67871606983256,101.572606505329));
#243465=CARTESIAN_POINT('Ctrl Pts',(-6.19131310945317,6.43964932691215,
101.890515236978));
#243466=CARTESIAN_POINT('Ctrl Pts',(-8.31106697441633,-0.345787858584055,
102.155439180019));
#243467=CARTESIAN_POINT('Ctrl Pts',(-6.04740567602245,-5.00229435562004,
102.367378334452));
#243468=CARTESIAN_POINT('Ctrl Pts',(-1.87519599256411,-8.11111111382233,
102.579317488886));
#243469=CARTESIAN_POINT('Ctrl Pts',(3.73980203610677,-7.43544733576923,
102.791256643318));
#243470=CARTESIAN_POINT('Ctrl Pts',(7.06984832096886,-3.42574559434119,
103.003195797751));
#243471=CARTESIAN_POINT('Ctrl Pts',(7.86435371782322,0.36791263871619,103.162150163576));
#243472=CARTESIAN_POINT('Ctrl Pts',(6.71495058411182,4.07772899782774,103.321104529401));
#243473=CARTESIAN_POINT('Ctrl Pts',(3.0321817214842,7.74608328857064,103.533043683834));
#243474=CARTESIAN_POINT('Ctrl Pts',(-4.05719768200587,7.95120130117371,
103.797967626875));
#243475=CARTESIAN_POINT('Ctrl Pts',(-8.89111699463826,0.865725164553574,
104.115876358525));
#243476=CARTESIAN_POINT('Ctrl Pts',(-6.08878786620442,-5.66745673267461,
104.380800301566));
#243477=CARTESIAN_POINT('Ctrl Pts',(-1.34098110058904,-7.73277659825497,
104.592739455999));
#243478=CARTESIAN_POINT('Ctrl Pts',(3.85021150553996,-7.38121635463353,
104.804678610432));
#243479=CARTESIAN_POINT('Ctrl Pts',(7.67635852451879,-3.21644464515006,
105.016617764865));
#243480=CARTESIAN_POINT('Ctrl Pts',(7.59854001320767,1.99516360891437,105.228556919298));
#243481=CARTESIAN_POINT('Ctrl Pts',(5.73504582378576,5.39376199955503,105.387511285123));
#243482=CARTESIAN_POINT('Ctrl Pts',(2.44934844243884,7.46452458863333,105.546465650948));
#243483=CARTESIAN_POINT('Ctrl Pts',(-2.73390432686058,7.85631589468939,
105.758404805381));
#243484=CARTESIAN_POINT('Ctrl Pts',(-8.25287417603857,3.40184111873792,
106.023328748422));
#243485=CARTESIAN_POINT('Ctrl Pts',(-7.31729310683559,-5.12432074147813,
106.341237480071));
#243486=CARTESIAN_POINT('Ctrl Pts',(-0.939855903853375,-8.26499088785765,
106.606161423113));
#243487=CARTESIAN_POINT('Ctrl Pts',(4.01000299171803,-6.7464020216015,106.818100577546));
#243488=CARTESIAN_POINT('Ctrl Pts',(7.72496617432305,-3.10344665120341,
107.030039731979));
#243489=CARTESIAN_POINT('Ctrl Pts',(7.92317625394474,2.54858282211741,107.241978886412));
#243490=CARTESIAN_POINT('Ctrl Pts',(4.47489739759916,6.45707220337623,107.453918040845));
#243491=CARTESIAN_POINT('Ctrl Pts',(0.849115659828287,7.82703147463972,
107.612872406669));
#243492=CARTESIAN_POINT('Ctrl Pts',(-2.99356398945314,7.26340207945554,
107.771826772494));
#243493=CARTESIAN_POINT('Ctrl Pts',(-7.18590470216688,4.19031095707143,
107.983765926927));
#243494=CARTESIAN_POINT('Ctrl Pts',(-8.48170237564872,-2.78265699890864,
108.248689869968));
#243495=CARTESIAN_POINT('Ctrl Pts',(-2.22631979187741,-8.65129710836367,
108.566598601618));
#243496=CARTESIAN_POINT('Ctrl Pts',(4.6608296790759,-6.88985269791904,108.831522544659));
#243497=CARTESIAN_POINT('Ctrl Pts',(7.4335284570037,-2.51728403434591,109.043461699092));
#243498=CARTESIAN_POINT('Ctrl Pts',(7.88661820280942,2.66603391471617,109.255400853525));
#243499=CARTESIAN_POINT('Ctrl Pts',(4.36161916279933,7.08860174018598,109.467340007958));
#243500=CARTESIAN_POINT('Ctrl Pts',(-0.799661217785712,7.81530742168362,
109.679279162391));
#243501=CARTESIAN_POINT('Ctrl Pts',(-4.44495267940158,6.49813933265885,
109.838233528216));
#243502=CARTESIAN_POINT('Ctrl Pts',(-6.99758204921451,3.5710335466501,109.997187894041));
#243503=CARTESIAN_POINT('Ctrl Pts',(-8.18390914785682,-1.48981991032531,
110.209127048474));
#243504=CARTESIAN_POINT('Ctrl Pts',(-4.63369311415609,-7.62963585543128,
110.474050991515));
#243505=CARTESIAN_POINT('Ctrl Pts',(3.93476227318016,-8.01991816207902,
110.791959723165));
#243506=CARTESIAN_POINT('Ctrl Pts',(8.02122856083205,-2.20301971649602,
111.056883666206));
#243507=CARTESIAN_POINT('Ctrl Pts',(7.28403450478502,2.92179834412948,111.268822820639));
#243508=CARTESIAN_POINT('Ctrl Pts',(4.25746750011996,7.15405157912097,111.480761975072));
#243509=CARTESIAN_POINT('Ctrl Pts',(-1.29640531265514,8.22139462728711,
111.692701129505));
#243510=CARTESIAN_POINT('Ctrl Pts',(-5.68985256060279,5.41701633717821,
111.904640283938));
#243511=CARTESIAN_POINT('Ctrl Pts',(-7.60249832617733,2.04583437971828,
112.063594649763));
#243512=CARTESIAN_POINT('Ctrl Pts',(-7.63812384302203,-1.83779740054446,
112.222549015588));
#243513=CARTESIAN_POINT('Ctrl Pts',(-5.24821421168279,-6.45385000552909,
112.43448817002));
#243514=CARTESIAN_POINT('Ctrl Pts',(1.44155931555731,-8.80933379446994,
112.699412113062));
#243515=CARTESIAN_POINT('Ctrl Pts',(8.20455111367348,-3.53366417419736,
113.017320844711));
#243516=CARTESIAN_POINT('Ctrl Pts',(7.52612254126613,3.54272253926597,113.282244787752));
#243517=CARTESIAN_POINT('Ctrl Pts',(3.63337729289704,6.95648141506293,113.494183942186));
#243518=CARTESIAN_POINT('Ctrl Pts',(-1.41808877366636,8.20338392014562,
113.706123096618));
#243519=CARTESIAN_POINT('Ctrl Pts',(-6.3312961871736,5.40247026299526,113.918062251052));
#243520=CARTESIAN_POINT('Ctrl Pts',(-7.84514434672058,0.414967875590241,
114.130001405485));
#243521=CARTESIAN_POINT('Ctrl Pts',(-7.10580705194119,-3.3898267285143,
114.28895577131));
#243522=CARTESIAN_POINT('Ctrl Pts',(-4.60730486081632,-6.36326779621038,
114.447910137134));
#243523=CARTESIAN_POINT('Ctrl Pts',(0.210101226185732,-8.31575551470409,
114.659849291567));
#243524=CARTESIAN_POINT('Ctrl Pts',(6.82390803799858,-5.75471408947469,
114.924773234609));
#243525=CARTESIAN_POINT('Ctrl Pts',(8.53071875050506,2.65109016683102,115.242681966258));
#243526=CARTESIAN_POINT('Ctrl Pts',(3.41349058714555,7.58561042420752,115.507605909299));
#243527=CARTESIAN_POINT('Ctrl Pts',(-1.76370864307955,7.64744375938669,
115.719545063732));
#243528=CARTESIAN_POINT('Ctrl Pts',(-6.41202275282373,5.30965608383186,
115.931484218165));
#243529=CARTESIAN_POINT('Ctrl Pts',(-8.32296951761604,-0.0132197239513161,
116.143423372598));
#243530=CARTESIAN_POINT('Ctrl Pts',(-6.22956833484834,-4.78654014086465,
116.355362527031));
#243531=CARTESIAN_POINT('Ctrl Pts',(-3.19361979615618,-7.19612477006659,
116.514316892856));
#243532=CARTESIAN_POINT('Ctrl Pts',(0.638073442077508,-7.83015308977449,
116.673271258681));
#243533=CARTESIAN_POINT('Ctrl Pts',(5.56742885387138,-6.18058801916594,
116.885210413114));
#243534=CARTESIAN_POINT('Ctrl Pts',(8.92625910332977,0.065981685964151,
117.150134356155));
#243535=CARTESIAN_POINT('Ctrl Pts',(4.75648858606023,7.5615645076641,117.468043087805));
#243536=CARTESIAN_POINT('Ctrl Pts',(-2.3398787664328,7.98237877169294,117.732967030846));
#243537=CARTESIAN_POINT('Ctrl Pts',(-6.31304572533293,4.66256559208677,
117.944906185279));
#243538=CARTESIAN_POINT('Ctrl Pts',(-8.32393694368881,-0.136225066689908,
118.156845339712));
#243539=CARTESIAN_POINT('Ctrl Pts',(-6.31410234165591,-5.42255548347479,
118.368784494145));
#243540=CARTESIAN_POINT('Ctrl Pts',(-1.61967155702648,-7.68733713362521,
118.580723648578));
#243541=CARTESIAN_POINT('Ctrl Pts',(2.25362118408763,-7.5435144771783,118.739678014403));
#243542=CARTESIAN_POINT('Ctrl Pts',(5.57675367937275,-5.53337632249897,
118.898632380228));
#243543=CARTESIAN_POINT('Ctrl Pts',(8.24870142701377,-1.0746427655538,119.11057153466));
#243544=CARTESIAN_POINT('Ctrl Pts',(6.73809089691147,5.85496252999263,119.375495477702));
#243545=CARTESIAN_POINT('Ctrl Pts',(-1.30400794239072,8.83747728478373,
119.693404209351));
#243546=CARTESIAN_POINT('Ctrl Pts',(-6.96855581333222,4.54231586009295,
119.958328152393));
#243547=CARTESIAN_POINT('Ctrl Pts',(-7.82793757869164,-0.56343366491826,
120.170267306826));
#243548=CARTESIAN_POINT('Ctrl Pts',(-6.23484562258053,-5.51662791693352,
120.382206461258));
#243549=CARTESIAN_POINT('Ctrl Pts',(-1.27028206080914,-8.22547140522983,
120.594145615692));
#243550=CARTESIAN_POINT('Ctrl Pts',(3.76874082838451,-6.89311836015612,
120.806084770125));
#243551=CARTESIAN_POINT('Ctrl Pts',(6.61763065495857,-4.26501859589367,
120.965039135949));
#243552=CARTESIAN_POINT('Ctrl Pts',(7.83489676687533,-0.576912280330592,
121.123993501774));
#243553=CARTESIAN_POINT('Ctrl Pts',(6.96513139029871,4.54784311750666,121.335932656207));
#243554=CARTESIAN_POINT('Ctrl Pts',(1.31117412703128,8.82968162343708,121.600856599248));
#243555=CARTESIAN_POINT('Ctrl Pts',(-6.73771656982127,5.86554489349819,
121.918765330898));
#243556=CARTESIAN_POINT('Ctrl Pts',(-8.24770842146538,-1.08106858749443,
122.183689273939));
#243557=CARTESIAN_POINT('Ctrl Pts',(-5.58023228461821,-5.5186114087115,
122.395628428372));
#243558=CARTESIAN_POINT('Ctrl Pts',(-1.14889694046579,-8.2453938251299,
122.607567582805));
#243559=CARTESIAN_POINT('Ctrl Pts',(4.3841153497589,-7.07471052074045,122.819506737238));
#243560=CARTESIAN_POINT('Ctrl Pts',(7.34566029529158,-2.78563511336829,
123.031445891671));
#243561=CARTESIAN_POINT('Ctrl Pts',(7.80079230035837,1.06351238612278,123.190400257496));
#243562=CARTESIAN_POINT('Ctrl Pts',(6.32709768517662,4.65685194192624,123.349354623321));
#243563=CARTESIAN_POINT('Ctrl Pts',(2.33368290703505,7.98435071843594,123.561293777754));
#243564=CARTESIAN_POINT('Ctrl Pts',(-4.74597506110222,7.56030263164477,
123.826217720795));
#243565=CARTESIAN_POINT('Ctrl Pts',(-8.9328565588375,0.0742642048415293,
124.144126452445));
#243566=CARTESIAN_POINT('Ctrl Pts',(-5.5624957204101,-6.1848237530909,124.409050395486));
#243567=CARTESIAN_POINT('Ctrl Pts',(-0.650317805169212,-7.82119882006179,
124.620989549919));
#243568=CARTESIAN_POINT('Ctrl Pts',(4.48928357889013,-7.0109069641245,124.832928704352));
#243569=CARTESIAN_POINT('Ctrl Pts',(7.9312322993893,-2.52340059550421,125.044867858785));
#243570=CARTESIAN_POINT('Ctrl Pts',(7.39179528733201,2.66079886290376,125.256807013218));
#243571=CARTESIAN_POINT('Ctrl Pts',(5.2344045194909,5.88085269625925,125.415761379043));
#243572=CARTESIAN_POINT('Ctrl Pts',(1.77809912245857,7.65224141265171,125.574715744867));
#243573=CARTESIAN_POINT('Ctrl Pts',(-3.41947976476801,7.58307921915096,
125.7866548993));
#243574=CARTESIAN_POINT('Ctrl Pts',(-8.52191134389828,2.65696861279858,
126.051578842342));
#243575=CARTESIAN_POINT('Ctrl Pts',(-6.83430612571826,-5.75271251262015,
126.369487573991));
#243576=CARTESIAN_POINT('Ctrl Pts',(-0.203599137767642,-8.31576520156013,
126.634411517033));
#243577=CARTESIAN_POINT('Ctrl Pts',(4.59218014777536,-6.36442815349768,
126.846350671465));
#243578=CARTESIAN_POINT('Ctrl Pts',(7.9696331985815,-2.40653904837824,127.058289825898));
#243579=CARTESIAN_POINT('Ctrl Pts',(7.66610218837164,3.24081372338967,127.270228980331));
#243580=CARTESIAN_POINT('Ctrl Pts',(3.88497043740519,6.82828623148893,127.482168134765));
#243581=CARTESIAN_POINT('Ctrl Pts',(0.152034040044715,7.87148682012707,
127.641122500589));
#243582=CARTESIAN_POINT('Ctrl Pts',(-3.62556525980116,6.96948431906636,
127.800076866414));
#243583=CARTESIAN_POINT('Ctrl Pts',(-7.52902626318211,3.5369048381165,128.012016020847));
#243584=CARTESIAN_POINT('Ctrl Pts',(-8.20168321673487,-3.52347095560442,
128.276939963888));
#243585=CARTESIAN_POINT('Ctrl Pts',(-1.45076006318804,-8.81457524285472,
128.594848695538));
#243586=CARTESIAN_POINT('Ctrl Pts',(5.25315994406895,-6.44962898920616,
128.859772638579));
#243587=CARTESIAN_POINT('Ctrl Pts',(7.62738866454065,-1.84851464443432,
129.071711793012));
#243588=CARTESIAN_POINT('Ctrl Pts',(7.61927788001662,3.354562281194,129.283650947445));
#243589=CARTESIAN_POINT('Ctrl Pts',(3.71616315598209,7.44728996013693,129.495590101878));
#243590=CARTESIAN_POINT('Ctrl Pts',(-1.48921456181703,7.71367150892115,
129.707529256311));
#243591=CARTESIAN_POINT('Ctrl Pts',(-5.00341352256318,6.07859130317289,
129.866483622136));
#243592=CARTESIAN_POINT('Ctrl Pts',(-7.28655587042038,2.93675648870235,
130.025437987961));
#243593=CARTESIAN_POINT('Ctrl Pts',(-8.01965111641687,-2.20932756215386,
130.237377142394));
#243594=CARTESIAN_POINT('Ctrl Pts',(-3.93921237678579,-8.01030967020114,
130.502301085435));
#243595=CARTESIAN_POINT('Ctrl Pts',(4.63011216219744,-7.63960096067819,
130.820209817085));
#243596=CARTESIAN_POINT('Ctrl Pts',(8.18492129553836,-1.48339707560108,
131.085133760126));
#243597=CARTESIAN_POINT('Ctrl Pts',(6.99639640437534,3.5559107948077,131.297072914559));
#243598=CARTESIAN_POINT('Ctrl Pts',(3.60662033617928,7.50325084671076,131.509012068992));
#243599=CARTESIAN_POINT('Ctrl Pts',(-2.01999667286217,8.07413213842702,
131.720951223425));
#243600=CARTESIAN_POINT('Ctrl Pts',(-6.14758975626172,4.89138307039339,
131.932890377858));
#243601=CARTESIAN_POINT('Ctrl Pts',(-7.75390713121773,1.36394403766155,
132.091844743683));
#243602=CARTESIAN_POINT('Ctrl Pts',(-7.44517129132054,-2.50756046804626,
132.250799109507));
#243603=CARTESIAN_POINT('Ctrl Pts',(-4.65552929510624,-6.89361874757744,
132.46273826394));
#243604=CARTESIAN_POINT('Ctrl Pts',(2.21669070319618,-8.64689177543339,
132.727662206981));
#243605=CARTESIAN_POINT('Ctrl Pts',(8.48546241963345,-2.79255592616151,
133.045570938631));
#243606=CARTESIAN_POINT('Ctrl Pts',(7.18249681313266,4.19584842527409,133.310494881672));
#243607=CARTESIAN_POINT('Ctrl Pts',(3.00249770744235,7.25114271918739,133.522434036105));
#243608=CARTESIAN_POINT('Ctrl Pts',(-2.13960469233783,8.04540715571849,
133.734373190538));
#243609=CARTESIAN_POINT('Ctrl Pts',(-6.78521991235738,4.82004042056871,
133.946312344972));
#243610=CARTESIAN_POINT('Ctrl Pts',(-7.85104779783532,-0.282010197456314,
134.158251499404));
#243611=CARTESIAN_POINT('Ctrl Pts',(-6.7773881513071,-4.00630074029798,
134.317205865229));
#243612=CARTESIAN_POINT('Ctrl Pts',(-4.02516939863429,-6.74658574968469,
134.476160231054));
#243613=CARTESIAN_POINT('Ctrl Pts',(0.946328029323823,-8.26440718691397,
134.688099385487));
#243614=CARTESIAN_POINT('Ctrl Pts',(7.3071206196513,-5.12723140280613,134.953023328528));
#243615=CARTESIAN_POINT('Ctrl Pts',(8.26215525051097,3.39675830243544,135.270932060178));
#243616=CARTESIAN_POINT('Ctrl Pts',(2.72773566717734,7.85831994690357,135.535856003219));
#243617=CARTESIAN_POINT('Ctrl Pts',(-2.43461772017353,7.46100312305416,
135.747795157652));
#243618=CARTESIAN_POINT('Ctrl Pts',(-6.85732892337842,4.72048345925153,
135.959734312085));
#243619=CARTESIAN_POINT('Ctrl Pts',(-8.28918936827278,-0.750959494552329,
136.171673466518));
#243620=CARTESIAN_POINT('Ctrl Pts',(-5.78061766663374,-5.31973450400921,
136.383612620951));
#243621=CARTESIAN_POINT('Ctrl Pts',(-2.54361228342804,-7.45111029376608,
136.542566986776));
#243622=CARTESIAN_POINT('Ctrl Pts',(1.33027488604519,-7.74233449640139,
136.701521352601));
#243623=CARTESIAN_POINT('Ctrl Pts',(6.09182165394096,-5.66376494878866,
136.913460507034));
#243624=CARTESIAN_POINT('Ctrl Pts',(8.88839239521778,0.858886091611861,
137.178384450075));
#243625=CARTESIAN_POINT('Ctrl Pts',(4.06211791741203,7.94990226154086,137.496293181724));
#243626=CARTESIAN_POINT('Ctrl Pts',(-3.02903681086098,7.74943205644144,
137.761217124766));
#243627=CARTESIAN_POINT('Ctrl Pts',(-6.71376182331183,4.07676873453249,
137.973156279199));
#243628=CARTESIAN_POINT('Ctrl Pts',(-7.86223692601581,0.380613488742994,
138.132110645024));
#243629=CARTESIAN_POINT('Ctrl Pts',(-7.07532856755501,-3.44087378386772,
138.291071725379));
#243630=CARTESIAN_POINT('Ctrl Pts',(-5.40397330502272,-5.41520356564519,
138.397048017128));
#243631=CARTESIAN_POINT('Ctrl Pts',(-4.38104157308948,-6.14454874685667,
138.450039520268));
#243632=CARTESIAN_POINT('Ctrl Pts',(-3.43252346058927,7.15950580248449,
8.01661173253155));
#243633=CARTESIAN_POINT('Ctrl Pts',(-4.62447820848135,6.58804200029991,
8.06960567665085));
#243634=CARTESIAN_POINT('Ctrl Pts',(-6.71314905678031,4.84304631147434,
8.17558440937839));
#243635=CARTESIAN_POINT('Ctrl Pts',(-8.21822261919714,1.02380062502623,
8.33454793071417));
#243636=CARTESIAN_POINT('Ctrl Pts',(-7.69455181722148,-3.01461142521582,
8.49350229653894));
#243637=CARTESIAN_POINT('Ctrl Pts',(-4.53770639023232,-7.48620479461186,
8.70544145097195));
#243638=CARTESIAN_POINT('Ctrl Pts',(2.77642922983875,-8.97322384561435,
8.97036539401322));
#243639=CARTESIAN_POINT('Ctrl Pts',(9.05827682897998,-2.49371283586009,
9.28827412566274));
#243640=CARTESIAN_POINT('Ctrl Pts',(7.3361722235595,4.77180027059814,9.553198068704));
#243641=CARTESIAN_POINT('Ctrl Pts',(2.77558310671645,7.78529932770683,9.76513722313702));
#243642=CARTESIAN_POINT('Ctrl Pts',(-1.29241060276714,8.18226981884739,
9.92409158896177));
#243643=CARTESIAN_POINT('Ctrl Pts',(-5.03220552019797,6.55694914733997,
10.0830459547865));
#243644=CARTESIAN_POINT('Ctrl Pts',(-8.45664565315574,2.2737476794153,10.2949851092195));
#243645=CARTESIAN_POINT('Ctrl Pts',(-7.95948972768491,-3.65595153354138,
10.5069242636526));
#243646=CARTESIAN_POINT('Ctrl Pts',(-3.8695326494975,-7.29446666417152,
10.7188634180856));
#243647=CARTESIAN_POINT('Ctrl Pts',(1.40980336588385,-8.6375761801721,10.9308025725186));
#243648=CARTESIAN_POINT('Ctrl Pts',(7.9513295390695,-5.01135990549878,11.1957265155599));
#243649=CARTESIAN_POINT('Ctrl Pts',(8.49909507792882,3.99642296432439,11.5136352472094));
#243650=CARTESIAN_POINT('Ctrl Pts',(2.47178529580885,8.39571392291258,11.7785591902507));
#243651=CARTESIAN_POINT('Ctrl Pts',(-2.95520506366149,7.71926692580053,
11.9904983446837));
#243652=CARTESIAN_POINT('Ctrl Pts',(-6.30234226822578,5.37533051525002,
12.1494527105084));
#243653=CARTESIAN_POINT('Ctrl Pts',(-8.08708929324349,1.70862130233454,
12.3084070763332));
#243654=CARTESIAN_POINT('Ctrl Pts',(-7.90270527679653,-3.77215503370355,
12.5203462307662));
#243655=CARTESIAN_POINT('Ctrl Pts',(-3.66916312400431,-7.9534470987693,
12.7322853851992));
#243656=CARTESIAN_POINT('Ctrl Pts',(1.80413946140186,-8.0577759930288,12.9442245396322));
#243657=CARTESIAN_POINT('Ctrl Pts',(6.68806173624078,-5.64488555735922,
13.1561636940653));
#243658=CARTESIAN_POINT('Ctrl Pts',(9.2993308505076,1.36385788062776,13.4210876371065));
#243659=CARTESIAN_POINT('Ctrl Pts',(3.85757222238032,8.56300679553197,13.738996368756));
#243660=CARTESIAN_POINT('Ctrl Pts',(-3.58207705629457,7.98538822446524,
14.0039203117973));
#243661=CARTESIAN_POINT('Ctrl Pts',(-7.26489761136101,3.94228506414547,
14.2158594662303));
#243662=CARTESIAN_POINT('Ctrl Pts',(-8.28332376272661,-0.015007944899706,
14.374813832055));
#243663=CARTESIAN_POINT('Ctrl Pts',(-7.25464302603574,-3.96113142541196,
14.5337681978798));
#243664=CARTESIAN_POINT('Ctrl Pts',(-3.55036594805974,-8.00479875340866,
14.7457073523128));
#243665=CARTESIAN_POINT('Ctrl Pts',(2.38486011653395,-8.42807925187489,
14.9576465067459));
#243666=CARTESIAN_POINT('Ctrl Pts',(6.61060311566235,-4.94798956303239,
15.1695856611789));
#243667=CARTESIAN_POINT('Ctrl Pts',(8.7516382340282,0.0610727336051463,
15.3815248156119));
#243668=CARTESIAN_POINT('Ctrl Pts',(6.17747958716616,7.08353082689385,15.6464487586532));
#243669=CARTESIAN_POINT('Ctrl Pts',(-2.63813481369485,9.01366704844546,
15.9643574903027));
#243670=CARTESIAN_POINT('Ctrl Pts',(-7.91417201601133,3.73678769388132,
16.2292814333439));
#243671=CARTESIAN_POINT('Ctrl Pts',(-8.08262379672163,-1.72960731590742,
16.441220587777));
#243672=CARTESIAN_POINT('Ctrl Pts',(-6.28282180227127,-5.39813189592084,
16.6001749536017));
#243673=CARTESIAN_POINT('Ctrl Pts',(-2.93516049174163,-7.72691662301371,
16.7591293194265));
#243674=CARTESIAN_POINT('Ctrl Pts',(2.50850133434887,-8.38983447446427,
16.9710684738595));
#243675=CARTESIAN_POINT('Ctrl Pts',(7.29257035236751,-4.85164871973294,
17.1830076282925));
#243676=CARTESIAN_POINT('Ctrl Pts',(8.23959675927419,0.540110652007771,
17.3949467827255));
#243677=CARTESIAN_POINT('Ctrl Pts',(6.60862923386289,5.73767560128377,17.6068859371585));
#243678=CARTESIAN_POINT('Ctrl Pts',(0.0863446456689102,9.39841516573596,
17.8718098801998));
#243679=CARTESIAN_POINT('Ctrl Pts',(-7.86578898824371,5.13179428160162,
18.1897186118493));
#243680=CARTESIAN_POINT('Ctrl Pts',(-8.44222016347028,-2.30794707028898,
18.4546425548906));
#243681=CARTESIAN_POINT('Ctrl Pts',(-5.01533468106842,-6.57014207940362,
18.6665817093236));
#243682=CARTESIAN_POINT('Ctrl Pts',(-1.262402125502,-8.18657551350801,18.8255360751483));
#243683=CARTESIAN_POINT('Ctrl Pts',(2.79514403616855,-7.77866167334332,
18.9844904409731));
#243684=CARTESIAN_POINT('Ctrl Pts',(7.36162574056733,-4.74219020170966,
19.1964295954061));
#243685=CARTESIAN_POINT('Ctrl Pts',(8.69501446585794,1.05678809721589,19.4083687498392));
#243686=CARTESIAN_POINT('Ctrl Pts',(5.90812406652453,5.76859985493989,19.6203079042721));
#243687=CARTESIAN_POINT('Ctrl Pts',(1.28909905516634,8.65639216314757,19.8322470587052));
#243688=CARTESIAN_POINT('Ctrl Pts',(-6.04629294128532,7.19583245313094,
20.0971710017464));
#243689=CARTESIAN_POINT('Ctrl Pts',(-9.31265225685634,-1.21674027595255,
20.415079733396));
#243690=CARTESIAN_POINT('Ctrl Pts',(-4.91240847420854,-7.24333790115327,
20.6800036764372));
#243691=CARTESIAN_POINT('Ctrl Pts',(0.462638446148335,-8.252655001563,20.8919428308703));
#243692=CARTESIAN_POINT('Ctrl Pts',(4.3648070904711,-7.04003812687221,21.050897196695));
#243693=CARTESIAN_POINT('Ctrl Pts',(7.18192725065368,-4.09149466302802,
21.2098515625198));
#243694=CARTESIAN_POINT('Ctrl Pts',(8.67629167883199,1.18484773587382,21.4217907169528));
#243695=CARTESIAN_POINT('Ctrl Pts',(5.91808996568352,6.45726635674664,21.6337298713858));
#243696=CARTESIAN_POINT('Ctrl Pts',(0.736836858659884,8.22433861873278,
21.8456690258188));
#243697=CARTESIAN_POINT('Ctrl Pts',(-4.65005287944806,7.41430440935427,
22.0576081802518));
#243698=CARTESIAN_POINT('Ctrl Pts',(-9.27270339692655,1.53448191191556,
22.3225321232931));
#243699=CARTESIAN_POINT('Ctrl Pts',(-6.28327150021554,-6.98043323947992,
22.6404408549426));
#243700=CARTESIAN_POINT('Ctrl Pts',(0.978614444226989,-8.69712680931522,
22.9053647979839));
#243701=CARTESIAN_POINT('Ctrl Pts',(5.71823855617235,-5.96842497828208,
23.1173039524169));
#243702=CARTESIAN_POINT('Ctrl Pts',(7.89401660440229,-2.50961742388398,
23.2762583182416));
#243703=CARTESIAN_POINT('Ctrl Pts',(8.11662634786984,1.56230097623142,23.4352126840664));
#243704=CARTESIAN_POINT('Ctrl Pts',(5.82058834768326,6.54237363196179,23.6471518384994));
#243705=CARTESIAN_POINT('Ctrl Pts',(0.296560714988169,8.75397791785091,
23.8590909929324));
#243706=CARTESIAN_POINT('Ctrl Pts',(-4.7886202994179,6.72694506443021,24.0710301473655));
#243707=CARTESIAN_POINT('Ctrl Pts',(-8.35409811785603,2.60843751956376,
24.2829693017985));
#243708=CARTESIAN_POINT('Ctrl Pts',(-8.04207175181927,-4.86443675711376,
24.5478932448397));
#243709=CARTESIAN_POINT('Ctrl Pts',(-0.233756872348344,-9.3888927292246,
24.8658019764893));
#243710=CARTESIAN_POINT('Ctrl Pts',(6.39925395972027,-5.97053177922736,
25.1307259195305));
#243711=CARTESIAN_POINT('Ctrl Pts',(8.22529502190908,-0.815396044407385,
25.3426650739636));
#243712=CARTESIAN_POINT('Ctrl Pts',(7.62886725191158,3.22708261709433,25.5016194397883));
#243713=CARTESIAN_POINT('Ctrl Pts',(5.14996639153414,6.46515690276247,25.6605738056131));
#243714=CARTESIAN_POINT('Ctrl Pts',(0.167145651189453,8.75522494197968,
25.872512960046));
#243715=CARTESIAN_POINT('Ctrl Pts',(-5.46751419208695,6.84297933675263,
26.0844521144791));
#243716=CARTESIAN_POINT('Ctrl Pts',(-8.01236657929817,1.99616033193848,
26.296391268912));
#243717=CARTESIAN_POINT('Ctrl Pts',(-8.04264049467031,-3.4512078363557,
26.5083304233452));
#243718=CARTESIAN_POINT('Ctrl Pts',(-2.94591666217063,-8.92520240918457,
26.7732543663863));
#243719=CARTESIAN_POINT('Ctrl Pts',(5.9281159510523,-7.28446224694289,27.091163098036));
#243720=CARTESIAN_POINT('Ctrl Pts',(8.74401116873232,-0.374125178040082,
27.3560870410771));
#243721=CARTESIAN_POINT('Ctrl Pts',(6.77875946227417,4.72956330534926,27.5680261955102));
#243722=CARTESIAN_POINT('Ctrl Pts',(3.6968064209343,7.41264460573822,27.7269805613349));
#243723=CARTESIAN_POINT('Ctrl Pts',(-0.292090009824848,8.26045344018289,
27.8859349271598));
#243724=CARTESIAN_POINT('Ctrl Pts',(-5.56663771537859,6.7597667118843,28.0978740815927));
#243725=CARTESIAN_POINT('Ctrl Pts',(-8.6035592897919,1.6428162377245,28.3098132360258));
#243726=CARTESIAN_POINT('Ctrl Pts',(-7.38486758130208,-3.69410409686745,
28.5217523904587));
#243727=CARTESIAN_POINT('Ctrl Pts',(-3.86538605350254,-7.85198652021393,
28.7336915448917));
#243728=CARTESIAN_POINT('Ctrl Pts',(3.56623050945739,-8.69595670290421,
28.998615487933));
#243729=CARTESIAN_POINT('Ctrl Pts',(9.24056490732958,-1.67866290531658,
29.3165242195825));
#243730=CARTESIAN_POINT('Ctrl Pts',(6.88584887949192,5.40210941915832,29.5814481626238));
#243731=CARTESIAN_POINT('Ctrl Pts',(2.07392747915858,8.00119826762644,29.7933873170568));
#243732=CARTESIAN_POINT('Ctrl Pts',(-2.01217114630803,8.03522526397403,
29.9523416828816));
#243733=CARTESIAN_POINT('Ctrl Pts',(-5.59374965575332,6.08525861406302,
30.1112960487063));
#243734=CARTESIAN_POINT('Ctrl Pts',(-8.62474629812029,1.51514116386394,
30.3232352031394));
#243735=CARTESIAN_POINT('Ctrl Pts',(-7.60419486026038,-4.34698725223412,
30.5351743575724));
#243736=CARTESIAN_POINT('Ctrl Pts',(-3.20773863081272,-7.60875069563005,
30.7471135120054));
#243737=CARTESIAN_POINT('Ctrl Pts',(2.16981505528078,-8.4786086289031,30.9590526664384));
#243738=CARTESIAN_POINT('Ctrl Pts',(8.36422390723629,-4.28688948481131,
31.2239766094797));
#243739=CARTESIAN_POINT('Ctrl Pts',(8.11141953413463,4.7340069811436,31.5418853411291));
#243740=CARTESIAN_POINT('Ctrl Pts',(1.71791628470502,8.58175183785365,31.8068092841705));
#243741=CARTESIAN_POINT('Ctrl Pts',(-3.62776396260994,7.42695614220699,
32.0187484386034));
#243742=CARTESIAN_POINT('Ctrl Pts',(-6.7539732169225,4.79557332859529,32.1777028044282));
#243743=CARTESIAN_POINT('Ctrl Pts',(-8.2067028210019,0.985107313457929,
32.336657170253));
#243744=CARTESIAN_POINT('Ctrl Pts',(-7.53726155025489,-4.45775613693974,
32.548596324686));
#243745=CARTESIAN_POINT('Ctrl Pts',(-2.9497780491645,-8.24735637065377,
32.760535479119));
#243746=CARTESIAN_POINT('Ctrl Pts',(2.51123044048412,-7.86615509296918,
32.9724746335521));
#243747=CARTESIAN_POINT('Ctrl Pts',(7.16206712986657,-5.02988032496978,
33.184413787985));
#243748=CARTESIAN_POINT('Ctrl Pts',(9.14184735475931,2.18272535323379,33.4493377310263));
#243749=CARTESIAN_POINT('Ctrl Pts',(3.08341782822716,8.87121657118275,33.7672464626758));
#243750=CARTESIAN_POINT('Ctrl Pts',(-4.27575448790704,7.636466756747,34.0321704057171));
#243751=CARTESIAN_POINT('Ctrl Pts',(-7.58572479844854,3.28285366546854,
34.2441095601501));
#243752=CARTESIAN_POINT('Ctrl Pts',(-8.24939268619883,-0.749131546345857,
34.4030639259749));
#243753=CARTESIAN_POINT('Ctrl Pts',(-6.87500053726231,-4.58854826975936,
34.5620182917996));
#243754=CARTESIAN_POINT('Ctrl Pts',(-2.82689676236,-8.28797660157973,34.7739574462327));
#243755=CARTESIAN_POINT('Ctrl Pts',(3.12248686837969,-8.18352939755775,
34.9858966006656));
#243756=CARTESIAN_POINT('Ctrl Pts',(7.02314485697244,-4.34259261154448,
35.1978357550987));
#243757=CARTESIAN_POINT('Ctrl Pts',(8.71178110528462,0.836523538126509,
35.4097749095317));
#243758=CARTESIAN_POINT('Ctrl Pts',(5.52532631230719,7.60318565917569,35.674698852573));
#243759=CARTESIAN_POINT('Ctrl Pts',(-3.42666763322906,8.74436377832241,
35.9926075842225));
#243760=CARTESIAN_POINT('Ctrl Pts',(-8.21422981758254,3.02061739909196,
36.2575315272637));
#243761=CARTESIAN_POINT('Ctrl Pts',(-7.89751112140635,-2.43919392298781,
36.4694706816968));
#243762=CARTESIAN_POINT('Ctrl Pts',(-5.77963728315236,-5.93375687402476,
36.6284250475215));
#243763=CARTESIAN_POINT('Ctrl Pts',(-2.23874234079903,-7.95666012487542,
36.7873794133463));
#243764=CARTESIAN_POINT('Ctrl Pts',(3.24225168818117,-8.13447634724329,
36.9993185677793));
#243765=CARTESIAN_POINT('Ctrl Pts',(7.69388900236769,-4.18618557437927,
37.2112577222123));
#243766=CARTESIAN_POINT('Ctrl Pts',(8.15929592082769,1.26829190182066,37.4231968766453));
#243767=CARTESIAN_POINT('Ctrl Pts',(6.07406736985527,6.30084178841948,37.6351360310783));
#243768=CARTESIAN_POINT('Ctrl Pts',(-0.747012665881907,9.36907866881162,
37.9000599741196));
#243769=CARTESIAN_POINT('Ctrl Pts',(-8.28968198146107,4.41442200095284,
38.2179687057692));
#243770=CARTESIAN_POINT('Ctrl Pts',(-8.20443175221731,-3.04712989400972,
38.4828926488103));
#243771=CARTESIAN_POINT('Ctrl Pts',(-4.41325889417126,-6.98881211935876,
38.6948318032434));
#243772=CARTESIAN_POINT('Ctrl Pts',(-0.531826161575748,-8.26624695364861,
38.8537861690681));
#243773=CARTESIAN_POINT('Ctrl Pts',(3.4735956609319,-7.50030271359922,39.012740534893));
#243774=CARTESIAN_POINT('Ctrl Pts',(7.75297088062306,-4.07103721152057,
39.2246796893259));
#243775=CARTESIAN_POINT('Ctrl Pts',(8.56712613159509,1.82330126123921,39.436618843759));
#243776=CARTESIAN_POINT('Ctrl Pts',(5.37357826151764,6.26955588053925,39.6485579981919));
#243777=CARTESIAN_POINT('Ctrl Pts',(0.516776372933795,8.73658078636091,
39.860497152625));
#243778=CARTESIAN_POINT('Ctrl Pts',(-6.66029056348775,6.63160558502124,
40.1254210956662));
#243779=CARTESIAN_POINT('Ctrl Pts',(-9.16815589831957,-2.03736751234651,
40.4433298273158));
#243780=CARTESIAN_POINT('Ctrl Pts',(-4.25106985578304,-7.65023568584735,
40.708253770357));
#243781=CARTESIAN_POINT('Ctrl Pts',(1.19228200701667,-8.17916942741876,
40.9201929247901));
#243782=CARTESIAN_POINT('Ctrl Pts',(4.97161392719165,-6.62546094425101,
41.0791472906148));
#243783=CARTESIAN_POINT('Ctrl Pts',(7.51630599972235,-3.43882999431583,
41.2381016564396));
#243784=CARTESIAN_POINT('Ctrl Pts',(8.5371266166875,1.94919742048378,41.4500408108726));
#243785=CARTESIAN_POINT('Ctrl Pts',(5.32246579161211,6.95639529792656,41.6619799653056));
#243786=CARTESIAN_POINT('Ctrl Pts',(0.00498228527689334,8.2572785740032,
41.8739191197386));
#243787=CARTESIAN_POINT('Ctrl Pts',(-5.28890972002855,6.97297179326152,
42.0858582741717));
#243788=CARTESIAN_POINT('Ctrl Pts',(-9.37221561133872,0.706567448972694,
42.3507822172128));
#243789=CARTESIAN_POINT('Ctrl Pts',(-5.63983979118354,-7.50987057718307,
42.6686909488625));
#243790=CARTESIAN_POINT('Ctrl Pts',(1.7456225031276,-8.5761589913162,42.9336148919036));
#243791=CARTESIAN_POINT('Ctrl Pts',(6.22473749031018,-5.43810556015643,
43.1455540463367));
#243792=CARTESIAN_POINT('Ctrl Pts',(8.08538493741333,-1.80006338185378,
43.3045084121615));
#243793=CARTESIAN_POINT('Ctrl Pts',(7.94620884873859,2.27555983078824,43.4634627779862));
#243794=CARTESIAN_POINT('Ctrl Pts',(5.21780452959536,7.03252567320655,43.6754019324192));
#243795=CARTESIAN_POINT('Ctrl Pts',(-0.48050501054649,8.74581000129407,
43.8873410868522));
#243796=CARTESIAN_POINT('Ctrl Pts',(-5.36600848936145,6.27603594348851,
44.0992802412853));
#243797=CARTESIAN_POINT('Ctrl Pts',(-8.5524145007925,1.85771576482195,44.3112193957182));
#243798=CARTESIAN_POINT('Ctrl Pts',(-7.57926675468472,-5.55809126289773,
44.5761433387595));
#243799=CARTESIAN_POINT('Ctrl Pts',(0.599336602836362,-9.3726594194368,
44.8940520704091));
#243800=CARTESIAN_POINT('Ctrl Pts',(6.90325934010349,-5.37984306936858,
45.1589760134503));
#243801=CARTESIAN_POINT('Ctrl Pts',(8.2651942141464,-0.083147514205629,
45.3709151678833));
#243802=CARTESIAN_POINT('Ctrl Pts',(7.31281347293094,3.89055739900608,45.5298695337081));
#243803=CARTESIAN_POINT('Ctrl Pts',(4.55666596934872,6.89617305866435,45.6888238995329));
#243804=CARTESIAN_POINT('Ctrl Pts',(-0.609521261097548,8.73558156539363,
45.9007630539659));
#243805=CARTESIAN_POINT('Ctrl Pts',(-6.05251500548945,6.3314405747998,46.1127022083988));
#243806=CARTESIAN_POINT('Ctrl Pts',(-8.15775945374294,1.2781373035503,46.324641362832));
#243807=CARTESIAN_POINT('Ctrl Pts',(-7.70509314365592,-4.15047482871782,
46.5365805172648));
#243808=CARTESIAN_POINT('Ctrl Pts',(-2.14324752551869,-9.15118315135956,
46.8015044603062));
#243809=CARTESIAN_POINT('Ctrl Pts',(6.55043428269769,-6.73036103521313,
47.1194131919557));
#243810=CARTESIAN_POINT('Ctrl Pts',(8.7427573135604,0.402362428594548,47.3843371349969));
#243811=CARTESIAN_POINT('Ctrl Pts',(6.3328808615103,5.31177643548693,47.59627628943));
#243812=CARTESIAN_POINT('Ctrl Pts',(3.02524577395481,7.71113258685195,47.7552306552547));
#243813=CARTESIAN_POINT('Ctrl Pts',(-1.023096007437,8.20205353377038,47.9141850210795));
#243814=CARTESIAN_POINT('Ctrl Pts',(-6.14387295289784,6.23976975472853,
48.1261241755125));
#243815=CARTESIAN_POINT('Ctrl Pts',(-8.71530715530853,0.873784202491687,
48.3380633299456));
#243816=CARTESIAN_POINT('Ctrl Pts',(-7.02838021728527,-4.33411418782803,
48.5500024843785));
#243817=CARTESIAN_POINT('Ctrl Pts',(-3.15422136962083,-8.16368723112667,
48.7619416388116));
#243818=CARTESIAN_POINT('Ctrl Pts',(4.32295071883371,-8.34564318119966,
49.0268655818528));
#243819=CARTESIAN_POINT('Ctrl Pts',(9.35298292282078,-0.853029543263231,
49.3447743135024));
#243820=CARTESIAN_POINT('Ctrl Pts',(6.37993847010265,5.99116733913045,49.6096982565436));
#243821=CARTESIAN_POINT('Ctrl Pts',(1.35658827104663,8.15352789714588,49.8216374109767));
#243822=CARTESIAN_POINT('Ctrl Pts',(-2.71644454735151,7.82525442308462,
49.9805917768014));
#243823=CARTESIAN_POINT('Ctrl Pts',(-6.11109395564759,5.56551329856609,
50.1395461426262));
#243824=CARTESIAN_POINT('Ctrl Pts',(-8.72509444732845,0.744733736695816,
50.3514852970592));
#243825=CARTESIAN_POINT('Ctrl Pts',(-7.18897675376466,-5.00386759194602,
50.5634244514922));
#243826=CARTESIAN_POINT('Ctrl Pts',(-2.52072118608171,-7.86311890879807,
50.7753636059252));
#243827=CARTESIAN_POINT('Ctrl Pts',(2.91276677713683,-8.25292017156604,
50.9873027603582));
#243828=CARTESIAN_POINT('Ctrl Pts',(8.7112680552635,-3.52866432162581,51.2522267033995));
#243829=CARTESIAN_POINT('Ctrl Pts',(7.65990209328867,5.43432138150552,51.570135435049));
#243830=CARTESIAN_POINT('Ctrl Pts',(0.950521554408865,8.70024193585228,
51.8350593780902));
#243831=CARTESIAN_POINT('Ctrl Pts',(-4.27176562005544,7.07618310913376,
52.0469985325234));
#243832=CARTESIAN_POINT('Ctrl Pts',(-7.15244145934331,4.17806880454457,
52.2059528983479));
#243833=CARTESIAN_POINT('Ctrl Pts',(-8.26171734586479,0.253838744689786,
52.3649072641729));
#243834=CARTESIAN_POINT('Ctrl Pts',(-7.11248900476896,-5.10826796579968,
52.5768464186057));
#243835=CARTESIAN_POINT('Ctrl Pts',(-2.20717380217117,-8.47634717616648,
52.7887855730389));
#243836=CARTESIAN_POINT('Ctrl Pts',(3.19855434677107,-7.61261613130539,
53.0007247274718));
#243837=CARTESIAN_POINT('Ctrl Pts',(7.5796967531928,-4.37528270925114,53.2126638819049));
#243838=CARTESIAN_POINT('Ctrl Pts',(8.91240428482381,2.98441164875481,53.4775878249461));
#243839=CARTESIAN_POINT('Ctrl Pts',(2.28499249646148,9.10959704088886,53.7954965565956));
#243840=CARTESIAN_POINT('Ctrl Pts',(-4.93577556162372,7.22743526937714,
54.0604204996369));
#243841=CARTESIAN_POINT('Ctrl Pts',(-7.84684136797584,2.59758146214908,
54.2723596540699));
#243842=CARTESIAN_POINT('Ctrl Pts',(-8.15052697237911,-1.47735839841323,
54.4313140198947));
#243843=CARTESIAN_POINT('Ctrl Pts',(-6.44124186029901,-5.17984661050887,
54.5902683857195));
#243844=CARTESIAN_POINT('Ctrl Pts',(-2.08117581556965,-8.5059160986964,
54.8022075401524));
#243845=CARTESIAN_POINT('Ctrl Pts',(3.83553513755162,-7.87456334360853,
55.0141466945856));
#243846=CARTESIAN_POINT('Ctrl Pts',(7.38040430103625,-3.70301318187023,
55.2260858490184));
#243847=CARTESIAN_POINT('Ctrl Pts',(8.6033496725185,1.60538969369099,55.4380250034515));
#243848=CARTESIAN_POINT('Ctrl Pts',(4.82968073628349,8.06299243525258,55.7029489464928));
#243849=CARTESIAN_POINT('Ctrl Pts',(-4.18822762758455,8.40622973132391,
56.0208576781423));
#243850=CARTESIAN_POINT('Ctrl Pts',(-8.44962976254117,2.2806704811826,56.2857816211834));
#243851=CARTESIAN_POINT('Ctrl Pts',(-7.65023362318843,-3.12958054974059,
56.4977207756167));
#243852=CARTESIAN_POINT('Ctrl Pts',(-5.23095866816667,-6.42267461240047,
56.6566751414413));
#243853=CARTESIAN_POINT('Ctrl Pts',(-1.52470205308439,-8.12377321572858,
56.8156295072661));
#243854=CARTESIAN_POINT('Ctrl Pts',(3.95048083680223,-7.81508813843023,
57.027568661699));
#243855=CARTESIAN_POINT('Ctrl Pts',(8.0346456297457,-3.48777110033108,57.2395078161322));
#243856=CARTESIAN_POINT('Ctrl Pts',(8.01476963488675,1.98648986193146,57.4514469705651));
#243857=CARTESIAN_POINT('Ctrl Pts',(5.49169381979988,6.81441124718818,57.6633861249983));
#243858=CARTESIAN_POINT('Ctrl Pts',(-1.57448990846434,9.2659939862657,57.9283100680393));
#243859=CARTESIAN_POINT('Ctrl Pts',(-8.64832320050468,3.66230184117443,
58.246218799689));
#243860=CARTESIAN_POINT('Ctrl Pts',(-7.90206260926476,-3.76232740295407,
58.5111427427301));
#243861=CARTESIAN_POINT('Ctrl Pts',(-3.77644438347535,-7.35247011045913,
58.7230818971633));
#243862=CARTESIAN_POINT('Ctrl Pts',(0.202936042627704,-8.28085108714341,
58.8820362629879));
#243863=CARTESIAN_POINT('Ctrl Pts',(4.12470506917314,-7.16290553501901,
59.0409906288128));
#243864=CARTESIAN_POINT('Ctrl Pts',(8.08328893831205,-3.36783927661889,
59.2529297832456));
#243865=CARTESIAN_POINT('Ctrl Pts',(8.37180213684398,2.5754624100209,59.4648689376788));
#243866=CARTESIAN_POINT('Ctrl Pts',(4.79673463181595,6.72116144306895,59.6768080921117));
#243867=CARTESIAN_POINT('Ctrl Pts',(-0.259614085995455,8.747999896124,59.8887472465449));
#243868=CARTESIAN_POINT('Ctrl Pts',(-7.22186207613001,6.01517839957581,
60.1536711895859));
#243869=CARTESIAN_POINT('Ctrl Pts',(-8.95149290665923,-2.84195772281832,
60.4715799212356));
#243870=CARTESIAN_POINT('Ctrl Pts',(-3.55626917562253,-7.99691506258984,
60.7365038642768));
#243871=CARTESIAN_POINT('Ctrl Pts',(1.91254058587403,-8.04130197257024,
60.9484430187099));
#243872=CARTESIAN_POINT('Ctrl Pts',(5.53928697928919,-6.15873181149487,
61.1073973845346));
#243873=CARTESIAN_POINT('Ctrl Pts',(7.79152056097164,-2.75909676510714,
61.2663517503593));
#243874=CARTESIAN_POINT('Ctrl Pts',(8.33076203358052,2.6982041051833,61.4782909047926));
#243875=CARTESIAN_POINT('Ctrl Pts',(4.68494612183171,7.40076735747243,61.6902300592252));
#243876=CARTESIAN_POINT('Ctrl Pts',(-0.726911505889756,8.22522181673321,
61.9021692136586));
#243877=CARTESIAN_POINT('Ctrl Pts',(-5.88613519966566,6.47675181456649,
62.1141083680913));
#243878=CARTESIAN_POINT('Ctrl Pts',(-9.39795494785929,-0.126908720646365,
62.3790323111328));
#243879=CARTESIAN_POINT('Ctrl Pts',(-4.95201439452223,-7.98019438314016,
62.6969410427822));
#243880=CARTESIAN_POINT('Ctrl Pts',(2.49888999084336,-8.38768441117226,
62.9618649858234));
#243881=CARTESIAN_POINT('Ctrl Pts',(6.68223874686327,-4.86498039426644,
63.1738041402566));
#243882=CARTESIAN_POINT('Ctrl Pts',(8.21310960915687,-1.07634024026636,
63.3327585060813));
#243883=CARTESIAN_POINT('Ctrl Pts',(7.71324320523999,2.97090674173524,63.491712871906));
#243884=CARTESIAN_POINT('Ctrl Pts',(4.57394905114565,7.46732157677019,63.703652026339));
#243885=CARTESIAN_POINT('Ctrl Pts',(-1.25378846741183,8.66879992403101,
63.9155911807722));
#243886=CARTESIAN_POINT('Ctrl Pts',(-5.9011584396543,5.77572535201913,64.127530335205));
#243887=CARTESIAN_POINT('Ctrl Pts',(-8.68341102503059,1.09237110297249,
64.3394694896381));
#243888=CARTESIAN_POINT('Ctrl Pts',(-7.05680197762321,-6.20799556008093,
64.6043934326793));
#243889=CARTESIAN_POINT('Ctrl Pts',(1.42771243303241,-9.28264973834655,
64.9223021643289));
#243890=CARTESIAN_POINT('Ctrl Pts',(7.35292609561125,-4.74680722172566,
65.1872261073701));
#243891=CARTESIAN_POINT('Ctrl Pts',(8.24003438631967,0.649755507064886,
65.3991652618031));
#243892=CARTESIAN_POINT('Ctrl Pts',(6.93919728632182,4.52340787308913,65.5581196276279));
#243893=CARTESIAN_POINT('Ctrl Pts',(3.92749800249095,7.27290636896342,65.7170739934526));
#243894=CARTESIAN_POINT('Ctrl Pts',(-1.38139036042829,8.64717654067271,
65.9290131478857));
#243895=CARTESIAN_POINT('Ctrl Pts',(-6.58987378107479,5.77006422781667,
66.1409523023186));
#243896=CARTESIAN_POINT('Ctrl Pts',(-8.23893897492785,0.550053487929615,
66.3528914567518));
#243897=CARTESIAN_POINT('Ctrl Pts',(-7.30689557719576,-4.81707158756267,
66.5648306111847));
#243898=CARTESIAN_POINT('Ctrl Pts',(-1.32370793435634,-9.30513086042084,
66.829754554226));
#243899=CARTESIAN_POINT('Ctrl Pts',(7.12119123259477,-6.12328215812712,
67.1476632858755));
#243900=CARTESIAN_POINT('Ctrl Pts',(8.67268532647238,1.17568286167335,67.4125872289168));
#243901=CARTESIAN_POINT('Ctrl Pts',(5.83715333896189,5.85217821046453,67.6245263833497));
#243902=CARTESIAN_POINT('Ctrl Pts',(2.32987207101727,7.94892281369866,67.7834807491746));
#243903=CARTESIAN_POINT('Ctrl Pts',(-1.74604875975871,8.07909161515217,
67.9424351149993));
#243904=CARTESIAN_POINT('Ctrl Pts',(-6.67274703708215,5.67065679553783,
68.1543742694324));
#243905=CARTESIAN_POINT('Ctrl Pts',(-8.75845295486286,0.0978742208561194,
68.3663134238653));
#243906=CARTESIAN_POINT('Ctrl Pts',(-6.61656935417688,-4.94000853551062,
68.5782525782984));
#243907=CARTESIAN_POINT('Ctrl Pts',(-2.41822838793727,-8.41112793482519,
68.7901917327313));
#243908=CARTESIAN_POINT('Ctrl Pts',(5.0456430210861,-7.92963737654938,69.0551156757727));
#243909=CARTESIAN_POINT('Ctrl Pts',(9.39177951848075,-0.0206816296521539,
69.3730244074221));
#243910=CARTESIAN_POINT('Ctrl Pts',(5.82380861030514,6.53306615571522,69.6379483504635));
#243911=CARTESIAN_POINT('Ctrl Pts',(0.628570915073197,8.24167742695639,
69.8498875048964));
#243912=CARTESIAN_POINT('Ctrl Pts',(-3.39933595810127,7.55368764365964,
70.0088418707212));
#243913=CARTESIAN_POINT('Ctrl Pts',(-6.58033445871659,5.0019591291155,70.1677962365461));
#243914=CARTESIAN_POINT('Ctrl Pts',(-8.75676499863564,-0.031535311683235,
70.3797353909789));
#243915=CARTESIAN_POINT('Ctrl Pts',(-6.7171681344739,-5.62136124066343,
70.5916745454121));
#243916=CARTESIAN_POINT('Ctrl Pts',(-1.813865389671,-8.05559187373631,70.8036136998449));
#243917=CARTESIAN_POINT('Ctrl Pts',(3.63279868789117,-7.96227197870748,
71.0155528542781));
#243918=CARTESIAN_POINT('Ctrl Pts',(8.98972517918711,-2.74265778759378,
71.2804767973192));
#243919=CARTESIAN_POINT('Ctrl Pts',(7.14811970341057,6.09184979863643,71.5983855289689));
#243920=CARTESIAN_POINT('Ctrl Pts',(0.175594806760906,8.75026553285845,
71.86330947201));
#243921=CARTESIAN_POINT('Ctrl Pts',(-4.88207302152628,6.66968678879071,
72.0752486264431));
#243922=CARTESIAN_POINT('Ctrl Pts',(-7.49476079781095,3.52772811010838,
72.2342029922678));
#243923=CARTESIAN_POINT('Ctrl Pts',(-8.25141848381123,-0.479523465063083,
72.3931573580926));
#243924=CARTESIAN_POINT('Ctrl Pts',(-6.6323737200743,-5.71835230350754,
72.6050965125256));
#243925=CARTESIAN_POINT('Ctrl Pts',(-1.4459633342905,-8.63903494416697,
72.8170356669587));
#243926=CARTESIAN_POINT('Ctrl Pts',(3.85926018638893,-7.29866627444097,
73.0289748213916));
#243927=CARTESIAN_POINT('Ctrl Pts',(7.94102894798011,-3.68738514981999,
73.2409139758247));
#243928=CARTESIAN_POINT('Ctrl Pts',(8.60568699227863,3.76499989227933,73.5058379188659));
#243929=CARTESIAN_POINT('Ctrl Pts',(1.48089681516255,9.27222962841085,73.8237466505155));
#243930=CARTESIAN_POINT('Ctrl Pts',(-6.98781478096711,6.26620336683783,
74.141655382165));
#243931=CARTESIAN_POINT('Ctrl Pts',(-9.05505641808052,-2.48502531424726,
74.4595641138145));
#243932=CARTESIAN_POINT('Ctrl Pts',(-2.81052426251138,-8.95521152276751,
74.7774728454639));
#243933=CARTESIAN_POINT('Ctrl Pts',(6.00625529959161,-7.21749228854913,
75.0953815771136));
#243934=CARTESIAN_POINT('Ctrl Pts',(9.32196859427813,1.15497806266144,75.4132903087629));
#243935=CARTESIAN_POINT('Ctrl Pts',(4.94651276262872,7.22417894884408,75.6782142518044));
#243936=CARTESIAN_POINT('Ctrl Pts',(-0.40678230636204,8.24614738694012,
75.8901534062373));
#243937=CARTESIAN_POINT('Ctrl Pts',(-5.65301526785667,6.69082604108267,
76.1020925606704));
#243938=CARTESIAN_POINT('Ctrl Pts',(-8.62212040196883,1.5319836825875,76.3140317151032));
#243939=CARTESIAN_POINT('Ctrl Pts',(-7.34032809091788,-3.79939906645903,
76.5259708695365));
#243940=CARTESIAN_POINT('Ctrl Pts',(-4.64425086315509,-6.85909899005226,
76.6849252353611));
#243941=CARTESIAN_POINT('Ctrl Pts',(-0.793804143464836,-8.2273467065575,
76.8438796011859));
#243942=CARTESIAN_POINT('Ctrl Pts',(4.61737414584813,-7.43490661871054,
77.0558187556188));
#243943=CARTESIAN_POINT('Ctrl Pts',(9.25626449155225,-1.58991098048353,
77.3207426986603));
#243944=CARTESIAN_POINT('Ctrl Pts',(6.33052329467649,6.94707171063594,77.6386514303096));
#243945=CARTESIAN_POINT('Ctrl Pts',(-0.940243880013648,8.7012035268548,
77.903575373351));
#243946=CARTESIAN_POINT('Ctrl Pts',(-5.67157647317062,6.00132388702944,
78.1155145277839));
#243947=CARTESIAN_POINT('Ctrl Pts',(-8.64552997002301,1.40529764899067,
78.327453682217));
#243948=CARTESIAN_POINT('Ctrl Pts',(-7.54622056146987,-4.44257616196536,
78.53939283665));
#243949=CARTESIAN_POINT('Ctrl Pts',(-3.10542854980952,-7.66007246962735,
78.751331991083));
#243950=CARTESIAN_POINT('Ctrl Pts',(0.932450631858945,-8.23068756503138,
78.9102863569078));
#243951=CARTESIAN_POINT('Ctrl Pts',(4.74730033149722,-6.76634966343337,
79.0692407227326));
#243952=CARTESIAN_POINT('Ctrl Pts',(8.34267086175441,-2.64528694414241,
79.2811798771655));
#243953=CARTESIAN_POINT('Ctrl Pts',(8.0656297691254,4.81160749448224,79.5461038202069));
#243954=CARTESIAN_POINT('Ctrl Pts',(0.291347901712305,9.39429501452725,
79.8640125518562));
#243955=CARTESIAN_POINT('Ctrl Pts',(-6.37275616353708,5.99857320971597,
80.1289364948976));
#243956=CARTESIAN_POINT('Ctrl Pts',(-8.21124180344807,0.87073669662942,
80.3408756493307));
#243957=CARTESIAN_POINT('Ctrl Pts',(-7.48161788051808,-4.55471968572886,
80.5528148037635));
#243958=CARTESIAN_POINT('Ctrl Pts',(-2.84357433903173,-8.28226940470237,
80.7647539581967));
#243959=CARTESIAN_POINT('Ctrl Pts',(2.62232728429337,-7.83861003058117,
80.9766931126296));
#243960=CARTESIAN_POINT('Ctrl Pts',(6.06085450803398,-5.64621292530574,
81.1356474784545));
#243961=CARTESIAN_POINT('Ctrl Pts',(8.0066023109931,-2.05296574330638,81.2946018442791));
#243962=CARTESIAN_POINT('Ctrl Pts',(8.05792312660012,3.41578334339948,81.5065409987122));
#243963=CARTESIAN_POINT('Ctrl Pts',(2.99816836424723,8.90038962174408,81.7714649417535));
#243964=CARTESIAN_POINT('Ctrl Pts',(-5.88787901169365,7.32601827520863,
82.089373673403));
#243965=CARTESIAN_POINT('Ctrl Pts',(-8.74211725417119,0.412659145140834,
82.3542976164443));
#243966=CARTESIAN_POINT('Ctrl Pts',(-6.80407226898225,-4.67838378402576,
82.5662367708773));
#243967=CARTESIAN_POINT('Ctrl Pts',(-2.72156961391875,-8.32545112773004,
82.7781759253103));
#243968=CARTESIAN_POINT('Ctrl Pts',(3.22587080656452,-8.14098636485779,
82.9901150797432));
#243969=CARTESIAN_POINT('Ctrl Pts',(7.08962881161275,-4.24942006923645,
83.2020542341765));
#243970=CARTESIAN_POINT('Ctrl Pts',(8.27603181017464,-0.347814953384133,
83.3610086000008));
#243971=CARTESIAN_POINT('Ctrl Pts',(7.41742979179161,3.64720224151801,83.519962965826));
#243972=CARTESIAN_POINT('Ctrl Pts',(3.90003270325899,7.83501409579196,83.7319021202586));
#243973=CARTESIAN_POINT('Ctrl Pts',(-3.51040051647884,8.71108702574855,
83.9968260633002));
#243974=CARTESIAN_POINT('Ctrl Pts',(-9.23702247828752,1.7363982149788,84.3147347949496));
#243975=CARTESIAN_POINT('Ctrl Pts',(-6.90946916794436,-5.37160473913135,
84.5796587379909));
#243976=CARTESIAN_POINT('Ctrl Pts',(-2.12643939590146,-7.97877996735202,
84.7915978924239));
#243977=CARTESIAN_POINT('Ctrl Pts',(3.34663549462676,-8.09444924068338,
85.0035370468568));
#243978=CARTESIAN_POINT('Ctrl Pts',(7.74476036947559,-4.08663532417261,
85.21547620129));
#243979=CARTESIAN_POINT('Ctrl Pts',(8.14921063415244,1.38230736505511,85.4274153557229));
#243980=CARTESIAN_POINT('Ctrl Pts',(6.51322980775338,5.11776467183024,85.5863697215476));
#243981=CARTESIAN_POINT('Ctrl Pts',(3.26297588227619,7.59429636624497,85.7453240873726));
#243982=CARTESIAN_POINT('Ctrl Pts',(-2.13245773804618,8.48824628313803,
85.9572632418053));
#243983=CARTESIAN_POINT('Ctrl Pts',(-8.33165101509813,4.33469033713718,
86.2221871848468));
#243984=CARTESIAN_POINT('Ctrl Pts',(-8.14627432876946,-4.68784359655912,
86.5400959164963));
#243985=CARTESIAN_POINT('Ctrl Pts',(-1.7556973859211,-8.57393890492018,
86.8050198595376));
#243986=CARTESIAN_POINT('Ctrl Pts',(3.57329345238697,-7.44407470240509,
87.0169590139705));
#243987=CARTESIAN_POINT('Ctrl Pts',(7.8062379490363,-3.97274800697461,87.2288981684036));
#243988=CARTESIAN_POINT('Ctrl Pts',(8.54103296197277,1.93200864280407,87.4408373228366));
#243989=CARTESIAN_POINT('Ctrl Pts',(5.29177135405442,6.34961129106956,87.6527764772695));
#243990=CARTESIAN_POINT('Ctrl Pts',(1.61976156676342,8.12342601564617,87.8117308430944));
#243991=CARTESIAN_POINT('Ctrl Pts',(-2.45986863119688,7.89109594568021,
87.9706852089191));
#243992=CARTESIAN_POINT('Ctrl Pts',(-7.13995541190373,5.061495597527,88.1826243633521));
#243993=CARTESIAN_POINT('Ctrl Pts',(-9.14818813581019,-2.12523005533024,
88.4475483063934));
#243994=CARTESIAN_POINT('Ctrl Pts',(-3.13991644891066,-8.858814126012,88.7654570380429));
#243995=CARTESIAN_POINT('Ctrl Pts',(4.2419725378046,-7.65510095588199,89.0303809810843));
#243996=CARTESIAN_POINT('Ctrl Pts',(7.55547763402694,-3.33128083379027,
89.2423201355171));
#243997=CARTESIAN_POINT('Ctrl Pts',(8.51367345730509,2.05850477441118,89.4542592899503));
#243998=CARTESIAN_POINT('Ctrl Pts',(5.23195009707337,7.02200823376817,89.6661984443832));
#243999=CARTESIAN_POINT('Ctrl Pts',(-0.109224718809311,8.26489428680549,
89.8781375988163));
#244000=CARTESIAN_POINT('Ctrl Pts',(-4.05226554613339,7.22445995964139,
90.0370919646409));
#244001=CARTESIAN_POINT('Ctrl Pts',(-7.00034619274214,4.39494051022739,
90.1960463304658));
#244002=CARTESIAN_POINT('Ctrl Pts',(-8.71554326333916,-0.798126927639463,
90.4079854848986));
#244003=CARTESIAN_POINT('Ctrl Pts',(-5.56753298998327,-7.56363175741028,
90.6729094279402));
#244004=CARTESIAN_POINT('Ctrl Pts',(3.37568196270829,-8.77168366461165,
90.9908181595894));
#244005=CARTESIAN_POINT('Ctrl Pts',(8.20068473993648,-3.05674196693257,
91.2557421026311));
#244006=CARTESIAN_POINT('Ctrl Pts',(7.90602598470913,2.38273527714745,91.4676812570636));
#244007=CARTESIAN_POINT('Ctrl Pts',(5.12890419993768,7.10031121513393,91.6796204114972));
#244008=CARTESIAN_POINT('Ctrl Pts',(-0.591935717244415,8.73679080441012,
91.8915595659297));
#244009=CARTESIAN_POINT('Ctrl Pts',(-5.45772054990596,6.20755136993672,
92.103498720363));
#244010=CARTESIAN_POINT('Ctrl Pts',(-7.77652000100319,2.85296590215134,
92.2624530861876));
#244011=CARTESIAN_POINT('Ctrl Pts',(-8.17601886780652,-1.21369863637932,
92.4214074520124));
#244012=CARTESIAN_POINT('Ctrl Pts',(-6.10189507510199,-6.27411965619128,
92.6333466064455));
#244013=CARTESIAN_POINT('Ctrl Pts',(0.689227264725502,-9.36647824605471,
92.8982705494865));
#244014=CARTESIAN_POINT('Ctrl Pts',(8.26871616813045,-4.46833257001599,
93.2161792811364));
#244015=CARTESIAN_POINT('Ctrl Pts',(8.21763415981667,3.01087868763386,93.4811032241773));
#244016=CARTESIAN_POINT('Ctrl Pts',(4.45644300851865,6.95145955779684,93.6930423786106));
#244017=CARTESIAN_POINT('Ctrl Pts',(-0.721137693822396,8.72926331774012,
93.9049815330433));
#244018=CARTESIAN_POINT('Ctrl Pts',(-6.13130014661506,6.25212443618104,
94.1169206874767));
#244019=CARTESIAN_POINT('Ctrl Pts',(-8.1828940095445,1.16647041961204,94.3288598419095));
#244020=CARTESIAN_POINT('Ctrl Pts',(-7.76289181710849,-2.88984227955638,
94.4878142077343));
#244021=CARTESIAN_POINT('Ctrl Pts',(-5.42178472385128,-6.23895819146835,
94.6467685735592));
#244022=CARTESIAN_POINT('Ctrl Pts',(-0.555293887085499,-8.73437746303224,
94.8587077279919));
#244023=CARTESIAN_POINT('Ctrl Pts',(6.61470172236203,-6.66720856734195,
95.1236316710334));
#244024=CARTESIAN_POINT('Ctrl Pts',(9.18728742537818,1.98277905699441,95.4415404026827));
#244025=CARTESIAN_POINT('Ctrl Pts',(4.28467384452833,7.63128244151975,95.7064643457242));
#244026=CARTESIAN_POINT('Ctrl Pts',(-1.13518563206099,8.17887693101086,
95.9184035001571));
#244027=CARTESIAN_POINT('Ctrl Pts',(-6.22455563939611,6.1623846630958,96.1303426545902));
#244028=CARTESIAN_POINT('Ctrl Pts',(-8.72357765688459,0.762295426772799,
96.3422818090232));
#244029=CARTESIAN_POINT('Ctrl Pts',(-6.97485602638083,-4.43528928284595,
96.5542209634562));
#244030=CARTESIAN_POINT('Ctrl Pts',(-4.01793155330728,-7.24361124010522,
96.7131753292809));
#244031=CARTESIAN_POINT('Ctrl Pts',(-0.0615012174835848,-8.26538362732942,
96.8721296951056));
#244032=CARTESIAN_POINT('Ctrl Pts',(5.25821632703537,-6.99634633404169,
97.0840688495389));
#244033=CARTESIAN_POINT('Ctrl Pts',(9.36073618300337,-0.763260812873669,
97.3489927925797));
#244034=CARTESIAN_POINT('Ctrl Pts',(5.68987284831566,7.48084286664063,97.6669015242299));
#244035=CARTESIAN_POINT('Ctrl Pts',(-1.70776911520327,8.58361382550448,
97.9318254672705));
#244036=CARTESIAN_POINT('Ctrl Pts',(-6.18117294910438,5.47501372099833,
98.1437646217039));
#244037=CARTESIAN_POINT('Ctrl Pts',(-8.73606223445313,0.633477923574835,
98.3557037761367));
#244038=CARTESIAN_POINT('Ctrl Pts',(-7.12275729466399,-5.09394051542466,
98.5676429305698));
#244039=CARTESIAN_POINT('Ctrl Pts',(-2.41426532741029,-7.90517112655593,
98.7795820850029));
#244040=CARTESIAN_POINT('Ctrl Pts',(1.65829830086496,-8.11564689412926,
98.9385364508275));
#244041=CARTESIAN_POINT('Ctrl Pts',(5.32834362648309,-6.31894794287737,
99.0974908166525));
#244042=CARTESIAN_POINT('Ctrl Pts',(8.5442983962845,-1.89543290121545,99.3094299710852));
#244043=CARTESIAN_POINT('Ctrl Pts',(7.60741447147656,5.50755789941659,99.5743539141267));
#244044=CARTESIAN_POINT('Ctrl Pts',(-0.542451036991783,9.38314498970543,
99.8922626457761));
#244045=CARTESIAN_POINT('Ctrl Pts',(-6.87935126239726,5.41012272178607,
100.157186588818));
#244046=CARTESIAN_POINT('Ctrl Pts',(-8.256101354105,0.139515958245546,100.369125743251));
#244047=CARTESIAN_POINT('Ctrl Pts',(-7.04847008699869,-5.19991798748602,
100.581064897684));
#244048=CARTESIAN_POINT('Ctrl Pts',(-2.09829360246755,-8.50170955815468,
100.793004052116));
#244049=CARTESIAN_POINT('Ctrl Pts',(3.30677251906783,-7.57533254177048,
101.00494320655));
#244050=CARTESIAN_POINT('Ctrl Pts',(6.5374461147551,-5.08679428142266,101.163897572374));
#244051=CARTESIAN_POINT('Ctrl Pts',(8.1570527526437,-1.33523005406003,101.322851938199));
#244052=CARTESIAN_POINT('Ctrl Pts',(7.72345543585777,4.11654431508733,101.534791092632));
#244053=CARTESIAN_POINT('Ctrl Pts',(2.19749283155659,9.13109928823001,101.799715035674));
#244054=CARTESIAN_POINT('Ctrl Pts',(-6.51403897443435,6.775319864399,102.117623767323));
#244055=CARTESIAN_POINT('Ctrl Pts',(-8.74428626583565,-0.363812255637007,
102.382547710364));
#244056=CARTESIAN_POINT('Ctrl Pts',(-6.36263028075182,-5.26304191341087,
102.594486864797));
#244057=CARTESIAN_POINT('Ctrl Pts',(-1.97294169497133,-8.53390758750871,
102.80642601923));
#244058=CARTESIAN_POINT('Ctrl Pts',(3.93474143355371,-7.82302443460647,
103.018365173664));
#244059=CARTESIAN_POINT('Ctrl Pts',(7.43836835449544,-3.60431461364149,
103.230304328096));
#244060=CARTESIAN_POINT('Ctrl Pts',(8.2742878160075,0.387090303045284,103.389258693921));
#244061=CARTESIAN_POINT('Ctrl Pts',(7.06497136278176,4.2902830384196,103.548213059746));
#244062=CARTESIAN_POINT('Ctrl Pts',(3.1902359906745,8.14985247053979,103.760152214179));
#244063=CARTESIAN_POINT('Ctrl Pts',(-4.26868151559312,8.36566238110832,
104.02507615722));
#244064=CARTESIAN_POINT('Ctrl Pts',(-9.35457173711607,0.910851601809192,
104.34298488887));
#244065=CARTESIAN_POINT('Ctrl Pts',(-6.40616954212128,-5.96287627356382,
104.607908831911));
#244066=CARTESIAN_POINT('Ctrl Pts',(-1.41088053516091,-8.1358521611054,
104.819847986344));
#244067=CARTESIAN_POINT('Ctrl Pts',(4.05090606201291,-7.76596663144024,
105.031787140777));
#244068=CARTESIAN_POINT('Ctrl Pts',(8.07649326184086,-3.38410372843594,
105.24372629521));
#244069=CARTESIAN_POINT('Ctrl Pts',(7.9946184145099,2.09916269442086,105.455665449643));
#244070=CARTESIAN_POINT('Ctrl Pts',(6.03398848610383,5.67491504028099,105.614619815468));
#244071=CARTESIAN_POINT('Ctrl Pts',(2.57702218155512,7.8536173565084,105.773574181293));
#244072=CARTESIAN_POINT('Ctrl Pts',(-2.8764107100891,8.26583101657924,105.985513335726));
#244073=CARTESIAN_POINT('Ctrl Pts',(-8.6830601333559,3.57916410308085,106.250437278767));
#244074=CARTESIAN_POINT('Ctrl Pts',(-7.698711346468,-5.39142899694823,106.568346010416));
#244075=CARTESIAN_POINT('Ctrl Pts',(-0.988846449827039,-8.69580843595914,
106.833269953458));
#244076=CARTESIAN_POINT('Ctrl Pts',(4.21902677410503,-7.09806222508963,
107.045209107891));
#244077=CARTESIAN_POINT('Ctrl Pts',(8.12763461419744,-3.26521564708898,
107.257148262323));
#244078=CARTESIAN_POINT('Ctrl Pts',(8.33617651168416,2.68142921208433,107.469087416757));
#244079=CARTESIAN_POINT('Ctrl Pts',(4.70815407640191,6.79365091862457,107.68102657119));
#244080=CARTESIAN_POINT('Ctrl Pts',(0.893376316806882,8.23502012877987,
107.839980937014));
#244081=CARTESIAN_POINT('Ctrl Pts',(-3.14960528647604,7.64201121734848,
107.998935302839));
#244082=CARTESIAN_POINT('Ctrl Pts',(-7.56047424334183,4.40873339900752,
108.210874457272));
#244083=CARTESIAN_POINT('Ctrl Pts',(-8.92381613848062,-2.92770464405993,
108.475798400314));
#244084=CARTESIAN_POINT('Ctrl Pts',(-2.34236803040989,-9.10225109714528,
108.793707131963));
#244085=CARTESIAN_POINT('Ctrl Pts',(4.90377818824009,-7.2489903529232,109.058631075004));
#244086=CARTESIAN_POINT('Ctrl Pts',(7.82100553314839,-2.64849895645091,
109.270570229437));
#244087=CARTESIAN_POINT('Ctrl Pts',(8.29771285046806,2.80500251248967,109.482509383871));
#244088=CARTESIAN_POINT('Ctrl Pts',(4.58897114648115,7.45809930680315,109.694448538303));
#244089=CARTESIAN_POINT('Ctrl Pts',(-0.841344032665456,8.22268495261532,
109.906387692737));
#244090=CARTESIAN_POINT('Ctrl Pts',(-4.6766484720228,6.83685869635818,110.065342058561));
#244091=CARTESIAN_POINT('Ctrl Pts',(-7.36233516049885,3.75717578656633,
110.224296424386));
#244092=CARTESIAN_POINT('Ctrl Pts',(-8.61050026220927,-1.56747765606163,
110.436235578819));
#244093=CARTESIAN_POINT('Ctrl Pts',(-4.87522711379125,-8.02733514593802,
110.70115952186));
#244094=CARTESIAN_POINT('Ctrl Pts',(4.13986408852363,-8.43796114911191,
111.01906825351));
#244095=CARTESIAN_POINT('Ctrl Pts',(8.4393398531768,-2.31785342479099,111.283992196551));
#244096=CARTESIAN_POINT('Ctrl Pts',(7.66371912007564,3.07409881435952,111.495931350984));
#244097=CARTESIAN_POINT('Ctrl Pts',(4.47939051666135,7.52696075738007,111.707870505417));
#244098=CARTESIAN_POINT('Ctrl Pts',(-1.36398120786484,8.64993969446986,
111.91980965985));
#244099=CARTESIAN_POINT('Ctrl Pts',(-5.98643949729513,5.69938152403339,
112.131748814283));
#244100=CARTESIAN_POINT('Ctrl Pts',(-7.99878305688911,2.15247470918116,
112.290703180108));
#244101=CARTESIAN_POINT('Ctrl Pts',(-8.03626557491185,-1.93359367917992,
112.449657545933));
#244102=CARTESIAN_POINT('Ctrl Pts',(-5.5217804877095,-6.79026076180513,
112.661596700365));
#244103=CARTESIAN_POINT('Ctrl Pts',(1.51670144919076,-9.26852553917179,
112.926520643407));
#244104=CARTESIAN_POINT('Ctrl Pts',(8.6322182027274,-3.71785851342826,113.244429375056));
#244105=CARTESIAN_POINT('Ctrl Pts',(7.91842613892663,3.72738905114509,113.509353318098));
#244106=CARTESIAN_POINT('Ctrl Pts',(3.8227692375331,7.31909213143469,113.721292472531));
#244107=CARTESIAN_POINT('Ctrl Pts',(-1.49200749139442,8.63099016854494,
113.933231626964));
#244108=CARTESIAN_POINT('Ctrl Pts',(-6.66131875303892,5.68407722711321,
114.145170781397));
#244109=CARTESIAN_POINT('Ctrl Pts',(-8.25407714505212,0.43659832202693,
114.35710993583));
#244110=CARTESIAN_POINT('Ctrl Pts',(-7.47620145562958,-3.56652345564748,
114.516064301654));
#244111=CARTESIAN_POINT('Ctrl Pts',(-4.84746335710774,-6.694956901144,114.675018667479));
#244112=CARTESIAN_POINT('Ctrl Pts',(0.221052877113095,-8.74921919906447,
114.886957821912));
#244113=CARTESIAN_POINT('Ctrl Pts',(7.17960828852418,-6.05468197179771,
115.151881764953));
#244114=CARTESIAN_POINT('Ctrl Pts',(8.97538752092487,2.78927981288996,115.469790496603));
#244115=CARTESIAN_POINT('Ctrl Pts',(3.59142080693308,7.98101486302093,115.734714439644));
#244116=CARTESIAN_POINT('Ctrl Pts',(-1.85564300132502,8.04607129744028,
115.946653594077));
#244117=CARTESIAN_POINT('Ctrl Pts',(-6.74625323876447,5.58642505385656,
116.15859274851));
#244118=CARTESIAN_POINT('Ctrl Pts',(-8.75680923615344,-0.0139088098970721,
116.370531902943));
#244119=CARTESIAN_POINT('Ctrl Pts',(-6.55428827612388,-5.03604138234919,
116.582471057376));
#244120=CARTESIAN_POINT('Ctrl Pts',(-3.36008912066162,-7.57122703833746,
116.741425423201));
#244121=CARTESIAN_POINT('Ctrl Pts',(0.671333398386882,-8.23830445995342,
116.900379789026));
#244122=CARTESIAN_POINT('Ctrl Pts',(5.85763438229858,-6.50275483245934,
117.112318943459));
#244123=CARTESIAN_POINT('Ctrl Pts',(9.39154564904932,0.069421020448106,
117.3772428865));
#244124=CARTESIAN_POINT('Ctrl Pts',(5.00442337244051,7.95571553882744,117.69515161815));
#244125=CARTESIAN_POINT('Ctrl Pts',(-2.4618463338131,8.39846499575511,117.960075561191));
#244126=CARTESIAN_POINT('Ctrl Pts',(-6.64211697505903,4.90560458674478,
118.172014715624));
#244127=CARTESIAN_POINT('Ctrl Pts',(-8.75782708988359,-0.143325879022417,
118.383953870057));
#244128=CARTESIAN_POINT('Ctrl Pts',(-6.64322866813353,-5.70520940161391,
118.59589302449));
#244129=CARTESIAN_POINT('Ctrl Pts',(-1.70409789680017,-8.0880441374531,
118.807832178923));
#244130=CARTESIAN_POINT('Ctrl Pts',(2.37109252386944,-7.93672463980526,
118.966786544748));
#244131=CARTESIAN_POINT('Ctrl Pts',(5.86744526985531,-5.82180684254729,
119.125740910572));
#244132=CARTESIAN_POINT('Ctrl Pts',(8.67866987731518,-1.13065915657217,
119.337680065005));
#244133=CARTESIAN_POINT('Ctrl Pts',(7.08931787809962,6.1601559216884,119.602604008047));
#244134=CARTESIAN_POINT('Ctrl Pts',(-1.37198012918096,9.29813602559685,
119.920512739696));
#244135=CARTESIAN_POINT('Ctrl Pts',(-7.33179591486946,4.77908676620727,
120.185436682737));
#244136=CARTESIAN_POINT('Ctrl Pts',(-8.2359734640424,-0.592802978609528,
120.397375837171));
#244137=CARTESIAN_POINT('Ctrl Pts',(-6.55984064560654,-5.80418541641674,
120.609314991604));
#244138=CARTESIAN_POINT('Ctrl Pts',(-1.33649626603419,-8.65422897687898,
120.821254146037));
#244139=CARTESIAN_POINT('Ctrl Pts',(3.96518867752886,-7.25242623973973,
121.03319330047));
#244140=CARTESIAN_POINT('Ctrl Pts',(6.9625785746472,-4.4873352177773,121.192147666294));
#244141=CARTESIAN_POINT('Ctrl Pts',(8.24329540403443,-0.606984174837291,
121.351102032119));
#244142=CARTESIAN_POINT('Ctrl Pts',(7.32819299175547,4.78490213518995,121.563041186552));
#244143=CARTESIAN_POINT('Ctrl Pts',(1.37951985544195,9.28993401078269,121.827965129593));
#244144=CARTESIAN_POINT('Ctrl Pts',(-7.08892403898856,6.17128989716245,
122.145873861243));
#244145=CARTESIAN_POINT('Ctrl Pts',(-8.67762511076401,-1.13741992829038,
122.410797804284));
#244146=CARTESIAN_POINT('Ctrl Pts',(-5.87110519946018,-5.80627229887907,
122.622736958717));
#244147=CARTESIAN_POINT('Ctrl Pts',(-1.20878387435662,-8.67518986472293,
122.83467611315));
#244148=CARTESIAN_POINT('Ctrl Pts',(4.61263996051857,-7.44348399931125,
123.046615267583));
#244149=CARTESIAN_POINT('Ctrl Pts',(7.72855719143385,-2.93083799449995,
123.258554422016));
#244150=CARTESIAN_POINT('Ctrl Pts',(8.20741322198891,1.11894859951792,123.417508787841));
#244151=CARTESIAN_POINT('Ctrl Pts',(6.65690140163672,4.89959310918416,123.576463153666));
#244152=CARTESIAN_POINT('Ctrl Pts',(2.45532751157165,8.40053973139096,123.788402308099));
#244153=CARTESIAN_POINT('Ctrl Pts',(-4.99336182376418,7.9543878867723,124.05332625114));
#244154=CARTESIAN_POINT('Ctrl Pts',(-9.39848700083521,0.0781352705295933,
124.37123498279));
#244155=CARTESIAN_POINT('Ctrl Pts',(-5.85244410633151,-6.5072113565259,
124.636158925831));
#244156=CARTESIAN_POINT('Ctrl Pts',(-0.684216006160355,-8.22888344362542,
124.848098080264));
#244157=CARTESIAN_POINT('Ctrl Pts',(4.72329014591897,-7.37635464449487,
125.060037234697));
#244158=CARTESIAN_POINT('Ctrl Pts',(8.34465248327202,-2.65493434698441,
125.27197638913));
#244159=CARTESIAN_POINT('Ctrl Pts',(7.77709699727505,2.79949458049909,125.483915543563));
#244160=CARTESIAN_POINT('Ctrl Pts',(5.50725095712811,6.18739562821485,125.642869909388));
#244161=CARTESIAN_POINT('Ctrl Pts',(1.87078359296915,8.05111903122513,125.801824275212));
#244162=CARTESIAN_POINT('Ctrl Pts',(-3.59772217398919,7.97835171740039,
126.013763429645));
#244163=CARTESIAN_POINT('Ctrl Pts',(-8.96612102302944,2.7954646763365,126.278687372687));
#244164=CARTESIAN_POINT('Ctrl Pts',(-7.19054838272788,-6.05257606156408,
126.596596104336));
#244165=CARTESIAN_POINT('Ctrl Pts',(-0.214211863482096,-8.74922939085366,
126.861520047377));
#244166=CARTESIAN_POINT('Ctrl Pts',(4.8315502594368,-6.69617774274212,127.073459201811));
#244167=CARTESIAN_POINT('Ctrl Pts',(8.38505505209209,-2.53198132245899,
127.285398356243));
#244168=CARTESIAN_POINT('Ctrl Pts',(8.06570230809352,3.40974305932135,127.497337510677));
#244169=CARTESIAN_POINT('Ctrl Pts',(4.08747682380009,7.18421469794477,127.709276665109));
#244170=CARTESIAN_POINT('Ctrl Pts',(0.159958904481424,8.28179273549621,
127.868231030934));
#244171=CARTESIAN_POINT('Ctrl Pts',(-3.81454999758313,7.33277281951486,
128.027185396759));
#244172=CARTESIAN_POINT('Ctrl Pts',(-7.92148121906867,3.72126809887472,
128.239124551192));
#244173=CARTESIAN_POINT('Ctrl Pts',(-8.62920081496092,-3.70713396727616,
128.504048494233));
#244174=CARTESIAN_POINT('Ctrl Pts',(-1.52638179124352,-9.27404020116001,
128.821957225883));
#244175=CARTESIAN_POINT('Ctrl Pts',(5.52698401932788,-6.78581972250434,
129.086881168924));
#244176=CARTESIAN_POINT('Ctrl Pts',(8.02497081889033,-1.94486956575818,
129.298820323357));
#244177=CARTESIAN_POINT('Ctrl Pts',(8.01643725491605,3.52942082811193,129.51075947779));
#244178=CARTESIAN_POINT('Ctrl Pts',(3.90987036279272,7.83548436278796,129.722698632223));
#244179=CARTESIAN_POINT('Ctrl Pts',(-1.5668407534036,8.11575120766773,129.934637786656));
#244180=CARTESIAN_POINT('Ctrl Pts',(-5.26421941759418,6.39544147719898,
130.093592152481));
#244181=CARTESIAN_POINT('Ctrl Pts',(-7.66637191338927,3.08983666108217,
130.252546518306));
#244182=CARTESIAN_POINT('Ctrl Pts',(-8.43768018353644,-2.32449007064272,
130.464485672739));
#244183=CARTESIAN_POINT('Ctrl Pts',(-4.14454615641619,-8.42785180890101,
130.72940961578));
#244184=CARTESIAN_POINT('Ctrl Pts',(4.87145950259031,-8.0378196882011,131.047318347429));
#244185=CARTESIAN_POINT('Ctrl Pts',(8.61156516868868,-1.56072002727027,
131.312242290471));
#244186=CARTESIAN_POINT('Ctrl Pts',(7.36108771321945,3.74126475232265,131.524181444904));
#244187=CARTESIAN_POINT('Ctrl Pts',(3.79461755858945,7.89436224373846,131.736120599337));
#244188=CARTESIAN_POINT('Ctrl Pts',(-2.12529019654376,8.49500106110592,
131.94805975377));
#244189=CARTESIAN_POINT('Ctrl Pts',(-6.46803651554601,5.14634931171196,
132.159998908203));
#244190=CARTESIAN_POINT('Ctrl Pts',(-8.15808413562142,1.43504042893685,
132.318953274028));
#244191=CARTESIAN_POINT('Ctrl Pts',(-7.83325525710364,-2.63826854349615,
132.477907639852));
#244192=CARTESIAN_POINT('Ctrl Pts',(-4.8982015186142,-7.25295271015235,
132.689846794285));
#244193=CARTESIAN_POINT('Ctrl Pts',(2.33223701977551,-9.09761613362508,
132.954770737327));
#244194=CARTESIAN_POINT('Ctrl Pts',(8.92777217698664,-2.93811955876141,
133.272679468976));
#244195=CARTESIAN_POINT('Ctrl Pts',(7.55688871607167,4.41455951102258,133.537603412017));
#244196=CARTESIAN_POINT('Ctrl Pts',(3.15900467980914,7.6291128306614,133.74954256645));
#244197=CARTESIAN_POINT('Ctrl Pts',(-2.25113285491774,8.46477877165042,
133.961481720883));
#244198=CARTESIAN_POINT('Ctrl Pts',(-7.13890352140618,5.07128788398544,
134.173420875317));
#244199=CARTESIAN_POINT('Ctrl Pts',(-8.26028831705473,-0.296710146126478,
134.385360029749));
#244200=CARTESIAN_POINT('Ctrl Pts',(-7.13066352516941,-4.21513154063565,
134.544314395574));
#244201=CARTESIAN_POINT('Ctrl Pts',(-4.2349837389692,-7.09825553010841,
134.703268761399));
#244202=CARTESIAN_POINT('Ctrl Pts',(0.995655938673994,-8.69519430925777,
134.915207915832));
#244203=CARTESIAN_POINT('Ctrl Pts',(7.68800861236119,-5.3944913782222,135.180131858873));
#244204=CARTESIAN_POINT('Ctrl Pts',(8.6928249893351,3.5738163419672,135.498040590523));
#244205=CARTESIAN_POINT('Ctrl Pts',(2.86992050536337,8.26793953120299,135.762964533564));
#244206=CARTESIAN_POINT('Ctrl Pts',(-2.56152361166258,7.8499123324488,135.974903687997));
#244207=CARTESIAN_POINT('Ctrl Pts',(-7.21477125736058,4.96654145705927,
136.18684284243));
#244208=CARTESIAN_POINT('Ctrl Pts',(-8.72126827650654,-0.790103703246512,
136.398781996863));
#244209=CARTESIAN_POINT('Ctrl Pts',(-6.08193578826746,-5.59702881765901,
136.610721151296));
#244210=CARTESIAN_POINT('Ctrl Pts',(-2.67619958111933,-7.83950383357153,
136.769675517121));
#244211=CARTESIAN_POINT('Ctrl Pts',(1.3996162528399,-8.14590827035688,136.928629882946));
#244212=CARTESIAN_POINT('Ctrl Pts',(6.40936146784205,-5.95899205325436,
137.140569037379));
#244213=CARTESIAN_POINT('Ctrl Pts',(9.35170511633603,0.903656038138216,
137.40549298042));
#244214=CARTESIAN_POINT('Ctrl Pts',(4.27385822118494,8.36429562826514,137.723401712069));
#244215=CARTESIAN_POINT('Ctrl Pts',(-3.18692714972201,8.15337579492017,
137.988325655111));
#244216=CARTESIAN_POINT('Ctrl Pts',(-7.06372063712096,4.28927272083034,
138.200264809544));
#244217=CARTESIAN_POINT('Ctrl Pts',(-8.27206068517265,0.40045319240588,
138.359219175368));
#244218=CARTESIAN_POINT('Ctrl Pts',(-7.44413426218233,-3.62023136901316,
138.518180255724));
#244219=CARTESIAN_POINT('Ctrl Pts',(-5.68565861609716,-5.69747426071045,
138.624156547473));
#244220=CARTESIAN_POINT('Ctrl Pts',(-4.60940596141801,-6.46483699172352,
138.677148050613));
#244221=CARTESIAN_POINT('Ctrl Pts',(-3.42490370648437,7.13754033682952,
138.));
#244222=CARTESIAN_POINT('Ctrl Pts',(-3.60315378289199,7.03782110867972,
138.));
#244223=CARTESIAN_POINT('Ctrl Pts',(-3.77697596682028,6.93110617027609,
138.));
#244224=CARTESIAN_POINT('Ctrl Pts',(-3.94592285661015,6.81740720159191,
138.));
#244225=CARTESIAN_POINT('Ctrl Pts',(-4.11538230205325,6.70336328989492,
138.));
#244226=CARTESIAN_POINT('Ctrl Pts',(-4.27993741495876,6.5822926792708,138.));
#244227=CARTESIAN_POINT('Ctrl Pts',(-4.43932721728487,6.45467407365266,
138.));
#244228=CARTESIAN_POINT('Ctrl Pts',(-4.59985158806564,6.32614705330504,
138.));
#244229=CARTESIAN_POINT('Ctrl Pts',(-4.75513728704195,6.19097784029614,
138.));
#244230=CARTESIAN_POINT('Ctrl Pts',(-4.90487911920266,6.04961867430912,
138.));
#244231=CARTESIAN_POINT('Ctrl Pts',(-5.05399550788871,5.90884993897649,
138.));
#244232=CARTESIAN_POINT('Ctrl Pts',(-5.19761460421856,5.76194216159953,
138.));
#244233=CARTESIAN_POINT('Ctrl Pts',(-5.33539102092455,5.60931572741658,
138.));
#244234=CARTESIAN_POINT('Ctrl Pts',(-5.44873023956294,5.48376041680946,
138.));
#244235=CARTESIAN_POINT('Ctrl Pts',(-5.55811488447614,5.35433451946705,
138.));
#244236=CARTESIAN_POINT('Ctrl Pts',(-5.66332759072228,5.2212635732539,138.));
#244237=CARTESIAN_POINT('Ctrl Pts',(-5.67874041195431,5.20176974234377,
138.));
#244238=CARTESIAN_POINT('Ctrl Pts',(-5.69406497234922,5.18219598688969,
138.));
#244239=CARTESIAN_POINT('Ctrl Pts',(-5.70929635822883,5.1625484140524,138.));
#244240=CARTESIAN_POINT('Ctrl Pts',(-5.83335269592323,5.00252319047495,
138.));
#244241=CARTESIAN_POINT('Ctrl Pts',(-5.95094323302251,4.83797793878056,
138.));
#244242=CARTESIAN_POINT('Ctrl Pts',(-6.06181278565512,4.66936481397146,
138.));
#244243=CARTESIAN_POINT('Ctrl Pts',(-6.17280782281805,4.50056084922218,
138.));
#244244=CARTESIAN_POINT('Ctrl Pts',(-6.27706702203869,4.32767912330544,
138.));
#244245=CARTESIAN_POINT('Ctrl Pts',(-6.3742898456234,4.15114664381216,138.));
#244246=CARTESIAN_POINT('Ctrl Pts',(-6.41202336569123,4.08263195135644,
138.));
#244247=CARTESIAN_POINT('Ctrl Pts',(-6.44869647661346,4.01356710710628,
138.));
#244248=CARTESIAN_POINT('Ctrl Pts',(-6.48428962272322,3.9439763260544,138.));
#244249=CARTESIAN_POINT('Ctrl Pts',(-6.57620068165998,3.76427424636205,
138.));
#244250=CARTESIAN_POINT('Ctrl Pts',(-6.66091404102716,3.58106572388496,
138.));
#244251=CARTESIAN_POINT('Ctrl Pts',(-6.73826053739278,3.39476139218723,
138.));
#244252=CARTESIAN_POINT('Ctrl Pts',(-6.81486615435339,3.2102416150447,138.));
#244253=CARTESIAN_POINT('Ctrl Pts',(-6.88424542684704,3.0226844125455,138.));
#244254=CARTESIAN_POINT('Ctrl Pts',(-6.94618315954604,2.83248581782527,
138.));
#244255=CARTESIAN_POINT('Ctrl Pts',(-6.96453053523597,2.77614463578707,
138.));
#244256=CARTESIAN_POINT('Ctrl Pts',(-6.98222458498384,2.71957169207803,
138.));
#244257=CARTESIAN_POINT('Ctrl Pts',(-6.99925883342174,2.66277735691564,
138.));
#244258=CARTESIAN_POINT('Ctrl Pts',(-7.00951057192051,2.62859676630024,
138.));
#244259=CARTESIAN_POINT('Ctrl Pts',(-7.01952332218084,2.59433598864154,
138.));
#244260=CARTESIAN_POINT('Ctrl Pts',(-7.02929560087802,2.55999729648689,
138.));
#244261=CARTESIAN_POINT('Ctrl Pts',(-7.03613199613462,2.53597496971556,
138.));
#244262=CARTESIAN_POINT('Ctrl Pts',(-7.04284847966699,2.51192225244768,
138.));
#244263=CARTESIAN_POINT('Ctrl Pts',(-7.04944318094255,2.48784598206391,
138.));
#244264=CARTESIAN_POINT('Ctrl Pts',(-7.10167376413709,2.29715991597125,
138.));
#244265=CARTESIAN_POINT('Ctrl Pts',(-7.14630341841885,2.1048780735385,138.));
#244266=CARTESIAN_POINT('Ctrl Pts',(-7.18322675984256,1.91140034900355,
138.));
#244267=CARTESIAN_POINT('Ctrl Pts',(-7.22000686923813,1.71867315802871,
138.));
#244268=CARTESIAN_POINT('Ctrl Pts',(-7.24914041866994,1.524758701822,138.));
#244269=CARTESIAN_POINT('Ctrl Pts',(-7.27047217192691,1.33004595658973,
138.));
#244270=CARTESIAN_POINT('Ctrl Pts',(-7.29148754274809,1.13822109834324,
138.));
#244271=CARTESIAN_POINT('Ctrl Pts',(-7.30493081407415,0.945620872512938,
138.));
#244272=CARTESIAN_POINT('Ctrl Pts',(-7.3106035273759,0.752620165465328,
138.));
#244273=CARTESIAN_POINT('Ctrl Pts',(-7.31455505027739,0.618178907228735,
138.));
#244274=CARTESIAN_POINT('Ctrl Pts',(-7.31473503652726,0.483543379414253,
138.));
#244275=CARTESIAN_POINT('Ctrl Pts',(-7.3110617236461,0.348843391340057,
138.));
#244276=CARTESIAN_POINT('Ctrl Pts',(-7.30698329038145,0.199287682397503,
138.));
#244277=CARTESIAN_POINT('Ctrl Pts',(-7.29815477473225,0.0496521820743232,
138.));
#244278=CARTESIAN_POINT('Ctrl Pts',(-7.28460785612623,-0.099828577738282,
138.));
#244279=CARTESIAN_POINT('Ctrl Pts',(-7.27923431788771,-0.159121809072706,
138.));
#244280=CARTESIAN_POINT('Ctrl Pts',(-7.27311821566584,-0.218390598344035,
138.));
#244281=CARTESIAN_POINT('Ctrl Pts',(-7.26626087139555,-0.27761989288037,
138.));
#244282=CARTESIAN_POINT('Ctrl Pts',(-7.26368656164304,-0.299855111727345,
138.));
#244283=CARTESIAN_POINT('Ctrl Pts',(-7.26100889000677,-0.3220751844165,
138.));
#244284=CARTESIAN_POINT('Ctrl Pts',(-7.25822828218742,-0.344278585099771,
138.));
#244285=CARTESIAN_POINT('Ctrl Pts',(-7.23431083840358,-0.535261500402182,
138.));
#244286=CARTESIAN_POINT('Ctrl Pts',(-7.20277958541697,-0.725030926027641,
138.));
#244287=CARTESIAN_POINT('Ctrl Pts',(-7.163817492447,-0.913118345634504,
138.));
#244288=CARTESIAN_POINT('Ctrl Pts',(-7.12463947625704,-1.10224812303549,
138.));
#244289=CARTESIAN_POINT('Ctrl Pts',(-7.07794778369885,-1.28967793268298,
138.));
#244290=CARTESIAN_POINT('Ctrl Pts',(-7.0238779237268,-1.47491810765451,
138.));
#244291=CARTESIAN_POINT('Ctrl Pts',(-6.97016135742329,-1.65894791919977,
138.));
#244292=CARTESIAN_POINT('Ctrl Pts',(-6.90916240290187,-1.84081728860338,
138.));
#244293=CARTESIAN_POINT('Ctrl Pts',(-6.84096862416969,-2.02002252000683,
138.));
#244294=CARTESIAN_POINT('Ctrl Pts',(-6.77414302540993,-2.19563233533101,
138.));
#244295=CARTESIAN_POINT('Ctrl Pts',(-6.70040803332846,-2.36868437319925,
138.));
#244296=CARTESIAN_POINT('Ctrl Pts',(-6.61980768402212,-2.53867320106378,
138.));
#244297=CARTESIAN_POINT('Ctrl Pts',(-6.57470303536745,-2.63380041108253,
138.));
#244298=CARTESIAN_POINT('Ctrl Pts',(-6.52744775912282,-2.72796772928592,
138.));
#244299=CARTESIAN_POINT('Ctrl Pts',(-6.47804480086152,-2.82108121632785,
138.));
#244300=CARTESIAN_POINT('Ctrl Pts',(-6.46323930063093,-2.84898626093223,
138.));
#244301=CARTESIAN_POINT('Ctrl Pts',(-6.44824088784976,-2.87679662862212,
138.));
#244302=CARTESIAN_POINT('Ctrl Pts',(-6.43304958529191,-2.90450971444846,
138.));
#244303=CARTESIAN_POINT('Ctrl Pts',(-6.42219754347207,-2.92430680328918,
138.));
#244304=CARTESIAN_POINT('Ctrl Pts',(-6.41124835080748,-2.9440518496595,
138.));
#244305=CARTESIAN_POINT('Ctrl Pts',(-6.4002062787239,-2.96373661052125,
138.));
#244306=CARTESIAN_POINT('Ctrl Pts',(-6.37888604171424,-3.00174431087616,
138.));
#244307=CARTESIAN_POINT('Ctrl Pts',(-6.35721514239056,-3.03953534017548,
138.));
#244308=CARTESIAN_POINT('Ctrl Pts',(-6.33519494702275,-3.07710388684579,
138.));
#244309=CARTESIAN_POINT('Ctrl Pts',(-6.23932871838984,-3.2406607865165,
138.));
#244310=CARTESIAN_POINT('Ctrl Pts',(-6.13684529840294,-3.40000354179732,
138.));
#244311=CARTESIAN_POINT('Ctrl Pts',(-6.02808002948692,-3.55482687716532,
138.));
#244312=CARTESIAN_POINT('Ctrl Pts',(-5.91930392863085,-3.70966563139914,
138.));
#244313=CARTESIAN_POINT('Ctrl Pts',(-5.80424417060215,-3.85998451885378,
138.));
#244314=CARTESIAN_POINT('Ctrl Pts',(-5.68320070145349,-4.0054404017757,
138.));
#244315=CARTESIAN_POINT('Ctrl Pts',(-5.57833647525666,-4.13145396298363,
138.));
#244316=CARTESIAN_POINT('Ctrl Pts',(-5.46898049117472,-4.25381724526501,
138.));
#244317=CARTESIAN_POINT('Ctrl Pts',(-5.35531105443876,-4.37228026380955,
138.));
#244318=CARTESIAN_POINT('Ctrl Pts',(-5.33628706891599,-4.39210651451059,
138.));
#244319=CARTESIAN_POINT('Ctrl Pts',(-5.31714211142194,-4.41182350054872,
138.));
#244320=CARTESIAN_POINT('Ctrl Pts',(-5.29788733618046,-4.43141968005266,
138.));
#244321=CARTESIAN_POINT('Ctrl Pts',(-5.1670532765616,-4.56457354372363,
138.));
#244322=CARTESIAN_POINT('Ctrl Pts',(-5.0310357855152,-4.69227461210752,
138.));
#244323=CARTESIAN_POINT('Ctrl Pts',(-4.89014018822931,-4.8142080523858,
138.));
#244324=CARTESIAN_POINT('Ctrl Pts',(-4.75091868359083,-4.93469270448491,
138.));
#244325=CARTESIAN_POINT('Ctrl Pts',(-4.60693372766405,-5.04954629887319,
138.));
#244326=CARTESIAN_POINT('Ctrl Pts',(-4.4584541052344,-5.15842196959294,
138.));
#244327=CARTESIAN_POINT('Ctrl Pts',(-4.31052817018024,-5.26689163790383,
138.));
#244328=CARTESIAN_POINT('Ctrl Pts',(-4.15814051823896,-5.36942825198228,
138.));
#244329=CARTESIAN_POINT('Ctrl Pts',(-4.0015392161787,-5.46564050896491,
138.));
#244330=CARTESIAN_POINT('Ctrl Pts',(-3.97741995172579,-5.48045883320132,
138.));
#244331=CARTESIAN_POINT('Ctrl Pts',(-3.95320070856606,-5.49512703602489,
138.));
#244332=CARTESIAN_POINT('Ctrl Pts',(-3.92888236737319,-5.50964357679733,
138.));
#244333=CARTESIAN_POINT('Ctrl Pts',(-3.93307528793382,-5.51266228421142,
8.));
#244334=CARTESIAN_POINT('Ctrl Pts',(-4.08477702892364,-5.42354303040725,
8.));
#244335=CARTESIAN_POINT('Ctrl Pts',(-4.2326033773089,-5.32840285450346,
8.));
#244336=CARTESIAN_POINT('Ctrl Pts',(-4.37614884580116,-5.22732383700667,
8.));
#244337=CARTESIAN_POINT('Ctrl Pts',(-4.52451204222272,-5.12285236685515,
8.));
#244338=CARTESIAN_POINT('Ctrl Pts',(-4.66830321494952,-5.01203736235522,
8.));
#244339=CARTESIAN_POINT('Ctrl Pts',(-4.80734470112666,-4.89535635028057,
8.));
#244340=CARTESIAN_POINT('Ctrl Pts',(-4.90085472814102,-4.81688448629847,
8.));
#244341=CARTESIAN_POINT('Ctrl Pts',(-4.9922160791375,-4.73575833801607,
8.));
#244342=CARTESIAN_POINT('Ctrl Pts',(-5.08136863104384,-4.65211150438784,
8.));
#244343=CARTESIAN_POINT('Ctrl Pts',(-5.16684420744904,-4.57191457041387,
8.));
#244344=CARTESIAN_POINT('Ctrl Pts',(-5.25028943769945,-4.48940047532547,
8.));
#244345=CARTESIAN_POINT('Ctrl Pts',(-5.33164630104632,-4.4046799163009,
8.));
#244346=CARTESIAN_POINT('Ctrl Pts',(-5.36052043404078,-4.3746119836397,
8.));
#244347=CARTESIAN_POINT('Ctrl Pts',(-5.38911990294402,-4.34427800399018,
8.));
#244348=CARTESIAN_POINT('Ctrl Pts',(-5.41743426293231,-4.31369271508244,
8.));
#244349=CARTESIAN_POINT('Ctrl Pts',(-5.54469908345851,-4.17622072895257,
8.));
#244350=CARTESIAN_POINT('Ctrl Pts',(-5.66626061200855,-4.03361876143901,
8.));
#244351=CARTESIAN_POINT('Ctrl Pts',(-5.78192961588972,-3.88639015566724,
8.));
#244352=CARTESIAN_POINT('Ctrl Pts',(-5.89884602501638,-3.73757379752478,
8.));
#244353=CARTESIAN_POINT('Ctrl Pts',(-6.00974262846789,-3.58402994987003,
8.));
#244354=CARTESIAN_POINT('Ctrl Pts',(-6.11439363561345,-3.42623394506887,
8.));
#244355=CARTESIAN_POINT('Ctrl Pts',(-6.20326627145087,-3.29222905344095,
8.));
#244356=CARTESIAN_POINT('Ctrl Pts',(-6.2876342928174,-3.15515659780525,
7.99999999999999));
#244357=CARTESIAN_POINT('Ctrl Pts',(-6.36733843599083,-3.01528734055045,
8.));
#244358=CARTESIAN_POINT('Ctrl Pts',(-6.38616415319831,-2.98225092640356,
8.));
#244359=CARTESIAN_POINT('Ctrl Pts',(-6.40473029313281,-2.94905712598991,
8.));
#244360=CARTESIAN_POINT('Ctrl Pts',(-6.42303229992168,-2.91571354682276,
8.));
#244361=CARTESIAN_POINT('Ctrl Pts',(-6.4370381909391,-2.890196862159,8.));
#244362=CARTESIAN_POINT('Ctrl Pts',(-6.45088590547151,-2.86459878170226,
8.));
#244363=CARTESIAN_POINT('Ctrl Pts',(-6.46457090104649,-2.83892831167736,
8.));
#244364=CARTESIAN_POINT('Ctrl Pts',(-6.50871475005265,-2.75612277867679,
8.));
#244365=CARTESIAN_POINT('Ctrl Pts',(-6.55117967921877,-2.67253853642597,
8.));
#244366=CARTESIAN_POINT('Ctrl Pts',(-6.59194388268187,-2.58823590697107,
8.));
#244367=CARTESIAN_POINT('Ctrl Pts',(-6.67487547307193,-2.41672878697819,
8.));
#244368=CARTESIAN_POINT('Ctrl Pts',(-6.75077053581255,-2.24225053131111,
8.));
#244369=CARTESIAN_POINT('Ctrl Pts',(-6.81961261254839,-2.06524773591551,
8.));
#244370=CARTESIAN_POINT('Ctrl Pts',(-6.88950151585512,-1.88555340014043,
8.));
#244371=CARTESIAN_POINT('Ctrl Pts',(-6.9521216439269,-1.70325663984402,
8.));
#244372=CARTESIAN_POINT('Ctrl Pts',(-7.00741369037057,-1.51879182789295,
8.));
#244373=CARTESIAN_POINT('Ctrl Pts',(-7.0628309406438,-1.3339093120882,8.));
#244374=CARTESIAN_POINT('Ctrl Pts',(-7.11088715402154,-1.14684829515692,
8.));
#244375=CARTESIAN_POINT('Ctrl Pts',(-7.15147618870233,-0.958022046524551,
8.));
#244376=CARTESIAN_POINT('Ctrl Pts',(-7.19180261574612,-0.770417487822679,
8.));
#244377=CARTESIAN_POINT('Ctrl Pts',(-7.2247583831861,-0.581069823050405,
8.));
#244378=CARTESIAN_POINT('Ctrl Pts',(-7.25019015456882,-0.390370100156946,
8.));
#244379=CARTESIAN_POINT('Ctrl Pts',(-7.25461100843692,-0.357220399536,8.));
#244380=CARTESIAN_POINT('Ctrl Pts',(-7.25880438016642,-0.324029821772479,
8.));
#244381=CARTESIAN_POINT('Ctrl Pts',(-7.26276930380526,-0.290800398970626,
8.));
#244382=CARTESIAN_POINT('Ctrl Pts',(-7.26536291111864,-0.269063770009185,
8.));
#244383=CARTESIAN_POINT('Ctrl Pts',(-7.2678582400438,-0.247314718960559,
8.));
#244384=CARTESIAN_POINT('Ctrl Pts',(-7.27025432548459,-0.225561724677436,
8.));
#244385=CARTESIAN_POINT('Ctrl Pts',(-7.29190456618673,-0.029008816252474,
8.));
#244386=CARTESIAN_POINT('Ctrl Pts',(-7.30547920730303,0.168056767898447,
8.));
#244387=CARTESIAN_POINT('Ctrl Pts',(-7.31093639138176,0.365179631119353,
8.));
#244388=CARTESIAN_POINT('Ctrl Pts',(-7.31601373382377,0.548581961934194,
8.));
#244389=CARTESIAN_POINT('Ctrl Pts',(-7.31406402678812,0.732034590064997,
8.));
#244390=CARTESIAN_POINT('Ctrl Pts',(-7.30501644905688,0.915186995232694,
8.));
#244391=CARTESIAN_POINT('Ctrl Pts',(-7.29543570235443,1.10913247478293,
8.));
#244392=CARTESIAN_POINT('Ctrl Pts',(-7.27789678584438,1.30274173829146,
8.));
#244393=CARTESIAN_POINT('Ctrl Pts',(-7.25262567498423,1.49556132410732,
8.));
#244394=CARTESIAN_POINT('Ctrl Pts',(-7.22706505774481,1.69058985516706,
8.));
#244395=CARTESIAN_POINT('Ctrl Pts',(-7.19359401339139,1.88481121070243,
8.));
#244396=CARTESIAN_POINT('Ctrl Pts',(-7.15239307289344,2.07775770668224,
8.00000000000001));
#244397=CARTESIAN_POINT('Ctrl Pts',(-7.12126212790101,2.22354580472647,
8.00000000000001));
#244398=CARTESIAN_POINT('Ctrl Pts',(-7.08571697074218,2.36860617775617,
8.));
#244399=CARTESIAN_POINT('Ctrl Pts',(-7.04581601192821,2.51273388279635,
8.));
#244400=CARTESIAN_POINT('Ctrl Pts',(-7.03758572487512,2.54246280210164,
8.));
#244401=CARTESIAN_POINT('Ctrl Pts',(-7.0291688248226,2.5721560492647,8.));
#244402=CARTESIAN_POINT('Ctrl Pts',(-7.02057375510083,2.60178484484585,
8.));
#244403=CARTESIAN_POINT('Ctrl Pts',(-6.96487859664556,2.79377636069724,
8.));
#244404=CARTESIAN_POINT('Ctrl Pts',(-6.90165155752994,2.98326793251129,
8.));
#244405=CARTESIAN_POINT('Ctrl Pts',(-6.83116652485267,3.16979076589306,
8.));
#244406=CARTESIAN_POINT('Ctrl Pts',(-6.7599815615844,3.35816580863119,8.));
#244407=CARTESIAN_POINT('Ctrl Pts',(-6.68139363798646,3.54351357239222,
8.));
#244408=CARTESIAN_POINT('Ctrl Pts',(-6.59563147485587,3.72535328419925,
8.));
#244409=CARTESIAN_POINT('Ctrl Pts',(-6.50963684921469,3.90768588138123,
8.00000000000001));
#244410=CARTESIAN_POINT('Ctrl Pts',(-6.41642887221547,4.08649212780057,
8.00000000000001));
#244411=CARTESIAN_POINT('Ctrl Pts',(-6.31618684025996,4.26127846250173,
8.00000000000001));
#244412=CARTESIAN_POINT('Ctrl Pts',(-6.27693611103826,4.32971772855785,
8.00000000000001));
#244413=CARTESIAN_POINT('Ctrl Pts',(-6.23660638793653,4.39754050986302,
8.));
#244414=CARTESIAN_POINT('Ctrl Pts',(-6.19520638596164,4.46471642251084,
8.));
#244415=CARTESIAN_POINT('Ctrl Pts',(-6.08977872012769,4.63578403924718,
8.));
#244416=CARTESIAN_POINT('Ctrl Pts',(-5.97741342575072,4.80265872580366,
8.00000000000001));
#244417=CARTESIAN_POINT('Ctrl Pts',(-5.85843694593526,4.96505810776332,
8.));
#244418=CARTESIAN_POINT('Ctrl Pts',(-5.83953977033486,4.99085219448575,
8.));
#244419=CARTESIAN_POINT('Ctrl Pts',(-5.82047572315112,5.0165333219891,8.));
#244420=CARTESIAN_POINT('Ctrl Pts',(-5.80124601398966,5.04210028898929,
8.));
#244421=CARTESIAN_POINT('Ctrl Pts',(-5.78077292230514,5.06932040215351,
8.));
#244422=CARTESIAN_POINT('Ctrl Pts',(-5.76011205307566,5.09641111474705,
8.00000000000001));
#244423=CARTESIAN_POINT('Ctrl Pts',(-5.73926483449688,5.12337095070669,
8.));
#244424=CARTESIAN_POINT('Ctrl Pts',(-5.71429336715346,5.15566430728594,
8.));
#244425=CARTESIAN_POINT('Ctrl Pts',(-5.68904997949879,5.18777534729725,
8.));
#244426=CARTESIAN_POINT('Ctrl Pts',(-5.66356734128388,5.21966427514444,
8.));
#244427=CARTESIAN_POINT('Ctrl Pts',(-5.53736200954869,5.37759740136523,
8.00000000000001));
#244428=CARTESIAN_POINT('Ctrl Pts',(-5.40516318792086,5.5302553487043,8.));
#244429=CARTESIAN_POINT('Ctrl Pts',(-5.26739364824614,5.67740877299484,
8.));
#244430=CARTESIAN_POINT('Ctrl Pts',(-5.12711751743733,5.82723951964233,
8.));
#244431=CARTESIAN_POINT('Ctrl Pts',(-4.98106582098125,5.971364160092,8.));
#244432=CARTESIAN_POINT('Ctrl Pts',(-4.82963500543593,6.10951954978689,
8.));
#244433=CARTESIAN_POINT('Ctrl Pts',(-4.67771471353531,6.24812150510563,
8.));
#244434=CARTESIAN_POINT('Ctrl Pts',(-4.52038003859389,6.38071607588409,
8.));
#244435=CARTESIAN_POINT('Ctrl Pts',(-4.35798729149729,6.50700863540348,
8.));
#244436=CARTESIAN_POINT('Ctrl Pts',(-4.19674147632236,6.63240922794422,
8.));
#244437=CARTESIAN_POINT('Ctrl Pts',(-4.03050829304627,6.75159697672051,
8.));
#244438=CARTESIAN_POINT('Ctrl Pts',(-3.85960026731181,6.86424773665911,
8.));
#244439=CARTESIAN_POINT('Ctrl Pts',(-3.71651503581681,6.95855963333356,
8.));
#244440=CARTESIAN_POINT('Ctrl Pts',(-3.57015237858456,7.04828919588474,
8.));
#244441=CARTESIAN_POINT('Ctrl Pts',(-3.42067962509762,7.13322310757501,
7.99999999999999));
#244442=CARTESIAN_POINT('Ctrl Pts',(4.60640650704272,-6.46396313977181,
7.32419035487299));
#244443=CARTESIAN_POINT('Ctrl Pts',(5.68304415359234,-5.69672795305586,
7.3772077233627));
#244444=CARTESIAN_POINT('Ctrl Pts',(7.44170011697942,-3.61976711392297,
7.48320988046067));
#244445=CARTESIAN_POINT('Ctrl Pts',(8.2695054703986,0.400329493614926,7.64219682616689));
#244446=CARTESIAN_POINT('Ctrl Pts',(7.06153867496872,4.28794777733252,7.80115119199166));
#244447=CARTESIAN_POINT('Ctrl Pts',(3.18594271746802,8.15085724155371,8.01309034642465));
#244448=CARTESIAN_POINT('Ctrl Pts',(-4.27253803917999,8.36171192239284,
8.27801428946594));
#244449=CARTESIAN_POINT('Ctrl Pts',(-9.34881640263045,0.90337690149306,
8.59592302111545));
#244450=CARTESIAN_POINT('Ctrl Pts',(-6.40738163527747,-5.9571513384547,
8.86084696415672));
#244451=CARTESIAN_POINT('Ctrl Pts',(-1.39918391556983,-8.14339202368617,
9.07278611858973));
#244452=CARTESIAN_POINT('Ctrl Pts',(2.67537291108373,-7.83708223431333,
9.2317404844145));
#244453=CARTESIAN_POINT('Ctrl Pts',(6.08005709651601,-5.59529991221756,
9.39069485023925));
#244454=CARTESIAN_POINT('Ctrl Pts',(8.71857430285288,-0.789859642577828,
9.60263400467228));
#244455=CARTESIAN_POINT('Ctrl Pts',(7.21254263612409,4.96500730727687,9.81457315910527));
#244456=CARTESIAN_POINT('Ctrl Pts',(2.56073236468874,7.84748751803708,10.0265123135383));
#244457=CARTESIAN_POINT('Ctrl Pts',(-2.86903399551457,8.2653855894407,10.2384514679713));
#244458=CARTESIAN_POINT('Ctrl Pts',(-8.69013980172793,3.57271240080031,
10.5033754110126));
#244459=CARTESIAN_POINT('Ctrl Pts',(-7.68563380952286,-5.39282503599071,
10.8212841426621));
#244460=CARTESIAN_POINT('Ctrl Pts',(-0.995348383535201,-8.69250838977446,
11.0862080857034));
#244461=CARTESIAN_POINT('Ctrl Pts',(4.2336755651751,-7.09606290023127,11.2981472401364));
#244462=CARTESIAN_POINT('Ctrl Pts',(7.12846088456057,-4.21382949912462,
11.4571016059612));
#244463=CARTESIAN_POINT('Ctrl Pts',(8.25773673872998,-0.296618493249961,
11.6160559717859));
#244464=CARTESIAN_POINT('Ctrl Pts',(7.13669833548613,5.06972137834538,11.8279951262189));
#244465=CARTESIAN_POINT('Ctrl Pts',(2.25043748671926,8.46216402683687,12.0399342806519));
#244466=CARTESIAN_POINT('Ctrl Pts',(-3.15802887272445,7.6267562205539,12.251873435085));
#244467=CARTESIAN_POINT('Ctrl Pts',(-7.55455441577774,4.41319586680862,
12.4638125895179));
#244468=CARTESIAN_POINT('Ctrl Pts',(-8.92501441489603,-2.93721198242924,
12.7287365325592));
#244469=CARTESIAN_POINT('Ctrl Pts',(-2.3315165987433,-9.0948059072455,13.0466452642087));
#244470=CARTESIAN_POINT('Ctrl Pts',(4.89668847883403,-7.25071229477944,
13.31156920725));
#244471=CARTESIAN_POINT('Ctrl Pts',(7.83083558801256,-2.63745359024292,
13.523508361683));
#244472=CARTESIAN_POINT('Ctrl Pts',(8.1555641278621,1.43459714924663,13.6824627275078));
#244473=CARTESIAN_POINT('Ctrl Pts',(6.46603855843502,5.1447596198217,13.8414170933326));
#244474=CARTESIAN_POINT('Ctrl Pts',(2.12463370076545,8.49237698071761,14.0533562477656));
#244475=CARTESIAN_POINT('Ctrl Pts',(-3.7934454125899,7.89192369888149,14.2652954021985));
#244476=CARTESIAN_POINT('Ctrl Pts',(-7.35881389526889,3.74010908684348,
14.4772345566316));
#244477=CARTESIAN_POINT('Ctrl Pts',(-8.60890508199618,-1.56023792552856,
14.6891737110646));
#244478=CARTESIAN_POINT('Ctrl Pts',(-4.86995472333722,-8.03533682977006,
14.9540976541059));
#244479=CARTESIAN_POINT('Ctrl Pts',(4.1432659185206,-8.42524847071499,15.2720063857554));
#244480=CARTESIAN_POINT('Ctrl Pts',(8.43507380939552,-2.32377204262004,
15.5369303287966));
#244481=CARTESIAN_POINT('Ctrl Pts',(7.66400379406276,3.08888221979113,15.7488694832297));
#244482=CARTESIAN_POINT('Ctrl Pts',(5.26259331597973,6.39346594447912,15.9078238490544));
#244483=CARTESIAN_POINT('Ctrl Pts',(1.56635676098601,8.1132442764234,16.0667782148792));
#244484=CARTESIAN_POINT('Ctrl Pts',(-3.90866261554707,7.83306400513209,
16.2787173693122));
#244485=CARTESIAN_POINT('Ctrl Pts',(-8.01396100145449,3.5283306005865,16.4906565237452));
#244486=CARTESIAN_POINT('Ctrl Pts',(-8.02249192943588,-1.94426880137432,
16.7025956781782));
#244487=CARTESIAN_POINT('Ctrl Pts',(-5.52527675051475,-6.78372360311353,
16.9145348326112));
#244488=CARTESIAN_POINT('Ctrl Pts',(1.52591029648008,-9.27117547791387,
17.1794587756525));
#244489=CARTESIAN_POINT('Ctrl Pts',(8.62653528067062,-3.70598884469431,
17.4973675073021));
#244490=CARTESIAN_POINT('Ctrl Pts',(7.91903429724152,3.72011861030341,17.7622914503433));
#244491=CARTESIAN_POINT('Ctrl Pts',(3.81337169451136,7.33050774795007,17.9742306047763));
#244492=CARTESIAN_POINT('Ctrl Pts',(-0.159909493655665,8.27923451452099,
18.1331849706011));
#244493=CARTESIAN_POINT('Ctrl Pts',(-4.08621421445045,7.18199551553807,
18.2921393364258));
#244494=CARTESIAN_POINT('Ctrl Pts',(-8.06321083680452,3.4086897999003,18.5040784908588));
#244495=CARTESIAN_POINT('Ctrl Pts',(-8.38246493369623,-2.53119920101162,
18.7160176452919));
#244496=CARTESIAN_POINT('Ctrl Pts',(-4.83005780802961,-6.69410931349035,
18.9279567997249));
#244497=CARTESIAN_POINT('Ctrl Pts',(0.214145694079805,-8.74652678009534,
19.1398959541579));
#244498=CARTESIAN_POINT('Ctrl Pts',(7.18832724386593,-6.05070643894309,
19.4048198971992));
#244499=CARTESIAN_POINT('Ctrl Pts',(8.96335141509527,2.79460116567021,19.7227286288486));
#244500=CARTESIAN_POINT('Ctrl Pts',(3.59661084838262,7.97588722844733,19.98765257189));
#244501=CARTESIAN_POINT('Ctrl Pts',(-1.87020571352034,8.04863206466617,
20.1995917263229));
#244502=CARTESIAN_POINT('Ctrl Pts',(-5.50554978380011,6.18548436023368,
20.3585460921477));
#244503=CARTESIAN_POINT('Ctrl Pts',(-7.77469467530229,2.79862982500579,
20.5175004579725));
#244504=CARTESIAN_POINT('Ctrl Pts',(-8.34207484510865,-2.65411424571596,
20.7294396124055));
#244505=CARTESIAN_POINT('Ctrl Pts',(-4.72183113573663,-7.37407611063491,
20.9413787668385));
#244506=CARTESIAN_POINT('Ctrl Pts',(0.684004653885784,-8.22634156617198,
21.1533179212715));
#244507=CARTESIAN_POINT('Ctrl Pts',(5.85063630387345,-6.50520129842388,
21.3652570757045));
#244508=CARTESIAN_POINT('Ctrl Pts',(9.39558383634547,0.0781111347793227,
21.6301810187458));
#244509=CARTESIAN_POINT('Ctrl Pts',(4.99181938924929,7.95193080017495,21.9480897503953));
#244510=CARTESIAN_POINT('Ctrl Pts',(-2.45456906825707,8.39794482982405,
22.2130136934366));
#244511=CARTESIAN_POINT('Ctrl Pts',(-6.65484510472912,4.89807963954436,
22.4249528478696));
#244512=CARTESIAN_POINT('Ctrl Pts',(-8.20487797662277,1.11860295964548,
22.5839072136944));
#244513=CARTESIAN_POINT('Ctrl Pts',(-7.72616986326117,-2.92993266742093,
22.7428615795191));
#244514=CARTESIAN_POINT('Ctrl Pts',(-4.61121512984712,-7.44118472939463,
22.9548007339522));
#244515=CARTESIAN_POINT('Ctrl Pts',(1.20841048463845,-8.67251012455243,
23.1667398883851));
#244516=CARTESIAN_POINT('Ctrl Pts',(5.86929163264628,-5.80447875875298,
23.3786790428182));
#244517=CARTESIAN_POINT('Ctrl Pts',(8.67494461835349,-1.13706858267993,
23.5906181972512));
#244518=CARTESIAN_POINT('Ctrl Pts',(7.08673429158096,6.16938360419446,23.8555421402925));
#244519=CARTESIAN_POINT('Ctrl Pts',(-1.37909372589059,9.28706437798646,
24.173450871942));
#244520=CARTESIAN_POINT('Ctrl Pts',(-7.3259293348859,4.78342409324861,24.4383748149832));
#244521=CARTESIAN_POINT('Ctrl Pts',(-8.24074907476951,-0.606796679244106,
24.6503139694162));
#244522=CARTESIAN_POINT('Ctrl Pts',(-6.96042785497538,-4.48594909336698,
24.809268335241));
#244523=CARTESIAN_POINT('Ctrl Pts',(-3.96396384261985,-7.2501859869929,
24.9682227010657));
#244524=CARTESIAN_POINT('Ctrl Pts',(1.33608342634073,-8.65155571146394,
25.1801618554988));
#244525=CARTESIAN_POINT('Ctrl Pts',(6.55781433047578,-5.80239252092228,
25.3921010099317));
#244526=CARTESIAN_POINT('Ctrl Pts',(8.23342939650299,-0.592619863543954,
25.6040401643649));
#244527=CARTESIAN_POINT('Ctrl Pts',(7.32953114506682,4.77761052061731,25.8159793187978));
#244528=CARTESIAN_POINT('Ctrl Pts',(1.37155632862688,9.29526385922294,26.0809032618391));
#244529=CARTESIAN_POINT('Ctrl Pts',(-7.08712800903743,6.15825306797093,
26.3988119934886));
#244530=CARTESIAN_POINT('Ctrl Pts',(-8.67598906217926,-1.13030989934556,
26.6637359365299));
#244531=CARTESIAN_POINT('Ctrl Pts',(-5.86563283358155,-5.82000850384829,
26.8756750909629));
#244532=CARTESIAN_POINT('Ctrl Pts',(-2.37036010048857,-7.93427300933166,
27.0346294567876));
#244533=CARTESIAN_POINT('Ctrl Pts',(1.70357150606366,-8.08554576483948,
27.1935838226124));
#244534=CARTESIAN_POINT('Ctrl Pts',(6.64117659469234,-5.70344707951407,
27.4055229770454));
#244535=CARTESIAN_POINT('Ctrl Pts',(8.75512182332181,-0.14328160608686,
27.6174621314784));
#244536=CARTESIAN_POINT('Ctrl Pts',(6.64006524501561,4.9040892601789,27.8294012859115));
#244537=CARTESIAN_POINT('Ctrl Pts',(2.46108587685203,8.39587073506834,28.0413404403444));
#244538=CARTESIAN_POINT('Ctrl Pts',(-5.00287752104787,7.95325804212126,
28.3062643833857));
#244539=CARTESIAN_POINT('Ctrl Pts',(-9.38864462872237,0.0693995765018132,
28.6241731150352));
#244540=CARTESIAN_POINT('Ctrl Pts',(-5.85582497657862,-6.50074615096535,
28.8890970580765));
#244541=CARTESIAN_POINT('Ctrl Pts',(-0.671126025509802,-8.2357596723763,
29.1010362125095));
#244542=CARTESIAN_POINT('Ctrl Pts',(3.359051199195,-7.56888830897797,29.2599905783343));
#244543=CARTESIAN_POINT('Ctrl Pts',(6.55226367610338,-5.03448576424663,
29.4189449441591));
#244544=CARTESIAN_POINT('Ctrl Pts',(8.75410428400366,-0.0139045135065831,
29.630884098592));
#244545=CARTESIAN_POINT('Ctrl Pts',(6.74416934134095,5.58469942388712,29.842823253025));
#244546=CARTESIAN_POINT('Ctrl Pts',(1.85506979875823,8.04358589011153,30.0547624074581));
#244547=CARTESIAN_POINT('Ctrl Pts',(-3.59031142780148,7.97854955142952,
30.266701561891));
#244548=CARTESIAN_POINT('Ctrl Pts',(-8.97261505059773,2.78841821270769,
30.5316255049324));
#244549=CARTESIAN_POINT('Ctrl Pts',(-7.17739052902341,-6.05281169866873,
30.8495342365819));
#244550=CARTESIAN_POINT('Ctrl Pts',(-0.220984594540438,-8.74651659145448,
31.1144581796232));
#244551=CARTESIAN_POINT('Ctrl Pts',(4.84596599019363,-6.69288884900557,
31.3263973340562));
#244552=CARTESIAN_POINT('Ctrl Pts',(7.47389207938856,-3.56542176723172,
31.4853516998809));
#244553=CARTESIAN_POINT('Ctrl Pts',(8.25152748533976,0.436463458113405,
31.6443060657057));
#244554=CARTESIAN_POINT('Ctrl Pts',(6.65926109162368,5.6823214326799,31.8562452201387));
#244555=CARTESIAN_POINT('Ctrl Pts',(1.49154661474766,8.62832408152842,32.0681843745717));
#244556=CARTESIAN_POINT('Ctrl Pts',(-3.82158839556387,7.3168312857929,32.2801235290048));
#244557=CARTESIAN_POINT('Ctrl Pts',(-7.91598016080529,3.7262376718286,32.4920626834377));
#244558=CARTESIAN_POINT('Ctrl Pts',(-8.6295517363744,-3.71671007806775,
32.7569866264791));
#244559=CARTESIAN_POINT('Ctrl Pts',(-1.51623294465423,-9.26566251938852,
33.0748953581285));
#244560=CARTESIAN_POINT('Ctrl Pts',(5.52007482625293,-6.78816327058959,
33.3398193011698));
#244561=CARTESIAN_POINT('Ctrl Pts',(8.03378319654136,-1.93299639788226,
33.5517584556028));
#244562=CARTESIAN_POINT('Ctrl Pts',(7.996312256756,2.15180981618979,33.7107128214276));
#244563=CARTESIAN_POINT('Ctrl Pts',(5.98459030406109,5.6976210021485,33.8696671872523));
#244564=CARTESIAN_POINT('Ctrl Pts',(1.36355987815356,8.64726775400164,34.0816063416853));
#244565=CARTESIAN_POINT('Ctrl Pts',(-4.47800684634566,7.524635701742,34.2935454961184));
#244566=CARTESIAN_POINT('Ctrl Pts',(-7.66135182018962,3.07314923444068,
34.5054846505514));
#244567=CARTESIAN_POINT('Ctrl Pts',(-8.43673296636848,-2.31713744680997,
34.7174238049844));
#244568=CARTESIAN_POINT('Ctrl Pts',(-4.13858529690325,-8.43535468818172,
34.9823477480256));
#244569=CARTESIAN_POINT('Ctrl Pts',(4.87372117073586,-8.02485552614977,
35.3002564796752));
#244570=CARTESIAN_POINT('Ctrl Pts',(8.60784050446359,-1.56699346690693,
35.5651804227164));
#244571=CARTESIAN_POINT('Ctrl Pts',(7.36006095721478,3.75601520621774,35.7771195771495));
#244572=CARTESIAN_POINT('Ctrl Pts',(4.67520386931402,6.83474681118095,35.9360739429742));
#244573=CARTESIAN_POINT('Ctrl Pts',(0.841084144012684,8.22014498985731,
36.095028308799));
#244574=CARTESIAN_POINT('Ctrl Pts',(-4.58755362703686,7.45579552226102,
36.306967463232));
#244575=CARTESIAN_POINT('Ctrl Pts',(-8.29514971181719,2.80413605561278,
36.518906617665));
#244576=CARTESIAN_POINT('Ctrl Pts',(-7.81858964795988,-2.64768084305508,
36.730845772098));
#244577=CARTESIAN_POINT('Ctrl Pts',(-4.90226342584214,-7.24675116151151,
36.942784926531));
#244578=CARTESIAN_POINT('Ctrl Pts',(2.3416444799405,-9.09943943903892,37.2077088695723));
#244579=CARTESIAN_POINT('Ctrl Pts',(8.92105959839902,-2.926800284862,37.5256176012218));
#244580=CARTESIAN_POINT('Ctrl Pts',(7.55813883548847,4.40737155446349,37.7905415442631));
#244581=CARTESIAN_POINT('Ctrl Pts',(3.14863238283442,7.63965062296849,38.0024806986961));
#244582=CARTESIAN_POINT('Ctrl Pts',(-0.893100355538415,8.23247635572276,
38.1614350645209));
#244583=CARTESIAN_POINT('Ctrl Pts',(-4.70669974170726,6.79155238019986,
38.3203894303456));
#244584=CARTESIAN_POINT('Ctrl Pts',(-8.33360149172359,2.68060092662989,
38.5323285847787));
#244585=CARTESIAN_POINT('Ctrl Pts',(-8.12512401220396,-3.26420703175445,
38.7442677392116));
#244586=CARTESIAN_POINT('Ctrl Pts',(-4.21772352936819,-7.09586965492464,
38.9562068936447));
#244587=CARTESIAN_POINT('Ctrl Pts',(0.988540998120691,-8.69312232677373,
39.1681460480777));
#244588=CARTESIAN_POINT('Ctrl Pts',(7.6963332375881,-5.38976360067576,39.4330699911189));
#244589=CARTESIAN_POINT('Ctrl Pts',(8.68037796208286,3.57805851000828,39.7509787227685));
#244590=CARTESIAN_POINT('Ctrl Pts',(2.87552219543382,8.26327772613146,40.0159026658097));
#244591=CARTESIAN_POINT('Ctrl Pts',(-2.57622614712117,7.8511913976253,40.2278418202428));
#244592=CARTESIAN_POINT('Ctrl Pts',(-6.03212460513054,5.67316207601861,
40.3867961860675));
#244593=CARTESIAN_POINT('Ctrl Pts',(-7.99214890082263,2.09851426934996,
40.5457505518923));
#244594=CARTESIAN_POINT('Ctrl Pts',(-8.07399845725793,-3.38305838892906,
40.7576897063253));
#244595=CARTESIAN_POINT('Ctrl Pts',(-4.04965474926068,-7.76356774760414,
40.9696288607583));
#244596=CARTESIAN_POINT('Ctrl Pts',(1.41044471838918,-8.13333902073644,
41.1815680151913));
#244597=CARTESIAN_POINT('Ctrl Pts',(6.40419069553413,-5.96103435893907,
41.3935071696244));
#244598=CARTESIAN_POINT('Ctrl Pts',(9.35168213791974,0.910570242477697,
41.6584311126656));
#244599=CARTESIAN_POINT('Ctrl Pts',(4.26736293265541,8.36307825305098,41.9763398443152));
#244600=CARTESIAN_POINT('Ctrl Pts',(-3.1892505363311,8.14733500551711,42.2412637873563));
#244601=CARTESIAN_POINT('Ctrl Pts',(-7.06278901428503,4.28895778283618,
42.4532029417895));
#244602=CARTESIAN_POINT('Ctrl Pts',(-8.27173191327942,0.386970732009184,
42.6121573076141));
#244603=CARTESIAN_POINT('Ctrl Pts',(-7.4360706647855,-3.60320125165142,
42.771111673439));
#244604=CARTESIAN_POINT('Ctrl Pts',(-3.93352600370737,-7.82060792578586,
42.9830508278718));
#244605=CARTESIAN_POINT('Ctrl Pts',(1.9723322591907,-8.53127148901054,43.194989982305));
#244606=CARTESIAN_POINT('Ctrl Pts',(6.36066488331213,-5.26141617552407,
43.4069291367379));
#244607=CARTESIAN_POINT('Ctrl Pts',(8.7415851819939,-0.363699875120048,
43.618868291171));
#244608=CARTESIAN_POINT('Ctrl Pts',(6.51202680730175,6.77322698838271,43.8837922342122));
#244609=CARTESIAN_POINT('Ctrl Pts',(-2.19681403260211,9.12827871900386,
44.2017009658618));
#244610=CARTESIAN_POINT('Ctrl Pts',(-7.72106968360267,4.11527272687538,
44.466624908903));
#244611=CARTESIAN_POINT('Ctrl Pts',(-8.15453306347553,-1.33481760549541,
44.6785640633361));
#244612=CARTESIAN_POINT('Ctrl Pts',(-6.53542671722701,-5.0852229859026,
44.8375184291608));
#244613=CARTESIAN_POINT('Ctrl Pts',(-3.30575106693872,-7.5729925442337,
44.9964727949856));
#244614=CARTESIAN_POINT('Ctrl Pts',(2.09764544585784,-8.49908340553139,
45.2084119494186));
#244615=CARTESIAN_POINT('Ctrl Pts',(7.04629283569648,-5.1983117483911,45.4203511038516));
#244616=CARTESIAN_POINT('Ctrl Pts',(8.2535510691205,0.139472862184186,45.6322902582846));
#244617=CARTESIAN_POINT('Ctrl Pts',(6.87722625139314,5.40845155107887,45.8442294127176));
#244618=CARTESIAN_POINT('Ctrl Pts',(0.542283475490215,9.38024656431713,
46.1091533557589));
#244619=CARTESIAN_POINT('Ctrl Pts',(-7.60506456392797,5.50585663127388,
46.4270620874084));
#244620=CARTESIAN_POINT('Ctrl Pts',(-8.54165908809657,-1.89484740766892,
46.6919860304496));
#244621=CARTESIAN_POINT('Ctrl Pts',(-5.32669771709283,-6.31699603878098,
46.9039251848827));
#244622=CARTESIAN_POINT('Ctrl Pts',(-1.65778605748533,-8.11313999510693,
47.0628795507074));
#244623=CARTESIAN_POINT('Ctrl Pts',(2.41351956808077,-7.90272924286775,
47.2218339165322));
#244624=CARTESIAN_POINT('Ctrl Pts',(7.12055709626584,-5.09236701245357,
47.4337730709653));
#244625=CARTESIAN_POINT('Ctrl Pts',(8.73336369099004,0.633282244141819,
47.6457122253982));
#244626=CARTESIAN_POINT('Ctrl Pts',(6.17926360329026,5.47332250565583,47.8576513798313));
#244627=CARTESIAN_POINT('Ctrl Pts',(1.70724159043718,8.5809623728985,48.0695905342643));
#244628=CARTESIAN_POINT('Ctrl Pts',(-5.68811526363237,7.478532056681,48.3345144773055));
#244629=CARTESIAN_POINT('Ctrl Pts',(-9.35784467962813,-0.763025043894934,
48.6524232089551));
#244630=CARTESIAN_POINT('Ctrl Pts',(-5.25659207975775,-6.99418518361079,
48.9173471519963));
#244631=CARTESIAN_POINT('Ctrl Pts',(0.0614822199421796,-8.26283047507858,
49.1292863064293));
#244632=CARTESIAN_POINT('Ctrl Pts',(4.01669042628314,-7.24137371028467,
49.2882406722541));
#244633=CARTESIAN_POINT('Ctrl Pts',(6.97270151424152,-4.43391923526801,
49.4471950380788));
#244634=CARTESIAN_POINT('Ctrl Pts',(8.7208829698701,0.762059955998786,49.6591341925119));
#244635=CARTESIAN_POINT('Ctrl Pts',(6.22263289279893,6.16048112092758,49.8710733469448));
#244636=CARTESIAN_POINT('Ctrl Pts',(1.13483497661836,8.17635050041949,50.083012501378));
#244637=CARTESIAN_POINT('Ctrl Pts',(-4.28335032160907,7.62892516122616,
50.2949516558109));
#244638=CARTESIAN_POINT('Ctrl Pts',(-9.18444949980501,1.98216658248081,
50.5598755988522));
#244639=CARTESIAN_POINT('Ctrl Pts',(-6.61265846080802,-6.6651490865816,
50.8777843305017));
#244640=CARTESIAN_POINT('Ctrl Pts',(0.555122358467198,-8.73167943998994,
51.1427082735429));
#244641=CARTESIAN_POINT('Ctrl Pts',(5.42010995078664,-6.23703099596596,
51.354647427976));
#244642=CARTESIAN_POINT('Ctrl Pts',(7.76049388307317,-2.88894961592975,
51.5136017938007));
#244643=CARTESIAN_POINT('Ctrl Pts',(8.18036633808948,1.16611010039288,51.6725561596255));
#244644=CARTESIAN_POINT('Ctrl Pts',(6.12940620636044,6.25019317366569,51.8844953140585));
#244645=CARTESIAN_POINT('Ctrl Pts',(0.720914936547745,8.72656687444214,
52.0964344684915));
#244646=CARTESIAN_POINT('Ctrl Pts',(-4.45506642661906,6.94931227275606,
52.3083736229245));
#244647=CARTESIAN_POINT('Ctrl Pts',(-8.21509575723348,3.00994863622323,
52.5203127773576));
#244648=CARTESIAN_POINT('Ctrl Pts',(-8.26616198646753,-4.46695231546649,
52.7852367203988));
#244649=CARTESIAN_POINT('Ctrl Pts',(-0.689014364486892,-9.36358496897353,
53.1031454520484));
#244650=CARTESIAN_POINT('Ctrl Pts',(6.10001021798649,-6.27218159941767,
53.3680693950896));
#244651=CARTESIAN_POINT('Ctrl Pts',(8.17349332006236,-1.2133237285046,53.5800085495226));
#244652=CARTESIAN_POINT('Ctrl Pts',(7.77411785726235,2.85208462952825,53.7389629153473));
#244653=CARTESIAN_POINT('Ctrl Pts',(5.45603467637146,6.20563387590808,53.8979172811722));
#244654=CARTESIAN_POINT('Ctrl Pts',(0.59175287007345,8.734092035894,54.1098564356051));
#244655=CARTESIAN_POINT('Ctrl Pts',(-5.12731989678988,7.09811795026197,
54.3217955900382));
#244656=CARTESIAN_POINT('Ctrl Pts',(-7.90358383695811,2.38199925735514,
54.5337347444712));
#244657=CARTESIAN_POINT('Ctrl Pts',(-8.19815157297799,-3.05579774849325,
54.7456738989042));
#244658=CARTESIAN_POINT('Ctrl Pts',(-3.37463922465833,-8.76897411779567,
55.0105978419453));
#244659=CARTESIAN_POINT('Ctrl Pts',(5.56581319571568,-7.56129537421026,
55.3285065735951));
#244660=CARTESIAN_POINT('Ctrl Pts',(8.71285105812484,-0.797880388621073,
55.5934305166362));
#244661=CARTESIAN_POINT('Ctrl Pts',(6.99818380676628,4.39358292626538,55.8053696710693));
#244662=CARTESIAN_POINT('Ctrl Pts',(4.05101381344076,7.22222834559451,55.964324036894));
#244663=CARTESIAN_POINT('Ctrl Pts',(0.109190979620403,8.26234128571045,
56.1232784027188));
#244664=CARTESIAN_POINT('Ctrl Pts',(-5.2303339633563,7.01983915645279,56.3352175571518));
#244665=CARTESIAN_POINT('Ctrl Pts',(-8.51104360906945,2.05786890845034,
56.5471567115849));
#244666=CARTESIAN_POINT('Ctrl Pts',(-7.55314376961135,-3.33025181111693,
56.7590958660178));
#244667=CARTESIAN_POINT('Ctrl Pts',(-4.24066220519041,-7.65273631812093,
56.9710350204508));
#244668=CARTESIAN_POINT('Ctrl Pts',(3.13894653812266,-8.85607766485711,
57.2359589634921));
#244669=CARTESIAN_POINT('Ctrl Pts',(9.14536228789039,-2.12457357813009,
57.5538676951416));
#244670=CARTESIAN_POINT('Ctrl Pts',(7.13774990105824,5.0599321166944,57.8187916381829));
#244671=CARTESIAN_POINT('Ctrl Pts',(2.45910878514273,7.8886584097735,58.0307307926159));
#244672=CARTESIAN_POINT('Ctrl Pts',(-1.61926122726644,8.12091671367639,
58.1896851584407));
#244673=CARTESIAN_POINT('Ctrl Pts',(-5.29013674173023,6.34764991515613,
58.3486395242654));
#244674=CARTESIAN_POINT('Ctrl Pts',(-8.53839466246798,1.93141185111956,
58.5605786786985));
#244675=CARTESIAN_POINT('Ctrl Pts',(-7.80382662551038,-3.97152083701247,
58.7725178331314));
#244676=CARTESIAN_POINT('Ctrl Pts',(-3.57218967273978,-7.44177525002184,
58.9844569875644));
#244677=CARTESIAN_POINT('Ctrl Pts',(1.75515505625667,-8.57129044086796,
59.1963961419975));
#244678=CARTESIAN_POINT('Ctrl Pts',(8.1437579690245,-4.68639553571003,59.4613200850388));
#244679=CARTESIAN_POINT('Ctrl Pts',(8.32907739304941,4.33335136427322,59.7792288166883));
#244680=CARTESIAN_POINT('Ctrl Pts',(2.13179902823639,8.4856242892802,60.0441527597295));
#244681=CARTESIAN_POINT('Ctrl Pts',(-3.26196795879774,7.59195051083932,
60.2560919141626));
#244682=CARTESIAN_POINT('Ctrl Pts',(-6.51121789057064,5.11618380964859,
60.4150462799873));
#244683=CARTESIAN_POINT('Ctrl Pts',(-8.14669336739134,1.38188037444908,
60.5740006458121));
#244684=CARTESIAN_POINT('Ctrl Pts',(-7.7423680361898,-4.08537297475924,
60.785939800245));
#244685=CARTESIAN_POINT('Ctrl Pts',(-3.34560172894389,-8.09194888955291,
60.9978789546782));
#244686=CARTESIAN_POINT('Ctrl Pts',(2.12578254514033,-7.97631534611332,
61.209818109111));
#244687=CARTESIAN_POINT('Ctrl Pts',(6.90733485360991,-5.36994546651301,
61.4217572635443));
#244688=CARTESIAN_POINT('Ctrl Pts',(9.23416918970506,1.7358618467706,61.6866812065853));
#244689=CARTESIAN_POINT('Ctrl Pts',(3.50931616427147,8.70839619705249,62.004589938235));
#244690=CARTESIAN_POINT('Ctrl Pts',(-3.89882799483674,7.83259388340096,
62.269513881276));
#244691=CARTESIAN_POINT('Ctrl Pts',(-7.41513856994077,3.64607563166662,
62.4814530357093));
#244692=CARTESIAN_POINT('Ctrl Pts',(-8.27347536873333,-0.347707514385417,
62.6404074015339));
#244693=CARTESIAN_POINT('Ctrl Pts',(-7.08743884650086,-4.2481074361057,
62.7993617673587));
#244694=CARTESIAN_POINT('Ctrl Pts',(-3.22487434473777,-8.13847163854236,
63.0113009217918));
#244695=CARTESIAN_POINT('Ctrl Pts',(2.72072892922625,-8.32287942082066,
63.2232400762246));
#244696=CARTESIAN_POINT('Ctrl Pts',(6.80197051142163,-4.67693864526975,
63.4351792306578));
#244697=CARTESIAN_POINT('Ctrl Pts',(8.73941684035996,0.412531675932698,
63.6471183850907));
#244698=CARTESIAN_POINT('Ctrl Pts',(5.88606026343599,7.32375529017553,63.912042328132));
#244699=CARTESIAN_POINT('Ctrl Pts',(-2.99724223890796,8.89764031791383,
64.2299510597815));
#244700=CARTESIAN_POINT('Ctrl Pts',(-8.05543405846353,3.41472821837216,
64.4948750028228));
#244701=CARTESIAN_POINT('Ctrl Pts',(-8.00412909525724,-2.05233158863933,
64.7068141572559));
#244702=CARTESIAN_POINT('Ctrl Pts',(-6.05898232879026,-5.64446882638074,
64.8657685230806));
#244703=CARTESIAN_POINT('Ctrl Pts',(-2.62151725419616,-7.83618870864836,
65.0247228889054));
#244704=CARTESIAN_POINT('Ctrl Pts',(2.84269596503497,-8.2797110336745,65.2366620433383));
#244705=CARTESIAN_POINT('Ctrl Pts',(7.47930683576014,-4.55331275184693,
65.4486011977714));
#244706=CARTESIAN_POINT('Ctrl Pts',(8.20870537006574,0.870467734972957,
65.6605403522044));
#244707=CARTESIAN_POINT('Ctrl Pts',(6.37078765082055,5.99672025367893,65.8724795066374));
#244708=CARTESIAN_POINT('Ctrl Pts',(-0.291257931997344,9.39139317630174,
66.1374034496787));
#244709=CARTESIAN_POINT('Ctrl Pts',(-8.06313827302813,4.81012114802201,
66.4553121813282));
#244710=CARTESIAN_POINT('Ctrl Pts',(-8.34009391566828,-2.64446972925217,
66.7202361243695));
#244711=CARTESIAN_POINT('Ctrl Pts',(-4.74583379392158,-6.76425968799533,
66.9321752788024));
#244712=CARTESIAN_POINT('Ctrl Pts',(-0.932162842170672,-8.22814484734424,
67.0911296446274));
#244713=CARTESIAN_POINT('Ctrl Pts',(3.10446974242751,-7.6577068235964,67.2500840104519));
#244714=CARTESIAN_POINT('Ctrl Pts',(7.54388852932836,-4.44120266009448,
67.4620231648852));
#244715=CARTESIAN_POINT('Ctrl Pts',(8.6428613613827,1.40486124923329,67.6739623193179));
#244716=CARTESIAN_POINT('Ctrl Pts',(5.66982223737212,5.99947279384697,67.885901473751));
#244717=CARTESIAN_POINT('Ctrl Pts',(0.939958826895868,8.69850944202151,
68.0978406281841));
#244718=CARTESIAN_POINT('Ctrl Pts',(-6.32857928004383,6.94493921256201,
68.3627645712253));
#244719=CARTESIAN_POINT('Ctrl Pts',(-9.25338504462195,-1.58944354354721,
68.6806733028749));
#244720=CARTESIAN_POINT('Ctrl Pts',(-4.6159820866088,-7.43256989263452,
68.9455972459161));
#244721=CARTESIAN_POINT('Ctrl Pts',(0.793606342692045,-8.22486083743239,
69.1575364003492));
#244722=CARTESIAN_POINT('Ctrl Pts',(4.6427128645978,-6.85685909553858,69.3164907661738));
#244723=CARTESIAN_POINT('Ctrl Pts',(7.3382534308987,-3.798451248715,69.4754451319988));
#244724=CARTESIAN_POINT('Ctrl Pts',(8.61901727285212,1.53202566838775,69.6873842864315));
#244725=CARTESIAN_POINT('Ctrl Pts',(5.65211232994788,6.68777139916866,69.8993234408648));
#244726=CARTESIAN_POINT('Ctrl Pts',(0.405670874433816,8.24475487152382,
70.1112625952976));
#244727=CARTESIAN_POINT('Ctrl Pts',(-4.94268127029696,7.21925138814969,
70.3232017497307));
#244728=CARTESIAN_POINT('Ctrl Pts',(-9.32397158221413,1.16030971141512,
70.588125692772));
#244729=CARTESIAN_POINT('Ctrl Pts',(-5.99590603536385,-7.22501731502557,
70.9060344244214));
#244730=CARTESIAN_POINT('Ctrl Pts',(1.32691188893416,-8.64811949535424,
71.1709583674628));
#244731=CARTESIAN_POINT('Ctrl Pts',(5.95151754507708,-5.73206742692903,
71.3828975218956));
#244732=CARTESIAN_POINT('Ctrl Pts',(7.9861670350496,-2.18976184285739,71.5418518877206));
#244733=CARTESIAN_POINT('Ctrl Pts',(8.04452003161391,1.88662359923558,71.7008062535452));
#244734=CARTESIAN_POINT('Ctrl Pts',(5.55197452254941,6.76876230204749,71.9127454079784));
#244735=CARTESIAN_POINT('Ctrl Pts',(-0.056676988297962,8.75631944978158,
72.1246845624112));
#244736=CARTESIAN_POINT('Ctrl Pts',(-5.05197385037126,6.52685787508822,
72.3366237168444));
#244737=CARTESIAN_POINT('Ctrl Pts',(-8.45305692825313,2.27051267268757,
72.5485628712773));
#244738=CARTESIAN_POINT('Ctrl Pts',(-7.83028221592002,-5.18317005046361,
72.8134868143186));
#244739=CARTESIAN_POINT('Ctrl Pts',(0.130805184506471,-9.38593239092925,
73.1313955459682));
#244740=CARTESIAN_POINT('Ctrl Pts',(7.95627519325664,-4.97374396463105,
73.4493042776175));
#244741=CARTESIAN_POINT('Ctrl Pts',(8.49225628872148,3.99956479643668,73.7672130092672));
#244742=CARTESIAN_POINT('Ctrl Pts',(1.23306637670374,9.30161229503668,74.0851217409166));
#244743=CARTESIAN_POINT('Ctrl Pts',(-7.1526073352008,6.07890164024892,74.4030304725663));
#244744=CARTESIAN_POINT('Ctrl Pts',(-8.98311340169015,-2.735369255759,74.7209392042156));
#244745=CARTESIAN_POINT('Ctrl Pts',(-3.63348368341516,-7.96286352711625,
74.9858631472571));
#244746=CARTESIAN_POINT('Ctrl Pts',(1.81407828852932,-8.05179690935647,
75.19780230169));
#244747=CARTESIAN_POINT('Ctrl Pts',(6.71443182649054,-5.62074264088269,
75.409741456123));
#244748=CARTESIAN_POINT('Ctrl Pts',(8.75440499161001,-0.0309425844198426,
75.6216806105561));
#244749=CARTESIAN_POINT('Ctrl Pts',(6.57815063855531,5.00015852955729,75.833619764989));
#244750=CARTESIAN_POINT('Ctrl Pts',(3.39836701499377,7.55149140710295,75.9925741308139));
#244751=CARTESIAN_POINT('Ctrl Pts',(-0.62841393059698,8.23906875854624,
76.1515284966386));
#244752=CARTESIAN_POINT('Ctrl Pts',(-5.82198280292298,6.53109349262364,
76.3634676510716));
#244753=CARTESIAN_POINT('Ctrl Pts',(-9.3888942806352,-0.0207020382397817,
76.6283915941129));
#244754=CARTESIAN_POINT('Ctrl Pts',(-5.0440754447665,-7.92717273684912,
76.9463003257624));
#244755=CARTESIAN_POINT('Ctrl Pts',(2.41747718053897,-8.40853690166243,
77.2112242688036));
#244756=CARTESIAN_POINT('Ctrl Pts',(6.61452732186301,-4.93847952898536,
77.4231634232367));
#244757=CARTESIAN_POINT('Ctrl Pts',(8.75574595011106,0.0978413767321471,
77.6351025776695));
#244758=CARTESIAN_POINT('Ctrl Pts',(6.67068665116703,5.6689065083369,77.8470417321028));
#244759=CARTESIAN_POINT('Ctrl Pts',(1.74550905742564,8.07659541114981,78.0589808865355));
#244760=CARTESIAN_POINT('Ctrl Pts',(-2.32915219108236,7.94646773541228,
78.2179352523606));
#244761=CARTESIAN_POINT('Ctrl Pts',(-5.83535034661537,5.85037034336685,
78.3768896181851));
#244762=CARTESIAN_POINT('Ctrl Pts',(-8.6700062972319,1.17531980275567,78.5888287726184));
#244763=CARTESIAN_POINT('Ctrl Pts',(-7.11899155498003,-6.12139075719558,
78.8537527156595));
#244764=CARTESIAN_POINT('Ctrl Pts',(1.3232990659429,-9.30225649786416,79.171661447309));
#244765=CARTESIAN_POINT('Ctrl Pts',(7.3046384891676,-4.8155836252492,79.4365853903503));
#244766=CARTESIAN_POINT('Ctrl Pts',(8.23639399556954,0.549883585184681,
79.6485245447833));
#244767=CARTESIAN_POINT('Ctrl Pts',(6.5878381851895,5.76828186615729,79.8604636992164));
#244768=CARTESIAN_POINT('Ctrl Pts',(1.38096365496417,8.64450545691486,80.0724028536493));
#244769=CARTESIAN_POINT('Ctrl Pts',(-3.92628481094429,7.27065978857151,
80.2843420080824));
#244770=CARTESIAN_POINT('Ctrl Pts',(-6.93705378861793,4.52201060669062,
80.4432963739071));
#244771=CARTESIAN_POINT('Ctrl Pts',(-8.23748906457628,0.649554799191576,
80.6022507397318));
#244772=CARTESIAN_POINT('Ctrl Pts',(-7.35065479861294,-4.74534094694224,
80.8141898941649));
#244773=CARTESIAN_POINT('Ctrl Pts',(-1.42727141702365,-9.27978235578654,
81.0791138372061));
#244774=CARTESIAN_POINT('Ctrl Pts',(7.05462215267386,-6.20607792875995,
81.3970225688557));
#244775=CARTESIAN_POINT('Ctrl Pts',(8.68072874534535,1.0920336727712,81.6619465118969));
#244776=CARTESIAN_POINT('Ctrl Pts',(5.89933558949375,5.77394124777071,81.87388566633));
#244777=CARTESIAN_POINT('Ctrl Pts',(1.2534011759003,8.66612215767996,82.085824820763));
#244778=CARTESIAN_POINT('Ctrl Pts',(-4.57253617197667,7.46501494350422,
82.2977639751959));
#244779=CARTESIAN_POINT('Ctrl Pts',(-7.71086060751405,2.96998903753608,
82.509703129629));
#244780=CARTESIAN_POINT('Ctrl Pts',(-8.21057260419263,-1.07600776198775,
82.6686574954537));
#244781=CARTESIAN_POINT('Ctrl Pts',(-6.68017462332549,-4.86347761639228,
82.8276118612785));
#244782=CARTESIAN_POINT('Ctrl Pts',(-2.49811809120793,-8.38509348057498,
83.0395510157114));
#244783=CARTESIAN_POINT('Ctrl Pts',(4.95048473210504,-7.97772932499307,
83.3044749587528));
#244784=CARTESIAN_POINT('Ctrl Pts',(9.39505194771926,-0.126869518922279,
83.6223836904022));
#244785=CARTESIAN_POINT('Ctrl Pts',(5.88431699012904,6.47475116532634,83.8873076334436));
#244786=CARTESIAN_POINT('Ctrl Pts',(0.726686965102308,8.22268107034541,
84.0992467878765));
#244787=CARTESIAN_POINT('Ctrl Pts',(-4.68349895600442,7.39848128259805,
84.3111859423098));
#244788=CARTESIAN_POINT('Ctrl Pts',(-8.32818868613579,2.69737063801516,
84.5231250967425));
#244789=CARTESIAN_POINT('Ctrl Pts',(-7.78911378360293,-2.75824448837895,
84.7350642511757));
#244790=CARTESIAN_POINT('Ctrl Pts',(-5.53757591012922,-6.15682939768139,
84.8940186170005));
#244791=CARTESIAN_POINT('Ctrl Pts',(-1.91194980781425,-8.03881803847154,
85.0529729828251));
#244792=CARTESIAN_POINT('Ctrl Pts',(3.55517065472387,-7.99444483947463,
85.2649121372583));
#244793=CARTESIAN_POINT('Ctrl Pts',(8.94872781730662,-2.84107985058827,
85.5298360802993));
#244794=CARTESIAN_POINT('Ctrl Pts',(7.21963126456139,6.01332032898139,85.8477448119492));
#244795=CARTESIAN_POINT('Ctrl Pts',(0.259533891981588,8.74529766515297,
86.1126687549902));
#244796=CARTESIAN_POINT('Ctrl Pts',(-4.79525293485256,6.71908529642643,
86.3246079094232));
#244797=CARTESIAN_POINT('Ctrl Pts',(-8.36921611223426,2.57466685739491,
86.5365470638563));
#244798=CARTESIAN_POINT('Ctrl Pts',(-8.08079203456533,-3.36679896115177,
86.7484862182892));
#244799=CARTESIAN_POINT('Ctrl Pts',(-4.12343096012912,-7.16069293494938,
86.9604253727224));
#244800=CARTESIAN_POINT('Ctrl Pts',(-0.20287335629181,-8.27829315704055,
87.119379738547));
#244801=CARTESIAN_POINT('Ctrl Pts',(3.77527785111434,-7.35019895445982,
87.2783341043719));
#244802=CARTESIAN_POINT('Ctrl Pts',(7.89962168578836,-3.76116523128593,
87.4902732588048));
#244803=CARTESIAN_POINT('Ctrl Pts',(8.64565175936641,3.6611705671027,87.7551972018461));
#244804=CARTESIAN_POINT('Ctrl Pts',(1.57400355324675,9.26313174847145,88.0731059334957));
#244805=CARTESIAN_POINT('Ctrl Pts',(-5.48999745202445,6.81230629596051,
88.3380298765369));
#244806=CARTESIAN_POINT('Ctrl Pts',(-8.01229389654767,1.98587624116183,
88.54996903097));
#244807=CARTESIAN_POINT('Ctrl Pts',(-8.0321637517713,-3.48669373828258,
88.7619081854028));
#244808=CARTESIAN_POINT('Ctrl Pts',(-3.94926054510204,-7.8126740811074,
88.9738473398362));
#244809=CARTESIAN_POINT('Ctrl Pts',(1.52423107718599,-8.12126380650983,
89.1857864942687));
#244810=CARTESIAN_POINT('Ctrl Pts',(5.22934284069866,-6.42069066744618,
89.3447408600939));
#244811=CARTESIAN_POINT('Ctrl Pts',(7.64787048893159,-3.12861383168092,
89.5036952259183));
#244812=CARTESIAN_POINT('Ctrl Pts',(8.44701969721102,2.27996598890042,89.7156343803516));
#244813=CARTESIAN_POINT('Ctrl Pts',(4.18693389661271,8.40363307213325,89.9805583233925));
#244814=CARTESIAN_POINT('Ctrl Pts',(-4.82818886236687,8.06050180103496,
90.2984670550424));
#244815=CARTESIAN_POINT('Ctrl Pts',(-8.60069212356836,1.60489379362226,
90.5633909980834));
#244816=CARTESIAN_POINT('Ctrl Pts',(-7.37812451624919,-3.70186933218736,
90.7753301525166));
#244817=CARTESIAN_POINT('Ctrl Pts',(-3.83435035223363,-7.87213091457285,
90.9872693069495));
#244818=CARTESIAN_POINT('Ctrl Pts',(2.08053294659223,-8.50328864668548,
91.1992084613827));
#244819=CARTESIAN_POINT('Ctrl Pts',(6.43925217997725,-5.17824657140275,
91.4111476158157));
#244820=CARTESIAN_POINT('Ctrl Pts',(8.14800929900498,-1.47690204682834,
91.5701019816404));
#244821=CARTESIAN_POINT('Ctrl Pts',(7.84441750217561,2.5967790770139,91.7290563474652));
#244822=CARTESIAN_POINT('Ctrl Pts',(4.93425091533369,7.22520273626573,91.940995501898));
#244823=CARTESIAN_POINT('Ctrl Pts',(-2.2842866691219,9.10678311364272,92.2059194449396));
#244824=CARTESIAN_POINT('Ctrl Pts',(-8.90965126982931,2.98348977293375,
92.5238281765888));
#244825=CARTESIAN_POINT('Ctrl Pts',(-7.57735540756411,-4.37393119752425,
92.7887521196303));
#244826=CARTESIAN_POINT('Ctrl Pts',(-3.19756632291204,-7.61026461697919,
93.0006912740631));
#244827=CARTESIAN_POINT('Ctrl Pts',(2.20649201279304,-8.47372885790721,
93.2126304284962));
#244828=CARTESIAN_POINT('Ctrl Pts',(7.11029197821448,-5.10669003712246,
93.4245695829292));
#244829=CARTESIAN_POINT('Ctrl Pts',(8.25916532611732,0.253760334661598,
93.6365087373623));
#244830=CARTESIAN_POINT('Ctrl Pts',(7.15023209159534,4.17677821160243,93.7954631031868));
#244831=CARTESIAN_POINT('Ctrl Pts',(4.27044608444791,7.07399729736161,93.954417469012));
#244832=CARTESIAN_POINT('Ctrl Pts',(-0.950227941146778,8.69755445717221,
94.1663566234446));
#244833=CARTESIAN_POINT('Ctrl Pts',(-7.65753597247037,5.43264273590476,
94.4312805664861));
#244834=CARTESIAN_POINT('Ctrl Pts',(-8.7085771706482,-3.5275743277836,94.7491892981357));
#244835=CARTESIAN_POINT('Ctrl Pts',(-2.91186703220212,-8.25037086923931,
95.0141132411768));
#244836=CARTESIAN_POINT('Ctrl Pts',(2.51994254285583,-7.8606900149142,95.22605239561));
#244837=CARTESIAN_POINT('Ctrl Pts',(7.1867561003735,-5.00232191223157,95.4379915500428));
#244838=CARTESIAN_POINT('Ctrl Pts',(8.72239929178196,0.744503690674433,
95.6499307044759));
#244839=CARTESIAN_POINT('Ctrl Pts',(6.10920625702525,5.56379412817455,95.8618698589088));
#244840=CARTESIAN_POINT('Ctrl Pts',(2.71560544576572,7.82283722542689,96.0208242247336));
#244841=CARTESIAN_POINT('Ctrl Pts',(-1.35616922499205,8.15100929679513,
96.1797785905584));
#244842=CARTESIAN_POINT('Ctrl Pts',(-6.37796772621453,5.98931668548074,
96.3917177449913));
#244843=CARTESIAN_POINT('Ctrl Pts',(-9.35009381440451,-0.85276604499158,
96.6566416880326));
#244844=CARTESIAN_POINT('Ctrl Pts',(-4.32161537230249,-8.34306523701283,
96.9745504196823));
#244845=CARTESIAN_POINT('Ctrl Pts',(3.15324704008515,-8.16116549258814,
97.2394743627233));
#244846=CARTESIAN_POINT('Ctrl Pts',(7.02620917168331,-4.33277539293464,
97.4514135171566));
#244847=CARTESIAN_POINT('Ctrl Pts',(8.71261502302726,0.873514293167906,
97.6633526715894));
#244848=CARTESIAN_POINT('Ctrl Pts',(6.14197512894139,6.23784230853676,97.8752918260226));
#244849=CARTESIAN_POINT('Ctrl Pts',(1.0227799761445,8.19951994399571,98.0872309804555));
#244850=CARTESIAN_POINT('Ctrl Pts',(-3.02431128459427,7.70875064108789,
98.2461853462802));
#244851=CARTESIAN_POINT('Ctrl Pts',(-6.33092465357644,5.31013564365306,
98.405139712105));
#244852=CARTESIAN_POINT('Ctrl Pts',(-8.7400567020074,0.402238140045645,
98.6170788665382));
#244853=CARTESIAN_POINT('Ctrl Pts',(-6.54841087316406,-6.72828204684399,
98.8820028095792));
#244854=CARTESIAN_POINT('Ctrl Pts',(2.142585482776,-9.14835637828844,99.1999115412288));
#244855=CARTESIAN_POINT('Ctrl Pts',(7.70271306345742,-4.14919275947252,
99.4648354842702));
#244856=CARTESIAN_POINT('Ctrl Pts',(8.15523954627708,1.27774249076433,99.6767746387031));
#244857=CARTESIAN_POINT('Ctrl Pts',(6.05064540172951,6.32948481176616,99.8887137931363));
#244858=CARTESIAN_POINT('Ctrl Pts',(0.609332981805773,8.73288317040774,
100.100652947569));
#244859=CARTESIAN_POINT('Ctrl Pts',(-4.55525842887585,6.89404285145814,
100.312592102002));
#244860=CARTESIAN_POINT('Ctrl Pts',(-7.3105545667479,3.88935561747675,100.471546467826));
#244861=CARTESIAN_POINT('Ctrl Pts',(-8.26264112040473,-0.0831218301869292,
100.630500833652));
#244862=CARTESIAN_POINT('Ctrl Pts',(-6.90112694396627,-5.37818125195461,
100.842439988084));
#244863=CARTESIAN_POINT('Ctrl Pts',(-0.599151469554942,-9.36976423300961,
101.107363931126));
#244864=CARTESIAN_POINT('Ctrl Pts',(7.57692554188092,-5.55637438515131,
101.425272662775));
#244865=CARTESIAN_POINT('Ctrl Pts',(8.54977268556443,1.85714192198488,101.690196605817));
#244866=CARTESIAN_POINT('Ctrl Pts',(5.36435094540862,6.2740972947795,101.902135760249));
#244867=CARTESIAN_POINT('Ctrl Pts',(0.480356583988195,8.74310844677501,
102.114074914683));
#244868=CARTESIAN_POINT('Ctrl Pts',(-5.21619276540107,7.03035334708608,
102.326014069115));
#244869=CARTESIAN_POINT('Ctrl Pts',(-7.9437542886209,2.27485691717137,102.537953223549));
#244870=CARTESIAN_POINT('Ctrl Pts',(-8.08288738621888,-1.79950734766523,
102.696907589373));
#244871=CARTESIAN_POINT('Ctrl Pts',(-6.22281468754034,-5.43642574563372,
102.855861955198));
#244872=CARTESIAN_POINT('Ctrl Pts',(-1.7450832855641,-8.57350984148596,
103.067801109631));
#244873=CARTESIAN_POINT('Ctrl Pts',(5.63809766156071,-7.50755080065118,
103.332725052672));
#244874=CARTESIAN_POINT('Ctrl Pts',(9.36932056200261,0.706349192403,103.650633784322));
#244875=CARTESIAN_POINT('Ctrl Pts',(5.28727599165471,6.97081786315566,103.915557727363));
#244876=CARTESIAN_POINT('Ctrl Pts',(-0.00498074626342562,8.25472792537904,
104.127496881796));
#244877=CARTESIAN_POINT('Ctrl Pts',(-5.32082169786743,6.95424648825107,
104.339436036229));
#244878=CARTESIAN_POINT('Ctrl Pts',(-8.53448952384093,1.94859531923814,
104.551375190662));
#244879=CARTESIAN_POINT('Ctrl Pts',(-7.51398423530762,-3.43776775002822,
104.763314345095));
#244880=CARTESIAN_POINT('Ctrl Pts',(-4.97007821053796,-6.62341435920571,
104.92226871092));
#244881=CARTESIAN_POINT('Ctrl Pts',(-1.19191371467555,-8.17664290647606,
105.081223076745));
#244882=CARTESIAN_POINT('Ctrl Pts',(4.24975671303451,-7.64787255095371,
105.293162231178));
#244883=CARTESIAN_POINT('Ctrl Pts',(9.16532388241747,-2.03673817562357,
105.558086174219));
#244884=CARTESIAN_POINT('Ctrl Pts',(6.65823321967812,6.6295571019147,105.875994905869));
#244885=CARTESIAN_POINT('Ctrl Pts',(-0.51661674225922,8.73388208271878,
106.14091884891));
#244886=CARTESIAN_POINT('Ctrl Pts',(-5.37191837928407,6.26761923350293,
106.352858003343));
#244887=CARTESIAN_POINT('Ctrl Pts',(-8.56447977198818,1.82273804894021,
106.564797157776));
#244888=CARTESIAN_POINT('Ctrl Pts',(-7.75057601113544,-4.06977968031675,
106.776736312209));
#244889=CARTESIAN_POINT('Ctrl Pts',(-3.47252267763465,-7.49798589255131,
106.988675466642));
#244890=CARTESIAN_POINT('Ctrl Pts',(0.531661882066579,-8.26369353471885,
107.147629832466));
#244891=CARTESIAN_POINT('Ctrl Pts',(4.41189565171434,-6.98665329622418,
107.306584198291));
#244892=CARTESIAN_POINT('Ctrl Pts',(8.20189742781796,-3.04618864471102,
107.518523352724));
#244893=CARTESIAN_POINT('Ctrl Pts',(8.28712132352169,4.41305839921567,107.783447295766));
#244894=CARTESIAN_POINT('Ctrl Pts',(0.74678191590698,9.36618458846757,108.101356027415));
#244895=CARTESIAN_POINT('Ctrl Pts',(-6.07219110863386,6.29889547725997,
108.366279970456));
#244896=CARTESIAN_POINT('Ctrl Pts',(-8.15677553875159,1.26790013025069,
108.578219124889));
#244897=CARTESIAN_POINT('Ctrl Pts',(-7.69151238309534,-4.18489247419079,
108.790158279322));
#244898=CARTESIAN_POINT('Ctrl Pts',(-3.24125016634453,-8.13196363185907,
109.002097433755));
#244899=CARTESIAN_POINT('Ctrl Pts',(2.23805079999365,-7.95420233639011,
109.214036588188));
#244900=CARTESIAN_POINT('Ctrl Pts',(5.77785197050303,-5.931923954296,109.372990954013));
#244901=CARTESIAN_POINT('Ctrl Pts',(7.89507160387075,-2.43844046328999,
109.531945319838));
#244902=CARTESIAN_POINT('Ctrl Pts',(8.21169246659059,3.01968433942239,109.743884474271));
#244903=CARTESIAN_POINT('Ctrl Pts',(3.4256091458593,8.74166267053705,110.008808417312));
#244904=CARTESIAN_POINT('Ctrl Pts',(-5.52361955555509,7.60083705789452,
110.326717148962));
#244905=CARTESIAN_POINT('Ctrl Pts',(-8.7090900621896,0.836265138511122,
110.591641092003));
#244906=CARTESIAN_POINT('Ctrl Pts',(-7.02097542855796,-4.34125119769074,
110.803580246436));
#244907=CARTESIAN_POINT('Ctrl Pts',(-3.12152234153726,-8.18100152983312,
111.015519400869));
#244908=CARTESIAN_POINT('Ctrl Pts',(2.82602354241485,-8.28541647042698,
111.227458555302));
#244909=CARTESIAN_POINT('Ctrl Pts',(6.87287687018398,-4.58713088094033,
111.439397709735));
#244910=CARTESIAN_POINT('Ctrl Pts',(8.24684447350177,-0.748900141855164,
111.59835207556));
#244911=CARTESIAN_POINT('Ctrl Pts',(7.58338159077484,3.2818396018016,111.757306441385));
#244912=CARTESIAN_POINT('Ctrl Pts',(4.27443372015049,7.63410787503385,111.969245595818));
#244913=CARTESIAN_POINT('Ctrl Pts',(-3.08246536969312,8.86847627895,112.234169538859));
#244914=CARTESIAN_POINT('Ctrl Pts',(-9.13902346548749,2.1820511159092,112.552078270508));
#244915=CARTESIAN_POINT('Ctrl Pts',(-7.15985478877821,-5.02832660999927,
112.81700221355));
#244916=CARTESIAN_POINT('Ctrl Pts',(-2.51045472892191,-7.86372526121687,
113.028941367983));
#244917=CARTESIAN_POINT('Ctrl Pts',(2.94886687155791,-8.24480878696875,
113.240880522416));
#244918=CARTESIAN_POINT('Ctrl Pts',(7.53493331273293,-4.45637914941877,
113.452819676849));
#244919=CARTESIAN_POINT('Ctrl Pts',(8.20416779507647,0.984803016758322,
113.664758831282));
#244920=CARTESIAN_POINT('Ctrl Pts',(6.75188693482159,4.79409199035459,113.823713197106));
#244921=CARTESIAN_POINT('Ctrl Pts',(3.62664335718611,7.42466197769528,113.982667562931));
#244922=CARTESIAN_POINT('Ctrl Pts',(-1.71738562550865,8.5791009604101,114.194606717364));
#244923=CARTESIAN_POINT('Ctrl Pts',(-8.10891394093082,4.73254466056412,
114.459530660406));
#244924=CARTESIAN_POINT('Ctrl Pts',(-8.36164022351918,-4.28556527748645,
114.777439392055));
#244925=CARTESIAN_POINT('Ctrl Pts',(-2.16914480590855,-8.47598961208767,
115.042363335096));
#244926=CARTESIAN_POINT('Ctrl Pts',(3.20674776995516,-7.60640037532565,
115.254302489529));
#244927=CARTESIAN_POINT('Ctrl Pts',(7.60184594723935,-4.34564448088987,
115.466241643962));
#244928=CARTESIAN_POINT('Ctrl Pts',(8.62208213981668,1.51467314129497,115.678180798395));
#244929=CARTESIAN_POINT('Ctrl Pts',(5.59202176323629,6.0833788958997,115.890119952828));
#244930=CARTESIAN_POINT('Ctrl Pts',(2.01154959266723,8.03274320695225,116.049074318653));
#244931=CARTESIAN_POINT('Ctrl Pts',(-2.07328684917035,7.9987267214422,116.208028684478));
#244932=CARTESIAN_POINT('Ctrl Pts',(-6.88372186139305,5.40044072373649,
116.419967838911));
#244933=CARTESIAN_POINT('Ctrl Pts',(-9.23771052450177,-1.67814437137133,
116.684891781952));
#244934=CARTESIAN_POINT('Ctrl Pts',(-3.56512891153324,-8.69327054791941,
117.002800513602));
#244935=CARTESIAN_POINT('Ctrl Pts',(3.86419204732527,-7.84956106509181,
117.267724456643));
#244936=CARTESIAN_POINT('Ctrl Pts',(7.38258641782075,-3.69296299917493,
117.479663611076));
#244937=CARTESIAN_POINT('Ctrl Pts',(8.60090167609176,1.64230877670762,117.691602765509));
#244938=CARTESIAN_POINT('Ctrl Pts',(5.56491819765861,6.75767864018963,117.903541919942));
#244939=CARTESIAN_POINT('Ctrl Pts',(0.291999784095893,8.25790181085207,
118.115481074375));
#244940=CARTESIAN_POINT('Ctrl Pts',(-3.69566448850107,7.41035486201767,
118.2744354402));
#244941=CARTESIAN_POINT('Ctrl Pts',(-6.77666552377574,4.72810235740781,
118.433389806024));
#244942=CARTESIAN_POINT('Ctrl Pts',(-8.74131016986724,-0.374009611892281,
118.645328960458));
#244943=CARTESIAN_POINT('Ctrl Pts',(-5.92628477378799,-7.28221209836851,
118.910252903499));
#244944=CARTESIAN_POINT('Ctrl Pts',(2.94500667733487,-8.92244544088817,
119.228161635148));
#244945=CARTESIAN_POINT('Ctrl Pts',(8.04015614710591,-3.45014176859058,
119.49308557819));
#244946=CARTESIAN_POINT('Ctrl Pts',(8.00989158325591,1.99554372398919,119.705024732623));
#244947=CARTESIAN_POINT('Ctrl Pts',(5.46582529332645,6.84086556092725,119.916963887056));
#244948=CARTESIAN_POINT('Ctrl Pts',(-0.167094020397713,8.75252047921361,
120.128903041489));
#244949=CARTESIAN_POINT('Ctrl Pts',(-5.14837558233741,6.46315983515627,
120.340842195922));
#244950=CARTESIAN_POINT('Ctrl Pts',(-7.62651071766266,3.22608578093847,
120.499796561746));
#244951=CARTESIAN_POINT('Ctrl Pts',(-8.22275425290849,-0.815144171010343,
120.658750927571));
#244952=CARTESIAN_POINT('Ctrl Pts',(-6.39727724933591,-5.96868749983967,
120.870690082004));
#244953=CARTESIAN_POINT('Ctrl Pts',(0.233684665549838,-9.38599252837668,
121.135614025046));
#244954=CARTESIAN_POINT('Ctrl Pts',(8.03958757993772,-4.86293414716715,
121.453522756695));
#244955=CARTESIAN_POINT('Ctrl Pts',(8.35151756196486,2.60763178102463,121.718446699736));
#244956=CARTESIAN_POINT('Ctrl Pts',(4.78714110894806,6.72486713124396,121.930385854169));
#244957=CARTESIAN_POINT('Ctrl Pts',(-0.296469108270646,8.75127384028694,
122.142325008602));
#244958=CARTESIAN_POINT('Ctrl Pts',(-5.81879038537252,6.54035271233923,
122.354264163035));
#244959=CARTESIAN_POINT('Ctrl Pts',(-8.11411914629701,1.56181838613904,
122.566203317468));
#244960=CARTESIAN_POINT('Ctrl Pts',(-7.89157816631291,-2.5088422105765,
122.725157683293));
#244961=CARTESIAN_POINT('Ctrl Pts',(-5.71647220940666,-5.96658134967907,
122.884112049118));
#244962=CARTESIAN_POINT('Ctrl Pts',(-0.978312153156251,-8.69444029288825,
123.096051203551));
#244963=CARTESIAN_POINT('Ctrl Pts',(6.28133061646463,-6.97827700455636,
123.360975146592));
#244964=CARTESIAN_POINT('Ctrl Pts',(9.26983908661552,1.53400791504753,123.678883878242));
#244965=CARTESIAN_POINT('Ctrl Pts',(4.64861649203921,7.41201415292483,123.943807821283));
#244966=CARTESIAN_POINT('Ctrl Pts',(-0.736609251960068,8.22179814516222,
124.155746975716));
#244967=CARTESIAN_POINT('Ctrl Pts',(-5.91626188541497,6.45527172650657,
124.367686130149));
#244968=CARTESIAN_POINT('Ctrl Pts',(-8.67361159831449,1.18448173995706,
124.579625284582));
#244969=CARTESIAN_POINT('Ctrl Pts',(-7.17970877483334,-4.09023081257849,
124.791564439015));
#244970=CARTESIAN_POINT('Ctrl Pts',(-4.3634588146324,-7.03786348017661,
124.95051880484));
#244971=CARTESIAN_POINT('Ctrl Pts',(-0.462495538518424,-8.25010578114652,
125.109473170664));
#244972=CARTESIAN_POINT('Ctrl Pts',(4.91089104594106,-7.24110045576698,
125.321412325098));
#244973=CARTESIAN_POINT('Ctrl Pts',(9.30977560646184,-1.21636442852571,
125.586336268139));
#244974=CARTESIAN_POINT('Ctrl Pts',(6.04442525950268,7.19360968203438,125.904244999789));
#244975=CARTESIAN_POINT('Ctrl Pts',(-1.28870085632782,8.65371822953107,
126.169168942829));
#244976=CARTESIAN_POINT('Ctrl Pts',(-5.90629906469245,5.76681795171991,
126.381108097263));
#244977=CARTESIAN_POINT('Ctrl Pts',(-8.69232860192757,1.05646165853806,
126.593047251695));
#244978=CARTESIAN_POINT('Ctrl Pts',(-7.35935175642168,-4.74072535335686,
126.804986406129));
#244979=CARTESIAN_POINT('Ctrl Pts',(-2.79428062454671,-7.77625886804627,
127.016925560562));
#244980=CARTESIAN_POINT('Ctrl Pts',(1.26201217326531,-8.18404670484764,
127.175879926386));
#244981=CARTESIAN_POINT('Ctrl Pts',(5.01378545920402,-6.56811258219065,
127.334834292211));
#244982=CARTESIAN_POINT('Ctrl Pts',(8.4396123869428,-2.30723415235086,127.546773446644));
#244983=CARTESIAN_POINT('Ctrl Pts',(7.86335926958056,5.13020908571511,127.811697389686));
#244984=CARTESIAN_POINT('Ctrl Pts',(-0.0863179740656035,9.3955120234359,
128.129606121335));
#244985=CARTESIAN_POINT('Ctrl Pts',(-6.60658784808237,5.73590325047324,
128.394530064376));
#244986=CARTESIAN_POINT('Ctrl Pts',(-8.23705157250959,0.539943813445461,
128.606469218809));
#244987=CARTESIAN_POINT('Ctrl Pts',(-7.29031769922452,-4.85015005997164,
128.818408373242));
#244988=CARTESIAN_POINT('Ctrl Pts',(-2.5077264657993,-8.38724287971926,
129.030347527675));
#244989=CARTESIAN_POINT('Ctrl Pts',(2.93425382945483,-7.72452980160819,
129.242286682108));
#244990=CARTESIAN_POINT('Ctrl Pts',(6.28088105743071,-5.39646442914402,
129.401241047933));
#244991=CARTESIAN_POINT('Ctrl Pts',(8.08012709843497,-1.72907304538782,
129.560195413758));
#244992=CARTESIAN_POINT('Ctrl Pts',(7.91172735197586,3.73563341135219,129.772134568191));
#244993=CARTESIAN_POINT('Ctrl Pts',(2.63731990175192,9.0108827536864,130.037058511232));
#244994=CARTESIAN_POINT('Ctrl Pts',(-6.17557138222025,7.0813427454344,130.354967242881));
#244995=CARTESIAN_POINT('Ctrl Pts',(-8.74893487918551,0.0610538684213404,
130.619891185923));
#244996=CARTESIAN_POINT('Ctrl Pts',(-6.60856112015652,-4.94646114387313,
130.831830340356));
#244997=CARTESIAN_POINT('Ctrl Pts',(-2.38412344038647,-8.42547584343258,
131.043769494789));
#244998=CARTESIAN_POINT('Ctrl Pts',(3.54926925064944,-8.00232609504537,
131.255708649222));
#244999=CARTESIAN_POINT('Ctrl Pts',(7.25240208852943,-3.95990784377751,
131.467647803655));
#245000=CARTESIAN_POINT('Ctrl Pts',(8.28076506882167,-0.0150033089913116,
131.62660216948));
#245001=CARTESIAN_POINT('Ctrl Pts',(7.26265350624478,3.94106730409408,131.785556535304));
#245002=CARTESIAN_POINT('Ctrl Pts',(3.58097056341955,7.98292156195555,131.997495689737));
#245003=CARTESIAN_POINT('Ctrl Pts',(-3.85638062987201,8.56036170837607,
132.262419632779));
#245004=CARTESIAN_POINT('Ctrl Pts',(-9.29645831505568,1.36343658901342,
132.580328364428));
#245005=CARTESIAN_POINT('Ctrl Pts',(-6.6859958139991,-5.64314186911429,
132.845252307469));
#245006=CARTESIAN_POINT('Ctrl Pts',(-1.80358216812555,-8.05528697015432,
133.057191461902));
#245007=CARTESIAN_POINT('Ctrl Pts',(3.66802973050227,-7.95099030277828,
133.269130616335));
#245008=CARTESIAN_POINT('Ctrl Pts',(7.90026415480175,-3.77098982631053,
133.481069770768));
#245009=CARTESIAN_POINT('Ctrl Pts',(8.08459121557868,1.70809351433024,133.693008925202));
#245010=CARTESIAN_POINT('Ctrl Pts',(6.3003954935726,5.37367009175038,133.851963291026));
#245011=CARTESIAN_POINT('Ctrl Pts',(2.95429220966773,7.71688246736308,134.010917656851));
#245012=CARTESIAN_POINT('Ctrl Pts',(-2.47102176873227,8.39312051202395,
134.222856811284));
#245013=CARTESIAN_POINT('Ctrl Pts',(-8.49646973291041,3.99518848123922,
134.487780754325));
#245014=CARTESIAN_POINT('Ctrl Pts',(-7.94887339718645,-5.00981191143028,
134.805689485975));
#245015=CARTESIAN_POINT('Ctrl Pts',(-1.4093678818468,-8.63490805875611,
135.070613429016));
#245016=CARTESIAN_POINT('Ctrl Pts',(3.86833736244917,-7.29221342526346,
135.282552583449));
#245017=CARTESIAN_POINT('Ctrl Pts',(7.95703106514325,-3.65482222106151,
135.494491737882));
#245018=CARTESIAN_POINT('Ctrl Pts',(8.45403342063807,2.2730453255652,135.706430892315));
#245019=CARTESIAN_POINT('Ctrl Pts',(5.03065108698298,6.55492372538339,135.918370046748));
#245020=CARTESIAN_POINT('Ctrl Pts',(1.292011381003,8.17974234020297,136.077324412573));
#245021=CARTESIAN_POINT('Ctrl Pts',(-2.77472573740587,7.78289447205871,
136.236278778398));
#245022=CARTESIAN_POINT('Ctrl Pts',(-7.33390610192825,4.7703262757849,136.448217932831));
#245023=CARTESIAN_POINT('Ctrl Pts',(-9.05547875439378,-2.49294253543202,
136.713141875872));
#245024=CARTESIAN_POINT('Ctrl Pts',(-2.77557159916479,-8.97045204363947,
137.031050607521));
#245025=CARTESIAN_POINT('Ctrl Pts',(4.53630470631618,-7.48389232836955,
137.295974550563));
#245026=CARTESIAN_POINT('Ctrl Pts',(7.69217499320704,-3.01368022077503,
137.507913704996));
#245027=CARTESIAN_POINT('Ctrl Pts',(8.21568403484059,1.02348437607822,137.666868070821));
#245028=CARTESIAN_POINT('Ctrl Pts',(6.71054899145757,4.84288607544307,137.825887206215));
#245029=CARTESIAN_POINT('Ctrl Pts',(4.62085797159542,6.58783761712044,137.931921553001));
#245030=CARTESIAN_POINT('Ctrl Pts',(3.42771117511922,7.15909185610951,137.984971111179));
#245031=CARTESIAN_POINT('Ctrl Pts',(4.3786726516329,-6.14439445976196,7.5507492878767));
#245032=CARTESIAN_POINT('Ctrl Pts',(5.4020829415103,-5.4150902343734,7.60376665636641));
#245033=CARTESIAN_POINT('Ctrl Pts',(7.07379358162461,-3.44081123600024,
7.70976881346437));
#245034=CARTESIAN_POINT('Ctrl Pts',(7.86067347517091,0.380537801570955,
7.8687557591706));
#245035=CARTESIAN_POINT('Ctrl Pts',(6.71242675331904,4.07595804571959,8.02771012499535));
#245036=CARTESIAN_POINT('Ctrl Pts',(3.02843446954156,7.74789103749108,8.23964927942837));
#245037=CARTESIAN_POINT('Ctrl Pts',(-4.06131014199803,7.94832137794174,
8.50457322246963));
#245038=CARTESIAN_POINT('Ctrl Pts',(-8.88662488748039,0.858715297192927,
8.82248195411916));
#245039=CARTESIAN_POINT('Ctrl Pts',(-6.09061026031311,-5.66263867668864,
9.08740589716043));
#245040=CARTESIAN_POINT('Ctrl Pts',(-1.3300103532646,-7.74079488884142,
9.29934505159343));
#245041=CARTESIAN_POINT('Ctrl Pts',(2.54310647155665,-7.44962859780676,
9.45829941741821));
#245042=CARTESIAN_POINT('Ctrl Pts',(5.77946815770139,-5.31867664433347,
9.61725378324296));
#245043=CARTESIAN_POINT('Ctrl Pts',(8.28754101548936,-0.750810161955585,
9.82919293767598));
#245044=CARTESIAN_POINT('Ctrl Pts',(6.85596530424556,4.71954476407852,10.041132092109));
#245045=CARTESIAN_POINT('Ctrl Pts',(2.43413358249498,7.45951945984923,10.253071246542));
#245046=CARTESIAN_POINT('Ctrl Pts',(-2.72719324131664,7.85675727497228,
10.465010400975));
#245047=CARTESIAN_POINT('Ctrl Pts',(-8.26051227361675,3.39608283759135,
10.7299343440162));
#245048=CARTESIAN_POINT('Ctrl Pts',(-7.30566755686335,-5.12621182347484,
11.0478430756658));
#245049=CARTESIAN_POINT('Ctrl Pts',(-0.946139846574816,-8.26276376220919,
11.312767018707));
#245050=CARTESIAN_POINT('Ctrl Pts',(4.0243689706447,-6.74524415246625,11.5247061731401));
#245051=CARTESIAN_POINT('Ctrl Pts',(6.77604042885482,-4.00550406444893,
11.6836605389648));
#245052=CARTESIAN_POINT('Ctrl Pts',(7.84948657201265,-0.281954118113144,
11.8426149047896));
#245053=CARTESIAN_POINT('Ctrl Pts',(6.78387063251435,4.81908192792366,12.0545540592226));
#245054=CARTESIAN_POINT('Ctrl Pts',(2.13917921968976,8.04380728042435,12.2664932136556));
#245055=CARTESIAN_POINT('Ctrl Pts',(-3.00190064357618,7.24970078792561,
12.4784323680886));
#245056=CARTESIAN_POINT('Ctrl Pts',(-7.18106853250261,4.19501405678216,
12.6903715225216));
#245057=CARTESIAN_POINT('Ctrl Pts',(-8.48377503682947,-2.79200061042099,
12.9552954655629));
#245058=CARTESIAN_POINT('Ctrl Pts',(-2.2162499015533,-8.64517229147749,
13.2732041972124));
#245059=CARTESIAN_POINT('Ctrl Pts',(4.6546035164407,-6.89224791200518,13.5381281402537));
#245060=CARTESIAN_POINT('Ctrl Pts',(7.44369077636594,-2.50706182528472,
13.7500672946867));
#245061=CARTESIAN_POINT('Ctrl Pts',(7.75236522237301,1.3636728095776,13.9090216605115));
#245062=CARTESIAN_POINT('Ctrl Pts',(6.1463672728273,4.8904103908539,14.0679760263362));
#245063=CARTESIAN_POINT('Ctrl Pts',(2.0195949849537,8.07252655100552,14.2799151807692));
#245064=CARTESIAN_POINT('Ctrl Pts',(-3.60590313906814,7.50175878230377,
14.4918543352022));
#245065=CARTESIAN_POINT('Ctrl Pts',(-6.99500513087751,3.555203681579,14.7037934896353));
#245066=CARTESIAN_POINT('Ctrl Pts',(-8.18329367705831,-1.48310209359639,
14.9157326440683));
#245067=CARTESIAN_POINT('Ctrl Pts',(-4.6291914378742,-7.63808178227025,
15.1806565871096));
#245068=CARTESIAN_POINT('Ctrl Pts',(3.93842904184229,-8.00871677424294,
15.4985653187591));
#245069=CARTESIAN_POINT('Ctrl Pts',(8.01805636285859,-2.20888822471383,
15.7634892618003));
#245070=CARTESIAN_POINT('Ctrl Pts',(7.28510689705072,2.93617249785386,15.9754284162333));
#245071=CARTESIAN_POINT('Ctrl Pts',(5.00241856512635,6.07738254047629,16.1343827820581));
#245072=CARTESIAN_POINT('Ctrl Pts',(1.48891842297151,7.71213760116044,16.2933371478829));
#245073=CARTESIAN_POINT('Ctrl Pts',(-3.71542417565377,7.44580902387277,
16.5052763023159));
#245074=CARTESIAN_POINT('Ctrl Pts',(-7.61776274296967,3.35389520727049,
16.7172154567489));
#245075=CARTESIAN_POINT('Ctrl Pts',(-7.62587191461766,-1.84814705670977,
16.9291546111819));
#245076=CARTESIAN_POINT('Ctrl Pts',(-5.2521153231257,-6.44834644354046,
17.1410937656149));
#245077=CARTESIAN_POINT('Ctrl Pts',(1.45047157124013,-8.81282241408086,
17.4060177086562));
#245078=CARTESIAN_POINT('Ctrl Pts',(8.20005226505081,-3.52277029322367,
17.7239264403057));
#245079=CARTESIAN_POINT('Ctrl Pts',(7.52752907318606,3.53620150433122,17.988850383347));
#245080=CARTESIAN_POINT('Ctrl Pts',(3.62484429538331,6.96809839719076,18.20078953778));
#245081=CARTESIAN_POINT('Ctrl Pts',(-0.152003807205115,7.86992152988776,
18.3597439036047));
#245082=CARTESIAN_POINT('Ctrl Pts',(-3.88419788878212,6.82692838766171,
18.5186982694295));
#245083=CARTESIAN_POINT('Ctrl Pts',(-7.66457774004274,3.24016926901836,
18.7306374238625));
#245084=CARTESIAN_POINT('Ctrl Pts',(-7.96804839137267,-2.40606049430473,
18.9425765782956));
#245085=CARTESIAN_POINT('Ctrl Pts',(-4.59126696645052,-6.3631625505062,
19.1545157327285));
#245086=CARTESIAN_POINT('Ctrl Pts',(0.203558650913005,-8.31411156401997,
19.3664548871616));
#245087=CARTESIAN_POINT('Ctrl Pts',(6.83294708480065,-5.75156855278744,
19.6313788302028));
#245088=CARTESIAN_POINT('Ctrl Pts',(8.52021671301704,2.65644025937182,19.9492875618523));
#245089=CARTESIAN_POINT('Ctrl Pts',(3.41879978163113,7.58157128041503,20.2142115048936));
#245090=CARTESIAN_POINT('Ctrl Pts',(-1.77774553726379,7.65071972061739,
20.4261506593266));
#245091=CARTESIAN_POINT('Ctrl Pts',(-5.23336362817136,5.87968325501715,
20.5851050251514));
#245092=CARTESIAN_POINT('Ctrl Pts',(-7.39032538650155,2.66026974780967,
20.7440593909761));
#245093=CARTESIAN_POINT('Ctrl Pts',(-7.92965512841919,-2.52289880284267,
20.9559985454091));
#245094=CARTESIAN_POINT('Ctrl Pts',(-4.48839085913739,-7.00951280511866,
21.1679376998422));
#245095=CARTESIAN_POINT('Ctrl Pts',(0.650188485748879,-7.81964352987934,
21.3798768542752));
#245096=CARTESIAN_POINT('Ctrl Pts',(5.56138958627605,-6.18359386546308,
21.5918160087082));
#245097=CARTESIAN_POINT('Ctrl Pts',(8.93108020914646,0.0742494369790274,
21.8567399517494));
#245098=CARTESIAN_POINT('Ctrl Pts',(4.74503129677803,7.55879922216376,22.174648683399));
#245099=CARTESIAN_POINT('Ctrl Pts',(-2.33321884082268,7.982762984564,22.4395726264402));
#245100=CARTESIAN_POINT('Ctrl Pts',(-6.3258395055626,4.65592590024462,22.6515117808733));
#245101=CARTESIAN_POINT('Ctrl Pts',(-7.79924106812923,1.06330090059327,
22.810466146698));
#245102=CARTESIAN_POINT('Ctrl Pts',(-7.34419956866848,-2.78508117387092,
22.9694205125228));
#245103=CARTESIAN_POINT('Ctrl Pts',(-4.38324354331086,-7.07330367403193,
23.1813596669558));
#245104=CARTESIAN_POINT('Ctrl Pts',(1.14866847572867,-8.24375418134102,
23.3932988213888));
#245105=CARTESIAN_POINT('Ctrl Pts',(5.57912262346678,-5.51751400122422,
23.6052379758219));
#245106=CARTESIAN_POINT('Ctrl Pts',(8.24606831740575,-1.08085361081387,
23.8171771302548));
#245107=CARTESIAN_POINT('Ctrl Pts',(6.73637673629011,5.86437849630028,24.0821010732962));
#245108=CARTESIAN_POINT('Ctrl Pts',(-1.3109133925462,8.82792579067301,24.4000098049456));
#245109=CARTESIAN_POINT('Ctrl Pts',(-6.96374633402792,4.54693875285423,
24.6649337479869));
#245110=CARTESIAN_POINT('Ctrl Pts',(-7.83333875277766,-0.57679755801928,
24.8768729024199));
#245111=CARTESIAN_POINT('Ctrl Pts',(-6.61631470119941,-4.26417047251733,
25.0358272682447));
#245112=CARTESIAN_POINT('Ctrl Pts',(-3.7679913926847,-6.89174762408888,
25.1947816340694));
#245113=CARTESIAN_POINT('Ctrl Pts',(1.27002945794566,-8.22383572312823,
25.4067207885025));
#245114=CARTESIAN_POINT('Ctrl Pts',(6.23360578781741,-5.51553090387492,
25.6186599429354));
#245115=CARTESIAN_POINT('Ctrl Pts',(7.82638094846845,-0.563321622906876,
25.8305990973685));
#245116=CARTESIAN_POINT('Ctrl Pts',(6.96717007609529,4.54141259456727,26.0425382518014));
#245117=CARTESIAN_POINT('Ctrl Pts',(1.30374863294259,8.83571990180765,26.3074621948428));
#245118=CARTESIAN_POINT('Ctrl Pts',(-6.73675098894321,5.85379823715844,
26.6253709264922));
#245119=CARTESIAN_POINT('Ctrl Pts',(-8.24706112548936,-1.07442906668484,
26.8902948695336));
#245120=CARTESIAN_POINT('Ctrl Pts',(-5.57564470996179,-5.53227597892406,
27.1022340239665));
#245121=CARTESIAN_POINT('Ctrl Pts',(-2.25317303860719,-7.54201440611787,
27.2611883897913));
#245122=CARTESIAN_POINT('Ctrl Pts',(1.61934947606041,-7.68580846260585,
27.4201427556161));
#245123=CARTESIAN_POINT('Ctrl Pts',(6.31284674624026,-5.42147717725839,
27.632081910049));
#245124=CARTESIAN_POINT('Ctrl Pts',(8.32228168115093,-0.136197977555209,
27.8440210644821));
#245125=CARTESIAN_POINT('Ctrl Pts',(6.31179034003158,4.66163841421322,28.0559602189151));
#245126=CARTESIAN_POINT('Ctrl Pts',(2.33941346813801,7.98079142995397,28.2678993733482));
#245127=CARTESIAN_POINT('Ctrl Pts',(-4.75554273106144,7.56006084725168,
28.5328233163894));
#245128=CARTESIAN_POINT('Ctrl Pts',(-8.92448406558058,0.0659685651278762,
28.850732048039));
#245129=CARTESIAN_POINT('Ctrl Pts',(-5.56632173875549,-6.17935897383808,
29.1156559910802));
#245130=CARTESIAN_POINT('Ctrl Pts',(-0.637946557518925,-7.82859601898417,
29.3275951455132));
#245131=CARTESIAN_POINT('Ctrl Pts',(3.19298472656766,-7.19469377943924,
29.486549511338));
#245132=CARTESIAN_POINT('Ctrl Pts',(6.22832954950417,-4.78558830994203,
29.6455038771627));
#245133=CARTESIAN_POINT('Ctrl Pts',(8.32131444745636,-0.0132170951335337,
29.8574430315957));
#245134=CARTESIAN_POINT('Ctrl Pts',(6.41074768537356,5.30860022830765,30.0693821860288));
#245135=CARTESIAN_POINT('Ctrl Pts',(1.76335791951407,7.64592302139324,30.2813213404618));
#245136=CARTESIAN_POINT('Ctrl Pts',(-3.41281179499102,7.584101982127,30.4932604948948));
#245137=CARTESIAN_POINT('Ctrl Pts',(-8.52902236822057,2.65056298236675,
30.758184437936));
#245138=CARTESIAN_POINT('Ctrl Pts',(-6.82255106480021,-5.75356973161703,
31.0760931695856));
#245139=CARTESIAN_POINT('Ctrl Pts',(-0.210059446353434,-8.31410187909029,
31.3410171126268));
#245140=CARTESIAN_POINT('Ctrl Pts',(4.60638867185572,-6.36200242396248,
31.5529562670599));
#245141=CARTESIAN_POINT('Ctrl Pts',(7.10439402150931,-3.38915264205359,
31.7119106328846));
#245142=CARTESIAN_POINT('Ctrl Pts',(7.84358429483301,0.414885356851344,
31.8708649987094));
#245143=CARTESIAN_POINT('Ctrl Pts',(6.33003717266334,5.40139595083994,32.0828041531424));
#245144=CARTESIAN_POINT('Ctrl Pts',(1.41780677859154,8.20175263026691,32.2947433075754));
#245145=CARTESIAN_POINT('Ctrl Pts',(-3.63265477501151,6.95509807888935,
32.5066824620084));
#245146=CARTESIAN_POINT('Ctrl Pts',(-7.5246259286918,3.5420180485976,32.7186216164415));
#245147=CARTESIAN_POINT('Ctrl Pts',(-8.20291959169172,-3.53296148483668,
32.9835455594827));
#245148=CARTESIAN_POINT('Ctrl Pts',(-1.44127265323067,-8.80758200798813,
33.3014542911322));
#245149=CARTESIAN_POINT('Ctrl Pts',(5.24717057422674,-6.45256662049017,
33.5663782341735));
#245150=CARTESIAN_POINT('Ctrl Pts',(7.63660495834726,-1.83743194400528,
33.7783173886065));
#245151=CARTESIAN_POINT('Ctrl Pts',(7.60098652584082,2.0454275538338,33.9372717544313));
#245152=CARTESIAN_POINT('Ctrl Pts',(5.68872110083175,5.41593913245269,34.096226120256));
#245153=CARTESIAN_POINT('Ctrl Pts',(1.29614751503337,8.21975975587624,34.3081652746891));
#245154=CARTESIAN_POINT('Ctrl Pts',(-4.25662087832244,7.15262895498851,
34.520104429122));
#245155=CARTESIAN_POINT('Ctrl Pts',(-7.28258603280336,2.92121732779361,
34.7320435835551));
#245156=CARTESIAN_POINT('Ctrl Pts',(-8.0196334935899,-2.20258163340734,
34.943982737988));
#245157=CARTESIAN_POINT('Ctrl Pts',(-3.93397982316526,-8.01832335541715,
35.2089066810293));
#245158=CARTESIAN_POINT('Ctrl Pts',(4.63277167774011,-7.62811865864157,
35.5268154126789));
#245159=CARTESIAN_POINT('Ctrl Pts',(8.18228173064822,-1.489523651103,35.7917393557201));
#245160=CARTESIAN_POINT('Ctrl Pts',(6.99619053994434,3.57032342617563,36.0036785101531));
#245161=CARTESIAN_POINT('Ctrl Pts',(4.44406877510223,6.4968471404334,36.1626328759779));
#245162=CARTESIAN_POINT('Ctrl Pts',(0.79950220057253,7.81375330303946,36.3215872418026));
#245163=CARTESIAN_POINT('Ctrl Pts',(-4.36075182984694,7.08719213112898,
36.5335263962357));
#245164=CARTESIAN_POINT('Ctrl Pts',(-7.88504990360797,2.66550375860217,
36.7454655506687));
#245165=CARTESIAN_POINT('Ctrl Pts',(-7.43205025729338,-2.51678345799743,
36.9574047051017));
#245166=CARTESIAN_POINT('Ctrl Pts',(-4.65990284639874,-6.88848261124738,
37.1693438595348));
#245167=CARTESIAN_POINT('Ctrl Pts',(2.2258770754351,-8.64957674838206,37.4342678025759));
#245168=CARTESIAN_POINT('Ctrl Pts',(8.48001574055104,-2.78210365162642,
37.7521765342255));
#245169=CARTESIAN_POINT('Ctrl Pts',(7.18447574385862,4.18947768973679,38.0171004772667));
#245170=CARTESIAN_POINT('Ctrl Pts',(2.99296870210795,7.2619577103497,38.2290396316998));
#245171=CARTESIAN_POINT('Ctrl Pts',(-0.848946808315632,7.82547502460054,
38.3879939975245));
#245172=CARTESIAN_POINT('Ctrl Pts',(-4.47400753862085,6.45578817758485,
38.5469483633493));
#245173=CARTESIAN_POINT('Ctrl Pts',(-7.92160068496547,2.54807602182595,
38.7588875177823));
#245174=CARTESIAN_POINT('Ctrl Pts',(-7.7234300205534,-3.10282951306144,
38.9708266722154));
#245175=CARTESIAN_POINT('Ctrl Pts',(-4.0092055796552,-6.74506046091847,
39.1827658266483));
#245176=CARTESIAN_POINT('Ctrl Pts',(0.939669008123714,-8.26334734708059,
39.3947049810814));
#245177=CARTESIAN_POINT('Ctrl Pts',(7.3158380211903,-5.12330174094849,39.6596289241226));
#245178=CARTESIAN_POINT('Ctrl Pts',(8.25123304473913,3.40116464314677,39.9775376557722));
#245179=CARTESIAN_POINT('Ctrl Pts',(2.73336067432644,7.85475362127551,40.2424615988134));
#245180=CARTESIAN_POINT('Ctrl Pts',(-2.4488613754721,7.46304022516467,40.4544007532464));
#245181=CARTESIAN_POINT('Ctrl Pts',(-5.73390537707544,5.39268941908779,
40.6133551190712));
#245182=CARTESIAN_POINT('Ctrl Pts',(-7.59702900000426,1.99476685920308,
40.7723094848959));
#245183=CARTESIAN_POINT('Ctrl Pts',(-7.67483203665867,-3.2158050367097,
40.984248639329));
#245184=CARTESIAN_POINT('Ctrl Pts',(-3.84944586892954,-7.3797485574843,
41.1961877937619));
#245185=CARTESIAN_POINT('Ctrl Pts',(1.3407144388163,-7.73123889133776,41.4081269481951));
#245186=CARTESIAN_POINT('Ctrl Pts',(6.08757707586265,-5.66632972644233,
41.6200661026279));
#245187=CARTESIAN_POINT('Ctrl Pts',(8.88934894509868,0.865553010145839,
41.8849900456693));
#245188=CARTESIAN_POINT('Ctrl Pts',(4.05639088500875,7.94962015925316,42.2028987773188));
#245189=CARTESIAN_POINT('Ctrl Pts',(-3.03157875478146,7.74454293554194,
42.4678227203601));
#245190=CARTESIAN_POINT('Ctrl Pts',(-6.71361527772728,4.07691811806076,
42.6797618747931));
#245191=CARTESIAN_POINT('Ctrl Pts',(-7.86278984604215,0.36783947718078,
42.8387162406178));
#245192=CARTESIAN_POINT('Ctrl Pts',(-7.06844244113665,-3.42506436520817,
42.9976706064427));
#245193=CARTESIAN_POINT('Ctrl Pts',(-3.73905835505177,-7.43396875447881,
43.2096097608755));
#245194=CARTESIAN_POINT('Ctrl Pts',(1.87482309910048,-8.10949817291979,
43.4215489153087));
#245195=CARTESIAN_POINT('Ctrl Pts',(6.04620311476629,-5.00129962073608,
43.6334880697416));
#245196=CARTESIAN_POINT('Ctrl Pts',(8.30941427114553,-0.345719096687952,
43.8454272241747));
#245197=CARTESIAN_POINT('Ctrl Pts',(6.19008193137986,6.43836876575923,44.1103511672159));
#245198=CARTESIAN_POINT('Ctrl Pts',(-2.08820682902614,8.67699025743347,
44.4282598988655));
#245199=CARTESIAN_POINT('Ctrl Pts',(-7.33935153427196,3.91181979176889,
44.6931838419066));
#245200=CARTESIAN_POINT('Ctrl Pts',(-7.75138513226923,-1.26882621739172,
44.9051229963398));
#245201=CARTESIAN_POINT('Ctrl Pts',(-6.21232498471946,-4.83381715916377,
45.0640773621644));
#245202=CARTESIAN_POINT('Ctrl Pts',(-3.1423196732166,-7.19859510743567,
45.2230317279893));
#245203=CARTESIAN_POINT('Ctrl Pts',(1.99394098904562,-8.07890142019655,
45.4349708824222));
#245204=CARTESIAN_POINT('Ctrl Pts',(6.69793464556163,-4.9413149821981,45.6469100368553));
#245205=CARTESIAN_POINT('Ctrl Pts',(7.84550783565501,0.132577532259812,
45.8588491912883));
#245206=CARTESIAN_POINT('Ctrl Pts',(6.5372264605892,5.14106578700417,46.0707883457213));
#245207=CARTESIAN_POINT('Ctrl Pts',(0.515473790672442,8.9165011889322,46.3357122887626));
#245208=CARTESIAN_POINT('Ctrl Pts',(-7.22908153439403,5.23365530556507,
46.653621020412));
#245209=CARTESIAN_POINT('Ctrl Pts',(-8.11937222462681,-1.80116898287009,
46.9185449634533));
#245210=CARTESIAN_POINT('Ctrl Pts',(-5.06335374042494,-6.00469319266439,
47.1304841178864));
#245211=CARTESIAN_POINT('Ctrl Pts',(-1.57582759165378,-7.71203847535647,
47.2894384837111));
#245212=CARTESIAN_POINT('Ctrl Pts',(2.29419876660426,-7.51203011633953,
47.448392849536));
#245213=CARTESIAN_POINT('Ctrl Pts',(6.76852739204454,-4.84060799571636,
47.6603320039688));
#245214=CARTESIAN_POINT('Ctrl Pts',(8.30159923837348,0.601973716159747,
47.8722711584019));
#245215=CARTESIAN_POINT('Ctrl Pts',(5.87377004300275,5.2027296185087,48.0842103128349));
#245216=CARTESIAN_POINT('Ctrl Pts',(1.62283811694658,8.15673241374986,48.2961494672681));
#245217=CARTESIAN_POINT('Ctrl Pts',(-5.40690334344646,7.10880460525727,
48.5610734103091));
#245218=CARTESIAN_POINT('Ctrl Pts',(-8.89520681995229,-0.725302225738014,
48.8789821419588));
#245219=CARTESIAN_POINT('Ctrl Pts',(-4.99671402105694,-6.64840311794251,
49.1439060849999));
#245220=CARTESIAN_POINT('Ctrl Pts',(0.0584426308466855,-7.8543284816466,
49.3558452394331));
#245221=CARTESIAN_POINT('Ctrl Pts',(3.81811125282832,-6.88337101317528,
49.5147996052577));
#245222=CARTESIAN_POINT('Ctrl Pts',(6.62798156908878,-4.21471289286708,
49.6737539710826));
#245223=CARTESIAN_POINT('Ctrl Pts',(8.28973554545862,0.724384850345556,
49.8856931255155));
#245224=CARTESIAN_POINT('Ctrl Pts',(5.91499521963495,5.85591613850521,50.0976322799486));
#245225=CARTESIAN_POINT('Ctrl Pts',(1.0787304308988,7.77212394772737,50.3095714343816));
#245226=CARTESIAN_POINT('Ctrl Pts',(-4.07158788133815,7.25176249941163,
50.5215105888146));
#245227=CARTESIAN_POINT('Ctrl Pts',(-8.73038403875477,1.88417122814108,
50.7864345318559));
#245228=CARTESIAN_POINT('Ctrl Pts',(-6.2857385062876,-6.3356340739471,51.1043432635053));
#245229=CARTESIAN_POINT('Ctrl Pts',(0.527677938456462,-8.29999825422641,
51.3692672065466));
#245230=CARTESIAN_POINT('Ctrl Pts',(5.1521478128489,-5.92868150209316,51.5812063609797));
#245231=CARTESIAN_POINT('Ctrl Pts',(7.37682666022324,-2.74612426321454,
51.7401607268044));
#245232=CARTESIAN_POINT('Ctrl Pts',(7.77594124838299,1.10845935928047,51.8991150926292));
#245233=CARTESIAN_POINT('Ctrl Pts',(5.82637752128669,5.94119296139214,52.1110542470622));
#245234=CARTESIAN_POINT('Ctrl Pts',(0.685273979183349,8.29513844628072,
52.3229934014952));
#245235=CARTESIAN_POINT('Ctrl Pts',(-4.23481459867255,6.60574865675754,
52.5349325559282));
#245236=CARTESIAN_POINT('Ctrl Pts',(-7.80895369693254,2.86114127272587,
52.7468717103612));
#245237=CARTESIAN_POINT('Ctrl Pts',(-7.85749528809018,-4.24611286693366,
53.0117956534025));
#245238=CARTESIAN_POINT('Ctrl Pts',(-0.654950523743482,-8.90066331796877,
53.3297043850521));
#245239=CARTESIAN_POINT('Ctrl Pts',(5.7984348266577,-5.96209431222774,53.5946283280932));
#245240=CARTESIAN_POINT('Ctrl Pts',(7.76940802209826,-1.15333881615956,
53.8065674825263));
#245241=CARTESIAN_POINT('Ctrl Pts',(7.38977708548394,2.71108182666114,53.965521848351));
#245242=CARTESIAN_POINT('Ctrl Pts',(5.18629647367542,5.89883660874095,54.1244762141758));
#245243=CARTESIAN_POINT('Ctrl Pts',(0.562497492298242,8.30229157499353,
54.3364153686088));
#245244=CARTESIAN_POINT('Ctrl Pts',(-4.87383286167256,6.74719760389385,
54.5483545230418));
#245245=CARTESIAN_POINT('Ctrl Pts',(-7.51284246057468,2.264236772948,54.7602936774749));
#245246=CARTESIAN_POINT('Ctrl Pts',(-7.79284720783111,-2.90472367338639,
54.9722328319079));
#245247=CARTESIAN_POINT('Ctrl Pts',(-3.20780210334241,-8.33544913888216,
55.2371567749491));
#245248=CARTESIAN_POINT('Ctrl Pts',(5.29064770703959,-7.18747622802216,
55.5550655065987));
#245249=CARTESIAN_POINT('Ctrl Pts',(8.28210071942974,-0.758434374298012,
55.8199894496399));
#245250=CARTESIAN_POINT('Ctrl Pts',(6.65220405514383,4.17637075071561,56.031928604073));
#245251=CARTESIAN_POINT('Ctrl Pts',(3.85073774300707,6.86517216671053,56.1908829698977));
#245252=CARTESIAN_POINT('Ctrl Pts',(0.103792740727409,7.85386347706992,
56.3498373357225));
#245253=CARTESIAN_POINT('Ctrl Pts',(-4.97175406669828,6.67278879669655,
56.5617764901554));
#245254=CARTESIAN_POINT('Ctrl Pts',(-8.09027032914091,1.9561309442193,56.7737156445885));
#245255=CARTESIAN_POINT('Ctrl Pts',(-7.17972762657543,-3.16560913720782,
56.9856547990215));
#245256=CARTESIAN_POINT('Ctrl Pts',(-4.03101020161681,-7.27439646828475,
57.1975939534545));
#245257=CARTESIAN_POINT('Ctrl Pts',(2.98376171108668,-8.41824641671605,
57.4625178964958));
#245258=CARTESIAN_POINT('Ctrl Pts',(8.69322924019813,-2.01953783469166,
57.7804266281453));
#245259=CARTESIAN_POINT('Ctrl Pts',(6.78487021025572,4.80977663274288,58.0453505711865));
#245260=CARTESIAN_POINT('Ctrl Pts',(2.33753412088888,7.49865492421042,58.2572897256197));
#245261=CARTESIAN_POINT('Ctrl Pts',(-1.53920737148137,7.71943072457896,
58.4162440914443));
#245262=CARTESIAN_POINT('Ctrl Pts',(-5.02860028505904,6.03383158719109,
58.5751984572691));
#245263=CARTESIAN_POINT('Ctrl Pts',(-8.11626918732383,1.83592573486714,
58.7871376117021));
#245264=CARTESIAN_POINT('Ctrl Pts',(-7.41801709661686,-3.77517478056459,
58.9990767661352));
#245265=CARTESIAN_POINT('Ctrl Pts',(-3.39558595242505,-7.07386500020164,
59.2110159205681));
#245266=CARTESIAN_POINT('Ctrl Pts',(1.66838281260135,-8.14753864758852,
59.4229550750012));
#245267=CARTESIAN_POINT('Ctrl Pts',(7.74114274238885,-4.45470714223283,
59.6878790180424));
#245268=CARTESIAN_POINT('Ctrl Pts',(7.91730025097074,4.11911694715805,60.0057877496919));
#245269=CARTESIAN_POINT('Ctrl Pts',(2.02640606933998,8.06610770254379,60.2707116927332));
#245270=CARTESIAN_POINT('Ctrl Pts',(-3.10070113652638,7.21661582049712,
60.4826508471663));
#245271=CARTESIAN_POINT('Ctrl Pts',(-6.18931300628282,4.86324732604201,
60.6416052129909));
#245272=CARTESIAN_POINT('Ctrl Pts',(-7.74393301904625,1.31356227336414,
60.8005595788158));
#245273=CARTESIAN_POINT('Ctrl Pts',(-7.35959692812879,-3.88339823872434,
61.0124987332486));
#245274=CARTESIAN_POINT('Ctrl Pts',(-3.18020017803199,-7.69189502639994,
61.2244378876819));
#245275=CARTESIAN_POINT('Ctrl Pts',(2.02068703217843,-7.58197823258349,
61.4363770421147));
#245276=CARTESIAN_POINT('Ctrl Pts',(6.56584653849631,-5.10446338572904,
61.6483161965479));
#245277=CARTESIAN_POINT('Ctrl Pts',(8.77764566147108,1.65004343056681,61.9132401395891));
#245278=CARTESIAN_POINT('Ctrl Pts',(3.33582081627798,8.27786610003282,62.2311488712386));
#245279=CARTESIAN_POINT('Ctrl Pts',(-3.70607576389775,7.44536214425762,
62.4960728142798));
#245280=CARTESIAN_POINT('Ctrl Pts',(-7.04854519778669,3.46581909993344,
62.7080119687128));
#245281=CARTESIAN_POINT('Ctrl Pts',(-7.86444710766331,-0.330517374373583,
62.8669663345378));
#245282=CARTESIAN_POINT('Ctrl Pts',(-6.73704645906731,-4.0380873514387,
63.0259207003624));
#245283=CARTESIAN_POINT('Ctrl Pts',(-3.06544137532573,-7.73611776018765,
63.2378598547954));
#245284=CARTESIAN_POINT('Ctrl Pts',(2.58622015592732,-7.9114086972287,63.4497990092285));
#245285=CARTESIAN_POINT('Ctrl Pts',(6.46569125196403,-4.44571778632658,
63.6617381636614));
#245286=CARTESIAN_POINT('Ctrl Pts',(8.30735312908238,0.39213672622584,63.8736773180945));
#245287=CARTESIAN_POINT('Ctrl Pts',(5.59506223820433,6.96167977083983,64.1386012611357));
#245288=CARTESIAN_POINT('Ctrl Pts',(-2.84906306070886,8.45775427430321,
64.4565099927852));
#245289=CARTESIAN_POINT('Ctrl Pts',(-7.65718543400385,3.24590915710281,
64.7214339358265));
#245290=CARTESIAN_POINT('Ctrl Pts',(-7.60841691152547,-1.95086738122589,
64.9333730902595));
#245291=CARTESIAN_POINT('Ctrl Pts',(-5.75943529500526,-5.36541472084175,
65.0923274560842));
#245292=CARTESIAN_POINT('Ctrl Pts',(-2.49191335788211,-7.44877924671545,
65.2512818219091));
#245293=CARTESIAN_POINT('Ctrl Pts',(2.70215732371306,-7.8703744906464,65.4632209763419));
#245294=CARTESIAN_POINT('Ctrl Pts',(7.10954108041586,-4.32820377236875,
65.6751601307752));
#245295=CARTESIAN_POINT('Ctrl Pts',(7.80287924095887,0.827433110696188,
65.887099285208));
#245296=CARTESIAN_POINT('Ctrl Pts',(6.05582542777371,5.70025136386296,66.0990384396412));
#245297=CARTESIAN_POINT('Ctrl Pts',(-0.276858574999038,8.92709672907416,
66.3639623826822));
#245298=CARTESIAN_POINT('Ctrl Pts',(-7.66450876371097,4.57231594512697,
66.681871114332));
#245299=CARTESIAN_POINT('Ctrl Pts',(-7.92777213317072,-2.51373109686328,
66.9467950573731));
#245300=CARTESIAN_POINT('Ctrl Pts',(-4.51120686176332,-6.42984479530528,
67.1587342118062));
#245301=CARTESIAN_POINT('Ctrl Pts',(-0.886078103971636,-7.8213576595246,
67.3176885776309));
#245302=CARTESIAN_POINT('Ctrl Pts',(2.95098939665996,-7.27912123939608,
67.4766429434557));
#245303=CARTESIAN_POINT('Ctrl Pts',(7.17092995154372,-4.2216362360521,67.6885820978886));
#245304=CARTESIAN_POINT('Ctrl Pts',(8.21557120872505,1.33540700803337,67.9005212523217));
#245305=CARTESIAN_POINT('Ctrl Pts',(5.38951469707404,5.70286782255762,68.1124604067547));
#245306=CARTESIAN_POINT('Ctrl Pts',(0.893488666859789,8.26846813139917,
68.3243995611877));
#245307=CARTESIAN_POINT('Ctrl Pts',(-6.01570377578533,6.60159179412591,
68.589323504229));
#245308=CARTESIAN_POINT('Ctrl Pts',(-8.79591151323072,-1.51086382949544,
68.9072322358786));
#245309=CARTESIAN_POINT('Ctrl Pts',(-4.38777482885245,-7.06511474193006,
69.1721561789197));
#245310=CARTESIAN_POINT('Ctrl Pts',(0.75437163081327,-7.81823600615633,
69.3840953333529));
#245311=CARTESIAN_POINT('Ctrl Pts',(4.41318407711473,-6.51786622649009,
69.5430496991776));
#245312=CARTESIAN_POINT('Ctrl Pts',(6.97546114514699,-3.61066149413494,
69.7020040650023));
#245313=CARTESIAN_POINT('Ctrl Pts',(8.19290593630667,1.4562846082975,69.9139432194354));
#245314=CARTESIAN_POINT('Ctrl Pts',(5.37268034101302,6.35713797319922,70.1258823738682));
#245315=CARTESIAN_POINT('Ctrl Pts',(0.385615112503278,7.83714650892533,
70.3378215283014));
#245316=CARTESIAN_POINT('Ctrl Pts',(-4.69832249301022,6.86234238559436,
70.5497606827343));
#245317=CARTESIAN_POINT('Ctrl Pts',(-8.86300835786554,1.10294573286832,
70.8146846257757));
#245318=CARTESIAN_POINT('Ctrl Pts',(-5.69947739928546,-6.86782325365974,
71.1325933574252));
#245319=CARTESIAN_POINT('Ctrl Pts',(1.26131134764555,-8.22056938840904,
71.3975173004663));
#245320=CARTESIAN_POINT('Ctrl Pts',(5.65728340963835,-5.44868257745799,
71.6094564548995));
#245321=CARTESIAN_POINT('Ctrl Pts',(7.59134286873771,-2.08150328900666,
71.7684108207242));
#245322=CARTESIAN_POINT('Ctrl Pts',(7.64681098033558,1.79335174723873,71.927365186549));
#245323=CARTESIAN_POINT('Ctrl Pts',(5.27749319719932,6.4341248068459,72.139304340982));
#245324=CARTESIAN_POINT('Ctrl Pts',(-0.0538749626755808,8.32342009874787,
72.351243495415));
#245325=CARTESIAN_POINT('Ctrl Pts',(-4.80221181121656,6.20417977333355,
72.563182649848));
#245326=CARTESIAN_POINT('Ctrl Pts',(-8.03515042318792,2.15826191845753,
72.775121804281));
#245327=CARTESIAN_POINT('Ctrl Pts',(-7.44316476216323,-4.92692186719272,
73.0400457473223));
#245328=CARTESIAN_POINT('Ctrl Pts',(0.124338371616316,-8.92190591677168,
73.3579544789718));
#245329=CARTESIAN_POINT('Ctrl Pts',(7.56292883494232,-4.72784949414696,
73.6758632106214));
#245330=CARTESIAN_POINT('Ctrl Pts',(8.07241182584164,3.8018322885345,73.9937719422708));
#245331=CARTESIAN_POINT('Ctrl Pts',(1.1721054173287,8.84175448043975,74.3116806739204));
#245332=CARTESIAN_POINT('Ctrl Pts',(-6.79899311505185,5.77836982546636,
74.6295894055698));
#245333=CARTESIAN_POINT('Ctrl Pts',(-8.53900169652047,-2.60013668658995,
74.9474981372195));
#245334=CARTESIAN_POINT('Ctrl Pts',(-3.45384967879028,-7.56919145141941,
75.2124220802606));
#245335=CARTESIAN_POINT('Ctrl Pts',(1.72439296830596,-7.65372810011474,
75.4243612346938));
#245336=CARTESIAN_POINT('Ctrl Pts',(6.38248034882689,-5.34286152250664,
75.6363003891266));
#245337=CARTESIAN_POINT('Ctrl Pts',(8.32160028852796,-0.0294128292769415,
75.8482395435598));
#245338=CARTESIAN_POINT('Ctrl Pts',(6.25293669920985,4.75295816244786,76.0601786979928));
#245339=CARTESIAN_POINT('Ctrl Pts',(3.23035682717462,7.1781569544004,76.2191330638176));
#245340=CARTESIAN_POINT('Ctrl Pts',(-0.597346084762983,7.83174150887795,
76.3780874296422));
#245341=CARTESIAN_POINT('Ctrl Pts',(-5.5341526716022,6.20820598826635,76.5900265840752));
#245342=CARTESIAN_POINT('Ctrl Pts',(-8.92472137507585,-0.0196785603991093,
76.8549505271166));
#245343=CARTESIAN_POINT('Ctrl Pts',(-4.79470389098473,-7.53526516049846,
77.1728592587661));
#245344=CARTESIAN_POINT('Ctrl Pts',(2.29796072061545,-7.99283140019599,
77.4377832018074));
#245345=CARTESIAN_POINT('Ctrl Pts',(6.28751497364375,-4.69432847951197,
77.6497223562402));
#245346=CARTESIAN_POINT('Ctrl Pts',(8.32287495204422,0.0930042452481067,
77.8616615106735));
#245347=CARTESIAN_POINT('Ctrl Pts',(6.34089786961344,5.3886442403136,78.0736006651065));
#245348=CARTESIAN_POINT('Ctrl Pts',(1.65921369754144,7.67730060102996,78.2855398195393));
#245349=CARTESIAN_POINT('Ctrl Pts',(-2.2140023866738,7.55360624316107,78.4444941853642));
#245350=CARTESIAN_POINT('Ctrl Pts',(-5.54685934390654,5.56113677446008,
78.6034485511889));
#245351=CARTESIAN_POINT('Ctrl Pts',(-8.24137413950221,1.11721374771911,
78.8153877056219));
#245352=CARTESIAN_POINT('Ctrl Pts',(-6.76703924878134,-5.8187583439523,
79.0803116486632));
#245353=CARTESIAN_POINT('Ctrl Pts',(1.25787713722511,-8.84236683484207,
79.3982203803127));
#245354=CARTESIAN_POINT('Ctrl Pts',(6.94350807591193,-4.57750836564132,
79.663144323354));
#245355=CARTESIAN_POINT('Ctrl Pts',(7.82919898218652,0.522698162297944,
79.875083477787));
#245356=CARTESIAN_POINT('Ctrl Pts',(6.26214530801236,5.4831066289172,80.08702263222));
#245357=CARTESIAN_POINT('Ctrl Pts',(1.31269087512095,8.21713402263037,80.298961786653));
#245358=CARTESIAN_POINT('Ctrl Pts',(-3.73217515603941,6.91120923150708,
80.510900941086));
#245359=CARTESIAN_POINT('Ctrl Pts',(-6.59409621375978,4.29844915850133,
80.6698553069108));
#245360=CARTESIAN_POINT('Ctrl Pts',(-7.83023991261764,0.617441780400932,
80.8288096727356));
#245361=CARTESIAN_POINT('Ctrl Pts',(-6.98724940777033,-4.51073838040169,
81.0407488271686));
#245362=CARTESIAN_POINT('Ctrl Pts',(-1.35670925061133,-8.82100378077065,
81.3056727702099));
#245363=CARTESIAN_POINT('Ctrl Pts',(6.70585217355222,-5.89925870828381,
81.6235815018593));
#245364=CARTESIAN_POINT('Ctrl Pts',(8.25156648580112,1.03804515956493,81.8885054449006));
#245365=CARTESIAN_POINT('Ctrl Pts',(5.60768125197603,5.48848621915918,82.1004445993336));
#245366=CARTESIAN_POINT('Ctrl Pts',(1.19143489443458,8.23768202600654,82.3123837537668));
#245367=CARTESIAN_POINT('Ctrl Pts',(-4.34647681532778,7.09595575796037,
82.5243229081995));
#245368=CARTESIAN_POINT('Ctrl Pts',(-7.32964717965211,2.82315721689529,
82.7362620626329));
#245369=CARTESIAN_POINT('Ctrl Pts',(-7.80465416182032,-1.02281154586677,
82.8952164284572));
#245370=CARTESIAN_POINT('Ctrl Pts',(-6.34991677060407,-4.62303454941871,
83.0541707942825));
#245371=CARTESIAN_POINT('Ctrl Pts',(-2.37461486514492,-7.97054698682075,
83.266109948715));
#245372=CARTESIAN_POINT('Ctrl Pts',(4.7057401633254,-7.58332230646015,83.5310338917566));
#245373=CARTESIAN_POINT('Ctrl Pts',(8.93057461629925,-0.120597279459235,
83.8489426234059));
#245374=CARTESIAN_POINT('Ctrl Pts',(5.59340514972506,6.15464914145068,84.1138665664474));
#245375=CARTESIAN_POINT('Ctrl Pts',(0.690760647269976,7.81616400349735,
84.3258057208802));
#245376=CARTESIAN_POINT('Ctrl Pts',(-4.45195376509949,7.03271142184339,
84.5377448753135));
#245377=CARTESIAN_POINT('Ctrl Pts',(-7.91645548039882,2.56401666373547,
84.7496840297463));
#245378=CARTESIAN_POINT('Ctrl Pts',(-7.40403163563121,-2.62188100188642,
84.9616231841794));
#245379=CARTESIAN_POINT('Ctrl Pts',(-5.26380643066461,-5.85244495100042,
85.1205775500041));
#245380=CARTESIAN_POINT('Ctrl Pts',(-1.81742586590513,-7.64139088521482,
85.279531915829));
#245381=CARTESIAN_POINT('Ctrl Pts',(3.37940832923157,-7.59921143087983,
85.4914710702619));
#245382=CARTESIAN_POINT('Ctrl Pts',(8.50631608405412,-2.70062110755077,
85.756395013303));
#245383=CARTESIAN_POINT('Ctrl Pts',(6.86270348148387,5.71603075624413,86.0743037449527));
#245384=CARTESIAN_POINT('Ctrl Pts',(0.246702924124477,8.31294321468396,
86.3392276879939));
#245385=CARTESIAN_POINT('Ctrl Pts',(-4.5581827942018,6.38690375816221,86.5511668424269));
#245386=CARTESIAN_POINT('Ctrl Pts',(-7.95545457184888,2.44737917470092,
86.7631059968599));
#245387=CARTESIAN_POINT('Ctrl Pts',(-7.6812897496541,-3.20034945074897,
86.975045151293));
#245388=CARTESIAN_POINT('Ctrl Pts',(-3.91957469415952,-6.8066789748294,
87.186984305726));
#245389=CARTESIAN_POINT('Ctrl Pts',(-0.192843600664311,-7.86902671171469,
87.3459386715508));
#245390=CARTESIAN_POINT('Ctrl Pts',(3.58863375468831,-6.98681609987104,
87.5048930373757));
#245391=CARTESIAN_POINT('Ctrl Pts',(7.50907619223898,-3.57521884169963,
87.7168321918084));
#245392=CARTESIAN_POINT('Ctrl Pts',(8.21822365360159,3.48016776431378,87.9817561348498));
#245393=CARTESIAN_POINT('Ctrl Pts',(1.49618716924779,8.80517635460401,88.2996648664993));
#245394=CARTESIAN_POINT('Ctrl Pts',(-5.21858018044238,6.47551605075817,
88.5645888095405));
#245395=CARTESIAN_POINT('Ctrl Pts',(-7.61617805723871,1.88769748683935,
88.7765279639737));
#245396=CARTESIAN_POINT('Ctrl Pts',(-7.63506557650729,-3.31431680922974,
88.9884671184066));
#245397=CARTESIAN_POINT('Ctrl Pts',(-3.75401500422844,-7.42642714722755,
89.2004062728397));
#245398=CARTESIAN_POINT('Ctrl Pts',(1.44887537003911,-7.71976065766127,
89.4123454272726));
#245399=CARTESIAN_POINT('Ctrl Pts',(4.97081194366405,-6.10326131381598,
89.5712997930973));
#245400=CARTESIAN_POINT('Ctrl Pts',(7.26977119842067,-2.97393983821432,
89.7302541589222));
#245401=CARTESIAN_POINT('Ctrl Pts',(8.02941166382867,2.16724787684003,89.942193313355));
#245402=CARTESIAN_POINT('Ctrl Pts',(3.97993814034131,7.98817000867177,90.2071172563967));
#245403=CARTESIAN_POINT('Ctrl Pts',(-4.58949041866838,7.66200263495448,
90.5250259880459));
#245404=CARTESIAN_POINT('Ctrl Pts',(-8.17548675502426,1.52555024229132,
90.7899499310872));
#245405=CARTESIAN_POINT('Ctrl Pts',(-7.01336106360832,-3.51885444325954,
91.0018890855202));
#245406=CARTESIAN_POINT('Ctrl Pts',(-3.64478579961144,-7.4829445236792,
91.2138282399533));
#245407=CARTESIAN_POINT('Ctrl Pts',(1.97767450617641,-8.08289876051093,
91.4257673943862));
#245408=CARTESIAN_POINT('Ctrl Pts',(6.12090517289929,-4.92224179758123,
91.6377065488193));
#245409=CARTESIAN_POINT('Ctrl Pts',(7.74518389296699,-1.40388621623011,
91.7966609146438));
#245410=CARTESIAN_POINT('Ctrl Pts',(7.45660122098534,2.46839819921847,91.955615280469));
#245411=CARTESIAN_POINT('Ctrl Pts',(4.69030892220141,6.86799950795086,92.1675544349015));
#245412=CARTESIAN_POINT('Ctrl Pts',(-2.17135494908673,8.65655736268543,
92.4324783779433));
#245413=CARTESIAN_POINT('Ctrl Pts',(-8.46917142270095,2.83599049610602,
92.7503871095924));
#245414=CARTESIAN_POINT('Ctrl Pts',(-7.20274227732176,-4.15769057408234,
93.0153110526339));
#245415=CARTESIAN_POINT('Ctrl Pts',(-3.03948342129891,-7.23402450459174,
93.2272502070669));
#245416=CARTESIAN_POINT('Ctrl Pts',(2.09740634433605,-8.05480036352543,
93.4391893614998));
#245417=CARTESIAN_POINT('Ctrl Pts',(6.75876976609282,-4.85422291144522,
93.6511285159329));
#245418=CARTESIAN_POINT('Ctrl Pts',(7.85084453217398,0.241214802851541,
93.8630676703659));
#245419=CARTESIAN_POINT('Ctrl Pts',(6.79673529994191,3.97028453722395,94.0220220361907));
#245420=CARTESIAN_POINT('Ctrl Pts',(4.05932161038303,6.72426944003453,94.1809764020154));
#245421=CARTESIAN_POINT('Ctrl Pts',(-0.903250091444178,8.26756035957407,
94.3929155564486));
#245422=CARTESIAN_POINT('Ctrl Pts',(-7.27895883489408,5.16406099579625,
94.6578394994895));
#245423=CARTESIAN_POINT('Ctrl Pts',(-8.27803812656465,-3.35317632346431,
94.9757482311394));
#245424=CARTESIAN_POINT('Ctrl Pts',(-2.76790867666667,-7.84248486010434,
95.2406721741806));
#245425=CARTESIAN_POINT('Ctrl Pts',(2.39536034850992,-7.47206924500643,
95.4526113286135));
#245426=CARTESIAN_POINT('Ctrl Pts',(6.83145361629515,-4.75501459071554,
95.6645504830465));
#245427=CARTESIAN_POINT('Ctrl Pts',(8.29117690268064,0.707696540548531,
95.8764896374795));
#245428=CARTESIAN_POINT('Ctrl Pts',(5.80717622726645,5.28872845918113,96.0884287919126));
#245429=CARTESIAN_POINT('Ctrl Pts',(2.5813499698349,7.43608784087639,96.2473831577373));
#245430=CARTESIAN_POINT('Ctrl Pts',(-1.28912224472129,7.74803557534874,
96.406337523562));
#245431=CARTESIAN_POINT('Ctrl Pts',(-6.06265053096723,5.6932138170156,96.6182766779951));
#245432=CARTESIAN_POINT('Ctrl Pts',(-8.88783914592498,-0.81060656581987,
96.8832006210364));
#245433=CARTESIAN_POINT('Ctrl Pts',(-4.10796116509668,-7.93059655682706,
97.2011093526859));
#245434=CARTESIAN_POINT('Ctrl Pts',(2.99735521759814,-7.75768966399591,
97.4660332957272));
#245435=CARTESIAN_POINT('Ctrl Pts',(6.67884388789089,-4.11856945098259,
97.67797245016));
#245436=CARTESIAN_POINT('Ctrl Pts',(8.2818763535548,0.830329051605735,97.8899116045933));
#245437=CARTESIAN_POINT('Ctrl Pts',(5.83832505511409,5.92945270458212,98.1018507590259));
#245438=CARTESIAN_POINT('Ctrl Pts',(0.972215262230236,7.79414792862997,
98.3137899134594));
#245439=CARTESIAN_POINT('Ctrl Pts',(-2.87479385321957,7.3276415268139,98.4727442792838));
#245440=CARTESIAN_POINT('Ctrl Pts',(-6.01793319755471,5.04761047115112,
98.631698645109));
#245441=CARTESIAN_POINT('Ctrl Pts',(-8.30796135692593,0.382352087374534,
98.8436377995414));
#245442=CARTESIAN_POINT('Ctrl Pts',(-6.2246672233863,-6.39564583497924,
99.1085617425833));
#245443=CARTESIAN_POINT('Ctrl Pts',(2.03665925768212,-8.69607530724048,
99.4264704742322));
#245444=CARTESIAN_POINT('Ctrl Pts',(7.32190243800059,-3.94406286863336,
99.6913944172741));
#245445=CARTESIAN_POINT('Ctrl Pts',(7.75205668761658,1.21457281105868,99.9033335717067));
#245446=CARTESIAN_POINT('Ctrl Pts',(5.75151053316249,6.01656453937227,100.11527272614));
#245447=CARTESIAN_POINT('Ctrl Pts',(0.579208469572439,8.30114247401078,
100.327211880573));
#245448=CARTESIAN_POINT('Ctrl Pts',(-4.33005325803172,6.55321167307216,
100.539151035006));
#245449=CARTESIAN_POINT('Ctrl Pts',(-6.94913167145573,3.69707168672269,
100.69810540083));
#245450=CARTESIAN_POINT('Ctrl Pts',(-7.85414848838492,-0.0790124110920571,
100.857059766655));
#245451=CARTESIAN_POINT('Ctrl Pts',(-6.55994553863086,-5.11229200624264,
101.068998921088));
#245452=CARTESIAN_POINT('Ctrl Pts',(-0.569530316075434,-8.9065370884232,
101.33392286413));
#245453=CARTESIAN_POINT('Ctrl Pts',(7.20233366355529,-5.28167553716792,
101.651831595779));
#245454=CARTESIAN_POINT('Ctrl Pts',(8.12708469795813,1.76532760006358,101.91675553882));
#245455=CARTESIAN_POINT('Ctrl Pts',(5.09914544938941,5.96391529847259,102.128694693253));
#245456=CARTESIAN_POINT('Ctrl Pts',(0.456608472163056,8.31086222799173,
102.340633847686));
#245457=CARTESIAN_POINT('Ctrl Pts',(-4.95831198844199,6.68278318145386,
102.55257300212));
#245458=CARTESIAN_POINT('Ctrl Pts',(-7.5510269451248,2.16239138998465,102.764512156552));
#245459=CARTESIAN_POINT('Ctrl Pts',(-7.68328151025241,-1.71054239298817,
102.923466522377));
#245460=CARTESIAN_POINT('Ctrl Pts',(-5.91516802671592,-5.1676569791757,
103.082420888202));
#245461=CARTESIAN_POINT('Ctrl Pts',(-1.65880897520462,-8.14964832435577,
103.294360042635));
#245462=CARTESIAN_POINT('Ctrl Pts',(5.35935853689139,-7.13638870588163,
103.559283985677));
#245463=CARTESIAN_POINT('Ctrl Pts',(8.90611535184792,0.671428343666077,
103.877192717326));
#245464=CARTESIAN_POINT('Ctrl Pts',(5.02588096619366,6.62619104289825,104.142116660367));
#245465=CARTESIAN_POINT('Ctrl Pts',(-0.00473450560939821,7.84662650989841,
104.3540558148));
#245466=CARTESIAN_POINT('Ctrl Pts',(-5.05776822281027,6.61043893201059,
104.565994969233));
#245467=CARTESIAN_POINT('Ctrl Pts',(-8.11255711291596,1.85225967799525,
104.777934123666));
#245468=CARTESIAN_POINT('Ctrl Pts',(-7.14250408114055,-3.26780964873582,
104.989873278099));
#245469=CARTESIAN_POINT('Ctrl Pts',(-4.72436496945928,-6.29596264913808,
105.148827643924));
#245470=CARTESIAN_POINT('Ctrl Pts',(-1.13298728142614,-7.77240189766538,
105.307782009749));
#245471=CARTESIAN_POINT('Ctrl Pts',(4.03965509058027,-7.26977315849979,
105.519721164181));
#245472=CARTESIAN_POINT('Ctrl Pts',(8.71220396331585,-1.93604488325272,
105.784645107223));
#245473=CARTESIAN_POINT('Ctrl Pts',(6.32906011717109,6.30180170382518,106.102553838872));
#245474=CARTESIAN_POINT('Ctrl Pts',(-0.49107598238367,8.30209200158962,
106.367477781914));
#245475=CARTESIAN_POINT('Ctrl Pts',(-5.10633876063979,5.9577575028673,106.579416936347));
#245476=CARTESIAN_POINT('Ctrl Pts',(-8.14106468800239,1.73262460310113,
106.79135609078));
#245477=CARTESIAN_POINT('Ctrl Pts',(-7.36739911305641,-3.8685758534616,
107.003295245213));
#245478=CARTESIAN_POINT('Ctrl Pts',(-3.30084634464836,-7.12729667254717,
107.215234399646));
#245479=CARTESIAN_POINT('Ctrl Pts',(0.505377312957478,-7.85514887290774,
107.37418876547));
#245480=CARTESIAN_POINT('Ctrl Pts',(4.1937781223789,-6.64124359581554,107.533143131295));
#245481=CARTESIAN_POINT('Ctrl Pts',(7.7964078732041,-2.89558962933918,107.745082285728));
#245482=CARTESIAN_POINT('Ctrl Pts',(7.87741842683513,4.19488338538094,108.01000622877));
#245483=CARTESIAN_POINT('Ctrl Pts',(0.70986213373019,8.90313441615905,108.327914960419));
#245484=CARTESIAN_POINT('Ctrl Pts',(-5.77199105250775,5.98748749586195,
108.59283890346));
#245485=CARTESIAN_POINT('Ctrl Pts',(-7.75351674291794,1.20521704214434,
108.804778057893));
#245486=CARTESIAN_POINT('Ctrl Pts',(-7.31125550254137,-3.97799764279321,
109.016717212326));
#245487=CARTESIAN_POINT('Ctrl Pts',(-3.08100760077888,-7.72993149963135,
109.228656366759));
#245488=CARTESIAN_POINT('Ctrl Pts',(2.12740491224856,-7.56095845702261,
109.440595521192));
#245489=CARTESIAN_POINT('Ctrl Pts',(5.49220360160253,-5.63865849671179,
109.599549887017));
#245490=CARTESIAN_POINT('Ctrl Pts',(7.50475105957328,-2.3178876099886,109.758504252842));
#245491=CARTESIAN_POINT('Ctrl Pts',(7.80571865989455,2.87039565730397,109.970443407275));
#245492=CARTESIAN_POINT('Ctrl Pts',(3.2562521477919,8.30948792877077,110.235367350316));
#245493=CARTESIAN_POINT('Ctrl Pts',(-5.25054005740826,7.22506302994313,
110.553276081966));
#245494=CARTESIAN_POINT('Ctrl Pts',(-8.27852566151433,0.794921439503049,
110.818200025007));
#245495=CARTESIAN_POINT('Ctrl Pts',(-6.67386889320644,-4.12662622461439,
111.03013917944));
#245496=CARTESIAN_POINT('Ctrl Pts',(-2.96719894074821,-7.77654503719568,
111.242078333873));
#245497=CARTESIAN_POINT('Ctrl Pts',(2.6863091607575,-7.87579785913017,111.454017488306));
#245498=CARTESIAN_POINT('Ctrl Pts',(6.53309210628831,-4.36034998368643,
111.665956642739));
#245499=CARTESIAN_POINT('Ctrl Pts',(7.83913280410349,-0.711875637752233,
111.824911008564));
#245500=CARTESIAN_POINT('Ctrl Pts',(7.20847053503805,3.11959035518978,111.983865374389));
#245501=CARTESIAN_POINT('Ctrl Pts',(4.06311210333432,7.25668898759164,112.195804528821));
#245502=CARTESIAN_POINT('Ctrl Pts',(-2.93007288723742,8.4300320618526,112.460728471863));
#245503=CARTESIAN_POINT('Ctrl Pts',(-8.68720379970417,2.07417376887848,
112.778637203512));
#245504=CARTESIAN_POINT('Ctrl Pts',(-6.80588226535307,-4.77973365507787,
113.043561146554));
#245505=CARTESIAN_POINT('Ctrl Pts',(-2.38634159792211,-7.47495443326655,
113.255500300987));
#245506=CARTESIAN_POINT('Ctrl Pts',(2.80307929924439,-7.83719775887135,
113.46743945542));
#245507=CARTESIAN_POINT('Ctrl Pts',(7.16241746747704,-4.23606242241895,
113.679378609853));
#245508=CARTESIAN_POINT('Ctrl Pts',(7.79856599689762,0.936115826975124,
113.891317764286));
#245509=CARTESIAN_POINT('Ctrl Pts',(6.4180837325631,4.55707924506528,114.05027213011));
#245510=CARTESIAN_POINT('Ctrl Pts',(3.44734752807005,7.05759778249045,114.209226495935));
#245511=CARTESIAN_POINT('Ctrl Pts',(-1.63248064607929,8.15496302671398,
114.421165650368));
#245512=CARTESIAN_POINT('Ctrl Pts',(-7.70802135098465,4.4985747233042,114.686089593409));
#245513=CARTESIAN_POINT('Ctrl Pts',(-7.94825322375326,-4.07369333310623,
115.003998325059));
#245514=CARTESIAN_POINT('Ctrl Pts',(-2.06190552756128,-8.05694934939675,
115.2689222681));
#245515=CARTESIAN_POINT('Ctrl Pts',(3.0482109513173,-7.23035130527238,115.480861422533));
#245516=CARTESIAN_POINT('Ctrl Pts',(7.22602204130568,-4.13080231045666,
115.692800576966));
#245517=CARTESIAN_POINT('Ctrl Pts',(8.19581928082761,1.43978996421828,115.904739731399));
#245518=CARTESIAN_POINT('Ctrl Pts',(5.31556056214004,5.78262573228654,116.116678885832));
#245519=CARTESIAN_POINT('Ctrl Pts',(1.91210158620413,7.63561638428962,116.275633251657));
#245520=CARTESIAN_POINT('Ctrl Pts',(-1.9707866449849,7.6032816230003,116.434587617482));
#245521=CARTESIAN_POINT('Ctrl Pts',(-6.54340093733515,5.13345100299747,
116.646526771915));
#245522=CARTESIAN_POINT('Ctrl Pts',(-8.78101191796645,-1.59517942091727,
116.911450714956));
#245523=CARTESIAN_POINT('Ctrl Pts',(-3.38887426470333,-8.26348824039407,
117.229359446606));
#245524=CARTESIAN_POINT('Ctrl Pts',(3.67315216588268,-7.46149049383586,
117.494283389647));
#245525=CARTESIAN_POINT('Ctrl Pts',(7.01760237543226,-3.5103884260452,117.70622254408));
#245526=CARTESIAN_POINT('Ctrl Pts',(8.17568594758414,1.56111548451284,117.918161698513));
#245527=CARTESIAN_POINT('Ctrl Pts',(5.2897969563499,6.4235891046705,118.130100852946));
#245528=CARTESIAN_POINT('Ctrl Pts',(0.277563751038976,7.84964348321566,
118.342040007379));
#245529=CARTESIAN_POINT('Ctrl Pts',(-3.51295635777461,7.04399798923642,
118.500994373204));
#245530=CARTESIAN_POINT('Ctrl Pts',(-6.44163730509991,4.49435204097877,
118.659948739028));
#245531=CARTESIAN_POINT('Ctrl Pts',(-8.30915285520757,-0.355519135476897,
118.871887893461));
#245532=CARTESIAN_POINT('Ctrl Pts',(-5.63329810886282,-6.92219041236727,
119.136811836503));
#245533=CARTESIAN_POINT('Ctrl Pts',(2.7994099472563,-8.48133306905832,119.454720568152));
#245534=CARTESIAN_POINT('Ctrl Pts',(7.64266283975747,-3.27957191430878,
119.719644511194));
#245535=CARTESIAN_POINT('Ctrl Pts',(7.61389451072705,1.89688702375895,119.931583665626));
#245536=CARTESIAN_POINT('Ctrl Pts',(5.19560305715608,6.50266338833404,120.14352282006));
#245537=CARTESIAN_POINT('Ctrl Pts',(-0.158833141679201,8.31980894360886,
120.355461974492));
#245538=CARTESIAN_POINT('Ctrl Pts',(-4.89384758558535,6.14363086932643,
120.567401128926));
#245539=CARTESIAN_POINT('Ctrl Pts',(-7.24946742233022,3.06659291993062,
120.72635549475));
#245540=CARTESIAN_POINT('Ctrl Pts',(-7.8162335680239,-0.77484466107856,
120.885309860575));
#245541=CARTESIAN_POINT('Ctrl Pts',(-6.0810054201158,-5.67360450749057,
121.097249015008));
#245542=CARTESIAN_POINT('Ctrl Pts',(0.222131644826142,-8.92196308111358,
121.362172958049));
#245543=CARTESIAN_POINT('Ctrl Pts',(7.64212238170054,-4.62251794850072,
121.680081689699));
#245544=CARTESIAN_POINT('Ctrl Pts',(7.93863101146212,2.47871436175757,121.94500563274));
#245545=CARTESIAN_POINT('Ctrl Pts',(4.55047200485095,6.39239974770443,122.156944787173));
#245546=CARTESIAN_POINT('Ctrl Pts',(-0.281812118503283,8.31862393664814,
122.368883941606));
#245547=CARTESIAN_POINT('Ctrl Pts',(-5.53111808240576,6.21700744599316,
122.580823096039));
#245548=CARTESIAN_POINT('Ctrl Pts',(-7.71296921877461,1.48460441859632,
122.792762250472));
#245549=CARTESIAN_POINT('Ctrl Pts',(-7.50143033234909,-2.38480880007381,
122.951716616297));
#245550=CARTESIAN_POINT('Ctrl Pts',(-5.43385836418954,-5.67160248224722,
123.110670982122));
#245551=CARTESIAN_POINT('Ctrl Pts',(-0.929945861972466,-8.26460015491946,
123.322610136555));
#245552=CARTESIAN_POINT('Ctrl Pts',(5.97079101554063,-6.63328141549309,
123.587534079596));
#245553=CARTESIAN_POINT('Ctrl Pts',(8.81155209197163,1.458168855644,123.905442811246));
#245554=CARTESIAN_POINT('Ctrl Pts',(4.41879583803649,7.04557524727988,124.170366754287));
#245555=CARTESIAN_POINT('Ctrl Pts',(-0.700192391089372,7.8153247288161,
124.38230590872));
#245556=CARTESIAN_POINT('Ctrl Pts',(-5.62377073711546,6.13613273698301,
124.594245063153));
#245557=CARTESIAN_POINT('Ctrl Pts',(-8.24480119988584,1.12592273243385,
124.806184217586));
#245558=CARTESIAN_POINT('Ctrl Pts',(-6.82475470000086,-3.88801591229979,
125.018123372019));
#245559=CARTESIAN_POINT('Ctrl Pts',(-4.14773593015482,-6.68992202478464,
125.177077737843));
#245560=CARTESIAN_POINT('Ctrl Pts',(-0.439630450095629,-7.84223287757092,
125.336032103669));
#245561=CARTESIAN_POINT('Ctrl Pts',(4.66810392984963,-6.88311126795273,
125.547971258101));
#245562=CARTESIAN_POINT('Ctrl Pts',(8.84951420994463,-1.15622918851469,
125.812895201143));
#245563=CARTESIAN_POINT('Ctrl Pts',(5.74559790547405,6.83796836711839,126.130803932792));
#245564=CARTESIAN_POINT('Ctrl Pts',(-1.22498941140125,8.22589132953309,
126.395727875834));
#245565=CARTESIAN_POINT('Ctrl Pts',(-5.61430046336432,5.48171508822294,
126.607667030266));
#245566=CARTESIAN_POINT('Ctrl Pts',(-8.26259286280484,1.00423177256909,
126.8196061847));
#245567=CARTESIAN_POINT('Ctrl Pts',(-6.99551640097889,-4.50635097486713,
127.031545339132));
#245568=CARTESIAN_POINT('Ctrl Pts',(-2.65613556532327,-7.39181224789329,
127.243484493566));
#245569=CARTESIAN_POINT('Ctrl Pts',(1.19962017695458,-7.77943966330736,
127.40243885939));
#245570=CARTESIAN_POINT('Ctrl Pts',(4.76591139705247,-6.24339490935429,
127.561393225215));
#245571=CARTESIAN_POINT('Ctrl Pts',(8.02237055991287,-2.19316794303078,
127.773332379648));
#245572=CARTESIAN_POINT('Ctrl Pts',(7.47460653571026,4.87657921341394,128.038256322689));
#245573=CARTESIAN_POINT('Ctrl Pts',(-0.0820505423925757,8.93101194655986,
128.356165054339));
#245574=CARTESIAN_POINT('Ctrl Pts',(-6.27996801558465,5.45232876361717,
128.62108899738));
#245575=CARTESIAN_POINT('Ctrl Pts',(-7.82982404950507,0.513249798023501,
128.833028151813));
#245576=CARTESIAN_POINT('Ctrl Pts',(-6.92989528442777,-4.61036588747517,
129.044967306246));
#245577=CARTESIAN_POINT('Ctrl Pts',(-2.38374821605209,-7.9725901228827,
129.256906460679));
#245578=CARTESIAN_POINT('Ctrl Pts',(2.78918870410998,-7.34264058921324,
129.468845615112));
#245579=CARTESIAN_POINT('Ctrl Pts',(5.97036368203372,-5.12967129046876,
129.627799980937));
#245580=CARTESIAN_POINT('Ctrl Pts',(7.68065768697234,-1.64359025738219,
129.786754346762));
#245581=CARTESIAN_POINT('Ctrl Pts',(7.52058337237721,3.55094927679636,129.998693501194));
#245582=CARTESIAN_POINT('Ctrl Pts',(2.50693474615304,8.56539817324321,130.263617444236));
#245583=CARTESIAN_POINT('Ctrl Pts',(-5.87026035982546,6.73125174012964,
130.581526175885));
#245584=CARTESIAN_POINT('Ctrl Pts',(-8.316400610289,0.0580354563857965,
130.846450118927));
#245585=CARTESIAN_POINT('Ctrl Pts',(-6.28184373203611,-4.70191549528422,
131.05838927336));
#245586=CARTESIAN_POINT('Ctrl Pts',(-2.26625593954398,-8.00893290599279,
131.270328427793));
#245587=CARTESIAN_POINT('Ctrl Pts',(3.37379868175747,-7.60670304895033,
131.482267582226));
#245588=CARTESIAN_POINT('Ctrl Pts',(6.89385416487644,-3.76413591636517,
131.694206736659));
#245589=CARTESIAN_POINT('Ctrl Pts',(7.87137641587059,-0.014261567811148,
131.853161102484));
#245590=CARTESIAN_POINT('Ctrl Pts',(6.90359876781664,3.74622682481395,132.012115468308));
#245591=CARTESIAN_POINT('Ctrl Pts',(3.40393272898892,7.58825784698442,132.224054622741));
#245592=CARTESIAN_POINT('Ctrl Pts',(-3.66572693323746,8.13715021530282,
132.488978565783));
#245593=CARTESIAN_POINT('Ctrl Pts',(-8.8368553055286,1.29603032112415,132.806887297432));
#245594=CARTESIAN_POINT('Ctrl Pts',(-6.35545017030808,-5.36415336635995,
133.071811240473));
#245595=CARTESIAN_POINT('Ctrl Pts',(-1.7144157604137,-7.65704561752096,
133.283750394906));
#245596=CARTESIAN_POINT('Ctrl Pts',(3.48668782092298,-7.5579052215536,133.49568954934));
#245597=CARTESIAN_POINT('Ctrl Pts',(7.50968689854422,-3.58455772342483,
133.707628703772));
#245598=CARTESIAN_POINT('Ctrl Pts',(7.68490110483432,1.62364792299449,133.919567858206));
#245599=CARTESIAN_POINT('Ctrl Pts',(5.98891335360918,5.10800387105895,134.07852222403));
#245600=CARTESIAN_POINT('Ctrl Pts',(2.8082364167446,7.3353713277473,134.237476589855));
#245601=CARTESIAN_POINT('Ctrl Pts',(-2.34885814436791,7.97817717382807,
134.449415744288));
#245602=CARTESIAN_POINT('Ctrl Pts',(-8.07641696364469,3.79767233182262,
134.714339687329));
#245603=CARTESIAN_POINT('Ctrl Pts',(-7.55589297261149,-4.76213429554381,
135.032248418979));
#245604=CARTESIAN_POINT('Ctrl Pts',(-1.33969083946443,-8.20801110549739,
135.29717236202));
#245605=CARTESIAN_POINT('Ctrl Pts',(3.67709254282027,-6.93169728860364,
135.509111516453));
#245606=CARTESIAN_POINT('Ctrl Pts',(7.56364733765227,-3.47413327101668,
135.721050670886));
#245607=CARTESIAN_POINT('Ctrl Pts',(8.03607863924848,2.16066936076013,135.932989825319));
#245608=CARTESIAN_POINT('Ctrl Pts',(4.78194321339305,6.23085808992206,136.144928979752));
#245609=CARTESIAN_POINT('Ctrl Pts',(1.22813626868337,7.77534810001959,136.303883345577));
#245610=CARTESIAN_POINT('Ctrl Pts',(-2.63754744258561,7.39811979755767,
136.462837711402));
#245611=CARTESIAN_POINT('Ctrl Pts',(-6.97132874162559,4.53448847191684,
136.674776865835));
#245612=CARTESIAN_POINT('Ctrl Pts',(-8.60778941430539,-2.36969518111316,
136.939700808876));
#245613=CARTESIAN_POINT('Ctrl Pts',(-2.63835148620368,-8.52696629709462,
137.257609540525));
#245614=CARTESIAN_POINT('Ctrl Pts',(4.31203657919717,-7.11389987312211,
137.522533483567));
#245615=CARTESIAN_POINT('Ctrl Pts',(7.31188535419881,-2.86468837331265,
137.734472637999));
#245616=CARTESIAN_POINT('Ctrl Pts',(7.80951289097387,0.972884837682936,
137.893427003825));
#245617=CARTESIAN_POINT('Ctrl Pts',(6.37878947535717,4.60346102348882,138.052446139219));
#245618=CARTESIAN_POINT('Ctrl Pts',(4.39240965737021,6.26214476802734,138.158480486005));
#245619=CARTESIAN_POINT('Ctrl Pts',(3.2582502558657,6.80515705093528,138.211530044183));
#245620=CARTESIAN_POINT('Ctrl Pts',(4.1509387962231,-5.82482577975211,7.77730822088039));
#245621=CARTESIAN_POINT('Ctrl Pts',(5.12112172942826,-5.13345251569094,
7.83032558937012));
#245622=CARTESIAN_POINT('Ctrl Pts',(6.70588704626977,-3.2618553580775,7.93632774646809));
#245623=CARTESIAN_POINT('Ctrl Pts',(7.45184147994325,0.360746109526988,
8.09531469217431));
#245624=CARTESIAN_POINT('Ctrl Pts',(6.36331483166936,3.86396831410664,8.25426905799906));
#245625=CARTESIAN_POINT('Ctrl Pts',(2.87092622161512,7.34492483342846,8.46620821243209));
#245626=CARTESIAN_POINT('Ctrl Pts',(-3.85008224481605,7.53493083349062,
8.73113215547334));
#245627=CARTESIAN_POINT('Ctrl Pts',(-8.42443337233034,0.814053692892807,
9.04904088712287));
#245628=CARTESIAN_POINT('Ctrl Pts',(-5.77383888534872,-5.36812601492259,
9.31396483016413));
#245629=CARTESIAN_POINT('Ctrl Pts',(-1.26083679095937,-7.33819775399668,
9.52590398459714));
#245630=CARTESIAN_POINT('Ctrl Pts',(2.41084003202958,-7.06217496130019,
9.6848583504219));
#245631=CARTESIAN_POINT('Ctrl Pts',(5.47887921888675,-5.04205337644938,
9.84381271624667));
#245632=CARTESIAN_POINT('Ctrl Pts',(7.85650772812585,-0.711760681333348,
10.0557518706797));
#245633=CARTESIAN_POINT('Ctrl Pts',(6.49938797236703,4.47408222088017,10.2676910251127));
#245634=CARTESIAN_POINT('Ctrl Pts',(2.30753480030124,7.07155140166136,10.4796301795457));
#245635=CARTESIAN_POINT('Ctrl Pts',(-2.58535248711871,7.44812896050389,
10.6915693339788));
#245636=CARTESIAN_POINT('Ctrl Pts',(-7.83088474550556,3.21945327438235,
10.95649327702));
#245637=CARTESIAN_POINT('Ctrl Pts',(-6.92570130420384,-4.85959861095894,
11.2744020086696));
#245638=CARTESIAN_POINT('Ctrl Pts',(-0.896931309614421,-7.83301913464394,
11.5393259517108));
#245639=CARTESIAN_POINT('Ctrl Pts',(3.81506237611427,-6.39442540470123,
11.7512651061438));
#245640=CARTESIAN_POINT('Ctrl Pts',(6.42361997314908,-3.79717862977323,
11.9102194719686));
#245641=CARTESIAN_POINT('Ctrl Pts',(7.44123640529532,-0.267289742976332,
12.0691738377934));
#245642=CARTESIAN_POINT('Ctrl Pts',(6.4310429295426,4.56844247750195,12.2811129922264));
#245643=CARTESIAN_POINT('Ctrl Pts',(2.02792095266024,7.62545053401183,12.4930521466594));
#245644=CARTESIAN_POINT('Ctrl Pts',(-2.8457724144279,6.87264535529731,12.7049913010924));
#245645=CARTESIAN_POINT('Ctrl Pts',(-6.8075826492275,3.97683224675571,12.9169304555254));
#245646=CARTESIAN_POINT('Ctrl Pts',(-8.0425356587629,-2.64678923841271,
13.1818543985667));
#245647=CARTESIAN_POINT('Ctrl Pts',(-2.1009832043633,-8.1955386757095,13.4997631302162));
#245648=CARTESIAN_POINT('Ctrl Pts',(4.4125185540474,-6.53378352923089,13.7646870732574));
#245649=CARTESIAN_POINT('Ctrl Pts',(7.05654596471932,-2.37667006032655,
13.9766262276905));
#245650=CARTESIAN_POINT('Ctrl Pts',(7.34916631688393,1.29274846990858,14.1355805935152));
#245651=CARTESIAN_POINT('Ctrl Pts',(5.82669598721959,4.6360611618861,14.29453495934));
#245652=CARTESIAN_POINT('Ctrl Pts',(1.91455626914196,7.65267612129344,14.506474113773));
#245653=CARTESIAN_POINT('Ctrl Pts',(-3.41836086554637,7.11159386572605,
14.718413268206));
#245654=CARTESIAN_POINT('Ctrl Pts',(-6.63119636648613,3.37029827631453,
14.930352422639));
#245655=CARTESIAN_POINT('Ctrl Pts',(-7.75768227212046,-1.40596626166421,
15.1422915770721));
#245656=CARTESIAN_POINT('Ctrl Pts',(-4.38842815241116,-7.24082673477043,
15.4072155201133));
#245657=CARTESIAN_POINT('Ctrl Pts',(3.73359216516395,-7.5921850777709,15.7251242517628));
#245658=CARTESIAN_POINT('Ctrl Pts',(7.60103891632166,-2.09400440680762,
15.9900481948041));
#245659=CARTESIAN_POINT('Ctrl Pts',(6.90621000003866,2.78346277591659,16.2019873492371));
#245660=CARTESIAN_POINT('Ctrl Pts',(4.74224381427298,5.76129913647346,16.3609417150619));
#245661=CARTESIAN_POINT('Ctrl Pts',(1.41148008495701,7.31103092589749,16.5198960808866));
#245662=CARTESIAN_POINT('Ctrl Pts',(-3.52218573576049,7.05855404261346,
16.7318352353197));
#245663=CARTESIAN_POINT('Ctrl Pts',(-7.22156448448482,3.17945981395448,
16.9437743897527));
#245664=CARTESIAN_POINT('Ctrl Pts',(-7.22925189979947,-1.75202531204523,
17.1557135441857));
#245665=CARTESIAN_POINT('Ctrl Pts',(-4.97895389573663,-6.11296928396743,
17.3676526986187));
#245666=CARTESIAN_POINT('Ctrl Pts',(1.37503284600016,-8.35446935024785,
17.6325766416599));
#245667=CARTESIAN_POINT('Ctrl Pts',(7.77356924943103,-3.33955174175305,
17.9504853733095));
#245668=CARTESIAN_POINT('Ctrl Pts',(7.13602384913055,3.35228439835905,18.2154093163507));
#245669=CARTESIAN_POINT('Ctrl Pts',(3.4363168962553,6.60568904643142,18.4273484707838));
#245670=CARTESIAN_POINT('Ctrl Pts',(-0.144098120754572,7.46060854525456,
18.5863028366085));
#245671=CARTESIAN_POINT('Ctrl Pts',(-3.68218156311378,6.47186125978534,
18.7452572024333));
#245672=CARTESIAN_POINT('Ctrl Pts',(-7.26594464328095,3.07164873813643,
18.9571963568663));
#245673=CARTESIAN_POINT('Ctrl Pts',(-7.5536318490491,-2.28092178759782,
19.1691355112993));
#245674=CARTESIAN_POINT('Ctrl Pts',(-4.35247612487143,-6.03221578752203,
19.3810746657323));
#245675=CARTESIAN_POINT('Ctrl Pts',(0.192971607746215,-7.88169634794461,
19.5930138201653));
#245676=CARTESIAN_POINT('Ctrl Pts',(6.47756692573537,-5.4524306666318,19.8579377632066));
#245677=CARTESIAN_POINT('Ctrl Pts',(8.07708201093883,2.51827935307344,20.1758464948561));
#245678=CARTESIAN_POINT('Ctrl Pts',(3.24098871487961,7.18725533238272,20.4407704378974));
#245679=CARTESIAN_POINT('Ctrl Pts',(-1.68528536100722,7.25280737656864,
20.6527095923304));
#245680=CARTESIAN_POINT('Ctrl Pts',(-4.96117747254263,5.57388214980061,
20.8116639581552));
#245681=CARTESIAN_POINT('Ctrl Pts',(-7.00595609770081,2.52190967061355,
20.9706183239799));
#245682=CARTESIAN_POINT('Ctrl Pts',(-7.51723541172976,-2.39168335996942,
21.182557478413));
#245683=CARTESIAN_POINT('Ctrl Pts',(-4.25495058253814,-6.64494949960238,
21.3944966328459));
#245684=CARTESIAN_POINT('Ctrl Pts',(0.616372317611963,-7.4129454935867,
21.606435787279));
#245685=CARTESIAN_POINT('Ctrl Pts',(5.27214286867867,-5.86198643250225,
21.818374941712));
#245686=CARTESIAN_POINT('Ctrl Pts',(8.46657658194745,0.0703877391787107,
22.0832988847532));
#245687=CARTESIAN_POINT('Ctrl Pts',(4.4982432043068,7.16566764415259,22.4012076164028));
#245688=CARTESIAN_POINT('Ctrl Pts',(-2.21186861338831,7.56758113930394,
22.666131559444));
#245689=CARTESIAN_POINT('Ctrl Pts',(-5.99683390639607,4.41377216094488,
22.8780707138771));
#245690=CARTESIAN_POINT('Ctrl Pts',(-7.3936041596357,1.00799884154107,23.0370250797018));
#245691=CARTESIAN_POINT('Ctrl Pts',(-6.96222927407579,-2.6402296803209,
23.1959794455266));
#245692=CARTESIAN_POINT('Ctrl Pts',(-4.15527195677464,-6.70542261866923,
23.4079185999596));
#245693=CARTESIAN_POINT('Ctrl Pts',(1.08892646681892,-7.8149982381296,23.6198577543926));
#245694=CARTESIAN_POINT('Ctrl Pts',(5.28895361428727,-5.23054924369547,
23.8317969088256));
#245695=CARTESIAN_POINT('Ctrl Pts',(7.81719201645802,-1.02463863894781,
24.0437360632586));
#245696=CARTESIAN_POINT('Ctrl Pts',(6.38601918099923,5.55937338840611,24.3086600063));
#245697=CARTESIAN_POINT('Ctrl Pts',(-1.24273305920179,8.36878720335955,
24.6265687379494));
#245698=CARTESIAN_POINT('Ctrl Pts',(-6.60156333316999,4.31045341245984,
24.8914926809907));
#245699=CARTESIAN_POINT('Ctrl Pts',(-7.42592843078579,-0.546798436794452,
25.1034318354237));
#245700=CARTESIAN_POINT('Ctrl Pts',(-6.27220154742346,-4.04239185166769,
25.2623862012485));
#245701=CARTESIAN_POINT('Ctrl Pts',(-3.57201894274956,-6.53330926118485,
25.4213405670732));
#245702=CARTESIAN_POINT('Ctrl Pts',(1.20397548955058,-7.79611573479253,
25.6332797215063));
#245703=CARTESIAN_POINT('Ctrl Pts',(5.90939724515907,-5.22866928682757,
25.8452188759392));
#245704=CARTESIAN_POINT('Ctrl Pts',(7.41933250043391,-0.534023382269806,
26.0571580303723));
#245705=CARTESIAN_POINT('Ctrl Pts',(6.60480900712377,4.30521466851727,26.2690971848052));
#245706=CARTESIAN_POINT('Ctrl Pts',(1.2359409372583,8.37617594439235,26.5340211278465));
#245707=CARTESIAN_POINT('Ctrl Pts',(-6.38637396884901,5.54934340634596,
26.8519298594961));
#245708=CARTESIAN_POINT('Ctrl Pts',(-7.81813318879946,-1.01854823402413,
27.1168538025373));
#245709=CARTESIAN_POINT('Ctrl Pts',(-5.28565658634204,-5.24454345399983,
27.3287929569704));
#245710=CARTESIAN_POINT('Ctrl Pts',(-2.13598597672581,-7.14975580290411,
27.4877473227951));
#245711=CARTESIAN_POINT('Ctrl Pts',(1.53512744605716,-7.28607116037218,
27.6467016886199));
#245712=CARTESIAN_POINT('Ctrl Pts',(5.98451689778819,-5.13950727500275,
27.8586408430529));
#245713=CARTESIAN_POINT('Ctrl Pts',(7.88944153898006,-0.129114349023541,
28.0705799974859));
#245714=CARTESIAN_POINT('Ctrl Pts',(5.98351543504755,4.41918756824753,28.2825191519189));
#245715=CARTESIAN_POINT('Ctrl Pts',(2.21774105942401,7.56571212483959,28.4944583063519));
#245716=CARTESIAN_POINT('Ctrl Pts',(-4.50820794107503,7.1668636523821,28.7593822493932));
#245717=CARTESIAN_POINT('Ctrl Pts',(-8.46032350243878,0.0625375537539325,
29.0772909810427));
#245718=CARTESIAN_POINT('Ctrl Pts',(-5.27681850093237,-5.8579717967108,
29.342214924084));
#245719=CARTESIAN_POINT('Ctrl Pts',(-0.60476708952805,-7.42143236559205,
29.554154078517));
#245720=CARTESIAN_POINT('Ctrl Pts',(3.02691825394032,-6.8204992499005,29.7131084443417));
#245721=CARTESIAN_POINT('Ctrl Pts',(5.90439542290494,-4.53669085563746,
29.8720628101665));
#245722=CARTESIAN_POINT('Ctrl Pts',(7.88852461090912,-0.0125296767604765,
30.0840019645995));
#245723=CARTESIAN_POINT('Ctrl Pts',(6.07732602940615,5.03250103272817,30.2959411190325));
#245724=CARTESIAN_POINT('Ctrl Pts',(1.67164604026992,7.24826015267495,30.5078802734656));
#245725=CARTESIAN_POINT('Ctrl Pts',(-3.23531216218057,7.18965441282447,
30.7198194278986));
#245726=CARTESIAN_POINT('Ctrl Pts',(-8.08542968584339,2.51270775202584,
30.9847433709398));
#245727=CARTESIAN_POINT('Ctrl Pts',(-6.46771160057704,-5.45432776456534,
31.3026521025894));
#245728=CARTESIAN_POINT('Ctrl Pts',(-0.199134298166419,-7.8816871667261,
31.5675760456306));
#245729=CARTESIAN_POINT('Ctrl Pts',(4.3668113535178,-6.0311159989194,31.7795152000637));
#245730=CARTESIAN_POINT('Ctrl Pts',(6.73489596363007,-3.21288351687546,
31.9384695658883));
#245731=CARTESIAN_POINT('Ctrl Pts',(7.43564110432626,0.393307255589283,
32.0974239317132));
#245732=CARTESIAN_POINT('Ctrl Pts',(6.000813253703,5.12047046899997,32.3093630861461));
#245733=CARTESIAN_POINT('Ctrl Pts',(1.34406694243543,7.77518117900539,32.5213022405792));
#245734=CARTESIAN_POINT('Ctrl Pts',(-3.44372115445915,6.5933648719858,32.7332413950122));
#245735=CARTESIAN_POINT('Ctrl Pts',(-7.13327169657829,3.35779842536662,
32.9451805494452));
#245736=CARTESIAN_POINT('Ctrl Pts',(-7.77628744700907,-3.34921289160561,
33.2101044924865));
#245737=CARTESIAN_POINT('Ctrl Pts',(-1.36631236180715,-8.34950149658773,
33.528013224136));
#245738=CARTESIAN_POINT('Ctrl Pts',(4.97426632220056,-6.11696997039077,
33.7929371671773));
#245739=CARTESIAN_POINT('Ctrl Pts',(7.23942672015315,-1.74186749012833,
34.0048763216103));
#245740=CARTESIAN_POINT('Ctrl Pts',(7.20566079492565,1.93904529147781,34.163830687435));
#245741=CARTESIAN_POINT('Ctrl Pts',(5.39285189760239,5.13425726275685,34.3227850532598));
#245742=CARTESIAN_POINT('Ctrl Pts',(1.22873515191321,7.79225175775088,34.5347242076927));
#245743=CARTESIAN_POINT('Ctrl Pts',(-4.03523491029923,6.78062220823502,
34.7466633621258));
#245744=CARTESIAN_POINT('Ctrl Pts',(-6.90382024541709,2.76928542114653,
34.9586025165588));
#245745=CARTESIAN_POINT('Ctrl Pts',(-7.60253402081132,-2.08802582000469,
35.1705416709919));
#245746=CARTESIAN_POINT('Ctrl Pts',(-3.72937434942724,-7.60129202265261,
35.4354656140331));
#245747=CARTESIAN_POINT('Ctrl Pts',(4.39182218474434,-7.23138179113334,
35.7533743456827));
#245748=CARTESIAN_POINT('Ctrl Pts',(7.75672295683287,-1.4120538352991,36.0182982887239));
#245749=CARTESIAN_POINT('Ctrl Pts',(6.63232012267388,3.38463164613355,36.2302374431569));
#245750=CARTESIAN_POINT('Ctrl Pts',(4.21293368089045,6.15894746968582,36.3891918089817));
#245751=CARTESIAN_POINT('Ctrl Pts',(0.75792025713238,7.40736161622165,36.5481461748064));
#245752=CARTESIAN_POINT('Ctrl Pts',(-4.13395003265704,6.71858873999691,
36.7600853292395));
#245753=CARTESIAN_POINT('Ctrl Pts',(-7.47495009539872,2.52687146159157,
36.9720244836724));
#245754=CARTESIAN_POINT('Ctrl Pts',(-7.0455108666269,-2.38588607293978,
37.1839636381055));
#245755=CARTESIAN_POINT('Ctrl Pts',(-4.41754226695533,-6.53021406098323,
37.3959027925385));
#245756=CARTESIAN_POINT('Ctrl Pts',(2.1101096709297,-8.19971405772523,37.6608267355797));
#245757=CARTESIAN_POINT('Ctrl Pts',(8.03897188270305,-2.63740701839083,
37.9787354672293));
#245758=CARTESIAN_POINT('Ctrl Pts',(6.81081265222878,3.97158382501008,38.2436594102705));
#245759=CARTESIAN_POINT('Ctrl Pts',(2.83730502138147,6.88426479773092,38.4555985647036));
#245760=CARTESIAN_POINT('Ctrl Pts',(-0.804793261092854,7.41847369347833,
38.6145529305283));
#245761=CARTESIAN_POINT('Ctrl Pts',(-4.24131533553443,6.12002397496985,
38.7735072963531));
#245762=CARTESIAN_POINT('Ctrl Pts',(-7.50959987820737,2.415551117022,38.9854464507861));
#245763=CARTESIAN_POINT('Ctrl Pts',(-7.32173602890284,-2.94145199436841,
39.1973856052191));
#245764=CARTESIAN_POINT('Ctrl Pts',(-3.80068762994222,-6.39425126691233,
39.4093247596522));
#245765=CARTESIAN_POINT('Ctrl Pts',(0.890797018126755,-7.83357236738745,
39.6212639140849));
#245766=CARTESIAN_POINT('Ctrl Pts',(6.93534280479247,-4.85683988122124,
39.8861878571265));
#245767=CARTESIAN_POINT('Ctrl Pts',(7.82208812739543,3.22427077628526,40.2040965887758));
#245768=CARTESIAN_POINT('Ctrl Pts',(2.59119915321904,7.44622951641959,40.4690205318172));
#245769=CARTESIAN_POINT('Ctrl Pts',(-2.32149660382302,7.07488905270405,
40.6809596862502));
#245770=CARTESIAN_POINT('Ctrl Pts',(-5.43568614902035,5.11221676215697,
40.839914052075));
#245771=CARTESIAN_POINT('Ctrl Pts',(-7.20190909918588,1.89101944905621,
40.9988684178997));
#245772=CARTESIAN_POINT('Ctrl Pts',(-7.27566561605945,-3.04855168449034,
41.2108075723328));
#245773=CARTESIAN_POINT('Ctrl Pts',(-3.64923698859839,-6.99592936736449,
41.4227467267657));
#245774=CARTESIAN_POINT('Ctrl Pts',(1.27098415924342,-7.32913876193906,
41.6346858811988));
#245775=CARTESIAN_POINT('Ctrl Pts',(5.77096345619118,-5.3716250939456,41.8466250356318));
#245776=CARTESIAN_POINT('Ctrl Pts',(8.42701575227761,0.820535777813988,
42.111548978673));
#245777=CARTESIAN_POINT('Ctrl Pts',(3.84541883736212,7.53616206545534,42.4294577103226));
#245778=CARTESIAN_POINT('Ctrl Pts',(-2.87390697323184,7.34175086556677,
42.6943816533638));
#245779=CARTESIAN_POINT('Ctrl Pts',(-6.36444154116952,3.86487845328535,
42.9063208077969));
#245780=CARTESIAN_POINT('Ctrl Pts',(-7.45384777880487,0.348708222352379,
43.0652751736216));
#245781=CARTESIAN_POINT('Ctrl Pts',(-6.70081421748781,-3.24692747876492,
43.2242295394464));
#245782=CARTESIAN_POINT('Ctrl Pts',(-3.54459070639618,-7.04732958317178,
43.4361686938793));
#245783=CARTESIAN_POINT('Ctrl Pts',(1.77731393901028,-7.68772485682904,
43.6481078483124));
#245784=CARTESIAN_POINT('Ctrl Pts',(5.73174134622043,-4.74118306594809,
43.8600470027454));
#245785=CARTESIAN_POINT('Ctrl Pts',(7.8772433602972,-0.327738318255859,
44.0719861571785));
#245786=CARTESIAN_POINT('Ctrl Pts',(5.86813705545796,6.10351054313575,44.3369101002196));
#245787=CARTESIAN_POINT('Ctrl Pts',(-1.97959962545018,8.22570179586308,
44.6548188318693));
#245788=CARTESIAN_POINT('Ctrl Pts',(-6.95763338494124,3.7083668566624,44.9197427749104));
#245789=CARTESIAN_POINT('Ctrl Pts',(-7.34823720106293,-1.20283482928803,
45.1316819293436));
#245790=CARTESIAN_POINT('Ctrl Pts',(-5.8892232522119,-4.58241133242498,
45.2906362951682));
#245791=CARTESIAN_POINT('Ctrl Pts',(-2.97888827949449,-6.8241976706376,
45.4495906609931));
#245792=CARTESIAN_POINT('Ctrl Pts',(1.89023653223341,-7.65871943486173,
45.661529815426));
#245793=CARTESIAN_POINT('Ctrl Pts',(6.34957645542678,-4.68431821600511,
45.8734689698591));
#245794=CARTESIAN_POINT('Ctrl Pts',(7.43746460218952,0.125682202335439,
46.085408124292));
#245795=CARTESIAN_POINT('Ctrl Pts',(6.19722666978529,4.87368002292947,46.2973472787251));
#245796=CARTESIAN_POINT('Ctrl Pts',(0.488664105854659,8.4527558135473,46.5622712217663));
#245797=CARTESIAN_POINT('Ctrl Pts',(-6.85309850486006,4.96145397985629,
46.8801799534159));
#245798=CARTESIAN_POINT('Ctrl Pts',(-7.69708536115706,-1.70749055807123,
47.1451038964571));
#245799=CARTESIAN_POINT('Ctrl Pts',(-4.80000976375706,-5.69239034654781,
47.3570430508902));
#245800=CARTESIAN_POINT('Ctrl Pts',(-1.49386912582224,-7.31093695560598,
47.5159974167149));
#245801=CARTESIAN_POINT('Ctrl Pts',(2.17487796512775,-7.12133098981132,
47.6749517825397));
#245802=CARTESIAN_POINT('Ctrl Pts',(6.41649768782323,-4.58884897897914,
47.8868909369727));
#245803=CARTESIAN_POINT('Ctrl Pts',(7.86983478575692,0.570665188177667,
48.0988300914057));
#245804=CARTESIAN_POINT('Ctrl Pts',(5.56827648271525,4.93213673136158,48.3107692458386));
#245805=CARTESIAN_POINT('Ctrl Pts',(1.538434643456,7.73250245460126,48.5227084002718));
#245806=CARTESIAN_POINT('Ctrl Pts',(-5.12569142326057,6.73907715383353,
48.7876323433129));
#245807=CARTESIAN_POINT('Ctrl Pts',(-8.43256896027644,-0.687579407581075,
49.1055410749626));
#245808=CARTESIAN_POINT('Ctrl Pts',(-4.73683596235613,-6.30262105227425,
49.3704650180036));
#245809=CARTESIAN_POINT('Ctrl Pts',(0.0554030417511936,-7.44582648821461,
49.5824041724369));
#245810=CARTESIAN_POINT('Ctrl Pts',(3.6195320793735,-6.52536831606588,49.7413585382614));
#245811=CARTESIAN_POINT('Ctrl Pts',(6.28326162393605,-3.99550655046614,
49.9003129040864));
#245812=CARTESIAN_POINT('Ctrl Pts',(7.85858812104716,0.686709744692324,
50.1122520585192));
#245813=CARTESIAN_POINT('Ctrl Pts',(5.60735754647097,5.55135115608286,50.3241912129523));
#245814=CARTESIAN_POINT('Ctrl Pts',(1.02262588517924,7.36789739503524,50.5361303673853));
#245815=CARTESIAN_POINT('Ctrl Pts',(-3.85982544106722,6.87459983759712,
50.7480695218184));
#245816=CARTESIAN_POINT('Ctrl Pts',(-8.27631857770454,1.78617587380135,
51.0129934648596));
#245817=CARTESIAN_POINT('Ctrl Pts',(-5.95881855176718,-6.00611906131259,
51.3309021965091));
#245818=CARTESIAN_POINT('Ctrl Pts',(0.500233518445705,-7.86831706846291,
51.5958261395504));
#245819=CARTESIAN_POINT('Ctrl Pts',(4.88418567491117,-5.62033200822035,
51.8077652939834));
#245820=CARTESIAN_POINT('Ctrl Pts',(6.9931594373733,-2.60329891049933,51.9667196598082));
#245821=CARTESIAN_POINT('Ctrl Pts',(7.37151615867653,1.05080861816805,52.1256740256329));
#245822=CARTESIAN_POINT('Ctrl Pts',(5.52334883621293,5.63219274911859,52.337613180066));
#245823=CARTESIAN_POINT('Ctrl Pts',(0.649633021818951,7.8637100181193,52.549552334499));
#245824=CARTESIAN_POINT('Ctrl Pts',(-4.01456277072602,6.26218504075905,
52.761491488932));
#245825=CARTESIAN_POINT('Ctrl Pts',(-7.40281163663164,2.7123339092285,52.973430643365));
#245826=CARTESIAN_POINT('Ctrl Pts',(-7.44882858971283,-4.02527341840082,
53.2383545864063));
#245827=CARTESIAN_POINT('Ctrl Pts',(-0.620886683000079,-8.43774166696402,
53.5562633180558));
#245828=CARTESIAN_POINT('Ctrl Pts',(5.49685943532892,-5.65200702503782,
53.8211872610971));
#245829=CARTESIAN_POINT('Ctrl Pts',(7.36532272413416,-1.09335390381452,
54.03312641553));
#245830=CARTESIAN_POINT('Ctrl Pts',(7.00543631370554,2.57007902379404,54.1920807813549));
#245831=CARTESIAN_POINT('Ctrl Pts',(4.91655827097942,5.59203934157381,54.3510351471795));
#245832=CARTESIAN_POINT('Ctrl Pts',(0.533242114523018,7.87049111409306,
54.5629743016127));
#245833=CARTESIAN_POINT('Ctrl Pts',(-4.62034582655523,6.39627725752574,
54.7749134560455));
#245834=CARTESIAN_POINT('Ctrl Pts',(-7.12210108419128,2.14647428854086,
54.9868526104786));
#245835=CARTESIAN_POINT('Ctrl Pts',(-7.38754284268422,-2.7536495982795,
55.1987917649117));
#245836=CARTESIAN_POINT('Ctrl Pts',(-3.0409649820265,-7.90192415996867,
55.4637157079528));
#245837=CARTESIAN_POINT('Ctrl Pts',(5.01548221836353,-6.81365708183404,
55.7816244396025));
#245838=CARTESIAN_POINT('Ctrl Pts',(7.85135038073463,-0.718988359974968,
56.0465483826436));
#245839=CARTESIAN_POINT('Ctrl Pts',(6.30622430352142,3.95915857516586,56.2584875370768));
#245840=CARTESIAN_POINT('Ctrl Pts',(3.65046167257338,6.50811598782652,56.4174419029014));
#245841=CARTESIAN_POINT('Ctrl Pts',(0.0983945018344138,7.44538566842941,
56.5763962687262));
#245842=CARTESIAN_POINT('Ctrl Pts',(-4.71317417004024,6.32573843694028,
56.7883354231592));
#245843=CARTESIAN_POINT('Ctrl Pts',(-7.66949704921241,1.85439297998827,
57.0002745775923));
#245844=CARTESIAN_POINT('Ctrl Pts',(-6.80631148353952,-3.00096646329874,
57.2122137320253));
#245845=CARTESIAN_POINT('Ctrl Pts',(-3.82135819804321,-6.89605661844852,
57.4241528864583));
#245846=CARTESIAN_POINT('Ctrl Pts',(2.8285768840507,-7.98041516857501,57.6890768294995));
#245847=CARTESIAN_POINT('Ctrl Pts',(8.24109619250587,-1.9145020912532,58.0069855611492));
#245848=CARTESIAN_POINT('Ctrl Pts',(6.43199051945318,4.55962114879134,58.2719095041902));
#245849=CARTESIAN_POINT('Ctrl Pts',(2.21595945663504,7.10865143864736,58.4838486586235));
#245850=CARTESIAN_POINT('Ctrl Pts',(-1.45915351569631,7.31794473548151,
58.6428030244481));
#245851=CARTESIAN_POINT('Ctrl Pts',(-4.76706382838783,5.72001325922605,
58.8017573902729));
#245852=CARTESIAN_POINT('Ctrl Pts',(-7.69414371217973,1.7404396186147,59.0136965447059));
#245853=CARTESIAN_POINT('Ctrl Pts',(-7.03220756772331,-3.5788287241167,
59.2256356991389));
#245854=CARTESIAN_POINT('Ctrl Pts',(-3.21898223211034,-6.70595475038146,
59.4375748535719));
#245855=CARTESIAN_POINT('Ctrl Pts',(1.58161056894603,-7.7237868543091,59.6495140080049));
#245856=CARTESIAN_POINT('Ctrl Pts',(7.33852751575318,-4.22301874875562,
59.9144379510463));
#245857=CARTESIAN_POINT('Ctrl Pts',(7.50552310889206,3.90488253004291,60.2323466826956));
#245858=CARTESIAN_POINT('Ctrl Pts',(1.92101311044358,7.64659111580737,60.497270625737));
#245859=CARTESIAN_POINT('Ctrl Pts',(-2.93943431425503,6.84128113015493,
60.70920978017));
#245860=CARTESIAN_POINT('Ctrl Pts',(-5.867408121995,4.61031084243544,60.8681641459948));
#245861=CARTESIAN_POINT('Ctrl Pts',(-7.34117267070119,1.24524417227922,
61.0271185118195));
#245862=CARTESIAN_POINT('Ctrl Pts',(-6.97682582006776,-3.68142350268944,
61.2390576662526));
#245863=CARTESIAN_POINT('Ctrl Pts',(-3.01479862712008,-7.29184116324697,
61.4509968206856));
#245864=CARTESIAN_POINT('Ctrl Pts',(1.91559151921653,-7.18764111905368,
61.6629359751185));
#245865=CARTESIAN_POINT('Ctrl Pts',(6.22435822338273,-4.83898130494505,
61.8748751295516));
#245866=CARTESIAN_POINT('Ctrl Pts',(8.3211221332371,1.56422501436302,62.1397990725929));
#245867=CARTESIAN_POINT('Ctrl Pts',(3.16232546828451,7.84733600301313,62.4577078042424));
#245868=CARTESIAN_POINT('Ctrl Pts',(-3.51332353295876,7.05813040511431,
62.7226317472836));
#245869=CARTESIAN_POINT('Ctrl Pts',(-6.68195182563262,3.28556256820024,
62.9345709017167));
#245870=CARTESIAN_POINT('Ctrl Pts',(-7.45541884659326,-0.313327234361745,
63.0935252675414));
#245871=CARTESIAN_POINT('Ctrl Pts',(-6.38665407163377,-3.82806726677171,
63.2524796333662));
#245872=CARTESIAN_POINT('Ctrl Pts',(-2.90600840591369,-7.33376388183294,
63.4644187877991));
#245873=CARTESIAN_POINT('Ctrl Pts',(2.45171138262837,-7.49993797363672,
63.6763579422323));
#245874=CARTESIAN_POINT('Ctrl Pts',(6.12941199250644,-4.21449692738344,
63.8882970966652));
#245875=CARTESIAN_POINT('Ctrl Pts',(7.87528941780481,0.371741776518995,
64.1002362510983));
#245876=CARTESIAN_POINT('Ctrl Pts',(5.30406421297267,6.59960425150415,64.3651601941394));
#245877=CARTESIAN_POINT('Ctrl Pts',(-2.70088388250976,8.01786823069259,
64.6830689257891));
#245878=CARTESIAN_POINT('Ctrl Pts',(-7.25893680954418,3.07709009583346,
64.9479928688302));
#245879=CARTESIAN_POINT('Ctrl Pts',(-7.21270472779369,-1.84940317381245,
65.1599320232634));
#245880=CARTESIAN_POINT('Ctrl Pts',(-5.45988826122027,-5.08636061530274,
65.318886389088));
#245881=CARTESIAN_POINT('Ctrl Pts',(-2.36230946156806,-7.06136978478256,
65.4778407549128));
#245882=CARTESIAN_POINT('Ctrl Pts',(2.56161868239115,-7.46103794761829,
65.6897799093458));
#245883=CARTESIAN_POINT('Ctrl Pts',(6.73977532507158,-4.10309479289059,
65.9017190637788));
#245884=CARTESIAN_POINT('Ctrl Pts',(7.39705311185201,0.784398486419424,
66.1136582182119));
#245885=CARTESIAN_POINT('Ctrl Pts',(5.74086320472686,5.403782474047,66.3255973726448));
#245886=CARTESIAN_POINT('Ctrl Pts',(-0.262459218000729,8.46280028184657,
66.5905213156862));
#245887=CARTESIAN_POINT('Ctrl Pts',(-7.2658792543938,4.33451074223193,66.9084300473356));
#245888=CARTESIAN_POINT('Ctrl Pts',(-7.51545035067317,-2.38299246447439,
67.1733539903769));
#245889=CARTESIAN_POINT('Ctrl Pts',(-4.27657992960506,-6.09542990261524,
67.3852931448099));
#245890=CARTESIAN_POINT('Ctrl Pts',(-0.839993365772602,-7.41457047170496,
67.5442475106347));
#245891=CARTESIAN_POINT('Ctrl Pts',(2.79750905089242,-6.90053565519577,
67.7032018764595));
#245892=CARTESIAN_POINT('Ctrl Pts',(6.79797137375908,-4.00206981200973,
67.9151410308924));
#245893=CARTESIAN_POINT('Ctrl Pts',(7.78828105606738,1.26595276683344,68.1270801853255));
#245894=CARTESIAN_POINT('Ctrl Pts',(5.10920715677595,5.40626285126827,68.3390193397585));
#245895=CARTESIAN_POINT('Ctrl Pts',(0.847018506823715,7.83842682077682,
68.5509584941915));
#245896=CARTESIAN_POINT('Ctrl Pts',(-5.70282827152682,6.25824437568983,
68.8158824372328));
#245897=CARTESIAN_POINT('Ctrl Pts',(-8.3384379818395,-1.43228411544367,
69.1337911688823));
#245898=CARTESIAN_POINT('Ctrl Pts',(-4.15956757109609,-6.69765959122558,
69.3987151119235));
#245899=CARTESIAN_POINT('Ctrl Pts',(0.715136918934491,-7.41161117488028,
69.6106542663566));
#245900=CARTESIAN_POINT('Ctrl Pts',(4.18365528963165,-6.1788733574416,69.7696086321812));
#245901=CARTESIAN_POINT('Ctrl Pts',(6.61266885939531,-3.42287173955488,
69.9285629980062));
#245902=CARTESIAN_POINT('Ctrl Pts',(7.76679459976119,1.38054354820726,70.140502152439));
#245903=CARTESIAN_POINT('Ctrl Pts',(5.09324835207816,6.02650454722979,70.3524413068722));
#245904=CARTESIAN_POINT('Ctrl Pts',(0.36555935057273,7.42953814632684,70.5643804613051));
#245905=CARTESIAN_POINT('Ctrl Pts',(-4.45396371572346,6.50543338303905,
70.7763196157382));
#245906=CARTESIAN_POINT('Ctrl Pts',(-8.40204513351695,1.04558175432152,
71.0412435587793));
#245907=CARTESIAN_POINT('Ctrl Pts',(-5.40304876320707,-6.5106291922939,
71.3591522904291));
#245908=CARTESIAN_POINT('Ctrl Pts',(1.19571080635691,-7.79301928146387,
71.62407623347));
#245909=CARTESIAN_POINT('Ctrl Pts',(5.36304927419964,-5.16529772798693,
71.8360153879034));
#245910=CARTESIAN_POINT('Ctrl Pts',(7.19651870242583,-1.97324473515594,
71.9949697537278));
#245911=CARTESIAN_POINT('Ctrl Pts',(7.24910192905725,1.70007989524192,72.1539241195528));
#245912=CARTESIAN_POINT('Ctrl Pts',(5.00301187184924,6.0994873116443,72.3658632739857));
#245913=CARTESIAN_POINT('Ctrl Pts',(-0.0510729370531945,7.89052074771417,
72.5778024284188));
#245914=CARTESIAN_POINT('Ctrl Pts',(-4.55244977206186,5.88150167157887,
72.7897415828518));
#245915=CARTESIAN_POINT('Ctrl Pts',(-7.61724391812272,2.04601116422751,
73.0016807372848));
#245916=CARTESIAN_POINT('Ctrl Pts',(-7.05604730840642,-4.67067368392185,
73.266604680326));
#245917=CARTESIAN_POINT('Ctrl Pts',(0.117871558726145,-8.45787944261411,
73.5845134119757));
#245918=CARTESIAN_POINT('Ctrl Pts',(7.16958247662802,-4.48195502366287,
73.902422143625));
#245919=CARTESIAN_POINT('Ctrl Pts',(7.65256736296178,3.60409978063233,74.2203308752747));
#245920=CARTESIAN_POINT('Ctrl Pts',(1.11114445795367,8.38189666584284,74.5382396069241));
#245921=CARTESIAN_POINT('Ctrl Pts',(-6.4453788949029,5.47783801068378,74.8561483385738));
#245922=CARTESIAN_POINT('Ctrl Pts',(-8.0948899913508,-2.46490411742087,
75.174057070223));
#245923=CARTESIAN_POINT('Ctrl Pts',(-3.27421567416541,-7.1755193757226,
75.4389810132645));
#245924=CARTESIAN_POINT('Ctrl Pts',(1.6347076480826,-7.25565929087297,75.6509201676975));
#245925=CARTESIAN_POINT('Ctrl Pts',(6.05052887116323,-5.06498040413063,
75.8628593221304));
#245926=CARTESIAN_POINT('Ctrl Pts',(7.88879558544593,-0.0278830741340137,
76.0747984765636));
#245927=CARTESIAN_POINT('Ctrl Pts',(5.92772275986439,4.50575779533842,76.2867376309964));
#245928=CARTESIAN_POINT('Ctrl Pts',(3.06234663935547,6.80482250169787,76.4456919968214));
#245929=CARTESIAN_POINT('Ctrl Pts',(-0.566278238928978,7.42441425920965,
76.604646362646));
#245930=CARTESIAN_POINT('Ctrl Pts',(-5.24632254028144,5.88531848390908,
76.8165855170791));
#245931=CARTESIAN_POINT('Ctrl Pts',(-8.46054846951648,-0.0186550825584463,
77.0815094601202));
#245932=CARTESIAN_POINT('Ctrl Pts',(-4.54533233720298,-7.14335758414781,
77.39941819177));
#245933=CARTESIAN_POINT('Ctrl Pts',(2.17844426069194,-7.57712589872956,
77.664342134811));
#245934=CARTESIAN_POINT('Ctrl Pts',(5.96050262542447,-4.45017743003856,
77.8762812892441));
#245935=CARTESIAN_POINT('Ctrl Pts',(7.89000395397738,0.0881671137640604,
78.0882204436772));
#245936=CARTESIAN_POINT('Ctrl Pts',(6.01110908805987,5.10838197229029,78.30015959811));
#245937=CARTESIAN_POINT('Ctrl Pts',(1.57291833765724,7.27800579091012,78.5120987525432));
#245938=CARTESIAN_POINT('Ctrl Pts',(-2.09885258226522,7.16074475090987,
78.6710531183679));
#245939=CARTESIAN_POINT('Ctrl Pts',(-5.25836834119772,5.27190320555331,
78.8300074841926));
#245940=CARTESIAN_POINT('Ctrl Pts',(-7.81274198177251,1.05910769268254,
79.0419466386258));
#245941=CARTESIAN_POINT('Ctrl Pts',(-6.41508694258267,-5.51612593070902,
79.3068705816669));
#245942=CARTESIAN_POINT('Ctrl Pts',(1.19245520850734,-8.38247717181995,
79.6247793133165));
#245943=CARTESIAN_POINT('Ctrl Pts',(6.58237766265624,-4.33943310603345,
79.8897032563578));
#245944=CARTESIAN_POINT('Ctrl Pts',(7.42200396880351,0.495512739411206,
80.1016424107907));
#245945=CARTESIAN_POINT('Ctrl Pts',(5.93645243083523,5.19793139167711,80.3135815652239));
#245946=CARTESIAN_POINT('Ctrl Pts',(1.24441809527773,7.78976258834587,80.5255207196566));
#245947=CARTESIAN_POINT('Ctrl Pts',(-3.53806550113452,6.55175867444267,
80.73745987409));
#245948=CARTESIAN_POINT('Ctrl Pts',(-6.25113863890163,4.07488771031202,
80.8964142399143));
#245949=CARTESIAN_POINT('Ctrl Pts',(-7.42299076065899,0.585328761610284,
81.0553686057394));
#245950=CARTESIAN_POINT('Ctrl Pts',(-6.62384401692773,-4.27613581386113,
81.2673077601722));
#245951=CARTESIAN_POINT('Ctrl Pts',(-1.286147084199,-8.36222520575478,81.5322317032136));
#245952=CARTESIAN_POINT('Ctrl Pts',(6.35708219443056,-5.59243948780764,
81.8501404348632));
#245953=CARTESIAN_POINT('Ctrl Pts',(7.8224042262569,0.984056646358646,82.1150643779043));
#245954=CARTESIAN_POINT('Ctrl Pts',(5.31602691445828,5.20303119054768,82.3270035323375));
#245955=CARTESIAN_POINT('Ctrl Pts',(1.12946861296887,7.8092418943331,82.5389426867703));
#245956=CARTESIAN_POINT('Ctrl Pts',(-4.12041745867891,6.72689657241653,
82.7508818412035));
#245957=CARTESIAN_POINT('Ctrl Pts',(-6.94843375179018,2.67632539625451,
82.9628209956364));
#245958=CARTESIAN_POINT('Ctrl Pts',(-7.39873571944801,-0.969615329745792,
83.1217753614612));
#245959=CARTESIAN_POINT('Ctrl Pts',(-6.01965891788265,-4.38259148244517,
83.280729727286));
#245960=CARTESIAN_POINT('Ctrl Pts',(-2.25111163908191,-7.55600049306653,
83.4926688817188));
#245961=CARTESIAN_POINT('Ctrl Pts',(4.46099559454575,-7.18891528792723,
83.7575928247604));
#245962=CARTESIAN_POINT('Ctrl Pts',(8.46609728487924,-0.114325039996204,
84.0755015564097));
#245963=CARTESIAN_POINT('Ctrl Pts',(5.3024933093211,5.83454711757506,84.340425499451));
#245964=CARTESIAN_POINT('Ctrl Pts',(0.654834329437635,7.40964693664927,
84.552364653884));
#245965=CARTESIAN_POINT('Ctrl Pts',(-4.22040857419456,6.66694156108873,
84.7643038083171));
#245966=CARTESIAN_POINT('Ctrl Pts',(-7.50472227466187,2.43066268945576,
84.9762429627499));
#245967=CARTESIAN_POINT('Ctrl Pts',(-7.01894948765949,-2.4855175153939,
85.1881821171831));
#245968=CARTESIAN_POINT('Ctrl Pts',(-4.99003695120001,-5.54806050431944,
85.3471364830078));
#245969=CARTESIAN_POINT('Ctrl Pts',(-1.72290192399602,-7.24396373195811,
85.5060908488326));
#245970=CARTESIAN_POINT('Ctrl Pts',(3.20364600373927,-7.20397802228505,
85.7180300032656));
#245971=CARTESIAN_POINT('Ctrl Pts',(8.06390435080163,-2.56016236451326,
85.9829539463069));
#245972=CARTESIAN_POINT('Ctrl Pts',(6.50577569840637,5.41874118350685,86.3008626779564));
#245973=CARTESIAN_POINT('Ctrl Pts',(0.233871956267354,7.88058876421495,
86.5657866209976));
#245974=CARTESIAN_POINT('Ctrl Pts',(-4.32111265355103,6.05472221989799,
86.7777257754307));
#245975=CARTESIAN_POINT('Ctrl Pts',(-7.54169303146352,2.32009149200691,
86.9896649298636));
#245976=CARTESIAN_POINT('Ctrl Pts',(-7.28178746474286,-3.03389994034617,
87.2016040842967));
#245977=CARTESIAN_POINT('Ctrl Pts',(-3.71571842818992,-6.45266501470942,
87.4135432387298));
#245978=CARTESIAN_POINT('Ctrl Pts',(-0.182813845036814,-7.45976026638884,
87.5724976045544));
#245979=CARTESIAN_POINT('Ctrl Pts',(3.40198965826229,-6.62343324528226,
87.7314519703793));
#245980=CARTESIAN_POINT('Ctrl Pts',(7.11853069868959,-3.38927245211331,
87.9433911248123));
#245981=CARTESIAN_POINT('Ctrl Pts',(7.79079554783678,3.29916496152483,88.2083150678536));
#245982=CARTESIAN_POINT('Ctrl Pts',(1.41837078524883,8.34722096073662,88.5262237995031));
#245983=CARTESIAN_POINT('Ctrl Pts',(-4.94716290886032,6.1387258055558,88.7911477425443));
#245984=CARTESIAN_POINT('Ctrl Pts',(-7.22006221792976,1.78951873251688,
89.0030868969774));
#245985=CARTESIAN_POINT('Ctrl Pts',(-7.23796740124329,-3.14193988017693,
89.2150260514101));
#245986=CARTESIAN_POINT('Ctrl Pts',(-3.55876946335482,-7.04018021334767,
89.4269652058435));
#245987=CARTESIAN_POINT('Ctrl Pts',(1.37351966289223,-7.31825750881274,
89.6389043602761));
#245988=CARTESIAN_POINT('Ctrl Pts',(4.71228104662943,-5.78583196018578,
89.7978587261012));
#245989=CARTESIAN_POINT('Ctrl Pts',(6.89167190790973,-2.81926584474774,
89.9568130919259));
#245990=CARTESIAN_POINT('Ctrl Pts',(7.61180363044634,2.05452976477962,90.1687522463588));
#245991=CARTESIAN_POINT('Ctrl Pts',(3.77294238406992,7.57270694521032,90.4336761894001));
#245992=CARTESIAN_POINT('Ctrl Pts',(-4.35079197496986,7.26350346887399,
90.7515849210497));
#245993=CARTESIAN_POINT('Ctrl Pts',(-7.75028138648021,1.44620669096039,
91.016508864091));
#245994=CARTESIAN_POINT('Ctrl Pts',(-6.64859761096745,-3.33583955433172,
91.2284480185239));
#245995=CARTESIAN_POINT('Ctrl Pts',(-3.45522124698925,-7.09375813278554,
91.4403871729571));
#245996=CARTESIAN_POINT('Ctrl Pts',(1.8748160657606,-7.66250887433638,91.6523263273899));
#245997=CARTESIAN_POINT('Ctrl Pts',(5.80255816582133,-4.66623702375972,
91.8642654818231));
#245998=CARTESIAN_POINT('Ctrl Pts',(7.34235848692903,-1.33087038563187,
92.0232198476477));
#245999=CARTESIAN_POINT('Ctrl Pts',(7.06878493979507,2.34001732142302,92.1821742134726));
#246000=CARTESIAN_POINT('Ctrl Pts',(4.44636692906912,6.51079627963601,92.3941133679054));
#246001=CARTESIAN_POINT('Ctrl Pts',(-2.05842322905156,8.20633161172813,
92.6590373109469));
#246002=CARTESIAN_POINT('Ctrl Pts',(-8.02869157557259,2.6884912192783,92.9769460425962));
#246003=CARTESIAN_POINT('Ctrl Pts',(-6.82812914707941,-3.94144995064046,
93.2418699856376));
#246004=CARTESIAN_POINT('Ctrl Pts',(-2.88140051968578,-6.85778439220427,
93.4538091400705));
#246005=CARTESIAN_POINT('Ctrl Pts',(1.98832067587906,-7.63587186914367,
93.6657482945037));
#246006=CARTESIAN_POINT('Ctrl Pts',(6.40724755397117,-4.601755785768,93.8776874489367));
#246007=CARTESIAN_POINT('Ctrl Pts',(7.44252373823067,0.228669271041487,
94.0896266033697));
#246008=CARTESIAN_POINT('Ctrl Pts',(6.44323850828845,3.76379086284547,94.2485809691943));
#246009=CARTESIAN_POINT('Ctrl Pts',(3.84819713631814,6.37454158270743,94.4075353350193));
#246010=CARTESIAN_POINT('Ctrl Pts',(-0.85627224174157,7.83756626197594,
94.6194744894521));
#246011=CARTESIAN_POINT('Ctrl Pts',(-6.90038169731781,4.89547925568775,
94.8843984324935));
#246012=CARTESIAN_POINT('Ctrl Pts',(-7.84749908248109,-3.17877831914504,
95.2023071641429));
#246013=CARTESIAN_POINT('Ctrl Pts',(-2.62395032113123,-7.43459885096939,
95.4672311071843));
#246014=CARTESIAN_POINT('Ctrl Pts',(2.27077815416402,-7.08344847509866,
95.6791702616173));
#246015=CARTESIAN_POINT('Ctrl Pts',(6.47615113221677,-4.50770726919954,
95.8911094160503));
#246016=CARTESIAN_POINT('Ctrl Pts',(7.85995451357935,0.670889390422631,
96.1030485704833));
#246017=CARTESIAN_POINT('Ctrl Pts',(5.50514619750763,5.01366279018771,96.3149877249164));
#246018=CARTESIAN_POINT('Ctrl Pts',(2.4470944939041,7.04933845632589,96.473942090741));
#246019=CARTESIAN_POINT('Ctrl Pts',(-1.22207526445053,7.34506185390236,
96.6328964565659));
#246020=CARTESIAN_POINT('Ctrl Pts',(-5.74733333571994,5.39711094855044,
96.844835610999));
#246021=CARTESIAN_POINT('Ctrl Pts',(-8.42558447744543,-0.768447086648144,
97.10975955404));
#246022=CARTESIAN_POINT('Ctrl Pts',(-3.89430695789088,-7.51812787664129,
97.4276682856896));
#246023=CARTESIAN_POINT('Ctrl Pts',(2.84146339511113,-7.35421383540367,
97.692592228731));
#246024=CARTESIAN_POINT('Ctrl Pts',(6.33147860409847,-3.90436350903053,
97.9045313831638));
#246025=CARTESIAN_POINT('Ctrl Pts',(7.85113768408234,0.78714381004357,98.1164705375972));
#246026=CARTESIAN_POINT('Ctrl Pts',(5.53467498128681,5.62106310062747,98.3284096920297));
#246027=CARTESIAN_POINT('Ctrl Pts',(0.921650548315969,7.38877591326425,
98.540348846463));
#246028=CARTESIAN_POINT('Ctrl Pts',(-2.72527642184487,6.94653241253989,
98.6993032122876));
#246029=CARTESIAN_POINT('Ctrl Pts',(-5.70494174153298,4.7850852986492,98.8582575781126));
#246030=CARTESIAN_POINT('Ctrl Pts',(-7.87586601184446,0.362466034703414,
99.0701967325454));
#246031=CARTESIAN_POINT('Ctrl Pts',(-5.90092357360854,-6.06300962311448,
99.3351206755868));
#246032=CARTESIAN_POINT('Ctrl Pts',(1.93073303258823,-8.24379423619251,
99.6530294072363));
#246033=CARTESIAN_POINT('Ctrl Pts',(6.94109181254378,-3.73893297779421,
99.9179533502775));
#246034=CARTESIAN_POINT('Ctrl Pts',(7.34887382895609,1.15140313135301,100.129892504711));
#246035=CARTESIAN_POINT('Ctrl Pts',(5.45237566459545,5.70364426697838,100.341831659144));
#246036=CARTESIAN_POINT('Ctrl Pts',(0.549083957339117,7.86940177761382,
100.553770813577));
#246037=CARTESIAN_POINT('Ctrl Pts',(-4.1048480871876,6.21238049468619,100.76570996801));
#246038=CARTESIAN_POINT('Ctrl Pts',(-6.58770877616357,3.50478775596863,
100.924664333834));
#246039=CARTESIAN_POINT('Ctrl Pts',(-7.4456558563651,-0.0749029919971758,
101.083618699659));
#246040=CARTESIAN_POINT('Ctrl Pts',(-6.21876413329544,-4.84640276053068,
101.295557854092));
#246041=CARTESIAN_POINT('Ctrl Pts',(-0.539909162595909,-8.44330994383676,
101.560481797134));
#246042=CARTESIAN_POINT('Ctrl Pts',(6.82774178522963,-5.00697668918455,
101.878390528783));
#246043=CARTESIAN_POINT('Ctrl Pts',(7.70439671035187,1.67351327814228,102.143314471825));
#246044=CARTESIAN_POINT('Ctrl Pts',(4.83393995337018,5.65373330216565,102.355253626257));
#246045=CARTESIAN_POINT('Ctrl Pts',(0.432860360337941,7.87861600920848,
102.567192780691));
#246046=CARTESIAN_POINT('Ctrl Pts',(-4.70043121148294,6.33521301582163,
102.779131935123));
#246047=CARTESIAN_POINT('Ctrl Pts',(-7.15829960162867,2.04992586279794,
102.991071089556));
#246048=CARTESIAN_POINT('Ctrl Pts',(-7.28367563428598,-1.6215774383111,
103.150025455381));
#246049=CARTESIAN_POINT('Ctrl Pts',(-5.6075213658915,-4.89888821271768,
103.308979821206));
#246050=CARTESIAN_POINT('Ctrl Pts',(-1.57253466484514,-7.72578680722558,
103.520918975639));
#246051=CARTESIAN_POINT('Ctrl Pts',(5.08061941222205,-6.76522661111206,
103.78584291868));
#246052=CARTESIAN_POINT('Ctrl Pts',(8.44291014169328,0.63650749492915,104.10375165033));
#246053=CARTESIAN_POINT('Ctrl Pts',(4.7644859407326,6.28156422264086,104.368675593371));
#246054=CARTESIAN_POINT('Ctrl Pts',(-0.00448826495536526,7.43852509441779,
104.580614747804));
#246055=CARTESIAN_POINT('Ctrl Pts',(-4.79471474775313,6.26663137577012,
104.792553902237));
#246056=CARTESIAN_POINT('Ctrl Pts',(-7.69062470199101,1.75592403675235,
105.00449305667));
#246057=CARTESIAN_POINT('Ctrl Pts',(-6.7710239269735,-3.0978515474434,105.216432211103));
#246058=CARTESIAN_POINT('Ctrl Pts',(-4.47865172838059,-5.96851093907047,
105.375386576928));
#246059=CARTESIAN_POINT('Ctrl Pts',(-1.07406084817673,-7.36816088885468,
105.534340942753));
#246060=CARTESIAN_POINT('Ctrl Pts',(3.82955346812604,-6.89167376604588,
105.746280097186));
#246061=CARTESIAN_POINT('Ctrl Pts',(8.25908404421422,-1.83535159088185,
106.011204040227));
#246062=CARTESIAN_POINT('Ctrl Pts',(5.99988701466406,5.97404630573564,106.329112771877));
#246063=CARTESIAN_POINT('Ctrl Pts',(-0.465535222508124,7.87030192046052,
106.594036714917));
#246064=CARTESIAN_POINT('Ctrl Pts',(-4.84075914199551,5.64789577223166,
106.805975869351));
#246065=CARTESIAN_POINT('Ctrl Pts',(-7.7176496040166,1.64251115726207,107.017915023784));
#246066=CARTESIAN_POINT('Ctrl Pts',(-6.98422221497737,-3.66737202660644,
107.229854178217));
#246067=CARTESIAN_POINT('Ctrl Pts',(-3.12917001166206,-6.75660745254302,
107.44179333265));
#246068=CARTESIAN_POINT('Ctrl Pts',(0.47909274384839,-7.44660421109663,
107.600747698475));
#246069=CARTESIAN_POINT('Ctrl Pts',(3.97566059304344,-6.29583389540692,
107.759702064299));
#246070=CARTESIAN_POINT('Ctrl Pts',(7.39091831859026,-2.74499061396732,
107.971641218732));
#246071=CARTESIAN_POINT('Ctrl Pts',(7.46771553014855,3.97670837154622,108.236565161774));
#246072=CARTESIAN_POINT('Ctrl Pts',(0.672942351553414,8.44008424385051,
108.554473893423));
#246073=CARTESIAN_POINT('Ctrl Pts',(-5.47179099638164,5.67607951446395,
108.819397836464));
#246074=CARTESIAN_POINT('Ctrl Pts',(-7.35025794708428,1.14253395403798,
109.031336990897));
#246075=CARTESIAN_POINT('Ctrl Pts',(-6.93099862198739,-3.77110281139561,
109.24327614533));
#246076=CARTESIAN_POINT('Ctrl Pts',(-2.92076503521324,-7.32789936740364,
109.455215299763));
#246077=CARTESIAN_POINT('Ctrl Pts',(2.01675902450346,-7.1677145776551,109.667154454196));
#246078=CARTESIAN_POINT('Ctrl Pts',(5.20655523270202,-5.34539303912755,
109.826108820021));
#246079=CARTESIAN_POINT('Ctrl Pts',(7.11443051527581,-2.19733475668721,
109.985063185846));
#246080=CARTESIAN_POINT('Ctrl Pts',(7.39974485319851,2.72110697518556,110.197002340279));
#246081=CARTESIAN_POINT('Ctrl Pts',(3.08689514972448,7.87731318700451,110.46192628332));
#246082=CARTESIAN_POINT('Ctrl Pts',(-4.97746055926141,6.84928900199175,
110.77983501497));
#246083=CARTESIAN_POINT('Ctrl Pts',(-7.84796126083906,0.753577740494986,
111.044758958011));
#246084=CARTESIAN_POINT('Ctrl Pts',(-6.32676235785494,-3.91200125153804,
111.256698112444));
#246085=CARTESIAN_POINT('Ctrl Pts',(-2.81287553995915,-7.37208854455821,
111.468637266877));
#246086=CARTESIAN_POINT('Ctrl Pts',(2.54659477910015,-7.46617924783338,
111.68057642131));
#246087=CARTESIAN_POINT('Ctrl Pts',(6.19330734239266,-4.13356908643254,
111.892515575743));
#246088=CARTESIAN_POINT('Ctrl Pts',(7.4314211347052,-0.674851133649304,
112.051469941568));
#246089=CARTESIAN_POINT('Ctrl Pts',(6.83355947930127,2.95734110857797,112.210424307393));
#246090=CARTESIAN_POINT('Ctrl Pts',(3.85179048651812,6.87927010014943,112.422363461825));
#246091=CARTESIAN_POINT('Ctrl Pts',(-2.7776804047817,7.99158784475522,112.687287404867));
#246092=CARTESIAN_POINT('Ctrl Pts',(-8.23538413392086,1.96629642184775,
113.005196136516));
#246093=CARTESIAN_POINT('Ctrl Pts',(-6.45190974192794,-4.53114070015648,
113.270120079558));
#246094=CARTESIAN_POINT('Ctrl Pts',(-2.26222846692231,-7.08618360531622,
113.482059233991));
#246095=CARTESIAN_POINT('Ctrl Pts',(2.65729172693086,-7.42958673077397,
113.693998388424));
#246096=CARTESIAN_POINT('Ctrl Pts',(6.78990162222115,-4.01574569541913,
113.905937542857));
#246097=CARTESIAN_POINT('Ctrl Pts',(7.39296419871876,0.887428637191924,
114.11787669729));
#246098=CARTESIAN_POINT('Ctrl Pts',(6.08428053030461,4.32006649977597,114.276831063114));
#246099=CARTESIAN_POINT('Ctrl Pts',(3.26805169895397,6.69053358728565,114.435785428939));
#246100=CARTESIAN_POINT('Ctrl Pts',(-1.54757566664994,7.73082509301787,
114.647724583372));
#246101=CARTESIAN_POINT('Ctrl Pts',(-7.30712876103848,4.26460478604429,
114.912648526414));
#246102=CARTESIAN_POINT('Ctrl Pts',(-7.53486622398735,-3.86182138872599,
115.230557258063));
#246103=CARTESIAN_POINT('Ctrl Pts',(-1.954666249214,-7.63790908670584,115.495481201104));
#246104=CARTESIAN_POINT('Ctrl Pts',(2.88967413267942,-6.85430223521909,
115.707420355537));
#246105=CARTESIAN_POINT('Ctrl Pts',(6.85019813537203,-3.91596014002346,
115.91935950997));
#246106=CARTESIAN_POINT('Ctrl Pts',(7.76955642183854,1.36490678714159,116.131298664403));
#246107=CARTESIAN_POINT('Ctrl Pts',(5.0390993610438,5.48187256867338,116.343237818836));
#246108=CARTESIAN_POINT('Ctrl Pts',(1.81265357974105,7.23848956162698,116.502192184661));
#246109=CARTESIAN_POINT('Ctrl Pts',(-1.86828644079946,7.20783652455841,
116.661146550486));
#246110=CARTESIAN_POINT('Ctrl Pts',(-6.20308001327729,4.86646128225844,
116.873085704919));
#246111=CARTESIAN_POINT('Ctrl Pts',(-8.32431331143111,-1.51221447046321,
117.13800964796));
#246112=CARTESIAN_POINT('Ctrl Pts',(-3.21261961787344,-7.83370593286875,
117.45591837961));
#246113=CARTESIAN_POINT('Ctrl Pts',(3.48211228444008,-7.07341992257992,
117.720842322651));
#246114=CARTESIAN_POINT('Ctrl Pts',(6.65261833304377,-3.32781385291546,
117.932781477084));
#246115=CARTESIAN_POINT('Ctrl Pts',(7.75047021907653,1.47992219231806,118.144720631517));
#246116=CARTESIAN_POINT('Ctrl Pts',(5.01467571504118,6.08949956915138,118.35665978595));
#246117=CARTESIAN_POINT('Ctrl Pts',(0.263127717982059,7.44138515557925,
118.568598940383));
#246118=CARTESIAN_POINT('Ctrl Pts',(-3.33024822704816,6.67764111645518,
118.727553306208));
#246119=CARTESIAN_POINT('Ctrl Pts',(-6.10660908642409,4.26060172454973,
118.886507672032));
#246120=CARTESIAN_POINT('Ctrl Pts',(-7.87699554054792,-0.337028659061501,
119.098446826465));
#246121=CARTESIAN_POINT('Ctrl Pts',(-5.34031144393764,-6.56216872636603,
119.363370769507));
#246122=CARTESIAN_POINT('Ctrl Pts',(2.65381321717774,-8.04022069722845,
119.681279501156));
#246123=CARTESIAN_POINT('Ctrl Pts',(7.24516953240903,-3.10900206002699,
119.946203444198));
#246124=CARTESIAN_POINT('Ctrl Pts',(7.21789743819818,1.7982303235287,120.158142598631));
#246125=CARTESIAN_POINT('Ctrl Pts',(4.92538082098571,6.16446121574084,120.370081753063));
#246126=CARTESIAN_POINT('Ctrl Pts',(-0.150572262960701,7.88709740800408,
120.582020907497));
#246127=CARTESIAN_POINT('Ctrl Pts',(-4.63931958883328,5.82410190349662,
120.79396006193));
#246128=CARTESIAN_POINT('Ctrl Pts',(-6.8724241269978,2.90710005892275,120.952914427754));
#246129=CARTESIAN_POINT('Ctrl Pts',(-7.40971288313931,-0.734545151146761,
121.111868793579));
#246130=CARTESIAN_POINT('Ctrl Pts',(-5.76473359089571,-5.3785215151415,
121.323807948012));
#246131=CARTESIAN_POINT('Ctrl Pts',(0.210578624102449,-8.45793363385046,
121.588731891054));
#246132=CARTESIAN_POINT('Ctrl Pts',(7.24465718346336,-4.38210174983432,
121.906640622703));
#246133=CARTESIAN_POINT('Ctrl Pts',(7.52574446095941,2.34979694249055,122.171564565744));
#246134=CARTESIAN_POINT('Ctrl Pts',(4.31380290075385,6.05993236416489,122.383503720177));
#246135=CARTESIAN_POINT('Ctrl Pts',(-0.267155128735916,7.88597403300938,
122.59544287461));
#246136=CARTESIAN_POINT('Ctrl Pts',(-5.24344577943899,5.89366217964708,
122.807382029043));
#246137=CARTESIAN_POINT('Ctrl Pts',(-7.31181929125222,1.40739045105361,
123.019321183476));
#246138=CARTESIAN_POINT('Ctrl Pts',(-7.11128249838525,-2.2607753895711,
123.178275549301));
#246139=CARTESIAN_POINT('Ctrl Pts',(-5.15124451897244,-5.37662361481536,
123.337229915126));
#246140=CARTESIAN_POINT('Ctrl Pts',(-0.881579570788664,-7.83476001695065,
123.549169069559));
#246141=CARTESIAN_POINT('Ctrl Pts',(5.66025141461661,-6.28828582642984,
123.8140930126));
#246142=CARTESIAN_POINT('Ctrl Pts',(8.35326509732775,1.38232979624049,124.13200174425));
#246143=CARTESIAN_POINT('Ctrl Pts',(4.18897518403377,6.67913634163493,124.396925687291));
#246144=CARTESIAN_POINT('Ctrl Pts',(-0.663775530218678,7.40885131246999,
124.608864841724));
#246145=CARTESIAN_POINT('Ctrl Pts',(-5.33127958881593,5.81699374745947,
124.820803996157));
#246146=CARTESIAN_POINT('Ctrl Pts',(-7.81599080145722,1.06736372491064,
125.03274315059));
#246147=CARTESIAN_POINT('Ctrl Pts',(-6.4698006251684,-3.68580101202109,
125.244682305023));
#246148=CARTESIAN_POINT('Ctrl Pts',(-3.93201304567724,-6.34198056939268,
125.403636670848));
#246149=CARTESIAN_POINT('Ctrl Pts',(-0.416765361672836,-7.43435997399531,
125.562591036672));
#246150=CARTESIAN_POINT('Ctrl Pts',(4.42531681375818,-6.52512208013845,
125.774530191105));
#246151=CARTESIAN_POINT('Ctrl Pts',(8.38925281342742,-1.09609394850368,
126.039454134147));
#246152=CARTESIAN_POINT('Ctrl Pts',(5.44677055144542,6.48232705220241,126.357362865796));
#246153=CARTESIAN_POINT('Ctrl Pts',(-1.16127796647469,7.79806442953511,
126.622286808837));
#246154=CARTESIAN_POINT('Ctrl Pts',(-5.32230186203618,5.19661222472599,
126.834225963271));
#246155=CARTESIAN_POINT('Ctrl Pts',(-7.83285712368212,0.952001886600132,
127.046165117703));
#246156=CARTESIAN_POINT('Ctrl Pts',(-6.63168104553608,-4.27197659637739,
127.258104272137));
#246157=CARTESIAN_POINT('Ctrl Pts',(-2.51799050609984,-7.00736562774031,
127.470043426569));
#246158=CARTESIAN_POINT('Ctrl Pts',(1.13722818064386,-7.37483262176709,
127.628997792394));
#246159=CARTESIAN_POINT('Ctrl Pts',(4.5180373349009,-5.91867723651794,127.787952158219));
#246160=CARTESIAN_POINT('Ctrl Pts',(7.60512873288296,-2.07910173371068,
127.999891312652));
#246161=CARTESIAN_POINT('Ctrl Pts',(7.08585380183994,4.62294934111277,128.264815255693));
#246162=CARTESIAN_POINT('Ctrl Pts',(-0.0777831107195537,8.46651186968383,
128.582723987343));
#246163=CARTESIAN_POINT('Ctrl Pts',(-5.95334818308693,5.16875427676112,
128.847647930384));
#246164=CARTESIAN_POINT('Ctrl Pts',(-7.42259652650057,0.486555782601546,
129.059587084817));
#246165=CARTESIAN_POINT('Ctrl Pts',(-6.56947286963103,-4.37058171497872,
129.27152623925));
#246166=CARTESIAN_POINT('Ctrl Pts',(-2.25976996630488,-7.55793736604614,
129.483465393683));
#246167=CARTESIAN_POINT('Ctrl Pts',(2.64412357876513,-6.9607513768183,129.695404548116));
#246168=CARTESIAN_POINT('Ctrl Pts',(5.65984630663675,-4.86287815179347,
129.854358913941));
#246169=CARTESIAN_POINT('Ctrl Pts',(7.28118827550971,-1.55810746937658,
130.013313279766));
#246170=CARTESIAN_POINT('Ctrl Pts',(7.12943939277857,3.36626514224055,130.225252434199));
#246171=CARTESIAN_POINT('Ctrl Pts',(2.37654959055416,8.11991359279997,130.49017637724));
#246172=CARTESIAN_POINT('Ctrl Pts',(-5.56494933743067,6.38116073482492,
130.808085108889));
#246173=CARTESIAN_POINT('Ctrl Pts',(-7.88386634139248,0.0550170443502282,
131.073009051931));
#246174=CARTESIAN_POINT('Ctrl Pts',(-5.95512634391571,-4.45736984669529,
131.284948206364));
#246175=CARTESIAN_POINT('Ctrl Pts',(-2.14838843870147,-7.59238996855304,
131.496887360797));
#246176=CARTESIAN_POINT('Ctrl Pts',(3.19832811286549,-7.21108000285525,
131.70882651523));
#246177=CARTESIAN_POINT('Ctrl Pts',(6.53530624122347,-3.56836398895286,
131.920765669663));
#246178=CARTESIAN_POINT('Ctrl Pts',(7.4619877629195,-0.0135198266309791,
132.079720035487));
#246179=CARTESIAN_POINT('Ctrl Pts',(6.5445440293885,3.55138634553384,132.238674401312));
#246180=CARTESIAN_POINT('Ctrl Pts',(3.2268948945583,7.19359413201327,132.450613555745));
#246181=CARTESIAN_POINT('Ctrl Pts',(-3.47507323660292,7.71393872222958,
132.715537498787));
#246182=CARTESIAN_POINT('Ctrl Pts',(-8.37725229600153,1.22862405323487,
133.033446230436));
#246183=CARTESIAN_POINT('Ctrl Pts',(-6.02490452661707,-5.08516486360561,
133.298370173477));
#246184=CARTESIAN_POINT('Ctrl Pts',(-1.62524935270184,-7.25880426488761,
133.51030932791));
#246185=CARTESIAN_POINT('Ctrl Pts',(3.30534591134366,-7.16482014032892,
133.722248482344));
#246186=CARTESIAN_POINT('Ctrl Pts',(7.11910964228672,-3.39812562053916,
133.934187636776));
#246187=CARTESIAN_POINT('Ctrl Pts',(7.28521099408995,1.53920233165873,134.146126791209));
#246188=CARTESIAN_POINT('Ctrl Pts',(5.67743121364578,4.84233765036753,134.305081157034));
#246189=CARTESIAN_POINT('Ctrl Pts',(2.66218062382144,6.95386018813151,134.464035522859));
#246190=CARTESIAN_POINT('Ctrl Pts',(-2.22669452000353,7.56323383563218,
134.675974677292));
#246191=CARTESIAN_POINT('Ctrl Pts',(-7.65636419437899,3.60015618240601,
134.940898620333));
#246192=CARTESIAN_POINT('Ctrl Pts',(-7.16291254803651,-4.51445667965736,
135.258807351983));
#246193=CARTESIAN_POINT('Ctrl Pts',(-1.27001379708206,-7.78111415223867,
135.523731295024));
#246194=CARTESIAN_POINT('Ctrl Pts',(3.48584772319138,-6.57118115194385,
135.735670449457));
#246195=CARTESIAN_POINT('Ctrl Pts',(7.17026361016127,-3.29344432097186,
135.94760960389));
#246196=CARTESIAN_POINT('Ctrl Pts',(7.61812385785892,2.04829339595507,136.159548758323));
#246197=CARTESIAN_POINT('Ctrl Pts',(4.53323533980309,5.90679245446073,136.371487912756));
#246198=CARTESIAN_POINT('Ctrl Pts',(1.16426115636376,7.37095385983623,136.530442278581));
#246199=CARTESIAN_POINT('Ctrl Pts',(-2.50036914776536,7.01334512305659,
136.689396644406));
#246200=CARTESIAN_POINT('Ctrl Pts',(-6.6087513813229,4.29865066804881,136.901335798838));
#246201=CARTESIAN_POINT('Ctrl Pts',(-8.16010007421704,-2.24644782679431,
137.16625974188));
#246202=CARTESIAN_POINT('Ctrl Pts',(-2.50113137324256,-8.08348055054976,
137.484168473529));
#246203=CARTESIAN_POINT('Ctrl Pts',(4.08776845207816,-6.74390741787467,
137.749092416571));
#246204=CARTESIAN_POINT('Ctrl Pts',(6.93159571519058,-2.71569652585027,
137.961031571004));
#246205=CARTESIAN_POINT('Ctrl Pts',(7.40334174710716,0.922285299287664,
138.119985936828));
#246206=CARTESIAN_POINT('Ctrl Pts',(6.04702995925678,4.36403597153456,138.279005072222));
#246207=CARTESIAN_POINT('Ctrl Pts',(4.16396134314499,5.93645191893425,138.385039419009));
#246208=CARTESIAN_POINT('Ctrl Pts',(3.08878933661219,6.45122224576104,138.438088977186));
#246209=CARTESIAN_POINT('Ctrl Pts',(3.92320494081329,-5.50525709974226,
8.0038671538841));
#246210=CARTESIAN_POINT('Ctrl Pts',(4.84016051734621,-4.85181479700849,
8.05688452237381));
#246211=CARTESIAN_POINT('Ctrl Pts',(6.33798051091494,-3.08289948015477,
8.16288667947178));
#246212=CARTESIAN_POINT('Ctrl Pts',(7.04300948471557,0.34095441748302,8.32187362517801));
#246213=CARTESIAN_POINT('Ctrl Pts',(6.01420291001966,3.65197858249371,8.48082799100276));
#246214=CARTESIAN_POINT('Ctrl Pts',(2.71341797368867,6.94195862936583,8.6927671454358));
#246215=CARTESIAN_POINT('Ctrl Pts',(-3.63885434763407,7.12154028903951,
8.95769108847704));
#246216=CARTESIAN_POINT('Ctrl Pts',(-7.96224185718031,0.769392088592678,
9.2755998201266));
#246217=CARTESIAN_POINT('Ctrl Pts',(-5.45706751038434,-5.07361335315654,
9.54052376316782));
#246218=CARTESIAN_POINT('Ctrl Pts',(-1.19166322865416,-6.93560061915194,
9.75246291760087));
#246219=CARTESIAN_POINT('Ctrl Pts',(2.27857359250251,-6.67472132479364,
9.9114172834256));
#246220=CARTESIAN_POINT('Ctrl Pts',(5.17829028007211,-4.76543010856528,
10.0703716492504));
#246221=CARTESIAN_POINT('Ctrl Pts',(7.42547444076233,-0.672711200711117,
10.2823108036834));
#246222=CARTESIAN_POINT('Ctrl Pts',(6.1428106404885,4.22861967768184,10.4942499581164));
#246223=CARTESIAN_POINT('Ctrl Pts',(2.18093601810749,6.6835833434735,10.7061891125494));
#246224=CARTESIAN_POINT('Ctrl Pts',(-2.44351173292077,7.03950064603549,
10.9181282669824));
#246225=CARTESIAN_POINT('Ctrl Pts',(-7.40125721739437,3.04282371117337,
11.1830522100237));
#246226=CARTESIAN_POINT('Ctrl Pts',(-6.54573505154432,-4.59298539844305,
11.5009609416732));
#246227=CARTESIAN_POINT('Ctrl Pts',(-0.847722772654031,-7.40327450707869,
11.7658848847145));
#246228=CARTESIAN_POINT('Ctrl Pts',(3.60575578158385,-6.0436066569362,11.9778240391475));
#246229=CARTESIAN_POINT('Ctrl Pts',(6.07119951744335,-3.58885319509753,
12.1367784049723));
#246230=CARTESIAN_POINT('Ctrl Pts',(7.03298623857799,-0.252625367839518,
12.295732770797));
#246231=CARTESIAN_POINT('Ctrl Pts',(6.07821522657084,4.31780302708026,12.5076719252301));
#246232=CARTESIAN_POINT('Ctrl Pts',(1.91666268563073,7.20709378759929,12.719611079663));
#246233=CARTESIAN_POINT('Ctrl Pts',(-2.68964418527962,6.49558992266904,
12.9315502340961));
#246234=CARTESIAN_POINT('Ctrl Pts',(-6.4340967659524,3.75865043672924,13.1434893885291));
#246235=CARTESIAN_POINT('Ctrl Pts',(-7.60129628069631,-2.50157786640446,
13.4084133315703));
#246236=CARTESIAN_POINT('Ctrl Pts',(-1.98571650717331,-7.74590505994148,
13.7263220632199));
#246237=CARTESIAN_POINT('Ctrl Pts',(4.17043359165409,-6.17531914645662,
13.9912460062611));
#246238=CARTESIAN_POINT('Ctrl Pts',(6.6694011530727,-2.24627829536837,14.2031851606941));
#246239=CARTESIAN_POINT('Ctrl Pts',(6.94596741139484,1.22182413023957,14.3621395265189));
#246240=CARTESIAN_POINT('Ctrl Pts',(5.50702470161187,4.3817119329183,14.5210938923437));
#246241=CARTESIAN_POINT('Ctrl Pts',(1.80951755333021,7.23282569158136,14.7330330467767));
#246242=CARTESIAN_POINT('Ctrl Pts',(-3.2308185920246,6.72142894914833,14.9449722012097));
#246243=CARTESIAN_POINT('Ctrl Pts',(-6.26738760209476,3.18539287105005,
15.1569113556427));
#246244=CARTESIAN_POINT('Ctrl Pts',(-7.33207086718258,-1.32883042973204,
15.3688505100757));
#246245=CARTESIAN_POINT('Ctrl Pts',(-4.14766486694815,-6.84357168727062,
15.633774453117));
#246246=CARTESIAN_POINT('Ctrl Pts',(3.52875528848565,-7.17565338129885,
15.9516831847665));
#246247=CARTESIAN_POINT('Ctrl Pts',(7.18402146978472,-1.97912058890141,
16.2166071278078));
#246248=CARTESIAN_POINT('Ctrl Pts',(6.52731310302662,2.63075305397933,16.4285462822408));
#246249=CARTESIAN_POINT('Ctrl Pts',(4.4820690634196,5.44521573247064,16.5875006480655));
#246250=CARTESIAN_POINT('Ctrl Pts',(1.33404174694253,6.90992425063454,16.7464550138903));
#246251=CARTESIAN_POINT('Ctrl Pts',(-3.32894729586721,6.67129906135416,
16.9583941683233));
#246252=CARTESIAN_POINT('Ctrl Pts',(-6.82536622599997,3.00502442063848,
17.1703333227564));
#246253=CARTESIAN_POINT('Ctrl Pts',(-6.83263188498128,-1.65590356738068,
17.3822724771893));
#246254=CARTESIAN_POINT('Ctrl Pts',(-4.70579246834758,-5.77759212439439,
17.5942116316224));
#246255=CARTESIAN_POINT('Ctrl Pts',(1.29959412076021,-7.89611628641483,
17.8591355746636));
#246256=CARTESIAN_POINT('Ctrl Pts',(7.34708623381123,-3.15633319028242,
18.1770443063132));
#246257=CARTESIAN_POINT('Ctrl Pts',(6.74451862507508,3.16836729238686,18.4419682493544));
#246258=CARTESIAN_POINT('Ctrl Pts',(3.24778949712727,6.24327969567209,18.6539074037875));
#246259=CARTESIAN_POINT('Ctrl Pts',(-0.136192434304023,7.05129556062135,
18.8128617696122));
#246260=CARTESIAN_POINT('Ctrl Pts',(-3.48016523744545,6.11679413190897,
18.971816135437));
#246261=CARTESIAN_POINT('Ctrl Pts',(-6.86731154651915,2.90312820725449,
19.1837552898699));
#246262=CARTESIAN_POINT('Ctrl Pts',(-7.13921530672556,-2.15578308089093,
19.395694444303));
#246263=CARTESIAN_POINT('Ctrl Pts',(-4.11368528329232,-5.70126902453786,
19.607633598736));
#246264=CARTESIAN_POINT('Ctrl Pts',(0.182384564579414,-7.44928113186926,
19.819572753169));
#246265=CARTESIAN_POINT('Ctrl Pts',(6.12218676667009,-5.15329278047616,
20.0844966962103));
#246266=CARTESIAN_POINT('Ctrl Pts',(7.63394730886059,2.38011844677504,20.4024054278598));
#246267=CARTESIAN_POINT('Ctrl Pts',(3.06317764812811,6.79293938435044,20.6673293709011));
#246268=CARTESIAN_POINT('Ctrl Pts',(-1.59282518475065,6.85489503251987,
20.8792685253341));
#246269=CARTESIAN_POINT('Ctrl Pts',(-4.6889913169139,5.26808104458408,21.0382228911588));
#246270=CARTESIAN_POINT('Ctrl Pts',(-6.62158680890006,2.38354959341743,
21.1971772569836));
#246271=CARTESIAN_POINT('Ctrl Pts',(-7.10481569504033,-2.26046791709614,
21.4091164114166));
#246272=CARTESIAN_POINT('Ctrl Pts',(-4.02151030593889,-6.2803861940861,
21.6210555658497));
#246273=CARTESIAN_POINT('Ctrl Pts',(0.582556149475053,-7.00624745729406,
21.8329947202826));
#246274=CARTESIAN_POINT('Ctrl Pts',(4.98289615108128,-5.54037899954143,
22.0449338747157));
#246275=CARTESIAN_POINT('Ctrl Pts',(8.00207295474845,0.0665260413783972,
22.3098578177569));
#246276=CARTESIAN_POINT('Ctrl Pts',(4.25145511183555,6.77253606614142,22.6277665494065));
#246277=CARTESIAN_POINT('Ctrl Pts',(-2.09051838595393,7.15239929404389,
22.8926904924477));
#246278=CARTESIAN_POINT('Ctrl Pts',(-5.66782830722953,4.17161842164514,
23.1046296468807));
#246279=CARTESIAN_POINT('Ctrl Pts',(-6.98796725114217,0.952696782488859,
23.2635840127055));
#246280=CARTESIAN_POINT('Ctrl Pts',(-6.58025897948308,-2.49537818677088,
23.4225383785302));
#246281=CARTESIAN_POINT('Ctrl Pts',(-3.92730037023841,-6.33754156330653,
23.6344775329633));
#246282=CARTESIAN_POINT('Ctrl Pts',(1.02918445790915,-7.38624229491818,
23.8464166873963));
#246283=CARTESIAN_POINT('Ctrl Pts',(4.99878460510776,-4.94358448616671,
24.0583558418293));
#246284=CARTESIAN_POINT('Ctrl Pts',(7.38831571551028,-0.968423667081756,
24.2702949962623));
#246285=CARTESIAN_POINT('Ctrl Pts',(6.03566162570836,5.25436828051194,24.5352189393036));
#246286=CARTESIAN_POINT('Ctrl Pts',(-1.17455272585738,7.90964861604609,
24.8531276709531));
#246287=CARTESIAN_POINT('Ctrl Pts',(-6.23938033231202,4.07396807206546,
25.1180516139943));
#246288=CARTESIAN_POINT('Ctrl Pts',(-7.01851810879394,-0.516799315569627,
25.3299907684274));
#246289=CARTESIAN_POINT('Ctrl Pts',(-5.9280883936475,-3.82061323081804,
25.4889451342521));
#246290=CARTESIAN_POINT('Ctrl Pts',(-3.37604649281442,-6.17487089828082,
25.6478995000769));
#246291=CARTESIAN_POINT('Ctrl Pts',(1.13792152115551,-7.36839574645685,
25.8598386545099));
#246292=CARTESIAN_POINT('Ctrl Pts',(5.5851887025007,-4.94180766978019,26.0717778089429));
#246293=CARTESIAN_POINT('Ctrl Pts',(7.01228405239937,-0.504725141632746,
26.283716963376));
#246294=CARTESIAN_POINT('Ctrl Pts',(6.24244793815225,4.06901674246726,26.4956561178089));
#246295=CARTESIAN_POINT('Ctrl Pts',(1.16813324157401,7.91663198697703,26.7605800608503));
#246296=CARTESIAN_POINT('Ctrl Pts',(-6.03599694875479,5.24488857553349,
27.0784887924997));
#246297=CARTESIAN_POINT('Ctrl Pts',(-7.38920525210955,-0.962667401363433,
27.3434127355411));
#246298=CARTESIAN_POINT('Ctrl Pts',(-4.9956684627223,-4.95681092907559,
27.555351889974));
#246299=CARTESIAN_POINT('Ctrl Pts',(-2.01879891484442,-6.75749719969035,
27.7143062557988));
#246300=CARTESIAN_POINT('Ctrl Pts',(1.45090541605391,-6.88633385813854,
27.8732606216235));
#246301=CARTESIAN_POINT('Ctrl Pts',(5.65618704933612,-4.85753737274708,
28.0851997760566));
#246302=CARTESIAN_POINT('Ctrl Pts',(7.45660139680916,-0.122030720491899,
28.2971389304895));
#246303=CARTESIAN_POINT('Ctrl Pts',(5.65524053006352,4.17673672228185,28.5090780849226));
#246304=CARTESIAN_POINT('Ctrl Pts',(2.09606865070999,7.15063281972518,28.7210172393556));
#246305=CARTESIAN_POINT('Ctrl Pts',(-4.2608731510886,6.77366645751254,28.9859411823969));
#246306=CARTESIAN_POINT('Ctrl Pts',(-7.996162939297,0.0591065423799839,
29.3038499140464));
#246307=CARTESIAN_POINT('Ctrl Pts',(-4.98731526310924,-5.53658461958353,
29.5687738570877));
#246308=CARTESIAN_POINT('Ctrl Pts',(-0.571587621537175,-7.01426871219993,
29.7807130115207));
#246309=CARTESIAN_POINT('Ctrl Pts',(2.86085178131299,-6.44630472036177,
29.9396673773454));
#246310=CARTESIAN_POINT('Ctrl Pts',(5.58046129630571,-4.28779340133288,
30.0986217431702));
#246311=CARTESIAN_POINT('Ctrl Pts',(7.45573477436185,-0.0118422583874216,
30.3105608976032));
#246312=CARTESIAN_POINT('Ctrl Pts',(5.74390437343873,4.7564018371487,30.5225000520362));
#246313=CARTESIAN_POINT('Ctrl Pts',(1.57993416102576,6.85059728395666,30.7344392064692));
#246314=CARTESIAN_POINT('Ctrl Pts',(-3.05781252937014,6.79520684352195,
30.9463783609023));
#246315=CARTESIAN_POINT('Ctrl Pts',(-7.64183700346619,2.37485252168492,
31.2113023039435));
#246316=CARTESIAN_POINT('Ctrl Pts',(-6.11287213635388,-5.15508579751365,
31.529211035593));
#246317=CARTESIAN_POINT('Ctrl Pts',(-0.188209149979401,-7.4492724543619,
31.7941349786343));
#246318=CARTESIAN_POINT('Ctrl Pts',(4.12723403517989,-5.70022957387632,
32.0060741330673));
#246319=CARTESIAN_POINT('Ctrl Pts',(6.3653979057508,-3.03661439169733,32.1650284988921));
#246320=CARTESIAN_POINT('Ctrl Pts',(7.02769791381951,0.37172915432722,32.3239828647168));
#246321=CARTESIAN_POINT('Ctrl Pts',(5.67158933474266,4.83954498716,32.5359220191499));
#246322=CARTESIAN_POINT('Ctrl Pts',(1.27032710627931,7.34860972774388,32.7478611735828));
#246323=CARTESIAN_POINT('Ctrl Pts',(-3.25478753390679,6.23163166508225,
32.9598003280159));
#246324=CARTESIAN_POINT('Ctrl Pts',(-6.7419174644648,3.17357880213563,33.1717394824488));
#246325=CARTESIAN_POINT('Ctrl Pts',(-7.3496553023264,-3.16546429837453,
33.4366634254902));
#246326=CARTESIAN_POINT('Ctrl Pts',(-1.2913520703836,-7.89142098518733,
33.7545721571396));
#246327=CARTESIAN_POINT('Ctrl Pts',(4.70136207017436,-5.78137332029135,
34.019496100181));
#246328=CARTESIAN_POINT('Ctrl Pts',(6.84224848195906,-1.64630303625135,
34.2314352546139));
#246329=CARTESIAN_POINT('Ctrl Pts',(6.81033506401044,1.83266302912182,34.3903896204387));
#246330=CARTESIAN_POINT('Ctrl Pts',(5.09698269437306,4.85257539306103,34.5493439862634));
#246331=CARTESIAN_POINT('Ctrl Pts',(1.16132278879302,7.36474375962547,34.7612831406965));
#246332=CARTESIAN_POINT('Ctrl Pts',(-3.81384894227602,6.40861546148153,
34.9732222951295));
#246333=CARTESIAN_POINT('Ctrl Pts',(-6.52505445803083,2.61735351449946,
35.1851614495625));
#246334=CARTESIAN_POINT('Ctrl Pts',(-7.18543454803273,-1.97347000660205,
35.3971006039956));
#246335=CARTESIAN_POINT('Ctrl Pts',(-3.52476887568925,-7.18426068988804,
35.6620245470368));
#246336=CARTESIAN_POINT('Ctrl Pts',(4.15087269174857,-6.83464492362513,
35.9799332786863));
#246337=CARTESIAN_POINT('Ctrl Pts',(7.33116418301752,-1.33458401949517,
36.2448572217275));
#246338=CARTESIAN_POINT('Ctrl Pts',(6.26844970540344,3.19893986609144,36.4567963761606));
#246339=CARTESIAN_POINT('Ctrl Pts',(3.98179858667866,5.82104779893825,36.6157507419853));
#246340=CARTESIAN_POINT('Ctrl Pts',(0.716338313692228,7.0009699294038,36.7747051078101));
#246341=CARTESIAN_POINT('Ctrl Pts',(-3.90714823546713,6.34998534886486,
36.9866442622431));
#246342=CARTESIAN_POINT('Ctrl Pts',(-7.0648502871895,2.38823916458096,37.1985834166761));
#246343=CARTESIAN_POINT('Ctrl Pts',(-6.65897147596041,-2.25498868788211,
37.4105225711092));
#246344=CARTESIAN_POINT('Ctrl Pts',(-4.17518168751194,-6.17194551071909,
37.6224617255421));
#246345=CARTESIAN_POINT('Ctrl Pts',(1.9943422664243,-7.74985136706838,37.8873856685834));
#246346=CARTESIAN_POINT('Ctrl Pts',(7.59792802485505,-2.49271038515526,
38.205294400233));
#246347=CARTESIAN_POINT('Ctrl Pts',(6.43714956059893,3.75368996028338,38.4702183432742));
#246348=CARTESIAN_POINT('Ctrl Pts',(2.68164134065499,6.50657188511213,38.6821574977073));
#246349=CARTESIAN_POINT('Ctrl Pts',(-0.760639713870074,7.01147236235613,
38.841111863532));
#246350=CARTESIAN_POINT('Ctrl Pts',(-4.00862313244799,5.78425977235483,
39.0000662293568));
#246351=CARTESIAN_POINT('Ctrl Pts',(-7.09759907144927,2.28302621221805,
39.2120053837898));
#246352=CARTESIAN_POINT('Ctrl Pts',(-6.92004203725226,-2.78007447567538,
39.4239445382228));
#246353=CARTESIAN_POINT('Ctrl Pts',(-3.59216968022922,-6.04344207290618,
39.6358836926558));
#246354=CARTESIAN_POINT('Ctrl Pts',(0.84192502812979,-7.40379738769429,
39.8478228470888));
#246355=CARTESIAN_POINT('Ctrl Pts',(6.55484758839465,-4.59037802149398,
40.1127467901301));
#246356=CARTESIAN_POINT('Ctrl Pts',(7.39294321005172,3.04737690942376,40.4306555217796));
#246357=CARTESIAN_POINT('Ctrl Pts',(2.44903763211165,7.03770541156364,40.6955794648208));
#246358=CARTESIAN_POINT('Ctrl Pts',(-2.19413183217394,6.68673788024343,
40.9075186192539));
#246359=CARTESIAN_POINT('Ctrl Pts',(-5.13746692096526,4.83174410522615,
41.0664729850786));
#246360=CARTESIAN_POINT('Ctrl Pts',(-6.80678919836751,1.78727203890934,
41.2254273509034));
#246361=CARTESIAN_POINT('Ctrl Pts',(-6.8764991954602,-2.88129833227098,
41.4373665053365));
#246362=CARTESIAN_POINT('Ctrl Pts',(-3.44902810826724,-6.61211017724467,
41.6493056597694));
#246363=CARTESIAN_POINT('Ctrl Pts',(1.20125387967055,-6.92703863254039,
41.8612448142025));
#246364=CARTESIAN_POINT('Ctrl Pts',(5.4543498365197,-5.07692046144884,42.0731839686354));
#246365=CARTESIAN_POINT('Ctrl Pts',(7.96468255945656,0.775518545482133,
42.3381079116768));
#246366=CARTESIAN_POINT('Ctrl Pts',(3.63444678971545,7.12270397165751,42.6560166433262));
#246367=CARTESIAN_POINT('Ctrl Pts',(-2.71623519168221,6.93895879559161,
42.9209405863675));
#246368=CARTESIAN_POINT('Ctrl Pts',(-6.01526780461176,3.65283878850994,
43.1328797408005));
#246369=CARTESIAN_POINT('Ctrl Pts',(-7.0449057115676,0.329576967523976,
43.2918341066252));
#246370=CARTESIAN_POINT('Ctrl Pts',(-6.33318599383895,-3.06879059232167,
43.4507884724501));
#246371=CARTESIAN_POINT('Ctrl Pts',(-3.35012305774061,-6.66069041186473,
43.6627276268829));
#246372=CARTESIAN_POINT('Ctrl Pts',(1.67980477892008,-7.26595154073829,
43.8746667813162));
#246373=CARTESIAN_POINT('Ctrl Pts',(5.41727957767459,-4.48106651116011,
44.086605935749));
#246374=CARTESIAN_POINT('Ctrl Pts',(7.44507244944886,-0.309757539823755,
44.2985450901822));
#246375=CARTESIAN_POINT('Ctrl Pts',(5.54619217953605,5.76865232051224,44.5634690332233));
#246376=CARTESIAN_POINT('Ctrl Pts',(-1.8709924218742,7.77441333429271,44.8813777648729));
#246377=CARTESIAN_POINT('Ctrl Pts',(-6.57591523561052,3.50491392155589,
45.1463017079142));
#246378=CARTESIAN_POINT('Ctrl Pts',(-6.94508926985662,-1.13684344118434,
45.3582408623472));
#246379=CARTESIAN_POINT('Ctrl Pts',(-5.56612151970435,-4.33100550568619,
45.5171952281719));
#246380=CARTESIAN_POINT('Ctrl Pts',(-2.81545688577237,-6.44980023383955,
45.6761495939967));
#246381=CARTESIAN_POINT('Ctrl Pts',(1.78653207542118,-7.23853744952694,
45.8880887484297));
#246382=CARTESIAN_POINT('Ctrl Pts',(6.00121826529194,-4.4273214498121,46.1000279028627));
#246383=CARTESIAN_POINT('Ctrl Pts',(7.02942136872401,0.118786872411061,
46.3119670572958));
#246384=CARTESIAN_POINT('Ctrl Pts',(5.85722687898137,4.60629425885479,46.5239062117287));
#246385=CARTESIAN_POINT('Ctrl Pts',(0.461854421036876,7.98901043816237,
46.78883015477));
#246386=CARTESIAN_POINT('Ctrl Pts',(-6.47711547532611,4.68925265414749,
47.1067388864195));
#246387=CARTESIAN_POINT('Ctrl Pts',(-7.27479849768731,-1.61381213327239,
47.3716628294608));
#246388=CARTESIAN_POINT('Ctrl Pts',(-4.53666578708917,-5.38008750043123,
47.5836019838938));
#246389=CARTESIAN_POINT('Ctrl Pts',(-1.41191065999068,-6.90983543585552,
47.7425563497185));
#246390=CARTESIAN_POINT('Ctrl Pts',(2.05555716365124,-6.7306318632831,47.9015107155433));
#246391=CARTESIAN_POINT('Ctrl Pts',(6.06446798360192,-4.33708996224195,
48.1134498699764));
#246392=CARTESIAN_POINT('Ctrl Pts',(7.43807033314036,0.5393566601956,48.3253890244092));
#246393=CARTESIAN_POINT('Ctrl Pts',(5.26278292242774,4.66154384421445,48.5373281788424));
#246394=CARTESIAN_POINT('Ctrl Pts',(1.45403116996541,7.30827249545264,48.7492673332753));
#246395=CARTESIAN_POINT('Ctrl Pts',(-4.84447950307468,6.3693497024098,49.0141912763167));
#246396=CARTESIAN_POINT('Ctrl Pts',(-7.96993110060059,-0.649856589424143,
49.3321000079661));
#246397=CARTESIAN_POINT('Ctrl Pts',(-4.4769579036553,-5.95683898660598,
49.5970239510075));
#246398=CARTESIAN_POINT('Ctrl Pts',(0.0523634526556974,-7.03732449478264,
49.8089631054405));
#246399=CARTESIAN_POINT('Ctrl Pts',(3.42095290591867,-6.16736561895647,
49.9679174712652));
#246400=CARTESIAN_POINT('Ctrl Pts',(5.9385416787833,-3.77630020806522,50.12687183709));
#246401=CARTESIAN_POINT('Ctrl Pts',(7.42744069663569,0.6490346390391,50.338810991523));
#246402=CARTESIAN_POINT('Ctrl Pts',(5.29971987330698,5.24678617366048,50.550750145956));
#246403=CARTESIAN_POINT('Ctrl Pts',(0.966521339459677,6.96367084234314,
50.762689300389));
#246404=CARTESIAN_POINT('Ctrl Pts',(-3.64806300079631,6.49743717578258,
50.974628454822));
#246405=CARTESIAN_POINT('Ctrl Pts',(-7.8222531166543,1.68818051946163,51.2395523978633));
#246406=CARTESIAN_POINT('Ctrl Pts',(-5.63189859724677,-5.67660404867808,
51.5574611295129));
#246407=CARTESIAN_POINT('Ctrl Pts',(0.472789098434964,-7.4366358826994,
51.822385072554));
#246408=CARTESIAN_POINT('Ctrl Pts',(4.61622353697344,-5.31198251434755,
52.0343242269871));
#246409=CARTESIAN_POINT('Ctrl Pts',(6.60949221452337,-2.46047355778412,
52.1932785928118));
#246410=CARTESIAN_POINT('Ctrl Pts',(6.96709106897004,0.993157877055618,
52.3522329586366));
#246411=CARTESIAN_POINT('Ctrl Pts',(5.22032015113918,5.32319253684505,52.5641721130696));
#246412=CARTESIAN_POINT('Ctrl Pts',(0.613992064454545,7.43228158995788,
52.7761112675027));
#246413=CARTESIAN_POINT('Ctrl Pts',(-3.7943109427795,5.91862142476055,52.9880504219356));
#246414=CARTESIAN_POINT('Ctrl Pts',(-6.99666957633073,2.56352654573113,
53.1999895763688));
#246415=CARTESIAN_POINT('Ctrl Pts',(-7.04016189133548,-3.80443396986798,
53.4649135194098));
#246416=CARTESIAN_POINT('Ctrl Pts',(-0.586822842256673,-7.97482001595928,
53.7828222510596));
#246417=CARTESIAN_POINT('Ctrl Pts',(5.19528404400013,-5.34191973784788,
54.0477461941006));
#246418=CARTESIAN_POINT('Ctrl Pts',(6.96123742617008,-1.03336899146948,
54.2596853485338));
#246419=CARTESIAN_POINT('Ctrl Pts',(6.62109554192712,2.42907622092694,54.4186397143584));
#246420=CARTESIAN_POINT('Ctrl Pts',(4.6468200682834,5.28524207440665,54.5775940801833));
#246421=CARTESIAN_POINT('Ctrl Pts',(0.503986736747804,7.43869065319261,
54.7895332346163));
#246422=CARTESIAN_POINT('Ctrl Pts',(-4.36685879143792,6.04535691115763,
55.0014723890493));
#246423=CARTESIAN_POINT('Ctrl Pts',(-6.73135970780785,2.02871180413373,
55.2134115434823));
#246424=CARTESIAN_POINT('Ctrl Pts',(-6.98223847753735,-2.60257552317263,
55.4253506979153));
#246425=CARTESIAN_POINT('Ctrl Pts',(-2.87412786071058,-7.46839918105518,
55.6902746409566));
#246426=CARTESIAN_POINT('Ctrl Pts',(4.74031672968744,-6.43983793564593,
56.0081833726062));
#246427=CARTESIAN_POINT('Ctrl Pts',(7.42060004203954,-0.679542345651922,
56.2731073156473));
#246428=CARTESIAN_POINT('Ctrl Pts',(5.96024455189898,3.7419463996161,56.4850464700805));
#246429=CARTESIAN_POINT('Ctrl Pts',(3.45018560213969,6.15105980894251,56.6440008359051));
#246430=CARTESIAN_POINT('Ctrl Pts',(0.0929962629414194,7.03690785978889,
56.80295520173));
#246431=CARTESIAN_POINT('Ctrl Pts',(-4.45459427338222,5.97868807718401,
57.0148943561628));
#246432=CARTESIAN_POINT('Ctrl Pts',(-7.24872376928388,1.75265501575725,
57.226833510596));
#246433=CARTESIAN_POINT('Ctrl Pts',(-6.43289534050361,-2.83632378938966,
57.438772665029));
#246434=CARTESIAN_POINT('Ctrl Pts',(-3.61170619446961,-6.51771676861232,
57.6507118194619));
#246435=CARTESIAN_POINT('Ctrl Pts',(2.67339205701473,-7.54258392043396,
57.9156357625032));
#246436=CARTESIAN_POINT('Ctrl Pts',(7.78896314481361,-1.80946634781474,
58.2335444941528));
#246437=CARTESIAN_POINT('Ctrl Pts',(6.07911082865066,4.30946566483981,58.498468437194));
#246438=CARTESIAN_POINT('Ctrl Pts',(2.09438479238119,6.71864795308429,58.7104075916271));
#246439=CARTESIAN_POINT('Ctrl Pts',(-1.37909965991125,6.91645874638408,
58.8693619574518));
#246440=CARTESIAN_POINT('Ctrl Pts',(-4.50552737171663,5.40619493126099,
59.0283163232766));
#246441=CARTESIAN_POINT('Ctrl Pts',(-7.2720182370356,1.64495350236227,59.2402554777095));
#246442=CARTESIAN_POINT('Ctrl Pts',(-6.64639803882978,-3.38248266766881,
59.4521946321427));
#246443=CARTESIAN_POINT('Ctrl Pts',(-3.04237851179562,-6.33804450056128,
59.6641337865756));
#246444=CARTESIAN_POINT('Ctrl Pts',(1.4948383252907,-7.30003506102965,59.8760729410086));
#246445=CARTESIAN_POINT('Ctrl Pts',(6.93591228911752,-3.99133035527843,
60.1409968840499));
#246446=CARTESIAN_POINT('Ctrl Pts',(7.09374596681339,3.69064811292774,60.4589056156994));
#246447=CARTESIAN_POINT('Ctrl Pts',(1.81562015154718,7.22707452907096,60.7238295587406));
#246448=CARTESIAN_POINT('Ctrl Pts',(-2.77816749198367,6.46594643981271,
60.9357687131737));
#246449=CARTESIAN_POINT('Ctrl Pts',(-5.5455032377072,4.35737435882887,61.0947230789984));
#246450=CARTESIAN_POINT('Ctrl Pts',(-6.93841232235609,1.17692607119428,
61.2536774448232));
#246451=CARTESIAN_POINT('Ctrl Pts',(-6.59405471200675,-3.47944876665455,
61.4656165992562));
#246452=CARTESIAN_POINT('Ctrl Pts',(-2.84939707620817,-6.89178730009399,
61.6775557536893));
#246453=CARTESIAN_POINT('Ctrl Pts',(1.81049600625463,-6.79330400552387,
61.8894949081222));
#246454=CARTESIAN_POINT('Ctrl Pts',(5.88286990826912,-4.57349922416107,
62.1014340625553));
#246455=CARTESIAN_POINT('Ctrl Pts',(7.86459860500312,1.47840659815924,62.3663580055965));
#246456=CARTESIAN_POINT('Ctrl Pts',(2.98883012029103,7.41680590599346,62.6842667372461));
#246457=CARTESIAN_POINT('Ctrl Pts',(-3.32057130201977,6.67089866597099,
62.9491906802873));
#246458=CARTESIAN_POINT('Ctrl Pts',(-6.31535845347854,3.10530603646705,
63.1611298347204));
#246459=CARTESIAN_POINT('Ctrl Pts',(-7.04639058552322,-0.296137094349907,
63.3200842005451));
#246460=CARTESIAN_POINT('Ctrl Pts',(-6.03626168420024,-3.61804718210473,
63.4790385663698));
#246461=CARTESIAN_POINT('Ctrl Pts',(-2.74657543650164,-6.93141000347823,
63.6909777208029));
#246462=CARTESIAN_POINT('Ctrl Pts',(2.31720260932942,-7.08846725004475,
63.9029168752358));
#246463=CARTESIAN_POINT('Ctrl Pts',(5.79313273304886,-3.98327606844028,
64.1148560296689));
#246464=CARTESIAN_POINT('Ctrl Pts',(7.44322570652722,0.351346826812141,
64.3267951841019));
#246465=CARTESIAN_POINT('Ctrl Pts',(5.01306618774103,6.23752873216845,64.5917191271432));
#246466=CARTESIAN_POINT('Ctrl Pts',(-2.55270470431066,7.57798218708196,
64.9096278587927));
#246467=CARTESIAN_POINT('Ctrl Pts',(-6.8606881850845,2.9082710345641,65.1745518018339));
#246468=CARTESIAN_POINT('Ctrl Pts',(-6.81699254406192,-1.74793896639902,
65.386490956267));
#246469=CARTESIAN_POINT('Ctrl Pts',(-5.16034122743529,-4.80730650976375,
65.5454453220917));
#246470=CARTESIAN_POINT('Ctrl Pts',(-2.232705565254,-6.67396032284963,65.7043996879165));
#246471=CARTESIAN_POINT('Ctrl Pts',(2.42108004106924,-7.05170140459022,
65.9163388423495));
#246472=CARTESIAN_POINT('Ctrl Pts',(6.3700095697273,-3.87798581341241,66.1282779967825));
#246473=CARTESIAN_POINT('Ctrl Pts',(6.99122698274514,0.74136386214266,66.3402171512155));
#246474=CARTESIAN_POINT('Ctrl Pts',(5.42590098168002,5.10731358423102,66.5521563056486));
#246475=CARTESIAN_POINT('Ctrl Pts',(-0.248059861002422,7.998503834619,66.8170802486897));
#246476=CARTESIAN_POINT('Ctrl Pts',(-6.86724974507664,4.09670553933687,
67.1349889803395));
#246477=CARTESIAN_POINT('Ctrl Pts',(-7.10312856817561,-2.2522538320855,
67.3999129233804));
#246478=CARTESIAN_POINT('Ctrl Pts',(-4.0419529974468,-5.76101500992519,
67.6118520778137));
#246479=CARTESIAN_POINT('Ctrl Pts',(-0.793908627573567,-7.00778328388534,
67.7708064436383));
#246480=CARTESIAN_POINT('Ctrl Pts',(2.64402870512488,-6.52195007099546,
67.9297608094632));
#246481=CARTESIAN_POINT('Ctrl Pts',(6.42501279597442,-3.78250338796736,
68.141699963896));
#246482=CARTESIAN_POINT('Ctrl Pts',(7.36099090340974,1.19649852563351,68.3536391183292));
#246483=CARTESIAN_POINT('Ctrl Pts',(4.82889961647785,5.10965787997891,68.5655782727621));
#246484=CARTESIAN_POINT('Ctrl Pts',(0.800548346787644,7.40838551015447,
68.7775174271952));
#246485=CARTESIAN_POINT('Ctrl Pts',(-5.38995276726831,5.91489695725373,
69.0424413702364));
#246486=CARTESIAN_POINT('Ctrl Pts',(-7.88096445044827,-1.3537044013919,
69.3603501018861));
#246487=CARTESIAN_POINT('Ctrl Pts',(-3.93136031333972,-6.33020444052113,
69.6252740449271));
#246488=CARTESIAN_POINT('Ctrl Pts',(0.675902207055709,-7.00498634360421,
69.8372131993604));
#246489=CARTESIAN_POINT('Ctrl Pts',(3.95412650214858,-5.83988048839313,
69.9961675651849));
#246490=CARTESIAN_POINT('Ctrl Pts',(6.24987657364358,-3.23508198497481,
70.1551219310099));
#246491=CARTESIAN_POINT('Ctrl Pts',(7.34068326321575,1.304802488117,70.3670610854427));
#246492=CARTESIAN_POINT('Ctrl Pts',(4.81381636314329,5.69587112126037,70.5790002398758));
#246493=CARTESIAN_POINT('Ctrl Pts',(0.345503588642198,7.02192978372834,
70.7909393943088));
#246494=CARTESIAN_POINT('Ctrl Pts',(-4.20960493843672,6.14852438048371,
71.0028785487418));
#246495=CARTESIAN_POINT('Ctrl Pts',(-7.94108190916835,0.988217775774724,
71.2678024917831));
#246496=CARTESIAN_POINT('Ctrl Pts',(-5.1066201271287,-6.15343513092807,
71.5857112234327));
#246497=CARTESIAN_POINT('Ctrl Pts',(1.13011026506829,-7.36546917451868,
71.8506351664738));
#246498=CARTESIAN_POINT('Ctrl Pts',(5.06881513876091,-4.88191287851589,
72.0625743209069));
#246499=CARTESIAN_POINT('Ctrl Pts',(6.80169453611394,-1.86498618130522,
72.2215286867317));
#246500=CARTESIAN_POINT('Ctrl Pts',(6.85139287777893,1.60680804324508,72.3804830525564));
#246501=CARTESIAN_POINT('Ctrl Pts',(4.72853054649915,5.76484981644271,72.5924222069894));
#246502=CARTESIAN_POINT('Ctrl Pts',(-0.0482709114308084,7.45762139668047,
72.8043613614224));
#246503=CARTESIAN_POINT('Ctrl Pts',(-4.30268773290715,5.55882356982419,
73.0163005158555));
#246504=CARTESIAN_POINT('Ctrl Pts',(-7.19933741305753,1.93376040999748,
73.2282396702885));
#246505=CARTESIAN_POINT('Ctrl Pts',(-6.66892985464963,-4.41442550065097,
73.4931636133297));
#246506=CARTESIAN_POINT('Ctrl Pts',(0.11140474583598,-7.99385296845655,
73.8110723449793));
#246507=CARTESIAN_POINT('Ctrl Pts',(6.77623611831373,-4.23606055317877,
74.1289810766287));
#246508=CARTESIAN_POINT('Ctrl Pts',(7.23272290008192,3.40636727273015,74.4468898082783));
#246509=CARTESIAN_POINT('Ctrl Pts',(1.05018349857864,7.92203885124593,74.7647985399278));
#246510=CARTESIAN_POINT('Ctrl Pts',(-6.09176467475394,5.17730619590121,
75.0827072715773));
#246511=CARTESIAN_POINT('Ctrl Pts',(-7.65077828618112,-2.32967154825181,
75.4006160032269));
#246512=CARTESIAN_POINT('Ctrl Pts',(-3.09458166954053,-6.78184730002577,
75.6655399462681));
#246513=CARTESIAN_POINT('Ctrl Pts',(1.54502232785923,-6.85759048163122,
75.8774791007012));
#246514=CARTESIAN_POINT('Ctrl Pts',(5.71857739349959,-4.7870992857546,76.0894182551341));
#246515=CARTESIAN_POINT('Ctrl Pts',(7.45599088236389,-0.0263533189910901,
76.3013574095672));
#246516=CARTESIAN_POINT('Ctrl Pts',(5.60250882051894,4.25855742822898,76.5132965640002));
#246517=CARTESIAN_POINT('Ctrl Pts',(2.89433645153631,6.43148804899533,76.6722509298249));
#246518=CARTESIAN_POINT('Ctrl Pts',(-0.535210393094977,7.01708700954135,
76.8312052956498));
#246519=CARTESIAN_POINT('Ctrl Pts',(-4.95849240896067,5.5624309795518,77.0431444500826));
#246520=CARTESIAN_POINT('Ctrl Pts',(-7.99637556395713,-0.0176316047177856,
77.3080683931241));
#246521=CARTESIAN_POINT('Ctrl Pts',(-4.29596078342121,-6.75145000779716,
77.6259771247734));
#246522=CARTESIAN_POINT('Ctrl Pts',(2.05892780076842,-7.16142039726313,
77.8909010678148));
#246523=CARTESIAN_POINT('Ctrl Pts',(5.63349027720521,-4.20602638056516,
78.1028402222478));
#246524=CARTESIAN_POINT('Ctrl Pts',(7.45713295591053,0.0833299822800066,
78.3147793766808));
#246525=CARTESIAN_POINT('Ctrl Pts',(5.68132030650631,4.82811970426699,78.5267185311138));
#246526=CARTESIAN_POINT('Ctrl Pts',(1.48662297777303,6.87871098079028,78.7386576855468));
#246527=CARTESIAN_POINT('Ctrl Pts',(-1.98370277785666,6.76788325865866,
78.8976120513716));
#246528=CARTESIAN_POINT('Ctrl Pts',(-4.96987733848888,4.98266963664653,
79.0565664171964));
#246529=CARTESIAN_POINT('Ctrl Pts',(-7.38410982404283,1.00100163764598,
79.2685055716293));
#246530=CARTESIAN_POINT('Ctrl Pts',(-6.06313463638398,-5.21349351746575,
79.5334295146707));
#246531=CARTESIAN_POINT('Ctrl Pts',(1.12703327978956,-7.92258750879785,
79.85133824632));
#246532=CARTESIAN_POINT('Ctrl Pts',(6.22124724940058,-4.1013578464256,80.1162621893616));
#246533=CARTESIAN_POINT('Ctrl Pts',(7.01480895542049,0.468327316524474,
80.3282013437944));
#246534=CARTESIAN_POINT('Ctrl Pts',(5.6107595536581,4.91275615443702,80.5401404982275));
#246535=CARTESIAN_POINT('Ctrl Pts',(1.1761453154345,7.3623911540614,80.7520796526603));
#246536=CARTESIAN_POINT('Ctrl Pts',(-3.34395584622964,6.19230811737825,
80.9640188070936));
#246537=CARTESIAN_POINT('Ctrl Pts',(-5.90818106404349,3.85132626212272,
81.1229731729182));
#246538=CARTESIAN_POINT('Ctrl Pts',(-7.01574160870034,0.553215742819636,
81.2819275387429));
#246539=CARTESIAN_POINT('Ctrl Pts',(-6.26043862608513,-4.04153324732057,
81.4938666931761));
#246540=CARTESIAN_POINT('Ctrl Pts',(-1.21558491778668,-7.90344663073891,
81.7587906362172));
#246541=CARTESIAN_POINT('Ctrl Pts',(6.0083122153089,-5.28562026733149,82.0766993678669));
#246542=CARTESIAN_POINT('Ctrl Pts',(7.39324196671269,0.930068133152367,
82.341623310908));
#246543=CARTESIAN_POINT('Ctrl Pts',(5.02437257694055,4.91757616193617,82.5535624653411));
#246544=CARTESIAN_POINT('Ctrl Pts',(1.06750233150316,7.38080176265968,82.7655016197742));
#246545=CARTESIAN_POINT('Ctrl Pts',(-3.89435810203002,6.35783738687267,
82.9774407742069));
#246546=CARTESIAN_POINT('Ctrl Pts',(-6.56722032392826,2.52949357561374,
83.1893799286403));
#246547=CARTESIAN_POINT('Ctrl Pts',(-6.9928172770757,-0.91641911362483,
83.3483342944647));
#246548=CARTESIAN_POINT('Ctrl Pts',(-5.68940106516124,-4.1421484154716,
83.5072886602898));
#246549=CARTESIAN_POINT('Ctrl Pts',(-2.1276084130189,-7.14145399931232,
83.7192278147225));
#246550=CARTESIAN_POINT('Ctrl Pts',(4.21625102576613,-6.7945082693943,83.984151757764));
#246551=CARTESIAN_POINT('Ctrl Pts',(8.00161995345922,-0.108052800533174,
84.3020604894134));
#246552=CARTESIAN_POINT('Ctrl Pts',(5.01158146891714,5.51444509369941,84.5669844324547));
#246553=CARTESIAN_POINT('Ctrl Pts',(0.618908011605294,7.00312986980119,
84.7789235868877));
#246554=CARTESIAN_POINT('Ctrl Pts',(-3.98886338328963,6.30117170033406,
84.9908627413207));
#246555=CARTESIAN_POINT('Ctrl Pts',(-7.09298906892491,2.29730871517607,
85.2028018957538));
#246556=CARTESIAN_POINT('Ctrl Pts',(-6.63386733968778,-2.34915402890138,
85.4147410501868));
#246557=CARTESIAN_POINT('Ctrl Pts',(-4.71626747173541,-5.24367605763847,
85.5736954160115));
#246558=CARTESIAN_POINT('Ctrl Pts',(-1.62837798208691,-6.84653657870138,
85.7326497818363));
#246559=CARTESIAN_POINT('Ctrl Pts',(3.02788367824696,-6.80874461369026,
85.9445889362693));
#246560=CARTESIAN_POINT('Ctrl Pts',(7.62149261754915,-2.41970362147575,
86.2095128793105));
#246561=CARTESIAN_POINT('Ctrl Pts',(6.14884791532884,5.1214516107696,86.5274216109601));
#246562=CARTESIAN_POINT('Ctrl Pts',(0.221040988410256,7.44823431374593,
86.7923455540014));
#246563=CARTESIAN_POINT('Ctrl Pts',(-4.08404251290028,5.72254068163378,
87.0042847084344));
#246564=CARTESIAN_POINT('Ctrl Pts',(-7.12793149107813,2.19280380931291,
87.2162238628674));
#246565=CARTESIAN_POINT('Ctrl Pts',(-6.88228517983163,-2.86745042994337,
87.4281630173003));
#246566=CARTESIAN_POINT('Ctrl Pts',(-3.51186216222031,-6.09865105458944,
87.6401021717336));
#246567=CARTESIAN_POINT('Ctrl Pts',(-0.172784089409316,-7.05049382106299,
87.799056537558));
#246568=CARTESIAN_POINT('Ctrl Pts',(3.21534556183627,-6.26005039069349,
87.9580109033831));
#246569=CARTESIAN_POINT('Ctrl Pts',(6.72798520514021,-3.20332606252702,
88.1699500578158));
#246570=CARTESIAN_POINT('Ctrl Pts',(7.36336744207196,3.1181621587359,88.4348740008574));
#246571=CARTESIAN_POINT('Ctrl Pts',(1.34055440124988,7.88926556686919,88.7527827325067));
#246572=CARTESIAN_POINT('Ctrl Pts',(-4.67574563727826,5.80193556035346,
89.017706675548));
#246573=CARTESIAN_POINT('Ctrl Pts',(-6.82394637862079,1.69133997819441,
89.229645829981));
#246574=CARTESIAN_POINT('Ctrl Pts',(-6.8408692259793,-2.9695629511241,89.4415849844141));
#246575=CARTESIAN_POINT('Ctrl Pts',(-3.3635239224812,-6.65393327946781,
89.653524138847));
#246576=CARTESIAN_POINT('Ctrl Pts',(1.29816395574534,-6.91675435996419,
89.8654632932801));
#246577=CARTESIAN_POINT('Ctrl Pts',(4.45375014959483,-5.46840260655559,
90.0244176591047));
#246578=CARTESIAN_POINT('Ctrl Pts',(6.51357261739879,-2.66459185128115,
90.1833720249296));
#246579=CARTESIAN_POINT('Ctrl Pts',(7.19419559706401,1.94181165271923,90.3953111793625));
#246580=CARTESIAN_POINT('Ctrl Pts',(3.56594662779852,7.15724388174885,90.6602351224039));
#246581=CARTESIAN_POINT('Ctrl Pts',(-4.11209353127135,6.86500430279352,
90.9781438540534));
#246582=CARTESIAN_POINT('Ctrl Pts',(-7.32507601793611,1.36686313962944,
91.2430677970946));
#246583=CARTESIAN_POINT('Ctrl Pts',(-6.28383415832657,-3.1528246654039,
91.4550069515277));
#246584=CARTESIAN_POINT('Ctrl Pts',(-3.26565669436706,-6.70457174189187,
91.6669461059606));
#246585=CARTESIAN_POINT('Ctrl Pts',(1.77195762534478,-7.24211898816184,
91.8788852603937));
#246586=CARTESIAN_POINT('Ctrl Pts',(5.48421115874337,-4.41023224993819,
92.0908244148267));
#246587=CARTESIAN_POINT('Ctrl Pts',(6.93953308089106,-1.25785455503364,
92.2497787806513));
#246588=CARTESIAN_POINT('Ctrl Pts',(6.68096865860481,2.21163644362759,92.4087331464764));
#246589=CARTESIAN_POINT('Ctrl Pts',(4.20242493593684,6.15359305132114,92.6206723009091));
#246590=CARTESIAN_POINT('Ctrl Pts',(-1.94549150901639,7.75610586077085,
92.8855962439505));
#246591=CARTESIAN_POINT('Ctrl Pts',(-7.58821172844422,2.54099194245058,
93.2035049756));
#246592=CARTESIAN_POINT('Ctrl Pts',(-6.45351601683708,-3.72520932719855,
93.4684289186413));
#246593=CARTESIAN_POINT('Ctrl Pts',(-2.72331761807264,-6.48154427981681,
93.6803680730743));
#246594=CARTESIAN_POINT('Ctrl Pts',(1.87923500742207,-7.21694337476191,
93.8923072275072));
#246595=CARTESIAN_POINT('Ctrl Pts',(6.05572534184949,-4.34928866009077,
94.1042463819404));
#246596=CARTESIAN_POINT('Ctrl Pts',(7.03420294428734,0.216123739231432,
94.3161855363733));
#246597=CARTESIAN_POINT('Ctrl Pts',(6.08974171663501,3.557297188467,94.4751399021981));
#246598=CARTESIAN_POINT('Ctrl Pts',(3.63707266225326,6.02481372538034,94.6340942680227));
#246599=CARTESIAN_POINT('Ctrl Pts',(-0.809294392038973,7.4075721643778,
94.8460334224561));
#246600=CARTESIAN_POINT('Ctrl Pts',(-6.52180455974154,4.62689751557925,
95.110957365497));
#246601=CARTESIAN_POINT('Ctrl Pts',(-7.41696003839753,-3.00438031482576,
95.4288660971467));
#246602=CARTESIAN_POINT('Ctrl Pts',(-2.47999196559578,-7.02671284183443,
95.693790040188));
#246603=CARTESIAN_POINT('Ctrl Pts',(2.14619595981811,-6.69482770519087,
95.905729194621));
#246604=CARTESIAN_POINT('Ctrl Pts',(6.12084864813841,-4.26039994768352,
96.117668349054));
#246605=CARTESIAN_POINT('Ctrl Pts',(7.42873212447804,0.634082240296726,
96.329607503487));
#246606=CARTESIAN_POINT('Ctrl Pts',(5.20311616774883,4.73859712119429,96.54154665792));
#246607=CARTESIAN_POINT('Ctrl Pts',(2.3128390179733,6.66258907177538,96.7005010237446));
#246608=CARTESIAN_POINT('Ctrl Pts',(-1.15502828417975,6.94208813245597,
96.8594553895697));
#246609=CARTESIAN_POINT('Ctrl Pts',(-5.43201614047265,5.10100808008528,
97.0713945440023));
#246610=CARTESIAN_POINT('Ctrl Pts',(-7.96332980896591,-0.726287607476431,
97.336318487044));
#246611=CARTESIAN_POINT('Ctrl Pts',(-3.68065275068506,-7.10565919645552,
97.6542272186931));
#246612=CARTESIAN_POINT('Ctrl Pts',(2.68557157262411,-6.95073800681144,
97.9191511617346));
#246613=CARTESIAN_POINT('Ctrl Pts',(5.98411332030606,-3.69015756707848,
98.1310903161675));
#246614=CARTESIAN_POINT('Ctrl Pts',(7.42039901460989,0.743958568481396,
98.3430294706007));
#246615=CARTESIAN_POINT('Ctrl Pts',(5.23102490745951,5.31267349667283,98.5549686250335));
#246616=CARTESIAN_POINT('Ctrl Pts',(0.871085834401703,6.98340389789852,
98.7669077794666));
#246617=CARTESIAN_POINT('Ctrl Pts',(-2.57575899047016,6.56542329826589,
98.9258621452915));
#246618=CARTESIAN_POINT('Ctrl Pts',(-5.39195028551125,4.52256012614725,
99.0848165111161));
#246619=CARTESIAN_POINT('Ctrl Pts',(-7.44377066676299,0.342579982032306,
99.2967556655493));
#246620=CARTESIAN_POINT('Ctrl Pts',(-5.57717992383078,-5.73037341124973,
99.5616796085902));
#246621=CARTESIAN_POINT('Ctrl Pts',(1.82480680749437,-7.79151316514454,
99.8795883402401));
#246622=CARTESIAN_POINT('Ctrl Pts',(6.56028118708693,-3.53380308695505,
100.144512283282));
#246623=CARTESIAN_POINT('Ctrl Pts',(6.94569097029563,1.08823345164734,100.356451437714));
#246624=CARTESIAN_POINT('Ctrl Pts',(5.15324079602841,5.39072399458448,100.568390592148));
#246625=CARTESIAN_POINT('Ctrl Pts',(0.518959445105794,7.43766108121687,
100.780329746581));
#246626=CARTESIAN_POINT('Ctrl Pts',(-3.87964291634347,5.87154931630021,
100.992268901014));
#246627=CARTESIAN_POINT('Ctrl Pts',(-6.22628588087141,3.31250382521457,
101.151223266838));
#246628=CARTESIAN_POINT('Ctrl Pts',(-7.03716322434527,-0.0707935729022975,
101.310177632663));
#246629=CARTESIAN_POINT('Ctrl Pts',(-5.87758272796004,-4.58051351481871,
101.522116787096));
#246630=CARTESIAN_POINT('Ctrl Pts',(-0.510288009116391,-7.98008279925033,
101.787040730138));
#246631=CARTESIAN_POINT('Ctrl Pts',(6.45314990690399,-4.73227784120117,
102.104949461787));
#246632=CARTESIAN_POINT('Ctrl Pts',(7.28170872274559,1.58169895622098,102.369873404829));
#246633=CARTESIAN_POINT('Ctrl Pts',(4.56873445735095,5.34355130585872,102.58181255926));
#246634=CARTESIAN_POINT('Ctrl Pts',(0.409112248512814,7.44636979042522,
102.793751713695));
#246635=CARTESIAN_POINT('Ctrl Pts',(-4.44255043452387,5.98764285018941,
103.005690868127));
#246636=CARTESIAN_POINT('Ctrl Pts',(-6.76557225813255,1.93746033561121,
103.21763002256));
#246637=CARTESIAN_POINT('Ctrl Pts',(-6.88406975831953,-1.53261248363403,
103.376584388385));
#246638=CARTESIAN_POINT('Ctrl Pts',(-5.29987470506708,-4.63011944625967,
103.535538754209));
#246639=CARTESIAN_POINT('Ctrl Pts',(-1.48626035448566,-7.30192529009538,
103.747477908643));
#246640=CARTESIAN_POINT('Ctrl Pts',(4.80188028755272,-6.39406451634251,
104.012401851684));
#246641=CARTESIAN_POINT('Ctrl Pts',(7.97970493153861,0.60158664619224,104.330310583333));
#246642=CARTESIAN_POINT('Ctrl Pts',(4.50309091527155,5.93693740238345,104.595234526375));
#246643=CARTESIAN_POINT('Ctrl Pts',(-0.00424202430133235,7.03042367893717,
104.807173680808));
#246644=CARTESIAN_POINT('Ctrl Pts',(-4.53166127269599,5.92282381952964,
105.019112835241));
#246645=CARTESIAN_POINT('Ctrl Pts',(-7.26869229106604,1.65958839550948,
105.231051989674));
#246646=CARTESIAN_POINT('Ctrl Pts',(-6.39954377280644,-2.927893446151,105.442991144107));
#246647=CARTESIAN_POINT('Ctrl Pts',(-4.23293848730191,-5.64105922900283,
105.601945509932));
#246648=CARTESIAN_POINT('Ctrl Pts',(-1.0151344149273,-6.96391988004401,
105.760899875757));
#246649=CARTESIAN_POINT('Ctrl Pts',(3.61945184567181,-6.51357437359197,
105.97283903019));
#246650=CARTESIAN_POINT('Ctrl Pts',(7.80596412511259,-1.73465829851099,
106.237762973231));
#246651=CARTESIAN_POINT('Ctrl Pts',(5.67071391215704,5.64629090764611,106.555671704879));
#246652=CARTESIAN_POINT('Ctrl Pts',(-0.43999446263257,7.43851183933139,
106.820595647922));
#246653=CARTESIAN_POINT('Ctrl Pts',(-4.57517952335123,5.33803404159604,
107.032534802355));
#246654=CARTESIAN_POINT('Ctrl Pts',(-7.2942345200308,1.55239771142301,107.244473956788));
#246655=CARTESIAN_POINT('Ctrl Pts',(-6.60104531689834,-3.46616819975131,
107.456413111221));
#246656=CARTESIAN_POINT('Ctrl Pts',(-2.95749367867577,-6.38591823253887,
107.668352265654));
#246657=CARTESIAN_POINT('Ctrl Pts',(0.45280817473929,-7.03805954928553,
107.827306631479));
#246658=CARTESIAN_POINT('Ctrl Pts',(3.75754306370802,-5.9504241949983,107.986260997303));
#246659=CARTESIAN_POINT('Ctrl Pts',(6.98542876397639,-2.59439159859546,
108.198200151736));
#246660=CARTESIAN_POINT('Ctrl Pts',(7.05801263346198,3.75853335771147,108.463124094776));
#246661=CARTESIAN_POINT('Ctrl Pts',(0.636022569376616,7.977034071542,108.781032826427));
#246662=CARTESIAN_POINT('Ctrl Pts',(-5.17159094025551,5.36467153306593,
109.045956769468));
#246663=CARTESIAN_POINT('Ctrl Pts',(-6.94699915125064,1.07985086593164,
109.257895923901));
#246664=CARTESIAN_POINT('Ctrl Pts',(-6.5507417414334,-3.56420797999802,
109.469835078334));
#246665=CARTESIAN_POINT('Ctrl Pts',(-2.76052246964758,-6.92586723517592,
109.681774232767));
#246666=CARTESIAN_POINT('Ctrl Pts',(1.90611313675836,-6.77447069828759,
109.8937133872));
#246667=CARTESIAN_POINT('Ctrl Pts',(4.92090686380152,-5.05212758154333,
110.052667753025));
#246668=CARTESIAN_POINT('Ctrl Pts',(6.72410997097836,-2.07678190338583,
110.21162211885));
#246669=CARTESIAN_POINT('Ctrl Pts',(6.99377104650249,2.57181829306715,110.423561273283));
#246670=CARTESIAN_POINT('Ctrl Pts',(2.91753815165707,7.44513844523824,110.688485216324));
#246671=CARTESIAN_POINT('Ctrl Pts',(-4.70438106111458,6.47351497404037,
111.006393947974));
#246672=CARTESIAN_POINT('Ctrl Pts',(-7.41739686016381,0.712234041486918,
111.271317891015));
#246673=CARTESIAN_POINT('Ctrl Pts',(-5.97965582250344,-3.69737627846169,
111.483257045448));
#246674=CARTESIAN_POINT('Ctrl Pts',(-2.6585521391701,-6.96763205192077,
111.695196199881));
#246675=CARTESIAN_POINT('Ctrl Pts',(2.40688039744279,-7.05656063653657,
111.907135354314));
#246676=CARTESIAN_POINT('Ctrl Pts',(5.85352257849701,-3.90678818917865,
112.119074508747));
#246677=CARTESIAN_POINT('Ctrl Pts',(7.0237094653069,-0.637826629546366,
112.278028874572));
#246678=CARTESIAN_POINT('Ctrl Pts',(6.45864842356448,2.79509186196614,112.436983240397));
#246679=CARTESIAN_POINT('Ctrl Pts',(3.64046886970194,6.50185121270724,112.648922394829));
#246680=CARTESIAN_POINT('Ctrl Pts',(-2.62528792232601,7.55314362765783,
112.913846337871));
#246681=CARTESIAN_POINT('Ctrl Pts',(-7.78356446813755,1.85841907481702,
113.23175506952));
#246682=CARTESIAN_POINT('Ctrl Pts',(-6.09793721850281,-4.28254774523508,
113.496679012562));
#246683=CARTESIAN_POINT('Ctrl Pts',(-2.13811533592251,-6.6974127773659,
113.708618166994));
#246684=CARTESIAN_POINT('Ctrl Pts',(2.51150415461734,-7.02197570267657,
113.920557321428));
#246685=CARTESIAN_POINT('Ctrl Pts',(6.41738577696525,-3.79542896841933,
114.132496475861));
#246686=CARTESIAN_POINT('Ctrl Pts',(6.9873624005399,0.83874144740873,114.344435630294));
#246687=CARTESIAN_POINT('Ctrl Pts',(5.75047732804611,4.08305375448665,114.503389996118));
#246688=CARTESIAN_POINT('Ctrl Pts',(3.0887558698379,6.32346939208084,114.662344361943));
#246689=CARTESIAN_POINT('Ctrl Pts',(-1.46267068722058,7.30668715932174,
114.874283516376));
#246690=CARTESIAN_POINT('Ctrl Pts',(-6.90623617109233,4.03063484878436,
115.139207459416));
#246691=CARTESIAN_POINT('Ctrl Pts',(-7.12147922422141,-3.64994944434576,
115.457116191067));
#246692=CARTESIAN_POINT('Ctrl Pts',(-1.84742697086673,-7.21886882401493,
115.722040134108));
#246693=CARTESIAN_POINT('Ctrl Pts',(2.73113731404155,-6.47825316516581,
115.933979288542));
#246694=CARTESIAN_POINT('Ctrl Pts',(6.47437422943836,-3.70111796959026,
116.145918442974));
#246695=CARTESIAN_POINT('Ctrl Pts',(7.3432935628495,1.29002361006491,116.357857597407));
#246696=CARTESIAN_POINT('Ctrl Pts',(4.76263815994754,5.18111940506021,116.56979675184));
#246697=CARTESIAN_POINT('Ctrl Pts',(1.71320557327797,6.84136273896434,116.728751117665));
#246698=CARTESIAN_POINT('Ctrl Pts',(-1.76578623661401,6.81239142611651,
116.88770548349));
#246699=CARTESIAN_POINT('Ctrl Pts',(-5.86275908921941,4.59947156151941,
117.099644637923));
#246700=CARTESIAN_POINT('Ctrl Pts',(-7.86761470489579,-1.42924952000916,
117.364568580964));
#246701=CARTESIAN_POINT('Ctrl Pts',(-3.03636497104356,-7.4039236253434,
117.682477312614));
#246702=CARTESIAN_POINT('Ctrl Pts',(3.2910724029975,-6.68534935132399,117.947401255655));
#246703=CARTESIAN_POINT('Ctrl Pts',(6.28763429065526,-3.14523927978571,
118.159340410088));
#246704=CARTESIAN_POINT('Ctrl Pts',(7.32525449056893,1.39872890012328,118.371279564521));
#246705=CARTESIAN_POINT('Ctrl Pts',(4.73955447373246,5.75541003363227,118.583218718954));
#246706=CARTESIAN_POINT('Ctrl Pts',(0.248691684925148,7.03312682794283,
118.795157873387));
#246707=CARTESIAN_POINT('Ctrl Pts',(-3.14754009632173,6.31128424367394,
118.954112239212));
#246708=CARTESIAN_POINT('Ctrl Pts',(-5.77158086774825,4.02685140812069,
119.113066605036));
#246709=CARTESIAN_POINT('Ctrl Pts',(-7.44483822588827,-0.318538182646105,
119.32500575947));
#246710=CARTESIAN_POINT('Ctrl Pts',(-5.04732477901245,-6.2021470403648,
119.589929702511));
#246711=CARTESIAN_POINT('Ctrl Pts',(2.50821648709916,-7.5991083253986,119.90783843416));
#246712=CARTESIAN_POINT('Ctrl Pts',(6.84767622506058,-2.93843220574519,
120.172762377201));
#246713=CARTESIAN_POINT('Ctrl Pts',(6.82190036566931,1.69957362329846,120.384701531635));
#246714=CARTESIAN_POINT('Ctrl Pts',(4.65515858481535,5.82625904314762,120.596640686067));
#246715=CARTESIAN_POINT('Ctrl Pts',(-0.142311384242204,7.45438587239934,
120.8085798405));
#246716=CARTESIAN_POINT('Ctrl Pts',(-4.3847915920812,5.50457293766677,121.020518994933));
#246717=CARTESIAN_POINT('Ctrl Pts',(-6.4953808316654,2.74760719791489,121.179473360757));
#246718=CARTESIAN_POINT('Ctrl Pts',(-7.00319219825473,-0.694245641214978,
121.338427726583));
#246719=CARTESIAN_POINT('Ctrl Pts',(-5.44846176167561,-5.08343852279241,
121.550366881016));
#246720=CARTESIAN_POINT('Ctrl Pts',(0.199025603378755,-7.99390418658736,
121.815290824057));
#246721=CARTESIAN_POINT('Ctrl Pts',(6.84719198522617,-4.1416855511679,122.133199555707));
#246722=CARTESIAN_POINT('Ctrl Pts',(7.11285791045668,2.22087952322351,122.398123498748));
#246723=CARTESIAN_POINT('Ctrl Pts',(4.07713379665675,5.72746498062536,122.610062653181));
#246724=CARTESIAN_POINT('Ctrl Pts',(-0.252498138968556,7.45332412937059,
122.822001807614));
#246725=CARTESIAN_POINT('Ctrl Pts',(-4.9557734764722,5.570316913301,123.033940962047));
#246726=CARTESIAN_POINT('Ctrl Pts',(-6.91066936372984,1.3301764835109,123.245880116479));
#246727=CARTESIAN_POINT('Ctrl Pts',(-6.72113466442141,-2.13674197906841,
123.404834482305));
#246728=CARTESIAN_POINT('Ctrl Pts',(-4.86863067375534,-5.08164474738352,
123.56378884813));
#246729=CARTESIAN_POINT('Ctrl Pts',(-0.833213279604876,-7.40491987898185,
123.775728002563));
#246730=CARTESIAN_POINT('Ctrl Pts',(5.3497118136926,-5.94329023736657,124.040651945604));
#246731=CARTESIAN_POINT('Ctrl Pts',(7.89497810268386,1.30649073683698,124.358560677254));
#246732=CARTESIAN_POINT('Ctrl Pts',(3.95915453003105,6.31269743598997,124.623484620295));
#246733=CARTESIAN_POINT('Ctrl Pts',(-0.627358669347987,7.00237789612389,
124.835423774728));
#246734=CARTESIAN_POINT('Ctrl Pts',(-5.0387884405164,5.49785475793592,125.04736292916));
#246735=CARTESIAN_POINT('Ctrl Pts',(-7.38718040302859,1.00880471738742,
125.259302083594));
#246736=CARTESIAN_POINT('Ctrl Pts',(-6.11484655033592,-3.48358611174239,
125.471241238027));
#246737=CARTESIAN_POINT('Ctrl Pts',(-3.71629016119966,-5.9940391140007,
125.630195603852));
#246738=CARTESIAN_POINT('Ctrl Pts',(-0.393900273250039,-7.02648707041972,
125.789149969676));
#246739=CARTESIAN_POINT('Ctrl Pts',(4.18252969766674,-6.16713289232418,
126.001089124109));
#246740=CARTESIAN_POINT('Ctrl Pts',(7.92899141691023,-1.03595870849268,
126.266013067151));
#246741=CARTESIAN_POINT('Ctrl Pts',(5.14794319741676,6.12668573728643,126.5839217988));
#246742=CARTESIAN_POINT('Ctrl Pts',(-1.09756652154811,7.37023752953711,
126.848845741841));
#246743=CARTESIAN_POINT('Ctrl Pts',(-5.03030326070806,4.91150936122904,
127.060784896274));
#246744=CARTESIAN_POINT('Ctrl Pts',(-7.40312138455938,0.899772000631177,
127.272724050707));
#246745=CARTESIAN_POINT('Ctrl Pts',(-6.2678456900933,-4.03760221788769,
127.484663205141));
#246746=CARTESIAN_POINT('Ctrl Pts',(-2.3798454468764,-6.62291900758731,
127.696602359573));
#246747=CARTESIAN_POINT('Ctrl Pts',(1.07483618433314,-6.97022558022683,
127.855556725398));
#246748=CARTESIAN_POINT('Ctrl Pts',(4.27016327274933,-5.59395956368158,
128.014511091223));
#246749=CARTESIAN_POINT('Ctrl Pts',(7.18788690585305,-1.96503552439061,
128.226450245656));
#246750=CARTESIAN_POINT('Ctrl Pts',(6.69710106796964,4.36931946881163,128.491374188697));
#246751=CARTESIAN_POINT('Ctrl Pts',(-0.0735156790465368,8.00201179280775,
128.809282920347));
#246752=CARTESIAN_POINT('Ctrl Pts',(-5.6267283505892,4.88517978990507,129.074206863388));
#246753=CARTESIAN_POINT('Ctrl Pts',(-7.01536900349605,0.459861767179577,
129.28614601782));
#246754=CARTESIAN_POINT('Ctrl Pts',(-6.20905045483426,-4.13079754248224,
129.498085172254));
#246755=CARTESIAN_POINT('Ctrl Pts',(-2.13579171655767,-7.14328460920958,
129.710024326687));
#246756=CARTESIAN_POINT('Ctrl Pts',(2.49905845342029,-6.57886216442336,
129.92196348112));
#246757=CARTESIAN_POINT('Ctrl Pts',(5.34932893123977,-4.59608501311821,
130.080917846945));
#246758=CARTESIAN_POINT('Ctrl Pts',(6.88171886404708,-1.47262468137094,
130.23987221277));
#246759=CARTESIAN_POINT('Ctrl Pts',(6.73829541317992,3.18158100768473,130.451811367203));
#246760=CARTESIAN_POINT('Ctrl Pts',(2.24616443495528,7.67442901235677,130.716735310244));
#246761=CARTESIAN_POINT('Ctrl Pts',(-5.25963831503589,6.03106972952018,
131.034644041893));
#246762=CARTESIAN_POINT('Ctrl Pts',(-7.45133207249597,0.0519986323146828,
131.299567984935));
#246763=CARTESIAN_POINT('Ctrl Pts',(-5.62840895579532,-4.21282419810638,
131.511507139368));
#246764=CARTESIAN_POINT('Ctrl Pts',(-2.03052093785896,-7.17584703111325,
131.723446293801));
#246765=CARTESIAN_POINT('Ctrl Pts',(3.02285754397351,-6.81545695676022,
131.935385448233));
#246766=CARTESIAN_POINT('Ctrl Pts',(6.17675831757049,-3.37259206154052,
132.147324602667));
#246767=CARTESIAN_POINT('Ctrl Pts',(7.0525991099684,-0.0127780854508224,
132.306278968491));
#246768=CARTESIAN_POINT('Ctrl Pts',(6.18548929096036,3.35654586625373,132.465233334316));
#246769=CARTESIAN_POINT('Ctrl Pts',(3.04985706012767,6.79893041704212,132.677172488749));
#246770=CARTESIAN_POINT('Ctrl Pts',(-3.28441953996838,7.29072722915634,
132.942096431791));
#246771=CARTESIAN_POINT('Ctrl Pts',(-7.91764928647446,1.16121778534561,
133.26000516344));
#246772=CARTESIAN_POINT('Ctrl Pts',(-5.69435888292606,-4.80617636085127,
133.524929106481));
#246773=CARTESIAN_POINT('Ctrl Pts',(-1.53608294498999,-6.86056291225426,
133.736868260914));
#246774=CARTESIAN_POINT('Ctrl Pts',(3.12400400176437,-6.77173505910424,
133.948807415348));
#246775=CARTESIAN_POINT('Ctrl Pts',(6.7285323860292,-3.21169351765348,134.16074656978));
#246776=CARTESIAN_POINT('Ctrl Pts',(6.88552088334561,1.45475674032299,134.372685724214));
#246777=CARTESIAN_POINT('Ctrl Pts',(5.36594907368235,4.57667142967609,134.531640090038));
#246778=CARTESIAN_POINT('Ctrl Pts',(2.51612483089831,6.57234904851573,134.690594455863));
#246779=CARTESIAN_POINT('Ctrl Pts',(-2.10453089563916,7.14829049743629,
134.902533610296));
#246780=CARTESIAN_POINT('Ctrl Pts',(-7.23631142511329,3.4026400329894,135.167457553337));
#246781=CARTESIAN_POINT('Ctrl Pts',(-6.76993212346154,-4.26677906377091,
135.485366284987));
#246782=CARTESIAN_POINT('Ctrl Pts',(-1.20033675469971,-7.35421719897996,
135.750290228028));
#246783=CARTESIAN_POINT('Ctrl Pts',(3.29460290356249,-6.21066501528404,
135.962229382461));
#246784=CARTESIAN_POINT('Ctrl Pts',(6.77687988267027,-3.11275537092704,
136.174168536894));
#246785=CARTESIAN_POINT('Ctrl Pts',(7.20016907646936,1.93591743114999,136.386107691327));
#246786=CARTESIAN_POINT('Ctrl Pts',(4.28452746621314,5.58272681899942,136.59804684576));
#246787=CARTESIAN_POINT('Ctrl Pts',(1.10038604404414,6.96655961965286,136.757001211585));
#246788=CARTESIAN_POINT('Ctrl Pts',(-2.36319085294511,6.62857044855553,
136.91595557741));
#246789=CARTESIAN_POINT('Ctrl Pts',(-6.24617402102025,4.06281286418076,
137.127894731842));
#246790=CARTESIAN_POINT('Ctrl Pts',(-7.71241073412867,-2.12320047247547,
137.392818674884));
#246791=CARTESIAN_POINT('Ctrl Pts',(-2.36391126028145,-7.63999480400491,
137.710727406533));
#246792=CARTESIAN_POINT('Ctrl Pts',(3.86350032495916,-6.37391496262723,
137.975651349575));
#246793=CARTESIAN_POINT('Ctrl Pts',(6.55130607618235,-2.56670467838789,
138.187590504008));
#246794=CARTESIAN_POINT('Ctrl Pts',(6.99717060324046,0.871685760892387,
138.346544869832));
#246795=CARTESIAN_POINT('Ctrl Pts',(5.71527044315637,4.1246109195803,138.505564005226));
#246796=CARTESIAN_POINT('Ctrl Pts',(3.93551302891977,5.61075906984116,138.611598352013));
#246797=CARTESIAN_POINT('Ctrl Pts',(2.91932841735868,6.09728744058681,138.66464791019));
#246798=CARTESIAN_POINT('Ctrl Pts',(3.93307528793212,-5.51266228421277,
138.));
#246799=CARTESIAN_POINT('Ctrl Pts',(4.08486176364148,-5.42349325184365,
138.));
#246800=CARTESIAN_POINT('Ctrl Pts',(4.2326846053822,-5.3283456569208,138.));
#246801=CARTESIAN_POINT('Ctrl Pts',(4.37614884579843,-5.22732383700901,
138.));
#246802=CARTESIAN_POINT('Ctrl Pts',(4.52391818469271,-5.12327053774114,
138.));
#246803=CARTESIAN_POINT('Ctrl Pts',(4.66706455466681,-5.01298603196517,
138.));
#246804=CARTESIAN_POINT('Ctrl Pts',(4.80542684321419,-4.89696515575036,
138.));
#246805=CARTESIAN_POINT('Ctrl Pts',(4.94590248835348,-4.77917216745124,
138.));
#246806=CARTESIAN_POINT('Ctrl Pts',(5.08144724969525,-4.6554658264225,138.));
#246807=CARTESIAN_POINT('Ctrl Pts',(5.21187009830291,-4.52631398537958,
138.));
#246808=CARTESIAN_POINT('Ctrl Pts',(5.34430862911351,-4.39516610552716,
138.));
#246809=CARTESIAN_POINT('Ctrl Pts',(5.47146622839557,-4.25840263867453,
138.));
#246810=CARTESIAN_POINT('Ctrl Pts',(5.59311244077779,-4.11646896172721,
138.));
#246811=CARTESIAN_POINT('Ctrl Pts',(5.69160061880562,-4.0015554846071,138.));
#246812=CARTESIAN_POINT('Ctrl Pts',(5.78647562580018,-3.8832519703199,138.));
#246813=CARTESIAN_POINT('Ctrl Pts',(5.87759730129057,-3.76177727698624,
138.));
#246814=CARTESIAN_POINT('Ctrl Pts',(5.89385220890071,-3.74010779048387,
138.));
#246815=CARTESIAN_POINT('Ctrl Pts',(5.90998883697244,-3.71833560735108,
138.));
#246816=CARTESIAN_POINT('Ctrl Pts',(5.92599314981512,-3.69648023992614,
138.));
#246817=CARTESIAN_POINT('Ctrl Pts',(6.03816674779205,-3.54329683097485,
138.));
#246818=CARTESIAN_POINT('Ctrl Pts',(6.14398755043199,-3.38583986628415,
138.));
#246819=CARTESIAN_POINT('Ctrl Pts',(6.24327612830652,-3.22462877876666,
138.));
#246820=CARTESIAN_POINT('Ctrl Pts',(6.34256470618104,-3.06341769124917,
138.));
#246821=CARTESIAN_POINT('Ctrl Pts',(6.43532148595384,-2.89845187871061,
138.));
#246822=CARTESIAN_POINT('Ctrl Pts',(6.52133729465314,-2.73020783048089,
138.));
#246823=CARTESIAN_POINT('Ctrl Pts',(6.54540235632602,-2.68313737380591,
138.));
#246824=CARTESIAN_POINT('Ctrl Pts',(6.56893957507926,-2.63581008860474,
138.));
#246825=CARTESIAN_POINT('Ctrl Pts',(6.59194388268069,-2.58823590697392,
138.));
#246826=CARTESIAN_POINT('Ctrl Pts',(6.67513605841707,-2.4161898820591,138.));
#246827=CARTESIAN_POINT('Ctrl Pts',(6.75136213437869,-2.24091709476537,
138.));
#246828=CARTESIAN_POINT('Ctrl Pts',(6.82055045941942,-2.06283511800934,
138.));
#246829=CARTESIAN_POINT('Ctrl Pts',(6.88991117243377,-1.88430943646505,
138.));
#246830=CARTESIAN_POINT('Ctrl Pts',(6.95219929984553,-1.7029599431334,138.));
#246831=CARTESIAN_POINT('Ctrl Pts',(7.00729619903557,-1.51918376131994,
138.));
#246832=CARTESIAN_POINT('Ctrl Pts',(7.02222200681774,-1.46939860090232,
138.));
#246833=CARTESIAN_POINT('Ctrl Pts',(7.03661979311897,-1.41943524787105,
138.));
#246834=CARTESIAN_POINT('Ctrl Pts',(7.05048657229512,-1.36930139115022,
138.));
#246835=CARTESIAN_POINT('Ctrl Pts',(7.05874094265755,-1.33945859811108,
138.));
#246836=CARTESIAN_POINT('Ctrl Pts',(7.06680715224607,-1.30955538787954,
138.));
#246837=CARTESIAN_POINT('Ctrl Pts',(7.07468452464019,-1.27959337136282,
138.));
#246838=CARTESIAN_POINT('Ctrl Pts',(7.08043946017635,-1.25770415945831,
138.));
#246839=CARTESIAN_POINT('Ctrl Pts',(7.08609267172794,-1.23578700025731,
138.));
#246840=CARTESIAN_POINT('Ctrl Pts',(7.09164164408561,-1.21385215425006,
138.));
#246841=CARTESIAN_POINT('Ctrl Pts',(7.13960279074919,-1.02426383075656,
138.));
#246842=CARTESIAN_POINT('Ctrl Pts',(7.17983529772245,-0.833148244170129,
138.));
#246843=CARTESIAN_POINT('Ctrl Pts',(7.21231481660431,-0.640965875669055,
138.));
#246844=CARTESIAN_POINT('Ctrl Pts',(7.2449502246749,-0.447861105773331,
138.));
#246845=CARTESIAN_POINT('Ctrl Pts',(7.26975831462569,-0.253678666482718,
138.));
#246846=CARTESIAN_POINT('Ctrl Pts',(7.28666906892299,-0.0588585281659345,
138.));
#246847=CARTESIAN_POINT('Ctrl Pts',(7.30350913847585,0.135147287415994,
138.));
#246848=CARTESIAN_POINT('Ctrl Pts',(7.31251796317501,0.329786136287213,
138.));
#246849=CARTESIAN_POINT('Ctrl Pts',(7.31357807545766,0.524640804216316,
138.));
#246850=CARTESIAN_POINT('Ctrl Pts',(7.31428603059942,0.654766986429571,
138.));
#246851=CARTESIAN_POINT('Ctrl Pts',(7.31144808502855,0.784989760971824,
138.));
#246852=CARTESIAN_POINT('Ctrl Pts',(7.30501644905709,0.915186995230226,
138.));
#246853=CARTESIAN_POINT('Ctrl Pts',(7.29541239991929,1.10960419187653,138.));
#246854=CARTESIAN_POINT('Ctrl Pts',(7.27779751519746,1.30396484924485,138.));
#246855=CARTESIAN_POINT('Ctrl Pts',(7.25233008411155,1.49781397277794,138.));
#246856=CARTESIAN_POINT('Ctrl Pts',(7.25064901849204,1.51060965271297,138.));
#246857=CARTESIAN_POINT('Ctrl Pts',(7.24893371970543,1.52340310188329,138.));
#246858=CARTESIAN_POINT('Ctrl Pts',(7.24718422537979,1.53619418840126,138.));
#246859=CARTESIAN_POINT('Ctrl Pts',(7.24401930498186,1.55933388656357,138.));
#246860=CARTESIAN_POINT('Ctrl Pts',(7.24074365388209,1.58245715953455,138.));
#246861=CARTESIAN_POINT('Ctrl Pts',(7.23735822289073,1.60556014491937,138.));
#246862=CARTESIAN_POINT('Ctrl Pts',(7.20913527842305,1.79816022308357,138.));
#246863=CARTESIAN_POINT('Ctrl Pts',(7.17327751050791,1.9894185177033,138.));
#246864=CARTESIAN_POINT('Ctrl Pts',(7.13006388188138,2.17888639203352,138.));
#246865=CARTESIAN_POINT('Ctrl Pts',(7.08581849473728,2.37287795713814,138.));
#246866=CARTESIAN_POINT('Ctrl Pts',(7.03386183221965,2.56499323052619,138.));
#246867=CARTESIAN_POINT('Ctrl Pts',(6.97443939096877,2.75475966696422,138.));
#246868=CARTESIAN_POINT('Ctrl Pts',(6.91464739397427,2.94570628508201,138.));
#246869=CARTESIAN_POINT('Ctrl Pts',(6.84729634168636,3.13427548648786,138.));
#246870=CARTESIAN_POINT('Ctrl Pts',(6.77258332983085,3.31998438996726,138.));
#246871=CARTESIAN_POINT('Ctrl Pts',(6.6981710488299,3.50494578781337,138.));
#246872=CARTESIAN_POINT('Ctrl Pts',(6.61645574690026,3.68707059386329,138.));
#246873=CARTESIAN_POINT('Ctrl Pts',(6.52758237206456,3.86586940628296,138.));
#246874=CARTESIAN_POINT('Ctrl Pts',(6.47276241379817,3.97615826898282,138.));
#246875=CARTESIAN_POINT('Ctrl Pts',(6.41521797292606,4.0851813670272,138.));
#246876=CARTESIAN_POINT('Ctrl Pts',(6.35497407499007,4.19281964495557,138.));
#246877=CARTESIAN_POINT('Ctrl Pts',(6.33797951959163,4.22318395968162,138.));
#246878=CARTESIAN_POINT('Ctrl Pts',(6.32077010570966,4.25343804897414,138.));
#246879=CARTESIAN_POINT('Ctrl Pts',(6.30334629954177,4.28357918000919,138.));
#246880=CARTESIAN_POINT('Ctrl Pts',(6.29076653244945,4.30534069438027,138.));
#246881=CARTESIAN_POINT('Ctrl Pts',(6.27807965496324,4.32703527814749,138.));
#246882=CARTESIAN_POINT('Ctrl Pts',(6.26528698879689,4.34866051885305,138.));
#246883=CARTESIAN_POINT('Ctrl Pts',(6.24226933205953,4.3875704975042,138.));
#246884=CARTESIAN_POINT('Ctrl Pts',(6.21890827852989,4.42625757737068,138.));
#246885=CARTESIAN_POINT('Ctrl Pts',(6.19520638596214,4.46471642251,138.));
#246886=CARTESIAN_POINT('Ctrl Pts',(6.08983107847159,4.63569908225763,138.));
#246887=CARTESIAN_POINT('Ctrl Pts',(5.97772289519015,4.80217182705261,138.));
#246888=CARTESIAN_POINT('Ctrl Pts',(5.85928943886702,4.96389424887306,138.));
#246889=CARTESIAN_POINT('Ctrl Pts',(5.73914075688195,5.12795883359771,138.));
#246890=CARTESIAN_POINT('Ctrl Pts',(5.61248195284315,5.28713503441401,138.));
#246891=CARTESIAN_POINT('Ctrl Pts',(5.47968893077447,5.44115076767619,138.));
#246892=CARTESIAN_POINT('Ctrl Pts',(5.35498558079184,5.58578395388301,138.));
#246893=CARTESIAN_POINT('Ctrl Pts',(5.22487190446606,5.7258664220397,138.));
#246894=CARTESIAN_POINT('Ctrl Pts',(5.08962417547183,5.86114996981617,138.));
#246895=CARTESIAN_POINT('Ctrl Pts',(5.06750037681787,5.88327962769994,138.));
#246896=CARTESIAN_POINT('Ctrl Pts',(5.04523816074071,5.90528168859171,138.));
#246897=CARTESIAN_POINT('Ctrl Pts',(5.02285166040568,5.9271425397572,138.));
#246898=CARTESIAN_POINT('Ctrl Pts',(4.87519656581737,6.07133059944996,138.));
#246899=CARTESIAN_POINT('Ctrl Pts',(4.72201394798034,6.20950353456649,138.));
#246900=CARTESIAN_POINT('Ctrl Pts',(4.56370622067795,6.34139593385774,138.));
#246901=CARTESIAN_POINT('Ctrl Pts',(4.40476463903515,6.47381642215128,138.));
#246902=CARTESIAN_POINT('Ctrl Pts',(4.24065639042664,6.59990650300305,138.));
#246903=CARTESIAN_POINT('Ctrl Pts',(4.0717452682137,6.71936805595367,138.));
#246904=CARTESIAN_POINT('Ctrl Pts',(3.90357067072022,6.8383087054515,138.));
#246905=CARTESIAN_POINT('Ctrl Pts',(3.73063450900765,6.95067899177625,138.));
#246906=CARTESIAN_POINT('Ctrl Pts',(3.55325979428486,7.05614801072615,138.));
#246907=CARTESIAN_POINT('Ctrl Pts',(3.50933718657416,7.08226489188482,138.));
#246908=CARTESIAN_POINT('Ctrl Pts',(3.46514225877028,7.10795840003617,138.));
#246909=CARTESIAN_POINT('Ctrl Pts',(3.42067962509738,7.13322310757512,138.));
#246910=CARTESIAN_POINT('Ctrl Pts',(3.42490370648426,7.13754033682968,8.));
#246911=CARTESIAN_POINT('Ctrl Pts',(3.60303338065709,7.03788846583432,7.99999999999999));
#246912=CARTESIAN_POINT('Ctrl Pts',(3.77686286893927,6.93118228361841,7.99999999999999));
#246913=CARTESIAN_POINT('Ctrl Pts',(3.94592285660953,6.8174072015925,7.99999999999999));
#246914=CARTESIAN_POINT('Ctrl Pts',(4.11679905550406,6.70240983401064,7.99999999999999));
#246915=CARTESIAN_POINT('Ctrl Pts',(4.28280321834002,6.5801903541098,8.));
#246916=CARTESIAN_POINT('Ctrl Pts',(4.44364270499849,6.45121617950757,8.));
#246917=CARTESIAN_POINT('Ctrl Pts',(4.60504482065505,6.32179084324012,8.));
#246918=CARTESIAN_POINT('Ctrl Pts',(4.76124648814143,6.18556280407072,8.));
#246919=CARTESIAN_POINT('Ctrl Pts',(4.9119102565287,6.04297273661884,8.));
#246920=CARTESIAN_POINT('Ctrl Pts',(4.94377744841198,6.01281322920191,8.));
#246921=CARTESIAN_POINT('Ctrl Pts',(4.97539672828523,5.9823690099197,8.));
#246922=CARTESIAN_POINT('Ctrl Pts',(5.00676463700424,5.95164411183574,8.));
#246923=CARTESIAN_POINT('Ctrl Pts',(5.02880360356028,5.93005692196675,8.));
#246924=CARTESIAN_POINT('Ctrl Pts',(5.05071989143719,5.90832975933061,8.));
#246925=CARTESIAN_POINT('Ctrl Pts',(5.07250778250975,5.88646852196407,8.));
#246926=CARTESIAN_POINT('Ctrl Pts',(5.158239465655,5.80044823350066,8.));
#246927=CARTESIAN_POINT('Ctrl Pts',(5.24189935706624,5.71243742897355,8.));
#246928=CARTESIAN_POINT('Ctrl Pts',(5.32342886913692,5.62253662790359,8.));
#246929=CARTESIAN_POINT('Ctrl Pts',(5.46097401376483,5.47086861994824,8.));
#246930=CARTESIAN_POINT('Ctrl Pts',(5.59246025169705,5.3138206439058,8.));
#246931=CARTESIAN_POINT('Ctrl Pts',(5.71758256421037,5.15184052730674,8.));
#246932=CARTESIAN_POINT('Ctrl Pts',(5.84206463687843,4.99068924868794,8.));
#246933=CARTESIAN_POINT('Ctrl Pts',(5.96024808036236,4.82465548939151,8.));
#246934=CARTESIAN_POINT('Ctrl Pts',(6.07178603797319,4.65415854388629,8.));
#246935=CARTESIAN_POINT('Ctrl Pts',(6.11249389133456,4.59193251066087,8.));
#246936=CARTESIAN_POINT('Ctrl Pts',(6.15231607804158,4.5291118128463,8.));
#246937=CARTESIAN_POINT('Ctrl Pts',(6.19123404625067,4.46571638178551,8.));
#246938=CARTESIAN_POINT('Ctrl Pts',(6.22207638996413,4.41547574064682,8.));
#246939=CARTESIAN_POINT('Ctrl Pts',(6.25235065951106,4.36487441132344,8.));
#246940=CARTESIAN_POINT('Ctrl Pts',(6.28204768525483,4.31392140458892,8.));
#246941=CARTESIAN_POINT('Ctrl Pts',(6.30046683332831,4.28231854361794,8.));
#246942=CARTESIAN_POINT('Ctrl Pts',(6.31866374179757,4.25058040510658,8.));
#246943=CARTESIAN_POINT('Ctrl Pts',(6.33662197851953,4.21873508832127,8.));
#246944=CARTESIAN_POINT('Ctrl Pts',(6.3877624699296,4.12804772437101,8.));
#246945=CARTESIAN_POINT('Ctrl Pts',(6.43699714916998,4.03644132373437,8.));
#246946=CARTESIAN_POINT('Ctrl Pts',(6.48428962272374,3.94397632605379,8.));
#246947=CARTESIAN_POINT('Ctrl Pts',(6.57567872566177,3.76529476097158,8.));
#246948=CARTESIAN_POINT('Ctrl Pts',(6.65981818510592,3.58340802051667,8.));
#246949=CARTESIAN_POINT('Ctrl Pts',(6.73660877174782,3.39873683092503,8.));
#246950=CARTESIAN_POINT('Ctrl Pts',(6.81347023922936,3.21389518230254,8.));
#246951=CARTESIAN_POINT('Ctrl Pts',(6.88296940124662,3.02626327931723,8.));
#246952=CARTESIAN_POINT('Ctrl Pts',(6.94495644380309,2.83624949096006,8.));
#246953=CARTESIAN_POINT('Ctrl Pts',(7.0065419660172,2.64746651469209,8.));
#246954=CARTESIAN_POINT('Ctrl Pts',(7.06071245336442,2.45633176848018,8.));
#246955=CARTESIAN_POINT('Ctrl Pts',(7.10726979491501,2.26324214781201,8.));
#246956=CARTESIAN_POINT('Ctrl Pts',(7.14496638496124,2.10690117064093,8.));
#246957=CARTESIAN_POINT('Ctrl Pts',(7.17767099659649,1.94927840699215,8.));
#246958=CARTESIAN_POINT('Ctrl Pts',(7.20525302507637,1.79058709511881,8.));
#246959=CARTESIAN_POINT('Ctrl Pts',(7.21612231004232,1.72805140846221,8.));
#246960=CARTESIAN_POINT('Ctrl Pts',(7.22619584448681,1.66534982996421,8.));
#246961=CARTESIAN_POINT('Ctrl Pts',(7.23546463629665,1.60249563050015,8.));
#246962=CARTESIAN_POINT('Ctrl Pts',(7.2414327693778,1.56202409604274,8.));
#246963=CARTESIAN_POINT('Ctrl Pts',(7.24706820793831,1.52148084492807,8.));
#246964=CARTESIAN_POINT('Ctrl Pts',(7.25236235321427,1.48091914014147,8.));
#246965=CARTESIAN_POINT('Ctrl Pts',(7.27761224616607,1.28746417235747,8.));
#246966=CARTESIAN_POINT('Ctrl Pts',(7.29513326182066,1.09340516848697,8.00000000000001));
#246967=CARTESIAN_POINT('Ctrl Pts',(7.30480364597534,0.899123198458447,
8.));
#246968=CARTESIAN_POINT('Ctrl Pts',(7.31392911010541,0.715788894437285,
8.));
#246969=CARTESIAN_POINT('Ctrl Pts',(7.31606343307754,0.532255537961043,
8.));
#246970=CARTESIAN_POINT('Ctrl Pts',(7.31106172364628,0.348843391340116,
8.));
#246971=CARTESIAN_POINT('Ctrl Pts',(7.30573789570327,0.153619193556052,
8.));
#246972=CARTESIAN_POINT('Ctrl Pts',(7.29232950872236,-0.0414684692841456,
8.00000000000001));
#246973=CARTESIAN_POINT('Ctrl Pts',(7.27096643466698,-0.235911858864235,
8.00000000000001));
#246974=CARTESIAN_POINT('Ctrl Pts',(7.24977413424447,-0.428800893301357,
8.00000000000001));
#246975=CARTESIAN_POINT('Ctrl Pts',(7.22075348912854,-0.62105660412465,
8.00000000000001));
#246976=CARTESIAN_POINT('Ctrl Pts',(7.18398479930742,-0.81216290480137,
8.00000000000001));
#246977=CARTESIAN_POINT('Ctrl Pts',(7.15738132160842,-0.950435229241711,
8.00000000000001));
#246978=CARTESIAN_POINT('Ctrl Pts',(7.12672073322938,-1.08810544329263,
8.));
#246979=CARTESIAN_POINT('Ctrl Pts',(7.0920194960254,-1.22496823775203,8.));
#246980=CARTESIAN_POINT('Ctrl Pts',(7.08350694221174,-1.25854202349559,
8.));
#246981=CARTESIAN_POINT('Ctrl Pts',(7.07475002512292,-1.29207103794083,
8.));
#246982=CARTESIAN_POINT('Ctrl Pts',(7.06575857857453,-1.32551742518055,
8.));
#246983=CARTESIAN_POINT('Ctrl Pts',(7.01585043134197,-1.51116577550707,
8.));
#246984=CARTESIAN_POINT('Ctrl Pts',(6.95866555411597,-1.69449496168078,
8.));
#246985=CARTESIAN_POINT('Ctrl Pts',(6.89436543997893,-1.87503604479795,
8.));
#246986=CARTESIAN_POINT('Ctrl Pts',(6.83023212431252,-2.0551087931858,8.));
#246987=CARTESIAN_POINT('Ctrl Pts',(6.75902012696239,-2.23240857725891,
8.));
#246988=CARTESIAN_POINT('Ctrl Pts',(6.68084233139359,-2.40644947611183,
8.));
#246989=CARTESIAN_POINT('Ctrl Pts',(6.6038005184819,-2.57796142871745,8.));
#246990=CARTESIAN_POINT('Ctrl Pts',(6.51999351024779,-2.7463090970057,8.00000000000001));
#246991=CARTESIAN_POINT('Ctrl Pts',(6.42948842321972,-2.91099803412343,
8.00000000000001));
#246992=CARTESIAN_POINT('Ctrl Pts',(6.39882586075824,-2.96679362514386,
8.));
#246993=CARTESIAN_POINT('Ctrl Pts',(6.36739415792422,-3.02216897199648,
8.));
#246994=CARTESIAN_POINT('Ctrl Pts',(6.33519494702265,-3.07710388684608,
8.));
#246995=CARTESIAN_POINT('Ctrl Pts',(6.26232290414108,-3.20143051965874,
8.00000000000001));
#246996=CARTESIAN_POINT('Ctrl Pts',(6.18552036272165,-3.32350222199875,
8.));
#246997=CARTESIAN_POINT('Ctrl Pts',(6.10490764005655,-3.44316034524444,
8.));
#246998=CARTESIAN_POINT('Ctrl Pts',(6.06827231631093,-3.49754027361023,
8.));
#246999=CARTESIAN_POINT('Ctrl Pts',(6.03084992728334,-3.5514215248963,8.00000000000001));
#247000=CARTESIAN_POINT('Ctrl Pts',(5.99265116460685,-3.6047882158074,8.));
#247001=CARTESIAN_POINT('Ctrl Pts',(5.96951316952572,-3.63711382389726,
8.));
#247002=CARTESIAN_POINT('Ctrl Pts',(5.9460907821855,-3.66924999344316,8.00000000000001));
#247003=CARTESIAN_POINT('Ctrl Pts',(5.92238485722257,-3.70119504522787,
8.));
#247004=CARTESIAN_POINT('Ctrl Pts',(5.90199196396135,-3.72867560261125,
8.));
#247005=CARTESIAN_POINT('Ctrl Pts',(5.88138869951439,-3.75601516977367,
8.));
#247006=CARTESIAN_POINT('Ctrl Pts',(5.86059722504908,-3.78318498211917,
8.));
#247007=CARTESIAN_POINT('Ctrl Pts',(5.74709140037064,-3.93151173796224,
8.));
#247008=CARTESIAN_POINT('Ctrl Pts',(5.62785777030339,-4.07494918288655,
8.00000000000001));
#247009=CARTESIAN_POINT('Ctrl Pts',(5.503232290236,-4.21322289775717,8.));
#247010=CARTESIAN_POINT('Ctrl Pts',(5.37820579271597,-4.35194154710566,
8.));
#247011=CARTESIAN_POINT('Ctrl Pts',(5.24775214698824,-4.48546363618437,
8.));
#247012=CARTESIAN_POINT('Ctrl Pts',(5.1121747072249,-4.61347432725512,8.));
#247013=CARTESIAN_POINT('Ctrl Pts',(4.97745627898038,-4.74067394932832,
8.));
#247014=CARTESIAN_POINT('Ctrl Pts',(4.83767821573056,-4.86243216978443,
8.));
#247015=CARTESIAN_POINT('Ctrl Pts',(4.69311114269838,-4.97839674800658,
8.));
#247016=CARTESIAN_POINT('Ctrl Pts',(4.55125768635081,-5.09218459671703,
8.));
#247017=CARTESIAN_POINT('Ctrl Pts',(4.40479277614842,-5.2003945083745,8.));
#247018=CARTESIAN_POINT('Ctrl Pts',(4.25395421979913,-5.30264739511277,
8.));
#247019=CARTESIAN_POINT('Ctrl Pts',(4.14773939891244,-5.37465002038917,
8.));
#247020=CARTESIAN_POINT('Ctrl Pts',(4.03935555221588,-5.443697940156,8.));
#247021=CARTESIAN_POINT('Ctrl Pts',(3.92888236737293,-5.50964357679762,
8.));
#247022=CARTESIAN_POINT('Origin',(0.,0.,138.));
#247023=CARTESIAN_POINT('Origin',(0.,0.,4.));
#247024=CARTESIAN_POINT('',(-10.,-1.22464679914735E-15,4.));
#247025=CARTESIAN_POINT('Origin',(0.,0.,4.));
#247026=CARTESIAN_POINT('',(-6.,7.34788079488412E-16,4.));
#247027=CARTESIAN_POINT('Origin',(0.,0.,4.));
#247028=CARTESIAN_POINT('Origin',(0.,0.,4.));
#247029=CARTESIAN_POINT('',(-10.,-1.22464679914735E-15,8.));
#247030=CARTESIAN_POINT('Origin',(0.,0.,8.));
#247031=CARTESIAN_POINT('',(-10.,-1.22464679914735E-15,4.));
#247032=CARTESIAN_POINT('Origin',(0.,0.,-36.));
#247033=CARTESIAN_POINT('',(-6.,-7.34788079488412E-16,-36.));
#247034=CARTESIAN_POINT('',(-6.,-7.34788079488412E-16,-36.));
#247035=CARTESIAN_POINT('',(-6.,-7.34788079488412E-16,-36.));
#247036=CARTESIAN_POINT('Origin',(0.,0.,-36.));
#247037=CARTESIAN_POINT('Origin',(0.,0.,8.));
#247038=CARTESIAN_POINT('Origin',(0.,0.,-36.));
#247039=CARTESIAN_POINT('',(0.,0.,0.));
#247040=CARTESIAN_POINT('Origin',(-2.22044604925031E-15,0.,14.));
#247041=CARTESIAN_POINT('',(14.,0.,12.));
#247042=CARTESIAN_POINT('',(13.856406460551,-2.,14.));
#247043=CARTESIAN_POINT('Ctrl Pts',(14.,6.24500451351651E-16,12.));
#247044=CARTESIAN_POINT('Ctrl Pts',(14.,-0.251492536553737,12.));
#247045=CARTESIAN_POINT('Ctrl Pts',(13.992532457489,-0.519514815600169,
12.0503312082537));
#247046=CARTESIAN_POINT('Ctrl Pts',(13.965542073511,-1.01217331161422,12.2545461305954));
#247047=CARTESIAN_POINT('Ctrl Pts',(13.9463980317977,-1.23683805013847,
12.4084109253923));
#247048=CARTESIAN_POINT('Ctrl Pts',(13.9103782647342,-1.59159161400131,
12.7631644892551));
#247049=CARTESIAN_POINT('Ctrl Pts',(13.891148239315,-1.74545441720186,12.9878281297258));
#247050=CARTESIAN_POINT('Ctrl Pts',(13.8639606805058,-1.94966788779478,
13.4804828838555));
#247051=CARTESIAN_POINT('Ctrl Pts',(13.856406460551,-2.,13.7485038629575));
#247052=CARTESIAN_POINT('Ctrl Pts',(13.856406460551,-2.,14.));
#247053=CARTESIAN_POINT('',(14.,0.,16.));
#247054=CARTESIAN_POINT('Ctrl Pts',(14.,-2.77555756156289E-16,16.));
#247055=CARTESIAN_POINT('Ctrl Pts',(14.,0.251492536553738,16.));
#247056=CARTESIAN_POINT('Ctrl Pts',(13.992532457489,0.51951481560017,15.9496687917463));
#247057=CARTESIAN_POINT('Ctrl Pts',(13.965542073511,1.01217331161422,15.7454538694046));
#247058=CARTESIAN_POINT('Ctrl Pts',(13.9463980317977,1.23683805013847,15.5915890746077));
#247059=CARTESIAN_POINT('Ctrl Pts',(13.9103782647342,1.59159161400131,15.2368355107449));
#247060=CARTESIAN_POINT('Ctrl Pts',(13.891148239315,1.74545441720186,15.0121718702742));
#247061=CARTESIAN_POINT('Ctrl Pts',(13.8639606805058,1.94966788779478,14.5195171161445));
#247062=CARTESIAN_POINT('Ctrl Pts',(13.856406460551,2.,14.2514961370425));
#247063=CARTESIAN_POINT('Ctrl Pts',(13.856406460551,2.,13.7485038629575));
#247064=CARTESIAN_POINT('Ctrl Pts',(13.8639606805058,1.94966788779478,13.4804828838555));
#247065=CARTESIAN_POINT('Ctrl Pts',(13.891148239315,1.74545441720186,12.9878281297258));
#247066=CARTESIAN_POINT('Ctrl Pts',(13.9103782647342,1.59159161400131,12.7631644892551));
#247067=CARTESIAN_POINT('Ctrl Pts',(13.9463980317977,1.23683805013847,12.4084109253923));
#247068=CARTESIAN_POINT('Ctrl Pts',(13.965542073511,1.01217331161422,12.2545461305954));
#247069=CARTESIAN_POINT('Ctrl Pts',(13.992532457489,0.519514815600173,12.0503312082537));
#247070=CARTESIAN_POINT('Ctrl Pts',(14.,0.251492536553739,12.));
#247071=CARTESIAN_POINT('Ctrl Pts',(14.,6.41847686111419E-16,12.));
#247072=CARTESIAN_POINT('Ctrl Pts',(13.856406460551,-2.,14.));
#247073=CARTESIAN_POINT('Ctrl Pts',(13.856406460551,-2.,14.2514961370425));
#247074=CARTESIAN_POINT('Ctrl Pts',(13.8639606805058,-1.94966788779478,
14.5195171161445));
#247075=CARTESIAN_POINT('Ctrl Pts',(13.891148239315,-1.74545441720186,15.0121718702742));
#247076=CARTESIAN_POINT('Ctrl Pts',(13.9103782647342,-1.59159161400131,
15.2368355107449));
#247077=CARTESIAN_POINT('Ctrl Pts',(13.9463980317977,-1.23683805013847,
15.5915890746077));
#247078=CARTESIAN_POINT('Ctrl Pts',(13.965542073511,-1.01217331161422,15.7454538694046));
#247079=CARTESIAN_POINT('Ctrl Pts',(13.992532457489,-0.519514815600171,
15.9496687917463));
#247080=CARTESIAN_POINT('Ctrl Pts',(14.,-0.251492536553739,16.));
#247081=CARTESIAN_POINT('Ctrl Pts',(14.,5.03069808033274E-16,16.));
#247082=CARTESIAN_POINT('',(5.65685424949238,-2.,14.));
#247083=CARTESIAN_POINT('',(-2.22044604925031E-15,-2.,14.));
#247084=CARTESIAN_POINT('Ctrl Pts',(5.65685424949238,-2.,14.));
#247085=CARTESIAN_POINT('Ctrl Pts',(5.65685424949238,-2.,13.7467078791842));
#247086=CARTESIAN_POINT('Ctrl Pts',(5.67565356574251,-1.94898067853762,
13.477996053073));
#247087=CARTESIAN_POINT('Ctrl Pts',(5.74186082552466,-1.7443058152527,12.9858936400846));
#247088=CARTESIAN_POINT('Ctrl Pts',(5.78813771212597,-1.59074095999941,
12.7623138352532));
#247089=CARTESIAN_POINT('Ctrl Pts',(5.87374622031365,-1.23776803829002,
12.4093409135438));
#247090=CARTESIAN_POINT('Ctrl Pts',(5.9188739106068,-1.01415562391481,12.2557130277668));
#247091=CARTESIAN_POINT('Ctrl Pts',(5.98240475886912,-0.521932274441715,
12.0509911583939));
#247092=CARTESIAN_POINT('Ctrl Pts',(6.,-0.253174643734702,12.));
#247093=CARTESIAN_POINT('Ctrl Pts',(6.,0.253174643734703,12.));
#247094=CARTESIAN_POINT('Ctrl Pts',(5.98240475886912,0.521932274441715,
12.0509911583939));
#247095=CARTESIAN_POINT('Ctrl Pts',(5.9188739106068,1.01415562391481,12.2557130277668));
#247096=CARTESIAN_POINT('Ctrl Pts',(5.87374622031365,1.23776803829002,12.4093409135438));
#247097=CARTESIAN_POINT('Ctrl Pts',(5.78813771212597,1.59074095999941,12.7623138352532));
#247098=CARTESIAN_POINT('Ctrl Pts',(5.74186082552466,1.7443058152527,12.9858936400846));
#247099=CARTESIAN_POINT('Ctrl Pts',(5.67565356574251,1.94898067853762,13.477996053073));
#247100=CARTESIAN_POINT('Ctrl Pts',(5.65685424949238,2.,13.7467078791842));
#247101=CARTESIAN_POINT('Ctrl Pts',(5.65685424949238,2.,14.2532921208158));
#247102=CARTESIAN_POINT('Ctrl Pts',(5.67565356574251,1.94898067853763,14.522003946927));
#247103=CARTESIAN_POINT('Ctrl Pts',(5.74186082552466,1.74430581525271,15.0141063599154));
#247104=CARTESIAN_POINT('Ctrl Pts',(5.78813771212597,1.59074095999941,15.2376861647468));
#247105=CARTESIAN_POINT('Ctrl Pts',(5.87374622031365,1.23776803829002,15.5906590864562));
#247106=CARTESIAN_POINT('Ctrl Pts',(5.9188739106068,1.01415562391481,15.7442869722332));
#247107=CARTESIAN_POINT('Ctrl Pts',(5.98240475886912,0.521932274441714,
15.9490088416061));
#247108=CARTESIAN_POINT('Ctrl Pts',(6.,0.253174643734703,16.));
#247109=CARTESIAN_POINT('Ctrl Pts',(6.,-0.253174643734703,16.));
#247110=CARTESIAN_POINT('Ctrl Pts',(5.98240475886912,-0.521932274441715,
15.9490088416061));
#247111=CARTESIAN_POINT('Ctrl Pts',(5.9188739106068,-1.01415562391481,15.7442869722332));
#247112=CARTESIAN_POINT('Ctrl Pts',(5.87374622031365,-1.23776803829002,
15.5906590864562));
#247113=CARTESIAN_POINT('Ctrl Pts',(5.78813771212597,-1.59074095999941,
15.2376861647468));
#247114=CARTESIAN_POINT('Ctrl Pts',(5.74186082552466,-1.74430581525271,
15.0141063599154));
#247115=CARTESIAN_POINT('Ctrl Pts',(5.67565356574251,-1.94898067853763,
14.522003946927));
#247116=CARTESIAN_POINT('Ctrl Pts',(5.65685424949238,-2.,14.2532921208158));
#247117=CARTESIAN_POINT('Ctrl Pts',(5.65685424949238,-2.,14.));
#247118=CARTESIAN_POINT('Origin',(-2.22044604925031E-15,0.,14.));
#247119=CARTESIAN_POINT('',(-6.,-5.40866387341887E-16,12.));
#247120=CARTESIAN_POINT('',(-5.65685424949238,-2.,14.));
#247121=CARTESIAN_POINT('Ctrl Pts',(-6.,6.24500451351651E-16,12.));
#247122=CARTESIAN_POINT('Ctrl Pts',(-6.,-0.253174643734702,12.));
#247123=CARTESIAN_POINT('Ctrl Pts',(-5.98240475886912,-0.521932274441713,
12.0509911583939));
#247124=CARTESIAN_POINT('Ctrl Pts',(-5.9188739106068,-1.01415562391481,
12.2557130277668));
#247125=CARTESIAN_POINT('Ctrl Pts',(-5.87374622031365,-1.23776803829002,
12.4093409135438));
#247126=CARTESIAN_POINT('Ctrl Pts',(-5.78813771212597,-1.59074095999941,
12.7623138352532));
#247127=CARTESIAN_POINT('Ctrl Pts',(-5.74186082552466,-1.7443058152527,
12.9858936400846));
#247128=CARTESIAN_POINT('Ctrl Pts',(-5.67565356574251,-1.94898067853762,
13.477996053073));
#247129=CARTESIAN_POINT('Ctrl Pts',(-5.65685424949238,-2.,13.7467078791842));
#247130=CARTESIAN_POINT('Ctrl Pts',(-5.65685424949238,-2.,14.));
#247131=CARTESIAN_POINT('',(-6.,8.3634064009764E-17,16.));
#247132=CARTESIAN_POINT('Ctrl Pts',(-6.,-3.98986399474666E-16,16.));
#247133=CARTESIAN_POINT('Ctrl Pts',(-6.,0.253174643734703,16.));
#247134=CARTESIAN_POINT('Ctrl Pts',(-5.98240475886912,0.521932274441714,
15.9490088416061));
#247135=CARTESIAN_POINT('Ctrl Pts',(-5.9188739106068,1.01415562391481,15.7442869722332));
#247136=CARTESIAN_POINT('Ctrl Pts',(-5.87374622031365,1.23776803829002,
15.5906590864562));
#247137=CARTESIAN_POINT('Ctrl Pts',(-5.78813771212597,1.59074095999941,
15.2376861647468));
#247138=CARTESIAN_POINT('Ctrl Pts',(-5.74186082552466,1.74430581525271,
15.0141063599154));
#247139=CARTESIAN_POINT('Ctrl Pts',(-5.67565356574251,1.94898067853763,
14.522003946927));
#247140=CARTESIAN_POINT('Ctrl Pts',(-5.65685424949238,2.,14.2532921208158));
#247141=CARTESIAN_POINT('Ctrl Pts',(-5.65685424949238,2.,13.7467078791842));
#247142=CARTESIAN_POINT('Ctrl Pts',(-5.67565356574251,1.94898067853762,
13.477996053073));
#247143=CARTESIAN_POINT('Ctrl Pts',(-5.74186082552466,1.7443058152527,12.9858936400846));
#247144=CARTESIAN_POINT('Ctrl Pts',(-5.78813771212597,1.59074095999941,
12.7623138352532));
#247145=CARTESIAN_POINT('Ctrl Pts',(-5.87374622031365,1.23776803829002,
12.4093409135438));
#247146=CARTESIAN_POINT('Ctrl Pts',(-5.9188739106068,1.01415562391481,12.2557130277668));
#247147=CARTESIAN_POINT('Ctrl Pts',(-5.98240475886912,0.521932274441715,
12.0509911583939));
#247148=CARTESIAN_POINT('Ctrl Pts',(-6.,0.253174643734703,12.));
#247149=CARTESIAN_POINT('Ctrl Pts',(-6.,6.41847686111419E-16,12.));
#247150=CARTESIAN_POINT('Ctrl Pts',(-5.65685424949238,-2.,14.));
#247151=CARTESIAN_POINT('Ctrl Pts',(-5.65685424949238,-2.,14.2532921208158));
#247152=CARTESIAN_POINT('Ctrl Pts',(-5.67565356574251,-1.94898067853763,
14.522003946927));
#247153=CARTESIAN_POINT('Ctrl Pts',(-5.74186082552466,-1.74430581525271,
15.0141063599154));
#247154=CARTESIAN_POINT('Ctrl Pts',(-5.78813771212597,-1.59074095999941,
15.2376861647468));
#247155=CARTESIAN_POINT('Ctrl Pts',(-5.87374622031365,-1.23776803829002,
15.5906590864562));
#247156=CARTESIAN_POINT('Ctrl Pts',(-5.9188739106068,-1.01415562391481,
15.7442869722332));
#247157=CARTESIAN_POINT('Ctrl Pts',(-5.98240475886912,-0.521932274441715,
15.9490088416061));
#247158=CARTESIAN_POINT('Ctrl Pts',(-6.,-0.253174643734703,16.));
#247159=CARTESIAN_POINT('Ctrl Pts',(-6.,-3.98986399474666E-16,16.));
#247160=CARTESIAN_POINT('',(-13.856406460551,-2.,14.));
#247161=CARTESIAN_POINT('',(-2.22044604925031E-15,-2.,14.));
#247162=CARTESIAN_POINT('',(-14.,0.,16.));
#247163=CARTESIAN_POINT('Ctrl Pts',(-14.,-3.46944695195361E-16,16.));
#247164=CARTESIAN_POINT('Ctrl Pts',(-14.,-0.251492536553739,16.));
#247165=CARTESIAN_POINT('Ctrl Pts',(-13.992532457489,-0.519514815600171,
15.9496687917463));
#247166=CARTESIAN_POINT('Ctrl Pts',(-13.965542073511,-1.01217331161422,
15.7454538694046));
#247167=CARTESIAN_POINT('Ctrl Pts',(-13.9463980317977,-1.23683805013847,
15.5915890746077));
#247168=CARTESIAN_POINT('Ctrl Pts',(-13.9103782647342,-1.59159161400131,
15.2368355107449));
#247169=CARTESIAN_POINT('Ctrl Pts',(-13.891148239315,-1.74545441720187,
15.0121718702742));
#247170=CARTESIAN_POINT('Ctrl Pts',(-13.8639606805058,-1.94966788779478,
14.5195171161445));
#247171=CARTESIAN_POINT('Ctrl Pts',(-13.856406460551,-2.,14.2514961370425));
#247172=CARTESIAN_POINT('Ctrl Pts',(-13.856406460551,-2.,14.));
#247173=CARTESIAN_POINT('',(-14.,0.,12.));
#247174=CARTESIAN_POINT('Ctrl Pts',(-14.,6.07153216591882E-16,12.));
#247175=CARTESIAN_POINT('Ctrl Pts',(-14.,0.251492536553739,12.));
#247176=CARTESIAN_POINT('Ctrl Pts',(-13.992532457489,0.519514815600171,
12.0503312082537));
#247177=CARTESIAN_POINT('Ctrl Pts',(-13.965542073511,1.01217331161422,12.2545461305954));
#247178=CARTESIAN_POINT('Ctrl Pts',(-13.9463980317977,1.23683805013847,
12.4084109253923));
#247179=CARTESIAN_POINT('Ctrl Pts',(-13.9103782647342,1.59159161400131,
12.7631644892551));
#247180=CARTESIAN_POINT('Ctrl Pts',(-13.891148239315,1.74545441720186,12.9878281297258));
#247181=CARTESIAN_POINT('Ctrl Pts',(-13.8639606805058,1.94966788779478,
13.4804828838555));
#247182=CARTESIAN_POINT('Ctrl Pts',(-13.856406460551,2.,13.7485038629575));
#247183=CARTESIAN_POINT('Ctrl Pts',(-13.856406460551,2.,14.2514961370425));
#247184=CARTESIAN_POINT('Ctrl Pts',(-13.8639606805058,1.94966788779478,
14.5195171161445));
#247185=CARTESIAN_POINT('Ctrl Pts',(-13.891148239315,1.74545441720186,15.0121718702742));
#247186=CARTESIAN_POINT('Ctrl Pts',(-13.9103782647342,1.59159161400131,
15.2368355107449));
#247187=CARTESIAN_POINT('Ctrl Pts',(-13.9463980317977,1.23683805013847,
15.5915890746077));
#247188=CARTESIAN_POINT('Ctrl Pts',(-13.965542073511,1.01217331161422,15.7454538694046));
#247189=CARTESIAN_POINT('Ctrl Pts',(-13.992532457489,0.51951481560017,15.9496687917463));
#247190=CARTESIAN_POINT('Ctrl Pts',(-14.,0.251492536553738,16.));
#247191=CARTESIAN_POINT('Ctrl Pts',(-14.,-2.77555756156289E-16,16.));
#247192=CARTESIAN_POINT('Ctrl Pts',(-13.856406460551,-2.,14.));
#247193=CARTESIAN_POINT('Ctrl Pts',(-13.856406460551,-2.,13.7485038629575));
#247194=CARTESIAN_POINT('Ctrl Pts',(-13.8639606805058,-1.94966788779478,
13.4804828838555));
#247195=CARTESIAN_POINT('Ctrl Pts',(-13.891148239315,-1.74545441720186,
12.9878281297258));
#247196=CARTESIAN_POINT('Ctrl Pts',(-13.9103782647342,-1.59159161400131,
12.7631644892551));
#247197=CARTESIAN_POINT('Ctrl Pts',(-13.9463980317977,-1.23683805013847,
12.4084109253923));
#247198=CARTESIAN_POINT('Ctrl Pts',(-13.965542073511,-1.01217331161422,
12.2545461305954));
#247199=CARTESIAN_POINT('Ctrl Pts',(-13.992532457489,-0.519514815600169,
12.0503312082537));
#247200=CARTESIAN_POINT('Ctrl Pts',(-14.,-0.251492536553737,12.));
#247201=CARTESIAN_POINT('Ctrl Pts',(-14.,7.11236625150491E-16,12.));
#247202=CARTESIAN_POINT('Origin',(-13.,-22.5166604983954,4.));
#247203=CARTESIAN_POINT('',(-21.,-22.5166604983954,8.));
#247204=CARTESIAN_POINT('Origin',(-13.,-22.5166604983954,8.));
#247205=CARTESIAN_POINT('',(-21.,-22.5166604983954,0.));
#247206=CARTESIAN_POINT('',(-21.,-22.5166604983954,4.));
#247207=CARTESIAN_POINT('Origin',(-13.,-22.5166604983954,0.));
#247208=CARTESIAN_POINT('Origin',(-13.,22.5166604983954,4.));
#247209=CARTESIAN_POINT('',(-21.,22.5166604983954,8.));
#247210=CARTESIAN_POINT('Origin',(-13.,22.5166604983954,8.));
#247211=CARTESIAN_POINT('',(-21.,22.5166604983954,0.));
#247212=CARTESIAN_POINT('',(-21.,22.5166604983954,4.));
#247213=CARTESIAN_POINT('Origin',(-13.,22.5166604983954,0.));
#247214=CARTESIAN_POINT('Origin',(26.,0.,4.));
#247215=CARTESIAN_POINT('',(18.,9.79717439317883E-16,8.));
#247216=CARTESIAN_POINT('Origin',(26.,0.,8.));
#247217=CARTESIAN_POINT('',(18.,9.79717439317883E-16,0.));
#247218=CARTESIAN_POINT('',(18.,9.79717439317883E-16,4.));
#247219=CARTESIAN_POINT('Origin',(26.,0.,0.));
#247220=CARTESIAN_POINT('Origin',(13.,22.5166604983954,4.));
#247221=CARTESIAN_POINT('',(5.,22.5166604983954,8.));
#247222=CARTESIAN_POINT('Origin',(13.,22.5166604983954,8.));
#247223=CARTESIAN_POINT('',(5.,22.5166604983954,0.));
#247224=CARTESIAN_POINT('',(5.,22.5166604983954,4.));
#247225=CARTESIAN_POINT('Origin',(13.,22.5166604983954,0.));
#247226=CARTESIAN_POINT('Origin',(-26.,3.18408167778312E-15,4.));
#247227=CARTESIAN_POINT('',(-34.,4.163799117101E-15,8.));
#247228=CARTESIAN_POINT('Origin',(-26.,3.18408167778312E-15,8.));
#247229=CARTESIAN_POINT('',(-34.,4.163799117101E-15,0.));
#247230=CARTESIAN_POINT('',(-34.,4.163799117101E-15,4.));
#247231=CARTESIAN_POINT('Origin',(-26.,3.18408167778312E-15,0.));
#247232=CARTESIAN_POINT('Origin',(13.,-22.5166604983954,4.));
#247233=CARTESIAN_POINT('',(5.,-22.5166604983954,8.));
#247234=CARTESIAN_POINT('Origin',(13.,-22.5166604983954,8.));
#247235=CARTESIAN_POINT('',(5.,-22.5166604983954,0.));
#247236=CARTESIAN_POINT('',(5.,-22.5166604983954,4.));
#247237=CARTESIAN_POINT('Origin',(13.,-22.5166604983954,0.));
#247238=CARTESIAN_POINT('Origin',(0.,0.,0.));
#247239=CARTESIAN_POINT('',(-14.,-1.71450551880629E-15,20.));
#247240=CARTESIAN_POINT('Origin',(0.,0.,20.));
#247241=CARTESIAN_POINT('',(-14.,-1.71450551880629E-15,0.));
#247242=CARTESIAN_POINT('',(-14.,1.71450551880629E-15,8.));
#247243=CARTESIAN_POINT('',(-14.,-1.71450551880629E-15,0.));
#247244=CARTESIAN_POINT('Origin',(0.,0.,8.));
#247245=CARTESIAN_POINT('Origin',(0.,0.,20.));
#247246=CARTESIAN_POINT('',(-6.,-7.34788079488412E-16,20.));
#247247=CARTESIAN_POINT('Origin',(0.,0.,20.));
#247248=CARTESIAN_POINT('Origin',(0.,0.,0.));
#247249=CARTESIAN_POINT('',(-6.,-7.34788079488412E-16,0.));
#247250=CARTESIAN_POINT('Origin',(0.,0.,0.));
#247251=CARTESIAN_POINT('',(-6.,-7.34788079488412E-16,0.));
#247252=CARTESIAN_POINT('',(-6.,-7.34788079488412E-16,0.));
#247253=CARTESIAN_POINT('Origin',(0.,0.,0.));
#247254=CARTESIAN_POINT('',(-45.,5.51091059616309E-15,8.));
#247255=CARTESIAN_POINT('Origin',(0.,0.,8.));
#247256=CARTESIAN_POINT('',(-45.,5.51091059616309E-15,0.));
#247257=CARTESIAN_POINT('',(-45.,-5.51091059616309E-15,0.));
#247258=CARTESIAN_POINT('Origin',(0.,0.,0.));
#247259=CARTESIAN_POINT('Origin',(0.,0.,8.));
#247260=CARTESIAN_POINT('Origin',(0.,0.,0.));
#247261=CARTESIAN_POINT('',(0.,0.,0.));
#247262=CARTESIAN_POINT('Origin',(0.,0.,31.));
#247263=CARTESIAN_POINT('',(-1.5,-1.83697019872103E-16,32.));
#247264=CARTESIAN_POINT('Origin',(0.,0.,32.));
#247265=CARTESIAN_POINT('',(-1.5,-1.83697019872103E-16,30.));
#247266=CARTESIAN_POINT('',(-1.5,-1.83697019872103E-16,31.));
#247267=CARTESIAN_POINT('Origin',(0.,0.,30.));
#247268=CARTESIAN_POINT('Origin',(5.5,0.,30.));
#247269=CARTESIAN_POINT('',(-2.,2.44929359829471E-16,30.));
#247270=CARTESIAN_POINT('Origin',(0.,0.,30.));
#247271=CARTESIAN_POINT('Origin',(1.5,0.,32.));
#247272=CARTESIAN_POINT('',(-2.,-2.44929359829471E-16,32.));
#247273=CARTESIAN_POINT('Origin',(0.,0.,32.));
#247274=CARTESIAN_POINT('Origin',(0.,0.,0.));
#247275=CARTESIAN_POINT('',(-2.,-2.44929359829471E-16,33.));
#247276=CARTESIAN_POINT('Origin',(0.,0.,33.));
#247277=CARTESIAN_POINT('',(-2.,-2.44929359829471E-16,0.));
#247278=CARTESIAN_POINT('Origin',(0.,0.,0.));
#247279=CARTESIAN_POINT('',(-3.5,-4.28626379701574E-16,0.));
#247280=CARTESIAN_POINT('Origin',(0.,0.,0.));
#247281=CARTESIAN_POINT('',(-2.,-2.44929359829471E-16,0.));
#247282=CARTESIAN_POINT('Origin',(0.,0.,0.));
#247283=CARTESIAN_POINT('Origin',(0.,0.,-2.));
#247284=CARTESIAN_POINT('',(-3.5,-4.28626379701574E-16,-2.));
#247285=CARTESIAN_POINT('',(-3.5,-4.28626379701574E-16,-2.));
#247286=CARTESIAN_POINT('Origin',(0.,0.,-2.));
#247287=CARTESIAN_POINT('Origin',(0.,0.,-2.));
#247288=CARTESIAN_POINT('Origin',(0.,0.,0.));
#247289=CARTESIAN_POINT('',(-2.,-2.44929359829471E-16,0.));
#247290=CARTESIAN_POINT('Origin',(0.,0.,33.));
#247291=CARTESIAN_POINT('',(0.,0.,0.));
#247292=CARTESIAN_POINT('Origin',(0.,0.,0.));
#247293=CARTESIAN_POINT('',(-2.,-2.44929359829471E-16,0.));
#247294=CARTESIAN_POINT('Origin',(0.,0.,0.));
#247295=CARTESIAN_POINT('',(-2.,-2.44929359829471E-16,2.));
#247296=CARTESIAN_POINT('',(-2.,-2.44929359829471E-16,0.));
#247297=CARTESIAN_POINT('Origin',(0.,0.,2.));
#247298=CARTESIAN_POINT('Origin',(0.,0.,0.));
#247299=CARTESIAN_POINT('',(-3.5,-4.28626379701574E-16,2.));
#247300=CARTESIAN_POINT('Origin',(0.,0.,2.));
#247301=CARTESIAN_POINT('',(-3.5,-4.28626379701574E-16,0.));
#247302=CARTESIAN_POINT('',(-3.5,-4.28626379701574E-16,0.));
#247303=CARTESIAN_POINT('Origin',(0.,0.,0.));
#247304=CARTESIAN_POINT('Origin',(0.,0.,2.));
#247305=CARTESIAN_POINT('Origin',(0.,0.,0.));
#247306=CARTESIAN_POINT('',(0.,0.,0.));
#247307=CARTESIAN_POINT('Origin',(-1.,0.,1.));
#247308=CARTESIAN_POINT('',(-1.,1.11803398874989,0.));
#247309=CARTESIAN_POINT('',(-1.,1.11803398874989,1.));
#247310=CARTESIAN_POINT('',(-1.,1.11803398874989,0.));
#247311=CARTESIAN_POINT('',(-1.,3.35410196624968,0.));
#247312=CARTESIAN_POINT('',(-1.,0.,0.));
#247313=CARTESIAN_POINT('',(-1.,3.35410196624968,1.));
#247314=CARTESIAN_POINT('',(-1.,3.35410196624968,0.));
#247315=CARTESIAN_POINT('',(-1.,0.,1.));
#247316=CARTESIAN_POINT('Origin',(1.,7.,1.));
#247317=CARTESIAN_POINT('',(1.,1.11803398874989,1.));
#247318=CARTESIAN_POINT('',(1.,1.11803398874989,0.));
#247319=CARTESIAN_POINT('',(1.,1.11803398874989,0.));
#247320=CARTESIAN_POINT('',(1.,3.35410196624968,1.));
#247321=CARTESIAN_POINT('',(1.,3.5,1.));
#247322=CARTESIAN_POINT('',(1.,3.35410196624968,0.));
#247323=CARTESIAN_POINT('',(1.,3.35410196624968,0.));
#247324=CARTESIAN_POINT('',(1.,3.5,0.));
#247325=CARTESIAN_POINT('Origin',(0.,0.,0.));
#247326=CARTESIAN_POINT('Origin',(0.,0.,0.));
#247327=CARTESIAN_POINT('Origin',(0.,0.,0.));
#247328=CARTESIAN_POINT('Origin',(0.,0.,0.));
#247329=CARTESIAN_POINT('Origin',(0.,0.,1.));
#247330=CARTESIAN_POINT('Origin',(0.,0.,0.));
#247331=CARTESIAN_POINT('Origin',(0.,0.,1.));
#247332=CARTESIAN_POINT('Origin',(0.,0.,1.));
#247333=CARTESIAN_POINT('',(0.,0.,0.));
#247334=CARTESIAN_POINT('Origin',(0.,0.,0.));
#247335=CARTESIAN_POINT('',(-6.,-7.34788079488412E-16,0.));
#247336=CARTESIAN_POINT('Origin',(0.,0.,0.));
#247337=CARTESIAN_POINT('',(-6.,-7.34788079488412E-16,4.));
#247338=CARTESIAN_POINT('',(-6.,-7.34788079488412E-16,0.));
#247339=CARTESIAN_POINT('Origin',(0.,0.,4.));
#247340=CARTESIAN_POINT('Origin',(0.,0.,0.));
#247341=CARTESIAN_POINT('',(-12.,-1.46957615897682E-15,4.));
#247342=CARTESIAN_POINT('Origin',(0.,0.,4.));
#247343=CARTESIAN_POINT('',(-12.,-1.46957615897682E-15,0.));
#247344=CARTESIAN_POINT('',(-12.,-1.46957615897682E-15,0.));
#247345=CARTESIAN_POINT('Origin',(0.,0.,0.));
#247346=CARTESIAN_POINT('Origin',(0.,0.,4.));
#247347=CARTESIAN_POINT('Origin',(0.,0.,0.));
#247348=CARTESIAN_POINT('',(0.,0.,0.));
#247349=CARTESIAN_POINT('Origin',(0.,0.,19.5));
#247350=CARTESIAN_POINT('',(-3.933,4.81653586104654E-16,19.067));
#247351=CARTESIAN_POINT('',(-3.72907923291372,-0.00301811260641736,19.2709195457389));
#247352=CARTESIAN_POINT('',(-3.5,4.28626379701574E-16,19.5));
#247353=CARTESIAN_POINT('',(-3.48351403049219,-1.825212838262,19.0672818680215));
#247354=CARTESIAN_POINT('Origin',(0.,0.,19.067));
#247355=CARTESIAN_POINT('',(-3.1771036721075,0.540490350682607,19.77725));
#247356=CARTESIAN_POINT('Ctrl Pts',(-3.17710367210751,0.54049035068261,
19.77725));
#247357=CARTESIAN_POINT('Ctrl Pts',(-3.16458988313419,0.636662782213618,
19.7734573799255));
#247358=CARTESIAN_POINT('Ctrl Pts',(-3.14759826787415,0.732018576300735,
19.7698475455261));
#247359=CARTESIAN_POINT('Ctrl Pts',(-3.12629674287792,0.826357140292361,
19.7663337451368));
#247360=CARTESIAN_POINT('Ctrl Pts',(-3.12487753074456,0.832642438395861,
19.7660996385107));
#247361=CARTESIAN_POINT('Ctrl Pts',(-3.12343917326921,0.838923233893048,
19.7658659581679));
#247362=CARTESIAN_POINT('Ctrl Pts',(-3.12198171393402,0.845199472642916,
19.7656326784525));
#247363=CARTESIAN_POINT('Ctrl Pts',(-3.09807584703403,0.948145005711887,
19.7618063255022));
#247364=CARTESIAN_POINT('Ctrl Pts',(-3.06903398719535,1.04986083335664,
19.7580872627407));
#247365=CARTESIAN_POINT('Ctrl Pts',(-3.03503853293981,1.15004696575645,
19.7543772677843));
#247366=CARTESIAN_POINT('Ctrl Pts',(-3.01733595934536,1.20221724618924,
19.7524453489384));
#247367=CARTESIAN_POINT('Ctrl Pts',(-2.9982896999218,1.25397207251287,19.7505161810263));
#247368=CARTESIAN_POINT('Ctrl Pts',(-2.97792340270646,1.30526499304348,
19.7485780811387));
#247369=CARTESIAN_POINT('Ctrl Pts',(-2.96193234297344,1.34553879183044,
19.7470563380971));
#247370=CARTESIAN_POINT('Ctrl Pts',(-2.94512745587406,1.38552777067492,
19.7455291174391));
#247371=CARTESIAN_POINT('Ctrl Pts',(-2.9275198572165,1.42520831898889,19.7439915130774));
#247372=CARTESIAN_POINT('Ctrl Pts',(-2.91989399705739,1.44239398515292,
19.7433255758266));
#247373=CARTESIAN_POINT('Ctrl Pts',(-2.9121206622458,1.4595147225641,19.7426579721191));
#247374=CARTESIAN_POINT('Ctrl Pts',(-2.90420365992811,1.476563460031,19.7419885589767));
#247375=CARTESIAN_POINT('Ctrl Pts',(-2.85856365692285,1.57484616830884,
19.7381295203403));
#247376=CARTESIAN_POINT('Ctrl Pts',(-2.80812532886755,1.67079266491046,
19.7342056102415));
#247377=CARTESIAN_POINT('Ctrl Pts',(-2.75316165124206,1.76405727156329,
19.7301686381061));
#247378=CARTESIAN_POINT('Ctrl Pts',(-2.69776993998212,1.85804818311921,
19.7261002277566));
#247379=CARTESIAN_POINT('Ctrl Pts',(-2.6377820652722,1.94931490144401,19.7219168766214));
#247380=CARTESIAN_POINT('Ctrl Pts',(-2.57346776037294,2.03749724942546,
19.7176028035755));
#247381=CARTESIAN_POINT('Ctrl Pts',(-2.5312628736305,2.09536502884201,19.7147717854282));
#247382=CARTESIAN_POINT('Ctrl Pts',(-2.48719471026825,2.15190447451021,
19.7118851719569));
#247383=CARTESIAN_POINT('Ctrl Pts',(-2.44133692549877,2.20701319668367,
19.7089464856767));
#247384=CARTESIAN_POINT('Ctrl Pts',(-2.43027421564794,2.22030759820611,
19.7082375584177));
#247385=CARTESIAN_POINT('Ctrl Pts',(-2.41910619342676,2.23351998459099,
19.7075255580821));
#247386=CARTESIAN_POINT('Ctrl Pts',(-2.40784488962212,2.24663635551648,
19.7068112829041));
#247387=CARTESIAN_POINT('Ctrl Pts',(-2.33286625983243,2.3339661653562,19.7020555836467));
#247388=CARTESIAN_POINT('Ctrl Pts',(-2.25365629340451,2.41715985411514,
19.697189593479));
#247389=CARTESIAN_POINT('Ctrl Pts',(-2.17061375920421,2.49590001164361,
19.6922695152463));
#247390=CARTESIAN_POINT('Ctrl Pts',(-2.09136398447513,2.5710439099646,19.6875741492468));
#247391=CARTESIAN_POINT('Ctrl Pts',(-2.00862409412524,2.64213271644402,
19.6828301060477));
#247392=CARTESIAN_POINT('Ctrl Pts',(-1.92269565758021,2.70890454420114,
19.6781146285172));
#247393=CARTESIAN_POINT('Ctrl Pts',(-1.83796886681413,2.77474261721767,
19.6734650934604));
#247394=CARTESIAN_POINT('Ctrl Pts',(-1.7501425366723,2.8363847262143,19.6688437473422));
#247395=CARTESIAN_POINT('Ctrl Pts',(-1.65945464450637,2.89357888006934,
19.664345873392));
#247396=CARTESIAN_POINT('Ctrl Pts',(-1.60622192399477,2.92715117218405,
19.6617056745609));
#247397=CARTESIAN_POINT('Ctrl Pts',(-1.55200223306352,2.95919081438473,
19.6591083913824));
#247398=CARTESIAN_POINT('Ctrl Pts',(-1.49683447506739,2.98964404084263,
19.6565758664662));
#247399=CARTESIAN_POINT('Ctrl Pts',(-1.4744877757989,3.00197967161917,19.6555500213939));
#247400=CARTESIAN_POINT('Ctrl Pts',(-1.45198543586043,3.01405496715234,
19.6545348200898));
#247401=CARTESIAN_POINT('Ctrl Pts',(-1.42932970158584,3.02586618074696,
19.6535317811723));
#247402=CARTESIAN_POINT('Ctrl Pts',(-1.41605565619611,3.03278639721237,
19.6529440984269));
#247403=CARTESIAN_POINT('Ctrl Pts',(-1.40273752971901,3.03961148194378,
19.6523609716114));
#247404=CARTESIAN_POINT('Ctrl Pts',(-1.38937624925342,3.04634086757255,
19.6517827066583));
#247405=CARTESIAN_POINT('Ctrl Pts',(-1.36924390684754,3.05648048675114,
19.6509113958534));
#247406=CARTESIAN_POINT('Ctrl Pts',(-1.34901337628808,3.06640295336509,
19.6500511133982));
#247407=CARTESIAN_POINT('Ctrl Pts',(-1.3286867018512,3.0761068082297,19.6492028638974));
#247408=CARTESIAN_POINT('Ctrl Pts',(-1.23897459210359,3.11893493022734,
19.645459100866));
#247409=CARTESIAN_POINT('Ctrl Pts',(-1.14738809682255,3.1575087790561,19.6419487793584));
#247410=CARTESIAN_POINT('Ctrl Pts',(-1.05419368277925,3.19185082210001,
19.6385663785593));
#247411=CARTESIAN_POINT('Ctrl Pts',(-1.04888030346469,3.19380879675978,
19.6383735346144));
#247412=CARTESIAN_POINT('Ctrl Pts',(-1.04356168380452,3.1957530126226,19.6381811064871));
#247413=CARTESIAN_POINT('Ctrl Pts',(-1.03823786832269,3.19768347263257,
19.6379890746212));
#247414=CARTESIAN_POINT('Ctrl Pts',(-0.936912661247142,3.23442483997126,
19.6343342393538));
#247415=CARTESIAN_POINT('Ctrl Pts',(-0.833710131733674,3.26618357112524,
19.6308224475133));
#247416=CARTESIAN_POINT('Ctrl Pts',(-0.728987945023351,3.2929368227092,
19.6273369064872));
#247417=CARTESIAN_POINT('Ctrl Pts',(-0.618230512283943,3.32123189136611,
19.62365049019));
#247418=CARTESIAN_POINT('Ctrl Pts',(-0.505772563389774,3.34392695068221,
19.619992753164));
#247419=CARTESIAN_POINT('Ctrl Pts',(-0.392069459542977,3.36095412422278,
19.6162548727429));
#247420=CARTESIAN_POINT('Ctrl Pts',(-0.342324351610006,3.36840351264678,
19.6146195500586));
#247421=CARTESIAN_POINT('Ctrl Pts',(-0.292341372829587,3.37476761591482,
19.6129693154895));
#247422=CARTESIAN_POINT('Ctrl Pts',(-0.242160814847883,3.38003919219647,
19.6112971801835));
#247423=CARTESIAN_POINT('Ctrl Pts',(-0.221494449192876,3.38221023866141,
19.610608527824));
#247424=CARTESIAN_POINT('Ctrl Pts',(-0.200794587116868,3.38419597077201,
19.6099161769195));
#247425=CARTESIAN_POINT('Ctrl Pts',(-0.180064107341896,3.38599585119609,
19.6092197082279));
#247426=CARTESIAN_POINT('Ctrl Pts',(-0.164827432646491,3.38731874351745,
19.6087078113976));
#247427=CARTESIAN_POINT('Ctrl Pts',(-0.149584229007586,3.3885403673882,
19.60819402712));
#247428=CARTESIAN_POINT('Ctrl Pts',(-0.134335760330162,3.38966089776966,
19.6076782142061));
#247429=CARTESIAN_POINT('Ctrl Pts',(-0.0228498841094028,3.39785341296919,
19.603906959801));
#247430=CARTESIAN_POINT('Ctrl Pts',(0.0889175554404967,3.40064237400044,
19.600024130958));
#247431=CARTESIAN_POINT('Ctrl Pts',(0.20049137098505,3.39809487625733,19.595995655425));
#247432=CARTESIAN_POINT('Ctrl Pts',(0.31333184657006,3.39551845762827,19.5919214459627));
#247433=CARTESIAN_POINT('Ctrl Pts',(0.425973809192178,3.38748379911017,
19.5876982574808));
#247434=CARTESIAN_POINT('Ctrl Pts',(0.537937125635622,3.37405655392717,
19.5833299866338));
#247435=CARTESIAN_POINT('Ctrl Pts',(0.649538927040108,3.36067266357876,
19.5789758203672));
#247436=CARTESIAN_POINT('Ctrl Pts',(0.760466169508123,3.34193148245174,
19.5744776729821));
#247437=CARTESIAN_POINT('Ctrl Pts',(0.87026043105589,3.31788976175756,19.56987672393));
#247438=CARTESIAN_POINT('Ctrl Pts',(0.918145898551613,3.3074042498682,19.5678700744642));
#247439=CARTESIAN_POINT('Ctrl Pts',(0.965816099665759,3.29591033247577,
19.565844335427));
#247440=CARTESIAN_POINT('Ctrl Pts',(1.01323416596061,3.28341171682478,19.5638050146634));
#247441=CARTESIAN_POINT('Ctrl Pts',(1.05147591420847,3.27333182638387,19.5621603421297));
#247442=CARTESIAN_POINT('Ctrl Pts',(1.08955368553102,3.2625984600994,19.5605068605029));
#247443=CARTESIAN_POINT('Ctrl Pts',(1.12744847290062,3.25121313328311,19.5588480276107));
#247444=CARTESIAN_POINT('Ctrl Pts',(1.14260692398368,3.24665884147706,19.5581844709847));
#247445=CARTESIAN_POINT('Ctrl Pts',(1.15773540097485,3.24200036908579,19.5575200931108));
#247446=CARTESIAN_POINT('Ctrl Pts',(1.17281990695688,3.23724205230611,19.5568557045379));
#247447=CARTESIAN_POINT('Ctrl Pts',(1.28139605346562,3.20299235924881,19.5520735292964));
#247448=CARTESIAN_POINT('Ctrl Pts',(1.38786500384221,3.16352193443418,19.5472812256798));
#247449=CARTESIAN_POINT('Ctrl Pts',(1.49184806016234,3.11899167315108,19.5425848250758));
#247450=CARTESIAN_POINT('Ctrl Pts',(1.59436475009484,3.07508937646806,19.5379546529925));
#247451=CARTESIAN_POINT('Ctrl Pts',(1.69446626847233,3.02627009263741,19.5334182553453));
#247452=CARTESIAN_POINT('Ctrl Pts',(1.79182717787839,2.9726309517123,19.5290953037484));
#247453=CARTESIAN_POINT('Ctrl Pts',(1.83747794464135,2.94748053018609,19.5270683500533));
#247454=CARTESIAN_POINT('Ctrl Pts',(1.88252662676428,2.92126953380817,19.5250885318974));
#247455=CARTESIAN_POINT('Ctrl Pts',(1.92694138741515,2.89400248501213,19.5231690444041));
#247456=CARTESIAN_POINT('Ctrl Pts',(2.01674297995926,2.83887161477934,19.5192880590911));
#247457=CARTESIAN_POINT('Ctrl Pts',(2.10395873229359,2.77942316276847,19.5156532043811));
#247458=CARTESIAN_POINT('Ctrl Pts',(2.18842314999436,2.71585528229139,19.5121545622288));
#247459=CARTESIAN_POINT('Ctrl Pts',(2.1929279567887,2.71246496684649,19.5119679664129));
#247460=CARTESIAN_POINT('Ctrl Pts',(2.19742493888665,2.70906292154206,19.5117817580525));
#247461=CARTESIAN_POINT('Ctrl Pts',(2.2019140715046,2.70564917233842,19.5115959204723));
#247462=CARTESIAN_POINT('Ctrl Pts',(2.23107014013917,2.68347751590652,19.5103889404821));
#247463=CARTESIAN_POINT('Ctrl Pts',(2.25989446870579,2.66081260713164,19.5091976772753));
#247464=CARTESIAN_POINT('Ctrl Pts',(2.28837856765338,2.63766240727529,19.5080178345747));
#247465=CARTESIAN_POINT('Ctrl Pts',(2.30709383064093,2.62245174256993,19.5072426278017));
#247466=CARTESIAN_POINT('Ctrl Pts',(2.32566732334985,2.60702707649191,19.5064721401425));
#247467=CARTESIAN_POINT('Ctrl Pts',(2.34406866120866,2.59141470798129,19.5057063550408));
#247468=CARTESIAN_POINT('Ctrl Pts',(2.42801257768479,2.52019361697664,19.5022129677061));
#247469=CARTESIAN_POINT('Ctrl Pts',(2.50846443703766,2.44499936367937,19.49881193032));
#247470=CARTESIAN_POINT('Ctrl Pts',(2.58523998813779,2.36616437098485,19.4954030721373));
#247471=CARTESIAN_POINT('Ctrl Pts',(2.66463705873511,2.28463753866887,19.4918778176792));
#247472=CARTESIAN_POINT('Ctrl Pts',(2.74010185284196,2.19921651126464,19.4883437781998));
#247473=CARTESIAN_POINT('Ctrl Pts',(2.81139933026821,2.11026813746333,19.4847193844267));
#247474=CARTESIAN_POINT('Ctrl Pts',(2.88320120511787,2.02069049412569,19.481069349706));
#247475=CARTESIAN_POINT('Ctrl Pts',(2.95077593728325,1.9275352101032,19.4773274483407));
#247476=CARTESIAN_POINT('Ctrl Pts',(3.01386241038701,1.83118227639482,19.4734442924964));
#247477=CARTESIAN_POINT('Ctrl Pts',(3.05935422153283,1.76170193856714,19.4706441392523));
#247478=CARTESIAN_POINT('Ctrl Pts',(3.10251176849141,1.69055902194563,19.4677712482316));
#247479=CARTESIAN_POINT('Ctrl Pts',(3.14323283105931,1.61789790696629,19.4648187786741));
#247480=CARTESIAN_POINT('Ctrl Pts',(3.15256575919984,1.60124458502554,19.4641420972597));
#247481=CARTESIAN_POINT('Ctrl Pts',(3.1617706898004,1.58451151903962,19.463461277159));
#247482=CARTESIAN_POINT('Ctrl Pts',(3.1708463718576,1.56770045508266,19.4627763103263));
#247483=CARTESIAN_POINT('Ctrl Pts',(3.17845206332653,1.5536122835364,19.46220228775));
#247484=CARTESIAN_POINT('Ctrl Pts',(3.18596647279068,1.53947016049922,19.4616253866984));
#247485=CARTESIAN_POINT('Ctrl Pts',(3.1933829871923,1.52528680237208,19.4610460963189));
#247486=CARTESIAN_POINT('Ctrl Pts',(3.24720725577905,1.42235315511455,19.4568419811125));
#247487=CARTESIAN_POINT('Ctrl Pts',(3.2959619462958,1.31709019069266,19.4525025542234));
#247488=CARTESIAN_POINT('Ctrl Pts',(3.33950590367559,1.2099581232903,19.4480571033869));
#247489=CARTESIAN_POINT('Ctrl Pts',(3.38315102057343,1.10257717110673,19.4436013250632));
#247490=CARTESIAN_POINT('Ctrl Pts',(3.42156183143616,0.993318922576536,
19.4390392975554));
#247491=CARTESIAN_POINT('Ctrl Pts',(3.45459938143664,0.882610076888688,
19.4344344860811));
#247492=CARTESIAN_POINT('Ctrl Pts',(3.48721345282509,0.773320308230192,
19.4298886995396));
#247493=CARTESIAN_POINT('Ctrl Pts',(3.51459215543077,0.662617111471497,
19.4253016032098));
#247494=CARTESIAN_POINT('Ctrl Pts',(3.5365922265338,0.550869944812617,19.420762333558));
#247495=CARTESIAN_POINT('Ctrl Pts',(3.55580037483495,0.453304071531322,
19.416799120701));
#247496=CARTESIAN_POINT('Ctrl Pts',(3.57090886825469,0.354941774153412,
19.4128729457123));
#247497=CARTESIAN_POINT('Ctrl Pts',(3.58180565188396,0.256001776248793,
19.4090574165951));
#247498=CARTESIAN_POINT('Ctrl Pts',(3.58371650043283,0.238651761982868,
19.4083883294108));
#247499=CARTESIAN_POINT('Ctrl Pts',(3.58549782885556,0.221282662292161,
19.407722627683));
#247500=CARTESIAN_POINT('Ctrl Pts',(3.58714748111238,0.20391333437368,19.4070614117152));
#247501=CARTESIAN_POINT('Ctrl Pts',(3.59490511742215,0.122232526567783,
19.4039519848771));
#247502=CARTESIAN_POINT('Ctrl Pts',(3.59976225922983,0.0404590842984835,
19.4009381638359));
#247503=CARTESIAN_POINT('Ctrl Pts',(3.60169878861074,-0.0412946177144568,
19.3980644912308));
#247504=CARTESIAN_POINT('Ctrl Pts',(3.60419581238684,-0.146710491970134,
19.3943590845945));
#247505=CARTESIAN_POINT('Ctrl Pts',(3.60183841423843,-0.252098971576584,
19.3908860908306));
#247506=CARTESIAN_POINT('Ctrl Pts',(3.5947512689982,-0.357225533988951,
19.3875428351193));
#247507=CARTESIAN_POINT('Ctrl Pts',(3.59431849705639,-0.363645019551776,
19.3873386813709));
#247508=CARTESIAN_POINT('Ctrl Pts',(3.59386807825058,-0.370063540736907,
19.387135011397));
#247509=CARTESIAN_POINT('Ctrl Pts',(3.59340003682488,-0.376481048737694,
19.3869318018183));
#247510=CARTESIAN_POINT('Ctrl Pts',(3.58507504193675,-0.49062846896029,
19.383317338204));
#247511=CARTESIAN_POINT('Ctrl Pts',(3.57117718051369,-0.60445132204649,
19.3798480308315));
#247512=CARTESIAN_POINT('Ctrl Pts',(3.55182373931981,-0.717609841555423,
19.3764084446653));
#247513=CARTESIAN_POINT('Ctrl Pts',(3.53219721908766,-0.832365039369245,
19.3729203255859));
#247514=CARTESIAN_POINT('Ctrl Pts',(3.50695892089234,-0.946437013077343,
19.3694623301513));
#247515=CARTESIAN_POINT('Ctrl Pts',(3.4762079922568,-1.05942782808591,19.3659376273442));
#247516=CARTESIAN_POINT('Ctrl Pts',(3.46821757599952,-1.08878771037984,
19.3650217576823));
#247517=CARTESIAN_POINT('Ctrl Pts',(3.45985488460338,-1.11807437117177,
19.3641015253591));
#247518=CARTESIAN_POINT('Ctrl Pts',(3.45112154213351,-1.14728036824038,
19.3631755415022));
#247519=CARTESIAN_POINT('Ctrl Pts',(3.44618411254059,-1.16379209381565,
19.3626520328784));
#247520=CARTESIAN_POINT('Ctrl Pts',(3.44113041057629,-1.18027058518833,
19.3621269237154));
#247521=CARTESIAN_POINT('Ctrl Pts',(3.43596296363524,-1.19670873142764,
19.3616001765408));
#247522=CARTESIAN_POINT('Ctrl Pts',(3.40077392169046,-1.30864846184167,
19.3580131579157));
#247523=CARTESIAN_POINT('Ctrl Pts',(3.36028536534138,-1.41880322069132,
19.3543445904448));
#247524=CARTESIAN_POINT('Ctrl Pts',(3.31473956815417,-1.52677068406583,
19.3505442698383));
#247525=CARTESIAN_POINT('Ctrl Pts',(3.26862550536591,-1.63608523541021,
19.3466965334086));
#247526=CARTESIAN_POINT('Ctrl Pts',(3.21732720295,-1.74315713587502,19.3427136455698));
#247527=CARTESIAN_POINT('Ctrl Pts',(3.16108829899971,-1.84756939818066,
19.3385806146842));
#247528=CARTESIAN_POINT('Ctrl Pts',(3.10490387238151,-1.95188051873053,
19.3344515873704));
#247529=CARTESIAN_POINT('Ctrl Pts',(3.04378877524706,-2.05353694145685,
19.3301727796814));
#247530=CARTESIAN_POINT('Ctrl Pts',(2.97797551513044,-2.15212844821212,
19.3257660626574));
#247531=CARTESIAN_POINT('Ctrl Pts',(2.94523482079766,-2.20117562169605,
19.3235738148514));
#247532=CARTESIAN_POINT('Ctrl Pts',(2.91133120733824,-2.24946438412975,
19.321350476985));
#247533=CARTESIAN_POINT('Ctrl Pts',(2.87629176279623,-2.29694484308792,
19.3191020230224));
#247534=CARTESIAN_POINT('Ctrl Pts',(2.85048071464791,-2.33192029513323,
19.3174457480944));
#247535=CARTESIAN_POINT('Ctrl Pts',(2.82405331952821,-2.366457154258,19.3157758898878));
#247536=CARTESIAN_POINT('Ctrl Pts',(2.79701991565477,-2.40053558605405,
19.3140955643857));
#247537=CARTESIAN_POINT('Ctrl Pts',(2.78698082964753,-2.41319090350478,
19.3134715611224));
#247538=CARTESIAN_POINT('Ctrl Pts',(2.77685873720404,-2.42578219237878,
19.3128461579201));
#247539=CARTESIAN_POINT('Ctrl Pts',(2.76666237134247,-2.4382986711196,19.3122200327859));
#247540=CARTESIAN_POINT('Ctrl Pts',(2.69091998260967,-2.53127571914085,
19.3075689429799));
#247541=CARTESIAN_POINT('Ctrl Pts',(2.61096786415274,-2.62026940316246,
19.3028686272558));
#247542=CARTESIAN_POINT('Ctrl Pts',(2.5271193507041,-2.70497870613519,19.2982109712535));
#247543=CARTESIAN_POINT('Ctrl Pts',(2.44454139689091,-2.78840440589686,
19.2936238928854));
#247544=CARTESIAN_POINT('Ctrl Pts',(2.35818486874117,-2.86767578697296,
19.2890786950165));
#247545=CARTESIAN_POINT('Ctrl Pts',(2.26829076229067,-2.9425204355399,19.284684468869));
#247546=CARTESIAN_POINT('Ctrl Pts',(2.18040734951895,-3.01569100704323,
19.2803885299518));
#247547=CARTESIAN_POINT('Ctrl Pts',(2.08914318404235,-3.08463203363021,
19.2762373832327));
#247548=CARTESIAN_POINT('Ctrl Pts',(1.99466030529637,-3.14908455620803,
19.2723461432594));
#247549=CARTESIAN_POINT('Ctrl Pts',(1.93019574293449,-3.19305975802495,
19.2696911957679));
#247550=CARTESIAN_POINT('Ctrl Pts',(1.86422998226858,-3.2349460604959,19.2671574695618));
#247551=CARTESIAN_POINT('Ctrl Pts',(1.79684706521249,-3.27471586875336,
19.2647057148294));
#247552=CARTESIAN_POINT('Ctrl Pts',(1.76306020003609,-3.29465708246733,
19.2634763660537));
#247553=CARTESIAN_POINT('Ctrl Pts',(1.72891707848498,-3.314065937121,19.2622676486185));
#247554=CARTESIAN_POINT('Ctrl Pts',(1.69442865360166,-3.33293762892873,
19.2610747934098));
#247555=CARTESIAN_POINT('Ctrl Pts',(1.67966120721037,-3.34101821532914,
19.2605640300042));
#247556=CARTESIAN_POINT('Ctrl Pts',(1.66483933557783,-3.34899543928581,
19.260056483811));
#247557=CARTESIAN_POINT('Ctrl Pts',(1.64996551745785,-3.35686853107841,
19.2595518258176));
#247558=CARTESIAN_POINT('Ctrl Pts',(1.54790692001615,-3.41089075317367,
19.25608905072));
#247559=CARTESIAN_POINT('Ctrl Pts',(1.44338102079118,-3.46002494558198,
19.2527598044352));
#247560=CARTESIAN_POINT('Ctrl Pts',(1.33675738679763,-3.50423623360503,
19.2494544540736));
#247561=CARTESIAN_POINT('Ctrl Pts',(1.22748680308684,-3.5495450743183,19.2460670478311));
#247562=CARTESIAN_POINT('Ctrl Pts',(1.11601262685197,-3.5896826848128,19.2427043407588));
#247563=CARTESIAN_POINT('Ctrl Pts',(1.00274554376078,-3.62457714481419,
19.2392742583058));
#247564=CARTESIAN_POINT('Ctrl Pts',(0.887418485001359,-3.66010622642493,
19.23578179333));
#247565=CARTESIAN_POINT('Ctrl Pts',(0.770232609504335,-3.6901989429599,
19.2322191475815));
#247566=CARTESIAN_POINT('Ctrl Pts',(0.651638599037863,-3.71475692682424,
19.2285212596192));
#247567=CARTESIAN_POINT('Ctrl Pts',(0.557481316903401,-3.73425464855801,
19.2255853349565));
#247568=CARTESIAN_POINT('Ctrl Pts',(0.462436821599179,-3.75026305735668,
19.2225647675566));
#247569=CARTESIAN_POINT('Ctrl Pts',(0.366737966434126,-3.76272714493643,
19.2194428580875));
#247570=CARTESIAN_POINT('Ctrl Pts',(0.348578568571863,-3.76509227589814,
19.2188504581466));
#247571=CARTESIAN_POINT('Ctrl Pts',(0.330395625607895,-3.76732977506375,
19.2182544512168));
#247572=CARTESIAN_POINT('Ctrl Pts',(0.312190750748018,-3.76943925243843,
19.2176547827206));
#247573=CARTESIAN_POINT('Ctrl Pts',(0.295454775339816,-3.77137852209772,
19.2171034997658));
#247574=CARTESIAN_POINT('Ctrl Pts',(0.27870457594682,-3.77320905523334,
19.2165492635453));
#247575=CARTESIAN_POINT('Ctrl Pts',(0.261950803658832,-3.77492987456066,
19.2159923650463));
#247576=CARTESIAN_POINT('Ctrl Pts',(0.140494854890857,-3.78740490051092,
19.2119551467765));
#247577=CARTESIAN_POINT('Ctrl Pts',(0.0187071285680933,-3.79413133586308,
19.2077701623785));
#247578=CARTESIAN_POINT('Ctrl Pts',(-0.102919377231485,-3.79515191457483,
19.2034528248801));
#247579=CARTESIAN_POINT('Ctrl Pts',(-0.225323696673865,-3.7961790199893,
19.1991078775775));
#247580=CARTESIAN_POINT('Ctrl Pts',(-0.347564405183152,-3.7914276864069,
19.1946290698833));
#247581=CARTESIAN_POINT('Ctrl Pts',(-0.469169014359218,-3.78093380970734,
19.1900682371697));
#247582=CARTESIAN_POINT('Ctrl Pts',(-0.588890599908213,-3.77060242863931,
19.1855780280601));
#247583=CARTESIAN_POINT('Ctrl Pts',(-0.707995692757366,-3.75470586367773,
19.1810086717632));
#247584=CARTESIAN_POINT('Ctrl Pts',(-0.826064256043132,-3.73325957207986,
19.1764402466238));
#247585=CARTESIAN_POINT('Ctrl Pts',(-0.893094062371818,-3.72108409765832,
19.173846663338));
#247586=CARTESIAN_POINT('Ctrl Pts',(-0.95979036063892,-3.70711950966395,
19.1712539125421));
#247587=CARTESIAN_POINT('Ctrl Pts',(-1.02608048299624,-3.69136401974347,
19.1686804513533));
#247588=CARTESIAN_POINT('Ctrl Pts',(-1.0731344302124,-3.68018048342282,
19.166853761303));
#247589=CARTESIAN_POINT('Ctrl Pts',(-1.1199837936364,-3.66809454403529,
19.1650368471905));
#247590=CARTESIAN_POINT('Ctrl Pts',(-1.16660340215532,-3.65510416442421,
19.1632370478864));
#247591=CARTESIAN_POINT('Ctrl Pts',(-1.18354551570129,-3.65038330782828,
19.1625829796705));
#247592=CARTESIAN_POINT('Ctrl Pts',(-1.20044812808266,-3.64554552754666,
19.1619315314114));
#247593=CARTESIAN_POINT('Ctrl Pts',(-1.21730683248261,-3.64059209559565,
19.1612831921432));
#247594=CARTESIAN_POINT('Ctrl Pts',(-1.33463995018198,-3.6061172272822,
19.1567708840881));
#247595=CARTESIAN_POINT('Ctrl Pts',(-1.4498950175503,-3.56603139636547,
19.1524063055148));
#247596=CARTESIAN_POINT('Ctrl Pts',(-1.56273946469582,-3.5204123978789,
19.1483174993703));
#247597=CARTESIAN_POINT('Ctrl Pts',(-1.57762987331034,-3.51439273501348,
19.1477779602456));
#247598=CARTESIAN_POINT('Ctrl Pts',(-1.5924783670239,-3.50827662342372,
19.1472432353143));
#247599=CARTESIAN_POINT('Ctrl Pts',(-1.60728423194846,-3.50206414269901,
19.1467136283624));
#247600=CARTESIAN_POINT('Ctrl Pts',(-1.71029567872433,-3.45884095845543,
19.1430289008153));
#247601=CARTESIAN_POINT('Ctrl Pts',(-1.81124821300518,-3.41095457478404,
19.139591140223));
#247602=CARTESIAN_POINT('Ctrl Pts',(-1.90996741658097,-3.35860925792791,
19.1362930132009));
#247603=CARTESIAN_POINT('Ctrl Pts',(-1.91638568915619,-3.35520600405785,
19.1360785840174));
#247604=CARTESIAN_POINT('Ctrl Pts',(-1.9227945286344,-3.35178388555094,
19.1358647450661));
#247605=CARTESIAN_POINT('Ctrl Pts',(-1.92919388980695,-3.34834295154984,
19.1356514668496));
#247606=CARTESIAN_POINT('Ctrl Pts',(-2.03589817023458,-3.2909681016724,
19.1320952214654));
#247607=CARTESIAN_POINT('Ctrl Pts',(-2.13996474276898,-3.22836590874485,
19.1286943674431));
#247608=CARTESIAN_POINT('Ctrl Pts',(-2.2411130948938,-3.16077460424877,
19.1253278844567));
#247609=CARTESIAN_POINT('Ctrl Pts',(-2.30453714555583,-3.11839216073272,
19.1232169653662));
#247610=CARTESIAN_POINT('Ctrl Pts',(-2.36681264127981,-3.07404780448213,
19.1211199056681));
#247611=CARTESIAN_POINT('Ctrl Pts',(-2.42785977746311,-3.02779966215665,
19.1190112222297));
#247612=CARTESIAN_POINT('Ctrl Pts',(-2.44551288664286,-3.01442600440831,
19.1184014504813));
#247613=CARTESIAN_POINT('Ctrl Pts',(-2.4630632314328,-3.00089315573997,
19.1177907308758));
#247614=CARTESIAN_POINT('Ctrl Pts',(-2.48050876672247,-2.98720253689442,
19.1171785080672));
#247615=CARTESIAN_POINT('Ctrl Pts',(-2.49385060611702,-2.97673234868774,
19.1167102978202));
#247616=CARTESIAN_POINT('Ctrl Pts',(-2.50713106880999,-2.96616986439984,
19.116241209721));
#247617=CARTESIAN_POINT('Ctrl Pts',(-2.52033810050941,-2.95552493019762,
19.1157714081302));
#247618=CARTESIAN_POINT('Ctrl Pts',(-2.61722856965942,-2.87743072308156,
19.1123248125906));
#247619=CARTESIAN_POINT('Ctrl Pts',(-2.71032158081448,-2.79478006848099,
19.1088315555871));
#247620=CARTESIAN_POINT('Ctrl Pts',(-2.79933067258955,-2.70796263286715,
19.1052196678753));
#247621=CARTESIAN_POINT('Ctrl Pts',(-2.8882857381335,-2.62119789320547,
19.1016099724865));
#247622=CARTESIAN_POINT('Ctrl Pts',(-2.97316127057925,-2.53027135578799,
19.0978817066295));
#247623=CARTESIAN_POINT('Ctrl Pts',(-3.05366149423723,-2.43556820923745,
19.0939993569848));
#247624=CARTESIAN_POINT('Ctrl Pts',(-3.13423505475908,-2.34077878675562,
19.0901134704636));
#247625=CARTESIAN_POINT('Ctrl Pts',(-3.21042506006765,-2.24220613355532,
19.0860732072219));
#247626=CARTESIAN_POINT('Ctrl Pts',(-3.28193146579411,-2.14023119209007,
19.081880080732));
#247627=CARTESIAN_POINT('Ctrl Pts',(-3.35343787152057,-2.03825625062482,
19.0776869542421));
#247628=CARTESIAN_POINT('Ctrl Pts',(-3.4202607872896,-1.93287950230611,
19.0733410316596));
#247629=CARTESIAN_POINT('Ctrl Pts',(-3.48209799042183,-1.8244708936356,
19.0688805084781));
#247630=CARTESIAN_POINT('',(-3.22275,-3.50678552687464E-13,19.77725));
#247631=CARTESIAN_POINT('Origin',(0.,0.,19.77725));
#247632=CARTESIAN_POINT('',(-3.,-3.67394039744206E-16,20.));
#247633=CARTESIAN_POINT('',(-3.5,4.28626379701574E-16,19.5));
#247634=CARTESIAN_POINT('Origin',(0.,0.,20.));
#247635=CARTESIAN_POINT('',(-1.54513563095215,-2.82819261091993,19.77725));
#247636=CARTESIAN_POINT('Origin',(0.,0.,19.77725));
#247637=CARTESIAN_POINT('Ctrl Pts',(-3.72907923291372,-0.00301811260641736,
19.2709195457389));
#247638=CARTESIAN_POINT('Ctrl Pts',(-3.71732607315158,-0.0973557598520273,
19.2825963499489));
#247639=CARTESIAN_POINT('Ctrl Pts',(-3.70184284765992,-0.19102707851843,
19.2944247832023));
#247640=CARTESIAN_POINT('Ctrl Pts',(-3.68258976228466,-0.283865185503344,
19.3064858466733));
#247641=CARTESIAN_POINT('Ctrl Pts',(-3.65909155554632,-0.397173208015436,
19.3212062593969));
#247642=CARTESIAN_POINT('Ctrl Pts',(-3.62997830197441,-0.509247625521539,
19.3362734645736));
#247643=CARTESIAN_POINT('Ctrl Pts',(-3.59537764216538,-0.619795875562299,
19.3515911252785));
#247644=CARTESIAN_POINT('Ctrl Pts',(-3.56079454951504,-0.730287998966675,
19.3669010090283));
#247645=CARTESIAN_POINT('Ctrl Pts',(-3.52072781136372,-0.839255856288323,
19.3824605958806));
#247646=CARTESIAN_POINT('Ctrl Pts',(-3.47527674613691,-0.946329469354909,
19.3981826910836));
#247647=CARTESIAN_POINT('Ctrl Pts',(-3.46098767994945,-0.97999164946893,
19.4031254588239));
#247648=CARTESIAN_POINT('Ctrl Pts',(-3.44616634251706,-1.01346601192478,
19.4080843853173));
#247649=CARTESIAN_POINT('Ctrl Pts',(-3.43081567631547,-1.04673941322125,
19.4130570670775));
#247650=CARTESIAN_POINT('Ctrl Pts',(-3.42493621336561,-1.05948346794626,
19.4149616553075));
#247651=CARTESIAN_POINT('Ctrl Pts',(-3.41897973743929,-1.0721965657576,
19.4168680465519));
#247652=CARTESIAN_POINT('Ctrl Pts',(-3.41295050270049,-1.08486973062788,
19.4187748651731));
#247653=CARTESIAN_POINT('Ctrl Pts',(-3.3645837579527,-1.18653432936764,
19.4340714348914));
#247654=CARTESIAN_POINT('Ctrl Pts',(-3.31146599038082,-1.28578496005253,
19.4494162238301));
#247655=CARTESIAN_POINT('Ctrl Pts',(-3.25379544256635,-1.38229577327628,
19.4647593594095));
#247656=CARTESIAN_POINT('Ctrl Pts',(-3.19622520881502,-1.47863871239134,
19.4800758066301));
#247657=CARTESIAN_POINT('Ctrl Pts',(-3.13411702103349,-1.57225100599859,
19.4953903618227));
#247658=CARTESIAN_POINT('Ctrl Pts',(-3.0676673887165,-1.66276180456701,
19.5106791453749));
#247659=CARTESIAN_POINT('Ctrl Pts',(-3.0021465554394,-1.75200748939619,
19.5257542301151));
#247660=CARTESIAN_POINT('Ctrl Pts',(-2.93240420076956,-1.83823724984042,
19.5408041109178));
#247661=CARTESIAN_POINT('Ctrl Pts',(-2.85863980690601,-1.92105686787767,
19.5558337677679));
#247662=CARTESIAN_POINT('Ctrl Pts',(-2.81383532908736,-1.97136148701632,
19.5649627782795));
#247663=CARTESIAN_POINT('Ctrl Pts',(-2.76754725817361,-2.02040726935002,
19.574084881253));
#247664=CARTESIAN_POINT('Ctrl Pts',(-2.71982338200487,-2.06810000982114,
19.5832066378075));
#247665=CARTESIAN_POINT('Ctrl Pts',(-2.69328594074255,-2.09462013770045,
19.5882789013831));
#247666=CARTESIAN_POINT('Ctrl Pts',(-2.6663045863994,-2.12072182447228,
19.5933511331322));
#247667=CARTESIAN_POINT('Ctrl Pts',(-2.63888788001173,-2.14638835604203,
19.5984250385703));
#247668=CARTESIAN_POINT('Ctrl Pts',(-2.62778918242003,-2.1567785563853,
19.6004790322656));
#247669=CARTESIAN_POINT('Ctrl Pts',(-2.61662239946336,-2.16709434556364,
19.6025326982287));
#247670=CARTESIAN_POINT('Ctrl Pts',(-2.60539419598218,-2.17732943764041,
19.6045850921466));
#247671=CARTESIAN_POINT('Ctrl Pts',(-2.52605958296763,-2.2496470680111,
19.6190865996673));
#247672=CARTESIAN_POINT('Ctrl Pts',(-2.44357065075068,-2.31802061246615,
19.6335390243701));
#247673=CARTESIAN_POINT('Ctrl Pts',(-2.35818713366859,-2.38218174582851,
19.6480100794366));
#247674=CARTESIAN_POINT('Ctrl Pts',(-2.27399720972799,-2.44544595796592,
19.6622788407505));
#247675=CARTESIAN_POINT('Ctrl Pts',(-2.18699327598033,-2.50461492306674,
19.6765659173718));
#247676=CARTESIAN_POINT('Ctrl Pts',(-2.09740996719078,-2.55941822033091,
19.6909593237566));
#247677=CARTESIAN_POINT('Ctrl Pts',(-2.01001005421766,-2.61288580794571,
19.7050019225668));
#247678=CARTESIAN_POINT('Ctrl Pts',(-1.92015522309492,-2.66219835190401,
19.7191460218339));
#247679=CARTESIAN_POINT('Ctrl Pts',(-1.82804613218824,-2.7070875228198,
19.7334918463878));
#247680=CARTESIAN_POINT('Ctrl Pts',(-1.74640674880859,-2.74687430388468,
19.7462070329033));
#247681=CARTESIAN_POINT('Ctrl Pts',(-1.66299749211945,-2.7831858303728,
19.7590809473144));
#247682=CARTESIAN_POINT('Ctrl Pts',(-1.57794048331916,-2.81581954168268,
19.7721933359912));
#247683=CARTESIAN_POINT('Ctrl Pts',(-1.56703248807982,-2.82000459794824,
19.773874912563));
#247684=CARTESIAN_POINT('Ctrl Pts',(-1.55609743761987,-2.8241291126961,
19.7755604111672));
#247685=CARTESIAN_POINT('Ctrl Pts',(-1.54513563095217,-2.82819261092003,
19.7772499999999));
#247686=CARTESIAN_POINT('Origin',(0.,0.,-2.31077344927308));
#247687=CARTESIAN_POINT('',(-3.22274978348675,0.00118132810417647,1.06077344921939));
#247688=CARTESIAN_POINT('',(-3.22274921729244,0.00224609459589272,0.814226550726902));
#247689=CARTESIAN_POINT('',(-3.22275,-3.50678552687464E-13,-2.31077344927308));
#247690=CARTESIAN_POINT('',(-1.87152083515305,-2.62364771379239,7.67940544457724E-5));
#247691=CARTESIAN_POINT('Ctrl Pts',(-1.87152083515305,-2.62364771379239,
7.67940544461609E-5));
#247692=CARTESIAN_POINT('Ctrl Pts',(-1.79128701262451,-2.68088072939763,
0.00619382745291832));
#247693=CARTESIAN_POINT('Ctrl Pts',(-1.70827916512899,-2.73453404989049,
0.01231086085139));
#247694=CARTESIAN_POINT('Ctrl Pts',(-1.62285367642187,-2.78432460525421,
0.0184278942498621));
#247695=CARTESIAN_POINT('Ctrl Pts',(-1.53753803913513,-2.83405113331987,
0.0245370615557027));
#247696=CARTESIAN_POINT('Ctrl Pts',(-1.44981131701081,-2.8799245447086,
0.0306462288615435));
#247697=CARTESIAN_POINT('Ctrl Pts',(-1.36006067539097,-2.92170370191008,
0.0367553961673841));
#247698=CARTESIAN_POINT('Ctrl Pts',(-1.27012268459411,-2.96357007064094,
0.0428773160000743));
#247699=CARTESIAN_POINT('Ctrl Pts',(-1.17815268266129,-3.00132481674489,
0.0489992358327648));
#247700=CARTESIAN_POINT('Ctrl Pts',(-1.08456726970077,-3.03477040317613,
0.0551211556654549));
#247701=CARTESIAN_POINT('Ctrl Pts',(-0.991325256568774,-3.0680932652609,
0.0612206118881195));
#247702=CARTESIAN_POINT('Ctrl Pts',(-0.896480082078013,-3.09713837625361,
0.0673200681107845));
#247703=CARTESIAN_POINT('Ctrl Pts',(-0.800464647125199,-3.12175814425185,
0.073419524333449));
#247704=CARTESIAN_POINT('Ctrl Pts',(-0.704476256382932,-3.14637097771721,
0.0795172625513117));
#247705=CARTESIAN_POINT('Ctrl Pts',(-0.607318688578545,-3.16656083456988,
0.0856150007691736));
#247706=CARTESIAN_POINT('Ctrl Pts',(-0.509439092134675,-3.18223025155393,
0.0917127389870362));
#247707=CARTESIAN_POINT('Ctrl Pts',(-0.4115597591698,-3.19789962635798,
0.09781046079059));
#247708=CARTESIAN_POINT('Ctrl Pts',(-0.312958838800098,-3.20904851669443,
0.103908182594144));
#247709=CARTESIAN_POINT('Ctrl Pts',(-0.214091622340587,-3.21563093960479,
0.110005904397697));
#247710=CARTESIAN_POINT('Ctrl Pts',(-0.114544904462395,-3.22225860264495,
0.116145535043885));
#247711=CARTESIAN_POINT('Ctrl Pts',(-0.0147286687435439,-3.22425674435509,
0.122285165690072));
#247712=CARTESIAN_POINT('Ctrl Pts',(0.0848907776275571,-3.22163174779083,
0.12842479633626));
#247713=CARTESIAN_POINT('Ctrl Pts',(0.183965536554572,-3.21902110387278,
0.134530857435074));
#247714=CARTESIAN_POINT('Ctrl Pts',(0.282845212155482,-3.2118378409206,
0.140636918533888));
#247715=CARTESIAN_POINT('Ctrl Pts',(0.381076252659278,-3.20014038007072,
0.146742979632702));
#247716=CARTESIAN_POINT('Ctrl Pts',(0.480117366510128,-3.18834645479153,
0.152899395052576));
#247717=CARTESIAN_POINT('Ctrl Pts',(0.578498646385012,-3.17196361674406,
0.15905581047245));
#247718=CARTESIAN_POINT('Ctrl Pts',(0.675767254513531,-3.15110396214204,
0.165212225892324));
#247719=CARTESIAN_POINT('Ctrl Pts',(0.773035862642052,-3.13024430754001,
0.171368641312199));
#247720=CARTESIAN_POINT('Ctrl Pts',(0.869191376290511,-3.1049080144529,
0.177525056732073));
#247721=CARTESIAN_POINT('Ctrl Pts',(0.963799540515554,-3.07525738893544,
0.183681472151948));
#247722=CARTESIAN_POINT('Ctrl Pts',(1.0588688509138,-3.04546223812672,0.18986789563122));
#247723=CARTESIAN_POINT('Ctrl Pts',(1.15271366098345,-3.01120482551079,
0.196054319110491));
#247724=CARTESIAN_POINT('Ctrl Pts',(1.24488592317186,-2.97260434649291,
0.202240742589763));
#247725=CARTESIAN_POINT('Ctrl Pts',(1.33693776245938,-2.93405429893401,
0.208419083517474));
#247726=CARTESIAN_POINT('Ctrl Pts',(1.42732100254314,-2.89117263032656,
0.214597424445185));
#247727=CARTESIAN_POINT('Ctrl Pts',(1.51560286257366,-2.84412825404526,
0.220775765372896));
#247728=CARTESIAN_POINT('Ctrl Pts',(1.60379510779988,-2.79713163245073,
0.226947834674558));
#247729=CARTESIAN_POINT('Ctrl Pts',(1.68988983509325,-2.7459809074072,0.23311990397622));
#247730=CARTESIAN_POINT('Ctrl Pts',(1.77347523023534,-2.69089263446941,
0.239291973277882));
#247731=CARTESIAN_POINT('Ctrl Pts',(1.85700387082497,-2.63584176651452,
0.245459851739382));
#247732=CARTESIAN_POINT('Ctrl Pts',(1.93802620718757,-2.57685890354785,
0.251627730200881));
#247733=CARTESIAN_POINT('Ctrl Pts',(2.01615675376923,-2.51420554186222,
0.25779560866238));
#247734=CARTESIAN_POINT('Ctrl Pts',(2.09426018272848,-2.45157392596335,
0.263961346370915));
#247735=CARTESIAN_POINT('Ctrl Pts',(2.16947347983138,-2.38527461311472,
0.27012708407945));
#247736=CARTESIAN_POINT('Ctrl Pts',(2.24144250557063,-2.31561073082702,
0.276292821787985));
#247737=CARTESIAN_POINT('Ctrl Pts',(2.31340554305196,-2.24595264499537,
0.282458046469877));
#247738=CARTESIAN_POINT('Ctrl Pts',(2.38212453560621,-2.17293084695873,
0.288623271151769));
#247739=CARTESIAN_POINT('Ctrl Pts',(2.44728135326857,-2.0968861534294,0.294788495833661));
#247740=CARTESIAN_POINT('Ctrl Pts',(2.51244994239862,-2.02082772138913,
0.30095483434747));
#247741=CARTESIAN_POINT('Ctrl Pts',(2.57405479696641,-1.94174563691404,
0.30712117286128));
#247742=CARTESIAN_POINT('Ctrl Pts',(2.63181795262218,-1.86001393187137,
0.313287511375088));
#247743=CARTESIAN_POINT('Ctrl Pts',(2.68964329587142,-1.77819423478622,
0.319460488545465));
#247744=CARTESIAN_POINT('Ctrl Pts',(2.74361843185147,-1.6937195746257,0.325633465715842));
#247745=CARTESIAN_POINT('Ctrl Pts',(2.79350871979648,-1.60699302889622,
0.331806442886218));
#247746=CARTESIAN_POINT('Ctrl Pts',(2.8434276369906,-1.52021671564714,0.337982962383338));
#247747=CARTESIAN_POINT('Ctrl Pts',(2.88925683988024,-1.43118632719822,
0.344159481880458));
#247748=CARTESIAN_POINT('Ctrl Pts',(2.93080860004921,-1.34032776304067,
0.350336001377578));
#247749=CARTESIAN_POINT('Ctrl Pts',(2.97242830962644,-1.24932061827797,
0.356522621309513));
#247750=CARTESIAN_POINT('Ctrl Pts',(3.00975644428611,-1.15647972746503,
0.362709241241448));
#247751=CARTESIAN_POINT('Ctrl Pts',(3.04265413891859,-1.06224919553822,
0.368895861173383));
#247752=CARTESIAN_POINT('Ctrl Pts',(3.06516591177251,-0.997767585068575,
0.37312934270445));
#247753=CARTESIAN_POINT('Ctrl Pts',(3.08560412160844,-0.93263559411187,
0.377362824235516));
#247754=CARTESIAN_POINT('Ctrl Pts',(3.10393805760351,-0.86699832586953,
0.381596305766583));
#247755=CARTESIAN_POINT('Ctrl Pts',(3.13064891965725,-0.771370850237589,
0.387764099807853));
#247756=CARTESIAN_POINT('Ctrl Pts',(3.15298395288961,-0.674337722705913,
0.393931893849122));
#247757=CARTESIAN_POINT('Ctrl Pts',(3.17079708643209,-0.576336185896548,
0.400099687890392));
#247758=CARTESIAN_POINT('Ctrl Pts',(3.18858597964063,-0.478468010798811,
0.406259088720728));
#247759=CARTESIAN_POINT('Ctrl Pts',(3.20186512627604,-0.379634469888541,
0.412418489551064));
#247760=CARTESIAN_POINT('Ctrl Pts',(3.21053835167315,-0.280287450550098,
0.4185778903814));
#247761=CARTESIAN_POINT('Ctrl Pts',(3.21920234703497,-0.18104615618158,
0.424730736385312));
#247762=CARTESIAN_POINT('Ctrl Pts',(3.22327012806913,-0.081292900734927,
0.430883582389223));
#247763=CARTESIAN_POINT('Ctrl Pts',(3.22269683317995,0.0185117236352813,
0.437036428393134));
#247764=CARTESIAN_POINT('Ctrl Pts',(3.22212396099534,0.118242759572707,
0.443184737750598));
#247765=CARTESIAN_POINT('Ctrl Pts',(3.21691681880613,0.218024655391256,
0.449333047108062));
#247766=CARTESIAN_POINT('Ctrl Pts',(3.20708255632381,0.317394138924411,
0.455481356465526));
#247767=CARTESIAN_POINT('Ctrl Pts',(3.1972520475349,0.416725693576094,0.461627319041176));
#247768=CARTESIAN_POINT('Ctrl Pts',(3.18279797050033,0.515644716249514,
0.467773281616825));
#247769=CARTESIAN_POINT('Ctrl Pts',(3.16377947627986,0.613691280669986,
0.473919244192474));
#247770=CARTESIAN_POINT('Ctrl Pts',(3.14476313435015,0.711726749326874,
0.480064511239952));
#247771=CARTESIAN_POINT('Ctrl Pts',(3.12118348507223,0.808889528923773,
0.486209778287429));
#247772=CARTESIAN_POINT('Ctrl Pts',(3.09315094070796,0.904729142062675,
0.492355045334906));
#247773=CARTESIAN_POINT('Ctrl Pts',(3.06511404127982,1.00058364459696,0.49850126709524));
#247774=CARTESIAN_POINT('Ctrl Pts',(3.03262299497265,1.09511415479859,0.504647488855574));
#247775=CARTESIAN_POINT('Ctrl Pts',(2.99583800178979,1.18788561298308,0.510793710615907));
#247776=CARTESIAN_POINT('Ctrl Pts',(2.95901401252014,1.28075541898609,0.516946448038645));
#247777=CARTESIAN_POINT('Ctrl Pts',(2.91788714758439,1.37186204419843,0.523099185461383));
#247778=CARTESIAN_POINT('Ctrl Pts',(2.87266562126227,1.46079081011549,0.529251922884121));
#247779=CARTESIAN_POINT('Ctrl Pts',(2.82741878839573,1.54976934170717,0.535408103457402));
#247780=CARTESIAN_POINT('Ctrl Pts',(2.77807294608138,1.63656720882083,0.541564284030684));
#247781=CARTESIAN_POINT('Ctrl Pts',(2.72488105641269,1.72079655709305,0.547720464603965));
#247782=CARTESIAN_POINT('Ctrl Pts',(2.67160150018635,1.80516472534443,0.553886791294679));
#247783=CARTESIAN_POINT('Ctrl Pts',(2.61446348552986,1.88695556308096,0.560053117985394));
#247784=CARTESIAN_POINT('Ctrl Pts',(2.55376191401101,1.96581221103309,0.566219444676109));
#247785=CARTESIAN_POINT('Ctrl Pts',(2.51014725235934,2.02247146932511,0.570650009577805));
#247786=CARTESIAN_POINT('Ctrl Pts',(2.46469374932749,2.07761661373107,0.575080574479501));
#247787=CARTESIAN_POINT('Ctrl Pts',(2.41752243029318,2.1311271340606,0.579511139381198));
#247788=CARTESIAN_POINT('Ctrl Pts',(2.35174975841072,2.20573878300207,0.585688835860732));
#247789=CARTESIAN_POINT('Ctrl Pts',(2.28240614186831,2.27743157497007,0.591866532340266));
#247790=CARTESIAN_POINT('Ctrl Pts',(2.20978063521303,2.34584464676106,0.598044228819799));
#247791=CARTESIAN_POINT('Ctrl Pts',(2.13725244314113,2.41416604842284,0.604213647491896));
#247792=CARTESIAN_POINT('Ctrl Pts',(2.06145141495303,2.47921617061427,0.610383066163992));
#247793=CARTESIAN_POINT('Ctrl Pts',(1.9827059515682,2.54066815466248,0.616552484836088));
#247794=CARTESIAN_POINT('Ctrl Pts',(1.90404285857504,2.60205585787751,0.622715450089655));
#247795=CARTESIAN_POINT('Ctrl Pts',(1.82244179393401,2.65985264087373,0.628878415343223));
#247796=CARTESIAN_POINT('Ctrl Pts',(1.73826629504038,2.71377004368951,0.63504138059679));
#247797=CARTESIAN_POINT('Ctrl Pts',(1.65415124531696,2.76764872666042,0.641199920024072));
#247798=CARTESIAN_POINT('Ctrl Pts',(1.56746580117371,2.81765333547917,0.647358459451355));
#247799=CARTESIAN_POINT('Ctrl Pts',(1.47860397401242,2.86353764608302,0.653516998878637));
#247800=CARTESIAN_POINT('Ctrl Pts',(1.38977507297627,2.90940495509461,0.659673256371748));
#247801=CARTESIAN_POINT('Ctrl Pts',(1.29877177613583,2.95115480101006,0.66582951386486));
#247802=CARTESIAN_POINT('Ctrl Pts',(1.2060135139842,2.9885864495757,0.671985771357971));
#247803=CARTESIAN_POINT('Ctrl Pts',(1.11326493675272,3.02601418989081,0.678141386074247));
#247804=CARTESIAN_POINT('Ctrl Pts',(1.01876216053388,3.05912446716541,0.684297000790522));
#247805=CARTESIAN_POINT('Ctrl Pts',(0.922944527480625,3.08776471929025,
0.690452615506798));
#247806=CARTESIAN_POINT('Ctrl Pts',(0.827111400001406,3.11640960275748,
0.696609225631888));
#247807=CARTESIAN_POINT('Ctrl Pts',(0.729963408681899,3.14058290113278,
0.702765835756979));
#247808=CARTESIAN_POINT('Ctrl Pts',(0.631954016389179,3.16018222317473,
0.708922445882069));
#247809=CARTESIAN_POINT('Ctrl Pts',(0.533840905623936,3.17980228620586,
0.715085571241905));
#247810=CARTESIAN_POINT('Ctrl Pts',(0.434864999483574,3.19483862244009,
0.721248696601742));
#247811=CARTESIAN_POINT('Ctrl Pts',(0.33548876722234,3.20524021713937,0.727411821961578));
#247812=CARTESIAN_POINT('Ctrl Pts',(0.23605676392719,3.21564764932793,0.733578406135113));
#247813=CARTESIAN_POINT('Ctrl Pts',(0.136224419780004,3.22141513477925,
0.739744990308648));
#247814=CARTESIAN_POINT('Ctrl Pts',(0.0364560542900044,3.2225437962277,
0.745911574482183));
#247815=CARTESIAN_POINT('Ctrl Pts',(-0.0634751617003769,3.22367429997436,
0.75208822428437));
#247816=CARTESIAN_POINT('Ctrl Pts',(-0.163341757182965,3.22015087153828,
0.758264874086558));
#247817=CARTESIAN_POINT('Ctrl Pts',(-0.262682585611081,3.21202668446523,
0.764441523888745));
#247818=CARTESIAN_POINT('Ctrl Pts',(-0.332293457323671,3.20633384142113,
0.768769673591109));
#247819=CARTESIAN_POINT('Ctrl Pts',(-0.401646275419367,3.19838303131296,
0.773097823293472));
#247820=CARTESIAN_POINT('Ctrl Pts',(-0.470585672091414,3.18820744113715,
0.777425972995835));
#247821=CARTESIAN_POINT('Ctrl Pts',(-0.568975958136059,3.173684841921,0.783603106939803));
#247822=CARTESIAN_POINT('Ctrl Pts',(-0.666863183878244,3.15457832544767,
0.789780240883771));
#247823=CARTESIAN_POINT('Ctrl Pts',(-0.763787336524841,3.13093380113095,
0.795957374827739));
#247824=CARTESIAN_POINT('Ctrl Pts',(-0.860581873702995,3.10732089634364,
0.802126248167018));
#247825=CARTESIAN_POINT('Ctrl Pts',(-0.956415480169123,3.07918214831494,
0.808295121506298));
#247826=CARTESIAN_POINT('Ctrl Pts',(-1.05083523750127,3.04661498488497,
0.814463994845578));
#247827=CARTESIAN_POINT('Ctrl Pts',(-1.14515649358677,3.01408179640144,
0.820626432649208));
#247828=CARTESIAN_POINT('Ctrl Pts',(-1.23806642539856,2.97712951833294,
0.826788870452837));
#247829=CARTESIAN_POINT('Ctrl Pts',(-1.32912518798289,2.93590595850232,
0.832951308256467));
#247830=CARTESIAN_POINT('Ctrl Pts',(-1.42011898523278,2.89471180937613,
0.839109349505372));
#247831=CARTESIAN_POINT('Ctrl Pts',(-1.50926384531011,2.84925261556918,
0.845267390754277));
#247832=CARTESIAN_POINT('Ctrl Pts',(-1.59613875285414,2.79972474435206,
0.851425432003182));
#247833=CARTESIAN_POINT('Ctrl Pts',(-1.6829817249642,2.75021507970466,0.857581209540673));
#247834=CARTESIAN_POINT('Ctrl Pts',(-1.76755602643768,2.69663992421653,
0.863736987078165));
#247835=CARTESIAN_POINT('Ctrl Pts',(-1.84946495672966,2.63924173510669,
0.869892764615657));
#247836=CARTESIAN_POINT('Ctrl Pts',(-1.93136558545734,2.58184936336933,
0.876047918258016));
#247837=CARTESIAN_POINT('Ctrl Pts',(-2.0106010251037,2.52063497727754,0.882203071900374));
#247838=CARTESIAN_POINT('Ctrl Pts',(-2.08680413946703,2.45588396427911,
0.888358225542733));
#247839=CARTESIAN_POINT('Ctrl Pts',(-2.1630198194789,2.39112227404683,0.894514394150136));
#247840=CARTESIAN_POINT('Ctrl Pts',(-2.23620185057499,2.32282307924975,
0.900670562757539));
#247841=CARTESIAN_POINT('Ctrl Pts',(-2.30601749120835,2.25131092760222,
0.906826731364942));
#247842=CARTESIAN_POINT('Ctrl Pts',(-2.3759073959641,2.17972270722374,0.912989448396951));
#247843=CARTESIAN_POINT('Ctrl Pts',(-2.44242345656973,2.10491501642267,
0.919152165428961));
#247844=CARTESIAN_POINT('Ctrl Pts',(-2.50527112082526,2.02724793097908,
0.92531488246097));
#247845=CARTESIAN_POINT('Ctrl Pts',(-2.5681542409122,1.94953702925177,0.93148107622133));
#247846=CARTESIAN_POINT('Ctrl Pts',(-2.62736458637439,1.86896386958431,
0.93764726998169));
#247847=CARTESIAN_POINT('Ctrl Pts',(-2.68265033179356,1.78591846393611,
0.94381346374205));
#247848=CARTESIAN_POINT('Ctrl Pts',(-2.73802662326239,1.7027370479408,0.949989756389243));
#247849=CARTESIAN_POINT('Ctrl Pts',(-2.78946525347622,1.61707567059967,
0.956166049036436));
#247850=CARTESIAN_POINT('Ctrl Pts',(-2.83675978469182,1.52935002090928,
0.962342341683629));
#247851=CARTESIAN_POINT('Ctrl Pts',(-2.86993806495115,1.46780831372772,
0.966675163325904));
#247852=CARTESIAN_POINT('Ctrl Pts',(-2.90107785822629,1.40525120745208,
0.971007984968179));
#247853=CARTESIAN_POINT('Ctrl Pts',(-2.93012223651133,1.34182757521295,
0.975340806610454));
#247854=CARTESIAN_POINT('Ctrl Pts',(-2.97519609107558,1.24340069385822,
0.98206489519793));
#247855=CARTESIAN_POINT('Ctrl Pts',(-3.01535773768093,1.14258916682412,
0.988788983785406));
#247856=CARTESIAN_POINT('Ctrl Pts',(-3.05037101870565,1.0398818253728,0.995513072372882));
#247857=CARTESIAN_POINT('Ctrl Pts',(-3.08525396049592,0.937556818734572,
1.00221213009969));
#247858=CARTESIAN_POINT('Ctrl Pts',(-3.11502664347812,0.83335035784085,
1.0089111878265));
#247859=CARTESIAN_POINT('Ctrl Pts',(-3.13950132278114,0.727769885853671,
1.01561024555331));
#247860=CARTESIAN_POINT('Ctrl Pts',(-3.16391653004058,0.622445968257002,
1.02229302496047));
#247861=CARTESIAN_POINT('Ctrl Pts',(-3.18305930980102,0.515754989028655,
1.02897580436762));
#247862=CARTESIAN_POINT('Ctrl Pts',(-3.19679113100839,0.408220561958983,
1.03565858377478));
#247863=CARTESIAN_POINT('Ctrl Pts',(-3.21047458455517,0.301064903924503,
1.04231782439555));
#247864=CARTESIAN_POINT('Ctrl Pts',(-3.21878502250993,0.193072023646205,
1.04897706501631));
#247865=CARTESIAN_POINT('Ctrl Pts',(-3.22163478414336,0.0847754687252713,
1.05563630563708));
#247866=CARTESIAN_POINT('Ctrl Pts',(-3.22236758214641,0.0569277013004861,
1.05734868683118));
#247867=CARTESIAN_POINT('Ctrl Pts',(-3.22273956433623,0.0290599208778919,
1.05906106802528));
#247868=CARTESIAN_POINT('Ctrl Pts',(-3.22274978348675,0.00118132810417647,
1.06077344921939));
#247869=CARTESIAN_POINT('',(1.87158653173903,-2.62360084935058,0.));
#247870=CARTESIAN_POINT('Origin',(0.,0.,0.));
#247871=CARTESIAN_POINT('Ctrl Pts',(1.87158653173902,-2.62360084935058,
-3.99680288865056E-15));
#247872=CARTESIAN_POINT('Ctrl Pts',(1.95492543847218,-2.56414974212509,
0.00631946307768746));
#247873=CARTESIAN_POINT('Ctrl Pts',(2.03548387446147,-2.50068513957169,
0.0126389261553787));
#247874=CARTESIAN_POINT('Ctrl Pts',(2.11287029831822,-2.43349474315945,
0.0189583892330702));
#247875=CARTESIAN_POINT('Ctrl Pts',(2.19021266751125,-2.36634259700056,
0.0252742547569941));
#247876=CARTESIAN_POINT('Ctrl Pts',(2.26438631500752,-2.29546914473324,
0.0315901202809182));
#247877=CARTESIAN_POINT('Ctrl Pts',(2.33503251876323,-2.22120253439848,
0.0379059858048421));
#247878=CARTESIAN_POINT('Ctrl Pts',(2.40565481867404,-2.14696105290915,
0.0442197142929191));
#247879=CARTESIAN_POINT('Ctrl Pts',(2.47275177340866,-2.06932899274331,
0.0505334427809963));
#247880=CARTESIAN_POINT('Ctrl Pts',(2.53600172914556,-1.98867111214267,
0.0568471712690735));
#247881=CARTESIAN_POINT('Ctrl Pts',(2.59926252374806,-1.90799940955721,
0.0631619817129206));
#247882=CARTESIAN_POINT('Ctrl Pts',(2.65867474659795,-1.82430116432855,
0.0694767921567673));
#247883=CARTESIAN_POINT('Ctrl Pts',(2.71395737767804,-1.7379737957308,0.0757916026006145));
#247884=CARTESIAN_POINT('Ctrl Pts',(2.7692484525325,-1.65163324163867,0.0821073775577904));
#247885=CARTESIAN_POINT('Ctrl Pts',(2.82040846123542,-1.56266310548976,
0.0884231525149662));
#247886=CARTESIAN_POINT('Ctrl Pts',(2.86720056961815,-1.4714885171422,0.0947389274721422));
#247887=CARTESIAN_POINT('Ctrl Pts',(2.91400965186176,-1.38028085516681,
0.101056993479864));
#247888=CARTESIAN_POINT('Ctrl Pts',(2.95644749454226,-1.28686750908988,
0.107375059487585));
#247889=CARTESIAN_POINT('Ctrl Pts',(2.99432422469011,-1.19169627000087,
0.113693125495307));
#247890=CARTESIAN_POINT('Ctrl Pts',(3.0322226534121,-1.09647050983308,0.120014810955479));
#247891=CARTESIAN_POINT('Ctrl Pts',(3.06555461802173,-0.999485227527157,
0.126336496415651));
#247892=CARTESIAN_POINT('Ctrl Pts',(3.09417939463669,-0.901205546091291,
0.132658181875823));
#247893=CARTESIAN_POINT('Ctrl Pts',(3.12284606342699,-0.802782032977649,
0.138989119081756));
#247894=CARTESIAN_POINT('Ctrl Pts',(3.14679167349174,-0.703060726745416,
0.14532005628769));
#247895=CARTESIAN_POINT('Ctrl Pts',(3.16592605622274,-0.602519517551057,
0.151650993493623));
#247896=CARTESIAN_POINT('Ctrl Pts',(3.18507609504922,-0.501896043734193,
0.157987110786045));
#247897=CARTESIAN_POINT('Ctrl Pts',(3.19940700326259,-0.400451730043345,
0.164323228078468));
#247898=CARTESIAN_POINT('Ctrl Pts',(3.208880426794,-0.298670335049077,0.17065934537089));
#247899=CARTESIAN_POINT('Ctrl Pts',(3.21837017823093,-0.196713514877829,
0.17700638326916));
#247900=CARTESIAN_POINT('Ctrl Pts',(3.22298570268855,-0.0944188568314729,
0.183353421167431));
#247901=CARTESIAN_POINT('Ctrl Pts',(3.22274073245243,0.00772877040364258,
0.189700459065702));
#247902=CARTESIAN_POINT('Ctrl Pts',(3.2226368829715,0.0510319007561665,
0.192391139377135));
#247903=CARTESIAN_POINT('Ctrl Pts',(3.22166017418701,0.0943086603682532,
0.195081819688569));
#247904=CARTESIAN_POINT('Ctrl Pts',(3.21981445683011,0.137522456667455,
0.197772500000002));
#247905=CARTESIAN_POINT('Ctrl Pts',(3.21562008643828,0.235725286606468,
0.203887038496331));
#247906=CARTESIAN_POINT('Ctrl Pts',(3.20691991595699,0.333942178358137,
0.21000157699266));
#247907=CARTESIAN_POINT('Ctrl Pts',(3.19370248745656,0.431719798148999,
0.216116115488989));
#247908=CARTESIAN_POINT('Ctrl Pts',(3.18050477959944,0.529351531955746,
0.222221530982858));
#247909=CARTESIAN_POINT('Ctrl Pts',(3.16280326081571,0.626544861148386,
0.228326946476726));
#247910=CARTESIAN_POINT('Ctrl Pts',(3.14063845087156,0.722846929444312,
0.234432361970594));
#247911=CARTESIAN_POINT('Ctrl Pts',(3.11849984119223,0.819035162354429,
0.240530560461333));
#247912=CARTESIAN_POINT('Ctrl Pts',(3.09190852211019,0.914333798479899,
0.246628758952073));
#247913=CARTESIAN_POINT('Ctrl Pts',(3.06095661357545,1.00829666879779,0.252726957442812));
#247914=CARTESIAN_POINT('Ctrl Pts',(3.0300317624365,1.10217739908968,0.258819825038688));
#247915=CARTESIAN_POINT('Ctrl Pts',(2.99475403662924,1.19472426481479,0.264912692634564));
#247916=CARTESIAN_POINT('Ctrl Pts',(2.95526602375376,1.28550390561313,0.27100556023044));
#247917=CARTESIAN_POINT('Ctrl Pts',(2.91579631979057,1.37624145575259,0.277095602822721));
#247918=CARTESIAN_POINT('Ctrl Pts',(2.87212038204646,1.46521300198972,0.283185645415002));
#247919=CARTESIAN_POINT('Ctrl Pts',(2.82442945658175,1.55200380389139,0.289275688007284));
#247920=CARTESIAN_POINT('Ctrl Pts',(2.77674728024902,1.63877868359877,0.295364613351662));
#247921=CARTESIAN_POINT('Ctrl Pts',(2.7250517932753,1.72337322507659,0.301453538696042));
#247922=CARTESIAN_POINT('Ctrl Pts',(2.66958033235958,1.80539702325526,0.307542464040421));
#247923=CARTESIAN_POINT('Ctrl Pts',(2.61410350441056,1.88742875748696,0.313631978506926));
#247924=CARTESIAN_POINT('Ctrl Pts',(2.55485022641688,1.96688888746183,0.319721492973432));
#247925=CARTESIAN_POINT('Ctrl Pts',(2.49210067160407,2.04341669883813,0.325811007439938));
#247926=CARTESIAN_POINT('Ctrl Pts',(2.42928653909573,2.1200232675812,0.331906788832358));
#247927=CARTESIAN_POINT('Ctrl Pts',(2.36296922687978,2.19369114808772,0.338002570224777));
#247928=CARTESIAN_POINT('Ctrl Pts',(2.29346849125129,2.2640936027774,0.344098351617197));
#247929=CARTESIAN_POINT('Ctrl Pts',(2.22393109264782,2.3345331961162,0.350197348651562));
#247930=CARTESIAN_POINT('Ctrl Pts',(2.15120725402708,2.40170363400882,0.356296345685926));
#247931=CARTESIAN_POINT('Ctrl Pts',(2.07565116067855,2.46531738761438,0.36239534272029));
#247932=CARTESIAN_POINT('Ctrl Pts',(1.99996714770689,2.52903884196289,0.368504665611479));
#247933=CARTESIAN_POINT('Ctrl Pts',(1.92144165573973,2.5891913161499,0.374613988502668));
#247934=CARTESIAN_POINT('Ctrl Pts',(1.84045931761003,2.64552963746816,0.380723311393857));
#247935=CARTESIAN_POINT('Ctrl Pts',(1.77496951785463,2.69109000861698,0.385663874262568));
#247936=CARTESIAN_POINT('Ctrl Pts',(1.70787361394654,2.73415678273328,0.39060443713128));
#247937=CARTESIAN_POINT('Ctrl Pts',(1.6393860656107,2.77462265729621,0.395544999999991));
#247938=CARTESIAN_POINT('Ctrl Pts',(1.55363981683965,2.8252858366817,0.401730573043608));
#247939=CARTESIAN_POINT('Ctrl Pts',(1.46539703945234,2.87205664003861,0.407916146087224));
#247940=CARTESIAN_POINT('Ctrl Pts',(1.37504551440431,2.91468135407914,0.414101719130841));
#247941=CARTESIAN_POINT('Ctrl Pts',(1.28481470585698,2.95724911826387,0.420279027779005));
#247942=CARTESIAN_POINT('Ctrl Pts',(1.19248113794149,2.99568162203976,0.42645633642717));
#247943=CARTESIAN_POINT('Ctrl Pts',(1.09845941233454,3.02976970774243,0.432633645075335));
#247944=CARTESIAN_POINT('Ctrl Pts',(1.00453588072825,3.06382219267849,0.438804502292774));
#247945=CARTESIAN_POINT('Ctrl Pts',(0.908928101182369,3.0935391345434,0.444975359510213));
#247946=CARTESIAN_POINT('Ctrl Pts',(0.812072143685353,3.11875879092152,
0.451146216727652));
#247947=CARTESIAN_POINT('Ctrl Pts',(0.715286187601124,3.1439602201134,0.457312614036434));
#247948=CARTESIAN_POINT('Ctrl Pts',(0.617254264392215,3.16467071848417,
0.463479011345218));
#247949=CARTESIAN_POINT('Ctrl Pts',(0.518428299268892,3.18077815337964,
0.469645408654));
#247950=CARTESIAN_POINT('Ctrl Pts',(0.419639277575774,3.1968795669436,0.475809500820927));
#247951=CARTESIAN_POINT('Ctrl Pts',(0.32005722994316,3.20838126724278,0.481973592987853));
#247952=CARTESIAN_POINT('Ctrl Pts',(0.220144143290919,3.21522225027675,
0.48813768515478));
#247953=CARTESIAN_POINT('Ctrl Pts',(0.120242016159254,3.2220624829196,0.494301101179099));
#247954=CARTESIAN_POINT('Ctrl Pts',(0.0200093533601731,3.22424298544074,
0.500464517203419));
#247955=CARTESIAN_POINT('Ctrl Pts',(-0.0800878465952649,3.22175472364482,
0.506627933227738));
#247956=CARTESIAN_POINT('Ctrl Pts',(-0.18020050520609,3.21926607757061,
0.512792301108097));
#247957=CARTESIAN_POINT('Ctrl Pts',(-0.280177227367024,3.21210724569945,
0.518956668988456));
#247958=CARTESIAN_POINT('Ctrl Pts',(-0.37955411058339,3.20032127131625,
0.525121036868815));
#247959=CARTESIAN_POINT('Ctrl Pts',(-0.47903394953257,3.18852308651157,
0.531291791113808));
#247960=CARTESIAN_POINT('Ctrl Pts',(-0.577912278700772,3.17208823786559,
0.537462545358803));
#247961=CARTESIAN_POINT('Ctrl Pts',(-0.675732526357839,3.15111140953824,
0.543633299603796));
#247962=CARTESIAN_POINT('Ctrl Pts',(-0.773606755744829,3.13012300522831,
0.549807459155943));
#247963=CARTESIAN_POINT('Ctrl Pts',(-0.870421322734032,3.10458773902362,
0.555981618708089));
#247964=CARTESIAN_POINT('Ctrl Pts',(-0.965733991792374,3.07465045486422,
0.562155778260236));
#247965=CARTESIAN_POINT('Ctrl Pts',(-1.06119901609093,3.04466531660353,
0.568339807072902));
#247966=CARTESIAN_POINT('Ctrl Pts',(-1.15515694141851,3.01026425460189,
0.574523835885568));
#247967=CARTESIAN_POINT('Ctrl Pts',(-1.24718462932257,2.97164063488194,
0.580707864698233));
#247968=CARTESIAN_POINT('Ctrl Pts',(-1.3097347681446,2.94538861410085,0.58491107646549));
#247969=CARTESIAN_POINT('Ctrl Pts',(-1.37139362992841,2.9171868686106,0.589114288232746));
#247970=CARTESIAN_POINT('Ctrl Pts',(-1.43203530093296,2.88710797501269,
0.593317500000002));
#247971=CARTESIAN_POINT('Ctrl Pts',(-1.52129718861555,2.8428331590738,0.599504443902765));
#247972=CARTESIAN_POINT('Ctrl Pts',(-1.60865229565399,2.79434124124621,
0.605691387805528));
#247973=CARTESIAN_POINT('Ctrl Pts',(-1.69367664058628,2.74182001590775,
0.611878331708291));
#247974=CARTESIAN_POINT('Ctrl Pts',(-1.77859006068519,2.6893673110404,0.618057203973193));
#247975=CARTESIAN_POINT('Ctrl Pts',(-1.86117839897765,2.6328959738107,0.624236076238095));
#247976=CARTESIAN_POINT('Ctrl Pts',(-1.94104052614948,2.5726405186783,0.630414948502997));
#247977=CARTESIAN_POINT('Ctrl Pts',(-2.02082172249445,2.51244612532799,
0.636587559211149));
#247978=CARTESIAN_POINT('Ctrl Pts',(-2.09788185801057,2.44847549797177,
0.642760169919301));
#247979=CARTESIAN_POINT('Ctrl Pts',(-2.17184795978842,2.38100693028451,
0.648932780627453));
#247980=CARTESIAN_POINT('Ctrl Pts',(-2.24576396690791,2.31358405670262,
0.655101210841876));
#247981=CARTESIAN_POINT('Ctrl Pts',(-2.31658978840695,2.24266824334093,
0.6612696410563));
#247982=CARTESIAN_POINT('Ctrl Pts',(-2.38398548044491,2.16857805751323,
0.667438071270724));
#247983=CARTESIAN_POINT('Ctrl Pts',(-2.4513578618263,2.09451349781718,0.673604367963643));
#247984=CARTESIAN_POINT('Ctrl Pts',(-2.51530218115938,2.01727706684051,
0.679770664656563));
#247985=CARTESIAN_POINT('Ctrl Pts',(-2.57551596160632,1.93722355292596,
0.685936961349482));
#247986=CARTESIAN_POINT('Ctrl Pts',(-2.63572479590579,1.85717661485638,
0.692102751523585));
#247987=CARTESIAN_POINT('Ctrl Pts',(-2.69220344112948,1.77431339925425,
0.698268541697687));
#247988=CARTESIAN_POINT('Ctrl Pts',(-2.74469087675724,1.68902029400051,
0.70443433187179));
#247989=CARTESIAN_POINT('Ctrl Pts',(-2.79718784336744,1.60371170071465,
0.710601241666945));
#247990=CARTESIAN_POINT('Ctrl Pts',(-2.84569193412304,1.51597270901757,
0.716768151462101));
#247991=CARTESIAN_POINT('Ctrl Pts',(-2.88998699003919,1.42621623883065,
0.722935061257257));
#247992=CARTESIAN_POINT('Ctrl Pts',(-2.93432967906764,1.33636324816448,
0.729108602697882));
#247993=CARTESIAN_POINT('Ctrl Pts',(-2.97445410399483,1.24448883502799,
0.735282144138506));
#247994=CARTESIAN_POINT('Ctrl Pts',(-3.01019143545741,1.15102783823802,
0.741455685579131));
#247995=CARTESIAN_POINT('Ctrl Pts',(-3.04594929758766,1.05751314922794,
0.747632773645164));
#247996=CARTESIAN_POINT('Ctrl Pts',(-3.07731491134282,0.962410471336915,
0.753809861711195));
#247997=CARTESIAN_POINT('Ctrl Pts',(-3.10416934776438,0.866169857995585,
0.759986949777228));
#247998=CARTESIAN_POINT('Ctrl Pts',(-3.13106756177693,0.769772355038621,
0.766174107614626));
#247999=CARTESIAN_POINT('Ctrl Pts',(-3.15343981370364,0.672233632573876,
0.772361265452025));
#248000=CARTESIAN_POINT('Ctrl Pts',(-3.17121828160923,0.574014087708131,
0.778548423289423));
#248001=CARTESIAN_POINT('Ctrl Pts',(-3.18323079876677,0.507649315773298,
0.782728948859614));
#248002=CARTESIAN_POINT('Ctrl Pts',(-3.19314714429896,0.440973884319493,
0.786909474429804));
#248003=CARTESIAN_POINT('Ctrl Pts',(-3.2009598565266,0.374130404277991,
0.791089999999995));
#248004=CARTESIAN_POINT('Ctrl Pts',(-3.21537265460941,0.250818351700129,
0.798802183575631));
#248005=CARTESIAN_POINT('Ctrl Pts',(-3.22266251386311,0.126650208984342,
0.806514367151267));
#248006=CARTESIAN_POINT('Ctrl Pts',(-3.22274921729245,0.00224609459589272,
0.814226550726902));
#248007=CARTESIAN_POINT('Origin',(0.,0.,-2.31077344927308));
#248008=CARTESIAN_POINT('',(-3.22275,1.20843135519762E-10,2.31096825019553));
#248009=CARTESIAN_POINT('',(-3.22275,-8.28983494685339E-13,2.06147698899067));
#248010=CARTESIAN_POINT('',(-3.22275,-3.50678552687464E-13,-2.31077344927308));
#248011=CARTESIAN_POINT('Ctrl Pts',(-3.22275,1.20843127171533E-10,2.31096825019553));
#248012=CARTESIAN_POINT('Ctrl Pts',(-3.22274999999303,0.185834148167105,
2.30055492199149));
#248013=CARTESIAN_POINT('Ctrl Pts',(-3.20667711875127,0.371301546871853,
2.29005533248189));
#248014=CARTESIAN_POINT('Ctrl Pts',(-3.16694702710074,0.598835624703661,
2.27638194280519));
#248015=CARTESIAN_POINT('Ctrl Pts',(-3.15824378544306,0.64315897761156,
2.27368177435837));
#248016=CARTESIAN_POINT('Ctrl Pts',(-3.14386419459536,0.70903539333966,
2.26960698121429));
#248017=CARTESIAN_POINT('Ctrl Pts',(-3.13889091598327,0.730737327962122,
2.26825455001991));
#248018=CARTESIAN_POINT('Ctrl Pts',(-3.12955360841005,0.769627304868333,
2.26581211517507));
#248019=CARTESIAN_POINT('Ctrl Pts',(-3.12527178862818,0.786834292470408,
2.26472477396117));
#248020=CARTESIAN_POINT('Ctrl Pts',(-3.1158281473904,0.82349100290969,2.26239369798068));
#248021=CARTESIAN_POINT('Ctrl Pts',(-3.11062573776534,0.842929395817087,
2.2611486999294));
#248022=CARTESIAN_POINT('Ctrl Pts',(-3.09596489022453,0.895723729794777,
2.25774250956016));
#248023=CARTESIAN_POINT('Ctrl Pts',(-3.08614988448032,0.928977040919678,
2.25556993721904));
#248024=CARTESIAN_POINT('Ctrl Pts',(-3.02080416833628,1.13789274972979,
2.24174391301209));
#248025=CARTESIAN_POINT('Ctrl Pts',(-2.95084136202242,1.30865338519323,
2.22961935399385));
#248026=CARTESIAN_POINT('Ctrl Pts',(-2.78409157437045,1.63328916879489,
2.20510166453211));
#248027=CARTESIAN_POINT('Ctrl Pts',(-2.6881084969062,1.78686125667515,2.192764539701));
#248028=CARTESIAN_POINT('Ctrl Pts',(-2.53445030375698,1.99208251759074,
2.17577453438));
#248029=CARTESIAN_POINT('Ctrl Pts',(-2.48702759135021,2.05098189487471,
2.17083592560627));
#248030=CARTESIAN_POINT('Ctrl Pts',(-2.42494334104917,2.12276709731408,
2.16479050166764));
#248031=CARTESIAN_POINT('Ctrl Pts',(-2.4121817380035,2.13725750944807,2.16356880163992));
#248032=CARTESIAN_POINT('Ctrl Pts',(-2.39181116471069,2.15997277960522,
2.16165266822472));
#248033=CARTESIAN_POINT('Ctrl Pts',(-2.38428844123661,2.16827389739153,
2.16095222043271));
#248034=CARTESIAN_POINT('Ctrl Pts',(-2.36990823068031,2.18397672656969,
2.15962710199718));
#248035=CARTESIAN_POINT('Ctrl Pts',(-2.36305912914913,2.19138561606638,
2.15900187270809));
#248036=CARTESIAN_POINT('Ctrl Pts',(-2.34665672816707,2.20896229125239,
2.15751829466192));
#248037=CARTESIAN_POINT('Ctrl Pts',(-2.33707187447798,2.21910055516079,
2.15666230224761));
#248038=CARTESIAN_POINT('Ctrl Pts',(-2.30414095293798,2.25348281642948,
2.15375711652164));
#248039=CARTESIAN_POINT('Ctrl Pts',(-2.28048025023812,2.27742406315151,
2.15173033578387));
#248040=CARTESIAN_POINT('Ctrl Pts',(-2.22120415615729,2.33555266750864,
2.14678634335597));
#248041=CARTESIAN_POINT('Ctrl Pts',(-2.18516934129827,2.36930149970408,
2.14389548368513));
#248042=CARTESIAN_POINT('Ctrl Pts',(-2.02415609904709,2.51330064515287,
2.13139532634657));
#248043=CARTESIAN_POINT('Ctrl Pts',(-1.89150339907874,2.61459556494731,
2.12214954774121));
#248044=CARTESIAN_POINT('Ctrl Pts',(-1.58270805408277,2.81454049097386,
2.1015329444411));
#248045=CARTESIAN_POINT('Ctrl Pts',(-1.40396381556002,2.90782993318214,
2.09014694434025));
#248046=CARTESIAN_POINT('Ctrl Pts',(-1.18552916992628,2.99697273567516,
2.07607521791467));
#248047=CARTESIAN_POINT('Ctrl Pts',(-1.15314775717085,3.00958055242416,
2.07398646532869));
#248048=CARTESIAN_POINT('Ctrl Pts',(-1.10150120430541,3.02873344380082,
2.070647709429));
#248049=CARTESIAN_POINT('Ctrl Pts',(-1.08236652200441,3.03562413013318,
2.0694091618992));
#248050=CARTESIAN_POINT('Ctrl Pts',(-1.04645230798768,3.04817464642984,
2.06708101665008));
#248051=CARTESIAN_POINT('Ctrl Pts',(-1.02968879090546,3.05387820356598,
2.0659929081853));
#248052=CARTESIAN_POINT('Ctrl Pts',(-0.992037582917555,3.06634325989044,
2.06354545814926));
#248053=CARTESIAN_POINT('Ctrl Pts',(-0.971126244388909,3.0730299921914,
2.06218373135486));
#248054=CARTESIAN_POINT('Ctrl Pts',(-0.908516881791847,3.09234746349154,
2.05809868276745));
#248055=CARTESIAN_POINT('Ctrl Pts',(-0.866630668024983,3.1043464286363,
2.05535517302565));
#248056=CARTESIAN_POINT('Ctrl Pts',(-0.666507021961941,3.15730919393773,
2.04219170297967));
#248057=CARTESIAN_POINT('Ctrl Pts',(-0.505568001477319,3.18703950065206,
2.03142454040343));
#248058=CARTESIAN_POINT('Ctrl Pts',(-0.172943013101873,3.22265257413123,
2.00897383370336));
#248059=CARTESIAN_POINT('Ctrl Pts',(-0.00161943607923983,3.22728926705032,
1.99730631365715));
#248060=CARTESIAN_POINT('Ctrl Pts',(0.258362700504717,3.21361591616483,
1.97996331485864));
#248061=CARTESIAN_POINT('Ctrl Pts',(0.347239282800383,3.20523108327493,
1.97410352360909));
#248062=CARTESIAN_POINT('Ctrl Pts',(0.455442392935602,3.19046836609113,
1.96713972125666));
#248063=CARTESIAN_POINT('Ctrl Pts',(0.475199313984088,3.18758557948713,
1.96587523460691));
#248064=CARTESIAN_POINT('Ctrl Pts',(0.506254627591664,3.18275905291123,
1.96390006194163));
#248065=CARTESIAN_POINT('Ctrl Pts',(0.51757125662516,3.18093837422369,1.96318291201767));
#248066=CARTESIAN_POINT('Ctrl Pts',(0.538762926213483,3.17741286036991,
1.96184516525283));
#248067=CARTESIAN_POINT('Ctrl Pts',(0.548639733087155,3.17572234646466,
1.96122384003476));
#248068=CARTESIAN_POINT('Ctrl Pts',(0.571756537962713,3.17165460889896,
1.95977447296951));
#248069=CARTESIAN_POINT('Ctrl Pts',(0.584989734339,3.16924052768454,1.95894849116909));
#248070=CARTESIAN_POINT('Ctrl Pts',(0.628362813461217,3.16104721843311,
1.9562522892123));
#248071=CARTESIAN_POINT('Ctrl Pts',(0.658436268177177,3.15492015390587,
1.9544003503644));
#248072=CARTESIAN_POINT('Ctrl Pts',(0.73100361309739,3.13905263567001,1.94996412959465));
#248073=CARTESIAN_POINT('Ctrl Pts',(0.773397077552878,3.12887760071118,
1.94739967786598));
#248074=CARTESIAN_POINT('Ctrl Pts',(0.943391534685824,3.08441006931795,
1.93717937191521));
#248075=CARTESIAN_POINT('Ctrl Pts',(1.06904198731469,3.0431442533812,1.92976555118161));
#248076=CARTESIAN_POINT('Ctrl Pts',(1.40575683852297,2.90912180038783,1.90947112247632));
#248077=CARTESIAN_POINT('Ctrl Pts',(1.60993626957032,2.8012915199883,1.89663243332257));
#248078=CARTESIAN_POINT('Ctrl Pts',(1.83718208045462,2.64816844871361,1.88040132025763));
#248079=CARTESIAN_POINT('Ctrl Pts',(1.87298413272379,2.62296860355975,1.87778330112054));
#248080=CARTESIAN_POINT('Ctrl Pts',(1.92621999863589,2.58385192343228,1.87379114340837));
#248081=CARTESIAN_POINT('Ctrl Pts',(1.94404172129719,2.57046999456735,1.87243740259821));
#248082=CARTESIAN_POINT('Ctrl Pts',(1.97579370959435,2.54610905317501,1.86999346151878));
#248083=CARTESIAN_POINT('Ctrl Pts',(1.98977495880697,2.5351977609488,1.86890593594071));
#248084=CARTESIAN_POINT('Ctrl Pts',(2.0194168714634,2.51166827313903,1.86657540005744));
#248085=CARTESIAN_POINT('Ctrl Pts',(2.03505084645822,2.49901781471519,1.86533113492383));
#248086=CARTESIAN_POINT('Ctrl Pts',(2.07726686553157,2.46419924528422,1.86192936715591));
#248087=CARTESIAN_POINT('Ctrl Pts',(2.10361122323009,2.44174839485416,1.85976053663779));
#248088=CARTESIAN_POINT('Ctrl Pts',(2.26631642806333,2.29850221777508,1.84606905152189));
#248089=CARTESIAN_POINT('Ctrl Pts',(2.39257068277541,2.16676934973573,1.83408649965335));
#248090=CARTESIAN_POINT('Ctrl Pts',(2.61832809354431,1.88728890325952,1.80996006108117));
#248091=CARTESIAN_POINT('Ctrl Pts',(2.7180945507089,1.74053552425201,1.79787408462959));
#248092=CARTESIAN_POINT('Ctrl Pts',(2.84503214214245,1.51605627233366,1.78074837867811));
#248093=CARTESIAN_POINT('Ctrl Pts',(2.88211767435064,1.44431106296683,1.77546345127314));
#248094=CARTESIAN_POINT('Ctrl Pts',(2.92484006044386,1.3534455855131,1.76906485332629));
#248095=CARTESIAN_POINT('Ctrl Pts',(2.93304506947218,1.33557141215259,1.76782002500611));
#248096=CARTESIAN_POINT('Ctrl Pts',(2.94569838863813,1.30732774210726,1.76587599315759));
#248097=CARTESIAN_POINT('Ctrl Pts',(2.95025660127906,1.29700841082399,1.7651704889577));
#248098=CARTESIAN_POINT('Ctrl Pts',(2.95877889849914,1.27743739216432,1.76384179621177));
#248099=CARTESIAN_POINT('Ctrl Pts',(2.96275382727595,1.26819108271962,1.76321800603394));
#248100=CARTESIAN_POINT('Ctrl Pts',(2.97207134159564,1.24623416401556,1.76174580546783));
#248101=CARTESIAN_POINT('Ctrl Pts',(2.97737577012575,1.23350767747316,1.76089966381898));
#248102=CARTESIAN_POINT('Ctrl Pts',(2.99497286578714,1.19051346270818,1.75806392603069));
#248103=CARTESIAN_POINT('Ctrl Pts',(3.00688737235722,1.16009192986447,1.75609532663598));
#248104=CARTESIAN_POINT('Ctrl Pts',(3.03495405337296,1.08508951049969,1.75132196810032));
#248105=CARTESIAN_POINT('Ctrl Pts',(3.05058930858167,1.04032238050182,1.74854126041145));
#248106=CARTESIAN_POINT('Ctrl Pts',(3.11282241047156,0.848648154921171,
1.73686014852028));
#248107=CARTESIAN_POINT('Ctrl Pts',(3.1498411885631,0.698837394319297,1.72827721712706));
#248108=CARTESIAN_POINT('Ctrl Pts',(3.20998676144822,0.349583956248182,
1.70843617187904));
#248109=CARTESIAN_POINT('Ctrl Pts',(3.22550151798466,0.149507144973904,
1.69717030154135));
#248110=CARTESIAN_POINT('Ctrl Pts',(3.22164015293346,-0.0958858230904817,
1.6826419978657));
#248111=CARTESIAN_POINT('Ctrl Pts',(3.21997910290325,-0.141044827728787,
1.67994068861445));
#248112=CARTESIAN_POINT('Ctrl Pts',(3.21608307747443,-0.208381873450195,
1.67586459848443));
#248113=CARTESIAN_POINT('Ctrl Pts',(3.21456658974851,-0.230596982437728,
1.67451203777158));
#248114=CARTESIAN_POINT('Ctrl Pts',(3.21142928796425,-0.270469681621264,
1.67206957547851));
#248115=CARTESIAN_POINT('Ctrl Pts',(3.20989270879577,-0.288133126497392,
1.67098233892588));
#248116=CARTESIAN_POINT('Ctrl Pts',(3.20630173357278,-0.325808912498398,
1.6686517159574));
#248117=CARTESIAN_POINT('Ctrl Pts',(3.20420555322548,-0.345816421981687,
1.6674070684783));
#248118=CARTESIAN_POINT('Ctrl Pts',(3.19798909186975,-0.40022998698095,
1.66400243970232));
#248119=CARTESIAN_POINT('Ctrl Pts',(3.19350108696467,-0.434590534175425,
1.66183109278558));
#248120=CARTESIAN_POINT('Ctrl Pts',(3.16174168517603,-0.650563763439772,
1.64804323223134));
#248121=CARTESIAN_POINT('Ctrl Pts',(3.11954637970748,-0.829611317695499,
1.63595872021517));
#248122=CARTESIAN_POINT('Ctrl Pts',(3.00633787649355,-1.17489035562275,
1.61155043952407));
#248123=CARTESIAN_POINT('Ctrl Pts',(2.93613513970884,-1.3407259571393,1.5992831787055));
#248124=CARTESIAN_POINT('Ctrl Pts',(2.81662257503734,-1.56802041783545,
1.58225451540949));
#248125=CARTESIAN_POINT('Ctrl Pts',(2.77833881656349,-1.63489637303071,
1.57721898607882));
#248126=CARTESIAN_POINT('Ctrl Pts',(2.72745045345081,-1.71683091533526,
1.5710744211516));
#248127=CARTESIAN_POINT('Ctrl Pts',(2.71705978094946,-1.73322836273651,
1.56984603323711));
#248128=CARTESIAN_POINT('Ctrl Pts',(2.70042800130979,-1.75895769015101,
1.567921884263));
#248129=CARTESIAN_POINT('Ctrl Pts',(2.69428539809744,-1.76835226934616,
1.56722002549472));
#248130=CARTESIAN_POINT('Ctrl Pts',(2.6825327599891,-1.78612350805862,1.56589399531724));
#248131=CARTESIAN_POINT('Ctrl Pts',(2.67693238932781,-1.79450611020295,
1.56526924879722));
#248132=CARTESIAN_POINT('Ctrl Pts',(2.66351638142086,-1.8143845454588,1.56378922303953));
#248133=CARTESIAN_POINT('Ctrl Pts',(2.65566543970209,-1.82585647887927,
1.56293626930998));
#248134=CARTESIAN_POINT('Ctrl Pts',(2.62872710706015,-1.86467789295419,
1.56005254872316));
#248135=CARTESIAN_POINT('Ctrl Pts',(2.60928883463633,-1.8917827096265,1.55804375289821));
#248136=CARTESIAN_POINT('Ctrl Pts',(2.56040741693405,-1.95775597847468,
1.55315271287891));
#248137=CARTESIAN_POINT('Ctrl Pts',(2.53049570456691,-1.99626816001729,
1.55029609571321));
#248138=CARTESIAN_POINT('Ctrl Pts',(2.39707595295957,-2.16022957901623,
1.53805738936644));
#248139=CARTESIAN_POINT('Ctrl Pts',(2.28502444493128,-2.27842818645096,
1.5290238662057));
#248140=CARTESIAN_POINT('Ctrl Pts',(2.02427330294337,-2.51481013283664,
1.50930812980629));
#248141=CARTESIAN_POINT('Ctrl Pts',(1.87311072318561,-2.62933413634705,
1.49862460989673));
#248142=CARTESIAN_POINT('Ctrl Pts',(1.67439673277888,-2.75400917292916,
1.48473888013062));
#248143=CARTESIAN_POINT('Ctrl Pts',(1.63550979971264,-2.77727894465387,
1.4820300755438));
#248144=CARTESIAN_POINT('Ctrl Pts',(1.57677962844725,-2.81076156110673,
1.47794475941962));
#248145=CARTESIAN_POINT('Ctrl Pts',(1.55729903871607,-2.82160135664181,
1.47659061411639));
#248146=CARTESIAN_POINT('Ctrl Pts',(1.52212204009938,-2.84070001647051,
1.47414627861748));
#248147=CARTESIAN_POINT('Ctrl Pts',(1.50646682273241,-2.8490331308745,1.47305876777375));
#248148=CARTESIAN_POINT('Ctrl Pts',(1.47291924660825,-2.86653635248986,
1.47072863273186));
#248149=CARTESIAN_POINT('Ctrl Pts',(1.4550083242896,-2.87566905507895,1.46948475713349));
#248150=CARTESIAN_POINT('Ctrl Pts',(1.40605605806614,-2.9000551916817,1.46608501444263));
#248151=CARTESIAN_POINT('Ctrl Pts',(1.374853435774,-2.91497712424577,1.46391784130291));
#248152=CARTESIAN_POINT('Ctrl Pts',(1.17856211937092,-3.00499617209078,
1.45027897907652));
#248153=CARTESIAN_POINT('Ctrl Pts',(1.00764509862685,-3.06653608160793,
1.43835171535599));
#248154=CARTESIAN_POINT('Ctrl Pts',(0.662712591579352,-3.15876764879831,
1.41437823961773));
#248155=CARTESIAN_POINT('Ctrl Pts',(0.489513111421216,-3.1902003461873,
1.40239070936379));
#248156=CARTESIAN_POINT('Ctrl Pts',(0.232297303174221,-3.21543105741181,
1.38521455159657));
#248157=CARTESIAN_POINT('Ctrl Pts',(0.14969206047645,-3.2203343891187,1.37979567400837));
#248158=CARTESIAN_POINT('Ctrl Pts',(0.047196217307954,-3.22246516964836,
1.37326164059696));
#248159=CARTESIAN_POINT('Ctrl Pts',(0.0274053862454179,-3.22269425210146,
1.37200877394559));
#248160=CARTESIAN_POINT('Ctrl Pts',(-0.00369587151322278,-3.22276772316502,
1.37005499926958));
#248161=CARTESIAN_POINT('Ctrl Pts',(-0.0150051466959918,-3.2227349117801,
1.36934769096479));
#248162=CARTESIAN_POINT('Ctrl Pts',(-0.0363776369577231,-3.22256039652642,
1.36801723315083));
#248163=CARTESIAN_POINT('Ctrl Pts',(-0.0464403507838753,-3.22243109123781,
1.36739346541563));
#248164=CARTESIAN_POINT('Ctrl Pts',(-0.0702477089453369,-3.2220136259795,
1.3659237086186));
#248165=CARTESIAN_POINT('Ctrl Pts',(-0.0839913474430751,-3.22168465493525,
1.36507995956881));
#248166=CARTESIAN_POINT('Ctrl Pts',(-0.130108378113417,-3.22028547166179,
1.36226333691457));
#248167=CARTESIAN_POINT('Ctrl Pts',(-0.162468757136495,-3.21881512230102,
1.36031104742288));
#248168=CARTESIAN_POINT('Ctrl Pts',(-0.241577871545698,-3.21402452114527,
1.3555856313518));
#248169=CARTESIAN_POINT('Ctrl Pts',(-0.288287846514752,-3.2101719623515,
1.35283589683806));
#248170=CARTESIAN_POINT('Ctrl Pts',(-0.484817090053177,-3.18963801145944,
1.34137611863389));
#248171=CARTESIAN_POINT('Ctrl Pts',(-0.633461135311341,-3.16347454032089,
1.33297112179323));
#248172=CARTESIAN_POINT('Ctrl Pts',(-0.977733025119387,-3.07762834499138,
1.31310656690478));
#248173=CARTESIAN_POINT('Ctrl Pts',(-1.17057182219064,-3.00956940119656,
1.30164063185059));
#248174=CARTESIAN_POINT('Ctrl Pts',(-1.39681209740821,-2.90466690125933,
1.28687937703692));
#248175=CARTESIAN_POINT('Ctrl Pts',(-1.43754228318283,-2.88472628241025,
1.28416865861869));
#248176=CARTESIAN_POINT('Ctrl Pts',(-1.49765804969568,-2.85370556054669,
1.28008071032851));
#248177=CARTESIAN_POINT('Ctrl Pts',(-1.51737222441274,-2.84327215622488,
1.27872586816672));
#248178=CARTESIAN_POINT('Ctrl Pts',(-1.55257084686608,-2.82417352901214,
1.27628036883012));
#248179=CARTESIAN_POINT('Ctrl Pts',(-1.56809516180137,-2.81558340318886,
1.27519239326876));
#248180=CARTESIAN_POINT('Ctrl Pts',(-1.60106411562954,-2.79698333063702,
1.2728613503058));
#248181=CARTESIAN_POINT('Ctrl Pts',(-1.61848750012414,-2.78693742969881,
1.27161703183881));
#248182=CARTESIAN_POINT('Ctrl Pts',(-1.66562269013185,-2.75916933919876,
1.2682162714455));
#248183=CARTESIAN_POINT('Ctrl Pts',(-1.69514431900333,-2.74113114926068,
1.26604852271925));
#248184=CARTESIAN_POINT('Ctrl Pts',(-1.75996419529829,-2.70007756466549,
1.26120260807297));
#248185=CARTESIAN_POINT('Ctrl Pts',(-1.79511250833111,-2.67683836730967,
1.25851663239158));
#248186=CARTESIAN_POINT('Ctrl Pts',(-1.90435767397843,-2.60148882229082,
1.24998107316453));
#248187=CARTESIAN_POINT('Ctrl Pts',(-1.9767144585979,-2.54694325192496,
1.24404785221202));
#248188=CARTESIAN_POINT('Ctrl Pts',(-2.14979671615801,-2.40464427824107,
1.22917084389868));
#248189=CARTESIAN_POINT('Ctrl Pts',(-2.24754758245627,-2.31353982650047,
1.22014315557297));
#248190=CARTESIAN_POINT('Ctrl Pts',(-2.37652296516427,-2.17742396870072,
1.20747204368998));
#248191=CARTESIAN_POINT('Ctrl Pts',(-2.41269218531012,-2.13727703601834,
1.2038253795197));
#248192=CARTESIAN_POINT('Ctrl Pts',(-2.52376484040837,-2.00757448416984,
1.19236200812574));
#248193=CARTESIAN_POINT('Ctrl Pts',(-2.5948288806241,-1.9148401743512,1.18462302236009));
#248194=CARTESIAN_POINT('Ctrl Pts',(-2.67263107030621,-1.80100170001078,
1.17581811928718));
#248195=CARTESIAN_POINT('Ctrl Pts',(-2.68438122846769,-1.78344089782949,
1.17447850627666));
#248196=CARTESIAN_POINT('Ctrl Pts',(-2.7023821039717,-1.75595728597366,
1.17241229148214));
#248197=CARTESIAN_POINT('Ctrl Pts',(-2.7087525713782,-1.74611412661286,
1.17167825574094));
#248198=CARTESIAN_POINT('Ctrl Pts',(-2.72043998428536,-1.72783773359812,
1.17032666087447));
#248199=CARTESIAN_POINT('Ctrl Pts',(-2.72577155502347,-1.71941454438589,
1.16970818949788));
#248200=CARTESIAN_POINT('Ctrl Pts',(-2.73797621672805,-1.69993332340838,
1.16828787422502));
#248201=CARTESIAN_POINT('Ctrl Pts',(-2.74482146869559,-1.68885824918665,
1.16748782791784));
#248202=CARTESIAN_POINT('Ctrl Pts',(-2.76634669901203,-1.65355554951443,
1.16496003184757));
#248203=CARTESIAN_POINT('Ctrl Pts',(-2.78077488274044,-1.62917500261481,
1.16324758837465));
#248204=CARTESIAN_POINT('Ctrl Pts',(-2.85652054729852,-1.49724230236028,
1.15414076963792));
#248205=CARTESIAN_POINT('Ctrl Pts',(-2.91192962534587,-1.3864040593358,
1.14705223095193));
#248206=CARTESIAN_POINT('Ctrl Pts',(-3.05217345762915,-1.06012394442053,
1.12700296264413));
#248207=CARTESIAN_POINT('Ctrl Pts',(-3.12037052170006,-0.838398476945386,
1.11429958918481));
#248208=CARTESIAN_POINT('Ctrl Pts',(-3.1798950228356,-0.53027562905916,
1.09612869278267));
#248209=CARTESIAN_POINT('Ctrl Pts',(-3.19242674030653,-0.448703095731515,
1.09127729630226));
#248210=CARTESIAN_POINT('Ctrl Pts',(-3.20508536182478,-0.338188565996296,
1.08460480267479));
#248211=CARTESIAN_POINT('Ctrl Pts',(-3.2079739522668,-0.30959122043394,
1.08286937218141));
#248212=CARTESIAN_POINT('Ctrl Pts',(-3.21212201003229,-0.262192064140319,
1.07997669986104));
#248213=CARTESIAN_POINT('Ctrl Pts',(-3.21359980576588,-0.24341066278756,
1.07882630072219));
#248214=CARTESIAN_POINT('Ctrl Pts',(-3.21608548488812,-0.207833581932038,
1.07663872469654));
#248215=CARTESIAN_POINT('Ctrl Pts',(-3.21712667406909,-0.191040806918223,
1.07560262506271));
#248216=CARTESIAN_POINT('Ctrl Pts',(-3.21899170423312,-0.156595766204148,
1.07346985434961));
#248217=CARTESIAN_POINT('Ctrl Pts',(-3.21980194232736,-0.138943363555232,
1.07237279527519));
#248218=CARTESIAN_POINT('Ctrl Pts',(-3.22120479765994,-0.101693646886477,
1.07004897222391));
#248219=CARTESIAN_POINT('Ctrl Pts',(-3.22176383201439,-0.0820958580356578,
1.06882121079411));
#248220=CARTESIAN_POINT('Ctrl Pts',(-3.22255677868777,-0.0412124644936687,
1.06624891962182));
#248221=CARTESIAN_POINT('Ctrl Pts',(-3.22275868156198,-0.0199273287497446,
1.06490347292996));
#248222=CARTESIAN_POINT('Ctrl Pts',(-3.22274971398033,0.0013577701177717,
1.06355168448669));
#248223=CARTESIAN_POINT('Ctrl Pts',(-3.22274913564885,0.00236033357308065,
0.816219464231529));
#248224=CARTESIAN_POINT('Ctrl Pts',(-3.22286909096441,-0.1614240966976,
0.825608085954441));
#248225=CARTESIAN_POINT('Ctrl Pts',(-3.21050335524459,-0.324991258301196,
0.834672913528035));
#248226=CARTESIAN_POINT('Ctrl Pts',(-3.1604140557922,-0.652708508243162,
0.85328181329922));
#248227=CARTESIAN_POINT('Ctrl Pts',(-3.1221748315376,-0.816248156505571,
0.862807257899995));
#248228=CARTESIAN_POINT('Ctrl Pts',(-3.05795698999836,-1.01832372725381,
0.875362448731364));
#248229=CARTESIAN_POINT('Ctrl Pts',(-3.04365559516214,-1.06030396559574,
0.878013951006589));
#248230=CARTESIAN_POINT('Ctrl Pts',(-3.02086567945308,-1.1229361901449,
0.882041682122287));
#248231=CARTESIAN_POINT('Ctrl Pts',(-3.01302102409625,-1.14381790956262,
0.883396701528632));
#248232=CARTESIAN_POINT('Ctrl Pts',(-2.99852262649171,-1.18122689761408,
0.885846916177238));
#248233=CARTESIAN_POINT('Ctrl Pts',(-2.99194736003148,-1.19778374506526,
0.886939451114916));
#248234=CARTESIAN_POINT('Ctrl Pts',(-2.97747966255677,-1.23335157450746,
0.889304359451952));
#248235=CARTESIAN_POINT('Ctrl Pts',(-2.96954172138339,-1.25234307634294,
0.890578230696995));
#248236=CARTESIAN_POINT('Ctrl Pts',(-2.94761568434028,-1.30342029047189,
0.894035057233538));
#248237=CARTESIAN_POINT('Ctrl Pts',(-2.93328622055922,-1.33535555929732,
0.896229506738193));
#248238=CARTESIAN_POINT('Ctrl Pts',(-2.84247298990635,-1.52922771526697,
0.909760128481584));
#248239=CARTESIAN_POINT('Ctrl Pts',(-2.75313227779475,-1.68476552146076,
0.921541139942433));
#248240=CARTESIAN_POINT('Ctrl Pts',(-2.57989828553722,-1.93546937623926,
0.942009518664005));
#248241=CARTESIAN_POINT('Ctrl Pts',(-2.50245515066346,-2.03460910653372,
0.950548576390257));
#248242=CARTESIAN_POINT('Ctrl Pts',(-2.35995172448385,-2.19655406819115,
0.965079561172328));
#248243=CARTESIAN_POINT('Ctrl Pts',(-2.29767165179909,-2.2616208468479,
0.971099045246451));
#248244=CARTESIAN_POINT('Ctrl Pts',(-2.20769722116667,-2.34806240440204,
0.979265741386672));
#248245=CARTESIAN_POINT('Ctrl Pts',(-2.18226063843599,-2.37172148008052,
0.981519837156127));
#248246=CARTESIAN_POINT('Ctrl Pts',(-2.13763166392808,-2.41190575291921,
0.985374144341918));
#248247=CARTESIAN_POINT('Ctrl Pts',(-2.11861817407881,-2.42862422282353,
0.98698576889893));
#248248=CARTESIAN_POINT('Ctrl Pts',(-2.09011423909651,-2.45309806406821,
0.989354551877601));
#248249=CARTESIAN_POINT('Ctrl Pts',(-2.08077389078241,-2.46102573559374,
0.990123385983259));
#248250=CARTESIAN_POINT('Ctrl Pts',(-2.06363511571716,-2.47540503738035,
0.991520350426597));
#248251=CARTESIAN_POINT('Ctrl Pts',(-2.0558512992925,-2.48187337163248,
0.992149645667449));
#248252=CARTESIAN_POINT('Ctrl Pts',(-2.03878123805063,-2.49592314063498,
0.993518485475008));
#248253=CARTESIAN_POINT('Ctrl Pts',(-2.02948307877546,-2.50348950550907,
0.994256974265698));
#248254=CARTESIAN_POINT('Ctrl Pts',(-2.00331018720816,-2.52454601439626,
0.996316520030707));
#248255=CARTESIAN_POINT('Ctrl Pts',(-1.98634137237403,-2.53791889036635,
0.997629659672997));
#248256=CARTESIAN_POINT('Ctrl Pts',(-1.870362177989,-2.62744454545351,1.0064656123821));
#248257=CARTESIAN_POINT('Ctrl Pts',(-1.76712041277952,-2.69796438500549,
1.0136525579085));
#248258=CARTESIAN_POINT('Ctrl Pts',(-1.42368931182879,-2.90435171005929,
1.03633485440145));
#248259=CARTESIAN_POINT('Ctrl Pts',(-1.17010894421849,-3.01545914864115,
1.05139395941233));
#248260=CARTESIAN_POINT('Ctrl Pts',(-0.850609460254013,-3.10899497450193,
1.07095055048486));
#248261=CARTESIAN_POINT('Ctrl Pts',(-0.795325361273546,-3.12359459426378,
1.07434927130283));
#248262=CARTESIAN_POINT('Ctrl Pts',(-0.715584914688503,-3.14239858749436,
1.07928660494274));
#248263=CARTESIAN_POINT('Ctrl Pts',(-0.691421098572556,-3.14780359383477,
1.08078729327755));
#248264=CARTESIAN_POINT('Ctrl Pts',(-0.649168547291423,-3.15674474312338,
1.08342030574655));
#248265=CARTESIAN_POINT('Ctrl Pts',(-0.631107100899261,-3.16040519257544,
1.08454864983804));
#248266=CARTESIAN_POINT('Ctrl Pts',(-0.593700612013165,-3.16765279303163,
1.08689178902605));
#248267=CARTESIAN_POINT('Ctrl Pts',(-0.574352166982195,-3.17121809327191,
1.08810722046468));
#248268=CARTESIAN_POINT('Ctrl Pts',(-0.524329318061336,-3.17996289879882,
1.09125897186331));
#248269=CARTESIAN_POINT('Ctrl Pts',(-0.493610947167263,-3.18487572704859,
1.09320353977833));
#248270=CARTESIAN_POINT('Ctrl Pts',(-0.364498774602229,-3.20361206652839,
1.10141729700865));
#248271=CARTESIAN_POINT('Ctrl Pts',(-0.265572432593184,-3.21332500769714,
1.10781150495507));
#248272=CARTESIAN_POINT('Ctrl Pts',(0.0628457619002177,-3.23030108781832,
1.12936495692031));
#248273=CARTESIAN_POINT('Ctrl Pts',(0.292652254680948,-3.21762809599612,
1.1450250762266));
#248274=CARTESIAN_POINT('Ctrl Pts',(0.595040875317243,-3.16827397014781,
1.16556206322948));
#248275=CARTESIAN_POINT('Ctrl Pts',(0.670488929049658,-3.15316976613957,
1.17067354019613));
#248276=CARTESIAN_POINT('Ctrl Pts',(0.790406087210058,-3.12466360155229,
1.17871030673554));
#248277=CARTESIAN_POINT('Ctrl Pts',(0.835250330174358,-3.11297635538181,
1.18169562883888));
#248278=CARTESIAN_POINT('Ctrl Pts',(0.895239014336261,-3.0959523977076,
1.18564812793372));
#248279=CARTESIAN_POINT('Ctrl Pts',(0.91061616750354,-3.09146443641764,
1.18665762036896));
#248280=CARTESIAN_POINT('Ctrl Pts',(0.936181467492968,-3.08379566625165,
1.18832909331505));
#248281=CARTESIAN_POINT('Ctrl Pts',(0.946388258718718,-3.08067861418492,
1.18899458722347));
#248282=CARTESIAN_POINT('Ctrl Pts',(0.965744116338459,-3.07466225260615,
1.19025287654708));
#248283=CARTESIAN_POINT('Ctrl Pts',(0.974896025294655,-3.07177268223002,
1.19084623869258));
#248284=CARTESIAN_POINT('Ctrl Pts',(0.999295199861494,-3.06394900129731,
1.19242424933902));
#248285=CARTESIAN_POINT('Ctrl Pts',(1.01451902155037,-3.05894190173244,
1.19340476255508));
#248286=CARTESIAN_POINT('Ctrl Pts',(1.07052557509851,-3.04005728665629,
1.19699902484583));
#248287=CARTESIAN_POINT('Ctrl Pts',(1.11106805098352,-3.02547541628464,
1.1995754965506));
#248288=CARTESIAN_POINT('Ctrl Pts',(1.3425252598494,-2.93694681478146,1.21420306013822));
#248289=CARTESIAN_POINT('Ctrl Pts',(1.5263581985784,-2.84574747986912,1.2255211208592));
#248290=CARTESIAN_POINT('Ctrl Pts',(1.84281882243856,-2.64920350034945,
1.24641299679187));
#248291=CARTESIAN_POINT('Ctrl Pts',(1.97818696215714,-2.54971157413972,
1.25589864264067));
#248292=CARTESIAN_POINT('Ctrl Pts',(2.14596027113954,-2.40496809011715,
1.2689418937264));
#248293=CARTESIAN_POINT('Ctrl Pts',(2.18584088164418,-2.36877946334564,
1.2721476541899));
#248294=CARTESIAN_POINT('Ctrl Pts',(2.24227601767943,-2.31492973162574,
1.27685182230117));
#248295=CARTESIAN_POINT('Ctrl Pts',(2.25956888668173,-2.29805348061677,
1.27831710590944));
#248296=CARTESIAN_POINT('Ctrl Pts',(2.28962635724851,-2.26805286678018,
1.28090730550712));
#248297=CARTESIAN_POINT('Ctrl Pts',(2.30247208077044,-2.25501107713496,
1.28202859099051));
#248298=CARTESIAN_POINT('Ctrl Pts',(2.32901485856407,-2.22759992209547,
1.28437597394713));
#248299=CARTESIAN_POINT('Ctrl Pts',(2.34269161247608,-2.21321205609795,
1.28560287512141));
#248300=CARTESIAN_POINT('Ctrl Pts',(2.37811067712946,-2.17525523891722,
1.28882660935714));
#248301=CARTESIAN_POINT('Ctrl Pts',(2.39963525693648,-2.1514869887129,1.29083247438135));
#248302=CARTESIAN_POINT('Ctrl Pts',(2.49135662818551,-2.0471159446422,1.2995885839805));
#248303=CARTESIAN_POINT('Ctrl Pts',(2.55786742931069,-1.96337761384278,
1.30648521295537));
#248304=CARTESIAN_POINT('Ctrl Pts',(2.74081790964209,-1.70792998602518,
1.32715013580317));
#248305=CARTESIAN_POINT('Ctrl Pts',(2.84498867706062,-1.52811435177765,
1.34126824149459));
#248306=CARTESIAN_POINT('Ctrl Pts',(2.98431136334188,-1.22325629113519,
1.36381541703847));
#248307=CARTESIAN_POINT('Ctrl Pts',(3.03050097260132,-1.10387542316613,
1.37232101091366));
#248308=CARTESIAN_POINT('Ctrl Pts',(3.07600383140691,-0.961653157438882,
1.38185624290185));
#248309=CARTESIAN_POINT('Ctrl Pts',(3.08232761205328,-0.941186971149414,
1.38321420380309));
#248310=CARTESIAN_POINT('Ctrl Pts',(3.09182174806545,-0.909337884737007,
1.38530387210902));
#248311=CARTESIAN_POINT('Ctrl Pts',(3.09513422926783,-0.897998454091546,
1.38604326429945));
#248312=CARTESIAN_POINT('Ctrl Pts',(3.10119741735548,-0.876810521145158,
1.38741592089813));
#248313=CARTESIAN_POINT('Ctrl Pts',(3.10396361827285,-0.866967110726428,
1.38805001188597));
#248314=CARTESIAN_POINT('Ctrl Pts',(3.11024361416766,-0.844204629707802,
1.38950818339774));
#248315=CARTESIAN_POINT('Ctrl Pts',(3.11372380771394,-0.83127664474951,
1.39033035500236));
#248316=CARTESIAN_POINT('Ctrl Pts',(3.12479131300124,-0.789118954564906,
1.3929930496368));
#248317=CARTESIAN_POINT('Ctrl Pts',(3.13204862016663,-0.759803305073057,
1.39481596811506));
#248318=CARTESIAN_POINT('Ctrl Pts',(3.1778339480306,-0.563037902476248,
1.40688657569195));
#248319=CARTESIAN_POINT('Ctrl Pts',(3.20333362661943,-0.392820222940303,
1.41654333773793));
#248320=CARTESIAN_POINT('Ctrl Pts',(3.22632737545772,-0.0588545063100762,
1.43529701214256));
#248321=CARTESIAN_POINT('Ctrl Pts',(3.22517869050616,0.104265513338425,
1.44437327539808));
#248322=CARTESIAN_POINT('Ctrl Pts',(3.20634029344234,0.331216995898737,
1.45747997278169));
#248323=CARTESIAN_POINT('Ctrl Pts',(3.19902690426935,0.395662625043786,
1.46125432553624));
#248324=CARTESIAN_POINT('Ctrl Pts',(3.18285836569279,0.507818739866992,
1.46794708257281));
#248325=CARTESIAN_POINT('Ctrl Pts',(3.1748605937362,0.555632156082215,1.47084005049569));
#248326=CARTESIAN_POINT('Ctrl Pts',(3.16144954117865,0.626012400680083,
1.47516587434077));
#248327=CARTESIAN_POINT('Ctrl Pts',(3.15686584343416,0.648731632404412,
1.47657273136909));
#248328=CARTESIAN_POINT('Ctrl Pts',(3.1482545924279,0.689159137741823,1.47909569553666));
#248329=CARTESIAN_POINT('Ctrl Pts',(3.14432162537363,0.70688668890667,1.48020876262159));
#248330=CARTESIAN_POINT('Ctrl Pts',(3.13567462260323,0.744361729200727,
1.4825764421999));
#248331=CARTESIAN_POINT('Ctrl Pts',(3.13092339123425,0.764099738937444,
1.4838321977915));
#248332=CARTESIAN_POINT('Ctrl Pts',(3.11765737947424,0.817008432708395,
1.48722234779076));
#248333=CARTESIAN_POINT('Ctrl Pts',(3.10880002592167,0.850089742139968,
1.48936758838151));
#248334=CARTESIAN_POINT('Ctrl Pts',(3.06059056382652,1.01930539034497,1.50047624231283));
#248335=CARTESIAN_POINT('Ctrl Pts',(3.01282259744245,1.15286117632721,1.50970740186858));
#248336=CARTESIAN_POINT('Ctrl Pts',(2.87028055090618,1.48136647401607,1.53353483465706));
#248337=CARTESIAN_POINT('Ctrl Pts',(2.7643579421497,1.670711204747,1.54835941420533));
#248338=CARTESIAN_POINT('Ctrl Pts',(2.60820843424535,1.89380336034819,1.56645291954706));
#248339=CARTESIAN_POINT('Ctrl Pts',(2.57496588790332,1.93876087956273,1.57013152444463));
#248340=CARTESIAN_POINT('Ctrl Pts',(2.51780309014676,2.01200256059984,1.57615120959206));
#248341=CARTESIAN_POINT('Ctrl Pts',(2.49453543221871,2.04077925059272,1.57852349845452));
#248342=CARTESIAN_POINT('Ctrl Pts',(2.46136382450686,2.08038953134716,1.58179162124443));
#248343=CARTESIAN_POINT('Ctrl Pts',(2.45187464107815,2.09156478318943,1.58271396603745));
#248344=CARTESIAN_POINT('Ctrl Pts',(2.43554037211883,2.11053744168677,1.58427981820621));
#248345=CARTESIAN_POINT('Ctrl Pts',(2.4287333544413,2.11836717829471,1.58492599915673));
#248346=CARTESIAN_POINT('Ctrl Pts',(2.414432304586,2.13465733460855,1.5862701676898));
#248347=CARTESIAN_POINT('Ctrl Pts',(2.40693144787051,2.14311136059401,1.58696764831078));
#248348=CARTESIAN_POINT('Ctrl Pts',(2.38666847721577,2.16570866743081,1.58883228529697));
#248349=CARTESIAN_POINT('Ctrl Pts',(2.37382496276697,2.1797787819432,1.58999360857395));
#248350=CARTESIAN_POINT('Ctrl Pts',(2.31334295070601,2.24486841920629,1.59537210001377));
#248351=CARTESIAN_POINT('Ctrl Pts',(2.26417636975943,2.29444910193913,1.5994868889855));
#248352=CARTESIAN_POINT('Ctrl Pts',(2.07956423120677,2.46889726386049,1.61420630287181));
#248353=CARTESIAN_POINT('Ctrl Pts',(1.93508744159758,2.5836963394253,1.62438682578549));
#248354=CARTESIAN_POINT('Ctrl Pts',(1.64013546441197,2.77936813423737,1.64426087883806));
#248355=CARTESIAN_POINT('Ctrl Pts',(1.49150729193875,2.86187504257026,1.65390011069732));
#248356=CARTESIAN_POINT('Ctrl Pts',(1.29638575695095,2.95084770312298,1.66659959483267));
#248357=CARTESIAN_POINT('Ctrl Pts',(1.25530823103117,2.96855506144135,1.66927423459243));
#248358=CARTESIAN_POINT('Ctrl Pts',(1.19305070731933,2.99386923752831,1.67333618648865));
#248359=CARTESIAN_POINT('Ctrl Pts',(1.17213686172049,3.00211894165499,1.67470205121285));
#248360=CARTESIAN_POINT('Ctrl Pts',(1.13437155467025,3.01656112065541,1.67717168373143));
#248361=CARTESIAN_POINT('Ctrl Pts',(1.11755128771927,3.02283292915734,1.67827276512772));
#248362=CARTESIAN_POINT('Ctrl Pts',(1.08118548346784,3.03604771401498,1.68065616503584));
#248363=CARTESIAN_POINT('Ctrl Pts',(1.06162364319364,3.0429431443542,1.68193999290455));
#248364=CARTESIAN_POINT('Ctrl Pts',(1.00861061972943,3.06105650978373,1.68542454182457));
#248365=CARTESIAN_POINT('Ctrl Pts',(0.975040313014042,3.07191447945906,
1.68763685596779));
#248366=CARTESIAN_POINT('Ctrl Pts',(0.760836642009185,3.13733158013057,
1.70179407343206));
#248367=CARTESIAN_POINT('Ctrl Pts',(0.575911226341209,3.1764803833567,1.71423224605722));
#248368=CARTESIAN_POINT('Ctrl Pts',(0.252491394646808,3.21577032382659,
1.736136452538));
#248369=CARTESIAN_POINT('Ctrl Pts',(0.11541561776743,3.22360199009643,1.74545644895553));
#248370=CARTESIAN_POINT('Ctrl Pts',(-0.0959038079811421,3.22217632773535,
1.75961368338483));
#248371=CARTESIAN_POINT('Ctrl Pts',(-0.170031068386464,3.2191161136176,
1.76453807474508));
#248372=CARTESIAN_POINT('Ctrl Pts',(-0.289039910990113,3.21008015898365,
1.77231594456876));
#248373=CARTESIAN_POINT('Ctrl Pts',(-0.334014900976881,3.20571258999861,
1.77522557184541));
#248374=CARTESIAN_POINT('Ctrl Pts',(-0.39461015545749,3.1985389029578,1.77909264104674));
#248375=CARTESIAN_POINT('Ctrl Pts',(-0.410321118918131,3.19656141684924,
1.78009043798495));
#248376=CARTESIAN_POINT('Ctrl Pts',(-0.436531574789474,3.19306596614869,
1.78174624235564));
#248377=CARTESIAN_POINT('Ctrl Pts',(-0.447039157971009,3.19161183126196,
1.78240767136716));
#248378=CARTESIAN_POINT('Ctrl Pts',(-0.468353568368802,3.18855482070454,
1.7837442922526));
#248379=CARTESIAN_POINT('Ctrl Pts',(-0.479159751276847,3.18694883087511,
1.78441930847881));
#248380=CARTESIAN_POINT('Ctrl Pts',(-0.507088242975339,3.18265289868826,
1.78615754113685));
#248381=CARTESIAN_POINT('Ctrl Pts',(-0.524197639783479,3.1798796871099,
1.78721623235103));
#248382=CARTESIAN_POINT('Ctrl Pts',(-0.593583269519605,3.16805793025572,
1.79148758048805));
#248383=CARTESIAN_POINT('Ctrl Pts',(-0.645657598670931,3.15785672839533,
1.79464227807491));
#248384=CARTESIAN_POINT('Ctrl Pts',(-0.75890352182933,3.13275340497592,
1.8014371988924));
#248385=CARTESIAN_POINT('Ctrl Pts',(-0.819938497879905,3.11733541281106,
1.80505704576313));
#248386=CARTESIAN_POINT('Ctrl Pts',(-1.06480528049328,3.04778961281511,
1.81954493158093));
#248387=CARTESIAN_POINT('Ctrl Pts',(-1.24409133614876,2.97910596002563,
1.83009498852789));
#248388=CARTESIAN_POINT('Ctrl Pts',(-1.4992891042266,2.85426036640323,1.84620476556318));
#248389=CARTESIAN_POINT('Ctrl Pts',(-1.58056814750168,2.81006630673086,
1.85151016859105));
#248390=CARTESIAN_POINT('Ctrl Pts',(-1.71378472787176,2.73002224526434,
1.8606083139029));
#248391=CARTESIAN_POINT('Ctrl Pts',(-1.76677443288491,2.6960316923153,1.86434068711323));
#248392=CARTESIAN_POINT('Ctrl Pts',(-1.83990461213528,2.64603974148246,
1.8696732421494));
#248393=CARTESIAN_POINT('Ctrl Pts',(-1.86090269025632,2.6313145792619,1.87122618433916));
#248394=CARTESIAN_POINT('Ctrl Pts',(-1.89677310922655,2.60551588685585,
1.87391806665086));
#248395=CARTESIAN_POINT('Ctrl Pts',(-1.91172994159052,2.59456159544994,
1.87505243568036));
#248396=CARTESIAN_POINT('Ctrl Pts',(-1.94206249975424,2.57194153995899,
1.87737790356021));
#248397=CARTESIAN_POINT('Ctrl Pts',(-1.95742958612638,2.56026549944559,
1.87856937156763));
#248398=CARTESIAN_POINT('Ctrl Pts',(-1.99602083014927,2.53039302202824,
1.88159595961613));
#248399=CARTESIAN_POINT('Ctrl Pts',(-2.01910131312976,2.51201468855766,
1.88343817240581));
#248400=CARTESIAN_POINT('Ctrl Pts',(-2.10762268984663,2.43951942781959,
1.89063144395813));
#248401=CARTESIAN_POINT('Ctrl Pts',(-2.1711622693735,2.3831451349451,1.8960719105151));
#248402=CARTESIAN_POINT('Ctrl Pts',(-2.39272725293461,2.17034370394175,
1.9160838496602));
#248403=CARTESIAN_POINT('Ctrl Pts',(-2.53667947232337,2.00019283811771,
1.93118385179018));
#248404=CARTESIAN_POINT('Ctrl Pts',(-2.73385635827691,1.71126127713571,
1.95475449451254));
#248405=CARTESIAN_POINT('Ctrl Pts',(-2.79944173820837,1.60172335112025,
1.9632741085455));
#248406=CARTESIAN_POINT('Ctrl Pts',(-2.87175346579648,1.46287034557162,
1.97334898230511));
#248407=CARTESIAN_POINT('Ctrl Pts',(-2.88479407301754,1.43698326596089,
1.97519756130324));
#248408=CARTESIAN_POINT('Ctrl Pts',(-2.90331503417518,1.39894844732685,
1.97786675765037));
#248409=CARTESIAN_POINT('Ctrl Pts',(-2.90907173679522,1.38693784670786,
1.9787029014807));
#248410=CARTESIAN_POINT('Ctrl Pts',(-2.91910515437681,1.36566712102551,
1.98017140532332));
#248411=CARTESIAN_POINT('Ctrl Pts',(-2.9234125790301,1.35642194403075,1.98080558335603));
#248412=CARTESIAN_POINT('Ctrl Pts',(-2.9327007832531,1.33623656599427,1.98218123526536));
#248413=CARTESIAN_POINT('Ctrl Pts',(-2.93766430631603,1.32528882834039,
1.98292167889361));
#248414=CARTESIAN_POINT('Ctrl Pts',(-2.95144387796549,1.29443826601513,
1.98499308316205));
#248415=CARTESIAN_POINT('Ctrl Pts',(-2.96011988237994,1.27447311827945,
1.98631597109495));
#248416=CARTESIAN_POINT('Ctrl Pts',(-3.02005944895654,1.13262585127357,
1.99560099711645));
#248417=CARTESIAN_POINT('Ctrl Pts',(-3.06398752244789,1.00776425100688,
2.00318596802975));
#248418=CARTESIAN_POINT('Ctrl Pts',(-3.13893747152918,0.743888673340769,
2.01868324416095));
#248419=CARTESIAN_POINT('Ctrl Pts',(-3.16867440487929,0.604815865426179,
2.02656402916567));
#248420=CARTESIAN_POINT('Ctrl Pts',(-3.20464311655925,0.357722153633178,
2.04064324728881));
#248421=CARTESIAN_POINT('Ctrl Pts',(-3.21480116470452,0.250506898475419,
2.04677590744531));
#248422=CARTESIAN_POINT('Ctrl Pts',(-3.22167868485758,0.0956520733148445,
2.05581484351066));
#248423=CARTESIAN_POINT('Ctrl Pts',(-3.2227367334429,0.0482752566797369,
2.05860409443329));
#248424=CARTESIAN_POINT('Ctrl Pts',(-3.2227499586742,0.000595948182032424,
2.06144152017187));
#248425=CARTESIAN_POINT('Ctrl Pts',(-3.22275,0.000297973971232206,2.06145925399353));
#248426=CARTESIAN_POINT('Ctrl Pts',(-3.22275,-8.28983494685339E-13,2.06147698899067));
#248427=CARTESIAN_POINT('Origin',(0.,0.,-2.31077344927308));
#248428=CARTESIAN_POINT('',(-3.22275,5.4545833554047E-12,3.55815895351304));
#248429=CARTESIAN_POINT('',(-3.22275,-1.09907859225987E-10,3.31386231834285));
#248430=CARTESIAN_POINT('',(-3.22275,-3.50678552687464E-13,-2.31077344927308));
#248431=CARTESIAN_POINT('',(-3.2227498370861,0.00102472510551524,3.55809228455962));
#248432=CARTESIAN_POINT('Ctrl Pts',(-3.22275,5.4545833554047E-12,3.55815895351304));
#248433=CARTESIAN_POINT('Ctrl Pts',(-3.22275,0.00034157307004431,3.5581367286295));
#248434=CARTESIAN_POINT('Ctrl Pts',(-3.22274994569599,0.000683148107952332,
3.55811450564337));
#248435=CARTESIAN_POINT('Ctrl Pts',(-3.2227498370861,0.0010247251065684,
3.55809228455955));
#248436=CARTESIAN_POINT('Ctrl Pts',(-3.22274983586623,0.00102855442515937,
3.55809203544564));
#248437=CARTESIAN_POINT('Ctrl Pts',(-3.22273820483632,0.037471837150337,
3.55572124147969));
#248438=CARTESIAN_POINT('Ctrl Pts',(-3.22210841499878,0.0739142782399589,
3.55337358624429));
#248439=CARTESIAN_POINT('Ctrl Pts',(-3.22039852623606,0.123826453175173,
3.55019669928976));
#248440=CARTESIAN_POINT('Ctrl Pts',(-3.21985180090162,0.137310060918356,
3.54934232982271));
#248441=CARTESIAN_POINT('Ctrl Pts',(-3.21875217860318,0.160785916127353,
3.5478619901182));
#248442=CARTESIAN_POINT('Ctrl Pts',(-3.2182374079862,0.170779653668331,
3.54723407118625));
#248443=CARTESIAN_POINT('Ctrl Pts',(-3.21713844001681,0.190340995160105,
3.54600965721298));
#248444=CARTESIAN_POINT('Ctrl Pts',(-3.21655808997559,0.19990872924855,
3.54541296667737));
#248445=CARTESIAN_POINT('Ctrl Pts',(-3.21521109565124,0.220588360296694,
3.54412816129711));
#248446=CARTESIAN_POINT('Ctrl Pts',(-3.21442952688872,0.231699028081275,
3.54344087228762));
#248447=CARTESIAN_POINT('Ctrl Pts',(-3.212157952319,0.261763860703516,3.54158871112551));
#248448=CARTESIAN_POINT('Ctrl Pts',(-3.21055777090555,0.280709580645788,
3.54042973636602));
#248449=CARTESIAN_POINT('Ctrl Pts',(-3.2021098880226,0.371176249519088,
3.53493002489401));
#248450=CARTESIAN_POINT('Ctrl Pts',(-3.19303893754264,0.442474294200699,
3.53069849107339));
#248451=CARTESIAN_POINT('Ctrl Pts',(-3.15089964033089,0.703608249011111,
3.5153874968761));
#248452=CARTESIAN_POINT('Ctrl Pts',(-3.10321372094272,0.89067809468383,
3.50476689358768));
#248453=CARTESIAN_POINT('Ctrl Pts',(-2.9801910097107,1.23932235808301,3.48398237337513));
#248454=CARTESIAN_POINT('Ctrl Pts',(-2.90763474381403,1.40110942729422,
3.47388534453785));
#248455=CARTESIAN_POINT('Ctrl Pts',(-2.80553478614379,1.58627831501247,
3.46126581227636));
#248456=CARTESIAN_POINT('Ctrl Pts',(-2.78841865456458,1.6161762278175,3.45919389511154));
#248457=CARTESIAN_POINT('Ctrl Pts',(-2.76057494076108,1.66305339018981,
3.45588757526961));
#248458=CARTESIAN_POINT('Ctrl Pts',(-2.7501619970267,1.68021711219019,3.45466449058606));
#248459=CARTESIAN_POINT('Ctrl Pts',(-2.73024739295164,1.71236135046118,
3.45234966025601));
#248460=CARTESIAN_POINT('Ctrl Pts',(-2.72078104398913,1.72736293584379,
3.45125923462637));
#248461=CARTESIAN_POINT('Ctrl Pts',(-2.69911523808883,1.76107736011302,
3.44878529063712));
#248462=CARTESIAN_POINT('Ctrl Pts',(-2.68684419563857,1.77974289299521,
3.44739915891648));
#248463=CARTESIAN_POINT('Ctrl Pts',(-2.64896457219779,1.83607704426674,
3.44316449279439));
#248464=CARTESIAN_POINT('Ctrl Pts',(-2.62275143509932,1.87333040048548,
3.44029350634888));
#248465=CARTESIAN_POINT('Ctrl Pts',(-2.48152057090043,2.06526678645987,
3.42512004087489));
#248466=CARTESIAN_POINT('Ctrl Pts',(-2.35360178063439,2.20993422866937,
3.41232271326636));
#248467=CARTESIAN_POINT('Ctrl Pts',(-2.09758483754045,2.45187943035928,
3.38856857895729));
#248468=CARTESIAN_POINT('Ctrl Pts',(-1.97364074522804,2.55270835441169,
3.3777155285123));
#248469=CARTESIAN_POINT('Ctrl Pts',(-1.80312920065712,2.67154886197651,
3.36397108369889));
#248470=CARTESIAN_POINT('Ctrl Pts',(-1.76290539056583,2.69826115947316,
3.36080883179749));
#248471=CARTESIAN_POINT('Ctrl Pts',(-1.69410864082025,2.74175303542997,
3.35555193382845));
#248472=CARTESIAN_POINT('Ctrl Pts',(-1.66585034885558,2.75901370155642,
3.35343438149211));
#248473=CARTESIAN_POINT('Ctrl Pts',(-1.62539047440193,2.78287899714211,
3.35046653290972));
#248474=CARTESIAN_POINT('Ctrl Pts',(-1.61340554212683,2.78984449027362,
3.34959524338327));
#248475=CARTESIAN_POINT('Ctrl Pts',(-1.592631734027,2.80173932553383,3.34809899809088));
#248476=CARTESIAN_POINT('Ctrl Pts',(-1.58386409631974,2.80670511879655,
3.34747177838447));
#248477=CARTESIAN_POINT('Ctrl Pts',(-1.56526229419403,2.81712583459774,
3.34615021692128));
#248478=CARTESIAN_POINT('Ctrl Pts',(-1.55542273047473,2.82257048733811,
3.34545650807029));
#248479=CARTESIAN_POINT('Ctrl Pts',(-1.52844038516536,2.83731703153946,
3.34356820367578));
#248480=CARTESIAN_POINT('Ctrl Pts',(-1.51124103858267,2.84651515266133,
3.34237990363718));
#248481=CARTESIAN_POINT('Ctrl Pts',(-1.42456875341322,2.89186001139771,
3.33646306224073));
#248482=CARTESIAN_POINT('Ctrl Pts',(-1.35387262078618,2.92562496231921,
3.33186485165266));
#248483=CARTESIAN_POINT('Ctrl Pts',(-1.08476213433725,3.04230669904457,
3.31494644234621));
#248484=CARTESIAN_POINT('Ctrl Pts',(-0.879441533515686,3.10788230088653,
3.30316354797984));
#248485=CARTESIAN_POINT('Ctrl Pts',(-0.522907704142829,3.18355510868616,
3.28255340940763));
#248486=CARTESIAN_POINT('Ctrl Pts',(-0.374740084232653,3.20437479895645,
3.27395340601488));
#248487=CARTESIAN_POINT('Ctrl Pts',(-0.192449014036389,3.21717115309778,
3.26303687384691));
#248488=CARTESIAN_POINT('Ctrl Pts',(-0.159191599858462,3.21898815812914,
3.26103225874643));
#248489=CARTESIAN_POINT('Ctrl Pts',(-0.106098357815305,3.22106409703047,
3.25780868747769));
#248490=CARTESIAN_POINT('Ctrl Pts',(-0.0862774425607045,3.22165593358697,
3.25660007984606));
#248491=CARTESIAN_POINT('Ctrl Pts',(-0.0486759815078143,3.22243143545234,
3.25429692818853));
#248492=CARTESIAN_POINT('Ctrl Pts',(-0.0308968571526456,3.22265093853157,
3.25320354097748));
#248493=CARTESIAN_POINT('Ctrl Pts',(0.00962817657580653,3.22281588320249,
3.25070093048315));
#248494=CARTESIAN_POINT('Ctrl Pts',(0.0323733190128121,3.22266765968807,
3.24928885104319));
#248495=CARTESIAN_POINT('Ctrl Pts',(0.0918844051583125,3.22164976955488,
3.24557397995792));
#248496=CARTESIAN_POINT('Ctrl Pts',(0.128639545142351,3.22039154001892,
3.24325933036316));
#248497=CARTESIAN_POINT('Ctrl Pts',(0.43190691043073,3.20480992990229,3.22398762914779));
#248498=CARTESIAN_POINT('Ctrl Pts',(0.695673085753161,3.15805911561848,
3.20599016096453));
#248499=CARTESIAN_POINT('Ctrl Pts',(1.10240952090309,3.03249948105887,3.17724350798005));
#248500=CARTESIAN_POINT('Ctrl Pts',(1.25056238363601,2.97446872652255,3.16657749830486));
#248501=CARTESIAN_POINT('Ctrl Pts',(1.41346709145941,2.89632561825077,3.15503484744299));
#248502=CARTESIAN_POINT('Ctrl Pts',(1.43299647288497,2.88671309167331,3.15365444644216));
#248503=CARTESIAN_POINT('Ctrl Pts',(1.46289971728469,2.87161619953125,3.15154767000034));
#248504=CARTESIAN_POINT('Ctrl Pts',(1.47334311449402,2.86627201383727,3.15081320642945));
#248505=CARTESIAN_POINT('Ctrl Pts',(1.49261149654056,2.85627869221506,3.14946084621743));
#248506=CARTESIAN_POINT('Ctrl Pts',(1.50144413164689,2.85164558990546,3.1488420368096));
#248507=CARTESIAN_POINT('Ctrl Pts',(1.52156866650713,2.84096996822715,3.14743452475259));
#248508=CARTESIAN_POINT('Ctrl Pts',(1.53284619509809,2.83490107803413,3.14664747500901));
#248509=CARTESIAN_POINT('Ctrl Pts',(1.56769098308754,2.81588097551683,3.14422004275143));
#248510=CARTESIAN_POINT('Ctrl Pts',(1.59113318352275,2.80270155115572,3.14259317913196));
#248511=CARTESIAN_POINT('Ctrl Pts',(1.80403676723555,2.67947277931232,3.12784969511117));
#248512=CARTESIAN_POINT('Ctrl Pts',(1.9820041024881,2.55064866409071,3.11573089069606));
#248513=CARTESIAN_POINT('Ctrl Pts',(2.27814421780201,2.28642939986175,3.09349983088599));
#248514=CARTESIAN_POINT('Ctrl Pts',(2.40072549248626,2.15736160707306,3.08348084110783));
#248515=CARTESIAN_POINT('Ctrl Pts',(2.54574313657052,1.97691786424192,3.06985437633003));
#248516=CARTESIAN_POINT('Ctrl Pts',(2.57839055992683,1.93414425145221,3.06665114727982));
#248517=CARTESIAN_POINT('Ctrl Pts',(2.62393296537588,1.87127268127357,3.06196919740733));
#248518=CARTESIAN_POINT('Ctrl Pts',(2.63770034035068,1.85181600663214,3.06052384425123));
#248519=CARTESIAN_POINT('Ctrl Pts',(2.66144103184456,1.81746265306636,3.05797711547961));
#248520=CARTESIAN_POINT('Ctrl Pts',(2.67150833638669,1.80263197840953,3.05687934713849));
#248521=CARTESIAN_POINT('Ctrl Pts',(2.69215892592693,1.77165755238502,3.05458968550711));
#248522=CARTESIAN_POINT('Ctrl Pts',(2.70272190866169,1.75550118886462,3.05339709414926));
#248523=CARTESIAN_POINT('Ctrl Pts',(2.72979398434849,1.71327019695115,3.05028367826437));
#248524=CARTESIAN_POINT('Ctrl Pts',(2.74607450114559,1.68705207189909,3.04835457554762));
#248525=CARTESIAN_POINT('Ctrl Pts',(2.81393116932687,1.5741905120779,3.04006392425001));
#248526=CARTESIAN_POINT('Ctrl Pts',(2.86179773004745,1.48539377569277,3.0335722389042));
#248527=CARTESIAN_POINT('Ctrl Pts',(2.99595093446929,1.20588892317464,3.01323692386304));
#248528=CARTESIAN_POINT('Ctrl Pts',(3.06789238929154,1.00891577297083,2.99900515589237));
#248529=CARTESIAN_POINT('Ctrl Pts',(3.15103602008227,0.687200149257676,
2.97662867142827));
#248530=CARTESIAN_POINT('Ctrl Pts',(3.1749871855883,0.566333859810984,2.96841794070674));
#248531=CARTESIAN_POINT('Ctrl Pts',(3.19586231268883,0.416389820650886,
2.95868158424196));
#248532=CARTESIAN_POINT('Ctrl Pts',(3.19939131884632,0.38834484471867,2.95687982261189));
#248533=CARTESIAN_POINT('Ctrl Pts',(3.20400601091198,0.347321830891428,
2.95427589144665));
#248534=CARTESIAN_POINT('Ctrl Pts',(3.20538263977297,0.334378705055904,
2.95345891125379));
#248535=CARTESIAN_POINT('Ctrl Pts',(3.20767555737348,0.311503690749481,
2.95202353350335));
#248536=CARTESIAN_POINT('Ctrl Pts',(3.20862420551826,0.30157544265629,2.95140339779013));
#248537=CARTESIAN_POINT('Ctrl Pts',(3.21058883698534,0.279954668556267,
2.9500591909348));
#248538=CARTESIAN_POINT('Ctrl Pts',(3.21158705443249,0.268260877584965,
2.94933609668564));
#248539=CARTESIAN_POINT('Ctrl Pts',(3.21420783812306,0.235444895199184,
2.94731727043798));
#248540=CARTESIAN_POINT('Ctrl Pts',(3.21568608858832,0.214311359288031,
2.94602918755814));
#248541=CARTESIAN_POINT('Ctrl Pts',(3.22414844386557,0.0733792936525302,
2.93751054944187));
#248542=CARTESIAN_POINT('Ctrl Pts',(3.2246457926928,-0.0467273835608476,
2.93059136498316));
#248543=CARTESIAN_POINT('Ctrl Pts',(3.21579418261589,-0.21773281124742,
2.92088397833321));
#248544=CARTESIAN_POINT('Ctrl Pts',(3.21192856197228,-0.268802707770167,
2.91800357849531));
#248545=CARTESIAN_POINT('Ctrl Pts',(3.19343181518326,-0.454305345317533,
2.90754732518912));
#248546=CARTESIAN_POINT('Ctrl Pts',(3.17156195260599,-0.587872414287476,
2.90002477438403));
#248547=CARTESIAN_POINT('Ctrl Pts',(3.12145068564085,-0.806609428056208,
2.88728179814289));
#248548=CARTESIAN_POINT('Ctrl Pts',(3.09793332186683,-0.892681731611156,
2.88215640094006));
#248549=CARTESIAN_POINT('Ctrl Pts',(3.05234085060794,-1.03588933200876,
2.87334870506628));
#248550=CARTESIAN_POINT('Ctrl Pts',(3.03215261074513,-1.09357268218618,
2.86972236067306));
#248551=CARTESIAN_POINT('Ctrl Pts',(3.00140161624102,-1.17402399740174,
2.86453547998867));
#248552=CARTESIAN_POINT('Ctrl Pts',(2.99219348922953,-1.19729782332667,
2.86301946792215));
#248553=CARTESIAN_POINT('Ctrl Pts',(2.97585308277802,-1.23723253664806,
2.86039026907377));
#248554=CARTESIAN_POINT('Ctrl Pts',(2.96884954929545,-1.25394507564014,
2.85928142864144));
#248555=CARTESIAN_POINT('Ctrl Pts',(2.95426178019234,-1.28794851116944,
2.85700748722554));
#248556=CARTESIAN_POINT('Ctrl Pts',(2.94666579932208,-1.30523357158907,
2.85584202290379));
#248557=CARTESIAN_POINT('Ctrl Pts',(2.9270682821886,-1.34878567520039,2.85288076208835));
#248558=CARTESIAN_POINT('Ctrl Pts',(2.91486494312401,-1.37495956414327,
2.85107814981408));
#248559=CARTESIAN_POINT('Ctrl Pts',(2.86629731419576,-1.47557476667705,
2.84405746363688));
#248560=CARTESIAN_POINT('Ctrl Pts',(2.8274221226308,-1.54876187959743,2.83875414919275));
#248561=CARTESIAN_POINT('Ctrl Pts',(2.67273414190372,-1.81470541655516,
2.81873425374766));
#248562=CARTESIAN_POINT('Ctrl Pts',(2.53967868150552,-1.99666549417463,
2.803463033712));
#248563=CARTESIAN_POINT('Ctrl Pts',(2.32431186708538,-2.23448457818065,
2.78183730636758));
#248564=CARTESIAN_POINT('Ctrl Pts',(2.2566689232045,-2.30277974467909,2.7754038205973));
#248565=CARTESIAN_POINT('Ctrl Pts',(2.15958146972077,-2.39240993042038,
2.7667481715331));
#248566=CARTESIAN_POINT('Ctrl Pts',(2.13268125929044,-2.41642054758717,
2.76440685510545));
#248567=CARTESIAN_POINT('Ctrl Pts',(2.08525641111725,-2.45734204409144,
2.76038478612001));
#248568=CARTESIAN_POINT('Ctrl Pts',(2.06491525222595,-2.47445940115774,
2.75869224757462));
#248569=CARTESIAN_POINT('Ctrl Pts',(2.03454596640609,-2.49938023755613,
2.75621587841797));
#248570=CARTESIAN_POINT('Ctrl Pts',(2.02468032253591,-2.50737880375097,
2.75541914863242));
#248571=CARTESIAN_POINT('Ctrl Pts',(2.00774602050674,-2.52094315911444,
2.75406509516637));
#248572=CARTESIAN_POINT('Ctrl Pts',(2.00070103443402,-2.52653792212658,
2.75350575306733));
#248573=CARTESIAN_POINT('Ctrl Pts',(1.98454794107962,-2.53925593830009,
2.75223236105411));
#248574=CARTESIAN_POINT('Ctrl Pts',(1.97542484678221,-2.54635974185872,
2.75151967042854));
#248575=CARTESIAN_POINT('Ctrl Pts',(1.95009258142763,-2.56586692007177,
2.74955803571339));
#248576=CARTESIAN_POINT('Ctrl Pts',(1.93380320903282,-2.5781658838638,2.74831606767961));
#248577=CARTESIAN_POINT('Ctrl Pts',(1.83863505924553,-2.64861120169602,
2.74116483858797));
#248578=CARTESIAN_POINT('Ctrl Pts',(1.75724649293034,-2.70329588197189,
2.73546181601185));
#248579=CARTESIAN_POINT('Ctrl Pts',(1.53256202557386,-2.83981730948932,
2.72043723687877));
#248580=CARTESIAN_POINT('Ctrl Pts',(1.38527071204616,-2.9145047442422,2.71131554183506));
#248581=CARTESIAN_POINT('Ctrl Pts',(1.0705417756412,-3.04482176041822,2.69216110362256));
#248582=CARTESIAN_POINT('Ctrl Pts',(0.902971123622289,-3.09864996758937,
2.68213411828887));
#248583=CARTESIAN_POINT('Ctrl Pts',(0.698353142185645,-3.14636365309048,
2.66959437576612));
#248584=CARTESIAN_POINT('Ctrl Pts',(0.664723905270156,-3.15363969763416,
2.6675250051704));
#248585=CARTESIAN_POINT('Ctrl Pts',(0.611307864430769,-3.16430448979699,
2.66422181693925));
#248586=CARTESIAN_POINT('Ctrl Pts',(0.591594260856632,-3.16804930700748,
2.66299927997776));
#248587=CARTESIAN_POINT('Ctrl Pts',(0.554388869425165,-3.174757510376,2.66068490786022));
#248588=CARTESIAN_POINT('Ctrl Pts',(0.536905017613769,-3.17776104363946,
2.65959438665336));
#248589=CARTESIAN_POINT('Ctrl Pts',(0.497337561215314,-3.18422243762676,
2.65711943665369));
#248590=CARTESIAN_POINT('Ctrl Pts',(0.475241167969115,-3.18759517101655,
2.65573238589707));
#248591=CARTESIAN_POINT('Ctrl Pts',(0.409446430128924,-3.19693858378569,
2.65158686358277));
#248592=CARTESIAN_POINT('Ctrl Pts',(0.365660089473951,-3.20224219572318,
2.64880780033021));
#248593=CARTESIAN_POINT('Ctrl Pts',(0.10027185813783,-3.22887336654518,
2.63183484668577));
#248594=CARTESIAN_POINT('Ctrl Pts',(-0.122908437967073,-3.22808618412978,
2.61695712750408));
#248595=CARTESIAN_POINT('Ctrl Pts',(-0.48094219470975,-3.18962847467594,
2.59262365338703));
#248596=CARTESIAN_POINT('Ctrl Pts',(-0.61662219192827,-3.16619891788591,
2.58330775181483));
#248597=CARTESIAN_POINT('Ctrl Pts',(-0.793751734870082,-3.12378989679679,
2.57129422204483));
#248598=CARTESIAN_POINT('Ctrl Pts',(-0.836890628882467,-3.11251017509812,
2.56838101615001));
#248599=CARTESIAN_POINT('Ctrl Pts',(-0.909806294157113,-3.09181888516357,
2.56349350448069));
#248600=CARTESIAN_POINT('Ctrl Pts',(-0.939705018092214,-3.08286330483247,
2.56150001261691));
#248601=CARTESIAN_POINT('Ctrl Pts',(-0.982383558607825,-3.06940115554044,
2.55867429339445));
#248602=CARTESIAN_POINT('Ctrl Pts',(-0.995271420015805,-3.06524643798228,
2.557823617158));
#248603=CARTESIAN_POINT('Ctrl Pts',(-1.0176607305634,-3.05787259784906,
2.5563508265253));
#248604=CARTESIAN_POINT('Ctrl Pts',(-1.02717390512542,-3.0546901588129,
2.55572664750061));
#248605=CARTESIAN_POINT('Ctrl Pts',(-1.04747672608429,-3.04779268919275,
2.55439810189948));
#248606=CARTESIAN_POINT('Ctrl Pts',(-1.05826163582326,-3.04406473114278,
2.55369448788541));
#248607=CARTESIAN_POINT('Ctrl Pts',(-1.08764943832201,-3.033731356943,2.55178240636846));
#248608=CARTESIAN_POINT('Ctrl Pts',(-1.10621213648137,-3.02701205809077,
2.55058035387507));
#248609=CARTESIAN_POINT('Ctrl Pts',(-1.20492380877698,-2.99025121530015,
2.54421281295866));
#248610=CARTESIAN_POINT('Ctrl Pts',(-1.28392059334139,-2.95719363660581,
2.53920388534461));
#248611=CARTESIAN_POINT('Ctrl Pts',(-1.51895211333019,-2.84764358494459,
2.52430183747064));
#248612=CARTESIAN_POINT('Ctrl Pts',(-1.67020713366898,-2.76164872483479,
2.51469961725588));
#248613=CARTESIAN_POINT('Ctrl Pts',(-1.96281191971226,-2.56241793403974,
2.49480930804273));
#248614=CARTESIAN_POINT('Ctrl Pts',(-2.10303002708986,-2.4486465011688,
2.48453813131786));
#248615=CARTESIAN_POINT('Ctrl Pts',(-2.2579082061274,-2.29981782158523,
2.4717201379051));
#248616=CARTESIAN_POINT('Ctrl Pts',(-2.2824352725212,-2.2754780967696,2.46964212293087));
#248617=CARTESIAN_POINT('Ctrl Pts',(-2.32060166867222,-2.23636521497344,
2.46632829842681));
#248618=CARTESIAN_POINT('Ctrl Pts',(-2.33450265728251,-2.22185030869405,
2.46510389631652));
#248619=CARTESIAN_POINT('Ctrl Pts',(-2.36041359797178,-2.19428342817489,
2.46278794889375));
#248620=CARTESIAN_POINT('Ctrl Pts',(-2.37245337679163,-2.18126043190607,
2.46169773806644));
#248621=CARTESIAN_POINT('Ctrl Pts',(-2.39938992298103,-2.15163728723446,
2.4592261534708));
#248622=CARTESIAN_POINT('Ctrl Pts',(-2.41422296463741,-2.13498066865706,
2.45784218669277));
#248623=CARTESIAN_POINT('Ctrl Pts',(-2.45870132023615,-2.08397788262185,
2.45362096846656));
#248624=CARTESIAN_POINT('Ctrl Pts',(-2.48779432700483,-2.04915959609886,
2.45076147385152));
#248625=CARTESIAN_POINT('Ctrl Pts',(-2.63794060419737,-1.86155381978938,
2.43546293057711));
#248626=CARTESIAN_POINT('Ctrl Pts',(-2.74566309043722,-1.69865422440675,
2.42251617183928));
#248627=CARTESIAN_POINT('Ctrl Pts',(-2.91289611353815,-1.38785392708609,
2.3987111821227));
#248628=CARTESIAN_POINT('Ctrl Pts',(-2.97745277950062,-1.24333428675556,
2.38796211958973));
#248629=CARTESIAN_POINT('Ctrl Pts',(-3.05544361208147,-1.02737493749487,
2.37278034444477));
#248630=CARTESIAN_POINT('Ctrl Pts',(-3.07749691403045,-0.95929625738058,
2.36811743229979));
#248631=CARTESIAN_POINT('Ctrl Pts',(-3.10231684408046,-0.872972897974947,
2.3624037469124));
#248632=CARTESIAN_POINT('Ctrl Pts',(-3.10721698217725,-0.85536784092586,
2.36124873170681));
#248633=CARTESIAN_POINT('Ctrl Pts',(-3.11482024736893,-0.827123239765063,
2.35941310431767));
#248634=CARTESIAN_POINT('Ctrl Pts',(-3.11761914442909,-0.81651019946153,
2.35872727497787));
#248635=CARTESIAN_POINT('Ctrl Pts',(-3.1228806622513,-0.796137698523732,
2.35741854861118));
#248636=CARTESIAN_POINT('Ctrl Pts',(-3.12535184403775,-0.786380772181157,
2.3567951999368));
#248637=CARTESIAN_POINT('Ctrl Pts',(-3.13070829353867,-0.764807870739081,
2.35542425001323));
#248638=CARTESIAN_POINT('Ctrl Pts',(-3.13357248809667,-0.752986700465426,
2.35467782873675));
#248639=CARTESIAN_POINT('Ctrl Pts',(-3.14349140876524,-0.711012162798436,
2.35204355768091));
#248640=CARTESIAN_POINT('Ctrl Pts',(-3.15017862076739,-0.680772611206659,
2.35017517905102));
#248641=CARTESIAN_POINT('Ctrl Pts',(-3.20032911924268,-0.437404332589009,
2.33533964358688));
#248642=CARTESIAN_POINT('Ctrl Pts',(-3.22255453540802,-0.220443682782572,
2.32331999856126));
#248643=CARTESIAN_POINT('Ctrl Pts',(-3.22274957214941,-0.00191754697872536,
2.3110756989822));
#248644=CARTESIAN_POINT('Ctrl Pts',(-3.22275000000004,-0.000958768568118341,
2.3110219753754));
#248645=CARTESIAN_POINT('Ctrl Pts',(-3.22275,1.20843135519762E-10,2.31096825019553));
#248646=CARTESIAN_POINT('Ctrl Pts',(-3.22275,-8.28983494685339E-13,2.06147698899067));
#248647=CARTESIAN_POINT('Ctrl Pts',(-3.22274999999999,-0.0339972115249406,
2.06350045582317));
#248648=CARTESIAN_POINT('Ctrl Pts',(-3.22221203950403,-0.0679913131819596,
2.06553925904328));
#248649=CARTESIAN_POINT('Ctrl Pts',(-3.22043179503059,-0.124227760372896,
2.06894080846313));
#248650=CARTESIAN_POINT('Ctrl Pts',(-3.21949650969314,-0.146477536901708,
2.0702940719618));
#248651=CARTESIAN_POINT('Ctrl Pts',(-3.21738344095369,-0.186785377642087,
2.07275993161626));
#248652=CARTESIAN_POINT('Ctrl Pts',(-3.21628400070987,-0.204846745826508,
2.07387005087609));
#248653=CARTESIAN_POINT('Ctrl Pts',(-3.21358425686546,-0.243787334517675,
2.07627512342972));
#248654=CARTESIAN_POINT('Ctrl Pts',(-3.21193244198802,-0.26466204057638,
2.07757163061838));
#248655=CARTESIAN_POINT('Ctrl Pts',(-3.20678265582034,-0.322560899965624,
2.08118841681156));
#248656=CARTESIAN_POINT('Ctrl Pts',(-3.20284716525184,-0.359541913790397,
2.08352214890238));
#248657=CARTESIAN_POINT('Ctrl Pts',(-3.17322558534967,-0.5985102625577,
2.09876131070165));
#248658=CARTESIAN_POINT('Ctrl Pts',(-3.12908986305313,-0.797713385329973,
2.11224486322262));
#248659=CARTESIAN_POINT('Ctrl Pts',(-2.99914551331924,-1.19964385980282,
2.14071567900263));
#248660=CARTESIAN_POINT('Ctrl Pts',(-2.91077521656446,-1.40050675599089,
2.15566473164271));
#248661=CARTESIAN_POINT('Ctrl Pts',(-2.78920641741812,-1.61468099612505,
2.17148927341377));
#248662=CARTESIAN_POINT('Ctrl Pts',(-2.77538784506512,-1.63831913305582,
2.17323345583134));
#248663=CARTESIAN_POINT('Ctrl Pts',(-2.75455631395967,-1.6729335186778,
2.17578084657559));
#248664=CARTESIAN_POINT('Ctrl Pts',(-2.74777577437603,-1.68404731288453,
2.17659771413546));
#248665=CARTESIAN_POINT('Ctrl Pts',(-2.73557430817447,-1.7037765007393,
2.17804554150918));
#248666=CARTESIAN_POINT('Ctrl Pts',(-2.73017971346998,-1.71240763275635,
2.17867812660426));
#248667=CARTESIAN_POINT('Ctrl Pts',(-2.71820344872484,-1.73136870282536,
2.18006598769917));
#248668=CARTESIAN_POINT('Ctrl Pts',(-2.71160371612674,-1.74168678923196,
2.1808200798644));
#248669=CARTESIAN_POINT('Ctrl Pts',(-2.69217991172997,-1.77167612156242,
2.18300925680772));
#248670=CARTESIAN_POINT('Ctrl Pts',(-2.67919918337484,-1.7912455902901,
2.18443453910911));
#248671=CARTESIAN_POINT('Ctrl Pts',(-2.64885696131784,-1.8359210047047,
2.18768504944634));
#248672=CARTESIAN_POINT('Ctrl Pts',(-2.63135017996808,-1.86092597959875,
2.18950194148782));
#248673=CARTESIAN_POINT('Ctrl Pts',(-2.5704963333159,-1.94526742986716,
2.19563570470074));
#248674=CARTESIAN_POINT('Ctrl Pts',(-2.52547446985483,-2.00337134908094,
2.19987086709616));
#248675=CARTESIAN_POINT('Ctrl Pts',(-2.39031516647057,-2.16599799259079,
2.21190962411294));
#248676=CARTESIAN_POINT('Ctrl Pts',(-2.29540182003195,-2.26633772133248,
2.21957536104972));
#248677=CARTESIAN_POINT('Ctrl Pts',(-2.05578107840721,-2.48911188604598,
2.23793647238236));
#248678=CARTESIAN_POINT('Ctrl Pts',(-1.9061574350839,-2.60546837937968,
2.2486805173335));
#248679=CARTESIAN_POINT('Ctrl Pts',(-1.71756047742832,-2.72715017459533,
2.2620630584129));
#248680=CARTESIAN_POINT('Ctrl Pts',(-1.6876061982865,-2.7457871807857,2.26418312372979));
#248681=CARTESIAN_POINT('Ctrl Pts',(-1.63956900594751,-2.77459204583927,
2.26757767800525));
#248682=CARTESIAN_POINT('Ctrl Pts',(-1.62168296709077,-2.78508381729775,
2.26884043323253));
#248683=CARTESIAN_POINT('Ctrl Pts',(-1.588132153922,-2.80433161965916,2.2712075798081));
#248684=CARTESIAN_POINT('Ctrl Pts',(-1.57249301099894,-2.81313086813159,
2.27231036831007));
#248685=CARTESIAN_POINT('Ctrl Pts',(-1.53710673728504,-2.83265341241917,
2.27480463908018));
#248686=CARTESIAN_POINT('Ctrl Pts',(-1.51731945614875,-2.84330162031279,
2.27619870795483));
#248687=CARTESIAN_POINT('Ctrl Pts',(-1.45784640883252,-2.87450847234073,
2.28038757177748));
#248688=CARTESIAN_POINT('Ctrl Pts',(-1.41784395180717,-2.8944487073069,
2.28320359355855));
#248689=CARTESIAN_POINT('Ctrl Pts',(-1.22417047088155,-2.98601187386396,
2.29683642588812));
#248690=CARTESIAN_POINT('Ctrl Pts',(-1.06544228436468,-3.04625647769654,
2.30802652857114));
#248691=CARTESIAN_POINT('Ctrl Pts',(-0.726255394145973,-3.1452292423351,
2.33176844904113));
#248692=CARTESIAN_POINT('Ctrl Pts',(-0.545694585095951,-3.18152997631991,
2.34431360247577));
#248693=CARTESIAN_POINT('Ctrl Pts',(-0.293218791259436,-3.21015193640287,
2.36111259404778));
#248694=CARTESIAN_POINT('Ctrl Pts',(-0.223169519390601,-3.21578133873182,
2.36569274733126));
#248695=CARTESIAN_POINT('Ctrl Pts',(-0.133920771989147,-3.22002284727679,
2.37138169220627));
#248696=CARTESIAN_POINT('Ctrl Pts',(-0.114846186987461,-3.22075958497019,
2.37258904283301));
#248697=CARTESIAN_POINT('Ctrl Pts',(-0.0844608778842142,-3.22166289881622,
2.37449758551501));
#248698=CARTESIAN_POINT('Ctrl Pts',(-0.07315420465038,-3.22193946947361,
2.37520452576081));
#248699=CARTESIAN_POINT('Ctrl Pts',(-0.0514673560231443,-3.22235572710195,
2.37655394969274));
#248700=CARTESIAN_POINT('Ctrl Pts',(-0.0410877128160776,-3.22250479020141,
2.37719690160708));
#248701=CARTESIAN_POINT('Ctrl Pts',(-0.0160513173086691,-3.22274335593215,
2.37874106916979));
#248702=CARTESIAN_POINT('Ctrl Pts',(-0.00139412330314588,-3.2227830299668,
2.37963957861804));
#248703=CARTESIAN_POINT('Ctrl Pts',(0.0501838199945576,-3.22257076037367,
2.3827836196372));
#248704=CARTESIAN_POINT('Ctrl Pts',(0.0871009188320858,-3.22178435192632,
2.38500194341372));
#248705=CARTESIAN_POINT('Ctrl Pts',(0.179674846434587,-3.21821985137548,
2.39050227532089));
#248706=CARTESIAN_POINT('Ctrl Pts',(0.235289657990019,-3.21463240364879,
2.39375007957079));
#248707=CARTESIAN_POINT('Ctrl Pts',(0.504586891057592,-3.19023440326406,
2.40931872998733));
#248708=CARTESIAN_POINT('Ctrl Pts',(0.71592571992699,-3.14954977598937,
2.42108682620467));
#248709=CARTESIAN_POINT('Ctrl Pts',(1.05898053129865,-3.04716506466833,
2.44135583743441));
#248710=CARTESIAN_POINT('Ctrl Pts',(1.19340190003298,-2.9970718712757,2.44961095275508));
#248711=CARTESIAN_POINT('Ctrl Pts',(1.35536145635372,-2.92408849102193,
2.46021483728581));
#248712=CARTESIAN_POINT('Ctrl Pts',(1.38645912946501,-2.90947231088525,
2.46228170572547));
#248713=CARTESIAN_POINT('Ctrl Pts',(1.43558260532636,-2.88541744135682,
2.46559898352912));
#248714=CARTESIAN_POINT('Ctrl Pts',(1.45376349272485,-2.87630021130383,
2.46683833165537));
#248715=CARTESIAN_POINT('Ctrl Pts',(1.48802369245221,-2.85871182824981,
2.46919642596796));
#248716=CARTESIAN_POINT('Ctrl Pts',(1.50412007560849,-2.85027553109285,
2.47031392294028));
#248717=CARTESIAN_POINT('Ctrl Pts',(1.54057490840569,-2.8307743440377,2.47286716260956));
#248718=CARTESIAN_POINT('Ctrl Pts',(1.56088692555879,-2.81962522267304,
2.47430583092269));
#248719=CARTESIAN_POINT('Ctrl Pts',(1.62322425619025,-2.78452870317254,
2.47877183664026));
#248720=CARTESIAN_POINT('Ctrl Pts',(1.66483047305611,-2.75985437622065,
2.48182479159486));
#248721=CARTESIAN_POINT('Ctrl Pts',(1.7607120434375,-2.70003516873833,2.48903446976324));
#248722=CARTESIAN_POINT('Ctrl Pts',(1.81451490788503,-2.66417558895296,
2.49321531438081));
#248723=CARTESIAN_POINT('Ctrl Pts',(2.0164143960751,-2.52065584478898,2.50942666581588));
#248724=CARTESIAN_POINT('Ctrl Pts',(2.15630676687972,-2.40207456011241,
2.52180052860347));
#248725=CARTESIAN_POINT('Ctrl Pts',(2.30467916522628,-2.25284754000171,
2.53601445098197));
#248726=CARTESIAN_POINT('Ctrl Pts',(2.32374682863003,-2.23317459837365,
2.53786352740111));
#248727=CARTESIAN_POINT('Ctrl Pts',(2.43689292444735,-2.11341840971826,
2.54896320770817));
#248728=CARTESIAN_POINT('Ctrl Pts',(2.52475522660024,-2.00763627908183,
2.55812820082239));
#248729=CARTESIAN_POINT('Ctrl Pts',(2.61846289356527,-1.87889514845465,
2.56830392637445));
#248730=CARTESIAN_POINT('Ctrl Pts',(2.63114077578863,-1.86109999237588,
2.56968998637514));
#248731=CARTESIAN_POINT('Ctrl Pts',(2.65052238328633,-1.83330128183385,
2.57182197569998));
#248732=CARTESIAN_POINT('Ctrl Pts',(2.65735241253575,-1.82338713956691,
2.57257586790359));
#248733=CARTESIAN_POINT('Ctrl Pts',(2.66986541922957,-1.80500421361638,
2.57396150634533));
#248734=CARTESIAN_POINT('Ctrl Pts',(2.67556380224138,-1.79654666295264,
2.57459423093243));
#248735=CARTESIAN_POINT('Ctrl Pts',(2.68859873259164,-1.77700061388987,
2.57604569339867));
#248736=CARTESIAN_POINT('Ctrl Pts',(2.69590690768322,-1.76589362251439,
2.57686257192101));
#248737=CARTESIAN_POINT('Ctrl Pts',(2.7188568685721,-1.73053963930116,2.57943881716627));
#248738=CARTESIAN_POINT('Ctrl Pts',(2.73424233037289,-1.70612693639275,
2.58118239465844));
#248739=CARTESIAN_POINT('Ctrl Pts',(2.81520117897665,-1.57375779140271,
2.59046617722703));
#248740=CARTESIAN_POINT('Ctrl Pts',(2.87471929866967,-1.46221294221823,
2.59769046703219));
#248741=CARTESIAN_POINT('Ctrl Pts',(3.01904123741079,-1.14865197939621,
2.61716800091635));
#248742=CARTESIAN_POINT('Ctrl Pts',(3.09005199176125,-0.941057169957835,
2.62921374744402));
#248743=CARTESIAN_POINT('Ctrl Pts',(3.1595318075088,-0.64137342489453,2.64697391288844));
#248744=CARTESIAN_POINT('Ctrl Pts',(3.17600067870114,-0.554092780345073,
2.652182324925));
#248745=CARTESIAN_POINT('Ctrl Pts',(3.19317466451042,-0.436633626085735,
2.65929646023212));
#248746=CARTESIAN_POINT('Ctrl Pts',(3.19709186897456,-0.406960504697855,
2.66110236644904));
#248747=CARTESIAN_POINT('Ctrl Pts',(3.20286470411744,-0.357982101182787,
2.66409940041464));
#248748=CARTESIAN_POINT('Ctrl Pts',(3.20496042372282,-0.338706590640208,
2.6652830031103));
#248749=CARTESIAN_POINT('Ctrl Pts',(3.2087144316238,-0.30101671723573,2.66760586713654));
#248750=CARTESIAN_POINT('Ctrl Pts',(3.21038844297154,-0.282604654140058,
2.66874459033441));
#248751=CARTESIAN_POINT('Ctrl Pts',(3.21398232187494,-0.238910145150559,
2.67145679301039));
#248752=CARTESIAN_POINT('Ctrl Pts',(3.21576240228028,-0.213617734340076,
2.67303455120055));
#248753=CARTESIAN_POINT('Ctrl Pts',(3.22081270796597,-0.127332995099941,
2.67844489826843));
#248754=CARTESIAN_POINT('Ctrl Pts',(3.22264724878694,-0.0662729042080321,
2.68232125166998));
#248755=CARTESIAN_POINT('Ctrl Pts',(3.22288888114103,0.0834610978155122,
2.69194855098586));
#248756=CARTESIAN_POINT('Ctrl Pts',(3.2193731253348,0.172084415841955,2.69775199704938));
#248757=CARTESIAN_POINT('Ctrl Pts',(3.20127563992011,0.395291039741049,
2.71260789526754));
#248758=CARTESIAN_POINT('Ctrl Pts',(3.18186249727505,0.529309173606279,
2.72175356688097));
#248759=CARTESIAN_POINT('Ctrl Pts',(3.14384997502572,0.710500450187193,
2.73426146210632));
#248760=CARTESIAN_POINT('Ctrl Pts',(3.13248147094975,0.75905435352147,2.73762660675216));
#248761=CARTESIAN_POINT('Ctrl Pts',(3.08976581720199,0.924133316236075,
2.74908182365362));
#248762=CARTESIAN_POINT('Ctrl Pts',(3.05300161350705,1.03916421854592,2.75709106547839));
#248763=CARTESIAN_POINT('Ctrl Pts',(3.00218702352582,1.1719439044718,2.76617262429214));
#248764=CARTESIAN_POINT('Ctrl Pts',(2.99430479183625,1.19193888688421,2.76753560223551));
#248765=CARTESIAN_POINT('Ctrl Pts',(2.98172580224073,1.22293574185562,2.76963971354062));
#248766=CARTESIAN_POINT('Ctrl Pts',(2.97716698273,1.23399244570938,2.77038849644178));
#248767=CARTESIAN_POINT('Ctrl Pts',(2.96864024868737,1.25435038281447,2.7717635769591));
#248768=CARTESIAN_POINT('Ctrl Pts',(2.96469008596543,1.26365838217377,2.7723908508708));
#248769=CARTESIAN_POINT('Ctrl Pts',(2.95542156122623,1.28521565208063,2.77384043587277));
#248770=CARTESIAN_POINT('Ctrl Pts',(2.95007080783506,1.29745062338559,2.77466080282308));
#248771=CARTESIAN_POINT('Ctrl Pts',(2.93278997367838,1.33630514092619,2.77725960559082));
#248772=CARTESIAN_POINT('Ctrl Pts',(2.92057410786756,1.36279693028146,2.77902186013557));
#248773=CARTESIAN_POINT('Ctrl Pts',(2.85225312513648,1.50582083661421,2.78850239256062));
#248774=CARTESIAN_POINT('Ctrl Pts',(2.78952604380372,1.61907244460509,2.79588986640193));
#248775=CARTESIAN_POINT('Ctrl Pts',(2.59824043710923,1.92014257282073,2.81600137455967));
#248776=CARTESIAN_POINT('Ctrl Pts',(2.45637092190247,2.09858048985633,2.82851403657614));
#248777=CARTESIAN_POINT('Ctrl Pts',(2.24130872105471,2.31709629455826,2.84629415794579));
#248778=CARTESIAN_POINT('Ctrl Pts',(2.1836487816645,2.37151355884884,2.85095993644486));
#248779=CARTESIAN_POINT('Ctrl Pts',(2.10240051528213,2.44271527088062,2.85744155644524));
#248780=CARTESIAN_POINT('Ctrl Pts',(2.08050364850787,2.46139194544846,2.85917958194086));
#248781=CARTESIAN_POINT('Ctrl Pts',(2.04509837914269,2.49078044643053,2.86197751725359));
#248782=CARTESIAN_POINT('Ctrl Pts',(2.03174876338672,2.50168174580004,2.86302975170819));
#248783=CARTESIAN_POINT('Ctrl Pts',(2.00397955546707,2.52398920538355,2.86521332371793));
#248784=CARTESIAN_POINT('Ctrl Pts',(1.98954854180354,2.53538007907261,2.8663452126846));
#248785=CARTESIAN_POINT('Ctrl Pts',(1.95548045170669,2.56180117512994,2.86901109167864));
#248786=CARTESIAN_POINT('Ctrl Pts',(1.9357664901031,2.57672992366248,2.87054896567277));
#248787=CARTESIAN_POINT('Ctrl Pts',(1.86987923366042,2.62544136156591,2.87567426263755));
#248788=CARTESIAN_POINT('Ctrl Pts',(1.82298036366683,2.65821982215202,2.87929943821583));
#248789=CARTESIAN_POINT('Ctrl Pts',(1.54499861383155,2.84168918926618,2.90066598035169));
#248790=CARTESIAN_POINT('Ctrl Pts',(1.29622887312025,2.96343710384678,2.91945317482165));
#248791=CARTESIAN_POINT('Ctrl Pts',(0.917406062564434,3.09191198306876,
2.94634487035921));
#248792=CARTESIAN_POINT('Ctrl Pts',(0.797524700869486,3.12498228565185,
2.95460152209426));
#248793=CARTESIAN_POINT('Ctrl Pts',(0.654917886440115,3.15557696975978,
2.96391921129273));
#248794=CARTESIAN_POINT('Ctrl Pts',(0.633768059640023,3.15989264918445,
2.96528821019354));
#248795=CARTESIAN_POINT('Ctrl Pts',(0.600813912900344,3.1662728456083,2.96739961088764));
#248796=CARTESIAN_POINT('Ctrl Pts',(0.589039171830073,3.1684844887648,2.96814974308773));
#248797=CARTESIAN_POINT('Ctrl Pts',(0.56721110938089,3.17245855518935,2.96953206798627));
#248798=CARTESIAN_POINT('Ctrl Pts',(0.557161684310083,3.1742388990652,2.97016519869005));
#248799=CARTESIAN_POINT('Ctrl Pts',(0.533917474638405,3.17824302480967,
2.97162221876054));
#248800=CARTESIAN_POINT('Ctrl Pts',(0.520717121387442,3.18043240590058,
2.97244419523691));
#248801=CARTESIAN_POINT('Ctrl Pts',(0.478551650934126,3.18715631706283,
2.97505348921033));
#248802=CARTESIAN_POINT('Ctrl Pts',(0.449537258497794,3.19137798771895,
2.97682444093907));
#248803=CARTESIAN_POINT('Ctrl Pts',(0.290824799000282,3.21226352504861,
2.9863978198183));
#248804=CARTESIAN_POINT('Ctrl Pts',(0.160249238486313,3.22141944336741,
2.99386228963523));
#248805=CARTESIAN_POINT('Ctrl Pts',(-0.201932682346517,3.22473114139172,
3.0142765075678));
#248806=CARTESIAN_POINT('Ctrl Pts',(-0.432874271934596,3.20191883937146,
3.02701362313365));
#248807=CARTESIAN_POINT('Ctrl Pts',(-0.732692588004195,3.13924968093901,
3.04481592581066));
#248808=CARTESIAN_POINT('Ctrl Pts',(-0.805443235294792,3.12137580793723,
3.04923216854582));
#248809=CARTESIAN_POINT('Ctrl Pts',(-0.904602174981984,3.09331629866866,
3.05541884910837));
#248810=CARTESIAN_POINT('Ctrl Pts',(-0.931600459116803,3.08529274582015,
3.05712058502792));
#248811=CARTESIAN_POINT('Ctrl Pts',(-0.974836141146514,3.07182440961313,
3.05987517390189));
#248812=CARTESIAN_POINT('Ctrl Pts',(-0.991141707227044,3.06660215942896,
3.06092079666553));
#248813=CARTESIAN_POINT('Ctrl Pts',(-1.02493659301173,3.05548084573216,
3.06310243972369));
#248814=CARTESIAN_POINT('Ctrl Pts',(-1.04241835771957,3.04956097880955,
3.06423910615555));
#248815=CARTESIAN_POINT('Ctrl Pts',(-1.08361806953387,3.03521382682813,
3.06693761132399));
#248816=CARTESIAN_POINT('Ctrl Pts',(-1.10728976813531,3.0266582904924,3.06850361164821));
#248817=CARTESIAN_POINT('Ctrl Pts',(-1.18696588005761,2.99680157364479,
3.07382857306545));
#248818=CARTESIAN_POINT('Ctrl Pts',(-1.24247298768127,2.97421717228008,
3.07762944811582));
#248819=CARTESIAN_POINT('Ctrl Pts',(-1.37633851405468,2.91534939283921,
3.08702561863897));
#248820=CARTESIAN_POINT('Ctrl Pts',(-1.45392749616563,2.87744029339153,
3.09267015117679));
#248821=CARTESIAN_POINT('Ctrl Pts',(-1.65292457708602,2.77010778244356,
3.10765223492287));
#248822=CARTESIAN_POINT('Ctrl Pts',(-1.77149902601348,2.69581971125369,
3.11710175042262));
#248823=CARTESIAN_POINT('Ctrl Pts',(-1.92620082787275,2.58427250263613,
3.12998689256025));
#248824=CARTESIAN_POINT('Ctrl Pts',(-1.96682015103134,2.55349419912518,
3.1334256893051));
#248825=CARTESIAN_POINT('Ctrl Pts',(-2.09988849963314,2.44760515118789,
3.14484649812147));
#248826=CARTESIAN_POINT('Ctrl Pts',(-2.18891122441195,2.36832770096022,
3.15274871311623));
#248827=CARTESIAN_POINT('Ctrl Pts',(-2.28855250021586,2.26916398108028,
3.16172802000536));
#248828=CARTESIAN_POINT('Ctrl Pts',(-2.30360624163768,2.25388022296778,
3.16308840732691));
#248829=CARTESIAN_POINT('Ctrl Pts',(-2.32680722797041,2.22984943442775,
3.16518939216665));
#248830=CARTESIAN_POINT('Ctrl Pts',(-2.33506001915892,2.22120577478212,
3.16593760428103));
#248831=CARTESIAN_POINT('Ctrl Pts',(-2.35020755822701,2.20516309330068,
3.16731218757228));
#248832=CARTESIAN_POINT('Ctrl Pts',(-2.35711560724773,2.19777748020672,
3.16793952892136));
#248833=CARTESIAN_POINT('Ctrl Pts',(-2.3730737587362,2.18055432505028,3.16938997954952));
#248834=CARTESIAN_POINT('Ctrl Pts',(-2.38209754649554,2.17069286689037,
3.17021113640701));
#248835=CARTESIAN_POINT('Ctrl Pts',(-2.40952288441563,2.14034467465717,
3.17271087619193));
#248836=CARTESIAN_POINT('Ctrl Pts',(-2.42772394154997,2.11967743611935,
3.17437551696114));
#248837=CARTESIAN_POINT('Ctrl Pts',(-2.46429409611218,2.07706307621035,
3.17773798555687));
#248838=CARTESIAN_POINT('Ctrl Pts',(-2.48264022498827,2.055099519232,3.17943441010173));
#248839=CARTESIAN_POINT('Ctrl Pts',(-2.55368115274164,1.96771105110766,
3.18605476403195));
#248840=CARTESIAN_POINT('Ctrl Pts',(-2.60410494920358,1.90047714699355,
3.19086854400065));
#248841=CARTESIAN_POINT('Ctrl Pts',(-2.75168855990418,1.68677141260038,
3.20558003108914));
#248842=CARTESIAN_POINT('Ctrl Pts',(-2.83954078084347,1.53427429700553,
3.2152819860626));
#248843=CARTESIAN_POINT('Ctrl Pts',(-2.97363591010511,1.25011626080743,
3.23309495820934));
#248844=CARTESIAN_POINT('Ctrl Pts',(-3.02460349094454,1.12119072346685,
3.24108577169568));
#248845=CARTESIAN_POINT('Ctrl Pts',(-3.07757795773426,0.956970377384393,
3.25138829511855));
#248846=CARTESIAN_POINT('Ctrl Pts',(-3.08752267553488,0.924381947709918,
3.25343814919994));
#248847=CARTESIAN_POINT('Ctrl Pts',(-3.10255856068715,0.872157716926107,
3.25673451070762));
#248848=CARTESIAN_POINT('Ctrl Pts',(-3.10798441527301,0.852620402694395,
3.25797020377834));
#248849=CARTESIAN_POINT('Ctrl Pts',(-3.11792604297628,0.815466401802598,
3.26032543997177));
#248850=CARTESIAN_POINT('Ctrl Pts',(-3.12247778331461,0.797860096333169,
3.26144377656268));
#248851=CARTESIAN_POINT('Ctrl Pts',(-3.13251598505542,0.757629910652897,
3.26400470276786));
#248852=CARTESIAN_POINT('Ctrl Pts',(-3.13790675601796,0.734983417154233,
3.26545028405356));
#248853=CARTESIAN_POINT('Ctrl Pts',(-3.14864067099042,0.687618332342686,
3.26848261829641));
#248854=CARTESIAN_POINT('Ctrl Pts',(-3.15393913338513,0.662891341770996,
3.27007067762439));
#248855=CARTESIAN_POINT('Ctrl Pts',(-3.17155560542189,0.575680814400231,
3.27569021929638));
#248856=CARTESIAN_POINT('Ctrl Pts',(-3.18231140337217,0.512900186247806,
3.27976932644396));
#248857=CARTESIAN_POINT('Ctrl Pts',(-3.21221017864354,0.300798516452359,
3.29366493800713));
#248858=CARTESIAN_POINT('Ctrl Pts',(-3.22275000000513,0.150482448427344,
3.30371299133942));
#248859=CARTESIAN_POINT('Ctrl Pts',(-3.22275,-1.09908401824121E-10,3.31386231834285));
#248860=CARTESIAN_POINT('Origin',(0.,0.,-2.31077344927308));
#248861=CARTESIAN_POINT('',(-3.22275,1.54108685473619E-11,4.8132072728278));
#248862=CARTESIAN_POINT('',(-3.22275,-5.68635386092821E-12,4.56684192677376));
#248863=CARTESIAN_POINT('',(-3.22275,-3.50678552687464E-13,-2.31077344927308));
#248864=CARTESIAN_POINT('Ctrl Pts',(-3.22275,1.54108685473619E-11,4.8132072728278));
#248865=CARTESIAN_POINT('Ctrl Pts',(-3.22275,0.000690567994428604,4.81316239703151));
#248866=CARTESIAN_POINT('Ctrl Pts',(-3.22274977823664,0.00138113766044703,
4.81311751533792));
#248867=CARTESIAN_POINT('Ctrl Pts',(-3.2226605004907,0.140262159044363,
4.80409011264835));
#248868=CARTESIAN_POINT('Ctrl Pts',(-3.21368351261808,0.27829100368279,
4.79487241388675));
#248869=CARTESIAN_POINT('Ctrl Pts',(-3.1674056525901,0.634410425249026,
4.7706669772349));
#248870=CARTESIAN_POINT('Ctrl Pts',(-3.11647497344357,0.85001845992052,
4.75556697697216));
#248871=CARTESIAN_POINT('Ctrl Pts',(-3.03586907207272,1.08176304537931,
4.73980542849057));
#248872=CARTESIAN_POINT('Ctrl Pts',(-3.02759590809255,1.10470602731961,
4.73825086306142));
#248873=CARTESIAN_POINT('Ctrl Pts',(-3.01471685791979,1.13919011761568,
4.73592546964963));
#248874=CARTESIAN_POINT('Ctrl Pts',(-3.01030356728095,1.15080159106129,
4.73514439261771));
#248875=CARTESIAN_POINT('Ctrl Pts',(-3.00217046066613,1.171833029223,4.73373354037896));
#248876=CARTESIAN_POINT('Ctrl Pts',(-2.99847316706655,1.1812615291399,4.73310247713628));
#248877=CARTESIAN_POINT('Ctrl Pts',(-2.99072294959577,1.20075455960624,
4.73180095649328));
#248878=CARTESIAN_POINT('Ctrl Pts',(-2.98666356283178,1.21081627183805,
4.73113088529037));
#248879=CARTESIAN_POINT('Ctrl Pts',(-2.97584802131803,1.23723862725734,
4.72937534939798));
#248880=CARTESIAN_POINT('Ctrl Pts',(-2.96900765545248,1.25356469354103,
4.7282947702736));
#248881=CARTESIAN_POINT('Ctrl Pts',(-2.9365510525626,1.32927343023507,4.7232994683895));
#248882=CARTESIAN_POINT('Ctrl Pts',(-2.90928385373234,1.38793682143816,
4.71947381850408));
#248883=CARTESIAN_POINT('Ctrl Pts',(-2.82129697694418,1.56322772417038,
4.70806455249339));
#248884=CARTESIAN_POINT('Ctrl Pts',(-2.75518928374001,1.67700154164072,
4.70068638843717));
#248885=CARTESIAN_POINT('Ctrl Pts',(-2.55411474746019,1.97891437521934,
4.68037250045424));
#248886=CARTESIAN_POINT('Ctrl Pts',(-2.40558491573292,2.15702398560324,
4.6674819508797));
#248887=CARTESIAN_POINT('Ctrl Pts',(-2.20783201637952,2.34808596728322,
4.65119385748321));
#248888=CARTESIAN_POINT('Ctrl Pts',(-2.17576837761097,2.37782707893554,
4.64857865538862));
#248889=CARTESIAN_POINT('Ctrl Pts',(-2.12647410084897,2.42171874186909,
4.64459000623963));
#248890=CARTESIAN_POINT('Ctrl Pts',(-2.1096847765466,2.43635873214634,4.64323690542819));
#248891=CARTESIAN_POINT('Ctrl Pts',(-2.07925984564375,2.46233842424964,
4.64079372705171));
#248892=CARTESIAN_POINT('Ctrl Pts',(-2.06567974502613,2.4737419413753,4.63970631849662));
#248893=CARTESIAN_POINT('Ctrl Pts',(-2.03649545634545,2.49784075902408,
4.63737560663253));
#248894=CARTESIAN_POINT('Ctrl Pts',(-2.02086518862018,2.51050314906165,
4.63613104467078));
#248895=CARTESIAN_POINT('Ctrl Pts',(-1.97800071552304,2.54456882255352,
4.63272736493463));
#248896=CARTESIAN_POINT('Ctrl Pts',(-1.95053896367669,2.5656802071458,4.63055689590759));
#248897=CARTESIAN_POINT('Ctrl Pts',(-1.77581248757799,2.69557557184392,
4.6168055557308));
#248898=CARTESIAN_POINT('Ctrl Pts',(-1.61986456113914,2.79207046534781,
4.60475980484986));
#248899=CARTESIAN_POINT('Ctrl Pts',(-1.29710609886835,2.95560475306769,
4.58045774751439));
#248900=CARTESIAN_POINT('Ctrl Pts',(-1.13117222935722,3.0230007942635,4.56825844311235));
#248901=CARTESIAN_POINT('Ctrl Pts',(-0.885661793636314,3.09965616099004,
4.55119386632549));
#248902=CARTESIAN_POINT('Ctrl Pts',(-0.809984226825709,3.12028728543631,
4.54606546551623));
#248903=CARTESIAN_POINT('Ctrl Pts',(-0.714625775851233,3.14257986400173,
4.53982601086925));
#248904=CARTESIAN_POINT('Ctrl Pts',(-0.695587550801185,3.14684861467757,
4.53859127708239));
#248905=CARTESIAN_POINT('Ctrl Pts',(-0.665515142244039,3.15330519374782,
4.53665942173493));
#248906=CARTESIAN_POINT('Ctrl Pts',(-0.654506605945997,3.1556085247063,
4.53595612503024));
#248907=CARTESIAN_POINT('Ctrl Pts',(-0.633613069160272,3.15986606745569,
4.53462897602693));
#248908=CARTESIAN_POINT('Ctrl Pts',(-0.623730975216488,3.16183155123511,
4.53400454704237));
#248909=CARTESIAN_POINT('Ctrl Pts',(-0.60023447167596,3.16639040629807,
4.53252737451355));
#248910=CARTESIAN_POINT('Ctrl Pts',(-0.586612313987692,3.16894235277619,
4.53167694341117));
#248911=CARTESIAN_POINT('Ctrl Pts',(-0.540409303260744,3.17728979012759,
4.52881137511865));
#248912=CARTESIAN_POINT('Ctrl Pts',(-0.507754658317553,3.18267152300163,
4.52681783360016));
#248913=CARTESIAN_POINT('Ctrl Pts',(-0.427306241158793,3.19466027120379,
4.52197159205195));
#248914=CARTESIAN_POINT('Ctrl Pts',(-0.37943495423911,3.20069905499044,
4.51914390818901));
#248915=CARTESIAN_POINT('Ctrl Pts',(-0.172964482540289,3.22204672008978,
4.50712077764098));
#248916=CARTESIAN_POINT('Ctrl Pts',(-0.0134779655086782,3.22665874384267,
4.49826165749148));
#248917=CARTESIAN_POINT('Ctrl Pts',(0.338597384937704,3.21072476377755,
4.47852350317213));
#248918=CARTESIAN_POINT('Ctrl Pts',(0.530294766143791,3.18467867287266,
4.46763950924912));
#248919=CARTESIAN_POINT('Ctrl Pts',(0.762859269670118,3.13149071901396,
4.45351997451963));
#248920=CARTESIAN_POINT('Ctrl Pts',(0.806998630757631,3.1204072319042,4.45079995783708));
#248921=CARTESIAN_POINT('Ctrl Pts',(0.872424323048787,3.1024977000688,4.44670104947028));
#248922=CARTESIAN_POINT('Ctrl Pts',(0.893899394664907,3.09637853178865,
4.44534474940476));
#248923=CARTESIAN_POINT('Ctrl Pts',(0.93231617608023,3.0849989858915,4.44289809215583));
#248924=CARTESIAN_POINT('Ctrl Pts',(0.949281459488707,3.07982091785816,
4.44181043628652));
#248925=CARTESIAN_POINT('Ctrl Pts',(0.985359680890468,3.06848286436239,
4.43948169617216));
#248926=CARTESIAN_POINT('Ctrl Pts',(1.00445945053403,3.06228378385553,4.43823937612253));
#248927=CARTESIAN_POINT('Ctrl Pts',(1.05618859071846,3.04495839913953,4.4348482877582));
#248928=CARTESIAN_POINT('Ctrl Pts',(1.08869864047589,3.03348662677468,4.4326883096396));
#248929=CARTESIAN_POINT('Ctrl Pts',(1.28769317474859,2.95965685832944,4.41928434688513));
#248930=CARTESIAN_POINT('Ctrl Pts',(1.44894035199903,2.88414229997025,4.40760373495105));
#248931=CARTESIAN_POINT('Ctrl Pts',(1.74966899155727,2.71169953788741,4.38434374968966));
#248932=CARTESIAN_POINT('Ctrl Pts',(1.88938172783716,2.61627448081681,4.37282773664565));
#248933=CARTESIAN_POINT('Ctrl Pts',(2.09287919526187,2.45244706062507,4.35540623341453));
#248934=CARTESIAN_POINT('Ctrl Pts',(2.16227479770724,2.39148714067206,4.34933659006795));
#248935=CARTESIAN_POINT('Ctrl Pts',(2.24349880105755,2.3137060667886,4.34216383688442));
#248936=CARTESIAN_POINT('Ctrl Pts',(2.25790476232465,2.2996497049434,4.3408889361582));
#248937=CARTESIAN_POINT('Ctrl Pts',(2.28033268491936,2.27735210701625,4.33890113643941));
#248938=CARTESIAN_POINT('Ctrl Pts',(2.28844356620972,2.26920158360797,4.33818164207182));
#248939=CARTESIAN_POINT('Ctrl Pts',(2.3028299637214,2.25458928595253,4.33690464165469));
#248940=CARTESIAN_POINT('Ctrl Pts',(2.30912205422518,2.24814457525594,4.33634587086138));
#248941=CARTESIAN_POINT('Ctrl Pts',(2.32428686557893,2.23248109260962,4.33499840201047));
#248942=CARTESIAN_POINT('Ctrl Pts',(2.33313180715137,2.22323576024087,4.3342118245637));
#248943=CARTESIAN_POINT('Ctrl Pts',(2.36052369220078,2.19426039902338,4.33177286612426));
#248944=CARTESIAN_POINT('Ctrl Pts',(2.37887770684384,2.17434858389916,4.3301342834055));
#248945=CARTESIAN_POINT('Ctrl Pts',(2.49995216385011,2.03962942739909,4.31927664954797));
#248946=CARTESIAN_POINT('Ctrl Pts',(2.59458971937978,1.91780191177089,4.31054635744549));
#248947=CARTESIAN_POINT('Ctrl Pts',(2.82571527688974,1.5716729242753,4.28717711353406));
#248948=CARTESIAN_POINT('Ctrl Pts',(2.94412309129382,1.33676830086213,4.27269642663068));
#248949=CARTESIAN_POINT('Ctrl Pts',(3.04540417142833,1.05499961822504,4.25492419516252));
#248950=CARTESIAN_POINT('Ctrl Pts',(3.05741830944528,1.01965870419453,4.25269042137498));
#248951=CARTESIAN_POINT('Ctrl Pts',(3.07581025127226,0.962306364750547,
4.2490537951437));
#248952=CARTESIAN_POINT('Ctrl Pts',(3.08257204072811,0.940421083207358,
4.24766340421612));
#248953=CARTESIAN_POINT('Ctrl Pts',(3.09417244658499,0.901405146210326,
4.24517910884337));
#248954=CARTESIAN_POINT('Ctrl Pts',(3.09910355544604,0.884302832478413,
4.24408825045355));
#248955=CARTESIAN_POINT('Ctrl Pts',(3.10920452552743,0.848147685150697,
4.24177775919991));
#248956=CARTESIAN_POINT('Ctrl Pts',(3.11434147631253,0.82908649656522,4.24055711661903));
#248957=CARTESIAN_POINT('Ctrl Pts',(3.12757050911031,0.778140327182126,
4.23728731682261));
#248958=CARTESIAN_POINT('Ctrl Pts',(3.13534990122858,0.746177276044712,
4.23522827390119));
#248959=CARTESIAN_POINT('Ctrl Pts',(3.17405105953332,0.57586014262635,4.22421281309114));
#248960=CARTESIAN_POINT('Ctrl Pts',(3.19630386467259,0.43571479544884,4.21498619646364));
#248961=CARTESIAN_POINT('Ctrl Pts',(3.22804715399094,0.0898865294022592,
4.19189120079028));
#248962=CARTESIAN_POINT('Ctrl Pts',(3.22720906692133,-0.116116688744731,
4.17783530903838));
#248963=CARTESIAN_POINT('Ctrl Pts',(3.19736082628502,-0.414641859135027,
4.15781471954808));
#248964=CARTESIAN_POINT('Ctrl Pts',(3.18383042564079,-0.508203961729918,
4.15159800826799));
#248965=CARTESIAN_POINT('Ctrl Pts',(3.16243262716317,-0.620924234743594,
4.14427928744899));
#248966=CARTESIAN_POINT('Ctrl Pts',(3.15847148530748,-0.640769031093299,
4.14299735836021));
#248967=CARTESIAN_POINT('Ctrl Pts',(3.15196168916056,-0.671854039468318,
4.14100103493579));
#248968=CARTESIAN_POINT('Ctrl Pts',(3.1495392902683,-0.683119761778857,
4.14027995601536));
#248969=CARTESIAN_POINT('Ctrl Pts',(3.14511673039782,-0.703163825544851,
4.13900162105003));
#248970=CARTESIAN_POINT('Ctrl Pts',(3.1431401996556,-0.711946838740806,
4.13844308379712));
#248971=CARTESIAN_POINT('Ctrl Pts',(3.13827371066269,-0.733156491907248,
4.13709807216114));
#248972=CARTESIAN_POINT('Ctrl Pts',(3.13534673768895,-0.745574390530345,
4.1363136966152));
#248973=CARTESIAN_POINT('Ctrl Pts',(3.12602289816131,-0.784105343049968,
4.13388863232516));
#248974=CARTESIAN_POINT('Ctrl Pts',(3.11937279059531,-0.81015668126598,
4.13226151784306));
#248975=CARTESIAN_POINT('Ctrl Pts',(3.08367829222681,-0.943026484081717,
4.12401269905845));
#248976=CARTESIAN_POINT('Ctrl Pts',(3.04946766739934,-1.04839039574007,
4.11763635580063));
#248977=CARTESIAN_POINT('Ctrl Pts',(2.93841270899015,-1.3386022806623,4.10001800264333));
#248978=CARTESIAN_POINT('Ctrl Pts',(2.84969162408951,-1.51834950968589,
4.08901526744249));
#248979=CARTESIAN_POINT('Ctrl Pts',(2.68140884346065,-1.79188052064752,
4.07071042606615));
#248980=CARTESIAN_POINT('Ctrl Pts',(2.61217920809448,-1.89137633446193,
4.06368226062735));
#248981=CARTESIAN_POINT('Ctrl Pts',(2.51742844492292,-2.0123950267043,4.05449490904032));
#248982=CARTESIAN_POINT('Ctrl Pts',(2.49694965633281,-2.03774925259271,
4.05253241725571));
#248983=CARTESIAN_POINT('Ctrl Pts',(2.46349666298485,-2.0779049261223,4.0493606310607));
#248984=CARTESIAN_POINT('Ctrl Pts',(2.45076495477575,-2.09290606583203,
4.04816109696694));
#248985=CARTESIAN_POINT('Ctrl Pts',(2.42624588859265,-2.12126513932456,
4.04586479850591));
#248986=CARTESIAN_POINT('Ctrl Pts',(2.4144835374957,-2.13464379471166,4.04476908564888));
#248987=CARTESIAN_POINT('Ctrl Pts',(2.38726182284919,-2.16509328522513,
4.04224621205076));
#248988=CARTESIAN_POINT('Ctrl Pts',(2.37172931847406,-2.18209714280004,
4.04081602521338));
#248989=CARTESIAN_POINT('Ctrl Pts',(2.32240846611802,-2.2349412916537,4.0363027764898));
#248990=CARTESIAN_POINT('Ctrl Pts',(2.28798119520261,-2.27017296370971,
4.0331927235781));
#248991=CARTESIAN_POINT('Ctrl Pts',(2.20515780447031,-2.35113335472419,
4.025799766236));
#248992=CARTESIAN_POINT('Ctrl Pts',(2.1561265653091,-2.39617742591035,4.02149054162935));
#248993=CARTESIAN_POINT('Ctrl Pts',(1.95762645206896,-2.56750778236424,
4.00430970400565));
#248994=CARTESIAN_POINT('Ctrl Pts',(1.79819173677338,-2.68158357456211,
3.99104299975597));
#248995=CARTESIAN_POINT('Ctrl Pts',(1.50011919802168,-2.85625973403065,
3.9677294947056));
#248996=CARTESIAN_POINT('Ctrl Pts',(1.36567745801429,-2.92292864280902,
3.95769365067794));
#248997=CARTESIAN_POINT('Ctrl Pts',(1.20709336681111,-2.98822856146334,
3.94673594966196));
#248998=CARTESIAN_POINT('Ctrl Pts',(1.18703302523894,-2.99625382548308,
3.94536550986887));
#248999=CARTESIAN_POINT('Ctrl Pts',(1.15586600776289,-3.00836022987959,
3.94326212538279));
#249000=CARTESIAN_POINT('Ctrl Pts',(1.14481542801763,-3.01258280329858,
3.9425213309765));
#249001=CARTESIAN_POINT('Ctrl Pts',(1.12441553618103,-3.02024941439748,
3.94116327831991));
#249002=CARTESIAN_POINT('Ctrl Pts',(1.11507342917202,-3.0237109773978,3.94054504139871));
#249003=CARTESIAN_POINT('Ctrl Pts',(1.09361132009983,-3.03155041006686,
3.93913303462625));
#249004=CARTESIAN_POINT('Ctrl Pts',(1.0814809733793,-3.03589896496896,3.93834097599436));
#249005=CARTESIAN_POINT('Ctrl Pts',(1.04332208484769,-3.04932064072571,
3.9358672142036));
#249006=CARTESIAN_POINT('Ctrl Pts',(1.01720229144661,-3.05813291974347,
3.93419987860793));
#249007=CARTESIAN_POINT('Ctrl Pts',(0.879937177610846,-3.10249000179777,
3.92555722796821));
#249008=CARTESIAN_POINT('Ctrl Pts',(0.767024392593477,-3.13231744855377,
3.91885398987802));
#249009=CARTESIAN_POINT('Ctrl Pts',(0.450893821526948,-3.19770132804359,
3.90058755528953));
#249010=CARTESIAN_POINT('Ctrl Pts',(0.245519604976746,-3.21998761580007,
3.8892506482196));
#249011=CARTESIAN_POINT('Ctrl Pts',(-0.0702298625905273,-3.22385028649462,
3.87117857572261));
#249012=CARTESIAN_POINT('Ctrl Pts',(-0.179869213562804,-3.21959414531582,
3.86479186766123));
#249013=CARTESIAN_POINT('Ctrl Pts',(-0.32068080529009,-3.20691263436101,
3.85633439956107));
#249014=CARTESIAN_POINT('Ctrl Pts',(-0.35224558676475,-3.20359918879381,
3.85442219145808));
#249015=CARTESIAN_POINT('Ctrl Pts',(-0.403108358139404,-3.19749920023712,
3.85131219601143));
#249016=CARTESIAN_POINT('Ctrl Pts',(-0.422439455182285,-3.19500271748781,
3.85012348529319));
#249017=CARTESIAN_POINT('Ctrl Pts',(-0.459440728398727,-3.18988257843508,
3.84783480497384));
#249018=CARTESIAN_POINT('Ctrl Pts',(-0.477114111880822,-3.18728705188233,
3.8467357574827));
#249019=CARTESIAN_POINT('Ctrl Pts',(-0.517891603781801,-3.18095168336399,
3.84418595620492));
#249020=CARTESIAN_POINT('Ctrl Pts',(-0.540978149547474,-3.17710684756747,
3.84273195176244));
#249021=CARTESIAN_POINT('Ctrl Pts',(-0.614565084351167,-3.16402636186574,
3.83806313169127));
#249022=CARTESIAN_POINT('Ctrl Pts',(-0.664885498255447,-3.15383573671152,
3.83481860418387));
#249023=CARTESIAN_POINT('Ctrl Pts',(-0.909829856169486,-3.09810840731017,
3.81876253460645));
#249024=CARTESIAN_POINT('Ctrl Pts',(-1.10014525829515,-3.03574118243091,
3.8054303967669));
#249025=CARTESIAN_POINT('Ctrl Pts',(-1.46544386169624,-2.8771451393537,
3.77853679144732));
#249026=CARTESIAN_POINT('Ctrl Pts',(-1.63978132717997,-2.7814778529991,
3.76504129729913));
#249027=CARTESIAN_POINT('Ctrl Pts',(-1.82796989647494,-2.65432949786062,
3.75042940106515));
#249028=CARTESIAN_POINT('Ctrl Pts',(-1.85150443732313,-2.6379671101803,
3.74860179108884));
#249029=CARTESIAN_POINT('Ctrl Pts',(-1.88535122127449,-2.61375898366427,
3.74597657856255));
#249030=CARTESIAN_POINT('Ctrl Pts',(-1.89583868920558,-2.60616210741316,
3.74516360999163));
#249031=CARTESIAN_POINT('Ctrl Pts',(-1.91403499494291,-2.592813163306,3.74375427508686));
#249032=CARTESIAN_POINT('Ctrl Pts',(-1.92176426896241,-2.58708951625951,
3.7431560295348));
#249033=CARTESIAN_POINT('Ctrl Pts',(-1.92964008205009,-2.58120258064856,
3.74254689519827));
#249034=CARTESIAN_POINT('Ctrl Pts',(-1.92981204715722,-2.58107401506582,
3.74253359520822));
#249035=CARTESIAN_POINT('Ctrl Pts',(-1.93014307082761,-2.5808264815925,
3.74250799382814));
#249036=CARTESIAN_POINT('Ctrl Pts',(-1.93030213125146,-2.58070751617441,
3.74249569226481));
#249037=CARTESIAN_POINT('Ctrl Pts',(-1.93060867059499,-2.58047820325032,
3.74247198517327));
#249038=CARTESIAN_POINT('Ctrl Pts',(-1.93075615105184,-2.58036785780673,
3.74246057950191));
#249039=CARTESIAN_POINT('Ctrl Pts',(-1.93104067778801,-2.58015493576096,
3.74243857539119));
#249040=CARTESIAN_POINT('Ctrl Pts',(-1.93117772534017,-2.58005236089379,
3.74242797683323));
#249041=CARTESIAN_POINT('Ctrl Pts',(-1.9314423851412,-2.57985424022249,
3.7424075096412));
#249042=CARTESIAN_POINT('Ctrl Pts',(-1.93156999846312,-2.57975869587662,
3.74239764090726));
#249043=CARTESIAN_POINT('Ctrl Pts',(-1.93181666384316,-2.57957398845649,
3.74237856572067));
#249044=CARTESIAN_POINT('Ctrl Pts',(-1.93193571682413,-2.57948482660447,
3.74236935918244));
#249045=CARTESIAN_POINT('Ctrl Pts',(-1.93216602998031,-2.57931231424507,
3.74235154891883));
#249046=CARTESIAN_POINT('Ctrl Pts',(-1.93227729093776,-2.5792289647785,
3.74234294512095));
#249047=CARTESIAN_POINT('Ctrl Pts',(-1.93249269862829,-2.57906757359814,
3.7423262878275));
#249048=CARTESIAN_POINT('Ctrl Pts',(-1.93259684602564,-2.57898953277612,
3.74231823427034));
#249049=CARTESIAN_POINT('Ctrl Pts',(-1.93279862825931,-2.57883831210621,
3.74230263090213));
#249050=CARTESIAN_POINT('Ctrl Pts',(-1.93289626366706,-2.57876513302196,
3.74229508103816));
#249051=CARTESIAN_POINT('Ctrl Pts',(-1.93308555742652,-2.5786232379493,
3.74228044362118));
#249052=CARTESIAN_POINT('Ctrl Pts',(-1.93317721627542,-2.57855452261471,
3.74227335602225));
#249053=CARTESIAN_POINT('Ctrl Pts',(-1.9333550352852,-2.57842119942322,
3.74225960612276));
#249054=CARTESIAN_POINT('Ctrl Pts',(-1.93344119586268,-2.57835659214137,
3.74225294378355));
#249055=CARTESIAN_POINT('Ctrl Pts',(-1.93360844709125,-2.57823116615093,
3.74224001123042));
#249056=CARTESIAN_POINT('Ctrl Pts',(-1.93368953808833,-2.57817034795266,
3.74223374098417));
#249057=CARTESIAN_POINT('Ctrl Pts',(-1.93384703561819,-2.57805221329086,
3.742221562795));
#249058=CARTESIAN_POINT('Ctrl Pts',(-1.93392344246848,-2.57799489725911,
3.7422156548227));
#249059=CARTESIAN_POINT('Ctrl Pts',(-1.93407191933086,-2.57788350812713,
3.74220417428767));
#249060=CARTESIAN_POINT('Ctrl Pts',(-1.93414398962734,-2.5778294353984,
3.74219860169874));
#249061=CARTESIAN_POINT('Ctrl Pts',(-1.93428410775566,-2.57772429872202,
3.74218776761005));
#249062=CARTESIAN_POINT('Ctrl Pts',(-1.93435215584104,-2.57767323509617,
3.742182506087));
#249063=CARTESIAN_POINT('Ctrl Pts',(-1.93448451466634,-2.57757390417457,
3.74217227207351));
#249064=CARTESIAN_POINT('Ctrl Pts',(-1.93454882560649,-2.57752563717805,
3.74216729956437));
#249065=CARTESIAN_POINT('Ctrl Pts',(-1.93467396924573,-2.57743170637144,
3.7421576235352));
#249066=CARTESIAN_POINT('Ctrl Pts',(-1.93473480215083,-2.57738604280232,
3.74215291999642));
#249067=CARTESIAN_POINT('Ctrl Pts',(-1.93489158965743,-2.57726834325985,
3.74214079740648));
#249068=CARTESIAN_POINT('Ctrl Pts',(-1.93498754185828,-2.5771963040773,
3.74213337857657));
#249069=CARTESIAN_POINT('Ctrl Pts',(-1.93517842235295,-2.57705297777379,
3.7421186202012));
#249070=CARTESIAN_POINT('Ctrl Pts',(-1.93527335074042,-2.57698169075902,
3.74211128064726));
#249071=CARTESIAN_POINT('Ctrl Pts',(-1.93546222742072,-2.57683983641469,
3.7420966774322));
#249072=CARTESIAN_POINT('Ctrl Pts',(-1.9355561757973,-2.57676926918942,
3.74208941376342));
#249073=CARTESIAN_POINT('Ctrl Pts',(-1.93574313466924,-2.57662882321356,
3.74207495905099));
#249074=CARTESIAN_POINT('Ctrl Pts',(-1.93583614521817,-2.5765589445811,
3.74206776800208));
#249075=CARTESIAN_POINT('Ctrl Pts',(-1.93602126902772,-2.57641984576439,
3.74205345538718));
#249076=CARTESIAN_POINT('Ctrl Pts',(-1.9361133823625,-2.57635062567445,
3.74204633381442));
#249077=CARTESIAN_POINT('Ctrl Pts',(-1.9362967508696,-2.57621281498715,
3.74203215712333));
#249078=CARTESIAN_POINT('Ctrl Pts',(-1.93638800612883,-2.57614422446659,
3.7420251019973));
#249079=CARTESIAN_POINT('Ctrl Pts',(-1.93656969629851,-2.57600764491864,
3.74201105527285));
#249080=CARTESIAN_POINT('Ctrl Pts',(-1.93666013126483,-2.57593965598387,
3.74200406366918));
#249081=CARTESIAN_POINT('Ctrl Pts',(-1.93684021731373,-2.57580425259338,
3.74199014116712));
#249082=CARTESIAN_POINT('Ctrl Pts',(-1.93692986845239,-2.57573683822301,
3.74198321026352));
#249083=CARTESIAN_POINT('Ctrl Pts',(-1.9371084221011,-2.57560255782986,
3.74196940643301));
#249084=CARTESIAN_POINT('Ctrl Pts',(-1.93719732465869,-2.57553569189207,
3.74196253350159));
#249085=CARTESIAN_POINT('Ctrl Pts',(-1.93737441518375,-2.5754024831218,
3.74194884298113));
#249086=CARTESIAN_POINT('Ctrl Pts',(-1.93746260322022,-2.5753361403517,
3.74194202538596));
#249087=CARTESIAN_POINT('Ctrl Pts',(-1.93763829770002,-2.57520395343339,
3.74192844298436));
#249088=CARTESIAN_POINT('Ctrl Pts',(-1.93772580419423,-2.57513810935504,
3.74192167817326));
#249089=CARTESIAN_POINT('Ctrl Pts',(-1.93790016753006,-2.57500689610809,
3.74190819886802));
#249090=CARTESIAN_POINT('Ctrl Pts',(-1.93798702441897,-2.57494152700619,
3.74190148436952));
#249091=CARTESIAN_POINT('Ctrl Pts',(-1.93816011949252,-2.57481124072426,
3.74188810329459));
#249092=CARTESIAN_POINT('Ctrl Pts',(-1.9382463577253,-2.5747463236047,3.74188143671377));
#249093=CARTESIAN_POINT('Ctrl Pts',(-1.93841824553793,-2.57461691895322,
3.74186814914879));
#249094=CARTESIAN_POINT('Ctrl Pts',(-1.93850389515173,-2.57455243148708,
3.74186152816138));
#249095=CARTESIAN_POINT('Ctrl Pts',(-1.93867463484646,-2.5744238644888,
3.74184832952996));
#249096=CARTESIAN_POINT('Ctrl Pts',(-1.93875972497793,-2.57435978500482,
3.74184175188147));
#249097=CARTESIAN_POINT('Ctrl Pts',(-1.93892937407035,-2.57423201286794,
3.74182863773333));
#249098=CARTESIAN_POINT('Ctrl Pts',(-1.93901393305621,-2.57416832027761,
3.74182210123122));
#249099=CARTESIAN_POINT('Ctrl Pts',(-1.93918254737945,-2.57404130143913,
3.74180906724641));
#249100=CARTESIAN_POINT('Ctrl Pts',(-1.93926660275728,-2.57397797523712,
3.74180256976008));
#249101=CARTESIAN_POINT('Ctrl Pts',(-1.93943423665176,-2.57385166922161,
3.74178961173432));
#249102=CARTESIAN_POINT('Ctrl Pts',(-1.93951781521416,-2.57378868944572,
3.74178315119087));
#249103=CARTESIAN_POINT('Ctrl Pts',(-1.93968452161611,-2.57366305680027,
3.74177026502867));
#249104=CARTESIAN_POINT('Ctrl Pts',(-1.93976764947724,-2.57360040398217,
3.7417638394078));
#249105=CARTESIAN_POINT('Ctrl Pts',(-1.93993347992707,-2.57347540627158,
3.74175102112182));
#249106=CARTESIAN_POINT('Ctrl Pts',(-1.94001618253987,-2.57341306142447,
3.74174462845443));
#249107=CARTESIAN_POINT('Ctrl Pts',(-1.95027320703567,-2.56568009224111,
3.74095179588585));
#249108=CARTESIAN_POINT('Ctrl Pts',(-1.96040214740219,-2.55794905164122,
3.740169485119));
#249109=CARTESIAN_POINT('Ctrl Pts',(-1.98232492229874,-2.54100951188826,
3.73847698664242));
#249110=CARTESIAN_POINT('Ctrl Pts',(-1.99410107452955,-2.53177849749452,
3.7375682885136));
#249111=CARTESIAN_POINT('Ctrl Pts',(-2.02614295980632,-2.5062994495726,
3.73509573287671));
#249112=CARTESIAN_POINT('Ctrl Pts',(-2.04627763834667,-2.48988757536617,
3.73354193731715));
#249113=CARTESIAN_POINT('Ctrl Pts',(-2.11083510416449,-2.43595436224979,
3.7285516884782));
#249114=CARTESIAN_POINT('Ctrl Pts',(-2.15444326778432,-2.39747229949171,
3.72516769384942));
#249115=CARTESIAN_POINT('Ctrl Pts',(-2.3736802563351,-2.19319070549532,
3.70794450351096));
#249116=CARTESIAN_POINT('Ctrl Pts',(-2.53131077380543,-2.00920901385574,
3.69478215764833));
#249117=CARTESIAN_POINT('Ctrl Pts',(-2.73260364437299,-1.71250854976627,
3.67431769978638));
#249118=CARTESIAN_POINT('Ctrl Pts',(-2.79296659593321,-1.6121853664318,
3.66751967072787));
#249119=CARTESIAN_POINT('Ctrl Pts',(-2.86287577304075,-1.48023826858379,
3.65859186079497));
#249120=CARTESIAN_POINT('Ctrl Pts',(-2.87758227114909,-1.45144176009658,
3.65664451816991));
#249121=CARTESIAN_POINT('Ctrl Pts',(-2.90051238110816,-1.40482398859129,
3.65349135175389));
#249122=CARTESIAN_POINT('Ctrl Pts',(-2.9090110357424,-1.38713996389784,
3.6522950801908));
#249123=CARTESIAN_POINT('Ctrl Pts',(-2.92492272876894,-1.3532414496271,
3.65000114570518));
#249124=CARTESIAN_POINT('Ctrl Pts',(-2.93236374783051,-1.33704084475036,
3.64890449575432));
#249125=CARTESIAN_POINT('Ctrl Pts',(-2.94915274531775,-1.29967343674534,
3.64637384111156));
#249126=CARTESIAN_POINT('Ctrl Pts',(-2.95840785386545,-1.27846622291077,
3.6449367453212));
#249127=CARTESIAN_POINT('Ctrl Pts',(-2.98688090940351,-1.21125775843862,
3.64037874505704));
#249128=CARTESIAN_POINT('Ctrl Pts',(-3.00525952572255,-1.16491101204488,
3.63723008067478));
#249129=CARTESIAN_POINT('Ctrl Pts',(-3.04602452355081,-1.0547169422649,
3.62972746585643));
#249130=CARTESIAN_POINT('Ctrl Pts',(-3.0674893965274,-0.990555910421785,
3.62534611747546));
#249131=CARTESIAN_POINT('Ctrl Pts',(-3.17700624829429,-0.625379425581347,
3.60034898457542));
#249132=CARTESIAN_POINT('Ctrl Pts',(-3.22274999999998,-0.313514198417957,
3.57855815143349));
#249133=CARTESIAN_POINT('Ctrl Pts',(-3.22275000000001,5.45539308172138E-12,
3.55815895351304));
#249134=CARTESIAN_POINT('',(-3.22274864161822,-0.00290502672063927,3.31405834319998));
#249135=CARTESIAN_POINT('Ctrl Pts',(-3.22275,-1.09907859225987E-10,3.31386231834285));
#249136=CARTESIAN_POINT('Ctrl Pts',(-3.22274999999997,-0.000968490989623499,
3.31392763845649));
#249137=CARTESIAN_POINT('Ctrl Pts',(-3.2227495634281,-0.00193698879745099,
3.31399296222398));
#249138=CARTESIAN_POINT('Ctrl Pts',(-3.22274869026566,-0.00290549324082802,
3.31405828957594));
#249139=CARTESIAN_POINT('Ctrl Pts',(-3.22274869068103,-0.00290503247812938,
3.31405825849667));
#249140=CARTESIAN_POINT('Ctrl Pts',(-3.22258761851836,-0.181593258945338,
3.32611109786505));
#249141=CARTESIAN_POINT('Ctrl Pts',(-3.2075656848062,-0.359970542783448,
3.3382714130059));
#249142=CARTESIAN_POINT('Ctrl Pts',(-3.17038612993277,-0.58032053983041,
3.35289451087542));
#249143=CARTESIAN_POINT('Ctrl Pts',(-3.16202199513422,-0.624289576077566,
3.35579099359991));
#249144=CARTESIAN_POINT('Ctrl Pts',(-3.14968992747057,-0.682486647066304,
3.35958398381453));
#249145=CARTESIAN_POINT('Ctrl Pts',(-3.14653663874808,-0.696880091531935,
3.3605187318783));
#249146=CARTESIAN_POINT('Ctrl Pts',(-3.14035122602267,-0.724215721059071,
3.36228696280049));
#249147=CARTESIAN_POINT('Ctrl Pts',(-3.1373375379251,-0.737161733242957,
3.36312138138069));
#249148=CARTESIAN_POINT('Ctrl Pts',(-3.13187021135824,-0.760006934933148,
3.36458807094616));
#249149=CARTESIAN_POINT('Ctrl Pts',(-3.12944957440491,-0.769913587886718,
3.36522214200679));
#249150=CARTESIAN_POINT('Ctrl Pts',(-3.12406810772593,-0.791492908465782,
3.36659899933795));
#249151=CARTESIAN_POINT('Ctrl Pts',(-3.12108885234614,-0.803160601878099,
3.36734074139752));
#249152=CARTESIAN_POINT('Ctrl Pts',(-3.11251711429248,-0.835962123428764,
3.36941907630098));
#249153=CARTESIAN_POINT('Ctrl Pts',(-3.10677478208397,-0.857056573775631,
3.37074751336503));
#249154=CARTESIAN_POINT('Ctrl Pts',(-3.06307135267211,-1.01138715118845,
3.38041777166932));
#249155=CARTESIAN_POINT('Ctrl Pts',(-3.0167642134933,-1.14212638645514,
3.38834497992889));
#249156=CARTESIAN_POINT('Ctrl Pts',(-2.90670168098247,-1.3989417334166,
3.40410568710466));
#249157=CARTESIAN_POINT('Ctrl Pts',(-2.84279789623171,-1.52461578898582,
3.41192093412923));
#249158=CARTESIAN_POINT('Ctrl Pts',(-2.70687462735731,-1.7534698508819,
3.42694560328845));
#249159=CARTESIAN_POINT('Ctrl Pts',(-2.63664456965658,-1.857398204448,3.43411334015358));
#249160=CARTESIAN_POINT('Ctrl Pts',(-2.5283266573769,-1.99912408497023,
3.44461522283098));
#249161=CARTESIAN_POINT('Ctrl Pts',(-2.49507281278966,-2.040476409855,3.44777417822137));
#249162=CARTESIAN_POINT('Ctrl Pts',(-2.44658730863064,-2.09781161618541,
3.45230172126968));
#249163=CARTESIAN_POINT('Ctrl Pts',(-2.4321880251138,-2.11448916043558,
3.45363701974798));
#249164=CARTESIAN_POINT('Ctrl Pts',(-2.41718554830607,-2.13150932850677,
3.45501923999838));
#249165=CARTESIAN_POINT('Ctrl Pts',(-2.41675181778127,-2.1320010890478,
3.45505919313904));
#249166=CARTESIAN_POINT('Ctrl Pts',(-2.4040970867804,-2.14634010801313,
3.456224661956));
#249167=CARTESIAN_POINT('Ctrl Pts',(-2.39175763122639,-2.1600819598472,
3.45735502630952));
#249168=CARTESIAN_POINT('Ctrl Pts',(-2.36776411413128,-2.18634471794267,
3.45954180278764));
#249169=CARTESIAN_POINT('Ctrl Pts',(-2.35612711985948,-2.19888042036685,
3.46059747584587));
#249170=CARTESIAN_POINT('Ctrl Pts',(-2.32512917242755,-2.23174369750116,
3.46339698933537));
#249171=CARTESIAN_POINT('Ctrl Pts',(-2.30560179198641,-2.25191160955721,
3.46514790553473));
#249172=CARTESIAN_POINT('Ctrl Pts',(-2.2334675682802,-2.32449012109322,
3.47157197551704));
#249173=CARTESIAN_POINT('Ctrl Pts',(-2.17932023313647,-2.37533020833573,
3.4763118632669));
#249174=CARTESIAN_POINT('Ctrl Pts',(-1.94818039897605,-2.57779193513913,
3.49622360391479));
#249175=CARTESIAN_POINT('Ctrl Pts',(-1.75677362054549,-2.7118513369829,
3.51203717013012));
#249176=CARTESIAN_POINT('Ctrl Pts',(-1.43860511811695,-2.886773796846,3.53651160904171));
#249177=CARTESIAN_POINT('Ctrl Pts',(-1.32088234220945,-2.94250296581392,
3.5452098624625));
#249178=CARTESIAN_POINT('Ctrl Pts',(-1.17295553786098,-3.00185750510564,
3.55546970617373));
#249179=CARTESIAN_POINT('Ctrl Pts',(-1.14566030407205,-3.01238041755164,
3.55733566420366));
#249180=CARTESIAN_POINT('Ctrl Pts',(-1.10568687833804,-3.02716910613166,
3.56002510312143));
#249181=CARTESIAN_POINT('Ctrl Pts',(-1.09312024735683,-3.03172960692806,
3.5608644291981));
#249182=CARTESIAN_POINT('Ctrl Pts',(-1.07099773541198,-3.03960255384739,
3.56233073521922));
#249183=CARTESIAN_POINT('Ctrl Pts',(-1.06145416635896,-3.04294838882461,
3.56295961296539));
#249184=CARTESIAN_POINT('Ctrl Pts',(-1.04059950484556,-3.05014967247437,
3.56432574466373));
#249185=CARTESIAN_POINT('Ctrl Pts',(-1.02928259329696,-3.05398718197573,
3.56506196608427));
#249186=CARTESIAN_POINT('Ctrl Pts',(-0.997595416466308,-3.06453600388561,
3.56710978015883));
#249187=CARTESIAN_POINT('Ctrl Pts',(-0.977178710676943,-3.07110718748708,
3.56841359075955));
#249188=CARTESIAN_POINT('Ctrl Pts',(-0.843127756837876,-3.11277973351913,
3.57688130232848));
#249189=CARTESIAN_POINT('Ctrl Pts',(-0.727678176750141,-3.14177539103797,
3.58374102801339));
#249190=CARTESIAN_POINT('Ctrl Pts',(-0.561906469245577,-3.1737779272468,
3.59331592299491));
#249191=CARTESIAN_POINT('Ctrl Pts',(-0.51272061806219,-3.18209411387246,
3.5961229863274));
#249192=CARTESIAN_POINT('Ctrl Pts',(-0.331094538621187,-3.20848213571036,
3.60642202858491));
#249193=CARTESIAN_POINT('Ctrl Pts',(-0.197761702633655,-3.21945193153625,
3.61385897174902));
#249194=CARTESIAN_POINT('Ctrl Pts',(0.0265329823053955,-3.22391651701158,
3.62658982575467));
#249195=CARTESIAN_POINT('Ctrl Pts',(0.117232522317018,-3.22189332209526,
3.63179677806883));
#249196=CARTESIAN_POINT('Ctrl Pts',(0.26966701059199,-3.21204770744448,
3.64074346597529));
#249197=CARTESIAN_POINT('Ctrl Pts',(0.331480357297423,-3.20625806875407,
3.64442557175297));
#249198=CARTESIAN_POINT('Ctrl Pts',(0.418405866603907,-3.19557583429122,
3.6496984134265));
#249199=CARTESIAN_POINT('Ctrl Pts',(0.443688137908328,-3.19216371156812,
3.65124336028755));
#249200=CARTESIAN_POINT('Ctrl Pts',(0.487244896755648,-3.18575780427341,
3.65392579050463));
#249201=CARTESIAN_POINT('Ctrl Pts',(0.505539232893881,-3.18290597388686,
3.65505878922268));
#249202=CARTESIAN_POINT('Ctrl Pts',(0.540623668982058,-3.17712669895831,
3.65724424392317));
#249203=CARTESIAN_POINT('Ctrl Pts',(0.557417152099547,-3.17422338747694,
3.65829590568656));
#249204=CARTESIAN_POINT('Ctrl Pts',(0.601474142285977,-3.16624626992806,
3.66106992510736));
#249205=CARTESIAN_POINT('Ctrl Pts',(0.62869610337194,-3.16095360908572,
3.66279911696278));
#249206=CARTESIAN_POINT('Ctrl Pts',(0.726292195445964,-3.14066781475323,
3.66905491504746));
#249207=CARTESIAN_POINT('Ctrl Pts',(0.796223698503015,-3.12367110928172,
3.67364378890512));
#249208=CARTESIAN_POINT('Ctrl Pts',(1.09114595593895,-3.04144383336252,
3.69346037110032));
#249209=CARTESIAN_POINT('Ctrl Pts',(1.30921389121566,-2.95413459175153,
3.70934763233808));
#249210=CARTESIAN_POINT('Ctrl Pts',(1.63211463333146,-2.7820269301989,3.73401782621837));
#249211=CARTESIAN_POINT('Ctrl Pts',(1.74447092614427,-2.71298720568552,
3.74282896584637));
#249212=CARTESIAN_POINT('Ctrl Pts',(1.87636648764199,-2.62034954248813,
3.75320541788491));
#249213=CARTESIAN_POINT('Ctrl Pts',(1.90020749734336,-2.60311246926652,
3.75508219188885));
#249214=CARTESIAN_POINT('Ctrl Pts',(1.93455934672457,-2.57755256265045,
3.75778418749249));
#249215=CARTESIAN_POINT('Ctrl Pts',(1.94525885506979,-2.56948731865943,
3.75862545568758));
#249216=CARTESIAN_POINT('Ctrl Pts',(1.96402063289817,-2.55516040777961,
3.76009961546359));
#249217=CARTESIAN_POINT('Ctrl Pts',(1.97210386002413,-2.54892685873635,
3.76073437511173));
#249218=CARTESIAN_POINT('Ctrl Pts',(1.98959992895737,-2.53530134574946,
3.76210744378303));
#249219=CARTESIAN_POINT('Ctrl Pts',(1.99900132194905,-2.52789527403994,
3.76284475938736));
#249220=CARTESIAN_POINT('Ctrl Pts',(2.02519857895498,-2.50702049601065,
3.76489861194788));
#249221=CARTESIAN_POINT('Ctrl Pts',(2.04190139578684,-2.49343534058479,
3.766207293532));
#249222=CARTESIAN_POINT('Ctrl Pts',(2.1523989195752,-2.40170768686351,3.77486896071459));
#249223=CARTESIAN_POINT('Ctrl Pts',(2.24183467364514,-2.31844876802866,
3.78190118549108));
#249224=CARTESIAN_POINT('Ctrl Pts',(2.51784361053033,-2.03055559610329,
3.80449762916262));
#249225=CARTESIAN_POINT('Ctrl Pts',(2.68281541239459,-1.80698468355226,
3.81959781185925));
#249226=CARTESIAN_POINT('Ctrl Pts',(2.84545308860876,-1.51423200287893,
3.83925770746937));
#249227=CARTESIAN_POINT('Ctrl Pts',(2.87232123957701,-1.46262500951657,
3.84271427900689));
#249228=CARTESIAN_POINT('Ctrl Pts',(2.90866799389909,-1.38794360297326,
3.84771846754082));
#249229=CARTESIAN_POINT('Ctrl Pts',(2.91929924156062,-1.3654408918766,3.8492265349319));
#249230=CARTESIAN_POINT('Ctrl Pts',(2.93733953851354,-1.32608179785532,
3.85186573935885));
#249231=CARTESIAN_POINT('Ctrl Pts',(2.94486682151639,-1.30928067300504,
3.85299278802608));
#249232=CARTESIAN_POINT('Ctrl Pts',(2.95914430496461,-1.27666680322901,
3.8551818693089));
#249233=CARTESIAN_POINT('Ctrl Pts',(2.96591274351086,-1.26086269031789,
3.85624323749));
#249234=CARTESIAN_POINT('Ctrl Pts',(2.98358387527426,-1.21867138891481,
3.85907861770062));
#249235=CARTESIAN_POINT('Ctrl Pts',(2.99426272608619,-1.1921926600421,3.86086004957385));
#249236=CARTESIAN_POINT('Ctrl Pts',(3.03265669395756,-1.0932218176259,3.86752771323817));
#249237=CARTESIAN_POINT('Ctrl Pts',(3.0581004840827,-1.01988252977222,3.87248744408377));
#249238=CARTESIAN_POINT('Ctrl Pts',(3.14803808095682,-0.726887060380422,
3.89238217693537));
#249239=CARTESIAN_POINT('Ctrl Pts',(3.19169549707302,-0.501561128582362,
3.90791777694789));
#249240=CARTESIAN_POINT('Ctrl Pts',(3.22214313978351,-0.144146217813104,
3.93209659249631));
#249241=CARTESIAN_POINT('Ctrl Pts',(3.22533558531727,-0.0141813625976974,
3.94077795065607));
#249242=CARTESIAN_POINT('Ctrl Pts',(3.2196262867641,0.144838821149949,3.95102032454814));
#249243=CARTESIAN_POINT('Ctrl Pts',(3.21818037448073,0.174031391206086,
3.95288465255639));
#249244=CARTESIAN_POINT('Ctrl Pts',(3.21549487345626,0.216538371257538,
3.95557219708008));
#249245=CARTESIAN_POINT('Ctrl Pts',(3.21456930682533,0.229870254080964,
3.95641122858429));
#249246=CARTESIAN_POINT('Ctrl Pts',(3.21279077863745,0.253371472397949,
3.95788294239884));
#249247=CARTESIAN_POINT('Ctrl Pts',(3.21197241286599,0.263543011996047,
3.95851747058732));
#249248=CARTESIAN_POINT('Ctrl Pts',(3.21008725766431,0.28565916454671,3.95989174627766));
#249249=CARTESIAN_POINT('Ctrl Pts',(3.20900210540162,0.297601845251194,
3.96063048398925));
#249250=CARTESIAN_POINT('Ctrl Pts',(3.20577227384963,0.331073672103552,
3.96269219115687));
#249251=CARTESIAN_POINT('Ctrl Pts',(3.20347737998515,0.352588118114054,
3.96400720942522));
#249252=CARTESIAN_POINT('Ctrl Pts',(3.18631328445752,0.499460203484161,
3.97292473857919));
#249253=CARTESIAN_POINT('Ctrl Pts',(3.16430474959837,0.623887282667455,
3.98018395824887));
#249254=CARTESIAN_POINT('Ctrl Pts',(3.12572180288597,0.785876225434057,
3.98960699699214));
#249255=CARTESIAN_POINT('Ctrl Pts',(3.11566099216859,0.824860531917362,
3.99187238185345));
#249256=CARTESIAN_POINT('Ctrl Pts',(3.07050841732539,0.987187325712524,
4.00132965224258));
#249257=CARTESIAN_POINT('Ctrl Pts',(3.02880182205437,1.10856652322391,4.00846565804865));
#249258=CARTESIAN_POINT('Ctrl Pts',(2.94374932019487,1.31510796677328,4.02111742234584));
#249259=CARTESIAN_POINT('Ctrl Pts',(2.9036471798791,1.40142792335283,4.02656855459159));
#249260=CARTESIAN_POINT('Ctrl Pts',(2.83017864655181,1.54283207426288,4.03589029913804));
#249261=CARTESIAN_POINT('Ctrl Pts',(2.79887414384019,1.59891985170751,4.0396963632809));
#249262=CARTESIAN_POINT('Ctrl Pts',(2.75265381972605,1.67621069236225,4.04511630841779));
#249263=CARTESIAN_POINT('Ctrl Pts',(2.73912514644251,1.69822810884001,4.04668077209535));
#249264=CARTESIAN_POINT('Ctrl Pts',(2.71542011612938,1.73578689268357,4.04938626454634));
#249265=CARTESIAN_POINT('Ctrl Pts',(2.70537134539315,1.75140754963326,4.05052259614647));
#249266=CARTESIAN_POINT('Ctrl Pts',(2.68463832335715,1.78303250057773,4.05284637424434));
#249267=CARTESIAN_POINT('Ctrl Pts',(2.67394464892622,1.79902968692595,4.05403413957572));
#249268=CARTESIAN_POINT('Ctrl Pts',(2.64664722279766,1.83908413165214,4.05703979586312));
#249269=CARTESIAN_POINT('Ctrl Pts',(2.62985850252061,1.86301264955017,4.05886458225399));
#249270=CARTESIAN_POINT('Ctrl Pts',(2.5643690305434,1.95370360165604,4.06589542607785));
#249271=CARTESIAN_POINT('Ctrl Pts',(2.51343599267419,2.01880753224785,4.0711857437557));
#249272=CARTESIAN_POINT('Ctrl Pts',(2.31518342580373,2.25307361224488,4.09115599368582));
#249273=CARTESIAN_POINT('Ctrl Pts',(2.1528438931671,2.40866265623148,4.10638606810754));
#249274=CARTESIAN_POINT('Ctrl Pts',(1.87438348094797,2.62473801120903,4.13013800245248));
#249275=CARTESIAN_POINT('Ctrl Pts',(1.76845590861693,2.69724541236611,4.13870571364588));
#249276=CARTESIAN_POINT('Ctrl Pts',(1.63356640435371,2.77820493240319,4.14883048942756));
#249277=CARTESIAN_POINT('Ctrl Pts',(1.60845064939524,2.79282088350849,4.15068379712695));
#249278=CARTESIAN_POINT('Ctrl Pts',(1.57152663327977,2.81364520896418,4.1533585364995));
#249279=CARTESIAN_POINT('Ctrl Pts',(1.55987282512971,2.82012271098336,4.15419557934603));
#249280=CARTESIAN_POINT('Ctrl Pts',(1.53923161332175,2.83142855717502,4.15566512384545));
#249281=CARTESIAN_POINT('Ctrl Pts',(1.53026105521298,2.83628678847731,4.15629945163804));
#249282=CARTESIAN_POINT('Ctrl Pts',(1.5106768143253,2.84677316222275,4.1576748248232));
#249283=CARTESIAN_POINT('Ctrl Pts',(1.500054615212,2.8523846228353,4.15841484569766));
#249284=CARTESIAN_POINT('Ctrl Pts',(1.47012954832996,2.86797993950919,4.16048364994763));
#249285=CARTESIAN_POINT('Ctrl Pts',(1.45075632379681,2.87782834251036,4.16180439509308));
#249286=CARTESIAN_POINT('Ctrl Pts',(1.31448240496268,2.94537745419819,4.17097561327199));
#249287=CARTESIAN_POINT('Ctrl Pts',(1.19426117756273,2.99614088933111,4.17845965620575));
#249288=CARTESIAN_POINT('Ctrl Pts',(1.03795467223725,3.05123194903325,4.18782729734363));
#249289=CARTESIAN_POINT('Ctrl Pts',(1.0044352525925,3.06242978480467,4.18981547561764));
#249290=CARTESIAN_POINT('Ctrl Pts',(0.79672592656325,3.12804204972523,4.20204298889468));
#249291=CARTESIAN_POINT('Ctrl Pts',(0.618367565812259,3.16812842197894,
4.21216609266073));
#249292=CARTESIAN_POINT('Ctrl Pts',(0.373633902622566,3.20166846709655,
4.22638682641243));
#249293=CARTESIAN_POINT('Ctrl Pts',(0.30944357503122,3.20850856646885,4.23014430814276));
#249294=CARTESIAN_POINT('Ctrl Pts',(0.196924432245244,3.21709062899586,
4.23681041436933));
#249295=CARTESIAN_POINT('Ctrl Pts',(0.148680569706699,3.21968089616628,
4.23969393387703));
#249296=CARTESIAN_POINT('Ctrl Pts',(0.0772502364507711,3.22190724980168,
4.24400911363017));
#249297=CARTESIAN_POINT('Ctrl Pts',(0.0540953414206763,3.22237917952252,
4.24541501224381));
#249298=CARTESIAN_POINT('Ctrl Pts',(0.0127666227477288,3.22277594610537,
4.24793788484352));
#249299=CARTESIAN_POINT('Ctrl Pts',(-0.00540542899463652,3.22279669629168,
4.24905183987339));
#249300=CARTESIAN_POINT('Ctrl Pts',(-0.0439211589359999,3.22251492250118,
4.25142316143626));
#249301=CARTESIAN_POINT('Ctrl Pts',(-0.0642636733894452,3.2221734348334,
4.25268168829634));
#249302=CARTESIAN_POINT('Ctrl Pts',(-0.11897980296284,3.22073657265357,
4.25608377926682));
#249303=CARTESIAN_POINT('Ctrl Pts',(-0.153340612515038,3.21928358097877,
4.25823829551716));
#249304=CARTESIAN_POINT('Ctrl Pts',(-0.331267306303314,3.20890475411463,
4.26949217876983));
#249305=CARTESIAN_POINT('Ctrl Pts',(-0.474123230275399,3.19092546846574,
4.27886761240281));
#249306=CARTESIAN_POINT('Ctrl Pts',(-0.825550386026511,3.1225739203204,
4.30270267862349));
#249307=CARTESIAN_POINT('Ctrl Pts',(-1.03120205845841,3.06081981913464,
4.31737070010911));
#249308=CARTESIAN_POINT('Ctrl Pts',(-1.2806586297594,2.95789276537326,4.33529758416999));
#249309=CARTESIAN_POINT('Ctrl Pts',(-1.33155958004648,2.9353306257068,4.33896001561896));
#249310=CARTESIAN_POINT('Ctrl Pts',(-1.41518458863889,2.89564006871776,
4.34495681337516));
#249311=CARTESIAN_POINT('Ctrl Pts',(-1.44824367123161,2.87924805485308,
4.34732205716297));
#249312=CARTESIAN_POINT('Ctrl Pts',(-1.49402926897528,2.85555752970776,
4.3505828395644));
#249313=CARTESIAN_POINT('Ctrl Pts',(-1.50699724391859,2.84873508559692,
4.35150468966395));
#249314=CARTESIAN_POINT('Ctrl Pts',(-1.52907109990915,2.83692912604252,
4.3530703367325));
#249315=CARTESIAN_POINT('Ctrl Pts',(-1.53820017455359,2.83198967685502,
4.35371679795972));
#249316=CARTESIAN_POINT('Ctrl Pts',(-1.55722679397468,2.82157583506806,
4.35506175391373));
#249317=CARTESIAN_POINT('Ctrl Pts',(-1.56711957091571,2.81609334724797,
4.35575973878881));
#249318=CARTESIAN_POINT('Ctrl Pts',(-1.59363408340467,2.80121625321076,
4.35762747759854));
#249319=CARTESIAN_POINT('Ctrl Pts',(-1.6102018186385,2.79172567282342,4.3587913627164));
#249320=CARTESIAN_POINT('Ctrl Pts',(-1.6873870038303,2.74659555779403,4.36420332729992));
#249321=CARTESIAN_POINT('Ctrl Pts',(-1.74691621291337,2.70912298014112,
4.36834744718454));
#249322=CARTESIAN_POINT('Ctrl Pts',(-1.95743452296027,2.56677802068385,
4.38306993538948));
#249323=CARTESIAN_POINT('Ctrl Pts',(-2.10061645113594,2.4509832340051,4.39322917830641));
#249324=CARTESIAN_POINT('Ctrl Pts',(-2.35537711849186,2.20613992392381,
4.41306932536024));
#249325=CARTESIAN_POINT('Ctrl Pts',(-2.46813008134808,2.07922578135291,
4.42269629312879));
#249326=CARTESIAN_POINT('Ctrl Pts',(-2.59733263870874,1.90839673616246,
4.43538035161858));
#249327=CARTESIAN_POINT('Ctrl Pts',(-2.62354652751897,1.87219610807684,
4.43805283002688));
#249328=CARTESIAN_POINT('Ctrl Pts',(-2.6617951365915,1.81699451594448,4.44211180378256));
#249329=CARTESIAN_POINT('Ctrl Pts',(-2.67439824756349,1.79839272530539,
4.44347688312329));
#249330=CARTESIAN_POINT('Ctrl Pts',(-2.69671424327869,1.76470162291268,
4.44594522887242));
#249331=CARTESIAN_POINT('Ctrl Pts',(-2.7064976412232,1.74965997424406,4.44704581215187));
#249332=CARTESIAN_POINT('Ctrl Pts',(-2.72731435251805,1.71706257874903,
4.44942827260592));
#249333=CARTESIAN_POINT('Ctrl Pts',(-2.73830481955926,1.69948055596741,
4.45071165978634));
#249334=CARTESIAN_POINT('Ctrl Pts',(-2.76753242025832,1.65170400498327,
4.45419530692381));
#249335=CARTESIAN_POINT('Ctrl Pts',(-2.78544430834579,1.62131479521157,
4.45640716230311));
#249336=CARTESIAN_POINT('Ctrl Pts',(-2.89644519416116,1.42572090910679,
4.47062296771631));
#249337=CARTESIAN_POINT('Ctrl Pts',(-2.97528437985863,1.2528914377389,4.48312576397147));
#249338=CARTESIAN_POINT('Ctrl Pts',(-3.08472684356091,0.943312849939473,
4.50520661615248));
#249339=CARTESIAN_POINT('Ctrl Pts',(-3.12248378576721,0.809613366588782,
4.5146391280033));
#249340=CARTESIAN_POINT('Ctrl Pts',(-3.16670361284636,0.602817580847188,
4.52879943928522));
#249341=CARTESIAN_POINT('Ctrl Pts',(-3.17949457738736,0.531240317593413,
4.533622811106));
#249342=CARTESIAN_POINT('Ctrl Pts',(-3.19620428997651,0.415187721105826,
4.54126079824792));
#249343=CARTESIAN_POINT('Ctrl Pts',(-3.20163915569329,0.370958047490449,
4.5441293755178));
#249344=CARTESIAN_POINT('Ctrl Pts',(-3.20775123873508,0.31096221751003,
4.54795087873103));
#249345=CARTESIAN_POINT('Ctrl Pts',(-3.20923234664428,0.295285080916615,
4.54894303851876));
#249346=CARTESIAN_POINT('Ctrl Pts',(-3.21151684438641,0.269052339403136,
4.55059181280767));
#249347=CARTESIAN_POINT('Ctrl Pts',(-3.21238322835734,0.258502626483601,
4.5512517961673));
#249348=CARTESIAN_POINT('Ctrl Pts',(-3.21403958164885,0.237037730192024,
4.55258810099946));
#249349=CARTESIAN_POINT('Ctrl Pts',(-3.21482595969784,0.226122477987101,
4.55326422556669));
#249350=CARTESIAN_POINT('Ctrl Pts',(-3.216720162461,0.197819389555422,4.55500906190687));
#249351=CARTESIAN_POINT('Ctrl Pts',(-3.21774262859818,0.180425944328434,
4.55607318094827));
#249352=CARTESIAN_POINT('Ctrl Pts',(-3.22134701236618,0.109263957526231,
4.56039658077629));
#249353=CARTESIAN_POINT('Ctrl Pts',(-3.22272281160825,0.055440052023331,
4.56359609952793));
#249354=CARTESIAN_POINT('Ctrl Pts',(-3.22274986700139,0.00106910844232826,
4.56677934809673));
#249355=CARTESIAN_POINT('Ctrl Pts',(-3.22275,0.000534553557451239,4.56681063984618));
#249356=CARTESIAN_POINT('Ctrl Pts',(-3.22275,-5.68635386092821E-12,4.56684192677376));
#249357=CARTESIAN_POINT('Origin',(0.,0.,-2.31077344927308));
#249358=CARTESIAN_POINT('',(-3.22275,2.79355756999193E-11,6.06189028282397));
#249359=CARTESIAN_POINT('',(-3.22275,-2.46480457644168E-12,5.81181920673623));
#249360=CARTESIAN_POINT('',(-3.22275,-3.50678552687464E-13,-2.31077344927308));
#249361=CARTESIAN_POINT('Ctrl Pts',(-3.22275,2.79355756999193E-11,6.06189028282397));
#249362=CARTESIAN_POINT('Ctrl Pts',(-3.22275000000001,0.0971439062167578,
6.05639764174954));
#249363=CARTESIAN_POINT('Ctrl Pts',(-3.21835769004865,0.194235148630419,
6.05084379826759));
#249364=CARTESIAN_POINT('Ctrl Pts',(-3.20472638919507,0.344593473675672,
6.04202940771024));
#249365=CARTESIAN_POINT('Ctrl Pts',(-3.19852309806985,0.398077144571545,
6.03885214157138));
#249366=CARTESIAN_POINT('Ctrl Pts',(-3.1876269961524,0.475106281598435,
6.03420238934845));
#249367=CARTESIAN_POINT('Ctrl Pts',(-3.18400608468515,0.498795601701799,
6.0327623053316));
#249368=CARTESIAN_POINT('Ctrl Pts',(-3.17722759346265,0.540056507391252,
6.03023526324292));
#249369=CARTESIAN_POINT('Ctrl Pts',(-3.17418754280275,0.55764651468537,
6.02915197650542));
#249370=CARTESIAN_POINT('Ctrl Pts',(-3.16777503594112,0.592997197078166,
6.02696239177531));
#249371=CARTESIAN_POINT('Ctrl Pts',(-3.16439895900502,0.610756548486171,
6.02585601635352));
#249372=CARTESIAN_POINT('Ctrl Pts',(-3.15717657953903,0.647080379400539,
6.02357961015912));
#249373=CARTESIAN_POINT('Ctrl Pts',(-3.15331552150017,0.665641171598705,
6.02240915101558));
#249374=CARTESIAN_POINT('Ctrl Pts',(-3.14308221678452,0.712746158379625,
6.01941970057964));
#249375=CARTESIAN_POINT('Ctrl Pts',(-3.1364848619716,0.741239184400215,
6.01759362975829));
#249376=CARTESIAN_POINT('Ctrl Pts',(-3.10894354816324,0.853227667488226,
6.01034407868926));
#249377=CARTESIAN_POINT('Ctrl Pts',(-3.08504720881984,0.935953502695616,
6.00482796140598));
#249378=CARTESIAN_POINT('Ctrl Pts',(-3.01394369164409,1.14961455198215,
5.99015310451358));
#249379=CARTESIAN_POINT('Ctrl Pts',(-2.96152040992606,1.27861669171392,
5.98085402507507));
#249380=CARTESIAN_POINT('Ctrl Pts',(-2.81517426253864,1.58103505802602,
5.95818929454772));
#249381=CARTESIAN_POINT('Ctrl Pts',(-2.71335254836097,1.75002994144372,
5.94477250312231));
#249382=CARTESIAN_POINT('Ctrl Pts',(-2.57398103533259,1.93964318749871,
5.92950945192888));
#249383=CARTESIAN_POINT('Ctrl Pts',(-2.55067047406933,1.97019656274585,
5.92704399569452));
#249384=CARTESIAN_POINT('Ctrl Pts',(-2.51769906959785,2.0118461163637,5.92368286930112));
#249385=CARTESIAN_POINT('Ctrl Pts',(-2.50850138080828,2.02330280548462,
5.92275828544569));
#249386=CARTESIAN_POINT('Ctrl Pts',(-2.49277583554952,2.0426185531503,5.921199988243));
#249387=CARTESIAN_POINT('Ctrl Pts',(-2.48628842772258,2.05051012805239,
5.92056349321495));
#249388=CARTESIAN_POINT('Ctrl Pts',(-2.47279894742059,2.06676119274584,
5.9192532999467));
#249389=CARTESIAN_POINT('Ctrl Pts',(-2.4657918311181,2.07511616926612,5.91857996992352));
#249390=CARTESIAN_POINT('Ctrl Pts',(-2.44713893692753,2.09712916608329,
5.91680614744469));
#249391=CARTESIAN_POINT('Ctrl Pts',(-2.43542105252485,2.1107259524534,5.91571072632346));
#249392=CARTESIAN_POINT('Ctrl Pts',(-2.38357656002721,2.16987685124993,
5.91094257518709));
#249393=CARTESIAN_POINT('Ctrl Pts',(-2.34227848795306,2.21439275537493,
5.90734705232182));
#249394=CARTESIAN_POINT('Ctrl Pts',(-2.11983076971391,2.44098123475763,
5.88884163618523));
#249395=CARTESIAN_POINT('Ctrl Pts',(-1.91864515468566,2.60209437306891,
5.87489853219412));
#249396=CARTESIAN_POINT('Ctrl Pts',(-1.62697310071655,2.78326393949472,
5.85537604714825));
#249397=CARTESIAN_POINT('Ctrl Pts',(-1.5516915859894,2.82592486619816,5.85039897227247));
#249398=CARTESIAN_POINT('Ctrl Pts',(-1.42164298618653,2.89285696704888,
5.84182066465821));
#249399=CARTESIAN_POINT('Ctrl Pts',(-1.36774915383201,2.91872434411009,
5.83827143641693));
#249400=CARTESIAN_POINT('Ctrl Pts',(-1.2905040740226,2.95319027506277,5.8331762201799));
#249401=CARTESIAN_POINT('Ctrl Pts',(-1.26772293920817,2.96304101604838,
5.83167260134459));
#249402=CARTESIAN_POINT('Ctrl Pts',(-1.22815013764021,2.97961269954699,
5.82905800533204));
#249403=CARTESIAN_POINT('Ctrl Pts',(-1.21141127560663,2.98645731601754,
5.82795124311025));
#249404=CARTESIAN_POINT('Ctrl Pts',(-1.17702019134184,3.00018332130682,
5.82567525303668));
#249405=CARTESIAN_POINT('Ctrl Pts',(-1.15936314847231,3.0070506410691,5.82450560728564));
#249406=CARTESIAN_POINT('Ctrl Pts',(-1.114353071075,3.02410096497071,5.8215207410963));
#249407=CARTESIAN_POINT('Ctrl Pts',(-1.08692081823974,3.03406863121012,
5.81969848424239));
#249408=CARTESIAN_POINT('Ctrl Pts',(-0.978572046449844,3.07177981569216,
5.81248714930083));
#249409=CARTESIAN_POINT('Ctrl Pts',(-0.896705627207794,3.09666778101928,
5.80700669511644));
#249410=CARTESIAN_POINT('Ctrl Pts',(-0.576719859925738,3.1801926708841,
5.7854601668821));
#249411=CARTESIAN_POINT('Ctrl Pts',(-0.333213222596353,3.21483640274297,
5.76872145949128));
#249412=CARTESIAN_POINT('Ctrl Pts',(-0.00823055482417009,3.2237317534507,
5.74689592256636));
#249413=CARTESIAN_POINT('Ctrl Pts',(0.0717770033805431,3.22294333701456,
5.741572124074));
#249414=CARTESIAN_POINT('Ctrl Pts',(0.198983382920385,3.21694980825102,
5.73326108779646));
#249415=CARTESIAN_POINT('Ctrl Pts',(0.246238107501246,3.21367823278527,
5.73020770460111));
#249416=CARTESIAN_POINT('Ctrl Pts',(0.30923286513669,3.20791913449751,5.72619741036557));
#249417=CARTESIAN_POINT('Ctrl Pts',(0.325048959733889,3.20635514817282,
5.7251956307641));
#249418=CARTESIAN_POINT('Ctrl Pts',(0.351250121256505,3.20356835941545,
5.72354522066061));
#249419=CARTESIAN_POINT('Ctrl Pts',(0.361641787519611,3.20241192025137,
5.72289304113583));
#249420=CARTESIAN_POINT('Ctrl Pts',(0.381270438432944,3.20013077774537,
5.72166590571767));
#249421=CARTESIAN_POINT('Ctrl Pts',(0.390508479323459,3.1990166105531,5.72109035541206));
#249422=CARTESIAN_POINT('Ctrl Pts',(0.414909645911928,3.19596639683822,
5.71957506421613));
#249423=CARTESIAN_POINT('Ctrl Pts',(0.430064253467761,3.19396242669063,
5.71863903895045));
#249424=CARTESIAN_POINT('Ctrl Pts',(0.484273714673252,3.18640120542509,
5.71530709812945));
#249425=CARTESIAN_POINT('Ctrl Pts',(0.523241677843993,3.18023460297524,
5.71294231862377));
#249426=CARTESIAN_POINT('Ctrl Pts',(0.855790231150312,3.12133108050151,
5.69294712328959));
#249427=CARTESIAN_POINT('Ctrl Pts',(1.14087829997956,3.02878305876367,5.67692873706354));
#249428=CARTESIAN_POINT('Ctrl Pts',(1.47938557329845,2.86419752252249,5.65543508441461));
#249429=CARTESIAN_POINT('Ctrl Pts',(1.54831037321241,2.82753301316698,5.65092489527404));
#249430=CARTESIAN_POINT('Ctrl Pts',(1.66381646441471,2.76059918357091,5.6430748589695));
#249431=CARTESIAN_POINT('Ctrl Pts',(1.71107156347548,2.73156121021883,5.63977561027405));
#249432=CARTESIAN_POINT('Ctrl Pts',(1.77776566987291,2.68816821282045,5.63497863747436));
#249433=CARTESIAN_POINT('Ctrl Pts',(1.79783063193502,2.67479047554919,5.63351667040417));
#249434=CARTESIAN_POINT('Ctrl Pts',(1.83258020517745,2.65105454504744,5.63095074031175));
#249435=CARTESIAN_POINT('Ctrl Pts',(1.84733199064832,2.64079626346014,5.62985055630425));
#249436=CARTESIAN_POINT('Ctrl Pts',(1.87576327492936,2.62067055729023,5.62770852546819));
#249437=CARTESIAN_POINT('Ctrl Pts',(1.88945263307856,2.61081802576101,5.62666726973743));
#249438=CARTESIAN_POINT('Ctrl Pts',(1.92582300737283,2.58420560538922,5.62387389126816));
#249439=CARTESIAN_POINT('Ctrl Pts',(1.94836202727434,2.56725499254312,5.62211445798598));
#249440=CARTESIAN_POINT('Ctrl Pts',(2.0321883242572,2.50247315947323,5.61546154747821));
#249441=CARTESIAN_POINT('Ctrl Pts',(2.09195667854685,2.45272846463051,5.6104938275079));
#249442=CARTESIAN_POINT('Ctrl Pts',(2.32082772858264,2.2477857843588,5.5905523536666));
#249443=CARTESIAN_POINT('Ctrl Pts',(2.47493294911913,2.07688806171453,5.57497270600437));
#249444=CARTESIAN_POINT('Ctrl Pts',(2.66671539386692,1.81224509674283,5.55293830591617));
#249445=CARTESIAN_POINT('Ctrl Pts',(2.72026571003837,1.73082639200155,5.54641318598829));
#249446=CARTESIAN_POINT('Ctrl Pts',(2.78863272048446,1.61584878560609,5.53764812663343));
#249447=CARTESIAN_POINT('Ctrl Pts',(2.80668727878983,1.58428106368615,5.53528619597426));
#249448=CARTESIAN_POINT('Ctrl Pts',(2.83709319752367,1.52896555439585,5.53123248140996));
#249449=CARTESIAN_POINT('Ctrl Pts',(2.8496899513464,1.50535735498699,5.52952867347749));
#249450=CARTESIAN_POINT('Ctrl Pts',(2.86784563221889,1.47028607203132,5.52703909975039));
#249451=CARTESIAN_POINT('Ctrl Pts',(2.87363263419062,1.4589431792616,5.52624024303432));
#249452=CARTESIAN_POINT('Ctrl Pts',(2.88339486346415,1.43952513771686,5.52488382457752));
#249453=CARTESIAN_POINT('Ctrl Pts',(2.88740367902103,1.4314672759165,5.52432422460227));
#249454=CARTESIAN_POINT('Ctrl Pts',(2.89647549953428,1.41303942043793,5.5230519574839));
#249455=CARTESIAN_POINT('Ctrl Pts',(2.90151661164644,1.40265893395652,5.52234063437426));
#249456=CARTESIAN_POINT('Ctrl Pts',(2.91527543874067,1.37393563189173,5.52038648878447));
#249457=CARTESIAN_POINT('Ctrl Pts',(2.92387585708866,1.35553680299991,5.51915055622134));
#249458=CARTESIAN_POINT('Ctrl Pts',(2.97212181874132,1.24972853076145,5.51212615090402));
#249459=CARTESIAN_POINT('Ctrl Pts',(3.00802443578682,1.16065584407663,5.50653539555241));
#249460=CARTESIAN_POINT('Ctrl Pts',(3.09512928251753,0.91321290959359,5.49153124631669));
#249461=CARTESIAN_POINT('Ctrl Pts',(3.13813163177877,0.752274796544907,
5.48233145616816));
#249462=CARTESIAN_POINT('Ctrl Pts',(3.20075301547494,0.415249867864579,
5.46305839222876));
#249463=CARTESIAN_POINT('Ctrl Pts',(3.21868172541316,0.239435604094995,
5.45299272507181));
#249464=CARTESIAN_POINT('Ctrl Pts',(3.22280678134039,0.0286260828562297,
5.44040892091165));
#249465=CARTESIAN_POINT('Ctrl Pts',(3.22292866306092,-0.00580508913796709,
5.43833813674266));
#249466=CARTESIAN_POINT('Ctrl Pts',(3.22224832831783,-0.060300309013837,
5.435033209645));
#249467=CARTESIAN_POINT('Ctrl Pts',(3.22181029250909,-0.0803668309714191,
5.43381036808096));
#249468=CARTESIAN_POINT('Ctrl Pts',(3.22063206192379,-0.118158217237558,
5.43149574030741));
#249469=CARTESIAN_POINT('Ctrl Pts',(3.21993289525594,-0.135883673867505,
5.430405271413));
#249470=CARTESIAN_POINT('Ctrl Pts',(3.21802247348689,-0.175920961738625,
5.42793087797457));
#249471=CARTESIAN_POINT('Ctrl Pts',(3.21672544716932,-0.198227601916761,
5.42654433623924));
#249472=CARTESIAN_POINT('Ctrl Pts',(3.21218146026364,-0.2644796865809,5.42240179883741));
#249473=CARTESIAN_POINT('Ctrl Pts',(3.20826515402188,-0.308372557199517,
5.41962525535792));
#249474=CARTESIAN_POINT('Ctrl Pts',(3.17900973163127,-0.574489429845016,
5.40258919301438));
#249475=CARTESIAN_POINT('Ctrl Pts',(3.13149616089561,-0.793625607532219,
5.38763866823074));
#249476=CARTESIAN_POINT('Ctrl Pts',(3.0189929642407,-1.13600795425366,5.36328415443066));
#249477=CARTESIAN_POINT('Ctrl Pts',(2.96805344355116,-1.26312891608525,
5.35401976750253));
#249478=CARTESIAN_POINT('Ctrl Pts',(2.89006211484203,-1.42675654995869,
5.34206489196169));
#249479=CARTESIAN_POINT('Ctrl Pts',(2.87010830429375,-1.46648285979311,
5.33916064733501));
#249480=CARTESIAN_POINT('Ctrl Pts',(2.83478907769937,-1.53331603239556,
5.33428650827851));
#249481=CARTESIAN_POINT('Ctrl Pts',(2.81984116193708,-1.56063549761402,
5.33229755608761));
#249482=CARTESIAN_POINT('Ctrl Pts',(2.79783396918563,-1.59950794464164,
5.329477058876));
#249483=CARTESIAN_POINT('Ctrl Pts',(2.79109472819697,-1.61123890764236,
5.32862715521531));
#249484=CARTESIAN_POINT('Ctrl Pts',(2.77923093741058,-1.63159233616332,
5.32715523962301));
#249485=CARTESIAN_POINT('Ctrl Pts',(2.77413971131905,-1.64023383316495,
5.32653117048161));
#249486=CARTESIAN_POINT('Ctrl Pts',(2.76316664932994,-1.6586615035197,5.32520234431484));
#249487=CARTESIAN_POINT('Ctrl Pts',(2.75727308277397,-1.66844031104205,
5.32449834449039));
#249488=CARTESIAN_POINT('Ctrl Pts',(2.74103312238073,-1.69506513316945,
5.32258413749414));
#249489=CARTESIAN_POINT('Ctrl Pts',(2.73058330791917,-1.71184789812527,
5.32138036918034));
#249490=CARTESIAN_POINT('Ctrl Pts',(2.67380929480595,-1.80118612094496,
5.31498180608123));
#249491=CARTESIAN_POINT('Ctrl Pts',(2.62474260682964,-1.87196593272686,
5.30994540535129));
#249492=CARTESIAN_POINT('Ctrl Pts',(2.46850262364561,-2.07910197953422,
5.29503855472475));
#249493=CARTESIAN_POINT('Ctrl Pts',(2.3531074906982,-2.2088597368398,5.28545514332235));
#249494=CARTESIAN_POINT('Ctrl Pts',(2.11748060354611,-2.43427919741146,
5.26713218780895));
#249495=CARTESIAN_POINT('Ctrl Pts',(1.99977777712679,-2.53186128681745,
5.2584521400424));
#249496=CARTESIAN_POINT('Ctrl Pts',(1.83384457428873,-2.6506167674389,5.24642251134698));
#249497=CARTESIAN_POINT('Ctrl Pts',(1.7913740865185,-2.67950249484282,5.24336144593831));
#249498=CARTESIAN_POINT('Ctrl Pts',(1.72856868626863,-2.72005804967191,
5.23885029439212));
#249499=CARTESIAN_POINT('Ctrl Pts',(1.70876680282965,-2.73254121032327,
5.23743019046927));
#249500=CARTESIAN_POINT('Ctrl Pts',(1.67361683542561,-2.75416835965136,
5.23491237297281));
#249501=CARTESIAN_POINT('Ctrl Pts',(1.65832526729757,-2.76340260419168,
5.23381800771791));
#249502=CARTESIAN_POINT('Ctrl Pts',(1.62619096076716,-2.78244503567971,
5.23151991162237));
#249503=CARTESIAN_POINT('Ctrl Pts',(1.60933447755556,-2.79222848820446,
5.23031534640659));
#249504=CARTESIAN_POINT('Ctrl Pts',(1.56480497491848,-2.81753610676699,
5.22713517377398));
#249505=CARTESIAN_POINT('Ctrl Pts',(1.53699016362341,-2.83280522532898,
5.22515061533734));
#249506=CARTESIAN_POINT('Ctrl Pts',(1.41213305569642,-2.89896612021009,
5.21624786635569));
#249507=CARTESIAN_POINT('Ctrl Pts',(1.31276740728948,-2.94529483229652,
5.20917431766811));
#249508=CARTESIAN_POINT('Ctrl Pts',(1.02009870960136,-3.06399459087948,
5.1883861726227));
#249509=CARTESIAN_POINT('Ctrl Pts',(0.821961912734697,-3.12298411213479,
5.17433696990364));
#249510=CARTESIAN_POINT('Ctrl Pts',(0.505095442632602,-3.18505950591686,
5.15261992758744));
#249511=CARTESIAN_POINT('Ctrl Pts',(0.389474168807351,-3.20125606041612,
5.14485634674332));
#249512=CARTESIAN_POINT('Ctrl Pts',(0.245758873802969,-3.21348404348153,
5.13558633325421));
#249513=CARTESIAN_POINT('Ctrl Pts',(0.218268081635785,-3.21546828358876,
5.13383032118401));
#249514=CARTESIAN_POINT('Ctrl Pts',(0.17789165435825,-3.21786235695231,
5.13127971098141));
#249515=CARTESIAN_POINT('Ctrl Pts',(0.165024403638235,-3.21854789437368,
5.13047111714878));
#249516=CARTESIAN_POINT('Ctrl Pts',(0.142201486829234,-3.21962661750934,
5.1290448237995));
#249517=CARTESIAN_POINT('Ctrl Pts',(0.132247700875389,-3.22005083396614,
5.12842546784221));
#249518=CARTESIAN_POINT('Ctrl Pts',(0.110470102880129,-3.2208778104986,
5.12707633947649));
#249519=CARTESIAN_POINT('Ctrl Pts',(0.0986459234983415,-3.22126163262434,
5.1263476067731));
#249520=CARTESIAN_POINT('Ctrl Pts',(0.0652201645634567,-3.22216243703899,
5.12429755996702));
#249521=CARTESIAN_POINT('Ctrl Pts',(0.0436146792168579,-3.22252730898203,
5.12298427427346));
#249522=CARTESIAN_POINT('Ctrl Pts',(-0.128407510517826,-3.22370198768397,
5.11261041285779));
#249523=CARTESIAN_POINT('Ctrl Pts',(-0.278728315887484,-3.21419734408733,
5.10404273106163));
#249524=CARTESIAN_POINT('Ctrl Pts',(-0.538304385539554,-3.17942838175692,
5.08930817921019));
#249525=CARTESIAN_POINT('Ctrl Pts',(-0.647916398784636,-3.15891453081912,
5.08310554866025));
#249526=CARTESIAN_POINT('Ctrl Pts',(-0.911529947639595,-3.09527850836576,
5.06785394724913));
#249527=CARTESIAN_POINT('Ctrl Pts',(-1.06379585760533,-3.04630371197736,
5.05874952423793));
#249528=CARTESIAN_POINT('Ctrl Pts',(-1.25173551391868,-2.9700393512815,
5.04672525391651));
#249529=CARTESIAN_POINT('Ctrl Pts',(-1.29134591953172,-2.95303250908413,
5.04414562203884));
#249530=CARTESIAN_POINT('Ctrl Pts',(-1.35051464403786,-2.92621013528758,
5.04021744453096));
#249531=CARTESIAN_POINT('Ctrl Pts',(-1.37033453844909,-2.91698110658641,
5.03888874432115));
#249532=CARTESIAN_POINT('Ctrl Pts',(-1.40602851323281,-2.89991632853603,
5.03647174572506));
#249533=CARTESIAN_POINT('Ctrl Pts',(-1.42193496711033,-2.89215003452836,
5.03538586981074));
#249534=CARTESIAN_POINT('Ctrl Pts',(-1.45603824759524,-2.87514983107137,
5.03303840603439));
#249535=CARTESIAN_POINT('Ctrl Pts',(-1.47421289180194,-2.86587338324543,
5.03177537427398));
#249536=CARTESIAN_POINT('Ctrl Pts',(-1.5233633008965,-2.84019546471198,
5.0283263410484));
#249537=CARTESIAN_POINT('Ctrl Pts',(-1.55416085345914,-2.82346062684813,
5.02612875141087));
#249538=CARTESIAN_POINT('Ctrl Pts',(-1.75359579012857,-2.71083958814724,
5.01165289847587));
#249539=CARTESIAN_POINT('Ctrl Pts',(-1.91352809934512,-2.60041101784718,
4.99884925699455));
#249540=CARTESIAN_POINT('Ctrl Pts',(-2.17041628043224,-2.3864452124865,
4.97634924471806));
#249541=CARTESIAN_POINT('Ctrl Pts',(-2.27230413910459,-2.28964227671207,
4.96680451949895));
#249542=CARTESIAN_POINT('Ctrl Pts',(-2.41477596487089,-2.13537321047692,
4.95275942543722));
#249543=CARTESIAN_POINT('Ctrl Pts',(-2.46033075838091,-2.08272307233226,
4.94814748105809));
#249544=CARTESIAN_POINT('Ctrl Pts',(-2.5312517595283,-1.99517823331353,
4.94081555129679));
#249545=CARTESIAN_POINT('Ctrl Pts',(-2.55768462403771,-1.96117858101826,
4.9380456394262));
#249546=CARTESIAN_POINT('Ctrl Pts',(-2.59260140394756,-1.91435913495794,
4.93434612644114));
#249547=CARTESIAN_POINT('Ctrl Pts',(-2.60168555146636,-1.90199507107719,
4.93337974689889));
#249548=CARTESIAN_POINT('Ctrl Pts',(-2.61674467326198,-1.88118893866705,
4.9317718130144));
#249549=CARTESIAN_POINT('Ctrl Pts',(-2.62276785853029,-1.8727822292678,
4.93112706489592));
#249550=CARTESIAN_POINT('Ctrl Pts',(-2.6349409214599,-1.8556180662377,4.92982091626052));
#249551=CARTESIAN_POINT('Ctrl Pts',(-2.64108781855827,-1.84685874114237,
4.92915970903332));
#249552=CARTESIAN_POINT('Ctrl Pts',(-2.65690012660457,-1.82408581749953,
4.92745404017584));
#249553=CARTESIAN_POINT('Ctrl Pts',(-2.66649847475332,-1.81002576372841,
4.92641397058985));
#249554=CARTESIAN_POINT('Ctrl Pts',(-2.70515279896411,-1.75242847133306,
4.92220316468132));
#249555=CARTESIAN_POINT('Ctrl Pts',(-2.73325910103646,-1.70826010341974,
4.91908914207751));
#249556=CARTESIAN_POINT('Ctrl Pts',(-2.7970137943147,-1.60246583913932,
4.91184933080062));
#249557=CARTESIAN_POINT('Ctrl Pts',(-2.83172159206399,-1.54030413864414,
4.90776428554631));
#249558=CARTESIAN_POINT('Ctrl Pts',(-2.88898980517162,-1.42924705378697,
4.90067045549339));
#249559=CARTESIAN_POINT('Ctrl Pts',(-2.91243587073341,-1.38084277020505,
4.89764395388316));
#249560=CARTESIAN_POINT('Ctrl Pts',(-2.98947793491511,-1.21108772028001,
4.88718524297691));
#249561=CARTESIAN_POINT('Ctrl Pts',(-3.03678605519984,-1.08703335179264,
4.8798063148235));
#249562=CARTESIAN_POINT('Ctrl Pts',(-3.10372140507184,-0.872633161128614,
4.86706760128167));
#249563=CARTESIAN_POINT('Ctrl Pts',(-3.12735642633569,-0.783718857501115,
4.86178997584171));
#249564=CARTESIAN_POINT('Ctrl Pts',(-3.16060406632569,-0.632929793834891,
4.8527478125322));
#249565=CARTESIAN_POINT('Ctrl Pts',(-3.17227534908156,-0.571564993537487,
4.84904344805756));
#249566=CARTESIAN_POINT('Ctrl Pts',(-3.18614905038585,-0.484983211031298,
4.84376398047287));
#249567=CARTESIAN_POINT('Ctrl Pts',(-3.18984915378901,-0.46001826843165,
4.84223563735827));
#249568=CARTESIAN_POINT('Ctrl Pts',(-3.19570655636985,-0.417021427437538,
4.8395918562448));
#249569=CARTESIAN_POINT('Ctrl Pts',(-3.19800538377502,-0.399009786401751,
4.83848089609451));
#249570=CARTESIAN_POINT('Ctrl Pts',(-3.20237656818334,-0.362292753544884,
4.83620872598666));
#249571=CARTESIAN_POINT('Ctrl Pts',(-3.20443752531751,-0.343586737613318,
4.83504720546761));
#249572=CARTESIAN_POINT('Ctrl Pts',(-3.20921609760914,-0.296423313247933,
4.8321083042675));
#249573=CARTESIAN_POINT('Ctrl Pts',(-3.21171908225268,-0.26794625309277,
4.83032431487426));
#249574=CARTESIAN_POINT('Ctrl Pts',(-3.21977934084448,-0.159758967577081,
4.82350895342058));
#249575=CARTESIAN_POINT('Ctrl Pts',(-3.22274999999999,-0.0798906883009946,
4.81839888084207));
#249576=CARTESIAN_POINT('Ctrl Pts',(-3.22275,1.54108685473619E-11,4.8132072728278));
#249577=CARTESIAN_POINT('',(-3.22274964543185,0.00151174366742828,5.81173083705462));
#249578=CARTESIAN_POINT('Ctrl Pts',(-3.22275,-5.68635386092821E-12,4.56684192677376));
#249579=CARTESIAN_POINT('Ctrl Pts',(-3.22274999999983,-0.0986548522817535,
4.57261610439067));
#249580=CARTESIAN_POINT('Ctrl Pts',(-3.21821994880484,-0.197264624384204,
4.57822708228791));
#249581=CARTESIAN_POINT('Ctrl Pts',(-3.1874477793893,-0.531435454229501,
4.59713258198355));
#249582=CARTESIAN_POINT('Ctrl Pts',(-3.13977764501502,-0.764224446223105,
4.6101742616043));
#249583=CARTESIAN_POINT('Ctrl Pts',(-3.04579227124887,-1.05548448265948,
4.62801654316085));
#249584=CARTESIAN_POINT('Ctrl Pts',(-3.0224487473042,-1.12058048520465,
4.63210282731022));
#249585=CARTESIAN_POINT('Ctrl Pts',(-2.98699269771024,-1.210263470703,4.63789754195369));
#249586=CARTESIAN_POINT('Ctrl Pts',(-2.9766322919091,-1.23552546483991,
4.63954841037038));
#249587=CARTESIAN_POINT('Ctrl Pts',(-2.95931572495307,-1.27626637121178,
4.64224252286054));
#249588=CARTESIAN_POINT('Ctrl Pts',(-2.95255596121336,-1.29182765454154,
4.64327914526764));
#249589=CARTESIAN_POINT('Ctrl Pts',(-2.93813676120055,-1.32431685700455,
4.6454597334517));
#249590=CARTESIAN_POINT('Ctrl Pts',(-2.93045319390485,-1.34123332078802,
4.64660448749106));
#249591=CARTESIAN_POINT('Ctrl Pts',(-2.91172027884689,-1.38154698397642,
4.6493554975104));
#249592=CARTESIAN_POINT('Ctrl Pts',(-2.90053472055626,-1.4048791136317,
4.65096636457358));
#249593=CARTESIAN_POINT('Ctrl Pts',(-2.86051444481726,-1.48584228917728,
4.6566230257277));
#249594=CARTESIAN_POINT('Ctrl Pts',(-2.83023471730324,-1.54273805336361,
4.6607181566678));
#249595=CARTESIAN_POINT('Ctrl Pts',(-2.75084742999899,-1.68169425877717,
4.67102731209234));
#249596=CARTESIAN_POINT('Ctrl Pts',(-2.699756844677,-1.76254575610088,4.67730417275568));
#249597=CARTESIAN_POINT('Ctrl Pts',(-2.59561775987218,-1.91217284840742,
4.68943590561957));
#249598=CARTESIAN_POINT('Ctrl Pts',(-2.54323284231886,-1.98131325789362,
4.69527064384686));
#249599=CARTESIAN_POINT('Ctrl Pts',(-2.36379596519379,-2.19928493189945,
4.71433461028405));
#249600=CARTESIAN_POINT('Ctrl Pts',(-2.22596393652188,-2.33869232057012,
4.72763054210887));
#249601=CARTESIAN_POINT('Ctrl Pts',(-2.05396595891868,-2.48358541314899,
4.74210669012912));
#249602=CARTESIAN_POINT('Ctrl Pts',(-2.03134540196986,-2.50212083245402,
4.74397208068401));
#249603=CARTESIAN_POINT('Ctrl Pts',(-1.9981325307271,-2.52858831009139,
4.74665190185437));
#249604=CARTESIAN_POINT('Ctrl Pts',(-1.98773941758833,-2.53676653916622,
4.74748225626082));
#249605=CARTESIAN_POINT('Ctrl Pts',(-1.96923158348602,-2.55114657155005,
4.74894598192547));
#249606=CARTESIAN_POINT('Ctrl Pts',(-1.96113733146996,-2.5573740899968,
4.749581102196));
#249607=CARTESIAN_POINT('Ctrl Pts',(-1.94352117302168,-2.5707947031525,
4.75095241475063));
#249608=CARTESIAN_POINT('Ctrl Pts',(-1.93398881160816,-2.57797347597473,
4.75168763781905));
#249609=CARTESIAN_POINT('Ctrl Pts',(-1.90678980646376,-2.59822113849531,
4.7537668842568));
#249610=CARTESIAN_POINT('Ctrl Pts',(-1.88902869700136,-2.61116278545878,
4.75510255170106));
#249611=CARTESIAN_POINT('Ctrl Pts',(-1.74764691782975,-2.71198305772239,
4.76557345018828));
#249612=CARTESIAN_POINT('Ctrl Pts',(-1.61807922520001,-2.79122781553408,
4.7742090443557));
#249613=CARTESIAN_POINT('Ctrl Pts',(-1.25666895854297,-2.97861127104595,
4.79711204509908));
#249614=CARTESIAN_POINT('Ctrl Pts',(-1.01679197724353,-3.06878931060516,
4.81118230517882));
#249615=CARTESIAN_POINT('Ctrl Pts',(-0.723089568302622,-3.14093514632293,
4.82900213805161));
#249616=CARTESIAN_POINT('Ctrl Pts',(-0.677150533653468,-3.15115834927157,
4.83180274421321));
#249617=CARTESIAN_POINT('Ctrl Pts',(-0.608159023441252,-3.1649333242609,
4.83603668765029));
#249618=CARTESIAN_POINT('Ctrl Pts',(-0.585263951846832,-3.1692469781298,
4.8374462798628));
#249619=CARTESIAN_POINT('Ctrl Pts',(-0.545527596141718,-3.1762884318237,
4.83990150631911));
#249620=CARTESIAN_POINT('Ctrl Pts',(-0.528707513479019,-3.17913147071711,
4.8409434879517));
#249621=CARTESIAN_POINT('Ctrl Pts',(-0.493598013269676,-3.18477957099909,
4.84312446549881));
#249622=CARTESIAN_POINT('Ctrl Pts',(-0.475305465807736,-3.18756091803992,
4.84426416302737));
#249623=CARTESIAN_POINT('Ctrl Pts',(-0.431808150409862,-3.19379185858663,
4.84698266841423));
#249624=CARTESIAN_POINT('Ctrl Pts',(-0.406584789288867,-3.19710079053359,
4.84856580851949));
#249625=CARTESIAN_POINT('Ctrl Pts',(-0.320144133022171,-3.20740106643206,
4.8540154782244));
#249626=CARTESIAN_POINT('Ctrl Pts',(-0.25876992512015,-3.21293497728788,
4.85792663711149));
#249627=CARTESIAN_POINT('Ctrl Pts',(-0.107697943617962,-3.22220009985294,
4.86766118228952));
#249628=CARTESIAN_POINT('Ctrl Pts',(-0.0179342315945053,-3.22394920783809,
4.8735386221631));
#249629=CARTESIAN_POINT('Ctrl Pts',(0.20566406224828,-3.2189678156127,4.88838322270597));
#249630=CARTESIAN_POINT('Ctrl Pts',(0.339226372805878,-3.2076429925882,
4.89743703731633));
#249631=CARTESIAN_POINT('Ctrl Pts',(0.522019698413308,-3.18059767929463,
4.90992088736739));
#249632=CARTESIAN_POINT('Ctrl Pts',(0.572167344919531,-3.17196009208536,
4.91335452123766));
#249633=CARTESIAN_POINT('Ctrl Pts',(0.739085122151661,-3.13912222685998,
4.92477963265236));
#249634=CARTESIAN_POINT('Ctrl Pts',(0.854725246695212,-3.10962790397464,
4.93269122995297));
#249635=CARTESIAN_POINT('Ctrl Pts',(0.988937721559243,-3.06734087691087,
4.94167950875389));
#249636=CARTESIAN_POINT('Ctrl Pts',(1.00933661333444,-3.06068906130979,
4.94304012647017));
#249637=CARTESIAN_POINT('Ctrl Pts',(1.04099305994269,-3.05001538442492,
4.94514139160854));
#249638=CARTESIAN_POINT('Ctrl Pts',(1.05229683266794,-3.04613390754304,
4.94588965667127));
#249639=CARTESIAN_POINT('Ctrl Pts',(1.07312526507173,-3.03885208568645,
4.94726428848358));
#249640=CARTESIAN_POINT('Ctrl Pts',(1.08265557460268,-3.03546977313781,
4.94789162594917));
#249641=CARTESIAN_POINT('Ctrl Pts',(1.10474481101625,-3.02751302259283,
4.94934200589844));
#249642=CARTESIAN_POINT('Ctrl Pts',(1.11729137056544,-3.02290525937947,
4.95016309667502));
#249643=CARTESIAN_POINT('Ctrl Pts',(1.15719014689239,-3.00796996291873,
4.95276662445287));
#249644=CARTESIAN_POINT('Ctrl Pts',(1.1844314777628,-2.99734791817495,4.95453279709229));
#249645=CARTESIAN_POINT('Ctrl Pts',(1.33196630639441,-2.93749497376177,
4.96405509436756));
#249646=CARTESIAN_POINT('Ctrl Pts',(1.44935388104242,-2.88138703051498,
4.97147720478038));
#249647=CARTESIAN_POINT('Ctrl Pts',(1.76344910931434,-2.70719065798654,
4.99172455820149));
#249648=CARTESIAN_POINT('Ctrl Pts',(1.95142015441589,-2.57499328518299,
5.00433781408325));
#249649=CARTESIAN_POINT('Ctrl Pts',(2.18191565297002,-2.37304355976495,
5.02212711194031));
#249650=CARTESIAN_POINT('Ctrl Pts',(2.23819578024565,-2.32003662484254,
5.02668038924848));
#249651=CARTESIAN_POINT('Ctrl Pts',(2.31254852651237,-2.2447827261485,5.03302920142302));
#249652=CARTESIAN_POINT('Ctrl Pts',(2.3323133519876,-2.22424021291845,5.03475110338649));
#249653=CARTESIAN_POINT('Ctrl Pts',(2.36355175806603,-2.19089843447372,
5.03752975887448));
#249654=CARTESIAN_POINT('Ctrl Pts',(2.37520024316876,-2.17826459603496,
5.03857903593065));
#249655=CARTESIAN_POINT('Ctrl Pts',(2.39912121389744,-2.15190011114326,
5.0407616339254));
#249656=CARTESIAN_POINT('Ctrl Pts',(2.41137813631746,-2.13815624985995,
5.04189554772472));
#249657=CARTESIAN_POINT('Ctrl Pts',(2.43994189858018,-2.10556929171489,
5.04457545757187));
#249658=CARTESIAN_POINT('Ctrl Pts',(2.45614912647858,-2.08664082287587,
5.04612545695101));
#249659=CARTESIAN_POINT('Ctrl Pts',(2.50957948737611,-2.02275431701971,
5.05133610861066));
#249660=CARTESIAN_POINT('Ctrl Pts',(2.54579881618331,-1.97697544632534,
5.05503626474707));
#249661=CARTESIAN_POINT('Ctrl Pts',(2.63061851811143,-1.86357055267236,
5.06412722885367));
#249662=CARTESIAN_POINT('Ctrl Pts',(2.677877823063,-1.7949979277509,5.0695631503027));
#249663=CARTESIAN_POINT('Ctrl Pts',(2.79876149765712,-1.60418136286022,
5.08450793902741));
#249664=CARTESIAN_POINT('Ctrl Pts',(2.86700823601016,-1.47875724061629,
5.09414606886764));
#249665=CARTESIAN_POINT('Ctrl Pts',(2.93988252757465,-1.32068045758809,
5.10590682926379));
#249666=CARTESIAN_POINT('Ctrl Pts',(2.95262741918425,-1.29193556039143,
5.10803004659204));
#249667=CARTESIAN_POINT('Ctrl Pts',(3.01993157016601,-1.1339370967351,5.11960469937688));
#249668=CARTESIAN_POINT('Ctrl Pts',(3.06643258941631,-1.0013987429798,5.12897375333015));
#249669=CARTESIAN_POINT('Ctrl Pts',(3.11002964776455,-0.845169598859093,
5.13933921764393));
#249670=CARTESIAN_POINT('Ctrl Pts',(3.11569481421617,-0.824040014475264,
5.14072698807235));
#249671=CARTESIAN_POINT('Ctrl Pts',(3.12414517777828,-0.791188692737247,
5.1428610512909));
#249672=CARTESIAN_POINT('Ctrl Pts',(3.127080420288,-0.779506699964299,5.1436153300966));
#249673=CARTESIAN_POINT('Ctrl Pts',(3.13237975052589,-0.757904121151732,
5.14500132908464));
#249674=CARTESIAN_POINT('Ctrl Pts',(3.13476226856351,-0.747988691117952,
5.14563403158122));
#249675=CARTESIAN_POINT('Ctrl Pts',(3.1401408294909,-0.725127361562234,
5.14708499968029));
#249676=CARTESIAN_POINT('Ctrl Pts',(3.14310391515902,-0.712174074424841,
5.1479014109949));
#249677=CARTESIAN_POINT('Ctrl Pts',(3.15223761637016,-0.671077966968531,
5.15047458706594));
#249678=CARTESIAN_POINT('Ctrl Pts',(3.15811119056082,-0.642869710461523,
5.15221561626061));
#249679=CARTESIAN_POINT('Ctrl Pts',(3.18761479197423,-0.49099859935512,
5.16147266265394));
#249680=CARTESIAN_POINT('Ctrl Pts',(3.20436365043623,-0.366097940569403,
5.16867477164358));
#249681=CARTESIAN_POINT('Ctrl Pts',(3.23000982107142,-0.023429972332404,
5.18806682828025));
#249682=CARTESIAN_POINT('Ctrl Pts',(3.22421853766283,0.194745799613003,
5.20004993365799));
#249683=CARTESIAN_POINT('Ctrl Pts',(3.1849946506127,0.500046321840096,5.21780988683606));
#249684=CARTESIAN_POINT('Ctrl Pts',(3.16976963971649,0.588893543495585,
5.22309327479103));
#249685=CARTESIAN_POINT('Ctrl Pts',(3.14452649461475,0.706381613134253,
5.23029401617538));
#249686=CARTESIAN_POINT('Ctrl Pts',(3.13779854853652,0.735691535770736,
5.23210827704359));
#249687=CARTESIAN_POINT('Ctrl Pts',(3.12605255217834,0.783766616708003,
5.2351155357479));
#249688=CARTESIAN_POINT('Ctrl Pts',(3.12127317579946,0.802588565138288,
5.23630090366181));
#249689=CARTESIAN_POINT('Ctrl Pts',(3.11161604578071,0.83922844546739,5.23862454266085));
#249690=CARTESIAN_POINT('Ctrl Pts',(3.10675460987071,0.857049923684429,
5.23976225052994));
#249691=CARTESIAN_POINT('Ctrl Pts',(3.0948824950718,0.899143001297471,5.24246767327893));
#249692=CARTESIAN_POINT('Ctrl Pts',(3.08773917394485,0.923375617485213,
5.24403960868963));
#249693=CARTESIAN_POINT('Ctrl Pts',(3.06252403059443,1.00534793012647,5.2494074775207));
#249694=CARTESIAN_POINT('Ctrl Pts',(3.04311240170282,1.06265894243753,5.25324624886556));
#249695=CARTESIAN_POINT('Ctrl Pts',(2.99170991578357,1.20143445084811,5.26275819533515));
#249696=CARTESIAN_POINT('Ctrl Pts',(2.95799303033413,1.28220440569085,5.2684822262022));
#249697=CARTESIAN_POINT('Ctrl Pts',(2.86297702889624,1.48605714776504,5.28339406667683));
#249698=CARTESIAN_POINT('Ctrl Pts',(2.79701461540177,1.60676966191795,5.29268404150515));
#249699=CARTESIAN_POINT('Ctrl Pts',(2.69665350019406,1.76542045184021,5.3053670955559));
#249700=CARTESIAN_POINT('Ctrl Pts',(2.66876065923517,1.80730908883245,5.30876307807839));
#249701=CARTESIAN_POINT('Ctrl Pts',(2.5710322324836,1.94687587081247,5.32020785079583));
#249702=CARTESIAN_POINT('Ctrl Pts',(2.49671682779944,2.04130922351024,5.32817621373671));
#249703=CARTESIAN_POINT('Ctrl Pts',(2.40309379623298,2.14749132587736,5.33721873895071));
#249704=CARTESIAN_POINT('Ctrl Pts',(2.38872931195625,2.16345813902699,5.33858073642223));
#249705=CARTESIAN_POINT('Ctrl Pts',(2.36612094801712,2.1880887023567,5.34068366941165));
#249706=CARTESIAN_POINT('Ctrl Pts',(2.35798693959434,2.19685186423434,5.34143224111474));
#249707=CARTESIAN_POINT('Ctrl Pts',(2.34288365398304,2.21294283777586,5.34280714009197));
#249708=CARTESIAN_POINT('Ctrl Pts',(2.33592861352483,2.22028316562009,5.34343444137163));
#249709=CARTESIAN_POINT('Ctrl Pts',(2.31970535949034,2.23724452317044,5.34488435856982));
#249710=CARTESIAN_POINT('Ctrl Pts',(2.31041175465772,2.24684079313815,5.34570502720339));
#249711=CARTESIAN_POINT('Ctrl Pts',(2.28061590662946,2.27722663938834,5.34830580716778));
#249712=CARTESIAN_POINT('Ctrl Pts',(2.25989007520149,2.2977961316083,5.35006970237861));
#249713=CARTESIAN_POINT('Ctrl Pts',(2.14566639873494,2.40811746070337,5.3595677286241));
#249714=CARTESIAN_POINT('Ctrl Pts',(2.0470897425368,2.4924575156919,5.36696971130355));
#249715=CARTESIAN_POINT('Ctrl Pts',(1.76174468179251,2.70821051542694,5.38713805184988));
#249716=CARTESIAN_POINT('Ctrl Pts',(1.56571590589933,2.82607137389018,5.39969277030554));
#249717=CARTESIAN_POINT('Ctrl Pts',(1.28776582640211,2.95532212385702,5.41747655410687));
#249718=CARTESIAN_POINT('Ctrl Pts',(1.21546495466953,2.98578519071791,5.42209514006862));
#249719=CARTESIAN_POINT('Ctrl Pts',(1.11532367101914,3.02373814846748,5.42852107775098));
#249720=CARTESIAN_POINT('Ctrl Pts',(1.088384884437,3.03353878254591,5.43025238272244));
#249721=CARTESIAN_POINT('Ctrl Pts',(1.04506596019011,3.04864740791368,5.43304227436132));
#249722=CARTESIAN_POINT('Ctrl Pts',(1.02876743151095,3.0541858870987,5.43409326871958));
#249723=CARTESIAN_POINT('Ctrl Pts',(0.994959743864795,3.06537291817463,
5.43627640215543));
#249724=CARTESIAN_POINT('Ctrl Pts',(0.977445056584141,3.0710026308408,5.43740910977572));
#249725=CARTESIAN_POINT('Ctrl Pts',(0.936202809504896,3.0838704938522,5.44008072817259));
#249726=CARTESIAN_POINT('Ctrl Pts',(0.912438237352037,3.09098517170136,
5.44162357184136));
#249727=CARTESIAN_POINT('Ctrl Pts',(0.833147204859636,3.11372937993529,
5.44678374970276));
#249728=CARTESIAN_POINT('Ctrl Pts',(0.777286033555698,3.12814172631091,
5.45043954755075));
#249729=CARTESIAN_POINT('Ctrl Pts',(0.45179222761321,3.20286335457135,5.47186930920237));
#249730=CARTESIAN_POINT('Ctrl Pts',(0.175712982882834,3.22978721300955,
5.49069059745284));
#249731=CARTESIAN_POINT('Ctrl Pts',(-0.223488210381403,3.21735125815338,
5.51753527790441));
#249732=CARTESIAN_POINT('Ctrl Pts',(-0.346321751064119,3.20645654334309,
5.52572010544602));
#249733=CARTESIAN_POINT('Ctrl Pts',(-0.489569334430889,3.18542056153159,
5.53496928938033));
#249734=CARTESIAN_POINT('Ctrl Pts',(-0.510866757840209,3.18207440206927,
5.53633654523143));
#249735=CARTESIAN_POINT('Ctrl Pts',(-0.543939505403389,3.17653754248131,
5.53844583333215));
#249736=CARTESIAN_POINT('Ctrl Pts',(-0.555738473941731,3.17449455876358,
5.53919557261394));
#249737=CARTESIAN_POINT('Ctrl Pts',(-0.577573332897452,3.17058839764178,
5.54057754690301));
#249738=CARTESIAN_POINT('Ctrl Pts',(-0.587611823457463,3.16874329835069,
5.54121071576184));
#249739=CARTESIAN_POINT('Ctrl Pts',(-0.610798530618598,3.16436754845529,
5.5426682997573));
#249740=CARTESIAN_POINT('Ctrl Pts',(-0.623939920735859,3.16180262138462,
5.54349079647664));
#249741=CARTESIAN_POINT('Ctrl Pts',(-0.665850878985013,3.15335099223102,
5.54610348977568));
#249742=CARTESIAN_POINT('Ctrl Pts',(-0.694557004318693,3.14715277304657,
5.54787726054944));
#249743=CARTESIAN_POINT('Ctrl Pts',(-0.851055991525991,3.11111584521567,
5.55748089215516));
#249744=CARTESIAN_POINT('Ctrl Pts',(-0.977032370339452,3.0738823889067,
5.5649704477637));
#249745=CARTESIAN_POINT('Ctrl Pts',(-1.31914727261272,2.9495989910338,5.58548337473681));
#249746=CARTESIAN_POINT('Ctrl Pts',(-1.52863264446049,2.84667567401028,
5.59829380447683));
#249747=CARTESIAN_POINT('Ctrl Pts',(-1.78728078892754,2.68274969186606,
5.61610460417383));
#249748=CARTESIAN_POINT('Ctrl Pts',(-1.84798740328848,2.64129890409673,
5.62044041103311));
#249749=CARTESIAN_POINT('Ctrl Pts',(-1.929759157357,2.58126498251226,5.62653174224741));
#249750=CARTESIAN_POINT('Ctrl Pts',(-1.95208033463764,2.56442617525084,
5.62822137530027));
#249751=CARTESIAN_POINT('Ctrl Pts',(-1.98768248800329,2.53683419900508,
5.63096154460233));
#249752=CARTESIAN_POINT('Ctrl Pts',(-2.00110226476565,2.52626188960205,
5.63200499709723));
#249753=CARTESIAN_POINT('Ctrl Pts',(-2.02817974734219,2.50457869520352,
5.63413237427724));
#249754=CARTESIAN_POINT('Ctrl Pts',(-2.04183171393983,2.49346160198148,
5.63521652427954));
#249755=CARTESIAN_POINT('Ctrl Pts',(-2.05592572867899,2.48179117602389,
5.63634804668832));
#249756=CARTESIAN_POINT('Ctrl Pts',(-2.05645961919156,2.48134880213718,
5.63639092792553));
#249757=CARTESIAN_POINT('Ctrl Pts',(-2.05751398644129,2.48047459480543,
5.63647564945486));
#249758=CARTESIAN_POINT('Ctrl Pts',(-2.05803447010627,2.48004276973805,
5.63651748940746));
#249759=CARTESIAN_POINT('Ctrl Pts',(-2.07560033262908,2.46545971856123,
5.63793014360183));
#249760=CARTESIAN_POINT('Ctrl Pts',(-2.09249912789394,2.45113355928242,
5.63930800904221));
#249761=CARTESIAN_POINT('Ctrl Pts',(-2.12944719994724,2.41914982744088,
5.64236312059056));
#249762=CARTESIAN_POINT('Ctrl Pts',(-2.14942715861677,2.40141501756703,
5.64404346983437));
#249763=CARTESIAN_POINT('Ctrl Pts',(-2.20301905089817,2.35264057939362,
5.64862894439861));
#249764=CARTESIAN_POINT('Ctrl Pts',(-2.23619326181725,2.32113118938754,
5.65155312275996));
#249765=CARTESIAN_POINT('Ctrl Pts',(-2.34107084796557,2.21718114079909,
5.66108082364586));
#249766=CARTESIAN_POINT('Ctrl Pts',(-2.41000737934355,2.14204721799929,
5.66779023663637));
#249767=CARTESIAN_POINT('Ctrl Pts',(-2.59930495367726,1.91500672674728,
5.68751308391195));
#249768=CARTESIAN_POINT('Ctrl Pts',(-2.70967525685434,1.7553612804268,5.70074453258324));
#249769=CARTESIAN_POINT('Ctrl Pts',(-2.85045144406285,1.5065025851044,5.71980994815918));
#249770=CARTESIAN_POINT('Ctrl Pts',(-2.89239878430832,1.42430890419627,
5.72587402046414));
#249771=CARTESIAN_POINT('Ctrl Pts',(-2.93925027477849,1.32187046831723,
5.73306008565515));
#249772=CARTESIAN_POINT('Ctrl Pts',(-2.94755896109007,1.30323824867788,
5.73435250557192));
#249773=CARTESIAN_POINT('Ctrl Pts',(-2.96035928985006,1.27378477368088,
5.7363711785142));
#249774=CARTESIAN_POINT('Ctrl Pts',(-2.96496965461113,1.26301612497903,
5.73710415575155));
#249775=CARTESIAN_POINT('Ctrl Pts',(-2.97350527290124,1.24277475207837,
5.73847206897431));
#249776=CARTESIAN_POINT('Ctrl Pts',(-2.97744404391373,1.23330842068044,
5.73910775648999));
#249777=CARTESIAN_POINT('Ctrl Pts',(-2.98658176180141,1.21104815793461,
5.74059333302139));
#249778=CARTESIAN_POINT('Ctrl Pts',(-2.99174373961122,1.19823940560914,
5.74144103847204));
#249779=CARTESIAN_POINT('Ctrl Pts',(-3.00849642592024,1.15588666161436,
5.74422187761295));
#249780=CARTESIAN_POINT('Ctrl Pts',(-3.01973346614564,1.12620365916316,
5.74613547777468));
#249781=CARTESIAN_POINT('Ctrl Pts',(-3.04595736486575,1.05371610609848,
5.75073430074019));
#249782=CARTESIAN_POINT('Ctrl Pts',(-3.06048306520564,1.01075105372816,
5.7533980440949));
#249783=CARTESIAN_POINT('Ctrl Pts',(-3.116332203421,0.833296619679835,5.76420082616484));
#249784=CARTESIAN_POINT('Ctrl Pts',(-3.14973700107303,0.696470863367105,
5.7720715455626));
#249785=CARTESIAN_POINT('Ctrl Pts',(-3.20638562499776,0.374172004119983,
5.79039355616449));
#249786=CARTESIAN_POINT('Ctrl Pts',(-3.22266215886783,0.188016439694972,
5.80082974578902));
#249787=CARTESIAN_POINT('Ctrl Pts',(-3.22274964543185,0.00151174366742828,
5.81173083705462));
#249788=CARTESIAN_POINT('Ctrl Pts',(-3.22274964711574,0.00150814964619596,
5.81173104712312));
#249789=CARTESIAN_POINT('Ctrl Pts',(-3.22274988237226,0.00100543239060466,
5.81176043066946));
#249790=CARTESIAN_POINT('Ctrl Pts',(-3.22275,0.000502715827386431,5.81178981720521));
#249791=CARTESIAN_POINT('Ctrl Pts',(-3.22275,-2.46480457644168E-12,5.81181920673623));
#249792=CARTESIAN_POINT('Origin',(0.,0.,-2.31077344927308));
#249793=CARTESIAN_POINT('',(-3.22275,-3.49632484551545E-13,7.3077847617826));
#249794=CARTESIAN_POINT('',(-3.22275,-1.40828092660302E-10,7.06317491433944));
#249795=CARTESIAN_POINT('',(-3.22275,-3.50678552687464E-13,-2.31077344927308));
#249796=CARTESIAN_POINT('',(-3.22274894051683,-0.00261321596174632,6.06203802249303));
#249797=CARTESIAN_POINT('Ctrl Pts',(-3.22275,-3.49632484551545E-13,7.3077847617826));
#249798=CARTESIAN_POINT('Ctrl Pts',(-3.22275,9.92968828600041E-6,7.30778413912117));
#249799=CARTESIAN_POINT('Ctrl Pts',(-3.22274999995411,1.98593771586289E-5,
7.30778351646216));
#249800=CARTESIAN_POINT('Ctrl Pts',(-3.22274990056665,0.0107721578420478,
7.3071092768844));
#249801=CARTESIAN_POINT('Ctrl Pts',(-3.22269609007642,0.0215146429154826,
7.30643851249414));
#249802=CARTESIAN_POINT('Ctrl Pts',(-3.22248534667233,0.0425687601278631,
7.30512975584816));
#249803=CARTESIAN_POINT('Ctrl Pts',(-3.22233263290866,0.05288019896246,
7.30449156074315));
#249804=CARTESIAN_POINT('Ctrl Pts',(-3.22183246382275,0.0783840571584081,
7.30291957959404));
#249805=CARTESIAN_POINT('Ctrl Pts',(-3.22142703847561,0.0935753280267247,
7.3019889396206));
#249806=CARTESIAN_POINT('Ctrl Pts',(-3.2194973597628,0.150720687044368,
7.29850770247362));
#249807=CARTESIAN_POINT('Ctrl Pts',(-3.21726078129448,0.192648416198304,
7.2959932056103));
#249808=CARTESIAN_POINT('Ctrl Pts',(-3.19470635481189,0.501763836330129,
7.27767028645722));
#249809=CARTESIAN_POINT('Ctrl Pts',(-3.14195334462456,0.765557875235954,
7.26314887218175));
#249810=CARTESIAN_POINT('Ctrl Pts',(-3.01261116089885,1.15329797079758,
7.23999119463465));
#249811=CARTESIAN_POINT('Ctrl Pts',(-2.95938772438528,1.28372113674657,
7.23187654620352));
#249812=CARTESIAN_POINT('Ctrl Pts',(-2.88304488375447,1.44059337587614,
7.2214584885312));
#249813=CARTESIAN_POINT('Ctrl Pts',(-2.86779777632045,1.47071168550149,
7.21942734060435));
#249814=CARTESIAN_POINT('Ctrl Pts',(-2.84280250890804,1.51821886732769,
7.21617114624924));
#249815=CARTESIAN_POINT('Ctrl Pts',(-2.83336102759058,1.53576687472613,
7.21495682616968));
#249816=CARTESIAN_POINT('Ctrl Pts',(-2.8151968950943,1.56878918455843,7.21264916746556));
#249817=CARTESIAN_POINT('Ctrl Pts',(-2.80650782780787,1.58428117967987,
7.21155705069021));
#249818=CARTESIAN_POINT('Ctrl Pts',(-2.7864839183745,1.61930068689068,7.20906624926801));
#249819=CARTESIAN_POINT('Ctrl Pts',(-2.77507112898384,1.63878233140046,
7.20766480808503));
#249820=CARTESIAN_POINT('Ctrl Pts',(-2.73936717251082,1.69828644288028,
7.20333461920212));
#249821=CARTESIAN_POINT('Ctrl Pts',(-2.71440871702244,1.73789939254625,
7.20038191083833));
#249822=CARTESIAN_POINT('Ctrl Pts',(-2.65427213999663,1.82888831123676,
7.19343125108904));
#249823=CARTESIAN_POINT('Ctrl Pts',(-2.61845129760521,1.87981516253603,
7.1894110801307));
#249824=CARTESIAN_POINT('Ctrl Pts',(-2.47841145631802,2.06713630457029,
7.17413037868015));
#249825=CARTESIAN_POINT('Ctrl Pts',(-2.36483468976505,2.19616078423416,
7.16256598829609));
#249826=CARTESIAN_POINT('Ctrl Pts',(-2.11987614033175,2.43329319902482,
7.13952174865675));
#249827=CARTESIAN_POINT('Ctrl Pts',(-1.98910914412167,2.54130781750367,
7.12808166467081));
#249828=CARTESIAN_POINT('Ctrl Pts',(-1.82629320997995,2.65549264062458,
7.11527317150592));
#249829=CARTESIAN_POINT('Ctrl Pts',(-1.80190493580973,2.67210156926538,
7.11339000053754));
#249830=CARTESIAN_POINT('Ctrl Pts',(-1.7661898598399,2.69571289996707,7.11068705902997));
#249831=CARTESIAN_POINT('Ctrl Pts',(-1.75504309604228,2.70298324181404,
7.10985108337329));
#249832=CARTESIAN_POINT('Ctrl Pts',(-1.73541542073565,2.71561254776196,
7.10839281845152));
#249833=CARTESIAN_POINT('Ctrl Pts',(-1.72695404252774,2.72100127482593,
7.10776862235713));
#249834=CARTESIAN_POINT('Ctrl Pts',(-1.70881537198541,2.73243440164455,
7.10644014792023));
#249835=CARTESIAN_POINT('Ctrl Pts',(-1.69913102574339,2.73846699841989,
7.10573662116968));
#249836=CARTESIAN_POINT('Ctrl Pts',(-1.67216217331049,2.75506835966679,
7.10379277510277));
#249837=CARTESIAN_POINT('Ctrl Pts',(-1.65480941242268,2.76552596376837,
7.10255938456042));
#249838=CARTESIAN_POINT('Ctrl Pts',(-1.5472301140943,2.82898322281394,7.09501193895917));
#249839=CARTESIAN_POINT('Ctrl Pts',(-1.45455628333657,2.8777313163928,7.0889354577235));
#249840=CARTESIAN_POINT('Ctrl Pts',(-1.23334877869778,2.98066762276816,
7.07502347487843));
#249841=CARTESIAN_POINT('Ctrl Pts',(-1.10334893106829,3.03119653588395,
7.06728303828353));
#249842=CARTESIAN_POINT('Ctrl Pts',(-0.7855903423067,3.13154274737149,7.04859510706689));
#249843=CARTESIAN_POINT('Ctrl Pts',(-0.595828782214898,3.17311950542628,
7.03759860876347));
#249844=CARTESIAN_POINT('Ctrl Pts',(-0.368973638569646,3.20174743709907,
7.02396100487141));
#249845=CARTESIAN_POINT('Ctrl Pts',(-0.334386019773027,3.20554426680463,
7.02186954228853));
#249846=CARTESIAN_POINT('Ctrl Pts',(-0.279484994904434,3.21067278565784,
7.01852742441718));
#249847=CARTESIAN_POINT('Ctrl Pts',(-0.259208212426221,3.21237337061352,
7.01728826463294));
#249848=CARTESIAN_POINT('Ctrl Pts',(-0.221259469102199,3.21519444553711,
7.0149595723535));
#249849=CARTESIAN_POINT('Ctrl Pts',(-0.203591666941271,3.216361529545,7.01387153568127));
#249850=CARTESIAN_POINT('Ctrl Pts',(-0.164011700420257,3.21864864491948,
7.01142504293399));
#249851=CARTESIAN_POINT('Ctrl Pts',(-0.142096074098543,3.21969060705654,
7.01006421003083));
#249852=CARTESIAN_POINT('Ctrl Pts',(-0.0767056934237409,3.2221306218554,
7.00598459602022));
#249853=CARTESIAN_POINT('Ctrl Pts',(-0.0332128620819631,3.22287233988978,
7.0032457069895));
#249854=CARTESIAN_POINT('Ctrl Pts',(0.173149674675503,3.22221407476818,
6.99012421587993));
#249855=CARTESIAN_POINT('Ctrl Pts',(0.335723127776088,3.20934904401457,
6.97939698001102));
#249856=CARTESIAN_POINT('Ctrl Pts',(0.664433778654918,3.1580841704323,6.95707273266367));
#249857=CARTESIAN_POINT('Ctrl Pts',(0.82992438424521,3.11868449703209,6.94549285844709));
#249858=CARTESIAN_POINT('Ctrl Pts',(1.07813899885514,3.03842356006187,6.92810418100185));
#249859=CARTESIAN_POINT('Ctrl Pts',(1.16352308682281,3.00676212580583,6.92212285788626));
#249860=CARTESIAN_POINT('Ctrl Pts',(1.26595478943538,2.96376085570955,6.9150379533545));
#249861=CARTESIAN_POINT('Ctrl Pts',(1.28437806163169,2.9558235705828,6.91376738323969));
#249862=CARTESIAN_POINT('Ctrl Pts',(1.31322965751872,2.94307276339479,6.91178483703123));
#249863=CARTESIAN_POINT('Ctrl Pts',(1.32370807210394,2.9383747843607,6.91106632028839));
#249864=CARTESIAN_POINT('Ctrl Pts',(1.34236283952437,2.92989091031711,6.90979013728379));
#249865=CARTESIAN_POINT('Ctrl Pts',(1.35054847642814,2.92612671538305,6.90923121645568));
#249866=CARTESIAN_POINT('Ctrl Pts',(1.37034119335466,2.9169242130583,6.90788220507077));
#249867=CARTESIAN_POINT('Ctrl Pts',(1.38193174731057,2.91145092858595,6.90709424875949));
#249868=CARTESIAN_POINT('Ctrl Pts',(1.41801548519087,2.89414745477862,6.90464656426738));
#249869=CARTESIAN_POINT('Ctrl Pts',(1.44239244008304,2.88207591237268,6.90300077599895));
#249870=CARTESIAN_POINT('Ctrl Pts',(1.56763469040185,2.81806841600179,6.89457076032574));
#249871=CARTESIAN_POINT('Ctrl Pts',(1.6658685108344,2.76113658404077,6.88804401156089));
#249872=CARTESIAN_POINT('Ctrl Pts',(1.76545001935222,2.69617011079135,6.88130898670823));
#249873=CARTESIAN_POINT('Ctrl Pts',(1.76998950273728,2.69319219470912,6.88100170212606));
#249874=CARTESIAN_POINT('Ctrl Pts',(1.94779231388993,2.57590925209789,6.86895475172678));
#249875=CARTESIAN_POINT('Ctrl Pts',(2.1096127577566,2.44514584111433,6.85753718341984));
#249876=CARTESIAN_POINT('Ctrl Pts',(2.33393448848163,2.22492020141764,6.83952796465508));
#249877=CARTESIAN_POINT('Ctrl Pts',(2.40636218236888,2.14637785044955,6.83330355665445));
#249878=CARTESIAN_POINT('Ctrl Pts',(2.49501186551378,2.04010624454021,6.82502407177305));
#249879=CARTESIAN_POINT('Ctrl Pts',(2.51491065990404,2.01552523288682,6.82311849188951));
#249880=CARTESIAN_POINT('Ctrl Pts',(2.54646872729053,1.97534644067041,6.82001663800918));
#249881=CARTESIAN_POINT('Ctrl Pts',(2.55835430474045,1.95992851027221,6.81882935200126));
#249882=CARTESIAN_POINT('Ctrl Pts',(2.58088100562111,1.93015288007785,6.81654162384857));
#249883=CARTESIAN_POINT('Ctrl Pts',(2.59154384516465,1.91581246053714,6.81544208642551));
#249884=CARTESIAN_POINT('Ctrl Pts',(2.61592592647397,1.88244504047772,6.81288848908343));
#249885=CARTESIAN_POINT('Ctrl Pts',(2.62955766319016,1.86335563778055,6.81143114692731));
#249886=CARTESIAN_POINT('Ctrl Pts',(2.6725251758865,1.80177489167004,6.8067402298617));
#249887=CARTESIAN_POINT('Ctrl Pts',(2.70104747157817,1.75872841634368,6.80347654566614));
#249888=CARTESIAN_POINT('Ctrl Pts',(2.87746594039411,1.47805386410286,6.78228333501577));
#249889=CARTESIAN_POINT('Ctrl Pts',(2.9948852858588,1.22272705100825,6.76324518793915));
#249890=CARTESIAN_POINT('Ctrl Pts',(3.11616109469286,0.83208319320178,6.73571935017519));
#249891=CARTESIAN_POINT('Ctrl Pts',(3.14702579791309,0.706440375824682,
6.72711694127453));
#249892=CARTESIAN_POINT('Ctrl Pts',(3.17411031207386,0.558211110288434,
6.71749158113461));
#249893=CARTESIAN_POINT('Ctrl Pts',(3.17774866245485,0.537112103405677,
6.71613379105527));
#249894=CARTESIAN_POINT('Ctrl Pts',(3.18306361112129,0.504343656094835,
6.71404567417669));
#249895=CARTESIAN_POINT('Ctrl Pts',(3.18488682955874,0.492699065371516,
6.71330766891566));
#249896=CARTESIAN_POINT('Ctrl Pts',(3.18813397148161,0.471188598342148,
6.71195214400059));
#249897=CARTESIAN_POINT('Ctrl Pts',(3.18957602125016,0.461326049453632,
6.71133367462751));
#249898=CARTESIAN_POINT('Ctrl Pts',(3.192785759684,0.438639067559258,6.70991784316439));
#249899=CARTESIAN_POINT('Ctrl Pts',(3.19452195983252,0.425810521480139,
6.70912222901144));
#249900=CARTESIAN_POINT('Ctrl Pts',(3.1997537213394,0.385319467081328,6.70662572376869));
#249901=CARTESIAN_POINT('Ctrl Pts',(3.20296772631286,0.357621071460053,
6.70493957857703));
#249902=CARTESIAN_POINT('Ctrl Pts',(3.21806136541277,0.210940404891598,
6.69610811044508));
#249903=CARTESIAN_POINT('Ctrl Pts',(3.22367294941302,0.0913959533191167,
6.68924816963208));
#249904=CARTESIAN_POINT('Ctrl Pts',(3.22007552636798,-0.319790651449177,
6.66600197014875));
#249905=CARTESIAN_POINT('Ctrl Pts',(3.17796370029111,-0.609667990583178,
6.65008176197737));
#249906=CARTESIAN_POINT('Ctrl Pts',(3.08548983642161,-0.931527342351729,
6.63023873720678));
#249907=CARTESIAN_POINT('Ctrl Pts',(3.07270221924298,-0.972877961567803,
6.62764986328819));
#249908=CARTESIAN_POINT('Ctrl Pts',(3.05210698965571,-1.03501331324056,
6.62369354040752));
#249909=CARTESIAN_POINT('Ctrl Pts',(3.0449106851032,-1.05599645685755,6.62234593721242));
#249910=CARTESIAN_POINT('Ctrl Pts',(3.03157556804165,-1.09360930455246,
6.61990871314423));
#249911=CARTESIAN_POINT('Ctrl Pts',(3.02551503695888,-1.11026594886001,
6.61882170576858));
#249912=CARTESIAN_POINT('Ctrl Pts',(3.01226223381168,-1.14577525113013,
6.61648749010996));
#249913=CARTESIAN_POINT('Ctrl Pts',(3.00502971663756,-1.16461198004802,
6.6152389831758));
#249914=CARTESIAN_POINT('Ctrl Pts',(2.98479607243098,-1.21586587592183,
6.61181312038411));
#249915=CARTESIAN_POINT('Ctrl Pts',(2.971444383829,-1.248140834654,6.60962416222343));
#249916=CARTESIAN_POINT('Ctrl Pts',(2.88047405663126,-1.45830566659103,
6.59515644053076));
#249917=CARTESIAN_POINT('Ctrl Pts',(2.78745774375217,-1.629062067312,6.58235105442465));
#249918=CARTESIAN_POINT('Ctrl Pts',(2.56991516257729,-1.9546564267444,6.55600107273));
#249919=CARTESIAN_POINT('Ctrl Pts',(2.44529027770861,-2.10848423433274,
6.54250614681055));
#249920=CARTESIAN_POINT('Ctrl Pts',(2.27049269015021,-2.28774326783346,
6.52610215632516));
#249921=CARTESIAN_POINT('Ctrl Pts',(2.23269861233805,-2.32464275490054,
6.52268600639115));
#249922=CARTESIAN_POINT('Ctrl Pts',(2.18150253628502,-2.37222594434649,
6.51824718474363));
#249923=CARTESIAN_POINT('Ctrl Pts',(2.16890013718429,-2.38375365157204,
6.51716910344834));
#249924=CARTESIAN_POINT('Ctrl Pts',(2.14824446049359,-2.40234844809482,
6.51542651682457));
#249925=CARTESIAN_POINT('Ctrl Pts',(2.14024671933528,-2.40947635727887,
6.51475766014646));
#249926=CARTESIAN_POINT('Ctrl Pts',(2.12446539479925,-2.42340073387847,
6.51344958346601));
#249927=CARTESIAN_POINT('Ctrl Pts',(2.11668444445044,-2.43019984718989,
6.51281018557082));
#249928=CARTESIAN_POINT('Ctrl Pts',(2.09730245005747,-2.4469724236332,6.51123079472882));
#249929=CARTESIAN_POINT('Ctrl Pts',(2.0856626534697,-2.4569010819002,6.51029401486487));
#249930=CARTESIAN_POINT('Ctrl Pts',(2.04124141690142,-2.49424886762088,
6.50676119509746));
#249931=CARTESIAN_POINT('Ctrl Pts',(2.00798491934538,-2.52109914332094,
6.50420265035953));
#249932=CARTESIAN_POINT('Ctrl Pts',(1.91978253991394,-2.58945804374075,
6.4976096477115));
#249933=CARTESIAN_POINT('Ctrl Pts',(1.86402174777053,-2.62988250526622,
6.49363002391463));
#249934=CARTESIAN_POINT('Ctrl Pts',(1.69026934368923,-2.74754132208565,
6.48165256698351));
#249935=CARTESIAN_POINT('Ctrl Pts',(1.56846774853541,-2.81884826405065,
6.47382015761052));
#249936=CARTESIAN_POINT('Ctrl Pts',(1.26794867288633,-2.96925468139527,
6.45497577567945));
#249937=CARTESIAN_POINT('Ctrl Pts',(1.08596934518146,-3.04053035076556,
6.44391673140866));
#249938=CARTESIAN_POINT('Ctrl Pts',(0.865283068253194,-3.10461138461063,
6.43021044176989));
#249939=CARTESIAN_POINT('Ctrl Pts',(0.831736859943135,-3.11376625543214,
6.42812029691482));
#249940=CARTESIAN_POINT('Ctrl Pts',(0.778340758447474,-3.12741379707448,
6.42477981277982));
#249941=CARTESIAN_POINT('Ctrl Pts',(0.758584589860587,-3.13226448198665,
6.42354094962034));
#249942=CARTESIAN_POINT('Ctrl Pts',(0.721548928330557,-3.14098682522939,
6.42121252058057));
#249943=CARTESIAN_POINT('Ctrl Pts',(0.704280808700624,-3.14490375290543,
6.42012444732169));
#249944=CARTESIAN_POINT('Ctrl Pts',(0.665538857599904,-3.15335650824511,
6.41767748441787));
#249945=CARTESIAN_POINT('Ctrl Pts',(0.644049365521355,-3.15781563995248,
6.41631621384987));
#249946=CARTESIAN_POINT('Ctrl Pts',(0.579804714302836,-3.17046353891684,
6.41223394590117));
#249947=CARTESIAN_POINT('Ctrl Pts',(0.536928788786448,-3.17800562289104,
6.40949280155574));
#249948=CARTESIAN_POINT('Ctrl Pts',(0.332690613915168,-3.20968113667216,
6.39635087698163));
#249949=CARTESIAN_POINT('Ctrl Pts',(0.169822668895752,-3.22240332598583,
6.38560421312784));
#249950=CARTESIAN_POINT('Ctrl Pts',(-0.163756445318266,-3.22309801782482,
6.36321845845729));
#249951=CARTESIAN_POINT('Ctrl Pts',(-0.333981225130233,-3.20992729097151,
6.35159596295352));
#249952=CARTESIAN_POINT('Ctrl Pts',(-0.591409786316228,-3.16930252761697,
6.33422929634166));
#249953=CARTESIAN_POINT('Ctrl Pts',(-0.679834515013803,-3.15151900362662,
6.32830692119331));
#249954=CARTESIAN_POINT('Ctrl Pts',(-0.786842538724266,-3.12528349678802,
6.32128072960539));
#249955=CARTESIAN_POINT('Ctrl Pts',(-0.806236439989325,-3.12033667501667,
6.32001309632444));
#249956=CARTESIAN_POINT('Ctrl Pts',(-0.836673498853508,-3.11227033587859,
6.31803411347751));
#249957=CARTESIAN_POINT('Ctrl Pts',(-0.847747872473475,-3.1092720597373,
6.31731626027007));
#249958=CARTESIAN_POINT('Ctrl Pts',(-0.867492042521257,-3.10381319180374,
6.31604062939932));
#249959=CARTESIAN_POINT('Ctrl Pts',(-0.87616757975041,-3.10137536392791,
6.31548160408613));
#249960=CARTESIAN_POINT('Ctrl Pts',(-0.897173176305563,-3.0953776096944,
6.31413153394572));
#249961=CARTESIAN_POINT('Ctrl Pts',(-0.909492338238396,-3.09178038587292,
6.31334263270765));
#249962=CARTESIAN_POINT('Ctrl Pts',(-0.947933725905005,-3.08030576599116,
6.31088895709953));
#249963=CARTESIAN_POINT('Ctrl Pts',(-0.973978348481327,-3.072169957538,
6.30923822031145));
#249964=CARTESIAN_POINT('Ctrl Pts',(-1.10846881845805,-3.0282755845197,
6.3007597119694));
#249965=CARTESIAN_POINT('Ctrl Pts',(-1.21507163760882,-2.98709928602528,
6.29419271233494));
#249966=CARTESIAN_POINT('Ctrl Pts',(-1.57902898757241,-2.82379915637499,
6.27160206127704));
#249967=CARTESIAN_POINT('Ctrl Pts',(-1.82218061619398,-2.67335576162192,
6.25607856667965));
#249968=CARTESIAN_POINT('Ctrl Pts',(-2.07896240590237,-2.46297905215695,
6.23652182583848));
#249969=CARTESIAN_POINT('Ctrl Pts',(-2.11485067051489,-2.43223288429633,
6.23370983321367));
#249970=CARTESIAN_POINT('Ctrl Pts',(-2.16915404099555,-2.38359939847418,
6.22932278716067));
#249971=CARTESIAN_POINT('Ctrl Pts',(-2.18805400213912,-2.36626181391754,
6.22777019616485));
#249972=CARTESIAN_POINT('Ctrl Pts',(-2.21990009643659,-2.33634050805216,
6.22510866133825));
#249973=CARTESIAN_POINT('Ctrl Pts',(-2.23295128327971,-2.32387003800486,
6.22400455008015));
#249974=CARTESIAN_POINT('Ctrl Pts',(-2.25781587823742,-2.29970894364226,
6.22187479444982));
#249975=CARTESIAN_POINT('Ctrl Pts',(-2.26964499380194,-2.28803526004887,
6.22084990319165));
#249976=CARTESIAN_POINT('Ctrl Pts',(-2.29731962633682,-2.26029847227512,
6.21842408318191));
#249977=CARTESIAN_POINT('Ctrl Pts',(-2.31308762715854,-2.24415958370711,
6.21701983521302));
#249978=CARTESIAN_POINT('Ctrl Pts',(-2.36871986864714,-2.18600955240233,
6.21198481231834));
#249979=CARTESIAN_POINT('Ctrl Pts',(-2.40761768514765,-2.1430930856171,
6.20831358679803));
#249980=CARTESIAN_POINT('Ctrl Pts',(-2.49971248225722,-2.0358104658504,
6.19923828357681));
#249981=CARTESIAN_POINT('Ctrl Pts',(-2.55160298927834,-1.97038247925033,
6.19378772811086));
#249982=CARTESIAN_POINT('Ctrl Pts',(-2.6928149508659,-1.77738533314449,
6.1779649041189));
#249983=CARTESIAN_POINT('Ctrl Pts',(-2.77550933578156,-1.64526389469577,
6.16742353444825));
#249984=CARTESIAN_POINT('Ctrl Pts',(-2.91730192578725,-1.37739019448851,
6.14695400670735));
#249985=CARTESIAN_POINT('Ctrl Pts',(-2.9772592161,-1.24249337954665,6.1370493421721));
#249986=CARTESIAN_POINT('Ctrl Pts',(-3.03795118879321,-1.07603586388396,
6.12563939903445));
#249987=CARTESIAN_POINT('Ctrl Pts',(-3.047744226582,-1.04797704146004,6.12374313096452));
#249988=CARTESIAN_POINT('Ctrl Pts',(-3.06130523570215,-1.00732338702539,
6.1210384806562));
#249989=CARTESIAN_POINT('Ctrl Pts',(-3.06538617129397,-0.994835557741038,
6.12021345088048));
#249990=CARTESIAN_POINT('Ctrl Pts',(-3.0724417050406,-0.972789659871621,
6.11876753570489));
#249991=CARTESIAN_POINT('Ctrl Pts',(-3.07544830106975,-0.963242186992404,
6.11814484719697));
#249992=CARTESIAN_POINT('Ctrl Pts',(-3.08181666335691,-0.942685581572961,
6.11681175580627));
#249993=CARTESIAN_POINT('Ctrl Pts',(-3.0851639741898,-0.931672321204153,
6.11610217561669));
#249994=CARTESIAN_POINT('Ctrl Pts',(-3.09437385812005,-0.900776150222252,
6.11412387401025));
#249995=CARTESIAN_POINT('Ctrl Pts',(-3.10010382781171,-0.880853877806726,
6.11286248755346));
#249996=CARTESIAN_POINT('Ctrl Pts',(-3.13669814305368,-0.74883873285409,
6.10458936781926));
#249997=CARTESIAN_POINT('Ctrl Pts',(-3.16167282775681,-0.635189267223042,
6.09787156647126));
#249998=CARTESIAN_POINT('Ctrl Pts',(-3.20846359115117,-0.34924018308778,
6.08142006333233));
#249999=CARTESIAN_POINT('Ctrl Pts',(-3.22260828707642,-0.176074090493909,
6.07184374685539));
#250000=CARTESIAN_POINT('Ctrl Pts',(-3.22274894051683,-0.00261321596174632,
6.06203802249303));
#250001=CARTESIAN_POINT('Ctrl Pts',(-3.22274894300508,-0.00261014551656878,
6.06203784892107));
#250002=CARTESIAN_POINT('Ctrl Pts',(-3.22274964767178,-0.00174009292913683,
6.06198866493141));
#250003=CARTESIAN_POINT('Ctrl Pts',(-3.22275,-0.000870044343129958,6.06193947624883));
#250004=CARTESIAN_POINT('Ctrl Pts',(-3.22275,2.79355756999193E-11,6.06189028282397));
#250005=CARTESIAN_POINT('Ctrl Pts',(-3.22275,-2.46480457644168E-12,5.81181920673623));
#250006=CARTESIAN_POINT('Ctrl Pts',(-3.22274999999997,-0.0434837801921187,
5.81436133457606));
#250007=CARTESIAN_POINT('Ctrl Pts',(-3.22186992859092,-0.0869620681209187,
5.81692596223994));
#250008=CARTESIAN_POINT('Ctrl Pts',(-3.21876213012256,-0.16370143329292,
5.8215013348071));
#250009=CARTESIAN_POINT('Ctrl Pts',(-3.21689761344425,-0.196970637444475,
5.8235011317141));
#250010=CARTESIAN_POINT('Ctrl Pts',(-3.2132447692424,-0.247978130235755,
5.82659471663913));
#250011=CARTESIAN_POINT('Ctrl Pts',(-3.21182452403085,-0.265741053369173,
5.82767716406584));
#250012=CARTESIAN_POINT('Ctrl Pts',(-3.20872449272806,-0.300845860292135,
5.82982699177066));
#250013=CARTESIAN_POINT('Ctrl Pts',(-3.2070512404925,-0.318187718373057,
5.8308941344599));
#250014=CARTESIAN_POINT('Ctrl Pts',(-3.20318487296555,-0.355123861307938,
5.83317832567699));
#250015=CARTESIAN_POINT('Ctrl Pts',(-3.20095239888262,-0.3747132236896,
5.83439656018849));
#250016=CARTESIAN_POINT('Ctrl Pts',(-3.19469099110278,-0.425507934445638,
5.83757361289999));
#250017=CARTESIAN_POINT('Ctrl Pts',(-3.19038463378829,-0.456676370873758,
5.83954099701342));
#250018=CARTESIAN_POINT('Ctrl Pts',(-3.16995062350541,-0.590129144996906,
5.84804415735175));
#250019=CARTESIAN_POINT('Ctrl Pts',(-3.14935635711355,-0.691657541877878,
5.85471705432241));
#250020=CARTESIAN_POINT('Ctrl Pts',(-3.07551957797401,-0.982890686845009,
5.87444655537153));
#250021=CARTESIAN_POINT('Ctrl Pts',(-3.00973527357927,-1.16892070316436,
5.88781763692185));
#250022=CARTESIAN_POINT('Ctrl Pts',(-2.87312121358051,-1.46565190533348,
5.90983649590704));
#250023=CARTESIAN_POINT('Ctrl Pts',(-2.81176894529414,-1.58016537397906,
5.91851154516345));
#250024=CARTESIAN_POINT('Ctrl Pts',(-2.72834464461649,-1.71554850246875,
5.92874739559476));
#250025=CARTESIAN_POINT('Ctrl Pts',(-2.71267934469497,-1.74021322663474,
5.93061111494307));
#250026=CARTESIAN_POINT('Ctrl Pts',(-2.68936369435831,-1.77584318601964,
5.93329795252256));
#250027=CARTESIAN_POINT('Ctrl Pts',(-2.68197760228885,-1.78697852738216,
5.93413687445286));
#250028=CARTESIAN_POINT('Ctrl Pts',(-2.6688803407211,-1.80645994943347,
5.93560273587624));
#250029=CARTESIAN_POINT('Ctrl Pts',(-2.66319886825772,-1.8148255067094,
5.9362315691915));
#250030=CARTESIAN_POINT('Ctrl Pts',(-2.65071542092706,-1.83302160717609,
5.93759791271207));
#250031=CARTESIAN_POINT('Ctrl Pts',(-2.64389805461189,-1.84284116040986,
5.93833438745232));
#250032=CARTESIAN_POINT('Ctrl Pts',(-2.62468625090145,-1.87018727170844,
5.94038359910477));
#250033=CARTESIAN_POINT('Ctrl Pts',(-2.61217086321912,-1.88762861389349,
5.94168853702127));
#250034=CARTESIAN_POINT('Ctrl Pts',(-2.52875214648964,-2.00146157631271,
5.95020111930038));
#250035=CARTESIAN_POINT('Ctrl Pts',(-2.45269395925307,-2.09397572825346,
5.95710078863815));
#250036=CARTESIAN_POINT('Ctrl Pts',(-2.33744502524973,-2.2192389766148,
5.96675188708547));
#250037=CARTESIAN_POINT('Ctrl Pts',(-2.30236158104117,-2.25561570424696,
5.96959502134017));
#250038=CARTESIAN_POINT('Ctrl Pts',(-2.17101005743024,-2.38555024846243,
5.97996112729002));
#250039=CARTESIAN_POINT('Ctrl Pts',(-2.06977974434252,-2.47389280448074,
5.98743089631052));
#250040=CARTESIAN_POINT('Ctrl Pts',(-1.8923612162319,-2.61019110226427,
6.00013383179475));
#250041=CARTESIAN_POINT('Ctrl Pts',(-1.81914719874243,-2.66173447535921,
6.00527579280438));
#250042=CARTESIAN_POINT('Ctrl Pts',(-1.69217285180737,-2.74343765765416,
6.01412222473061));
#250043=CARTESIAN_POINT('Ctrl Pts',(-1.6395200852128,-2.77522473155901,
6.01777084062713));
#250044=CARTESIAN_POINT('Ctrl Pts',(-1.56386350641135,-2.81799480037799,
6.02300387363359));
#250045=CARTESIAN_POINT('Ctrl Pts',(-1.54158762781295,-2.83024226723834,
6.0245434576738));
#250046=CARTESIAN_POINT('Ctrl Pts',(-1.50285447117774,-2.85094514736221,
6.02721957242242));
#250047=CARTESIAN_POINT('Ctrl Pts',(-1.48646476326562,-2.85952483467569,
6.02835167654317));
#250048=CARTESIAN_POINT('Ctrl Pts',(-1.45481789801272,-2.87574574470078,
6.03053753385242));
#250049=CARTESIAN_POINT('Ctrl Pts',(-1.43957210356486,-2.88340785278103,
6.03159051117639));
#250050=CARTESIAN_POINT('Ctrl Pts',(-1.39928962963657,-2.90325358030089,
6.03437291778503));
#250051=CARTESIAN_POINT('Ctrl Pts',(-1.37415507793311,-2.91523422103812,
6.03610926048347));
#250052=CARTESIAN_POINT('Ctrl Pts',(-1.28283947035231,-2.95731742446838,
6.04242001402605));
#250053=CARTESIAN_POINT('Ctrl Pts',(-1.21580365689693,-2.98550223324129,
6.04705813285214));
#250054=CARTESIAN_POINT('Ctrl Pts',(-0.929681320955207,-3.09456566158678,
6.06688466627563));
#250055=CARTESIAN_POINT('Ctrl Pts',(-0.703115906473292,-3.15376672359909,
6.08272465723729));
#250056=CARTESIAN_POINT('Ctrl Pts',(-0.342117300404767,-3.20723589531851,
6.107328791496));
#250057=CARTESIAN_POINT('Ctrl Pts',(-0.210979787273408,-3.21852454018246,
6.11612254515036));
#250058=CARTESIAN_POINT('Ctrl Pts',(-0.0501263333765563,-3.22249418519377,
6.12648104944104));
#250059=CARTESIAN_POINT('Ctrl Pts',(-0.0207340267677778,-3.22281734861643,
6.12835616498684));
#250060=CARTESIAN_POINT('Ctrl Pts',(0.0220534536508843,-3.22270237541045,
6.1310562359189));
#250061=CARTESIAN_POINT('Ctrl Pts',(0.0354470871757176,-3.22258288862273,
6.13189720693695));
#250062=CARTESIAN_POINT('Ctrl Pts',(0.0590457762746158,-3.22222521613324,
6.13337104162845));
#250063=CARTESIAN_POINT('Ctrl Pts',(0.0692509535850956,-3.22202204563668,
6.13400577041875));
#250064=CARTESIAN_POINT('Ctrl Pts',(0.0914227474266566,-3.22147524398119,
6.1353789986524));
#250065=CARTESIAN_POINT('Ctrl Pts',(0.103388550565497,-3.22111342311192,
6.13611650251022));
#250066=CARTESIAN_POINT('Ctrl Pts',(0.136881351187679,-3.21991384258314,
6.13817139368808));
#250067=CARTESIAN_POINT('Ctrl Pts',(0.158402803307684,-3.21892688114299,
6.13948091300208));
#250068=CARTESIAN_POINT('Ctrl Pts',(0.302342682603505,-3.21087873596547,
6.1481759156007));
#250069=CARTESIAN_POINT('Ctrl Pts',(0.424295494991865,-3.19705070855505,
6.15523774563957));
#250070=CARTESIAN_POINT('Ctrl Pts',(0.592610254043079,-3.16816145914844,
6.16491185220941));
#250071=CARTESIAN_POINT('Ctrl Pts',(0.639857846724015,-3.15895806007848,
6.16761914093297));
#250072=CARTESIAN_POINT('Ctrl Pts',(0.83250807587018,-3.11693181681067,
6.17868123678252));
#250073=CARTESIAN_POINT('Ctrl Pts',(0.975753039941638,-3.07509970124007,
6.18697016357154));
#250074=CARTESIAN_POINT('Ctrl Pts',(1.19105815897809,-2.99565850149194,
6.20005808361595));
#250075=CARTESIAN_POINT('Ctrl Pts',(1.26545890642882,-2.96499610419253,
6.20470069680824));
#250076=CARTESIAN_POINT('Ctrl Pts',(1.39041368338942,-2.9079387641284,6.2127707496896));
#250077=CARTESIAN_POINT('Ctrl Pts',(1.44155796667899,-2.88292700501812,
6.21615496389612));
#250078=CARTESIAN_POINT('Ctrl Pts',(1.51388736643585,-2.84514880851099,
6.22107267326997));
#250079=CARTESIAN_POINT('Ctrl Pts',(1.53563136380337,-2.83347189218761,
6.22256852240006));
#250080=CARTESIAN_POINT('Ctrl Pts',(1.5733280835242,-2.81266671094163,6.22519352312719));
#250081=CARTESIAN_POINT('Ctrl Pts',(1.58934100165527,-2.80364948662779,
6.22631871622271));
#250082=CARTESIAN_POINT('Ctrl Pts',(1.62023165496409,-2.7859045998588,6.22850948314495));
#250083=CARTESIAN_POINT('Ctrl Pts',(1.63511819422471,-2.77719346245137,
6.22957443754758));
#250084=CARTESIAN_POINT('Ctrl Pts',(1.67471534581362,-2.75359371328175,
6.23243222437584));
#250085=CARTESIAN_POINT('Ctrl Pts',(1.69929672151833,-2.73849235774925,
6.2342326941016));
#250086=CARTESIAN_POINT('Ctrl Pts',(1.79107630691541,-2.68039681418366,
6.24105714501779));
#250087=CARTESIAN_POINT('Ctrl Pts',(1.85686860321058,-2.6352454634842,6.24615917039027));
#250088=CARTESIAN_POINT('Ctrl Pts',(2.10309270887033,-2.45246740354339,
6.26608576567545));
#250089=CARTESIAN_POINT('Ctrl Pts',(2.27046339344333,-2.29838367772893,
6.28148897922877));
#250090=CARTESIAN_POINT('Ctrl Pts',(2.50553693557324,-2.03103084639467,
6.30548281140622));
#250091=CARTESIAN_POINT('Ctrl Pts',(2.58492722075026,-1.92897875492472,
6.31411501697992));
#250092=CARTESIAN_POINT('Ctrl Pts',(2.67446859591214,-1.79838404641024,
6.32430655114676));
#250093=CARTESIAN_POINT('Ctrl Pts',(2.69062783703285,-1.77411652035588,
6.32616612690197));
#250094=CARTESIAN_POINT('Ctrl Pts',(2.71370402399587,-1.73842062268418,
6.3288481505682));
#250095=CARTESIAN_POINT('Ctrl Pts',(2.72088228435699,-1.72716397614703,
6.32968632543366));
#250096=CARTESIAN_POINT('Ctrl Pts',(2.73337396831992,-1.70730388290779,
6.33115136684133));
#250097=CARTESIAN_POINT('Ctrl Pts',(2.73871712178513,-1.69871961658833,
6.33178011983613));
#250098=CARTESIAN_POINT('Ctrl Pts',(2.75029307720659,-1.67992518684091,
6.3331468611566));
#250099=CARTESIAN_POINT('Ctrl Pts',(2.75650950877249,-1.66970535800357,
6.33388380856446));
#250100=CARTESIAN_POINT('Ctrl Pts',(2.77374037667783,-1.64101925293855,
6.3359356281472));
#250101=CARTESIAN_POINT('Ctrl Pts',(2.78462734645388,-1.62247664484869,
6.33724266967249));
#250102=CARTESIAN_POINT('Ctrl Pts',(2.8555545724189,-1.4988566951796,6.34583906152488));
#250103=CARTESIAN_POINT('Ctrl Pts',(2.90982722216481,-1.39056649427554,
6.35281327951319));
#250104=CARTESIAN_POINT('Ctrl Pts',(2.97753217432288,-1.23404580301658,
6.36247851978687));
#250105=CARTESIAN_POINT('Ctrl Pts',(2.99613195870388,-1.1881752141994,6.36526278766254));
#250106=CARTESIAN_POINT('Ctrl Pts',(3.06161652968979,-1.01534935859894,
6.37563158174329));
#250107=CARTESIAN_POINT('Ctrl Pts',(3.10154639574376,-0.885911472376493,
6.38316223198478));
#250108=CARTESIAN_POINT('Ctrl Pts',(3.1539661248722,-0.668184252813939,
6.39588272071658));
#250109=CARTESIAN_POINT('Ctrl Pts',(3.17114689989669,-0.581204157903485,
6.40097651612725));
#250110=CARTESIAN_POINT('Ctrl Pts',(3.19407378258385,-0.433288461617131,
6.40974853126948));
#250111=CARTESIAN_POINT('Ctrl Pts',(3.20170944303909,-0.372695793936298,
6.41337219167467));
#250112=CARTESIAN_POINT('Ctrl Pts',(3.21007288546623,-0.28669213038376,
6.41857554178521));
#250113=CARTESIAN_POINT('Ctrl Pts',(3.2122288153374,-0.261431233461784,
6.42011110406467));
#250114=CARTESIAN_POINT('Ctrl Pts',(3.21544114280908,-0.217709942757812,
6.42278248875917));
#250115=CARTESIAN_POINT('Ctrl Pts',(3.21663713654521,-0.199260813090744,
6.42391392802023));
#250116=CARTESIAN_POINT('Ctrl Pts',(3.21876213748401,-0.161443011757707,
6.42624221872893));
#250117=CARTESIAN_POINT('Ctrl Pts',(3.21967520556881,-0.142074235520886,
6.42743951729091));
#250118=CARTESIAN_POINT('Ctrl Pts',(3.22155310608351,-0.0927859004338243,
6.4304991420596));
#250119=CARTESIAN_POINT('Ctrl Pts',(3.22227593910218,-0.0628594839236813,
6.43236887683812));
#250120=CARTESIAN_POINT('Ctrl Pts',(3.22348939228392,0.0558977309461934,
6.43983834612798));
#250121=CARTESIAN_POINT('Ctrl Pts',(3.22072405111211,0.144715592496733,
6.44553668549827));
#250122=CARTESIAN_POINT('Ctrl Pts',(3.19845322814192,0.45155282828387,6.46561259437435));
#250123=CARTESIAN_POINT('Ctrl Pts',(3.16042462564723,0.667607318405048,
6.48048139666669));
#250124=CARTESIAN_POINT('Ctrl Pts',(3.06640012289486,0.999629187325682,
6.50372882837039));
#250125=CARTESIAN_POINT('Ctrl Pts',(3.02487108279783,1.11903039912414,6.51216134606523));
#250126=CARTESIAN_POINT('Ctrl Pts',(2.96537368340655,1.26234264883259,6.5221459944541));
#250127=CARTESIAN_POINT('Ctrl Pts',(2.95395289252483,1.2888415288211,6.52398604136861));
#250128=CARTESIAN_POINT('Ctrl Pts',(2.93675162662851,1.32732219459556,6.5266453600994));
#250129=CARTESIAN_POINT('Ctrl Pts',(2.93125076900897,1.33942646994399,6.52747999941842));
#250130=CARTESIAN_POINT('Ctrl Pts',(2.9213982755777,1.36075482119124,6.52894692900998));
#250131=CARTESIAN_POINT('Ctrl Pts',(2.91707756644868,1.36999271855508,6.52958102155058));
#250132=CARTESIAN_POINT('Ctrl Pts',(2.90756054367352,1.39009143299319,6.53095775282469));
#250133=CARTESIAN_POINT('Ctrl Pts',(2.90234716864195,1.40094376427632,6.53169934901541));
#250134=CARTESIAN_POINT('Ctrl Pts',(2.88750137806793,1.43140866704053,6.53377687735812));
#250135=CARTESIAN_POINT('Ctrl Pts',(2.87772995098887,1.45095326189195,6.53510466369191));
#250136=CARTESIAN_POINT('Ctrl Pts',(2.8050358134513,1.59273080602215,6.54471045131479));
#250137=CARTESIAN_POINT('Ctrl Pts',(2.73454022203084,1.71094005118563,6.55258027867703));
#250138=CARTESIAN_POINT('Ctrl Pts',(2.63740694746517,1.85239410447137,6.56226186750096));
#250139=CARTESIAN_POINT('Ctrl Pts',(2.61766799416713,1.88018446980692,6.56417729415332));
#250140=CARTESIAN_POINT('Ctrl Pts',(2.51324224686741,2.02237200984046,6.57407284824353));
#250141=CARTESIAN_POINT('Ctrl Pts',(2.42148669302438,2.1313789139507,6.58199212384508));
#250142=CARTESIAN_POINT('Ctrl Pts',(2.26491028046179,2.2941840468394,6.59485350485533));
#250143=CARTESIAN_POINT('Ctrl Pts',(2.20467428323837,2.35212859985901,6.59966780867515));
#250144=CARTESIAN_POINT('Ctrl Pts',(2.09853868242801,2.44656442915691,6.6080060323586));
#250145=CARTESIAN_POINT('Ctrl Pts',(2.05377039497085,2.48426420610363,6.6114825839729));
#250146=CARTESIAN_POINT('Ctrl Pts',(1.98849235441949,2.53626455946217,6.61651062712068));
#250147=CARTESIAN_POINT('Ctrl Pts',(1.96880277933712,2.55157898606136,6.61802203505817));
#250148=CARTESIAN_POINT('Ctrl Pts',(1.93426822706409,2.57780202176966,6.6206651339773));
#250149=CARTESIAN_POINT('Ctrl Pts',(1.91950364424909,2.58881489786488,6.62179270097019));
#250150=CARTESIAN_POINT('Ctrl Pts',(1.89078881511507,2.60985254332799,6.6239813667044));
#250151=CARTESIAN_POINT('Ctrl Pts',(1.87685119808133,2.6198935481183,6.62504178889267));
#250152=CARTESIAN_POINT('Ctrl Pts',(1.83960097242881,2.64627973721825,6.62787123654757));
#250153=CARTESIAN_POINT('Ctrl Pts',(1.81615131161926,2.66242793628292,6.62964762460616));
#250154=CARTESIAN_POINT('Ctrl Pts',(1.72846374160248,2.72111493460486,6.63627439661543));
#250155=CARTESIAN_POINT('Ctrl Pts',(1.66292479284379,2.76165402253906,6.64119711894708));
#250156=CARTESIAN_POINT('Ctrl Pts',(1.39669269527074,2.91341701566903,6.661083732319));
#250157=CARTESIAN_POINT('Ctrl Pts',(1.18584232505115,3.00541212417166,6.67665399107499));
#250158=CARTESIAN_POINT('Ctrl Pts',(0.842986879369213,3.11326285673778,
6.70088123684733));
#250159=CARTESIAN_POINT('Ctrl Pts',(0.716662166643344,3.14474705712447,
6.70957543827166));
#250160=CARTESIAN_POINT('Ctrl Pts',(0.560017428313409,3.1738546442395,6.71983109103602));
#250161=CARTESIAN_POINT('Ctrl Pts',(0.531192211306453,3.17880603292495,
6.72169665743349));
#250162=CARTESIAN_POINT('Ctrl Pts',(0.489098777384011,3.18544794750114,
6.72438564046118));
#250163=CARTESIAN_POINT('Ctrl Pts',(0.475881989485765,3.18744922893152,
6.72522489505407));
#250164=CARTESIAN_POINT('Ctrl Pts',(0.452644766912786,3.19082004305697,
6.72669112185593));
#250165=CARTESIAN_POINT('Ctrl Pts',(0.442629839432663,3.19222472065259,
6.72731999116825));
#250166=CARTESIAN_POINT('Ctrl Pts',(0.420765931408192,3.19518644250604,
6.72868615860354));
#250167=CARTESIAN_POINT('Ctrl Pts',(0.408914770192005,3.19672474459167,
6.7294224236821));
#250168=CARTESIAN_POINT('Ctrl Pts',(0.375768312520601,3.20083986628428,
6.73147047887866));
#250169=CARTESIAN_POINT('Ctrl Pts',(0.354455018187135,3.20327010568336,
6.73277448401887));
#250170=CARTESIAN_POINT('Ctrl Pts',(0.214699744145634,3.21779365496335,
6.74124993639423));
#250171=CARTESIAN_POINT('Ctrl Pts',(0.095676831531037,3.22352974226774,
6.74811655439362));
#250172=CARTESIAN_POINT('Ctrl Pts',(-0.0742990084174624,3.22229543520331,
6.75775616151764));
#250173=CARTESIAN_POINT('Ctrl Pts',(-0.125181119712875,3.22072011832756,
6.76062021632438));
#250174=CARTESIAN_POINT('Ctrl Pts',(-0.309122202453196,3.21065945419343,
6.77095613217079));
#250175=CARTESIAN_POINT('Ctrl Pts',(-0.441658104199968,3.19512565755485,
6.77837530234735));
#250176=CARTESIAN_POINT('Ctrl Pts',(-0.706553295066735,3.14727825321421,
6.79365419546302));
#250177=CARTESIAN_POINT('Ctrl Pts',(-0.838583848678587,3.11469886899691,
6.80150519680006));
#250178=CARTESIAN_POINT('Ctrl Pts',(-0.99963117863456,3.06397520352493,
6.81159575059794));
#250179=CARTESIAN_POINT('Ctrl Pts',(-1.03095153974753,3.05357910386917,
6.81358256137524));
#250180=CARTESIAN_POINT('Ctrl Pts',(-1.08103224392659,3.03609761094416,
6.8168014344336));
#250181=CARTESIAN_POINT('Ctrl Pts',(-1.09989619576528,3.0293147320911,6.81802357708241));
#250182=CARTESIAN_POINT('Ctrl Pts',(-1.1357992252247,3.01602558107791,6.82036875067955));
#250183=CARTESIAN_POINT('Ctrl Pts',(-1.15284880043982,3.00954976824428,
6.82149073693595));
#250184=CARTESIAN_POINT('Ctrl Pts',(-1.19157149238932,2.99446468648838,
6.82405839361698));
#250185=CARTESIAN_POINT('Ctrl Pts',(-1.21320777545681,2.98576426199977,
6.82550705510592));
#250186=CARTESIAN_POINT('Ctrl Pts',(-1.27975267672658,2.95816237099969,
6.83000689416161));
#250187=CARTESIAN_POINT('Ctrl Pts',(-1.32432685217871,2.93847741255057,
6.83308406440381));
#250188=CARTESIAN_POINT('Ctrl Pts',(-1.60257200150501,2.80798118934138,
6.85270280318403));
#250189=CARTESIAN_POINT('Ctrl Pts',(-1.82260555600264,2.67040444290543,
6.87017896088731));
#250190=CARTESIAN_POINT('Ctrl Pts',(-2.1426996812463,2.41211507541641,6.89793681740898));
#250191=CARTESIAN_POINT('Ctrl Pts',(-2.25464277211062,2.3078251317209,6.90817570944262));
#250192=CARTESIAN_POINT('Ctrl Pts',(-2.37375902490236,2.17987829365035,
6.91934544891933));
#250193=CARTESIAN_POINT('Ctrl Pts',(-2.38858076105836,2.16362734600826,
6.92074047507661));
#250194=CARTESIAN_POINT('Ctrl Pts',(-2.41118862081899,2.13832399002285,
6.92287464803779));
#250195=CARTESIAN_POINT('Ctrl Pts',(-2.41909244815879,2.12937826356613,
6.92362198499067));
#250196=CARTESIAN_POINT('Ctrl Pts',(-2.43366557436497,2.11269820921734,
6.92500186392206));
#250197=CARTESIAN_POINT('Ctrl Pts',(-2.44034785531494,2.1049760568126,6.92563531396071));
#250198=CARTESIAN_POINT('Ctrl Pts',(-2.45559576764542,2.0871851196157,6.92708259997092));
#250199=CARTESIAN_POINT('Ctrl Pts',(-2.46413627394468,2.07709526383945,
6.92789463611117));
#250200=CARTESIAN_POINT('Ctrl Pts',(-2.49134864031281,2.04454217871398,
6.93048758337708));
#250201=CARTESIAN_POINT('Ctrl Pts',(-2.50977784328783,2.02187687046959,
6.93225217373322));
#250202=CARTESIAN_POINT('Ctrl Pts',(-2.64744288241673,1.84778510279578,
6.94552671743596));
#250203=CARTESIAN_POINT('Ctrl Pts',(-2.75320160660144,1.68616812097163,
6.95628291647143));
#250204=CARTESIAN_POINT('Ctrl Pts',(-2.91658001159659,1.37969398163169,
6.97572772606296));
#250205=CARTESIAN_POINT('Ctrl Pts',(-2.97936638809607,1.23829175574905,
6.98437688485443));
#250206=CARTESIAN_POINT('Ctrl Pts',(-3.05177592024263,1.03743091348531,
6.99671559524954));
#250207=CARTESIAN_POINT('Ctrl Pts',(-3.07025736679884,0.981385908372844,
7.00016224717586));
#250208=CARTESIAN_POINT('Ctrl Pts',(-3.10013791266096,0.881645225790939,
7.00632636900969));
#250209=CARTESIAN_POINT('Ctrl Pts',(-3.11217687395752,0.838157616008936,
7.00902384680454));
#250210=CARTESIAN_POINT('Ctrl Pts',(-3.12885784199226,0.772576712192959,
7.01311323980674));
#250211=CARTESIAN_POINT('Ctrl Pts',(-3.13418748932593,0.750662982831865,
7.01448324448297));
#250212=CARTESIAN_POINT('Ctrl Pts',(-3.14334528888919,0.711210350097816,
7.01695688879043));
#250213=CARTESIAN_POINT('Ctrl Pts',(-3.14725775490478,0.693691841559114,
7.01805779468869));
#250214=CARTESIAN_POINT('Ctrl Pts',(-3.15536142575268,0.65592630657276,
7.02043686852944));
#250215=CARTESIAN_POINT('Ctrl Pts',(-3.15950451986651,0.635669886135118,
7.02171650808363));
#250216=CARTESIAN_POINT('Ctrl Pts',(-3.17013787019608,0.581007157240908,
7.02517987838766));
#250217=CARTESIAN_POINT('Ctrl Pts',(-3.17626266387758,0.546533410817749,
7.02737497771469));
#250218=CARTESIAN_POINT('Ctrl Pts',(-3.20906871155223,0.342647366588913,
7.04042568250777));
#250219=CARTESIAN_POINT('Ctrl Pts',(-3.22275000000749,0.171449469762571,
7.05168326423443));
#250220=CARTESIAN_POINT('Ctrl Pts',(-3.22275,-1.40828737560383E-10,7.06317491433944));
#250221=CARTESIAN_POINT('Origin',(0.,0.,-2.31077344927308));
#250222=CARTESIAN_POINT('',(-3.22275,6.20733405470152E-11,8.56255098483899));
#250223=CARTESIAN_POINT('',(-3.22275,-3.27109834657983E-12,8.3171463242964));
#250224=CARTESIAN_POINT('',(-3.22275,-3.50678552687464E-13,-2.31077344927308));
#250225=CARTESIAN_POINT('',(-3.22274893538059,0.00261954256402689,8.56237746067257));
#250226=CARTESIAN_POINT('Ctrl Pts',(-3.22275,6.20733405470152E-11,8.56255098483899));
#250227=CARTESIAN_POINT('Ctrl Pts',(-3.22274999999998,0.000873176498947361,
8.56249315116623));
#250228=CARTESIAN_POINT('Ctrl Pts',(-3.22274964513048,0.00174635740424604,
8.56243530976668));
#250229=CARTESIAN_POINT('Ctrl Pts',(-3.22274893538059,0.00261954256399533,
8.56237746067257));
#250230=CARTESIAN_POINT('Ctrl Pts',(-3.22274893830454,0.00261594284377387,
8.56237769915637));
#250231=CARTESIAN_POINT('Ctrl Pts',(-3.22256516576624,0.229017201608468,
8.5473784713664));
#250232=CARTESIAN_POINT('Ctrl Pts',(-3.19852586970591,0.454758449831492,
8.53186200725869));
#250233=CARTESIAN_POINT('Ctrl Pts',(-3.13847030541308,0.734646266102758,
8.51280182570542));
#250234=CARTESIAN_POINT('Ctrl Pts',(-3.12428256145324,0.792817925200208,
8.50885435029793));
#250235=CARTESIAN_POINT('Ctrl Pts',(-3.09826356417928,0.887907324882827,
8.50245878119287));
#250236=CARTESIAN_POINT('Ctrl Pts',(-3.08737267217223,0.925065845381036,
8.4999742227873));
#250237=CARTESIAN_POINT('Ctrl Pts',(-3.07141595910779,0.976083329288819,
8.49659171460607));
#250238=CARTESIAN_POINT('Ctrl Pts',(-3.06692117279408,0.990115750214793,
8.49566438309405));
#250239=CARTESIAN_POINT('Ctrl Pts',(-3.05914486721358,1.01383172322626,
8.49410284435985));
#250240=CARTESIAN_POINT('Ctrl Pts',(-3.05591324766903,1.02353129673551,
8.49346582856823));
#250241=CARTESIAN_POINT('Ctrl Pts',(-3.04914432580199,1.04353007563975,
8.49215601334705));
#250242=CARTESIAN_POINT('Ctrl Pts',(-3.04560091040924,1.05382695020228,
8.49148356987967));
#250243=CARTESIAN_POINT('Ctrl Pts',(-3.03610122267661,1.08098411764399,
8.48971472099901));
#250244=CARTESIAN_POINT('Ctrl Pts',(-3.03005661083684,1.09781340184896,
8.48862333613525));
#250245=CARTESIAN_POINT('Ctrl Pts',(-3.0031036583681,1.17093637874964,8.48389856287013));
#250246=CARTESIAN_POINT('Ctrl Pts',(-2.98076301510413,1.22669328969606,
8.48034066427099));
#250247=CARTESIAN_POINT('Ctrl Pts',(-2.93227833574217,1.33853875066314,
8.47323325481358));
#250248=CARTESIAN_POINT('Ctrl Pts',(-2.90605160932365,1.3945633538104,8.46968862318166));
#250249=CARTESIAN_POINT('Ctrl Pts',(-2.85410152616811,1.49769764104126,
8.4631328011241));
#250250=CARTESIAN_POINT('Ctrl Pts',(-2.82878296611447,1.54498572694711,
8.46011439510555));
#250251=CARTESIAN_POINT('Ctrl Pts',(-2.71816207604229,1.73975099305964,
8.44754788922916));
#250252=CARTESIAN_POINT('Ctrl Pts',(-2.6224193552483,1.88097124489743,8.43809065262141));
#250253=CARTESIAN_POINT('Ctrl Pts',(-2.47206050327171,2.06880894309093,
8.42428928437099));
#250254=CARTESIAN_POINT('Ctrl Pts',(-2.42637608029303,2.12220446545546,
8.42021219203979));
#250255=CARTESIAN_POINT('Ctrl Pts',(-2.34463199771312,2.21165359354654,
8.41306816124801));
#250256=CARTESIAN_POINT('Ctrl Pts',(-2.30939404615842,2.24842379019215,
8.41003308261231));
#250257=CARTESIAN_POINT('Ctrl Pts',(-2.25810576027505,2.2994641785123,8.40566767077397));
#250258=CARTESIAN_POINT('Ctrl Pts',(-2.24276019747075,2.31443379590396,
8.40436789985169));
#250259=CARTESIAN_POINT('Ctrl Pts',(-2.22685433344969,2.32964324857572,
8.40302674155583));
#250260=CARTESIAN_POINT('Ctrl Pts',(-2.2264418559548,2.33003745679979,8.40299196623254));
#250261=CARTESIAN_POINT('Ctrl Pts',(-2.22560068041687,2.33084094805349,
8.40292105650763));
#250262=CARTESIAN_POINT('Ctrl Pts',(-2.22517197412512,2.33125022238333,
8.40288492173852));
#250263=CARTESIAN_POINT('Ctrl Pts',(-2.21174537637508,2.34406115511253,
8.40175336124031));
#250264=CARTESIAN_POINT('Ctrl Pts',(-2.19864433604815,2.3563538299562,8.40065333424121));
#250265=CARTESIAN_POINT('Ctrl Pts',(-2.17304203874568,2.37997699525984,
8.39851114544122));
#250266=CARTESIAN_POINT('Ctrl Pts',(-2.16055321348649,2.39132013638167,
8.39746957088449));
#250267=CARTESIAN_POINT('Ctrl Pts',(-2.12693239443544,2.42137831566538,
8.39467420786597));
#250268=CARTESIAN_POINT('Ctrl Pts',(-2.10564298792965,2.43991431911858,
8.39291308989584));
#250269=CARTESIAN_POINT('Ctrl Pts',(-2.02466899600205,2.50856666164642,
8.38624626848788));
#250270=CARTESIAN_POINT('Ctrl Pts',(-1.96342049994779,2.55678891088787,
8.38126592183347));
#250271=CARTESIAN_POINT('Ctrl Pts',(-1.69597408550167,2.75207489333075,
8.35976864844818));
#250272=CARTESIAN_POINT('Ctrl Pts',(-1.4745876183046,2.87676965641239,8.34248545069205));
#250273=CARTESIAN_POINT('Ctrl Pts',(-1.13960125366551,3.01653503696742,
8.31810947762373));
#250274=CARTESIAN_POINT('Ctrl Pts',(-1.03615871796513,3.05361329749542,
8.31081909360575));
#250275=CARTESIAN_POINT('Ctrl Pts',(-0.905376819231954,3.09307737232661,
8.30204590511184));
#250276=CARTESIAN_POINT('Ctrl Pts',(-0.879640706716284,3.10049466221572,
8.30034047399109));
#250277=CARTESIAN_POINT('Ctrl Pts',(-0.841531127769652,3.11096531417921,
8.29784899932326));
#250278=CARTESIAN_POINT('Ctrl Pts',(-0.829227931784571,3.11426730948811,
8.29704983712732));
#250279=CARTESIAN_POINT('Ctrl Pts',(-0.808198753215153,3.11977777184471,
8.2956930787246));
#250280=CARTESIAN_POINT('Ctrl Pts',(-0.79948270464364,3.12202273890778,
8.29513344143526));
#250281=CARTESIAN_POINT('Ctrl Pts',(-0.779573432645709,3.12706186555746,
8.29386133435046));
#250282=CARTESIAN_POINT('Ctrl Pts',(-0.768374509896765,3.12983246676215,
8.29315020641053));
#250283=CARTESIAN_POINT('Ctrl Pts',(-0.73743456169804,3.13731090041672,
8.29119712794687));
#250284=CARTESIAN_POINT('Ctrl Pts',(-0.717663204729228,3.14189258103911,
8.28996205511375));
#250285=CARTESIAN_POINT('Ctrl Pts',(-0.604437135116019,3.1670062238142,
8.28295629999623));
#250286=CARTESIAN_POINT('Ctrl Pts',(-0.510139426278922,3.1835567998964,
8.2773820935005));
#250287=CARTESIAN_POINT('Ctrl Pts',(-0.212428354284217,3.222237938988,8.26020876644491));
#250288=CARTESIAN_POINT('Ctrl Pts',(-0.00756736986425217,3.2292247309117,
8.24897959781515));
#250289=CARTESIAN_POINT('Ctrl Pts',(0.337816250873611,3.20811778630414,
8.22937079253028));
#250290=CARTESIAN_POINT('Ctrl Pts',(0.478315019225521,3.19019554116657,
8.22120795137853));
#250291=CARTESIAN_POINT('Ctrl Pts',(0.649443765073081,3.15680558133873,
8.21078843376565));
#250292=CARTESIAN_POINT('Ctrl Pts',(0.681616403522962,3.15001549863993,
8.2088088812646));
#250293=CARTESIAN_POINT('Ctrl Pts',(0.732926603091755,3.13836354583708,
8.20561612262152));
#250294=CARTESIAN_POINT('Ctrl Pts',(0.752133643901503,3.13381590177792,
8.20441291332319));
#250295=CARTESIAN_POINT('Ctrl Pts',(0.788579791638005,3.12483220415761,
8.20211388635386));
#250296=CARTESIAN_POINT('Ctrl Pts',(0.805826339366947,3.12042918244698,
8.20101916316113));
#250297=CARTESIAN_POINT('Ctrl Pts',(0.845187310501891,3.11003230265226,
8.1985047311464));
#250298=CARTESIAN_POINT('Ctrl Pts',(0.867275862060893,3.10394507833176,
8.19708206689853));
#250299=CARTESIAN_POINT('Ctrl Pts',(0.92519323358183,3.08731756880291,8.19332036651984));
#250300=CARTESIAN_POINT('Ctrl Pts',(0.960906174000562,3.07638934930804,
8.19096898129311));
#250301=CARTESIAN_POINT('Ctrl Pts',(1.24554923096658,2.98384823064309,8.1719651855904));
#250302=CARTESIAN_POINT('Ctrl Pts',(1.48383287017575,2.872792042607,8.15431647340847));
#250303=CARTESIAN_POINT('Ctrl Pts',(1.83679747051241,2.6525572410114,8.1262134737614));
#250304=CARTESIAN_POINT('Ctrl Pts',(1.96158014791696,2.56165908348011,8.11585010096142));
#250305=CARTESIAN_POINT('Ctrl Pts',(2.10008739437867,2.44468500173641,8.10420347614881));
#250306=CARTESIAN_POINT('Ctrl Pts',(2.12056902908312,2.42694023939971,8.10247754245812));
#250307=CARTESIAN_POINT('Ctrl Pts',(2.1503914736593,2.40043701513786,8.0999620742373));
#250308=CARTESIAN_POINT('Ctrl Pts',(2.1599072437576,2.39187835496144,8.09915906859326));
#250309=CARTESIAN_POINT('Ctrl Pts',(2.17603299885462,2.3771998406796,8.09779802278509));
#250310=CARTESIAN_POINT('Ctrl Pts',(2.1826686270984,2.37110867864724,8.09723790571617));
#250311=CARTESIAN_POINT('Ctrl Pts',(2.19771506940251,2.35718013576969,8.09596776166901));
#250312=CARTESIAN_POINT('Ctrl Pts',(2.20610956624229,2.34932550106059,8.0952590495035));
#250313=CARTESIAN_POINT('Ctrl Pts',(2.2290768342929,2.32760363458407,8.09331916685197));
#250314=CARTESIAN_POINT('Ctrl Pts',(2.24356234929104,2.31364436422788,8.09209472366204));
#250315=CARTESIAN_POINT('Ctrl Pts',(2.32364180441999,2.23501474786827,8.08531381867647));
#250316=CARTESIAN_POINT('Ctrl Pts',(2.38657624321483,2.16768519963862,8.0799391816895));
#250317=CARTESIAN_POINT('Ctrl Pts',(2.55659429886864,1.9693977041362,8.06497428472047));
#250318=CARTESIAN_POINT('Ctrl Pts',(2.65637782565291,1.83258384578791,8.05562508019494));
#250319=CARTESIAN_POINT('Ctrl Pts',(2.83011781469167,1.55014863299856,8.03698597571246));
#250320=CARTESIAN_POINT('Ctrl Pts',(2.90466570523152,1.40550224215686,8.02773299834416));
#250321=CARTESIAN_POINT('Ctrl Pts',(2.98491720060174,1.21584331976309,8.015527095778));
#250322=CARTESIAN_POINT('Ctrl Pts',(3.00103828843865,1.17548908819945,8.01292710717728));
#250323=CARTESIAN_POINT('Ctrl Pts',(3.02406078605224,1.11429570602391,8.00897413548107));
#250324=CARTESIAN_POINT('Ctrl Pts',(3.03157364727922,1.09369088083438,8.00764138543358));
#250325=CARTESIAN_POINT('Ctrl Pts',(3.04477057222164,1.05631586973668,8.00522008783156));
#250326=CARTESIAN_POINT('Ctrl Pts',(3.05052788382326,1.03957234693322,8.00413400370949));
#250327=CARTESIAN_POINT('Ctrl Pts',(3.06260652674807,1.00348050258098,8.00178954365318));
#250328=CARTESIAN_POINT('Ctrl Pts',(3.06888308131703,0.984118112705343,
8.0005297560088));
#250329=CARTESIAN_POINT('Ctrl Pts',(3.08539944250445,0.931472192703086,
7.99709830369803));
#250330=CARTESIAN_POINT('Ctrl Pts',(3.0952836527629,0.898080799813092,7.99491524727062));
#250331=CARTESIAN_POINT('Ctrl Pts',(3.15582447554704,0.680673602889096,
7.98065425361863));
#250332=CARTESIAN_POINT('Ctrl Pts',(3.19058205784246,0.492655610007064,
7.96806861545985));
#250333=CARTESIAN_POINT('Ctrl Pts',(3.22158747211894,0.164005740571538,
7.94586418685519));
#250334=CARTESIAN_POINT('Ctrl Pts',(3.22566549115339,0.0246141418466337,
7.93639376924152));
#250335=CARTESIAN_POINT('Ctrl Pts',(3.21813043917037,-0.187143636830151,
7.92220497898741));
#250336=CARTESIAN_POINT('Ctrl Pts',(3.21309907637538,-0.259580103156683,
7.91738859757074));
#250337=CARTESIAN_POINT('Ctrl Pts',(3.20106153988697,-0.375882523598728,
7.90977306584647));
#250338=CARTESIAN_POINT('Ctrl Pts',(3.19558818779224,-0.41988002117325,
7.9069195121529));
#250339=CARTESIAN_POINT('Ctrl Pts',(3.18697665390763,-0.479101156392063,
7.90312789085596));
#250340=CARTESIAN_POINT('Ctrl Pts',(3.18463400508372,-0.494433399686895,
7.90215073406484));
#250341=CARTESIAN_POINT('Ctrl Pts',(3.18053958125119,-0.519993449135298,
7.90052990388033));
#250342=CARTESIAN_POINT('Ctrl Pts',(3.17884895594334,-0.530230647830305,
7.89988292922826));
#250343=CARTESIAN_POINT('Ctrl Pts',(3.17553724394443,-0.54969864684475,
7.8986569867339));
#250344=CARTESIAN_POINT('Ctrl Pts',(3.17392529220638,-0.558930796016713,
7.89807749585145));
#250345=CARTESIAN_POINT('Ctrl Pts',(3.16996867309066,-0.581022401219024,
7.89669504989115));
#250346=CARTESIAN_POINT('Ctrl Pts',(3.16758597705393,-0.593874995594126,
7.895894190184));
#250347=CARTESIAN_POINT('Ctrl Pts',(3.16003092170776,-0.633288517059704,
7.89344784321252));
#250348=CARTESIAN_POINT('Ctrl Pts',(3.15460205239384,-0.659799794096786,
7.89181567171407));
#250349=CARTESIAN_POINT('Ctrl Pts',(3.11302122980016,-0.850594928022836,
7.88014546040248));
#250350=CARTESIAN_POINT('Ctrl Pts',(3.0643854813284,-1.01191287369005,7.87067861793006));
#250351=CARTESIAN_POINT('Ctrl Pts',(2.94087568448125,-1.32931014390101,
7.85159562389091));
#250352=CARTESIAN_POINT('Ctrl Pts',(2.86560173286738,-1.48463403263234,
7.84200574471944));
#250353=CARTESIAN_POINT('Ctrl Pts',(2.74665872677585,-1.68697239439719,
7.82847400958385));
#250354=CARTESIAN_POINT('Ctrl Pts',(2.71348798565185,-1.73982536823445,
7.82483695248746));
#250355=CARTESIAN_POINT('Ctrl Pts',(2.65273468018209,-1.83065982039452,
7.81837551119254));
#250356=CARTESIAN_POINT('Ctrl Pts',(2.62581714089898,-1.86906411626918,
7.81557446231823));
#250357=CARTESIAN_POINT('Ctrl Pts',(2.58470422236186,-1.9250797616251,7.81137728117581));
#250358=CARTESIAN_POINT('Ctrl Pts',(2.57114530557423,-1.94315202275065,
7.81000540378385));
#250359=CARTESIAN_POINT('Ctrl Pts',(2.54658821944538,-1.97517633619724,
7.80754167095056));
#250360=CARTESIAN_POINT('Ctrl Pts',(2.53566249647054,-1.98918294851917,
7.80645267418254));
#250361=CARTESIAN_POINT('Ctrl Pts',(2.51224173273012,-2.01870150403738,
7.80413287002825));
#250362=CARTESIAN_POINT('Ctrl Pts',(2.49971760301111,-2.03418931346044,
7.80290093388389));
#250363=CARTESIAN_POINT('Ctrl Pts',(2.46560861930843,-2.07557907003295,
7.79956803750673));
#250364=CARTESIAN_POINT('Ctrl Pts',(2.44375999127483,-2.1012594573266,7.7974565113822));
#250365=CARTESIAN_POINT('Ctrl Pts',(2.32909537552576,-2.23182607609774,
7.78648955815788));
#250366=CARTESIAN_POINT('Ctrl Pts',(2.22992810613304,-2.33091068841016,
7.77737212337351));
#250367=CARTESIAN_POINT('Ctrl Pts',(1.92280559998955,-2.60019081821858,
7.75021015919382));
#250368=CARTESIAN_POINT('Ctrl Pts',(1.69966223837185,-2.75123888063121,
7.73167041025852));
#250369=CARTESIAN_POINT('Ctrl Pts',(1.43475210289737,-2.88590205155199,
7.71234285873751));
#250370=CARTESIAN_POINT('Ctrl Pts',(1.40894729087121,-2.89858791437247,
7.71048732035853));
#250371=CARTESIAN_POINT('Ctrl Pts',(1.36280734284358,-2.92050890489379,
7.70722181786576));
#250372=CARTESIAN_POINT('Ctrl Pts',(1.34253973305436,-2.92988109763965,
7.70580502995511));
#250373=CARTESIAN_POINT('Ctrl Pts',(1.31136967718072,-2.94390345200097,
7.70365478631454));
#250374=CARTESIAN_POINT('Ctrl Pts',(1.30053670948763,-2.94870518068374,
7.70291273159243));
#250375=CARTESIAN_POINT('Ctrl Pts',(1.28054864398093,-2.95743333908937,
7.70155352696631));
#250376=CARTESIAN_POINT('Ctrl Pts',(1.27140174763619,-2.96137710956607,
7.70093538534946));
#250377=CARTESIAN_POINT('Ctrl Pts',(1.25040405208881,-2.97031524247129,
7.69952506353682));
#250378=CARTESIAN_POINT('Ctrl Pts',(1.23854150904905,-2.9752811424265,7.69873457829612));
#250379=CARTESIAN_POINT('Ctrl Pts',(1.20128938397193,-2.99061422817989,
7.69627083894764));
#250380=CARTESIAN_POINT('Ctrl Pts',(1.17579628695179,-3.00072871976973,
7.69461178726365));
#250381=CARTESIAN_POINT('Ctrl Pts',(0.947302054553337,-3.08802556763735,
7.6799548259521));
#250382=CARTESIAN_POINT('Ctrl Pts',(0.73708469238602,-3.14483933957551,
7.66793500941696));
#250383=CARTESIAN_POINT('Ctrl Pts',(0.345874379720156,-3.20914480737122,
7.64572960314135));
#250384=CARTESIAN_POINT('Ctrl Pts',(0.166922456073278,-3.22340934216191,
7.63563018239052));
#250385=CARTESIAN_POINT('Ctrl Pts',(-0.0661585020297892,-3.22252133387607,
7.62191094516255));
#250386=CARTESIAN_POINT('Ctrl Pts',(-0.120022711545808,-3.22096487825367,
7.61870322054083));
#250387=CARTESIAN_POINT('Ctrl Pts',(-0.1976336307,-3.21677279810791,7.61401588058594));
#250388=CARTESIAN_POINT('Ctrl Pts',(-0.221431339444422,-3.21522229432192,
7.61256974301212));
#250389=CARTESIAN_POINT('Ctrl Pts',(-0.263083982668706,-3.21204385865439,
7.61002211200481));
#250390=CARTESIAN_POINT('Ctrl Pts',(-0.280946811771764,-3.2105307661657,
7.60892423394666));
#250391=CARTESIAN_POINT('Ctrl Pts',(-0.318010105905912,-3.20707959447224,
7.60663481153101));
#250392=CARTESIAN_POINT('Ctrl Pts',(-0.337207603902068,-3.20511793214001,
7.60544257319093));
#250393=CARTESIAN_POINT('Ctrl Pts',(-0.387032350640315,-3.19957408858473,
7.60233112149887));
#250394=CARTESIAN_POINT('Ctrl Pts',(-0.417627294780195,-3.19572460110338,
7.60040364942186));
#250395=CARTESIAN_POINT('Ctrl Pts',(-0.547813944547506,-3.1774429794755,
7.59212741828171));
#250396=CARTESIAN_POINT('Ctrl Pts',(-0.646746739277233,-3.15879078181821,
7.58564906873014));
#250397=CARTESIAN_POINT('Ctrl Pts',(-0.948367520102334,-3.0871610740129,
7.56531700919316));
#250398=CARTESIAN_POINT('Ctrl Pts',(-1.14688361574539,-3.01904074183851,
7.55107334695094));
#250399=CARTESIAN_POINT('Ctrl Pts',(-1.44942736427279,-2.8810498217309,
7.52868036184968));
#250400=CARTESIAN_POINT('Ctrl Pts',(-1.55847771933964,-2.82355105997055,
7.52046520061428));
#250401=CARTESIAN_POINT('Ctrl Pts',(-1.6881879185444,-2.7453484917562,7.51072423907064));
#250402=CARTESIAN_POINT('Ctrl Pts',(-1.7122065529566,-2.73043323205823,
7.50892203436262));
#250403=CARTESIAN_POINT('Ctrl Pts',(-1.74699368568106,-2.70819129066408,
7.50631758802554));
#250404=CARTESIAN_POINT('Ctrl Pts',(-1.75791828770339,-2.70111279142114,
7.50550052772984));
#250405=CARTESIAN_POINT('Ctrl Pts',(-1.77713697606881,-2.68849422562496,
7.50406506262489));
#250406=CARTESIAN_POINT('Ctrl Pts',(-1.78544861135059,-2.68298160602879,
7.50344491888437));
#250407=CARTESIAN_POINT('Ctrl Pts',(-1.80348432908141,-2.67089864113393,
7.50210075601906));
#250408=CARTESIAN_POINT('Ctrl Pts',(-1.81319821691838,-2.66431370387102,
7.50137771320789));
#250409=CARTESIAN_POINT('Ctrl Pts',(-1.84034250979878,-2.64569567535157,
7.49935917425581));
#250410=CARTESIAN_POINT('Ctrl Pts',(-1.85769092364641,-2.6335433631997,
7.49807132375313));
#250411=CARTESIAN_POINT('Ctrl Pts',(-1.97239446501926,-2.55149768216892,
7.48956227679538));
#250412=CARTESIAN_POINT('Ctrl Pts',(-2.06591608850664,-2.47638391009125,
7.48265162962741));
#250413=CARTESIAN_POINT('Ctrl Pts',(-2.19322130822174,-2.36189208385287,
7.47294479453799));
#250414=CARTESIAN_POINT('Ctrl Pts',(-2.23057316056949,-2.32664941076407,
7.47005661380756));
#250415=CARTESIAN_POINT('Ctrl Pts',(-2.36489299881334,-2.19370537026154,
7.4594565106647));
#250416=CARTESIAN_POINT('Ctrl Pts',(-2.45641431549734,-2.09071515613957,
7.45179999133454));
#250417=CARTESIAN_POINT('Ctrl Pts',(-2.62241759286614,-1.87790747457348,
7.43646355931109));
#250418=CARTESIAN_POINT('Ctrl Pts',(-2.69726133190693,-1.76872443507827,
7.42881082168785));
#250419=CARTESIAN_POINT('Ctrl Pts',(-2.78178513447398,-1.62752389156052,
7.41897160363767));
#250420=CARTESIAN_POINT('Ctrl Pts',(-2.79796974717712,-1.59953985023089,
7.41702469080633));
#250421=CARTESIAN_POINT('Ctrl Pts',(-2.82329566761753,-1.55418918515955,
7.41387205278009));
#250422=CARTESIAN_POINT('Ctrl Pts',(-2.83270432016028,-1.53697386387557,
7.41267587394001));
#250423=CARTESIAN_POINT('Ctrl Pts',(-2.85036182149819,-1.50395242309228,
7.41038200615435));
#250424=CARTESIAN_POINT('Ctrl Pts',(-2.85863785754082,-1.48816161208251,
7.40928532908256));
#250425=CARTESIAN_POINT('Ctrl Pts',(-2.87717890656514,-1.45205957018702,
7.40677820029387));
#250426=CARTESIAN_POINT('Ctrl Pts',(-2.8873605582297,-1.43170682062964,
7.40536490933303));
#250427=CARTESIAN_POINT('Ctrl Pts',(-2.91381819758687,-1.3773886733909,
7.40159263321956));
#250428=CARTESIAN_POINT('Ctrl Pts',(-2.92971538825062,-1.34324368561402,
7.39922085862288));
#250429=CARTESIAN_POINT('Ctrl Pts',(-3.05023439663354,-1.0720625973999,
7.38037436783688));
#250430=CARTESIAN_POINT('Ctrl Pts',(-3.12650499082791,-0.823509052567751,
7.36292844953784));
#250431=CARTESIAN_POINT('Ctrl Pts',(-3.19229483663836,-0.456448987694319,
7.33773544373467));
#250432=CARTESIAN_POINT('Ctrl Pts',(-3.20643327838788,-0.34333729478466,
7.33006542802909));
#250433=CARTESIAN_POINT('Ctrl Pts',(-3.21878910424195,-0.170429634894116,
7.31867179497308));
#250434=CARTESIAN_POINT('Ctrl Pts',(-3.2213848981587,-0.111040043629163,
7.31481799965721));
#250435=CARTESIAN_POINT('Ctrl Pts',(-3.22261223720652,-0.034407617749416,
7.30994969608496));
#250436=CARTESIAN_POINT('Ctrl Pts',(-3.22275,-0.017204164504275,7.30886358410991));
#250437=CARTESIAN_POINT('Ctrl Pts',(-3.22275,-3.49632484551545E-13,7.3077847617826));
#250438=CARTESIAN_POINT('',(-3.2227498657163,0.000930336277219642,8.31709040082309));
#250439=CARTESIAN_POINT('Ctrl Pts',(-3.22275,-1.40828092660302E-10,7.06317491433944));
#250440=CARTESIAN_POINT('Ctrl Pts',(-3.22274999999996,-0.000953531021211235,
7.06323882613367));
#250441=CARTESIAN_POINT('Ctrl Pts',(-3.22274957684046,-0.00190706973096647,
7.06330274445318));
#250442=CARTESIAN_POINT('Ctrl Pts',(-3.22252667574421,-0.253025888032566,
7.08013750826466));
#250443=CARTESIAN_POINT('Ctrl Pts',(-3.19317800943748,-0.502316457797773,
7.09734588176947));
#250444=CARTESIAN_POINT('Ctrl Pts',(-3.12848874678906,-0.774299356712258,
7.11534388989034));
#250445=CARTESIAN_POINT('Ctrl Pts',(-3.12129716478292,-0.802798530885497,
7.11721890539666));
#250446=CARTESIAN_POINT('Ctrl Pts',(-3.11029875201956,-0.843999306421481,
7.11990987998768));
#250447=CARTESIAN_POINT('Ctrl Pts',(-3.10680207164883,-0.856781219402947,
7.12074194229381));
#250448=CARTESIAN_POINT('Ctrl Pts',(-3.10047035227186,-0.879377910673626,
7.12220755478895));
#250449=CARTESIAN_POINT('Ctrl Pts',(-3.09766735274477,-0.889201269152986,
7.12284287059426));
#250450=CARTESIAN_POINT('Ctrl Pts',(-3.09149385174459,-0.910453342516979,
7.12421328294044));
#250451=CARTESIAN_POINT('Ctrl Pts',(-3.08810664465587,-0.921876827985553,
7.12494742284139));
#250452=CARTESIAN_POINT('Ctrl Pts',(-3.0783171371103,-0.954232837354177,
7.12702042462482));
#250453=CARTESIAN_POINT('Ctrl Pts',(-3.07176468743532,-0.975119720127279,
7.12835100955111));
#250454=CARTESIAN_POINT('Ctrl Pts',(-3.01956137922603,-1.13577529114735,
7.13853817107374));
#250455=CARTESIAN_POINT('Ctrl Pts',(-2.96460066690011,-1.27235597560013,
7.14692538665781));
#250456=CARTESIAN_POINT('Ctrl Pts',(-2.79473371201036,-1.62310125157332,
7.16887031409096));
#250457=CARTESIAN_POINT('Ctrl Pts',(-2.66465457994802,-1.82882605445227,
7.18222979907216));
#250458=CARTESIAN_POINT('Ctrl Pts',(-2.47306894240764,-2.06737950812083,
7.20012497136034));
#250459=CARTESIAN_POINT('Ctrl Pts',(-2.43196980713013,-2.11557323232554,
7.20387671620316));
#250460=CARTESIAN_POINT('Ctrl Pts',(-2.37177528277691,-2.1820851722432,
7.20927231248871));
#250461=CARTESIAN_POINT('Ctrl Pts',(-2.35383183267888,-2.20142892953185,
7.21086886501484));
#250462=CARTESIAN_POINT('Ctrl Pts',(-2.32291506054037,-2.23394829102413,
7.21360118899848));
#250463=CARTESIAN_POINT('Ctrl Pts',(-2.31006198716238,-2.247236734024,7.21473181114377));
#250464=CARTESIAN_POINT('Ctrl Pts',(-2.28372809017572,-2.27399797588429,
7.2170380665918));
#250465=CARTESIAN_POINT('Ctrl Pts',(-2.27024067857951,-2.28746322830508,
7.2182139641804));
#250466=CARTESIAN_POINT('Ctrl Pts',(-2.23640142187085,-2.32065280846793,
7.22115166885254));
#250467=CARTESIAN_POINT('Ctrl Pts',(-2.21590762943885,-2.34022949159859,
7.22291974101126));
#250468=CARTESIAN_POINT('Ctrl Pts',(-2.1345712645501,-2.41589965578216,
7.22989594846167));
#250469=CARTESIAN_POINT('Ctrl Pts',(-2.07183995967479,-2.46990745824362,
7.23518948900365));
#250470=CARTESIAN_POINT('Ctrl Pts',(-1.89821176174216,-2.6081182311143,
7.24962050550192));
#250471=CARTESIAN_POINT('Ctrl Pts',(-1.78382851108215,-2.68764540471774,
7.25890820220459));
#250472=CARTESIAN_POINT('Ctrl Pts',(-1.4784990665978,-2.87183437263658,
7.28294502815948));
#250473=CARTESIAN_POINT('Ctrl Pts',(-1.2814257099444,-2.9650215208448,7.29779139859344));
#250474=CARTESIAN_POINT('Ctrl Pts',(-1.05051036632447,-3.04685139884914,
7.31353556825694));
#250475=CARTESIAN_POINT('Ctrl Pts',(-1.02444351974757,-3.05571449371794,
7.31528959362654));
#250476=CARTESIAN_POINT('Ctrl Pts',(-0.985858828249833,-3.06828456802298,
7.31784856597426));
#250477=CARTESIAN_POINT('Ctrl Pts',(-0.973427648319938,-3.07225103902177,
7.31866734137015));
#250478=CARTESIAN_POINT('Ctrl Pts',(-0.951255076351548,-3.07917764757313,
7.32011722518384));
#250479=CARTESIAN_POINT('Ctrl Pts',(-0.941523369377431,-3.08216725036393,
7.320749977743));
#250480=CARTESIAN_POINT('Ctrl Pts',(-0.920074233389323,-3.08864540227538,
7.32213662497717));
#250481=CARTESIAN_POINT('Ctrl Pts',(-0.908350998171864,-3.09211343441985,
7.32288935143317));
#250482=CARTESIAN_POINT('Ctrl Pts',(-0.874158532188023,-3.10201719657204,
7.32507054937929));
#250483=CARTESIAN_POINT('Ctrl Pts',(-0.851638166658515,-3.10827545939235,
7.32648932645618));
#250484=CARTESIAN_POINT('Ctrl Pts',(-0.799733764438047,-3.12209286827458,
7.32972262549627));
#250485=CARTESIAN_POINT('Ctrl Pts',(-0.770306742007576,-3.12948328439213,
7.3315289356792));
#250486=CARTESIAN_POINT('Ctrl Pts',(-0.669920195412353,-3.15319290622601,
7.33761364473023));
#250487=CARTESIAN_POINT('Ctrl Pts',(-0.598510540842762,-3.16752347483356,
7.34181174390286));
#250488=CARTESIAN_POINT('Ctrl Pts',(-0.389881453923603,-3.2020829695681,
7.35385548295524));
#250489=CARTESIAN_POINT('Ctrl Pts',(-0.25176649684484,-3.21589161607035,
7.36155891000548));
#250490=CARTESIAN_POINT('Ctrl Pts',(0.0762458684478214,-3.22741904230161,
7.37997732319351));
#250491=CARTESIAN_POINT('Ctrl Pts',(0.265874385737307,-3.21735072640884,
7.39074018283069));
#250492=CARTESIAN_POINT('Ctrl Pts',(0.488429866184755,-3.18571782468613,
7.4041434806085));
#250493=CARTESIAN_POINT('Ctrl Pts',(0.523267593151709,-3.18018123271999,
7.40626331180025));
#250494=CARTESIAN_POINT('Ctrl Pts',(0.578427575455487,-3.17048403462823,
7.40965752330677));
#250495=CARTESIAN_POINT('Ctrl Pts',(0.598813211306928,-3.1666970459578,
7.410920172178));
#250496=CARTESIAN_POINT('Ctrl Pts',(0.636769659202039,-3.15926635933357,
7.41328713759469));
#250497=CARTESIAN_POINT('Ctrl Pts',(0.65434940807425,-3.15567209319773,
7.41438985162708));
#250498=CARTESIAN_POINT('Ctrl Pts',(0.6938733381964,-3.14724676745014,7.41688397564538));
#250499=CARTESIAN_POINT('Ctrl Pts',(0.715798677445564,-3.14233267453331,
7.4182779722957));
#250500=CARTESIAN_POINT('Ctrl Pts',(0.781176479613671,-3.1269599133044,
7.42246668111982));
#250501=CARTESIAN_POINT('Ctrl Pts',(0.824463200142806,-3.11582655244611,
7.42528262080311));
#250502=CARTESIAN_POINT('Ctrl Pts',(1.03077672987471,-3.05816248832955,
7.43891504761489));
#250503=CARTESIAN_POINT('Ctrl Pts',(1.19017244796175,-2.99972224575463,
7.45010483838697));
#250504=CARTESIAN_POINT('Ctrl Pts',(1.51127630516548,-2.85235859203769,
7.47384509830776));
#250505=CARTESIAN_POINT('Ctrl Pts',(1.67147305428396,-2.76153673095869,
7.48638887995182));
#250506=CARTESIAN_POINT('Ctrl Pts',(1.88103229076042,-2.61778116730715,
7.50319070730147));
#250507=CARTESIAN_POINT('Ctrl Pts',(1.93769720796257,-2.57611952190976,
7.50777470461426));
#250508=CARTESIAN_POINT('Ctrl Pts',(2.00796130262482,-2.52082793241392,
7.51346757119507));
#250509=CARTESIAN_POINT('Ctrl Pts',(2.02285998857198,-2.508888113294,7.51467517446767));
#250510=CARTESIAN_POINT('Ctrl Pts',(2.0464144284822,-2.48966533167798,7.51658397811625));
#250511=CARTESIAN_POINT('Ctrl Pts',(2.05513921155751,-2.48246818853482,
7.51729093068752));
#250512=CARTESIAN_POINT('Ctrl Pts',(2.07179820249049,-2.46857803388579,
7.51864031065389));
#250513=CARTESIAN_POINT('Ctrl Pts',(2.07973815675831,-2.46189246370422,
7.51928320698627));
#250514=CARTESIAN_POINT('Ctrl Pts',(2.09880883259322,-2.4456765443024,7.52082709621985));
#250515=CARTESIAN_POINT('Ctrl Pts',(2.10990727635468,-2.43610828559084,
7.52172538501965));
#250516=CARTESIAN_POINT('Ctrl Pts',(2.14872163446305,-2.40218117126878,
7.52486783570805));
#250517=CARTESIAN_POINT('Ctrl Pts',(2.17608519410062,-2.37742140323437,
7.52708482535148));
#250518=CARTESIAN_POINT('Ctrl Pts',(2.24365136050259,-2.31414031090584,
7.53258111318452));
#250519=CARTESIAN_POINT('Ctrl Pts',(2.28329325135337,-2.27503612817723,
7.53582627075722));
#250520=CARTESIAN_POINT('Ctrl Pts',(2.47047641003316,-2.08056794131524,
7.55136765110232));
#250521=CARTESIAN_POINT('Ctrl Pts',(2.60329314780584,-1.91177701701462,
7.56311296168481));
#250522=CARTESIAN_POINT('Ctrl Pts',(2.79560838319224,-1.60977108245903,
7.58338124441627));
#250523=CARTESIAN_POINT('Ctrl Pts',(2.8646252263604,-1.4834772091751,7.59166208358882));
#250524=CARTESIAN_POINT('Ctrl Pts',(2.93941389977534,-1.32179651252657,
7.60229532830778));
#250525=CARTESIAN_POINT('Ctrl Pts',(2.95335009669646,-1.29035776648659,
7.60436383352325));
#250526=CARTESIAN_POINT('Ctrl Pts',(2.97472618599645,-1.23997402839485,
7.60768312632876));
#250527=CARTESIAN_POINT('Ctrl Pts',(2.98249453471051,-1.22117066533209,
7.60892282881088));
#250528=CARTESIAN_POINT('Ctrl Pts',(2.99686358167087,-1.18543513607,7.61128120822325));
#250529=CARTESIAN_POINT('Ctrl Pts',(3.00350013180096,-1.16851817528474,
7.61239863186569));
#250530=CARTESIAN_POINT('Ctrl Pts',(3.01826877967523,-1.12991483776668,
7.61495115998175));
#250531=CARTESIAN_POINT('Ctrl Pts',(3.02631080756419,-1.10819529799116,
7.61638918387486));
#250532=CARTESIAN_POINT('Ctrl Pts',(3.05040461772171,-1.04090513018184,
7.62085109799654));
#250533=CARTESIAN_POINT('Ctrl Pts',(3.06566568951295,-0.995060450743638,
7.62390053770755));
#250534=CARTESIAN_POINT('Ctrl Pts',(3.09889604482007,-0.887202190439704,
7.63110036182815));
#250535=CARTESIAN_POINT('Ctrl Pts',(3.11604338271559,-0.824958890782594,
7.63527477672648));
#250536=CARTESIAN_POINT('Ctrl Pts',(3.17448469572475,-0.584881724674091,
7.65144422524452));
#250537=CARTESIAN_POINT('Ctrl Pts',(3.20250882890306,-0.404184540027611,
7.66378062337057));
#250538=CARTESIAN_POINT('Ctrl Pts',(3.21744807614554,-0.187933170835252,
7.67842265555932));
#250539=CARTESIAN_POINT('Ctrl Pts',(3.21926391396761,-0.153723414628061,
7.68073442698605));
#250540=CARTESIAN_POINT('Ctrl Pts',(3.22540421270944,0.011770606368995,
7.69188158034767));
#250541=CARTESIAN_POINT('Ctrl Pts',(3.22224543175025,0.143221596182795,
7.70063001977925));
#250542=CARTESIAN_POINT('Ctrl Pts',(3.20922025119336,0.295797348931664,
7.71041462621891));
#250543=CARTESIAN_POINT('Ctrl Pts',(3.20715065436056,0.317451463312989,
7.71179443564843));
#250544=CARTESIAN_POINT('Ctrl Pts',(3.20359748639591,0.351034366725555,
7.71391888795789));
#250545=CARTESIAN_POINT('Ctrl Pts',(3.2022662042726,0.36297816636175,7.71467140810044));
#250546=CARTESIAN_POINT('Ctrl Pts',(3.19968137894554,0.385046360134685,
7.71605583801941));
#250547=CARTESIAN_POINT('Ctrl Pts',(3.19844657043142,0.39517232479427,7.71668871137639));
#250548=CARTESIAN_POINT('Ctrl Pts',(3.19548774346559,0.418513120822464,
7.71814219877517));
#250549=CARTESIAN_POINT('Ctrl Pts',(3.19372981958098,0.43172329659818,7.71896093402771));
#250550=CARTESIAN_POINT('Ctrl Pts',(3.18788332209423,0.473666283547361,
7.72154915400199));
#250551=CARTESIAN_POINT('Ctrl Pts',(3.18348843220928,0.502355807066949,
7.72330264217801));
#250552=CARTESIAN_POINT('Ctrl Pts',(3.15763268848809,0.65714003809271,7.73269038443449));
#250553=CARTESIAN_POINT('Ctrl Pts',(3.12906495024704,0.781944007393687,
7.74000090212326));
#250554=CARTESIAN_POINT('Ctrl Pts',(3.03045907033571,1.11906415631442,7.75981227087039));
#250555=CARTESIAN_POINT('Ctrl Pts',(2.94566356999454,1.32629213034917,7.77210337978645));
#250556=CARTESIAN_POINT('Ctrl Pts',(2.80057662288507,1.59683788075037,7.78986826591017));
#250557=CARTESIAN_POINT('Ctrl Pts',(2.75817217270412,1.66901324411107,7.79478618283662));
#250558=CARTESIAN_POINT('Ctrl Pts',(2.69716364558812,1.76416772331911,7.8015639503566));
#250559=CARTESIAN_POINT('Ctrl Pts',(2.68098103807282,1.7886643271088,7.80333615005662));
#250560=CARTESIAN_POINT('Ctrl Pts',(2.65362672810704,1.82886687516966,7.80629205124987));
#250561=CARTESIAN_POINT('Ctrl Pts',(2.64264457704182,1.8447001039809,7.80746864681965));
#250562=CARTESIAN_POINT('Ctrl Pts',(2.62080866357975,1.87558627476477,7.80978894519906));
#250563=CARTESIAN_POINT('Ctrl Pts',(2.60996555108171,1.89064584854694,7.81093221371985));
#250564=CARTESIAN_POINT('Ctrl Pts',(2.58376827185787,1.9263753654588,7.81367377419666));
#250565=CARTESIAN_POINT('Ctrl Pts',(2.56829544621929,1.94695633516277,7.81527659596907));
#250566=CARTESIAN_POINT('Ctrl Pts',(2.51374689442721,2.01773148391793,7.82087250912876));
#250567=CARTESIAN_POINT('Ctrl Pts',(2.4734350008627,2.06694997067148,7.82491352971956));
#250568=CARTESIAN_POINT('Ctrl Pts',(2.37009912950556,2.18576244655493,7.83505232600325));
#250569=CARTESIAN_POINT('Ctrl Pts',(2.30544310935422,2.25385379931654,7.84121025381088));
#250570=CARTESIAN_POINT('Ctrl Pts',(2.09233171637936,2.45951143799465,7.86090430607929));
#250571=CARTESIAN_POINT('Ctrl Pts',(1.93385504188494,2.58597116265882,7.87472963515643));
#250572=CARTESIAN_POINT('Ctrl Pts',(1.68386946247264,2.7495460470864,7.89467715365666));
#250573=CARTESIAN_POINT('Ctrl Pts',(1.60082542433281,2.79871064388989,7.90102822078808));
#250574=CARTESIAN_POINT('Ctrl Pts',(1.49750579643703,2.85377271521622,7.90849892163109));
#250575=CARTESIAN_POINT('Ctrl Pts',(1.47922464601704,2.86329125617286,7.90980490324973));
#250576=CARTESIAN_POINT('Ctrl Pts',(1.45036934892486,2.87796536499773,7.91184002374966));
#250577=CARTESIAN_POINT('Ctrl Pts',(1.4398564929783,2.88323935534855,7.91257606088977));
#250578=CARTESIAN_POINT('Ctrl Pts',(1.42105597551721,2.892542547139,7.91388239035409));
#250579=CARTESIAN_POINT('Ctrl Pts',(1.41277984433935,2.89659379039281,7.9144540016309));
#250580=CARTESIAN_POINT('Ctrl Pts',(1.3926808113147,2.9063258180604,7.91583399916982));
#250581=CARTESIAN_POINT('Ctrl Pts',(1.38084046441022,2.91196999100449,7.91664015324996));
#250582=CARTESIAN_POINT('Ctrl Pts',(1.34371569676275,2.92938963344834,7.91914760981549));
#250583=CARTESIAN_POINT('Ctrl Pts',(1.31831194088421,2.94090959437336,7.9208342912058));
#250584=CARTESIAN_POINT('Ctrl Pts',(1.18520068270418,2.99920067592472,7.92953755341671));
#250585=CARTESIAN_POINT('Ctrl Pts',(1.07513550448367,3.04039379387161,7.93628017357476));
#250586=CARTESIAN_POINT('Ctrl Pts',(0.765188682659938,3.13745040137833,
7.95465491746747));
#250587=CARTESIAN_POINT('Ctrl Pts',(0.561806150291263,3.18017034454195,
7.96606317156575));
#250588=CARTESIAN_POINT('Ctrl Pts',(0.249979193514176,3.21480150336395,
7.98403903669595));
#250589=CARTESIAN_POINT('Ctrl Pts',(0.143722608692009,3.22130080726887,
7.99024087744728));
#250590=CARTESIAN_POINT('Ctrl Pts',(0.00533877931180301,3.22290453713602,
7.99851876314798));
#250591=CARTESIAN_POINT('Ctrl Pts',(-0.026671224341357,3.22279858102165,
8.00044724962345));
#250592=CARTESIAN_POINT('Ctrl Pts',(-0.0785034403496282,3.22185476535973,
8.00359448381885));
#250593=CARTESIAN_POINT('Ctrl Pts',(-0.0983292668588446,3.22131064122808,
8.00480411159918));
#250594=CARTESIAN_POINT('Ctrl Pts',(-0.136436719884786,3.21991265318188,
8.00714086505246));
#250595=CARTESIAN_POINT('Ctrl Pts',(-0.154718616741983,3.21908598837162,
8.00826710166205));
#250596=CARTESIAN_POINT('Ctrl Pts',(-0.197129678575149,3.21680614185889,
8.01089226172787));
#250597=CARTESIAN_POINT('Ctrl Pts',(-0.22125126416158,3.21523711286866,
8.01239472401419));
#250598=CARTESIAN_POINT('Ctrl Pts',(-0.299132884207038,3.20929061968452,
8.01727714353183));
#250599=CARTESIAN_POINT('Ctrl Pts',(-0.352799033073016,3.20383505348674,
8.02069010004052));
#250600=CARTESIAN_POINT('Ctrl Pts',(-0.574938912025167,3.17560403984677,
8.03502657847184));
#250601=CARTESIAN_POINT('Ctrl Pts',(-0.741595117827573,3.14086590443657,
8.04630413137959));
#250602=CARTESIAN_POINT('Ctrl Pts',(-1.10451230971558,3.03471649314292,
8.07176760297457));
#250603=CARTESIAN_POINT('Ctrl Pts',(-1.29818488725824,2.95705522506851,
8.08598731440934));
#250604=CARTESIAN_POINT('Ctrl Pts',(-1.51762072480884,2.84331914133104,
8.10203333711949));
#250605=CARTESIAN_POINT('Ctrl Pts',(-1.55189513614819,2.82475807771813,
8.1045363500097));
#250606=CARTESIAN_POINT('Ctrl Pts',(-1.59923252330628,2.79800108208885,
8.10798014180331));
#250607=CARTESIAN_POINT('Ctrl Pts',(-1.6125847848581,2.7903270511897,8.10895002319282));
#250608=CARTESIAN_POINT('Ctrl Pts',(-1.63487157423647,2.77730461163928,
8.11056571734811));
#250609=CARTESIAN_POINT('Ctrl Pts',(-1.64383601835097,2.77200813954035,
8.11121472862217));
#250610=CARTESIAN_POINT('Ctrl Pts',(-1.66223068520974,2.76101938291241,
8.11254443670403));
#250611=CARTESIAN_POINT('Ctrl Pts',(-1.67165763788342,2.75532205627298,
8.1132248038879));
#250612=CARTESIAN_POINT('Ctrl Pts',(-1.69619746179007,2.74031872619947,
8.11499356254984));
#250613=CARTESIAN_POINT('Ctrl Pts',(-1.71126322378803,2.73093587657025,
8.11607712205303));
#250614=CARTESIAN_POINT('Ctrl Pts',(-1.77904317078882,2.68794184081215,
8.12094499398641));
#250615=CARTESIAN_POINT('Ctrl Pts',(-1.83085350028505,2.65292339059457,
8.12464672371816));
#250616=CARTESIAN_POINT('Ctrl Pts',(-1.98159942387934,2.54451335474954,
8.13546178023975));
#250617=CARTESIAN_POINT('Ctrl Pts',(-2.07738621806542,2.46693230739397,
8.14239587285383));
#250618=CARTESIAN_POINT('Ctrl Pts',(-2.34756303679599,2.22118324286179,
8.16286947326698));
#250619=CARTESIAN_POINT('Ctrl Pts',(-2.5076863413829,2.03867691820129,8.17631869411077));
#250620=CARTESIAN_POINT('Ctrl Pts',(-2.66840353093015,1.80756694530306,
8.19299932844885));
#250621=CARTESIAN_POINT('Ctrl Pts',(-2.69034180387487,1.7747496851045,8.19535857054753));
#250622=CARTESIAN_POINT('Ctrl Pts',(-2.72438899974833,1.72173633918532,
8.19915977865434));
#250623=CARTESIAN_POINT('Ctrl Pts',(-2.73688931883192,1.70179559739131,
8.20058738564981));
#250624=CARTESIAN_POINT('Ctrl Pts',(-2.75870241643252,1.66613692289908,
8.20313731398124));
#250625=CARTESIAN_POINT('Ctrl Pts',(-2.7681021378251,1.65047320528892,8.204256415402));
#250626=CARTESIAN_POINT('Ctrl Pts',(-2.78748208481103,1.61754714210972,
8.20660717254968));
#250627=CARTESIAN_POINT('Ctrl Pts',(-2.79743626019383,1.60027043712824,
8.20783970293279));
#250628=CARTESIAN_POINT('Ctrl Pts',(-2.8231929920192,1.55459166685591,8.21109655724054));
#250629=CARTESIAN_POINT('Ctrl Pts',(-2.83872700187022,1.52604154813008,
8.21313026720772));
#250630=CARTESIAN_POINT('Ctrl Pts',(-2.91338552114394,1.38374019643407,
8.22326073650538));
#250631=CARTESIAN_POINT('Ctrl Pts',(-2.96611117523795,1.26677925994366,
8.23157495481695));
#250632=CARTESIAN_POINT('Ctrl Pts',(-3.10551114465178,0.900751112335599,
8.25751308038769));
#250633=CARTESIAN_POINT('Ctrl Pts',(-3.1687325277635,0.643951241439419,
8.2756831860355));
#250634=CARTESIAN_POINT('Ctrl Pts',(-3.20664551714391,0.326632590981115,
8.29666089333697));
#250635=CARTESIAN_POINT('Ctrl Pts',(-3.21184552326581,0.270764653685991,
8.30029561595211));
#250636=CARTESIAN_POINT('Ctrl Pts',(-3.21676311648958,0.197142798860358,
8.30498476996007));
#250637=CARTESIAN_POINT('Ctrl Pts',(-3.21779639937825,0.179489820271894,
8.30610153431829));
#250638=CARTESIAN_POINT('Ctrl Pts',(-3.2192367304144,0.150842437076011,
8.30790055094247));
#250639=CARTESIAN_POINT('Ctrl Pts',(-3.21973285729915,0.13985314914494,
8.30858749710112));
#250640=CARTESIAN_POINT('Ctrl Pts',(-3.220556688238,0.119266076445391,8.30986820628513));
#250641=CARTESIAN_POINT('Ctrl Pts',(-3.22089777452835,0.109669083833807,
8.31046268952154));
#250642=CARTESIAN_POINT('Ctrl Pts',(-3.22152144770192,0.0895935262464321,
8.31170120631046));
#250643=CARTESIAN_POINT('Ctrl Pts',(-3.22179581953792,0.0791147401977138,
8.31234479286206));
#250644=CARTESIAN_POINT('Ctrl Pts',(-3.22249972328521,0.0460703270001148,
8.31436576064609));
#250645=CARTESIAN_POINT('Ctrl Pts',(-3.22274335007289,0.0235009802904541,
8.31573350607326));
#250646=CARTESIAN_POINT('Ctrl Pts',(-3.2227498657163,0.000930336277219642,
8.31709040082309));
#250647=CARTESIAN_POINT('Ctrl Pts',(-3.22274986493329,0.000933044715058097,
8.31709023799804));
#250648=CARTESIAN_POINT('Ctrl Pts',(-3.22274995497795,0.000622029195259805,
8.31710893554152));
#250649=CARTESIAN_POINT('Ctrl Pts',(-3.22275,0.000311014285896028,8.31712763097307));
#250650=CARTESIAN_POINT('Ctrl Pts',(-3.22275,-3.27109834657983E-12,8.3171463242964));
#250651=CARTESIAN_POINT('Origin',(0.,0.,-2.31077344927308));
#250652=CARTESIAN_POINT('',(-3.22275,1.94885615773067E-11,9.8126895994942));
#250653=CARTESIAN_POINT('',(-3.22275,-1.85372951893938E-11,9.562284768011));
#250654=CARTESIAN_POINT('',(-3.22275,-3.50678552687464E-13,-2.31077344927308));
#250655=CARTESIAN_POINT('Ctrl Pts',(-3.22275,1.94885615773067E-11,9.8126895994942));
#250656=CARTESIAN_POINT('Ctrl Pts',(-3.22275000000001,0.0988455592422595,
9.80700803712948));
#250657=CARTESIAN_POINT('Ctrl Pts',(-3.2182025068033,0.197631261900894,
9.80122982269705));
#250658=CARTESIAN_POINT('Ctrl Pts',(-3.20630297517147,0.326621490038495,
9.79347359146827));
#250659=CARTESIAN_POINT('Ctrl Pts',(-3.20304561883108,0.357154073828275,
9.79162224555709));
#250660=CARTESIAN_POINT('Ctrl Pts',(-3.19703483776758,0.406764205710066,
9.78858696404115));
#250661=CARTESIAN_POINT('Ctrl Pts',(-3.19454561689965,0.425872222001901,
9.78741130405184));
#250662=CARTESIAN_POINT('Ctrl Pts',(-3.18940869268016,0.462721833992583,
9.78513084305691));
#250663=CARTESIAN_POINT('Ctrl Pts',(-3.18678392163908,0.48046594140659,
9.78402680124839));
#250664=CARTESIAN_POINT('Ctrl Pts',(-3.18031406131337,0.521816097999275,
9.78143971545899));
#250665=CARTESIAN_POINT('Ctrl Pts',(-3.1763540817414,0.545402848367702,
9.77995311094355));
#250666=CARTESIAN_POINT('Ctrl Pts',(-3.16254898397611,0.622372957546348,
9.77506519345983));
#250667=CARTESIAN_POINT('Ctrl Pts',(-3.15161804072738,0.67554965144936,
9.77163010674489));
#250668=CARTESIAN_POINT('Ctrl Pts',(-3.09780676148598,0.907465109565107,
9.75638515759688));
#250669=CARTESIAN_POINT('Ctrl Pts',(-3.04102895179079,1.08260123155504,
9.74415192581572));
#250670=CARTESIAN_POINT('Ctrl Pts',(-2.88757695506529,1.4466001183839,9.7175019958554));
#250671=CARTESIAN_POINT('Ctrl Pts',(-2.78655674024109,1.63274813349019,
9.70309232820139));
#250672=CARTESIAN_POINT('Ctrl Pts',(-2.65236925050841,1.8308017671199,9.68771144179242));
#250673=CARTESIAN_POINT('Ctrl Pts',(-2.63640136263731,1.85372212793734,
9.68593126357213));
#250674=CARTESIAN_POINT('Ctrl Pts',(-2.61267422313975,1.88685326473907,
9.68336113089466));
#250675=CARTESIAN_POINT('Ctrl Pts',(-2.60514931133334,1.8972292738479,9.68255666878094));
#250676=CARTESIAN_POINT('Ctrl Pts',(-2.59165831078906,1.91560023568649,
9.68113356184292));
#250677=CARTESIAN_POINT('Ctrl Pts',(-2.58571675236563,1.92361273352193,
9.6805133096404));
#250678=CARTESIAN_POINT('Ctrl Pts',(-2.57271125440297,1.94098217466305,
9.67916975010088));
#250679=CARTESIAN_POINT('Ctrl Pts',(-2.56563339080009,1.95032825824069,
9.67844741117817));
#250680=CARTESIAN_POINT('Ctrl Pts',(-2.54529170059245,1.97688641270331,
9.67639584299928));
#250681=CARTESIAN_POINT('Ctrl Pts',(-2.53190430697451,1.9940036028236,9.67507484700015));
#250682=CARTESIAN_POINT('Ctrl Pts',(-2.42077112882318,2.13317504015373,
9.6643329567526));
#250683=CARTESIAN_POINT('Ctrl Pts',(-2.31442123982545,2.24811813168069,
9.65544607699868));
#250684=CARTESIAN_POINT('Ctrl Pts',(-2.00270714973908,2.53934651246845,
9.631469873342));
#250685=CARTESIAN_POINT('Ctrl Pts',(-1.78289263874554,2.69822140564367,
9.61657741837827));
#250686=CARTESIAN_POINT('Ctrl Pts',(-1.51392323977047,2.84525516848052,
9.59836858928018));
#250687=CARTESIAN_POINT('Ctrl Pts',(-1.48171570208415,2.86215984359172,
9.5961905311965));
#250688=CARTESIAN_POINT('Ctrl Pts',(-1.42901915174892,2.88869067889221,
9.59262689870506));
#250689=CARTESIAN_POINT('Ctrl Pts',(-1.40870222749015,2.89865271611693,
9.59125296878732));
#250690=CARTESIAN_POINT('Ctrl Pts',(-1.37224796508273,2.91605362973353,
9.5887869699881));
#250691=CARTESIAN_POINT('Ctrl Pts',(-1.35615069564134,2.92357461338874,
9.58769778052999));
#250692=CARTESIAN_POINT('Ctrl Pts',(-1.32189634464499,2.9392351941097,9.58537907583011));
#250693=CARTESIAN_POINT('Ctrl Pts',(-1.30372448298975,2.94734048195089,
9.58414844544484));
#250694=CARTESIAN_POINT('Ctrl Pts',(-1.2546483645017,2.96868749125039,9.58082285331471));
#250695=CARTESIAN_POINT('Ctrl Pts',(-1.22361068629477,2.98161444375182,
9.57871740537086));
#250696=CARTESIAN_POINT('Ctrl Pts',(-1.0474640628348,3.05176458483243,9.56675218123542));
#250697=CARTESIAN_POINT('Ctrl Pts',(-0.898572803182584,3.09887122066553,
9.55656164640332));
#250698=CARTESIAN_POINT('Ctrl Pts',(-0.55731968604107,3.18017025270206,
9.53314049461768));
#250699=CARTESIAN_POINT('Ctrl Pts',(-0.364067801303678,3.20804289941476,
9.51982352382647));
#250700=CARTESIAN_POINT('Ctrl Pts',(-0.0796188710241167,3.22302294678228,
9.50084331376008));
#250701=CARTESIAN_POINT('Ctrl Pts',(0.0104157261899073,3.22398984660574,
9.49493146995976));
#250702=CARTESIAN_POINT('Ctrl Pts',(0.120376080726387,3.22056320967653,
9.48791577458799));
#250703=CARTESIAN_POINT('Ctrl Pts',(0.14036637062032,3.21975389072774,9.48664867002654));
#250704=CARTESIAN_POINT('Ctrl Pts',(0.171805118165219,3.21818771143488,
9.48467032874919));
#250705=CARTESIAN_POINT('Ctrl Pts',(0.183258915773735,3.21755579965851,
9.48395259504536));
#250706=CARTESIAN_POINT('Ctrl Pts',(0.203704893531968,3.21631825166988,
9.48267706338429));
#250707=CARTESIAN_POINT('Ctrl Pts',(0.212697958220273,3.21573605268973,
9.48211801902361));
#250708=CARTESIAN_POINT('Ctrl Pts',(0.234494493502573,3.2142331372408,9.48076775717731));
#250709=CARTESIAN_POINT('Ctrl Pts',(0.247295051528603,3.21327364200759,
9.47997868497144));
#250710=CARTESIAN_POINT('Ctrl Pts',(0.28729954156046,3.21003454195876,9.47752392439355));
#250711=CARTESIAN_POINT('Ctrl Pts',(0.314481222292297,3.20748569112191,
9.47587229132811));
#250712=CARTESIAN_POINT('Ctrl Pts',(0.455304734749,3.19247308035518,9.46738497841751));
#250713=CARTESIAN_POINT('Ctrl Pts',(0.568267527192083,3.17431313740642,
9.46081067071436));
#250714=CARTESIAN_POINT('Ctrl Pts',(0.879128161140997,3.10720712283164,
9.44280178780318));
#250715=CARTESIAN_POINT('Ctrl Pts',(1.0736954260329,3.04545269958723,9.43159872471844));
#250716=CARTESIAN_POINT('Ctrl Pts',(1.36628520308246,2.92103375962386,9.41343258892693));
#250717=CARTESIAN_POINT('Ctrl Pts',(1.46897386430393,2.87076389857998,9.4067876065458));
#250718=CARTESIAN_POINT('Ctrl Pts',(1.59676178100323,2.79955286305026,9.39803890016618));
#250719=CARTESIAN_POINT('Ctrl Pts',(1.62451852171566,2.78353801489366,9.39610858633339));
#250720=CARTESIAN_POINT('Ctrl Pts',(1.66882380695965,2.75708671819037,9.39297634651653));
#250721=CARTESIAN_POINT('Ctrl Pts',(1.68552459252708,2.74690860644417,9.39178374103354));
#250722=CARTESIAN_POINT('Ctrl Pts',(1.71728367895618,2.72715469715855,9.38949239513758));
#250723=CARTESIAN_POINT('Ctrl Pts',(1.73235715279015,2.71760457962975,9.38839462392593));
#250724=CARTESIAN_POINT('Ctrl Pts',(1.76689871767813,2.69531588841356,9.38585488886143));
#250725=CARTESIAN_POINT('Ctrl Pts',(1.78630954568023,2.68249081614156,9.38440975817567));
#250726=CARTESIAN_POINT('Ctrl Pts',(1.84745482341426,2.64113309571356,9.37979932842482));
#250727=CARTESIAN_POINT('Ctrl Pts',(1.88865594263913,2.61182917206897,9.37660535448691));
#250728=CARTESIAN_POINT('Ctrl Pts',(2.15473551380437,2.41299388028354,9.35538504743334));
#250729=CARTESIAN_POINT('Ctrl Pts',(2.35722230946593,2.21559744462313,9.33622980504371));
#250730=CARTESIAN_POINT('Ctrl Pts',(2.6113610568486,1.89303621417104,9.30859599707018));
#250731=CARTESIAN_POINT('Ctrl Pts',(2.68511740468086,1.78688112523138,9.30000155340758));
#250732=CARTESIAN_POINT('Ctrl Pts',(2.76344644622969,1.65829416762707,9.29038373695233));
#250733=CARTESIAN_POINT('Ctrl Pts',(2.77440078311683,1.6399012649188,9.28902611191978));
#250734=CARTESIAN_POINT('Ctrl Pts',(2.79110082028487,1.61121465780451,9.28693819432081));
#250735=CARTESIAN_POINT('Ctrl Pts',(2.79697446770584,1.60099665825581,9.28620022551655));
#250736=CARTESIAN_POINT('Ctrl Pts',(2.80771206017983,1.58207771734311,9.28484473344258));
#250737=CARTESIAN_POINT('Ctrl Pts',(2.81259173033896,1.57338637306132,9.28422626083309));
#250738=CARTESIAN_POINT('Ctrl Pts',(2.82371655406337,1.55335442880377,9.28281037849427));
#250739=CARTESIAN_POINT('Ctrl Pts',(2.82993377498239,1.54199870350698,9.28201471718869));
#250740=CARTESIAN_POINT('Ctrl Pts',(2.84932674839883,1.50606516650349,9.27951790942258));
#250741=CARTESIAN_POINT('Ctrl Pts',(2.8622524014073,1.48135293336928,9.27783151392644));
#250742=CARTESIAN_POINT('Ctrl Pts',(2.92891205126769,1.34977711604699,9.26899751263772));
#250743=CARTESIAN_POINT('Ctrl Pts',(2.97699165276299,1.24014131050492,9.26213546966041));
#250744=CARTESIAN_POINT('Ctrl Pts',(3.12091495578911,0.854985203175454,
9.23889148732172));
#250745=CARTESIAN_POINT('Ctrl Pts',(3.18543006684272,0.569333836528587,
9.2229749702295));
#250746=CARTESIAN_POINT('Ctrl Pts',(3.21440612881801,0.235765640543175,
9.2031355070566));
#250747=CARTESIAN_POINT('Ctrl Pts',(3.21728332597761,0.19256150800319,9.20054563537087));
#250748=CARTESIAN_POINT('Ctrl Pts',(3.22031710669064,0.127151578323691,
9.19658808703209));
#250749=CARTESIAN_POINT('Ctrl Pts',(3.22111611723109,0.104979584072407,
9.19524027500394));
#250750=CARTESIAN_POINT('Ctrl Pts',(3.22214153330588,0.0650821452169431,
9.19280282531749));
#250751=CARTESIAN_POINT('Ctrl Pts',(3.22245074365331,0.0473595958562845,
9.19171580326542));
#250752=CARTESIAN_POINT('Ctrl Pts',(3.22279926085774,0.00946147154036004,
9.18938172343155));
#250753=CARTESIAN_POINT('Ctrl Pts',(3.22279533689981,-0.0107136497997664,
9.18813336853537));
#250754=CARTESIAN_POINT('Ctrl Pts',(3.2222673539085,-0.0658007884909828,
9.18470836132474));
#250755=CARTESIAN_POINT('Ctrl Pts',(3.22136537290233,-0.100705637038769,
9.18252011643383));
#250756=CARTESIAN_POINT('Ctrl Pts',(3.2117510543864,-0.329023317061161,
9.16808338118603));
#250757=CARTESIAN_POINT('Ctrl Pts',(3.18619300942496,-0.521299454672617,
9.15531103800266));
#250758=CARTESIAN_POINT('Ctrl Pts',(3.10020748318422,-0.901953506429309,
9.12905298927459));
#250759=CARTESIAN_POINT('Ctrl Pts',(3.03939388735818,-1.08944745710421,
9.11561729865114));
#250760=CARTESIAN_POINT('Ctrl Pts',(2.94061627282881,-1.31977246839704,
9.09918724606191));
#250761=CARTESIAN_POINT('Ctrl Pts',(2.91812834531447,-1.36877724630226,
9.09569826990591));
#250762=CARTESIAN_POINT('Ctrl Pts',(2.88685322128073,-1.43265213382302,
9.09118074014602));
#250763=CARTESIAN_POINT('Ctrl Pts',(2.87916244551326,-1.44804602840178,
9.09009437824143));
#250764=CARTESIAN_POINT('Ctrl Pts',(2.86647125687722,-1.47294788337783,
9.08834177604551));
#250765=CARTESIAN_POINT('Ctrl Pts',(2.86154607134036,-1.482493515369,9.08767109393355));
#250766=CARTESIAN_POINT('Ctrl Pts',(2.85179849271435,-1.50115598242906,
9.08636236779632));
#250767=CARTESIAN_POINT('Ctrl Pts',(2.84697992768021,-1.51027455176945,
9.08572412199129));
#250768=CARTESIAN_POINT('Ctrl Pts',(2.83495133138678,-1.53277511922437,
9.08415182683004));
#250769=CARTESIAN_POINT('Ctrl Pts',(2.82769012541347,-1.54612974648939,
9.08322092638036));
#250770=CARTESIAN_POINT('Ctrl Pts',(2.80000523153786,-1.59619965811925,
9.07973751520617));
#250771=CARTESIAN_POINT('Ctrl Pts',(2.7789578252253,-1.63256743313165,9.07722116301177));
#250772=CARTESIAN_POINT('Ctrl Pts',(2.61844777940571,-1.89780864678177,
9.05889344588966));
#250773=CARTESIAN_POINT('Ctrl Pts',(2.45161721041623,-2.10892236171782,
9.04436922798549));
#250774=CARTESIAN_POINT('Ctrl Pts',(2.16031459842974,-2.39560806092738,
9.02121276734335));
#250775=CARTESIAN_POINT('Ctrl Pts',(2.05373667529267,-2.48758040434914,
9.01310302402228));
#250776=CARTESIAN_POINT('Ctrl Pts',(1.9145618044599,-2.5926260471843,9.00269055170905));
#250777=CARTESIAN_POINT('Ctrl Pts',(1.88730554256204,-2.61253409242558,
9.00065971133069));
#250778=CARTESIAN_POINT('Ctrl Pts',(1.8434692722266,-2.64350820527525,8.997403895119));
#250779=CARTESIAN_POINT('Ctrl Pts',(1.82709016275755,-2.65485519352223,
8.99618964122244));
#250780=CARTESIAN_POINT('Ctrl Pts',(1.79591293049383,-2.67602873991179,
8.99388203552029));
#250781=CARTESIAN_POINT('Ctrl Pts',(1.78113668263124,-2.68588629108383,
8.99278990481542));
#250782=CARTESIAN_POINT('Ctrl Pts',(1.7473930736956,-2.70799646845851,8.99029897044064));
#250783=CARTESIAN_POINT('Ctrl Pts',(1.72837707138401,-2.72017280425203,
8.98889740911024));
#250784=CARTESIAN_POINT('Ctrl Pts',(1.66953696502145,-2.75698324441747,
8.98456646529523));
#250785=CARTESIAN_POINT('Ctrl Pts',(1.62930407134655,-2.78094914807715,
8.98161311002642));
#250786=CARTESIAN_POINT('Ctrl Pts',(1.53438466208592,-2.83472378560857,
8.97466064660419));
#250787=CARTESIAN_POINT('Ctrl Pts',(1.47932916877494,-2.86384001592262,
8.97063930294934));
#250788=CARTESIAN_POINT('Ctrl Pts',(1.26940216781119,-2.96719143655235,
8.95535136796648));
#250789=CARTESIAN_POINT('Ctrl Pts',(1.10953435010655,-3.03059892613544,
8.94378059685818));
#250790=CARTESIAN_POINT('Ctrl Pts',(0.78364615359253,-3.13059771829394,
8.92073970149784));
#250791=CARTESIAN_POINT('Ctrl Pts',(0.61822635421217,-3.16742000636907,
8.90930940428953));
#250792=CARTESIAN_POINT('Ctrl Pts',(0.421443125242144,-3.1952111645793,
8.8965090809936));
#250793=CARTESIAN_POINT('Ctrl Pts',(0.392161672726725,-3.19893701994791,
8.89462520268363));
#250794=CARTESIAN_POINT('Ctrl Pts',(0.34960680670148,-3.20375869795211,
8.89192143689016));
#250795=CARTESIAN_POINT('Ctrl Pts',(0.336372174169736,-3.20517526648536,
8.89108533109125));
#250796=CARTESIAN_POINT('Ctrl Pts',(0.313147726848543,-3.20751565837872,
8.88962691855068));
#250797=CARTESIAN_POINT('Ctrl Pts',(0.303161803515259,-3.20847489143776,
8.88900270374776));
#250798=CARTESIAN_POINT('Ctrl Pts',(0.281810321414084,-3.21042530690025,
8.88767428063474));
#250799=CARTESIAN_POINT('Ctrl Pts',(0.270443838352012,-3.21140278507544,
8.88697082309523));
#250800=CARTESIAN_POINT('Ctrl Pts',(0.238883840169156,-3.21394808520337,
8.88502736996646));
#250801=CARTESIAN_POINT('Ctrl Pts',(0.218679992692779,-3.21538596309506,
8.88379429857825));
#250802=CARTESIAN_POINT('Ctrl Pts',(0.0941414129397493,-3.2230698803466,
8.87625435804898));
#250803=CARTESIAN_POINT('Ctrl Pts',(-0.0104428233843836,-3.22442822891139,
8.87018451309583));
#250804=CARTESIAN_POINT('Ctrl Pts',(-0.254242440037465,-3.21572922430982,
8.8562735944833));
#250805=CARTESIAN_POINT('Ctrl Pts',(-0.393102184261726,-3.20172249912519,
8.84852820910064));
#250806=CARTESIAN_POINT('Ctrl Pts',(-0.722358174207838,-3.14676076159942,
8.82980753313708));
#250807=CARTESIAN_POINT('Ctrl Pts',(-0.910781150226642,-3.09747790689216,
8.81878266189032));
#250808=CARTESIAN_POINT('Ctrl Pts',(-1.12610154609363,-3.01980237023165,
8.80512743496005));
#250809=CARTESIAN_POINT('Ctrl Pts',(-1.15840694355028,-3.00755785698603,
8.803050513481));
#250810=CARTESIAN_POINT('Ctrl Pts',(-1.2093654099812,-2.98730056211288,
8.79972642472518));
#250811=CARTESIAN_POINT('Ctrl Pts',(-1.22815089588314,-2.97962660263139,
8.79849053983609));
#250812=CARTESIAN_POINT('Ctrl Pts',(-1.26319482297544,-2.96492328905652,
8.79616473913879));
#250813=CARTESIAN_POINT('Ctrl Pts',(-1.2794702817088,-2.95793628215516,
8.79507628372482));
#250814=CARTESIAN_POINT('Ctrl Pts',(-1.31584634632222,-2.9419637500749,
8.79262452842622));
#250815=CARTESIAN_POINT('Ctrl Pts',(-1.33591397401606,-2.93290574850897,
8.79125880597551));
#250816=CARTESIAN_POINT('Ctrl Pts',(-1.39570241887021,-2.90517788830226,
8.78714948688398));
#250817=CARTESIAN_POINT('Ctrl Pts',(-1.43513499622488,-2.88590211980396,
8.78438534319579));
#250818=CARTESIAN_POINT('Ctrl Pts',(-1.62181230664434,-2.78987672371328,
8.77103362329734));
#250819=CARTESIAN_POINT('Ctrl Pts',(-1.76335348165384,-2.70263908910153,
8.76008718118141));
#250820=CARTESIAN_POINT('Ctrl Pts',(-2.04025760024486,-2.50092939574657,
8.73708279213534));
#250821=CARTESIAN_POINT('Ctrl Pts',(-2.17419872257642,-2.3854054667584,
8.72503644765051));
#250822=CARTESIAN_POINT('Ctrl Pts',(-2.35516790057287,-2.20135181210443,
8.7078897104694));
#250823=CARTESIAN_POINT('Ctrl Pts',(-2.41011128877512,-2.14105849970406,
8.70255022770479));
#250824=CARTESIAN_POINT('Ctrl Pts',(-2.47543153566638,-2.06367272137655,
8.69609636158663));
#250825=CARTESIAN_POINT('Ctrl Pts',(-2.48801230048514,-2.04848754599388,
8.69484816260357));
#250826=CARTESIAN_POINT('Ctrl Pts',(-2.50757727759952,-2.0244261584238,
8.69290008276931));
#250827=CARTESIAN_POINT('Ctrl Pts',(-2.51465533488637,-2.01562735390928,
8.69219385878548));
#250828=CARTESIAN_POINT('Ctrl Pts',(-2.52795288216346,-1.99891796688255,
8.69086458490445));
#250829=CARTESIAN_POINT('Ctrl Pts',(-2.53418156634888,-1.99101547050132,
8.69024092574083));
#250830=CARTESIAN_POINT('Ctrl Pts',(-2.54884423566778,-1.97223227140974,
8.68877013154336));
#250831=CARTESIAN_POINT('Ctrl Pts',(-2.55724566051497,-1.96132651988827,
8.6879252516452));
#250832=CARTESIAN_POINT('Ctrl Pts',(-2.5852673501108,-1.92446586541293,
8.68509875281145));
#250833=CARTESIAN_POINT('Ctrl Pts',(-2.60456506827781,-1.89826687421996,
8.68313794025373));
#250834=CARTESIAN_POINT('Ctrl Pts',(-2.65084850258132,-1.83339655539997,
8.6783873752143));
#250835=CARTESIAN_POINT('Ctrl Pts',(-2.6773891907197,-1.79441585518096,
8.67562136957392));
#250836=CARTESIAN_POINT('Ctrl Pts',(-2.80953723011168,-1.59086464485736,
8.66155105530988));
#250837=CARTESIAN_POINT('Ctrl Pts',(-2.90086905856561,-1.41750451604792,
8.65077551218534));
#250838=CARTESIAN_POINT('Ctrl Pts',(-3.02605127227559,-1.11632761566876,
8.63244068732546));
#250839=CARTESIAN_POINT('Ctrl Pts',(-3.06879636522613,-0.992803350138108,
8.62502417564863));
#250840=CARTESIAN_POINT('Ctrl Pts',(-3.12108012090744,-0.805630830402293,
8.6136601090384));
#250841=CARTESIAN_POINT('Ctrl Pts',(-3.13640548974017,-0.743735142676799,
8.60988353157016));
#250842=CARTESIAN_POINT('Ctrl Pts',(-3.15540890375623,-0.65589238963739,
8.60447763747915));
#250843=CARTESIAN_POINT('Ctrl Pts',(-3.16062239090892,-0.630290582089017,
8.60289668357907));
#250844=CARTESIAN_POINT('Ctrl Pts',(-3.16892724074735,-0.586810678611111,
8.60020135028748));
#250845=CARTESIAN_POINT('Ctrl Pts',(-3.17218001604058,-0.568964458058292,
8.59909211439376));
#250846=CARTESIAN_POINT('Ctrl Pts',(-3.17812852830832,-0.534690320336822,
8.59695577067443));
#250847=CARTESIAN_POINT('Ctrl Pts',(-3.1808479853168,-0.518267073010762,
8.5959294495332));
#250848=CARTESIAN_POINT('Ctrl Pts',(-3.18627083675221,-0.483865905355045,
8.59377385388674));
#250849=CARTESIAN_POINT('Ctrl Pts',(-3.18894958269097,-0.465884746456411,
8.59264384253899));
#250850=CARTESIAN_POINT('Ctrl Pts',(-3.19493046185517,-0.423266769116533,
8.58995741252176));
#250851=CARTESIAN_POINT('Ctrl Pts',(-3.19809993621978,-0.398612790540039,
8.58839692174112));
#250852=CARTESIAN_POINT('Ctrl Pts',(-3.21548428706028,-0.249794168388317,
8.57893716533452));
#250853=CARTESIAN_POINT('Ctrl Pts',(-3.22275000000241,-0.124942616104005,
8.57082639181437));
#250854=CARTESIAN_POINT('Ctrl Pts',(-3.22275,6.20740264745123E-11,8.56255098483899));
#250855=CARTESIAN_POINT('Ctrl Pts',(-3.22275,-3.27265992083881E-12,8.3171463242964));
#250856=CARTESIAN_POINT('Ctrl Pts',(-3.22274999999986,-0.138871712641594,
8.32549312351733));
#250857=CARTESIAN_POINT('Ctrl Pts',(-3.21377374162208,-0.277619577087055,
8.33342285303866));
#250858=CARTESIAN_POINT('Ctrl Pts',(-3.18241204635537,-0.51891533647005,
8.34713443980879));
#250859=CARTESIAN_POINT('Ctrl Pts',(-3.16393047941058,-0.621742613134248,
8.35295178595872));
#250860=CARTESIAN_POINT('Ctrl Pts',(-3.10222418486365,-0.88959353889187,
8.3683833070302));
#250861=CARTESIAN_POINT('Ctrl Pts',(-3.05084565312801,-1.05237991766055,
8.3780599905183));
#250862=CARTESIAN_POINT('Ctrl Pts',(-2.97001384318958,-1.25185574018367,
8.3908048922322));
#250863=CARTESIAN_POINT('Ctrl Pts',(-2.95232359297695,-1.29302364002687,
8.39348395222062));
#250864=CARTESIAN_POINT('Ctrl Pts',(-2.92447309013411,-1.35428230193386,
8.39755093625097));
#250865=CARTESIAN_POINT('Ctrl Pts',(-2.91495078667706,-1.37465824124986,
8.39891731461877));
#250866=CARTESIAN_POINT('Ctrl Pts',(-2.89744882457046,-1.41110945661461,
8.40138705532542));
#250867=CARTESIAN_POINT('Ctrl Pts',(-2.88954662220992,-1.42722103656994,
8.4024877211873));
#250868=CARTESIAN_POINT('Ctrl Pts',(-2.87223178632144,-1.46179047554909,
8.40486927612088));
#250869=CARTESIAN_POINT('Ctrl Pts',(-2.86277492496354,-1.48022516056698,
8.40615166499027));
#250870=CARTESIAN_POINT('Ctrl Pts',(-2.83677128042319,-1.52973383510967,
8.40962990804915));
#250871=CARTESIAN_POINT('Ctrl Pts',(-2.81989237745962,-1.56062927275954,
8.41183729701543));
#250872=CARTESIAN_POINT('Ctrl Pts',(-2.70479377398057,-1.76334219900991,
8.42657146642839));
#250873=CARTESIAN_POINT('Ctrl Pts',(-2.59144755426381,-1.92604808273369,
8.43964553354388));
#250874=CARTESIAN_POINT('Ctrl Pts',(-2.37086820140168,-2.18767938900173,
8.46268540361899));
#250875=CARTESIAN_POINT('Ctrl Pts',(-2.27050682223379,-2.29167114989787,
8.47249946178378));
#250876=CARTESIAN_POINT('Ctrl Pts',(-2.11610965271627,-2.43151964924748,
8.48639746402007));
#250877=CARTESIAN_POINT('Ctrl Pts',(-2.06743783135525,-2.47303651449886,
8.49062397353537));
#250878=CARTESIAN_POINT('Ctrl Pts',(-1.9958492479982,-2.53050953568307,
8.49658856510336));
#250879=CARTESIAN_POINT('Ctrl Pts',(-1.97391263024284,-2.54765809455641,
8.49838377559063));
#250880=CARTESIAN_POINT('Ctrl Pts',(-1.93919333930804,-2.57408157973627,
8.50117118052213));
#250881=CARTESIAN_POINT('Ctrl Pts',(-1.92656052298175,-2.58355014658103,
8.50217444640652));
#250882=CARTESIAN_POINT('Ctrl Pts',(-1.90307564949418,-2.60088451189204,
8.50401865294826));
#250883=CARTESIAN_POINT('Ctrl Pts',(-1.89224317655639,-2.6087761397484,
8.50486119682657));
#250884=CARTESIAN_POINT('Ctrl Pts',(-1.88125997720383,-2.61667316956632,
8.5057070612078));
#250885=CARTESIAN_POINT('Ctrl Pts',(-1.88115837905766,-2.61674621067049,
8.50571488500447));
#250886=CARTESIAN_POINT('Ctrl Pts',(-1.88095510584785,-2.61689233021979,
8.50573053707531));
#250887=CARTESIAN_POINT('Ctrl Pts',(-1.88085343078481,-2.61696540865241,
8.50573836534846));
#250888=CARTESIAN_POINT('Ctrl Pts',(-1.88064997299479,-2.6171116249185,
8.50575402873597));
#250889=CARTESIAN_POINT('Ctrl Pts',(-1.88054819025442,-2.61718476274406,
8.50576186384995));
#250890=CARTESIAN_POINT('Ctrl Pts',(-1.88034448587217,-2.61733112018699,
8.50577754331885));
#250891=CARTESIAN_POINT('Ctrl Pts',(-1.88024256422565,-2.61740433978461,
8.50578538767228));
#250892=CARTESIAN_POINT('Ctrl Pts',(-1.88003855027385,-2.61755088351372,
8.50580108805802));
#250893=CARTESIAN_POINT('Ctrl Pts',(-1.8799364579533,-2.61762420762746,
8.50580894408921));
#250894=CARTESIAN_POINT('Ctrl Pts',(-1.87973207033225,-2.61777098351325,
8.50582467030998));
#250895=CARTESIAN_POINT('Ctrl Pts',(-1.87962977500507,-2.61784443526996,
8.50583254049885));
#250896=CARTESIAN_POINT('Ctrl Pts',(-1.8794730214717,-2.61795697607002,
8.50584459935918));
#250897=CARTESIAN_POINT('Ctrl Pts',(-1.87941856637409,-2.61799606939392,
8.50584878831658));
#250898=CARTESIAN_POINT('Ctrl Pts',(-1.87930846282484,-2.6180751075451,
8.50585725761032));
#250899=CARTESIAN_POINT('Ctrl Pts',(-1.87925281430645,-2.61811505230645,
8.50586153794263));
#250900=CARTESIAN_POINT('Ctrl Pts',(-1.87914026225081,-2.61819583725013,
8.5058701947013));
#250901=CARTESIAN_POINT('Ctrl Pts',(-1.87908335866791,-2.61823667734283,
8.50587457112132));
#250902=CARTESIAN_POINT('Ctrl Pts',(-1.87896823077708,-2.61831929973529,
8.50588342507882));
#250903=CARTESIAN_POINT('Ctrl Pts',(-1.87891000638037,-2.61836108196703,
8.50588790261249));
#250904=CARTESIAN_POINT('Ctrl Pts',(-1.87879216671046,-2.61844563857855,
8.50589696415966));
#250905=CARTESIAN_POINT('Ctrl Pts',(-1.87873255136201,-2.61848841287038,
8.5059015481675));
#250906=CARTESIAN_POINT('Ctrl Pts',(-1.87861185478983,-2.61857500698266,
8.50591082839499));
#250907=CARTESIAN_POINT('Ctrl Pts',(-1.8785507735042,-2.61861882669431,
8.50591552460705));
#250908=CARTESIAN_POINT('Ctrl Pts',(-1.87842706478953,-2.61870756876487,
8.50592503537669));
#250909=CARTESIAN_POINT('Ctrl Pts',(-1.87836443730723,-2.61875249099637,
8.505929849925));
#250910=CARTESIAN_POINT('Ctrl Pts',(-1.87823755018696,-2.61884349929906,
8.5059396039387));
#250911=CARTESIAN_POINT('Ctrl Pts',(-1.87817329047198,-2.61888958524618,
8.50594454339554));
#250912=CARTESIAN_POINT('Ctrl Pts',(-1.87804304656839,-2.61898298664363,
8.50595455427835));
#250913=CARTESIAN_POINT('Ctrl Pts',(-1.87797706227456,-2.61903030197501,
8.50595962569673));
#250914=CARTESIAN_POINT('Ctrl Pts',(-1.87784326992688,-2.61912623274476,
8.50596990808571));
#250915=CARTESIAN_POINT('Ctrl Pts',(-1.87777546178851,-2.61917484803255,
8.50597511904576));
#250916=CARTESIAN_POINT('Ctrl Pts',(-1.86962271773971,-2.62501950776203,
8.50660160724154));
#250917=CARTESIAN_POINT('Ctrl Pts',(-1.86151092387614,-2.63077813827006,
8.50722035290794));
#250918=CARTESIAN_POINT('Ctrl Pts',(-1.8437088079843,-2.64329243981024,
8.50856813551125));
#250919=CARTESIAN_POINT('Ctrl Pts',(-1.83400789964211,-2.65003247626621,
8.50929613689761));
#250920=CARTESIAN_POINT('Ctrl Pts',(-1.80709417885046,-2.66851312479392,
8.51129877312448));
#250921=CARTESIAN_POINT('Ctrl Pts',(-1.78980390595036,-2.68014061158269,
8.5125661645145));
#250922=CARTESIAN_POINT('Ctrl Pts',(-1.68904982004112,-2.7464865415766,
8.5198487605171));
#250923=CARTESIAN_POINT('Ctrl Pts',(-1.60318514528748,-2.79747722929399,
8.52565123682874));
#250924=CARTESIAN_POINT('Ctrl Pts',(-1.34061496909161,-2.93733638041824,
8.542638889234));
#250925=CARTESIAN_POINT('Ctrl Pts',(-1.15796184088172,-3.01402109964819,
8.55350967576711));
#250926=CARTESIAN_POINT('Ctrl Pts',(-0.87942278267192,-3.10187685626967,
8.57005774984639));
#250927=CARTESIAN_POINT('Ctrl Pts',(-0.788218928751897,-3.12629710050875,
8.57546709884884));
#250928=CARTESIAN_POINT('Ctrl Pts',(-0.633729432688189,-3.16047185636143,
8.58472483727696));
#250929=CARTESIAN_POINT('Ctrl Pts',(-0.570986416323133,-3.17240745468482,
8.58850989625081));
#250930=CARTESIAN_POINT('Ctrl Pts',(-0.482469479632645,-3.18653505882122,
8.59390494078081));
#250931=CARTESIAN_POINT('Ctrl Pts',(-0.456958492874086,-3.1902933026789,
8.59546613383067));
#250932=CARTESIAN_POINT('Ctrl Pts',(-0.413009018921934,-3.19622992382427,
8.59816775333666));
#250933=CARTESIAN_POINT('Ctrl Pts',(-0.394591515719277,-3.19855587553381,
8.59930351837891));
#250934=CARTESIAN_POINT('Ctrl Pts',(-0.357028783342164,-3.20297032209822,
8.60162773880666));
#250935=CARTESIAN_POINT('Ctrl Pts',(-0.337882899964659,-3.20504657639043,
8.60281652714158));
#250936=CARTESIAN_POINT('Ctrl Pts',(-0.289557429898766,-3.20984935875167,
8.60582799756248));
#250937=CARTESIAN_POINT('Ctrl Pts',(-0.260357601587371,-3.21234964474769,
8.6076576298247));
#250938=CARTESIAN_POINT('Ctrl Pts',(-0.14809568101732,-3.22042160633596,
8.61473217281969));
#250939=CARTESIAN_POINT('Ctrl Pts',(-0.0648693395975112,-3.2231719832213,
8.62006270525894));
#250940=CARTESIAN_POINT('Ctrl Pts',(0.242083126850591,-3.2214228157288,
8.64004278411705));
#250941=CARTESIAN_POINT('Ctrl Pts',(0.46504091812718,-3.19685533736955,
8.65523650750677));
#250942=CARTESIAN_POINT('Ctrl Pts',(0.808754587174836,-3.12224744308685,
8.67893766195811));
#250943=CARTESIAN_POINT('Ctrl Pts',(0.932167789778479,-3.08764996819362,
8.68749180547232));
#250944=CARTESIAN_POINT('Ctrl Pts',(1.08064628823913,-3.03630766924657,
8.69760252965113));
#250945=CARTESIAN_POINT('Ctrl Pts',(1.10795978861963,-3.02644773689932,
8.69945451380098));
#250946=CARTESIAN_POINT('Ctrl Pts',(1.14761205852608,-3.0115248271853,8.70212771450214));
#250947=CARTESIAN_POINT('Ctrl Pts',(1.16005776957652,-3.00675260163004,
8.70296451783457));
#250948=CARTESIAN_POINT('Ctrl Pts',(1.18197591072979,-2.99819188404856,
8.704433801318));
#250949=CARTESIAN_POINT('Ctrl Pts',(1.19146041685937,-2.99443545796566,
8.70506810523149));
#250950=CARTESIAN_POINT('Ctrl Pts',(1.21207751000303,-2.98615640023627,
8.70644361191999));
#250951=CARTESIAN_POINT('Ctrl Pts',(1.22320276642896,-2.98161649778246,
8.70718378839269));
#250952=CARTESIAN_POINT('Ctrl Pts',(1.25438787083266,-2.96868681400308,
8.70925345379271));
#250953=CARTESIAN_POINT('Ctrl Pts',(1.27438898852221,-2.96015592390702,
8.71057489389908));
#250954=CARTESIAN_POINT('Ctrl Pts',(1.41419854510252,-2.89884451377434,
8.71978007405008));
#250955=CARTESIAN_POINT('Ctrl Pts',(1.53079321618765,-2.83900280031649,
8.72729422105979));
#250956=CARTESIAN_POINT('Ctrl Pts',(1.76449308185378,-2.70046054916079,
8.74264812493615));
#250957=CARTESIAN_POINT('Ctrl Pts',(1.88072133441807,-2.62084170723687,
8.75045652086408));
#250958=CARTESIAN_POINT('Ctrl Pts',(2.10978917157012,-2.4408174690713,8.76687559314688));
#250959=CARTESIAN_POINT('Ctrl Pts',(2.22152309911971,-2.33957866938473,
8.77548651030867));
#250960=CARTESIAN_POINT('Ctrl Pts',(2.35503891767824,-2.20038583644537,
8.78692824316239));
#250961=CARTESIAN_POINT('Ctrl Pts',(2.38370996624741,-2.1692931297839,8.78946038801784));
#250962=CARTESIAN_POINT('Ctrl Pts',(2.42634837812063,-2.1211871291642,8.79334826630215));
#250963=CARTESIAN_POINT('Ctrl Pts',(2.44076766996782,-2.10457939584093,
8.79468525959255));
#250964=CARTESIAN_POINT('Ctrl Pts',(2.46559381910714,-2.07538702443204,
8.79702705324854));
#250965=CARTESIAN_POINT('Ctrl Pts',(2.47607722087527,-2.06286833387161,
8.79802868518783));
#250966=CARTESIAN_POINT('Ctrl Pts',(2.49951986638565,-2.03443827579246,
8.80029786556783));
#250967=CARTESIAN_POINT('Ctrl Pts',(2.5124230825974,-2.01848182642884,8.80156760173161));
#250968=CARTESIAN_POINT('Ctrl Pts',(2.54704921480069,-1.97481581898038,
8.80503258032998));
#250969=CARTESIAN_POINT('Ctrl Pts',(2.56847133747548,-1.94687237736057,
8.80723948342038));
#250970=CARTESIAN_POINT('Ctrl Pts',(2.68577887739204,-1.78854744782075,
8.81969007021221));
#250971=CARTESIAN_POINT('Ctrl Pts',(2.77218112189211,-1.6514565233853,8.83028851493101));
#250972=CARTESIAN_POINT('Ctrl Pts',(2.97044599114619,-1.27714379461894,
8.85862020696376));
#250973=CARTESIAN_POINT('Ctrl Pts',(3.06433467069823,-1.0317476905041,8.87666825468886));
#250974=CARTESIAN_POINT('Ctrl Pts',(3.13450705190292,-0.749549442219714,
8.89538209243264));
#250975=CARTESIAN_POINT('Ctrl Pts',(3.1411262463419,-0.72130774545741,8.89723201552028));
#250976=CARTESIAN_POINT('Ctrl Pts',(3.15022833624442,-0.679968011310853,
8.89990282012875));
#250977=CARTESIAN_POINT('Ctrl Pts',(3.15301250855036,-0.666938679584662,
8.90073925047146));
#250978=CARTESIAN_POINT('Ctrl Pts',(3.15778556569586,-0.643903671248034,
8.90220812777865));
#250979=CARTESIAN_POINT('Ctrl Pts',(3.15980784914751,-0.633905342266739,
8.90284239480194));
#250980=CARTESIAN_POINT('Ctrl Pts',(3.1641096133106,-0.612104884364183,
8.90421811050322));
#250981=CARTESIAN_POINT('Ctrl Pts',(3.16637056998124,-0.600299474258282,
8.90495853009412));
#250982=CARTESIAN_POINT('Ctrl Pts',(3.17253916188141,-0.567085875891002,
8.90702954124098));
#250983=CARTESIAN_POINT('Ctrl Pts',(3.17629616734186,-0.545649923993654,
8.90835206741264));
#250984=CARTESIAN_POINT('Ctrl Pts',(3.20127623402628,-0.394112322451382,
8.91761252754723));
#250985=CARTESIAN_POINT('Ctrl Pts',(3.21471887212368,-0.262839283720132,
8.9251756856096));
#250986=CARTESIAN_POINT('Ctrl Pts',(3.22145081768205,-0.0974873599437175,
8.93452603952649));
#250987=CARTESIAN_POINT('Ctrl Pts',(3.22229290629807,-0.0638563153275335,
8.93641852989922));
#250988=CARTESIAN_POINT('Ctrl Pts',(3.22380517304242,0.0974202337625863,
8.94547231077243));
#250989=CARTESIAN_POINT('Ctrl Pts',(3.21741784977303,0.225016397026926,
8.95257536077568));
#250990=CARTESIAN_POINT('Ctrl Pts',(3.19299922949613,0.447311592712934,
8.96523772584299));
#250991=CARTESIAN_POINT('Ctrl Pts',(3.17826077705034,0.542206862520621,
8.97073546687506));
#250992=CARTESIAN_POINT('Ctrl Pts',(3.14655065519546,0.699652108231218,
8.98012852397965));
#250993=CARTESIAN_POINT('Ctrl Pts',(3.13188884131935,0.762604454334836,
8.98395791850103));
#250994=CARTESIAN_POINT('Ctrl Pts',(3.10871385541442,0.850109796472525,
8.98940550770157));
#250995=CARTESIAN_POINT('Ctrl Pts',(3.10178096543433,0.875067588276021,
8.99097358626977));
#250996=CARTESIAN_POINT('Ctrl Pts',(3.08935844405652,0.917783938103222,
8.99368336252657));
#250997=CARTESIAN_POINT('Ctrl Pts',(3.08401457492498,0.935583792083977,
8.9948203234438));
#250998=CARTESIAN_POINT('Ctrl Pts',(3.07283013004021,0.971700649106543,
8.99714363044217));
#250999=CARTESIAN_POINT('Ctrl Pts',(3.06697901139717,0.990013574595633,
8.99833027986354));
#251000=CARTESIAN_POINT('Ctrl Pts',(3.05184546061892,1.03595675992544,9.00132958881494));
#251001=CARTESIAN_POINT('Ctrl Pts',(3.04235152575301,1.06351503462374,9.00314908417564));
#251002=CARTESIAN_POINT('Ctrl Pts',(3.00472615316497,1.16810225889175,9.01013439662061));
#251003=CARTESIAN_POINT('Ctrl Pts',(2.97403416798693,1.24417081105629,9.01538307968314));
#251004=CARTESIAN_POINT('Ctrl Pts',(2.84845398573691,1.5241335877863,9.03534353668843));
#251005=CARTESIAN_POINT('Ctrl Pts',(2.73522166173166,1.71907332218323,9.05061170205248));
#251006=CARTESIAN_POINT('Ctrl Pts',(2.52689865642948,2.00434494549809,9.07441685072121));
#251007=CARTESIAN_POINT('Ctrl Pts',(2.44500779261715,2.10346344091809,9.08299877038743));
#251008=CARTESIAN_POINT('Ctrl Pts',(2.33758508292927,2.21870661871043,9.09313825812359));
#251009=CARTESIAN_POINT('Ctrl Pts',(2.31747059021294,2.23970830213674,9.09499294975559));
#251010=CARTESIAN_POINT('Ctrl Pts',(2.28771959420334,2.26994151535602,9.09766929757518));
#251011=CARTESIAN_POINT('Ctrl Pts',(2.27830626650374,2.27938939091333,9.09850659047124));
#251012=CARTESIAN_POINT('Ctrl Pts',(2.26158905372992,2.29596093016854,9.09997640736427));
#251013=CARTESIAN_POINT('Ctrl Pts',(2.25430964712483,2.30310869597198,9.10061075998425));
#251014=CARTESIAN_POINT('Ctrl Pts',(2.23838656252992,2.31859599887127,9.10198599362348));
#251015=CARTESIAN_POINT('Ctrl Pts',(2.22973011416261,2.32692188051089,9.1027258519865));
#251016=CARTESIAN_POINT('Ctrl Pts',(2.20528936357461,2.35016767810853,9.10479375699021));
#251017=CARTESIAN_POINT('Ctrl Pts',(2.18940016856477,2.36497700872762,9.10611377645315));
#251018=CARTESIAN_POINT('Ctrl Pts',(2.07751830969872,2.46716108282812,9.1152505143857));
#251019=CARTESIAN_POINT('Ctrl Pts',(1.9764623039544,2.54883708027539,9.1227039976922));
#251020=CARTESIAN_POINT('Ctrl Pts',(1.83697665060975,2.64827378911859,9.13238792020146));
#251021=CARTESIAN_POINT('Ctrl Pts',(1.80274724615224,2.67169229682434,9.1347194434662));
#251022=CARTESIAN_POINT('Ctrl Pts',(1.65141396068678,2.77099612686269,9.1448731152008));
#251023=CARTESIAN_POINT('Ctrl Pts',(1.52990537793964,2.83989014209792,9.15263749559056));
#251024=CARTESIAN_POINT('Ctrl Pts',(1.32737900486418,2.93793968981156,9.16543737772343));
#251025=CARTESIAN_POINT('Ctrl Pts',(1.24899283547981,2.97211037649064,9.17035792676415));
#251026=CARTESIAN_POINT('Ctrl Pts',(1.11390527433192,3.02471025492896,9.17886144984751));
#251027=CARTESIAN_POINT('Ctrl Pts',(1.05788150545804,3.04475666516966,9.18239438762166));
#251028=CARTESIAN_POINT('Ctrl Pts',(0.97747792121327,3.07103965888363,9.18748969283881));
#251029=CARTESIAN_POINT('Ctrl Pts',(0.953528564650351,3.07855987357206,
9.18901045006191));
#251030=CARTESIAN_POINT('Ctrl Pts',(0.911832644431462,3.09111938099778,
9.19166447150273));
#251031=CARTESIAN_POINT('Ctrl Pts',(0.894125929603302,3.09628755108062,
9.1927935117546));
#251032=CARTESIAN_POINT('Ctrl Pts',(0.85763663308899,3.10659881186108,9.19512467764991));
#251033=CARTESIAN_POINT('Ctrl Pts',(0.838849882616714,3.11172421984555,
9.1963273194556));
#251034=CARTESIAN_POINT('Ctrl Pts',(0.790689683539448,3.12439547603439,
9.19941702500773));
#251035=CARTESIAN_POINT('Ctrl Pts',(0.761254584397249,3.13169740301161,
9.20131178835742));
#251036=CARTESIAN_POINT('Ctrl Pts',(0.641642722384108,3.15958342444384,
9.20903920692168));
#251037=CARTESIAN_POINT('Ctrl Pts',(0.550709468291767,3.17669469404434,
9.21497947844878));
#251038=CARTESIAN_POINT('Ctrl Pts',(0.195913013091476,3.22776665346799,
9.23840887808661));
#251039=CARTESIAN_POINT('Ctrl Pts',(-0.0710160717257073,3.23292233281573,
9.25667631422829));
#251040=CARTESIAN_POINT('Ctrl Pts',(-0.395495009308637,3.19895941854281,
9.27840397080948));
#251041=CARTESIAN_POINT('Ctrl Pts',(-0.455315691451798,3.19099452952216,
9.28238368066898));
#251042=CARTESIAN_POINT('Ctrl Pts',(-0.553473305392612,3.17510838816105,
9.28883621141655));
#251043=CARTESIAN_POINT('Ctrl Pts',(-0.591951236073455,3.16816035301142,
9.29134569372441));
#251044=CARTESIAN_POINT('Ctrl Pts',(-0.644990451313554,3.15758284491279,
9.29476859539456));
#251045=CARTESIAN_POINT('Ctrl Pts',(-0.659665522997785,3.15454965452598,
9.29571178946506));
#251046=CARTESIAN_POINT('Ctrl Pts',(-0.68452614582728,3.14923013912199,
9.29730244525827));
#251047=CARTESIAN_POINT('Ctrl Pts',(-0.694722624315437,3.14699650470987,
9.29795278337363));
#251048=CARTESIAN_POINT('Ctrl Pts',(-0.715821102949639,3.14226714046142,
9.29929396039003));
#251049=CARTESIAN_POINT('Ctrl Pts',(-0.726721198706648,3.13976415381342,
9.29998439236741));
#251050=CARTESIAN_POINT('Ctrl Pts',(-0.755633066626796,3.13296649930565,
9.30180971577636));
#251051=CARTESIAN_POINT('Ctrl Pts',(-0.773621522782923,3.12857318810004,
9.30293919216496));
#251052=CARTESIAN_POINT('Ctrl Pts',(-0.853585083963955,3.10831186364933,
9.30793636105959));
#251053=CARTESIAN_POINT('Ctrl Pts',(-0.915121499975737,3.0907545927545,
9.31171851506432));
#251054=CARTESIAN_POINT('Ctrl Pts',(-1.15559984020283,3.0143293692113,9.32639266697568));
#251055=CARTESIAN_POINT('Ctrl Pts',(-1.32976740692928,2.94165288655902,
9.33680255997277));
#251056=CARTESIAN_POINT('Ctrl Pts',(-1.64888516008725,2.77432199988384,
9.35702748682802));
#251057=CARTESIAN_POINT('Ctrl Pts',(-1.79451992412909,2.68241944435577,
9.36678407159005));
#251058=CARTESIAN_POINT('Ctrl Pts',(-1.96812510062245,2.55237630252674,
9.37962677292588));
#251059=CARTESIAN_POINT('Ctrl Pts',(-2.00355896184414,2.52465688614686,
9.38231635642619));
#251060=CARTESIAN_POINT('Ctrl Pts',(-2.0558475642037,2.48195805368222,9.38639614566082));
#251061=CARTESIAN_POINT('Ctrl Pts',(-2.07314511300689,2.46752797115906,
9.38776459761015));
#251062=CARTESIAN_POINT('Ctrl Pts',(-2.1039502594539,2.44127691914511,9.39023656874927));
#251063=CARTESIAN_POINT('Ctrl Pts',(-2.11751317425248,2.42952209841076,
9.39133737015744));
#251064=CARTESIAN_POINT('Ctrl Pts',(-2.14650130161633,2.40397129082512,
9.39371749797249));
#251065=CARTESIAN_POINT('Ctrl Pts',(-2.16189316647235,2.39013884743985,
9.39499830800429));
#251066=CARTESIAN_POINT('Ctrl Pts',(-2.20302561553596,2.35245133728751,
9.39846800844348));
#251067=CARTESIAN_POINT('Ctrl Pts',(-2.22851092987276,2.32832300973116,
9.40066833803993));
#251068=CARTESIAN_POINT('Ctrl Pts',(-2.38092814783271,2.17922618415016,
9.41414381981346));
#251069=CARTESIAN_POINT('Ctrl Pts',(-2.49769468477755,2.0443457195269,9.42585513849153));
#251070=CARTESIAN_POINT('Ctrl Pts',(-2.67661259410675,1.79932410080635,
9.44621665294377));
#251071=CARTESIAN_POINT('Ctrl Pts',(-2.74454895905638,1.69389266475163,
9.45472194852874));
#251072=CARTESIAN_POINT('Ctrl Pts',(-2.87078134556872,1.47037228885663,
9.4719984995253));
#251073=CARTESIAN_POINT('Ctrl Pts',(-2.92834112964672,1.35211155607308,
9.48074663081971));
#251074=CARTESIAN_POINT('Ctrl Pts',(-2.98674212113149,1.21076514330352,
9.49051330718898));
#251075=CARTESIAN_POINT('Ctrl Pts',(-2.99476117742538,1.19079229001067,
9.49187779278897));
#251076=CARTESIAN_POINT('Ctrl Pts',(-3.00687969139785,1.15971211395653,
9.49397538874179));
#251077=CARTESIAN_POINT('Ctrl Pts',(-3.01111888049899,1.1486604213875,9.494716268362));
#251078=CARTESIAN_POINT('Ctrl Pts',(-3.01890771861766,1.12801523639184,
9.49609064219623));
#251079=CARTESIAN_POINT('Ctrl Pts',(-3.02247260049738,1.11842816913565,
9.49672497460814));
#251080=CARTESIAN_POINT('Ctrl Pts',(-3.03059204095594,1.09627013175207,
9.49818230757814));
#251081=CARTESIAN_POINT('Ctrl Pts',(-3.03511408276803,1.08368761159811,
9.49900341478691));
#251082=CARTESIAN_POINT('Ctrl Pts',(-3.04954717926666,1.04272862519446,
9.50165653420581));
#251083=CARTESIAN_POINT('Ctrl Pts',(-3.05913990599278,1.01424068399603,
9.50347114763969));
#251084=CARTESIAN_POINT('Ctrl Pts',(-3.1193235302528,0.826883378583062,
9.51523078415365));
#251085=CARTESIAN_POINT('Ctrl Pts',(-3.15792492355337,0.664408295753191,
9.52462007141607));
#251086=CARTESIAN_POINT('Ctrl Pts',(-3.20961605577271,0.335037622274209,
9.5433072965792));
#251087=CARTESIAN_POINT('Ctrl Pts',(-3.22264408328298,0.16866344872347,
9.55258213906997));
#251088=CARTESIAN_POINT('Ctrl Pts',(-3.22274978560362,0.00135739825249329,
9.56220666773146));
#251089=CARTESIAN_POINT('Ctrl Pts',(-3.22275,0.000678697741503386,9.5622457156205));
#251090=CARTESIAN_POINT('Ctrl Pts',(-3.22275,-1.85372951893938E-11,9.562284768011));
#251091=CARTESIAN_POINT('Origin',(0.,0.,-2.31077344927308));
#251092=CARTESIAN_POINT('',(-3.22275,2.40369908895709E-12,11.0578560525147));
#251093=CARTESIAN_POINT('',(-3.22275,-7.2705680572429E-11,10.8125553006127));
#251094=CARTESIAN_POINT('',(-3.22275,-3.50678552687464E-13,-2.31077344927308));
#251095=CARTESIAN_POINT('Ctrl Pts',(-3.22275,2.40444816834717E-12,11.0578560525147));
#251096=CARTESIAN_POINT('Ctrl Pts',(-3.22275000000001,0.129559515672562,
11.0500824638212));
#251097=CARTESIAN_POINT('Ctrl Pts',(-3.21493720991752,0.259019917678811,
11.0426677662696));
#251098=CARTESIAN_POINT('Ctrl Pts',(-3.18771361783945,0.483687132446777,
11.029897752772));
#251099=CARTESIAN_POINT('Ctrl Pts',(-3.17176321528631,0.579128619885433,
11.0245043322675));
#251100=CARTESIAN_POINT('Ctrl Pts',(-3.11552323426711,0.842213631850827,
11.0094280728851));
#251101=CARTESIAN_POINT('Ctrl Pts',(-3.06604976184367,1.00754136211081,
10.9996978770402));
#251102=CARTESIAN_POINT('Ctrl Pts',(-2.98418509968392,1.21804217026348,
10.9864012326541));
#251103=CARTESIAN_POINT('Ctrl Pts',(-2.96352674057112,1.2674763142955,10.9832114858982));
#251104=CARTESIAN_POINT('Ctrl Pts',(-2.93192754731569,1.33808991118212,
10.9785457093997));
#251105=CARTESIAN_POINT('Ctrl Pts',(-2.92196825607857,1.35970041452184,
10.9771027185616));
#251106=CARTESIAN_POINT('Ctrl Pts',(-2.90409116951917,1.39738796538432,
10.9745587105735));
#251107=CARTESIAN_POINT('Ctrl Pts',(-2.89627679837646,1.41351311758217,
10.9734612763886));
#251108=CARTESIAN_POINT('Ctrl Pts',(-2.87975861372052,1.44688670264265,
10.9711709021882));
#251109=CARTESIAN_POINT('Ctrl Pts',(-2.8710333763337,1.46412367298211,10.9699772517989));
#251110=CARTESIAN_POINT('Ctrl Pts',(-2.84793373250783,1.50875716279774,
10.9668579223649));
#251111=CARTESIAN_POINT('Ctrl Pts',(-2.83331912727679,1.53602647687385,
10.9649239062851));
#251112=CARTESIAN_POINT('Ctrl Pts',(-2.76907404225313,1.65186367741078,
10.9565841915675));
#251113=CARTESIAN_POINT('Ctrl Pts',(-2.71567051762071,1.73826199208525,
10.9500464450712));
#251114=CARTESIAN_POINT('Ctrl Pts',(-2.51264845676957,2.03447128423172,
10.9264854137821));
#251115=CARTESIAN_POINT('Ctrl Pts',(-2.34206470399986,2.22871816785953,
10.9087913962321));
#251116=CARTESIAN_POINT('Ctrl Pts',(-2.10590428211393,2.44025078974346,
10.8876853480936));
#251117=CARTESIAN_POINT('Ctrl Pts',(-2.0604974497287,2.47871091541957,10.8837630858007));
#251118=CARTESIAN_POINT('Ctrl Pts',(-1.99345692417629,2.5323788946328,10.8781927051519));
#251119=CARTESIAN_POINT('Ctrl Pts',(-1.97266198190285,2.54861102814899,
10.8764942601736));
#251120=CARTESIAN_POINT('Ctrl Pts',(-1.93963780607322,2.57374267127287,
10.8738457817747));
#251121=CARTESIAN_POINT('Ctrl Pts',(-1.92754166185542,2.5828142244877,10.8728857884457));
#251122=CARTESIAN_POINT('Ctrl Pts',(-1.90500983863986,2.59946560081246,
10.8711168717255));
#251123=CARTESIAN_POINT('Ctrl Pts',(-1.8945916865607,2.60706851644924,10.8703065033178));
#251124=CARTESIAN_POINT('Ctrl Pts',(-1.88403504199095,2.61467579943866,
10.8694931644275));
#251125=CARTESIAN_POINT('Ctrl Pts',(-1.8839421101274,2.61474276006432,10.86948600508));
#251126=CARTESIAN_POINT('Ctrl Pts',(-1.88375602480442,2.6148768259124,10.8694716705297));
#251127=CARTESIAN_POINT('Ctrl Pts',(-1.88366287131279,2.61494393112326,
10.8694644953273));
#251128=CARTESIAN_POINT('Ctrl Pts',(-1.88347631387325,2.61507830682526,
10.8694501268533));
#251129=CARTESIAN_POINT('Ctrl Pts',(-1.88338290991514,2.61514557728422,
10.8694429335841));
#251130=CARTESIAN_POINT('Ctrl Pts',(-1.88319582210173,2.61528030456501,
10.8694285267194));
#251131=CARTESIAN_POINT('Ctrl Pts',(-1.88310213822827,2.6153477613555,10.869421313126));
#251132=CARTESIAN_POINT('Ctrl Pts',(-1.88291446051664,2.61548288281355,
10.8694068633089));
#251133=CARTESIAN_POINT('Ctrl Pts',(-1.88282046665552,2.61555054744818,
10.8693996270874));
#251134=CARTESIAN_POINT('Ctrl Pts',(-1.88263213821211,2.61568610658458,
10.8693851296589));
#251135=CARTESIAN_POINT('Ctrl Pts',(-1.88253780361161,2.6157540010448,10.8693778684549));
#251136=CARTESIAN_POINT('Ctrl Pts',(-1.88234876220566,2.61589004232521,
10.8693633186517));
#251137=CARTESIAN_POINT('Ctrl Pts',(-1.88225405537621,2.61595818910264,
10.8693560300556));
#251138=CARTESIAN_POINT('Ctrl Pts',(-1.88206423726578,2.61609475803781,
10.8693414230015));
#251139=CARTESIAN_POINT('Ctrl Pts',(-1.88196912592922,2.61616318016996,
10.8693341045446));
#251140=CARTESIAN_POINT('Ctrl Pts',(-1.88177846568662,2.61630032343963,
10.8693194352373));
#251141=CARTESIAN_POINT('Ctrl Pts',(-1.88168291675512,2.61636904452413,
10.8693120843908));
#251142=CARTESIAN_POINT('Ctrl Pts',(-1.88149134731724,2.61650680993905,
10.8692973477058));
#251143=CARTESIAN_POINT('Ctrl Pts',(-1.88139532676968,2.61657585422175,
10.8692899618705));
#251144=CARTESIAN_POINT('Ctrl Pts',(-1.88120277914009,2.61671429093594,
10.8692751525385));
#251145=CARTESIAN_POINT('Ctrl Pts',(-1.881106252016,2.61678368331414,10.8692677290453));
#251146=CARTESIAN_POINT('Ctrl Pts',(-1.88091265524343,2.61692284183828,
10.8692528416505));
#251147=CARTESIAN_POINT('Ctrl Pts',(-1.88081558555222,2.61699260792493,
10.8692453777529));
#251148=CARTESIAN_POINT('Ctrl Pts',(-1.88062086655704,2.61713254024876,
10.8692304067201));
#251149=CARTESIAN_POINT('Ctrl Pts',(-1.88052321721424,2.61720270641709,
10.8692228995896));
#251150=CARTESIAN_POINT('Ctrl Pts',(-1.88032730067245,2.61734346609033,
10.8692078391751));
#251151=CARTESIAN_POINT('Ctrl Pts',(-1.88022903341423,2.61741405953397,
10.8692002858949));
#251152=CARTESIAN_POINT('Ctrl Pts',(-1.88007235718182,2.61752659956531,
10.8691882441117));
#251153=CARTESIAN_POINT('Ctrl Pts',(-1.88001395080455,2.61756854971391,
10.8691837553688));
#251154=CARTESIAN_POINT('Ctrl Pts',(-1.87989486991375,2.61765407304937,
10.8691746040579));
#251155=CARTESIAN_POINT('Ctrl Pts',(-1.87983419529939,2.61769764607433,
10.8691699415011));
#251156=CARTESIAN_POINT('Ctrl Pts',(-1.8797104378243,2.6177865150668,10.8691604318536));
#251157=CARTESIAN_POINT('Ctrl Pts',(-1.87964735484877,2.61783181085822,
10.869155584775));
#251158=CARTESIAN_POINT('Ctrl Pts',(-1.87951862837204,2.6179242339366,10.8691456944473));
#251159=CARTESIAN_POINT('Ctrl Pts',(-1.87945298470475,2.61797136105697,
10.8691406512087));
#251160=CARTESIAN_POINT('Ctrl Pts',(-1.87931897094449,2.61806756502409,
10.8691303558859));
#251161=CARTESIAN_POINT('Ctrl Pts',(-1.87925060070609,2.61811664165843,
10.8691251038164));
#251162=CARTESIAN_POINT('Ctrl Pts',(-1.87911095272682,2.61821687366412,
10.8691143770005));
#251163=CARTESIAN_POINT('Ctrl Pts',(-1.87903967482744,2.61826802879724,
10.8691089022706));
#251164=CARTESIAN_POINT('Ctrl Pts',(-1.87889401345825,2.61837255887556,
10.869097715008));
#251165=CARTESIAN_POINT('Ctrl Pts',(-1.878819629823,2.61842593354739,10.8690920024945));
#251166=CARTESIAN_POINT('Ctrl Pts',(-1.87866753983554,2.61853505732013,
10.8690803230856));
#251167=CARTESIAN_POINT('Ctrl Pts',(-1.87858983328096,2.6185908061283,10.8690743562103));
#251168=CARTESIAN_POINT('Ctrl Pts',(-1.87518841643377,2.62103084630225,
10.8688131892507));
#251169=CARTESIAN_POINT('Ctrl Pts',(-1.87186015036279,2.62340882675942,
10.868558416429));
#251170=CARTESIAN_POINT('Ctrl Pts',(-1.86058206347832,2.63143440768492,
10.8676977517389));
#251171=CARTESIAN_POINT('Ctrl Pts',(-1.85261113647786,2.63705226271344,
10.8670939383376));
#251172=CARTESIAN_POINT('Ctrl Pts',(-1.83459453773166,2.64962823242715,
10.8657389134714));
#251173=CARTESIAN_POINT('Ctrl Pts',(-1.82453443193824,2.65656564112859,
10.8649890754729));
#251174=CARTESIAN_POINT('Ctrl Pts',(-1.7903420093807,2.67985874735681,10.8624624968122));
#251175=CARTESIAN_POINT('Ctrl Pts',(-1.7660265561831,2.69594468634451,10.8607025588543));
#251176=CARTESIAN_POINT('Ctrl Pts',(-1.60864653225793,2.79701658045753,
10.8495227339465));
#251177=CARTESIAN_POINT('Ctrl Pts',(-1.46969187544244,2.87246626845974,
10.8406027460142));
#251178=CARTESIAN_POINT('Ctrl Pts',(-1.20045221910409,2.99398231688377,
10.8240342908695));
#251179=CARTESIAN_POINT('Ctrl Pts',(-1.07166350145814,3.04245821673982,
10.8163871953811));
#251180=CARTESIAN_POINT('Ctrl Pts',(-0.856075191112018,3.10821232037135,
10.8035805598983));
#251181=CARTESIAN_POINT('Ctrl Pts',(-0.770964254086266,3.13040909811233,
10.7985249098889));
#251182=CARTESIAN_POINT('Ctrl Pts',(-0.625958286859991,3.16195376934715,
10.7898249647499));
#251183=CARTESIAN_POINT('Ctrl Pts',(-0.566513169271558,3.17314316655377,
10.7862347466975));
#251184=CARTESIAN_POINT('Ctrl Pts',(-0.482170066042086,3.18657357604678,
10.7810907875335));
#251185=CARTESIAN_POINT('Ctrl Pts',(-0.457504918898764,3.19020819449482,
10.7795805542101));
#251186=CARTESIAN_POINT('Ctrl Pts',(-0.414861040399264,3.19598742461422,
10.77695816986));
#251187=CARTESIAN_POINT('Ctrl Pts',(-0.396901607538267,3.19826740504563,
10.7758503038028));
#251188=CARTESIAN_POINT('Ctrl Pts',(-0.360145019859527,3.20261935428669,
10.7735754375195));
#251189=CARTESIAN_POINT('Ctrl Pts',(-0.341346959658448,3.20467742413583,
10.7724080486987));
#251190=CARTESIAN_POINT('Ctrl Pts',(-0.293657577687159,3.20947425100848,
10.7694359175106));
#251191=CARTESIAN_POINT('Ctrl Pts',(-0.264745840222058,3.21198837063366,
10.7676242580571));
#251192=CARTESIAN_POINT('Ctrl Pts',(-0.151965747621098,3.22026253570177,
10.7605171867695));
#251193=CARTESIAN_POINT('Ctrl Pts',(-0.0679248644470271,3.2231302406892,
10.7551337872344));
#251194=CARTESIAN_POINT('Ctrl Pts',(0.239870586383329,3.22159004666573,
10.7350934008747));
#251195=CARTESIAN_POINT('Ctrl Pts',(0.46287007883022,3.197172115212,10.7198935749299));
#251196=CARTESIAN_POINT('Ctrl Pts',(0.818417525960991,3.12024546143878,
10.6953756560294));
#251197=CARTESIAN_POINT('Ctrl Pts',(0.953264652701141,3.08172578692523,
10.6860242228825));
#251198=CARTESIAN_POINT('Ctrl Pts',(1.10536200847474,3.02733403948147,10.6757088239057));
#251199=CARTESIAN_POINT('Ctrl Pts',(1.12546321809909,3.01991873364581,10.6743504962642));
#251200=CARTESIAN_POINT('Ctrl Pts',(1.15638707723655,3.0081593072651,10.67227013515));
#251201=CARTESIAN_POINT('Ctrl Pts',(1.1672621925012,3.00395613718951,10.6715403170101));
#251202=CARTESIAN_POINT('Ctrl Pts',(1.18740757747724,2.99604414032993,10.6701920302247));
#251203=CARTESIAN_POINT('Ctrl Pts',(1.19668346033298,2.99235124024546,10.669572697588));
#251204=CARTESIAN_POINT('Ctrl Pts',(1.21791370270418,2.983784580234,10.6681584381055));
#251205=CARTESIAN_POINT('Ctrl Pts',(1.22985609129761,2.97888204134868,10.6673652264292));
#251206=CARTESIAN_POINT('Ctrl Pts',(1.26706696432384,2.96334446940346,10.6649000314335));
#251207=CARTESIAN_POINT('Ctrl Pts',(1.29223012277711,2.9524583922528,10.6632421724089));
#251208=CARTESIAN_POINT('Ctrl Pts',(1.5121369754719,2.8539721771141,10.6488089694089));
#251209=CARTESIAN_POINT('Ctrl Pts',(1.69789124088129,2.74752704567681,10.6369764680038));
#251210=CARTESIAN_POINT('Ctrl Pts',(2.0240181698143,2.51484562641522,10.6145419210475));
#251211=CARTESIAN_POINT('Ctrl Pts',(2.16650977791634,2.3931827868718,10.6040097190267));
#251212=CARTESIAN_POINT('Ctrl Pts',(2.33320013809648,2.22370549559047,10.5899896064324));
#251213=CARTESIAN_POINT('Ctrl Pts',(2.36789887790087,2.18671980424736,10.5869662548543));
#251214=CARTESIAN_POINT('Ctrl Pts',(2.41724078058268,2.13157385881052,10.5825005146122));
#251215=CARTESIAN_POINT('Ctrl Pts',(2.43258332572874,2.11404787711417,10.5810872403182));
#251216=CARTESIAN_POINT('Ctrl Pts',(2.45934402902874,2.08280173192541,10.5785771793172));
#251217=CARTESIAN_POINT('Ctrl Pts',(2.47084081787816,2.06915000429485,10.5774836712426));
#251218=CARTESIAN_POINT('Ctrl Pts',(2.49468847825476,2.0403502012787,10.5751829787462));
#251219=CARTESIAN_POINT('Ctrl Pts',(2.5070160961159,2.02518389646849,10.5739749211863));
#251220=CARTESIAN_POINT('Ctrl Pts',(2.5391511176897,1.98490605577609,10.5707752881733));
#251221=CARTESIAN_POINT('Ctrl Pts',(2.55872358141808,1.95961066671809,10.5687745618497));
#251222=CARTESIAN_POINT('Ctrl Pts',(2.64594959955199,1.84334491088647,10.5596149134085));
#251223=CARTESIAN_POINT('Ctrl Pts',(2.7091437683332,1.74914405162671,10.5522888671342));
#251224=CARTESIAN_POINT('Ctrl Pts',(2.87193251423436,1.47642925180776,10.5313543279428));
#251225=CARTESIAN_POINT('Ctrl Pts',(2.95970872311629,1.29149212229401,10.5174374203378));
#251226=CARTESIAN_POINT('Ctrl Pts',(3.06883075741024,0.990838920094808,
10.4959340487044));
#251227=CARTESIAN_POINT('Ctrl Pts',(3.10240214701306,0.880107884326185,
10.4882454789333));
#251228=CARTESIAN_POINT('Ctrl Pts',(3.13632429541335,0.741824089946173,
10.4791015506356));
#251229=CARTESIAN_POINT('Ctrl Pts',(3.14237363643059,0.715766094794129,
10.4773982422441));
#251230=CARTESIAN_POINT('Ctrl Pts',(3.15082256759938,0.677197765835653,
10.4749092535776));
#251231=CARTESIAN_POINT('Ctrl Pts',(3.15347341233552,0.664744399741812,
10.4741104909091));
#251232=CARTESIAN_POINT('Ctrl Pts',(3.15787195756625,0.643461931609997,
10.4727541770863));
#251233=CARTESIAN_POINT('Ctrl Pts',(3.15965656219293,0.634640822572474,
10.4721945885743));
#251234=CARTESIAN_POINT('Ctrl Pts',(3.16364526309505,0.61449116804347,10.4709222720665));
#251235=CARTESIAN_POINT('Ctrl Pts',(3.16582548377959,0.60315815680108,10.4702108887756));
#251236=CARTESIAN_POINT('Ctrl Pts',(3.17167504042756,0.571845803454318,
10.4682564141));
#251237=CARTESIAN_POINT('Ctrl Pts',(3.17521650160777,0.551842731757692,
10.4670202164048));
#251238=CARTESIAN_POINT('Ctrl Pts',(3.19442190942959,0.437053503647063,
10.4599900496432));
#251239=CARTESIAN_POINT('Ctrl Pts',(3.20603182205207,0.341629263778248,
10.4543941823359));
#251240=CARTESIAN_POINT('Ctrl Pts',(3.22604325100663,0.0800402408187453,
10.4393890944939));
#251241=CARTESIAN_POINT('Ctrl Pts',(3.22587776478429,-0.0864785839638742,
10.4301928452507));
#251242=CARTESIAN_POINT('Ctrl Pts',(3.19905479949046,-0.428122824957318,
10.4109251680659));
#251243=CARTESIAN_POINT('Ctrl Pts',(3.17083061495106,-0.602547191351914,
10.4008612632071));
#251244=CARTESIAN_POINT('Ctrl Pts',(3.12021418627865,-0.807196605100585,
10.388279466622));
#251245=CARTESIAN_POINT('Ctrl Pts',(3.11141303713501,-0.840483018070908,
10.3862087464774));
#251246=CARTESIAN_POINT('Ctrl Pts',(3.09663971301863,-0.892940588733594,
10.3829038980933));
#251247=CARTESIAN_POINT('Ctrl Pts',(3.09101861743526,-0.912208466166179,
10.3816810702794));
#251248=CARTESIAN_POINT('Ctrl Pts',(3.08009110039021,-0.948404479685862,
10.3793664539743));
#251249=CARTESIAN_POINT('Ctrl Pts',(3.07482414844154,-0.965343814469545,
10.3782759826455));
#251250=CARTESIAN_POINT('Ctrl Pts',(3.06260746957594,-1.0035199690134,10.3758015638254));
#251251=CARTESIAN_POINT('Ctrl Pts',(3.05557623719565,-1.02472955435905,
10.3744149989262));
#251252=CARTESIAN_POINT('Ctrl Pts',(3.03402455467029,-1.08754512388,10.370272325954));
#251253=CARTESIAN_POINT('Ctrl Pts',(3.01887116371246,-1.12892691789836,
10.367495668078));
#251254=CARTESIAN_POINT('Ctrl Pts',(2.9216945364884,-1.37834004650121,10.3504624208976));
#251255=CARTESIAN_POINT('Ctrl Pts',(2.81906256051531,-1.57764868651717,
10.3355151470663));
#251256=CARTESIAN_POINT('Ctrl Pts',(2.62172777414765,-1.87919798964267,
10.3111615725701));
#251257=CARTESIAN_POINT('Ctrl Pts',(2.53958033139242,-1.98881287674083,
10.301894887446));
#251258=CARTESIAN_POINT('Ctrl Pts',(2.42184087033945,-2.12668300612386,
10.2899373943055));
#251259=CARTESIAN_POINT('Ctrl Pts',(2.39227366546494,-2.15988909330625,
10.2870327490336));
#251260=CARTESIAN_POINT('Ctrl Pts',(2.34084151343558,-2.21529870969672,
10.2821580120184));
#251261=CARTESIAN_POINT('Ctrl Pts',(2.31932486032319,-2.23781583720903,
10.2801688567827));
#251262=CARTESIAN_POINT('Ctrl Pts',(2.28799675801897,-2.26966328647004,
10.2773481260236));
#251263=CARTESIAN_POINT('Ctrl Pts',(2.2784483766346,-2.27924847457159,10.2764981878265));
#251264=CARTESIAN_POINT('Ctrl Pts',(2.26171674059134,-2.29583438897668,
10.2750262332787));
#251265=CARTESIAN_POINT('Ctrl Pts',(2.25456074653232,-2.30286213372949,
10.2744021593844));
#251266=CARTESIAN_POINT('Ctrl Pts',(2.23918887936418,-2.31781817038377,
10.2730733464969));
#251267=CARTESIAN_POINT('Ctrl Pts',(2.23096358669727,-2.32573631190899,
10.2723693644935));
#251268=CARTESIAN_POINT('Ctrl Pts',(2.20838220792933,-2.34724441753236,
10.270455254444));
#251269=CARTESIAN_POINT('Ctrl Pts',(2.19394262994782,-2.36074651594631,
10.2692515641771));
#251270=CARTESIAN_POINT('Ctrl Pts',(2.11598168216531,-2.43231274509408,
10.2628544096569));
#251271=CARTESIAN_POINT('Ctrl Pts',(2.05027256359547,-2.48795273277165,
10.2578192561318));
#251272=CARTESIAN_POINT('Ctrl Pts',(1.84571755794919,-2.64754648481533,
10.2429126182326));
#251273=CARTESIAN_POINT('Ctrl Pts',(1.7006369409604,-2.74299392040663,10.233328347952));
#251274=CARTESIAN_POINT('Ctrl Pts',(1.40431094221198,-2.90535521079721,
10.2143422596809));
#251275=CARTESIAN_POINT('Ctrl Pts',(1.25422093900046,-2.97323049176442,
10.2049826725908));
#251276=CARTESIAN_POINT('Ctrl Pts',(1.05853854124332,-3.04426072922567,
10.1926463922301));
#251277=CARTESIAN_POINT('Ctrl Pts',(1.01716378329628,-3.05833366342234,
10.1900319395905));
#251278=CARTESIAN_POINT('Ctrl Pts',(0.954568151810045,-3.07821382147114,
10.1860613584832));
#251279=CARTESIAN_POINT('Ctrl Pts',(0.933552105159202,-3.08465251160618,
10.1847257406609));
#251280=CARTESIAN_POINT('Ctrl Pts',(0.895487776857363,-3.09588966478814,
10.1823013871994));
#251281=CARTESIAN_POINT('Ctrl Pts',(0.87846255451134,-3.10076356656255,
10.1812151439832));
#251282=CARTESIAN_POINT('Ctrl Pts',(0.841818634359222,-3.11092780497337,
10.1788727545809));
#251283=CARTESIAN_POINT('Ctrl Pts',(0.822188421630395,-3.11617338898441,
10.1776152191118));
#251284=CARTESIAN_POINT('Ctrl Pts',(0.76893714291606,-3.12986499718136,
10.1741959590729));
#251285=CARTESIAN_POINT('Ctrl Pts',(0.735228024672672,-3.13795456190473,
10.1720229780966));
#251286=CARTESIAN_POINT('Ctrl Pts',(0.526306521153107,-3.18454072381635,
10.1584984431316));
#251287=CARTESIAN_POINT('Ctrl Pts',(0.348290400572125,-3.20888985430075,
10.1467024106685));
#251288=CARTESIAN_POINT('Ctrl Pts',(0.0436929198071317,-3.22490365054046,
10.1262263081205));
#251289=CARTESIAN_POINT('Ctrl Pts',(-0.0820899289610667,-3.22415462304401,
10.1176942664966));
#251290=CARTESIAN_POINT('Ctrl Pts',(-0.327726135818035,-3.20830587946999,
10.1011263811008));
#251291=CARTESIAN_POINT('Ctrl Pts',(-0.447430289492116,-3.19381316820066,
10.0930982363304));
#251292=CARTESIAN_POINT('Ctrl Pts',(-0.593596385922959,-3.16773480216498,
10.0835519469774));
#251293=CARTESIAN_POINT('Ctrl Pts',(-0.621077384967557,-3.16246161236671,
10.0817686352589));
#251294=CARTESIAN_POINT('Ctrl Pts',(-0.661185426586292,-3.15422247818178,
10.0791861887806));
#251295=CARTESIAN_POINT('Ctrl Pts',(-0.673867993175267,-3.15153733142956,
10.0783725744861));
#251296=CARTESIAN_POINT('Ctrl Pts',(-0.696274348090948,-3.1466520261773,
10.0769408551081));
#251297=CARTESIAN_POINT('Ctrl Pts',(-0.706004553888015,-3.14448318814055,
10.0763210446372));
#251298=CARTESIAN_POINT('Ctrl Pts',(-0.72720402078029,-3.13965451602341,
10.0749749173961));
#251299=CARTESIAN_POINT('Ctrl Pts',(-0.738668887051276,-3.13697696090308,
10.0742496023513));
#251300=CARTESIAN_POINT('Ctrl Pts',(-0.770883027783834,-3.12926712811156,
10.0722185013975));
#251301=CARTESIAN_POINT('Ctrl Pts',(-0.791597755525732,-3.12409129988145,
10.0709205127041));
#251302=CARTESIAN_POINT('Ctrl Pts',(-0.934847582026179,-3.0867822427956,
10.0619908996144));
#251303=CARTESIAN_POINT('Ctrl Pts',(-1.05546026659361,-3.04765079909803,
10.0547067957531));
#251304=CARTESIAN_POINT('Ctrl Pts',(-1.30908287551892,-2.94849491488588,
10.0392999032399));
#251305=CARTESIAN_POINT('Ctrl Pts',(-1.4409503543999,-2.88634433468575,
10.0312281416478));
#251306=CARTESIAN_POINT('Ctrl Pts',(-1.6877552236746,-2.74887951241976,
10.0153116396247));
#251307=CARTESIAN_POINT('Ctrl Pts',(-1.80296991483538,-2.67472439604047,
10.0074985531772));
#251308=CARTESIAN_POINT('Ctrl Pts',(-1.95451730268703,-2.5629331975319,
9.99639704328105));
#251309=CARTESIAN_POINT('Ctrl Pts',(-1.99518045102844,-2.5314065249193,
9.99333072051505));
#251310=CARTESIAN_POINT('Ctrl Pts',(-2.05323296890008,-2.48412975146782,
9.98881324198336));
#251311=CARTESIAN_POINT('Ctrl Pts',(-2.07123376886894,-2.46914091885184,
9.98739219041687));
#251312=CARTESIAN_POINT('Ctrl Pts',(-2.10267298615895,-2.44237651827957,
9.98487329441997));
#251313=CARTESIAN_POINT('Ctrl Pts',(-2.11617999526046,-2.43068281585747,
9.98377880798886));
#251314=CARTESIAN_POINT('Ctrl Pts',(-2.1442116696344,-2.40600362503734,
9.98148106103961));
#251315=CARTESIAN_POINT('Ctrl Pts',(-2.1587171681153,-2.39299755318181,
9.98027697145764));
#251316=CARTESIAN_POINT('Ctrl Pts',(-2.19650898930915,-2.35848900695116,
9.97709944920224));
#251317=CARTESIAN_POINT('Ctrl Pts',(-2.21959712401429,-2.33677355101574,
9.97511709259614));
#251318=CARTESIAN_POINT('Ctrl Pts',(-2.32074258419305,-2.23879002540763,
9.96624484796009));
#251319=CARTESIAN_POINT('Ctrl Pts',(-2.39520908676409,-2.1589339924646,
9.95920095065294));
#251320=CARTESIAN_POINT('Ctrl Pts',(-2.59846943925162,-1.91747763768109,
9.93842971405541));
#251321=CARTESIAN_POINT('Ctrl Pts',(-2.7159618324353,-1.74708386750235,
9.92436463276535));
#251322=CARTESIAN_POINT('Ctrl Pts',(-2.87315530136083,-1.4644993501895,
9.90261469915405));
#251323=CARTESIAN_POINT('Ctrl Pts',(-2.92438204142517,-1.35932867975168,
9.8948350334685));
#251324=CARTESIAN_POINT('Ctrl Pts',(-2.98049777336008,-1.22617762563944,
9.88554819303935));
#251325=CARTESIAN_POINT('Ctrl Pts',(-2.99088472801249,-1.20061950972758,
9.88379050164617));
#251326=CARTESIAN_POINT('Ctrl Pts',(-3.00564195195522,-1.16292741397468,
9.88123793143092));
#251327=CARTESIAN_POINT('Ctrl Pts',(-3.01026933372748,-1.15089628774862,
9.88042902735747));
#251328=CARTESIAN_POINT('Ctrl Pts',(-3.01834520826996,-1.1295171667381,
9.87900239980745));
#251329=CARTESIAN_POINT('Ctrl Pts',(-3.02182268579938,-1.12018056157456,
9.87838301686273));
#251330=CARTESIAN_POINT('Ctrl Pts',(-3.02933335543215,-1.09972580700982,
9.87703407888066));
#251331=CARTESIAN_POINT('Ctrl Pts',(-3.03334868894276,-1.08860147458359,
9.87630556116738));
#251332=CARTESIAN_POINT('Ctrl Pts',(-3.04452129425325,-1.05710634739461,
9.87425670802984));
#251333=CARTESIAN_POINT('Ctrl Pts',(-3.0515353666761,-1.03668495866133,
9.87294438635643));
#251334=CARTESIAN_POINT('Ctrl Pts',(-3.10365722453508,-0.879818686650472,
9.86297600660099));
#251335=CARTESIAN_POINT('Ctrl Pts',(-3.13980374757823,-0.740548013958625,
9.85476901781731));
#251336=CARTESIAN_POINT('Ctrl Pts',(-3.20380124348284,-0.402411361627577,
9.83538110810482));
#251337=CARTESIAN_POINT('Ctrl Pts',(-3.22262044088577,-0.202468119866952,
9.82432452570155));
#251338=CARTESIAN_POINT('Ctrl Pts',(-3.222749777796,-0.00138189335566572,
9.81276902482661));
#251339=CARTESIAN_POINT('Ctrl Pts',(-3.22275,-0.000690945209040148,9.81272931446407));
#251340=CARTESIAN_POINT('Ctrl Pts',(-3.22275,1.94885615773067E-11,9.8126895994942));
#251341=CARTESIAN_POINT('Ctrl Pts',(-3.22275,-1.85372951893938E-11,9.562284768011));
#251342=CARTESIAN_POINT('Ctrl Pts',(-3.22274999999945,-0.0962321027425494,
9.56782198041187));
#251343=CARTESIAN_POINT('Ctrl Pts',(-3.21843979371273,-0.192408777702062,
9.57345181231487));
#251344=CARTESIAN_POINT('Ctrl Pts',(-3.20707792591733,-0.318932905869064,
9.58105853626993));
#251345=CARTESIAN_POINT('Ctrl Pts',(-3.2038820531936,-0.349580766234551,
9.58291653836422));
#251346=CARTESIAN_POINT('Ctrl Pts',(-3.19793787038363,-0.399617562483878,
9.58597732843694));
#251347=CARTESIAN_POINT('Ctrl Pts',(-3.19545139346795,-0.419036018576571,
9.58717192763092));
#251348=CARTESIAN_POINT('Ctrl Pts',(-3.19028530996339,-0.456657074450286,
9.58949996821545));
#251349=CARTESIAN_POINT('Ctrl Pts',(-3.18762643730845,-0.474861786908061,
9.59063271783305));
#251350=CARTESIAN_POINT('Ctrl Pts',(-3.18101618282989,-0.517560782271938,
9.59330462655044));
#251351=CARTESIAN_POINT('Ctrl Pts',(-3.17693756748288,-0.542033907005987,
9.59484772100777));
#251352=CARTESIAN_POINT('Ctrl Pts',(-3.16243381297604,-0.623265631179853,
9.60000966123524));
#251353=CARTESIAN_POINT('Ctrl Pts',(-3.15076730538574,-0.679788479129602,
9.60366700673457));
#251354=CARTESIAN_POINT('Ctrl Pts',(-3.0744917566204,-1.00496895145065,
9.62510002685287));
#251355=CARTESIAN_POINT('Ctrl Pts',(-2.97706596121778,-1.26470985862877,
9.64392310907279));
#251356=CARTESIAN_POINT('Ctrl Pts',(-2.7900972148905,-1.6176032882052,9.67076539476172));
#251357=CARTESIAN_POINT('Ctrl Pts',(-2.7262474916412,-1.72303908715321,
9.67894651569399));
#251358=CARTESIAN_POINT('Ctrl Pts',(-2.64430881096152,-1.84233904030726,
9.68819216376206));
#251359=CARTESIAN_POINT('Ctrl Pts',(-2.6319264157136,-1.85998538353255,
9.68955932979151));
#251360=CARTESIAN_POINT('Ctrl Pts',(-2.61239176967226,-1.88723877097242,
9.69166850935367));
#251361=CARTESIAN_POINT('Ctrl Pts',(-2.60536170788986,-1.89693208067139,
9.69241822870606));
#251362=CARTESIAN_POINT('Ctrl Pts',(-2.59223923766178,-1.91481525942628,
9.69380018551293));
#251363=CARTESIAN_POINT('Ctrl Pts',(-2.58616191181144,-1.92301542185027,
9.69443335660544));
#251364=CARTESIAN_POINT('Ctrl Pts',(-2.57202205498927,-1.94190612223838,
9.69589097047663));
#251365=CARTESIAN_POINT('Ctrl Pts',(-2.56393175221499,-1.95257543349369,
9.69671349454999));
#251366=CARTESIAN_POINT('Ctrl Pts',(-2.53788522016222,-1.98648398678553,
9.69932636638615));
#251367=CARTESIAN_POINT('Ctrl Pts',(-2.51967719653696,-2.00952904473933,
9.7011002851901));
#251368=CARTESIAN_POINT('Ctrl Pts',(-2.41838645004665,-2.13418638149031,
9.71070550690763));
#251369=CARTESIAN_POINT('Ctrl Pts',(-2.32946236532251,-2.23090939190069,
9.71819638101887));
#251370=CARTESIAN_POINT('Ctrl Pts',(-2.06713733959746,-2.4833976731781,
9.7387150502813));
#251371=CARTESIAN_POINT('Ctrl Pts',(-1.88240604270644,-2.6261882417984,
9.75152986706854));
#251372=CARTESIAN_POINT('Ctrl Pts',(-1.62131331104691,-2.78618911293639,
9.76934133879545));
#251373=CARTESIAN_POINT('Ctrl Pts',(-1.55743264850188,-2.82239419473062,
9.77367250458529));
#251374=CARTESIAN_POINT('Ctrl Pts',(-1.46760410592529,-2.86932689611946,
9.77975833009877));
#251375=CARTESIAN_POINT('Ctrl Pts',(-1.44266664334263,-2.88194578898451,
9.78144725880781));
#251376=CARTESIAN_POINT('Ctrl Pts',(-1.40222817996101,-2.90175214026934,
9.78418658944015));
#251377=CARTESIAN_POINT('Ctrl Pts',(-1.38682830694376,-2.90914361657339,
9.78522991609857));
#251378=CARTESIAN_POINT('Ctrl Pts',(-1.35464247041182,-2.92427820924333,
9.78741110559755));
#251379=CARTESIAN_POINT('Ctrl Pts',(-1.33784722831536,-2.93200000664033,
9.78854964927417));
#251380=CARTESIAN_POINT('Ctrl Pts',(-1.29787556437565,-2.94996246959092,
9.79126059027445));
#251381=CARTESIAN_POINT('Ctrl Pts',(-1.27464324029334,-2.96007501666025,
9.79283725521905));
#251382=CARTESIAN_POINT('Ctrl Pts',(-1.19510912032014,-2.99358463031365,
9.79823952638052));
#251383=CARTESIAN_POINT('Ctrl Pts',(-1.13826647228302,-3.01565637750549,
9.80210871915992));
#251384=CARTESIAN_POINT('Ctrl Pts',(-0.997518243332143,-3.06576194884772,
9.81171398015589));
#251385=CARTESIAN_POINT('Ctrl Pts',(-0.913022122182944,-3.09197792081681,
9.81750223093712));
#251386=CARTESIAN_POINT('Ctrl Pts',(-0.696752763617842,-3.14943990624143,
9.83234551167564));
#251387=CARTESIAN_POINT('Ctrl Pts',(-0.563891681021471,-3.1759185617064,
9.84149454060881));
#251388=CARTESIAN_POINT('Ctrl Pts',(-0.381604161391807,-3.20044645960606,
9.85392113059384));
#251389=CARTESIAN_POINT('Ctrl Pts',(-0.333299740472735,-3.20583696873979,
9.85720127972051));
#251390=CARTESIAN_POINT('Ctrl Pts',(-0.163201604872059,-3.2209327587457,
9.86867678295111));
#251391=CARTESIAN_POINT('Ctrl Pts',(-0.040982986919448,-3.22480528078886,
9.87679033448565));
#251392=CARTESIAN_POINT('Ctrl Pts',(0.102695183209003,-3.22118531498955,
9.88597150634783));
#251393=CARTESIAN_POINT('Ctrl Pts',(0.124213765143733,-3.22042732133966,
9.88733703168111));
#251394=CARTESIAN_POINT('Ctrl Pts',(0.157679791043669,-3.21891253141349,
9.88944422854073));
#251395=CARTESIAN_POINT('Ctrl Pts',(0.169632911883861,-3.21830475363847,
9.89019358375382));
#251396=CARTESIAN_POINT('Ctrl Pts',(0.191774043212813,-3.21705524903515,
9.89157522140595));
#251397=CARTESIAN_POINT('Ctrl Pts',(0.20196245435659,-3.21643170761852,
9.89220843358008));
#251398=CARTESIAN_POINT('Ctrl Pts',(0.225516870474322,-3.21487778986251,
9.8936665945339));
#251399=CARTESIAN_POINT('Ctrl Pts',(0.238880217683845,-3.21391246284122,
9.89448961933538));
#251400=CARTESIAN_POINT('Ctrl Pts',(0.281560742246336,-3.21056167478276,
9.89710576086434));
#251401=CARTESIAN_POINT('Ctrl Pts',(0.310852329389705,-3.20785811484842,
9.89888239083612));
#251402=CARTESIAN_POINT('Ctrl Pts',(0.471069344734558,-3.19085511220588,
9.90851677304215));
#251403=CARTESIAN_POINT('Ctrl Pts',(0.601073851334395,-3.16893989396507,
9.91603182619867));
#251404=CARTESIAN_POINT('Ctrl Pts',(0.957418243772569,-3.08614240151789,
9.9366464381391));
#251405=CARTESIAN_POINT('Ctrl Pts',(1.17898751756106,-3.00847290682051,
9.94953274391293));
#251406=CARTESIAN_POINT('Ctrl Pts',(1.45519285522081,-2.87640800732054,
9.96735325773499));
#251407=CARTESIAN_POINT('Ctrl Pts',(1.51913327412975,-2.84315709117237,
9.97160667169849));
#251408=CARTESIAN_POINT('Ctrl Pts',(1.60607639324364,-2.79417358979463,
9.97760019554757));
#251409=CARTESIAN_POINT('Ctrl Pts',(1.63007280461226,-2.78024279694901,
9.97927722934043));
#251410=CARTESIAN_POINT('Ctrl Pts',(1.66851539246745,-2.75725669674366,
9.98200240627509));
#251411=CARTESIAN_POINT('Ctrl Pts',(1.6830751332866,-2.74839338250801,9.98304361699469));
#251412=CARTESIAN_POINT('Ctrl Pts',(1.71330023562836,-2.72966345903398,
9.98522449255018));
#251413=CARTESIAN_POINT('Ctrl Pts',(1.72895222202218,-2.71977655118953,
9.98636487107372));
#251414=CARTESIAN_POINT('Ctrl Pts',(1.76595778086049,-2.69595268222535,
9.98908781307619));
#251415=CARTESIAN_POINT('Ctrl Pts',(1.78723258214847,-2.68189622961948,
9.99067474674864));
#251416=CARTESIAN_POINT('Ctrl Pts',(1.85965327847774,-2.6328028040623,9.99615234777263));
#251417=CARTESIAN_POINT('Ctrl Pts',(1.90995120648743,-2.59654510273198,
10.0000882650041));
#251418=CARTESIAN_POINT('Ctrl Pts',(2.03104674591429,-2.50382937036233,
10.0098993892052));
#251419=CARTESIAN_POINT('Ctrl Pts',(2.10056774832913,-2.44579747409989,
10.0158297760523));
#251420=CARTESIAN_POINT('Ctrl Pts',(2.26588843881952,-2.29554474566585,
10.0306628071818));
#251421=CARTESIAN_POINT('Ctrl Pts',(2.35860075298049,-2.20017619788263,
10.0396473615428));
#251422=CARTESIAN_POINT('Ctrl Pts',(2.4784402047365,-2.06059754898109,10.0520759032181));
#251423=CARTESIAN_POINT('Ctrl Pts',(2.51079736901623,-2.02104547585121,
10.0555239368598));
#251424=CARTESIAN_POINT('Ctrl Pts',(2.61519800545268,-1.88705144390188,
10.066930955144));
#251425=CARTESIAN_POINT('Ctrl Pts',(2.68296800521044,-1.78938876890679,
10.074810322345));
#251426=CARTESIAN_POINT('Ctrl Pts',(2.75642908178534,-1.6699329534434,10.0837677906333));
#251427=CARTESIAN_POINT('Ctrl Pts',(2.76747935558276,-1.65155545622524,
10.0851276238374));
#251428=CARTESIAN_POINT('Ctrl Pts',(2.78440043881926,-1.6227675519306,10.0872279406126));
#251429=CARTESIAN_POINT('Ctrl Pts',(2.79039794329759,-1.61243283890469,
10.087976031288));
#251430=CARTESIAN_POINT('Ctrl Pts',(2.8013653706757,-1.59328964759626,10.0893505113554));
#251431=CARTESIAN_POINT('Ctrl Pts',(2.80635134471072,-1.58449107754594,
10.0899778695918));
#251432=CARTESIAN_POINT('Ctrl Pts',(2.81783266566948,-1.56400619405702,
10.0914285135592));
#251433=CARTESIAN_POINT('Ctrl Pts',(2.8242967988455,-1.55230277758356,10.0922498450617));
#251434=CARTESIAN_POINT('Ctrl Pts',(2.84467436447653,-1.5148601852987,10.0948549406171));
#251435=CARTESIAN_POINT('Ctrl Pts',(2.85831061651877,-1.48897084421152,
10.0966224127509));
#251436=CARTESIAN_POINT('Ctrl Pts',(2.93068903691992,-1.34689579493752,
10.1061585811498));
#251437=CARTESIAN_POINT('Ctrl Pts',(2.98270803498406,-1.22740630954098,
10.1135921944741));
#251438=CARTESIAN_POINT('Ctrl Pts',(3.10614840340232,-0.889244185296949,
10.1338847828737));
#251439=CARTESIAN_POINT('Ctrl Pts',(3.1616257939694,-0.665606777878812,
10.1465315836843));
#251440=CARTESIAN_POINT('Ctrl Pts',(3.20326648867163,-0.362042963571825,
10.1643242298971));
#251441=CARTESIAN_POINT('Ctrl Pts',(3.21096945487758,-0.285771122407251,
10.1688402451533));
#251442=CARTESIAN_POINT('Ctrl Pts',(3.21779166730246,-0.180946760578022,
10.1751450112857));
#251443=CARTESIAN_POINT('Ctrl Pts',(3.21926192066327,-0.152569829133572,
10.1768614879856));
#251444=CARTESIAN_POINT('Ctrl Pts',(3.22101820945468,-0.107023242221201,
10.1796336647172));
#251445=CARTESIAN_POINT('Ctrl Pts',(3.22154260268476,-0.0898639048995677,
10.1806819548268));
#251446=CARTESIAN_POINT('Ctrl Pts',(3.22234553852381,-0.0542799798824783,
10.1828642698148));
#251447=CARTESIAN_POINT('Ctrl Pts',(3.22260320860138,-0.0358555929495794,
10.1839989017341));
#251448=CARTESIAN_POINT('Ctrl Pts',(3.22283799558696,0.00755435606473961,
10.1866837038063));
#251449=CARTESIAN_POINT('Ctrl Pts',(3.22268257216693,0.0325391646398068,
10.1882379188818));
#251450=CARTESIAN_POINT('Ctrl Pts',(3.22118770750078,0.116281926138336,
10.1934784907794));
#251451=CARTESIAN_POINT('Ctrl Pts',(3.21853155920852,0.17500176722095,10.1972049749834));
#251452=CARTESIAN_POINT('Ctrl Pts',(3.20817876671744,0.317445255741478,
10.2063753762966));
#251453=CARTESIAN_POINT('Ctrl Pts',(3.19880899899056,0.401000790314728,
10.2118654601272));
#251454=CARTESIAN_POINT('Ctrl Pts',(3.16488147802437,0.624305322738541,
10.2268152147687));
#251455=CARTESIAN_POINT('Ctrl Pts',(3.13434645275609,0.762954647294478,
10.2363993817619));
#251456=CARTESIAN_POINT('Ctrl Pts',(3.08350989373429,0.937932153507249,
10.2487103600646));
#251457=CARTESIAN_POINT('Ctrl Pts',(3.07150882078722,0.976516056120752,
10.2514381516863));
#251458=CARTESIAN_POINT('Ctrl Pts',(3.01753466588182,1.13919331200442,10.2629743340372));
#251459=CARTESIAN_POINT('Ctrl Pts',(2.96873745874446,1.26090518525626,10.2716979469752));
#251460=CARTESIAN_POINT('Ctrl Pts',(2.90335492570937,1.39897124631875,10.2814590954967));
#251461=CARTESIAN_POINT('Ctrl Pts',(2.89384958243091,1.41852917696301,10.2828384295427));
#251462=CARTESIAN_POINT('Ctrl Pts',(2.87878527280628,1.44874335037549,10.2849623078064));
#251463=CARTESIAN_POINT('Ctrl Pts',(2.87336362367431,1.4594668338615,10.2857147228123));
#251464=CARTESIAN_POINT('Ctrl Pts',(2.86322834589739,1.47923800304823,10.2870990593185));
#251465=CARTESIAN_POINT('Ctrl Pts',(2.85853170312195,1.48829369971653,10.2877319432777));
#251466=CARTESIAN_POINT('Ctrl Pts',(2.8475993285111,1.50912997370945,10.2891855830152));
#251467=CARTESIAN_POINT('Ctrl Pts',(2.84133343360045,1.52089432465362,10.2900044585259));
#251468=CARTESIAN_POINT('Ctrl Pts',(2.82118688531478,1.55816081400135,10.2925935883113));
#251469=CARTESIAN_POINT('Ctrl Pts',(2.80703409473307,1.58351516783993,10.2943478301863));
#251470=CARTESIAN_POINT('Ctrl Pts',(2.72863369319886,1.71961236355655,10.3037435251637));
#251471=CARTESIAN_POINT('Ctrl Pts',(2.6581666231115,1.82665415449185,10.3110606389115));
#251472=CARTESIAN_POINT('Ctrl Pts',(2.44762265656137,2.1083841273469,10.3308976438504));
#251473=CARTESIAN_POINT('Ctrl Pts',(2.29545567808049,2.27310831168819,10.3432076390063));
#251474=CARTESIAN_POINT('Ctrl Pts',(2.06489095450143,2.47573858532714,10.360973302694));
#251475=CARTESIAN_POINT('Ctrl Pts',(2.00021770514078,2.52827681544219,10.365869229625));
#251476=CARTESIAN_POINT('Ctrl Pts',(1.91013539180736,2.59583504141919,10.3726213964921));
#251477=CARTESIAN_POINT('Ctrl Pts',(1.88644681872817,2.61310066631415,10.3743908708388));
#251478=CARTESIAN_POINT('Ctrl Pts',(1.84680928101333,2.64117094607519,10.3773434491204));
#251479=CARTESIAN_POINT('Ctrl Pts',(1.83099277474013,2.65216023661717,10.3785194806386));
#251480=CARTESIAN_POINT('Ctrl Pts',(1.79974013650502,2.67346172342993,10.3808395965237));
#251481=CARTESIAN_POINT('Ctrl Pts',(1.78431150883124,2.68378362807107,10.3819832551557));
#251482=CARTESIAN_POINT('Ctrl Pts',(1.74724349426358,2.70812156638074,10.3847273046824));
#251483=CARTESIAN_POINT('Ctrl Pts',(1.72552366356987,2.72201217329395,10.3863322467823));
#251484=CARTESIAN_POINT('Ctrl Pts',(1.64945934111924,2.76938178499682,10.3919441145624));
#251485=CARTESIAN_POINT('Ctrl Pts',(1.59429155709696,2.80150407909379,10.395999337042));
#251486=CARTESIAN_POINT('Ctrl Pts',(1.45533017296593,2.87698229408727,10.406182735094));
#251487=CARTESIAN_POINT('Ctrl Pts',(1.37052117316731,2.91833552518431,10.4123717589124));
#251488=CARTESIAN_POINT('Ctrl Pts',(1.10179744717344,3.03506733001694,10.4318583370959));
#251489=CARTESIAN_POINT('Ctrl Pts',(0.912650132228294,3.09720115101598,
10.4454288095991));
#251490=CARTESIAN_POINT('Ctrl Pts',(0.62240769885971,3.16362821774711,10.465325395543));
#251491=CARTESIAN_POINT('Ctrl Pts',(0.524845115619453,3.18126958349547,
10.471855945961));
#251492=CARTESIAN_POINT('Ctrl Pts',(0.40605621806227,3.19713405529047,10.4795044810292));
#251493=CARTESIAN_POINT('Ctrl Pts',(0.385469468073379,3.19968141545888,
10.4808190564944));
#251494=CARTESIAN_POINT('Ctrl Pts',(0.353143426595405,3.20336484315521,
10.4828645937358));
#251495=CARTESIAN_POINT('Ctrl Pts',(0.341420445436577,3.2046354999902,10.4836025649908));
#251496=CARTESIAN_POINT('Ctrl Pts',(0.320529454716142,3.20678394100045,
10.4849105199478));
#251497=CARTESIAN_POINT('Ctrl Pts',(0.311364581027744,3.20768677958702,
10.4854818431183));
#251498=CARTESIAN_POINT('Ctrl Pts',(0.289181766969773,3.20977605615368,
10.486858828219));
#251499=CARTESIAN_POINT('Ctrl Pts',(0.276160326290791,3.21092259526601,
10.4876622852308));
#251500=CARTESIAN_POINT('Ctrl Pts',(0.235571560549808,3.21424770024315,
10.49015264114));
#251501=CARTESIAN_POINT('Ctrl Pts',(0.207982153600756,3.21615077026735,
10.49182520212));
#251502=CARTESIAN_POINT('Ctrl Pts',(0.0652600382944481,3.22415117184827,
10.5003887591813));
#251503=CARTESIAN_POINT('Ctrl Pts',(-0.0501256704311403,3.22442277834251,
10.5070154380644));
#251504=CARTESIAN_POINT('Ctrl Pts',(-0.370147389744503,3.20798794312745,
10.5251568717563));
#251505=CARTESIAN_POINT('Ctrl Pts',(-0.573531612139767,3.17793305548913,
10.5364429856697));
#251506=CARTESIAN_POINT('Ctrl Pts',(-0.880106872551583,3.10222074875802,
10.5545082077002));
#251507=CARTESIAN_POINT('Ctrl Pts',(-0.986085538519319,3.070178075699,10.5609495975644));
#251508=CARTESIAN_POINT('Ctrl Pts',(-1.12053779497783,3.02184578307338,
10.5694938388171));
#251509=CARTESIAN_POINT('Ctrl Pts',(-1.15070949953352,3.01048574519325,
10.5714358292591));
#251510=CARTESIAN_POINT('Ctrl Pts',(-1.19920500772803,2.99139101856716,
10.5745996435991));
#251511=CARTESIAN_POINT('Ctrl Pts',(-1.2176369658357,2.98393583519317,10.5758121647751));
#251512=CARTESIAN_POINT('Ctrl Pts',(-1.25288498278775,2.96929808445124,
10.5781507805286));
#251513=CARTESIAN_POINT('Ctrl Pts',(-1.26971125092759,2.96214199727008,
10.5792759494487));
#251514=CARTESIAN_POINT('Ctrl Pts',(-1.30853648615561,2.94523832154223,
10.5818930364675));
#251515=CARTESIAN_POINT('Ctrl Pts',(-1.33048877789817,2.93538686858313,
10.5833884249102));
#251516=CARTESIAN_POINT('Ctrl Pts',(-1.40070799685684,2.90292533188765,
10.5882233716066));
#251517=CARTESIAN_POINT('Ctrl Pts',(-1.44852302056825,2.87936432165036,
10.5915950388468));
#251518=CARTESIAN_POINT('Ctrl Pts',(-1.6288425468457,2.78488296833156,10.6046232451472));
#251519=CARTESIAN_POINT('Ctrl Pts',(-1.75689781451043,2.70591969534315,
10.6145469710705));
#251520=CARTESIAN_POINT('Ctrl Pts',(-2.02020092168454,2.51696763540905,
10.6363009701347));
#251521=CARTESIAN_POINT('Ctrl Pts',(-2.15300324799859,2.40435334144088,
10.6481544889736));
#251522=CARTESIAN_POINT('Ctrl Pts',(-2.33579508348467,2.22200239524783,
10.6653241976289));
#251523=CARTESIAN_POINT('Ctrl Pts',(-2.39315833723716,2.16009929588233,
10.6708546190297));
#251524=CARTESIAN_POINT('Ctrl Pts',(-2.4611460173667,2.08069327405424,10.6775195453369));
#251525=CARTESIAN_POINT('Ctrl Pts',(-2.47411772943321,2.0652519768859,10.6787964530447));
#251526=CARTESIAN_POINT('Ctrl Pts',(-2.49428642011847,2.04078075582713,
10.6807888258874));
#251527=CARTESIAN_POINT('Ctrl Pts',(-2.50158103330588,2.03183246907789,
10.6815109044545));
#251528=CARTESIAN_POINT('Ctrl Pts',(-2.51529060975761,2.01482920752362,
10.6828704846155));
#251529=CARTESIAN_POINT('Ctrl Pts',(-2.52171505660054,2.00678268945641,
10.6835086157571));
#251530=CARTESIAN_POINT('Ctrl Pts',(-2.53686384419113,1.98762145148082,
10.6850160190314));
#251531=CARTESIAN_POINT('Ctrl Pts',(-2.54555381481949,1.97647994960083,
10.6858829055886));
#251532=CARTESIAN_POINT('Ctrl Pts',(-2.5746759340121,1.93863149979293,10.6887968351944));
#251533=CARTESIAN_POINT('Ctrl Pts',(-2.59476401409998,1.91166110162229,
10.6908216864322));
#251534=CARTESIAN_POINT('Ctrl Pts',(-2.64309395920673,1.84460715484574,
10.6957439247588));
#251535=CARTESIAN_POINT('Ctrl Pts',(-2.67085087359908,1.80418328172941,
10.6986156427719));
#251536=CARTESIAN_POINT('Ctrl Pts',(-2.79449639261705,1.61500059957039,
10.7116973580481));
#251537=CARTESIAN_POINT('Ctrl Pts',(-2.87895610419706,1.45912878470321,
10.721493574949));
#251538=CARTESIAN_POINT('Ctrl Pts',(-3.00535912151205,1.1716314202764,10.7391169766518));
#251539=CARTESIAN_POINT('Ctrl Pts',(-3.05246063470123,1.04277684821285,
10.7468691586429));
#251540=CARTESIAN_POINT('Ctrl Pts',(-3.11085676321661,0.844696786475436,
10.7589062817746));
#251541=CARTESIAN_POINT('Ctrl Pts',(-3.12833864452524,0.777456606934578,
10.7630109678197));
#251542=CARTESIAN_POINT('Ctrl Pts',(-3.14965732297129,0.683025983857816,
10.7688275990454));
#251543=CARTESIAN_POINT('Ctrl Pts',(-3.15534085936503,0.65626956232807,
10.7704813878463));
#251544=CARTESIAN_POINT('Ctrl Pts',(-3.16399840365401,0.612796711582066,
10.7731789624255));
#251545=CARTESIAN_POINT('Ctrl Pts',(-3.16718217686836,0.596123099239622,
10.7742160920858));
#251546=CARTESIAN_POINT('Ctrl Pts',(-3.17357310110557,0.561156169897997,
10.776396683289));
#251547=CARTESIAN_POINT('Ctrl Pts',(-3.17675413072964,0.542858770945003,
10.7775409246045));
#251548=CARTESIAN_POINT('Ctrl Pts',(-3.18277267131403,0.50637386823863,
10.7798292443499));
#251549=CARTESIAN_POINT('Ctrl Pts',(-3.18561286102506,0.488187514195531,
10.7809731913038));
#251550=CARTESIAN_POINT('Ctrl Pts',(-3.19193261906208,0.445314739964485,
10.7836780628135));
#251551=CARTESIAN_POINT('Ctrl Pts',(-3.1952817954966,0.420610573029445,
10.7852429840813));
#251552=CARTESIAN_POINT('Ctrl Pts',(-3.21460151418605,0.264521413500904,
10.7951720862643));
#251553=CARTESIAN_POINT('Ctrl Pts',(-3.22275000000299,0.132315334174674,
10.8037745307319));
#251554=CARTESIAN_POINT('Ctrl Pts',(-3.22275,-7.27048976578715E-11,10.8125553006127));
#251555=CARTESIAN_POINT('Origin',(0.,0.,-2.31077344927308));
#251556=CARTESIAN_POINT('',(-3.22275,1.56756299712326E-10,12.3117125106066));
#251557=CARTESIAN_POINT('',(-3.22275,-3.23896726357594E-13,12.0672299157825));
#251558=CARTESIAN_POINT('',(-3.22275,-3.50678552687464E-13,-2.31077344927308));
#251559=CARTESIAN_POINT('',(-3.22274985281522,-0.000974001778823583,11.0579144994549));
#251560=CARTESIAN_POINT('Ctrl Pts',(-3.22275,1.56756299712326E-10,12.3117125106066));
#251561=CARTESIAN_POINT('Ctrl Pts',(-3.22274999999995,0.000963693077442329,
12.3116478163493));
#251562=CARTESIAN_POINT('Ctrl Pts',(-3.22274956776502,0.00192739439762696,
12.3115831158696));
#251563=CARTESIAN_POINT('Ctrl Pts',(-3.2225911459169,0.178522212106079,
12.2997259502982));
#251564=CARTESIAN_POINT('Ctrl Pts',(-3.20807700117422,0.35384475023305,
12.2877455189971));
#251565=CARTESIAN_POINT('Ctrl Pts',(-3.1657934191203,0.608884374812476,
12.2705632833884));
#251566=CARTESIAN_POINT('Ctrl Pts',(-3.14908513252086,0.690111124929629,
12.2651324203364));
#251567=CARTESIAN_POINT('Ctrl Pts',(-3.12452696344479,0.789835988465645,
12.2585863864486));
#251568=CARTESIAN_POINT('Ctrl Pts',(-3.11961505580837,0.809018901392957,
12.2573328889204));
#251569=CARTESIAN_POINT('Ctrl Pts',(-3.1116201763617,0.839086024001066,
12.2553784275076));
#251570=CARTESIAN_POINT('Ctrl Pts',(-3.10865626706594,0.85000099996604,
12.2546710538948));
#251571=CARTESIAN_POINT('Ctrl Pts',(-3.10294828711516,0.870592119491925,
12.2533409293721));
#251572=CARTESIAN_POINT('Ctrl Pts',(-3.10021638921003,0.880271011321753,
12.252717556468));
#251573=CARTESIAN_POINT('Ctrl Pts',(-3.09364747624946,0.903134203437649,
12.2512491943078));
#251574=CARTESIAN_POINT('Ctrl Pts',(-3.08977144978147,0.916306990302155,
12.250406438283));
#251575=CARTESIAN_POINT('Ctrl Pts',(-3.07648864362384,0.960406208132865,
12.2475947796619));
#251576=CARTESIAN_POINT('Ctrl Pts',(-3.06670047045955,0.991216859271332,
12.2456463876615));
#251577=CARTESIAN_POINT('Ctrl Pts',(-3.04162997563112,1.06620314858394,
12.2409319855267));
#251578=CARTESIAN_POINT('Ctrl Pts',(-3.02584673334668,1.11020449752553,
12.2381892520277));
#251579=CARTESIAN_POINT('Ctrl Pts',(-2.95540438051979,1.29391040658139,
12.2267781331871));
#251580=CARTESIAN_POINT('Ctrl Pts',(-2.89198062831041,1.43006053000821,
12.2184125530114));
#251581=CARTESIAN_POINT('Ctrl Pts',(-2.71968753645359,1.74117591139875,
12.198504724398));
#251582=CARTESIAN_POINT('Ctrl Pts',(-2.603103123981,1.91108243737097,12.1869564146417));
#251583=CARTESIAN_POINT('Ctrl Pts',(-2.44216990261269,2.10332121276743,
12.172114452214));
#251584=CARTESIAN_POINT('Ctrl Pts',(-2.41248030602323,2.1373096247501,12.1694166236801));
#251585=CARTESIAN_POINT('Ctrl Pts',(-2.36709696518064,2.18711336859659,
12.1653446596141));
#251586=CARTESIAN_POINT('Ctrl Pts',(-2.35193629140182,2.20340839898983,
12.1639926702756));
#251587=CARTESIAN_POINT('Ctrl Pts',(-2.32439657542084,2.23240061868887,
12.1615506981579));
#251588=CARTESIAN_POINT('Ctrl Pts',(-2.31207912042537,2.2451552470456,12.1604633731655));
#251589=CARTESIAN_POINT('Ctrl Pts',(-2.28555588992159,2.27217010190448,
12.1581319648365));
#251590=CARTESIAN_POINT('Ctrl Pts',(-2.27132056528108,2.28640013088012,
12.1568866148365));
#251591=CARTESIAN_POINT('Ctrl Pts',(-2.2321866287441,2.32479336208288,12.1534785066404));
#251592=CARTESIAN_POINT('Ctrl Pts',(-2.20703017992866,2.34868877395634,
12.1513043472628));
#251593=CARTESIAN_POINT('Ctrl Pts',(-2.04525566270625,2.49745959525713,
12.1374221888023));
#251594=CARTESIAN_POINT('Ctrl Pts',(-1.89849991118504,2.61075730102037,
12.1252383884002));
#251595=CARTESIAN_POINT('Ctrl Pts',(-1.58955625604591,2.80938496431507,
12.1005604558572));
#251596=CARTESIAN_POINT('Ctrl Pts',(-1.42817162976701,2.89476424771179,
12.088121658283));
#251597=CARTESIAN_POINT('Ctrl Pts',(-1.1927814290735,2.99479439869667,12.0711870998833));
#251598=CARTESIAN_POINT('Ctrl Pts',(-1.12415887734022,3.02122319403437,
12.0663883533706));
#251599=CARTESIAN_POINT('Ctrl Pts',(-1.03659271820144,3.05155039030755,
12.0604867475294));
#251600=CARTESIAN_POINT('Ctrl Pts',(-1.01844215192525,3.05765594407239,
12.0592752926703));
#251601=CARTESIAN_POINT('Ctrl Pts',(-0.989621448227486,3.06706564511141,
12.0573715088908));
#251602=CARTESIAN_POINT('Ctrl Pts',(-0.978987021674755,3.07047662462741,
12.0566732910213));
#251603=CARTESIAN_POINT('Ctrl Pts',(-0.958699919408675,3.0768675747511,
12.0553496844724));
#251604=CARTESIAN_POINT('Ctrl Pts',(-0.949050761282024,3.07985750687117,
12.0547237623751));
#251605=CARTESIAN_POINT('Ctrl Pts',(-0.925968819948526,3.08689100704529,
12.053234853844));
#251606=CARTESIAN_POINT('Ctrl Pts',(-0.912523229581137,3.09089238198121,
12.052374271049));
#251607=CARTESIAN_POINT('Ctrl Pts',(-0.866279992821032,3.10432619972791,
12.0494361774026));
#251608=CARTESIAN_POINT('Ctrl Pts',(-0.833357702142755,3.11332576655933,
12.0473817682768));
#251609=CARTESIAN_POINT('Ctrl Pts',(-0.751572086348426,3.13429212535857,
12.0423560900462));
#251610=CARTESIAN_POINT('Ctrl Pts',(-0.702558707112971,3.14564134884796,
12.0394123172423));
#251611=CARTESIAN_POINT('Ctrl Pts',(-0.483827117064786,3.19092147106733,
12.0264964483732));
#251612=CARTESIAN_POINT('Ctrl Pts',(-0.311796114549627,3.21229811272843,
12.0169122705348));
#251613=CARTESIAN_POINT('Ctrl Pts',(0.0540203983025983,3.22807620826352,
11.9963757628994));
#251614=CARTESIAN_POINT('Ctrl Pts',(0.247245864476833,3.21904503792961,
11.9854231697317));
#251615=CARTESIAN_POINT('Ctrl Pts',(0.472968393235273,3.18804480678933,
11.9718341534057));
#251616=CARTESIAN_POINT('Ctrl Pts',(0.50736743638302,3.18275147242569,11.969742188926));
#251617=CARTESIAN_POINT('Ctrl Pts',(0.561733342691843,3.17348189353023,
11.9663994488008));
#251618=CARTESIAN_POINT('Ctrl Pts',(0.581760428228291,3.16987167747703,
11.965160176046));
#251619=CARTESIAN_POINT('Ctrl Pts',(0.619146348702774,3.16276601533336,
11.9628313834419));
#251620=CARTESIAN_POINT('Ctrl Pts',(0.636513243754918,3.15931668873031,
11.9617433606346));
#251621=CARTESIAN_POINT('Ctrl Pts',(0.675331955683889,3.15127364286836,
11.9592970466123));
#251622=CARTESIAN_POINT('Ctrl Pts',(0.696766904098041,3.14660367159537,
11.9579363801263));
#251623=CARTESIAN_POINT('Ctrl Pts',(0.760541897275907,3.132025601941,11.953857774991));
#251624=CARTESIAN_POINT('Ctrl Pts',(0.802729502317106,3.12147936094992,
11.95111974325));
#251625=CARTESIAN_POINT('Ctrl Pts',(1.00176272456347,3.06742253648839,11.9380060128546));
#251626=CARTESIAN_POINT('Ctrl Pts',(1.15535706837004,3.01292990172172,11.9272861544259));
#251627=CARTESIAN_POINT('Ctrl Pts',(1.45927209187229,2.87843939230919,11.9049853199311));
#251628=CARTESIAN_POINT('Ctrl Pts',(1.60871915080358,2.79766163874941,11.8934216892821));
#251629=CARTESIAN_POINT('Ctrl Pts',(1.82779927317281,2.65586362669371,11.8760246452035));
#251630=CARTESIAN_POINT('Ctrl Pts',(1.9023472409322,2.60298671009137,11.8700208570501));
#251631=CARTESIAN_POINT('Ctrl Pts',(1.99042062380375,2.53470833995214,11.8629135939407));
#251632=CARTESIAN_POINT('Ctrl Pts',(2.00617269266835,2.522259265515,11.8616419144701));
#251633=CARTESIAN_POINT('Ctrl Pts',(2.03075315142967,2.50245702289312,11.8596580223799));
#251634=CARTESIAN_POINT('Ctrl Pts',(2.03966002531584,2.49520269799938,11.8589392551099));
#251635=CARTESIAN_POINT('Ctrl Pts',(2.05548293932161,2.48217417050535,11.8576628630791));
#251636=CARTESIAN_POINT('Ctrl Pts',(2.06241359809402,2.47641855899643,11.8571039811424));
#251637=CARTESIAN_POINT('Ctrl Pts',(2.07914194694156,2.4624074528448,11.8557553670191));
#251638=CARTESIAN_POINT('Ctrl Pts',(2.08891465608434,2.45412250545793,11.854967765569));
#251639=CARTESIAN_POINT('Ctrl Pts',(2.119256517291,2.42808721332919,11.8525223286303));
#251640=CARTESIAN_POINT('Ctrl Pts',(2.13965136253323,2.41013440656525,11.8508783965027));
#251641=CARTESIAN_POINT('Ctrl Pts',(2.24381412457637,2.31607939324094,11.8424665181471));
#251642=CARTESIAN_POINT('Ctrl Pts',(2.32376580993048,2.23585398078988,11.8359548242589));
#251643=CARTESIAN_POINT('Ctrl Pts',(2.40244253265057,2.14811756592693,11.8292788459993));
#251644=CARTESIAN_POINT('Ctrl Pts',(2.40554054023783,2.14464773545374,11.8290155124919));
#251645=CARTESIAN_POINT('Ctrl Pts',(2.54588581002622,1.98677153598284,11.8170646190865));
#251646=CARTESIAN_POINT('Ctrl Pts',(2.66797455915245,1.81953522875919,11.80570142103));
#251647=CARTESIAN_POINT('Ctrl Pts',(2.82864427799684,1.54813664889311,11.7876452220797));
#251648=CARTESIAN_POINT('Ctrl Pts',(2.87928981638901,1.45177210694855,11.7813066169731));
#251649=CARTESIAN_POINT('Ctrl Pts',(2.93825403024683,1.32430474105206,11.7729045932504));
#251650=CARTESIAN_POINT('Ctrl Pts',(2.9511208523704,1.29537847807131,11.7709970616652));
#251651=CARTESIAN_POINT('Ctrl Pts',(2.97121093874652,1.24835987402934,11.7678928105612));
#251652=CARTESIAN_POINT('Ctrl Pts',(2.97870014408853,1.23038296616007,11.7667051050945));
#251653=CARTESIAN_POINT('Ctrl Pts',(2.9927474593539,1.19578404125955,11.7644170978832));
#251654=CARTESIAN_POINT('Ctrl Pts',(2.99933117314083,1.17917315197769,11.7633177059887));
#251655=CARTESIAN_POINT('Ctrl Pts',(3.01423203105586,1.14064557076962,11.7607652326548));
#251656=CARTESIAN_POINT('Ctrl Pts',(3.0224487766503,1.11869137900034,11.7593088783283));
#251657=CARTESIAN_POINT('Ctrl Pts',(3.04796527117049,1.04818043280959,11.75462450893));
#251658=CARTESIAN_POINT('Ctrl Pts',(3.06433918118346,0.999299459266667,
11.7513665026158));
#251659=CARTESIAN_POINT('Ctrl Pts',(3.14239104239333,0.746298515899061,
11.7344412796831));
#251660=CARTESIAN_POINT('Ctrl Pts',(3.18486369257926,0.536842684056119,
11.7201728216996));
#251661=CARTESIAN_POINT('Ctrl Pts',(3.22484646623756,0.142097678477962,
11.6933601846317));
#251662=CARTESIAN_POINT('Ctrl Pts',(3.22770628425679,-0.0418295988159529,
11.6809143422886));
#251663=CARTESIAN_POINT('Ctrl Pts',(3.21282933745172,-0.254386129646373,
11.6671958464377));
#251664=CARTESIAN_POINT('Ctrl Pts',(3.21037081183381,-0.283732348616373,
11.6653171330022));
#251665=CARTESIAN_POINT('Ctrl Pts',(3.20623882728636,-0.326069757065285,
11.6626327610921));
#251666=CARTESIAN_POINT('Ctrl Pts',(3.20488796781486,-0.339090005165756,
11.6618107871241));
#251667=CARTESIAN_POINT('Ctrl Pts',(3.20236481893419,-0.362045861035351,
11.6603682951451));
#251668=CARTESIAN_POINT('Ctrl Pts',(3.20122554550895,-0.371984752143566,
11.6597460030266));
#251669=CARTESIAN_POINT('Ctrl Pts',(3.19867238223164,-0.393377334076807,
11.6584115115451));
#251670=CARTESIAN_POINT('Ctrl Pts',(3.19724323991786,-0.404828865289943,
11.6577001554735));
#251671=CARTESIAN_POINT('Ctrl Pts',(3.19305724295462,-0.43696503795704,
11.6557117108429));
#251672=CARTESIAN_POINT('Ctrl Pts',(3.19016090560161,-0.457631346343379,
11.6544420787852));
#251673=CARTESIAN_POINT('Ctrl Pts',(3.16922481933532,-0.597144239199672,
11.6459239728885));
#251674=CARTESIAN_POINT('Ctrl Pts',(3.14474659528526,-0.714942201310361,
11.6389899008823));
#251675=CARTESIAN_POINT('Ctrl Pts',(3.06222132852555,-1.02412244843787,
11.6208443663801));
#251676=CARTESIAN_POINT('Ctrl Pts',(2.99286821069288,-1.21192757377501,
11.6098551509194));
#251677=CARTESIAN_POINT('Ctrl Pts',(2.85403989590444,-1.50178677151969,
11.5915396559895));
#251678=CARTESIAN_POINT('Ctrl Pts',(2.79534666779884,-1.60839661234649,
11.5844843505457));
#251679=CARTESIAN_POINT('Ctrl Pts',(2.71345271568018,-1.73906753574873,
11.5752664960636));
#251680=CARTESIAN_POINT('Ctrl Pts',(2.69571262982075,-1.76644129117118,
11.5733023644131));
#251681=CARTESIAN_POINT('Ctrl Pts',(2.66660729191092,-1.80989239389886,
11.5701285624632));
#251682=CARTESIAN_POINT('Ctrl Pts',(2.65550463767422,-1.82614348271027,
11.568928675114));
#251683=CARTESIAN_POINT('Ctrl Pts',(2.6340713853629,-1.85690677989992,11.5666321172972));
#251684=CARTESIAN_POINT('Ctrl Pts',(2.62376792683427,-1.87143706772608,
11.5655365024892));
#251685=CARTESIAN_POINT('Ctrl Pts',(2.59987480534259,-1.90454677271582,
11.5630144546866));
#251686=CARTESIAN_POINT('Ctrl Pts',(2.58620560127245,-1.92306733035948,
11.5615850025024));
#251687=CARTESIAN_POINT('Ctrl Pts',(2.54270527519172,-1.98070374141064,
11.5570764949692));
#251688=CARTESIAN_POINT('Ctrl Pts',(2.51217738379846,-2.01928249529493,
11.5539705294072));
#251689=CARTESIAN_POINT('Ctrl Pts',(2.43835987510959,-2.10830145597239,
11.5465891541251));
#251690=CARTESIAN_POINT('Ctrl Pts',(2.39437031213473,-2.15812968807959,
11.5422875366351));
#251691=CARTESIAN_POINT('Ctrl Pts',(2.21538209279282,-2.34866193437792,
11.5251601368135));
#251692=CARTESIAN_POINT('Ctrl Pts',(2.06928005345775,-2.47834567706285,
11.5119420351349));
#251693=CARTESIAN_POINT('Ctrl Pts',(1.7910337812451,-2.68347566034152,11.488612801425));
#251694=CARTESIAN_POINT('Ctrl Pts',(1.66355165933186,-2.76431711375781,
11.4785150562626));
#251695=CARTESIAN_POINT('Ctrl Pts',(1.51185122516423,-2.84620630750429,
11.4675004864039));
#251696=CARTESIAN_POINT('Ctrl Pts',(1.49273328447478,-2.85627937557571,
11.4661298368622));
#251697=CARTESIAN_POINT('Ctrl Pts',(1.46299362190456,-2.87156876635247,
11.464026199295));
#251698=CARTESIAN_POINT('Ctrl Pts',(1.45244245234532,-2.87691995901624,
11.4632853587038));
#251699=CARTESIAN_POINT('Ctrl Pts',(1.43295171326653,-2.88667043654046,
11.4619272638798));
#251700=CARTESIAN_POINT('Ctrl Pts',(1.42402113919662,-2.89108640842544,
11.4613090304983));
#251701=CARTESIAN_POINT('Ctrl Pts',(1.40349347805576,-2.90111868775256,
11.4598970857338));
#251702=CARTESIAN_POINT('Ctrl Pts',(1.39188305337999,-2.90670692745881,
11.4591050849716));
#251703=CARTESIAN_POINT('Ctrl Pts',(1.35533566026791,-2.92402843799959,
11.4566316925433));
#251704=CARTESIAN_POINT('Ctrl Pts',(1.33028081304983,-2.93551190262471,
11.4549646623341));
#251705=CARTESIAN_POINT('Ctrl Pts',(1.19843132842138,-2.99390801040549,
11.4463250529576));
#251706=CARTESIAN_POINT('Ctrl Pts',(1.08928506683121,-3.03532308514604,
11.4396243390244));
#251707=CARTESIAN_POINT('Ctrl Pts',(0.781781365009663,-3.13327259021256,
11.4213629732329));
#251708=CARTESIAN_POINT('Ctrl Pts',(0.579896913569947,-3.17683803605767,
11.4100287142096));
#251709=CARTESIAN_POINT('Ctrl Pts',(0.266233129897482,-3.21360884943132,
11.3919550281511));
#251710=CARTESIAN_POINT('Ctrl Pts',(0.156660750219584,-3.22080980654466,
11.3855634609525));
#251711=CARTESIAN_POINT('Ctrl Pts',(0.0151997044228281,-3.22287050556823,
11.3771003957317));
#251712=CARTESIAN_POINT('Ctrl Pts',(-0.0165464409393103,-3.22286385601687,
11.3751877202728));
#251713=CARTESIAN_POINT('Ctrl Pts',(-0.0677775800882746,-3.22209617333433,
11.3720771506789));
#251714=CARTESIAN_POINT('Ctrl Pts',(-0.0872652822184042,-3.22162727440985,
11.3708883394308));
#251715=CARTESIAN_POINT('Ctrl Pts',(-0.124599842221143,-3.2203899621812,
11.3685995913553));
#251716=CARTESIAN_POINT('Ctrl Pts',(-0.142446960526051,-3.21964989903794,
11.3675005778605));
#251717=CARTESIAN_POINT('Ctrl Pts',(-0.183658427979339,-3.21759766524008,
11.3649510417142));
#251718=CARTESIAN_POINT('Ctrl Pts',(-0.207016253011651,-3.21617931380093,
11.3634972706141));
#251719=CARTESIAN_POINT('Ctrl Pts',(-0.281541254098987,-3.21083874726651,
11.3588299928986));
#251720=CARTESIAN_POINT('Ctrl Pts',(-0.332629008933642,-3.20594890791521,
11.3555868020444));
#251721=CARTESIAN_POINT('Ctrl Pts',(-0.605866923557042,-3.17319494074689,
11.3379975773843));
#251722=CARTESIAN_POINT('Ctrl Pts',(-0.824743198926465,-3.1234611668257,
11.3229800947625));
#251723=CARTESIAN_POINT('Ctrl Pts',(-1.20039791842574,-2.99584137056866,
11.2961638492071));
#251724=CARTESIAN_POINT('Ctrl Pts',(-1.35940413753662,-2.92712339426824,
11.2844712860359));
#251725=CARTESIAN_POINT('Ctrl Pts',(-1.53836386490308,-2.83203744851931,
11.2714209817448));
#251726=CARTESIAN_POINT('Ctrl Pts',(-1.56439640265915,-2.81774085572253,
11.2695259358915));
#251727=CARTESIAN_POINT('Ctrl Pts',(-1.60165236074997,-2.79660504553247,
11.2668226967218));
#251728=CARTESIAN_POINT('Ctrl Pts',(-1.613036598909,-2.79005430231818,11.2659978790847));
#251729=CARTESIAN_POINT('Ctrl Pts',(-1.63302541208704,-2.77838905638772,
11.2645522019124));
#251730=CARTESIAN_POINT('Ctrl Pts',(-1.64164666463526,-2.77330380300996,
11.2639295412818));
#251731=CARTESIAN_POINT('Ctrl Pts',(-1.66013304671509,-2.76228317997464,
11.2625963543221));
#251732=CARTESIAN_POINT('Ctrl Pts',(-1.66999017948205,-2.75633505022361,
11.2618866521051));
#251733=CARTESIAN_POINT('Ctrl Pts',(-1.69751373800415,-2.73952454811685,
11.2599076540621));
#251734=CARTESIAN_POINT('Ctrl Pts',(-1.71510784498788,-2.72854407536489,
11.2586457015125));
#251735=CARTESIAN_POINT('Ctrl Pts',(-1.75464596448653,-2.70333479303937,
11.2558139516282));
#251736=CARTESIAN_POINT('Ctrl Pts',(-1.77652545348577,-2.68900704077793,
11.2542498653663));
#251737=CARTESIAN_POINT('Ctrl Pts',(-1.84696986491845,-2.64164146251717,
11.2492153848583));
#251738=CARTESIAN_POINT('Ctrl Pts',(-1.89480860308141,-2.60754068112921,
11.2457984886084));
#251739=CARTESIAN_POINT('Ctrl Pts',(-2.13985978661189,-2.4225539032996,
11.228158791162));
#251740=CARTESIAN_POINT('Ctrl Pts',(-2.32008150021395,-2.25055574988141,
11.2146438093973));
#251741=CARTESIAN_POINT('Ctrl Pts',(-2.54927362206534,-1.97471293658918,
11.1941238923678));
#251742=CARTESIAN_POINT('Ctrl Pts',(-2.61536401824566,-1.88630715170443,
11.1877004123705));
#251743=CARTESIAN_POINT('Ctrl Pts',(-2.69449523997219,-1.7682827858394,
11.1792006057302));
#251744=CARTESIAN_POINT('Ctrl Pts',(-2.7118100814473,-1.74161263862841,
11.1772848857963));
#251745=CARTESIAN_POINT('Ctrl Pts',(-2.73910450642408,-1.69817681284528,
11.1741705762468));
#251746=CARTESIAN_POINT('Ctrl Pts',(-2.74933167917913,-1.68156869521908,
11.1729811103567));
#251747=CARTESIAN_POINT('Ctrl Pts',(-2.76863333196253,-1.64957751748529,
11.1706919201623));
#251748=CARTESIAN_POINT('Ctrl Pts',(-2.77773194889134,-1.63420981300014,
11.1695931271475));
#251749=CARTESIAN_POINT('Ctrl Pts',(-2.79844427213071,-1.59855362606852,
11.1670453123715));
#251750=CARTESIAN_POINT('Ctrl Pts',(-2.80996578011949,-1.57821301107996,
11.1655930564882));
#251751=CARTESIAN_POINT('Ctrl Pts',(-2.84600424569816,-1.51294316674483,
11.1609357834155));
#251752=CARTESIAN_POINT('Ctrl Pts',(-2.86967164331204,-1.46755625945328,
11.1577012609336));
#251753=CARTESIAN_POINT('Ctrl Pts',(-2.95802677042889,-1.2878010431249,
11.1449002748725));
#251754=CARTESIAN_POINT('Ctrl Pts',(-3.01443074422125,-1.14958748987026,
11.1350662179998));
#251755=CARTESIAN_POINT('Ctrl Pts',(-3.12744867545686,-0.806372191506612,
11.1108275094315));
#251756=CARTESIAN_POINT('Ctrl Pts',(-3.17375701598197,-0.598698486071854,
11.0962901551797));
#251757=CARTESIAN_POINT('Ctrl Pts',(-3.20604466864878,-0.332451161387822,
11.0786868543422));
#251758=CARTESIAN_POINT('Ctrl Pts',(-3.21133215489194,-0.276754079879095,
11.0750631673019));
#251759=CARTESIAN_POINT('Ctrl Pts',(-3.21636276069522,-0.203548945142041,
11.0704007648363));
#251760=CARTESIAN_POINT('Ctrl Pts',(-3.21741698234107,-0.186143962097813,
11.0692996788549));
#251761=CARTESIAN_POINT('Ctrl Pts',(-3.21889491245675,-0.157954291515767,
11.0675292667644));
#251762=CARTESIAN_POINT('Ctrl Pts',(-3.219405784378,-0.147174791080003,
11.0668553363545));
#251763=CARTESIAN_POINT('Ctrl Pts',(-3.22026076857828,-0.126990934723725,
11.0655994332744));
#251764=CARTESIAN_POINT('Ctrl Pts',(-3.22061784823918,-0.117587384997833,
11.0650167637878));
#251765=CARTESIAN_POINT('Ctrl Pts',(-3.22127651435933,-0.0979767878061537,
11.0638065099786));
#251766=CARTESIAN_POINT('Ctrl Pts',(-3.22157078921631,-0.0877695245606001,
11.063179324094));
#251767=CARTESIAN_POINT('Ctrl Pts',(-3.22211717083128,-0.065073271156808,
11.0617905206222));
#251768=CARTESIAN_POINT('Ctrl Pts',(-3.22234519383345,-0.0525838003462824,
11.0610301613137));
#251769=CARTESIAN_POINT('Ctrl Pts',(-3.22266282296568,-0.0270542178465188,
11.0594832828966));
#251770=CARTESIAN_POINT('Ctrl Pts',(-3.22274591169252,-0.0140142783986701,
11.0586970973044));
#251771=CARTESIAN_POINT('Ctrl Pts',(-3.22274985281522,-0.000974001778823583,
11.0579144994549));
#251772=CARTESIAN_POINT('Ctrl Pts',(-3.22274985195413,-0.000976846793707469,
11.0579146701954));
#251773=CARTESIAN_POINT('Ctrl Pts',(-3.22274995065157,-0.000651230577373808,
11.0578951286835));
#251774=CARTESIAN_POINT('Ctrl Pts',(-3.22275,-0.00032561497491421,11.057875589458));
#251775=CARTESIAN_POINT('Ctrl Pts',(-3.22275,2.40369908895709E-12,11.0578560525147));
#251776=CARTESIAN_POINT('',(-3.22274890077618,-0.00266177495324583,10.8127319644804));
#251777=CARTESIAN_POINT('Ctrl Pts',(-3.22275,-7.2705680572429E-11,10.8125553006127));
#251778=CARTESIAN_POINT('Ctrl Pts',(-3.22274999999998,-0.00088725350428013,
10.8126141809251));
#251779=CARTESIAN_POINT('Ctrl Pts',(-3.22274963359612,-0.00177451187261363,
10.8126730688928));
#251780=CARTESIAN_POINT('Ctrl Pts',(-3.22274890077618,-0.00266177495322464,
10.8127319644804));
#251781=CARTESIAN_POINT('Ctrl Pts',(-3.22274890347102,-0.00265851017456808,
10.8127317477678));
#251782=CARTESIAN_POINT('Ctrl Pts',(-3.2226069773852,-0.174706803165855,
10.8241521285412));
#251783=CARTESIAN_POINT('Ctrl Pts',(-3.20868771616605,-0.346465522279838,
10.8358494098271));
#251784=CARTESIAN_POINT('Ctrl Pts',(-3.15997717365837,-0.646600032517979,
10.8563154919063));
#251785=CARTESIAN_POINT('Ctrl Pts',(-3.13083714163604,-0.775508502628825,
10.8651076131163));
#251786=CARTESIAN_POINT('Ctrl Pts',(-3.08783682633512,-0.922954612464723,
10.8749161354524));
#251787=CARTESIAN_POINT('Ctrl Pts',(-3.08159925070548,-0.943571723987823,
10.876281750581));
#251788=CARTESIAN_POINT('Ctrl Pts',(-3.07161309486545,-0.975423369346211,
10.8783807004478));
#251789=CARTESIAN_POINT('Ctrl Pts',(-3.06800863672006,-0.986701965842342,
10.8791218198553));
#251790=CARTESIAN_POINT('Ctrl Pts',(-3.06117483661154,-1.00768586032651,
10.8804963946471));
#251791=CARTESIAN_POINT('Ctrl Pts',(-3.05796144445542,-1.01739568549116,
10.8811306908383));
#251792=CARTESIAN_POINT('Ctrl Pts',(-3.0504425666293,-1.03975781453091,
10.8825876357335));
#251793=CARTESIAN_POINT('Ctrl Pts',(-3.04610454666431,-1.05239881719149,
10.8834083946757));
#251794=CARTESIAN_POINT('Ctrl Pts',(-3.03176593553887,-1.09335004662847,
10.8860591864589));
#251795=CARTESIAN_POINT('Ctrl Pts',(-3.0214480264945,-1.12154847433009,
10.887871862882));
#251796=CARTESIAN_POINT('Ctrl Pts',(-2.95713248302473,-1.28998727504354,
10.8986466690472));
#251797=CARTESIAN_POINT('Ctrl Pts',(-2.89376801402038,-1.42646986391953,
10.9071603563856));
#251798=CARTESIAN_POINT('Ctrl Pts',(-2.73912617868258,-1.7064750944649,
10.9251228701839));
#251799=CARTESIAN_POINT('Ctrl Pts',(-2.64556679777714,-1.84820014937909,
10.934531108881));
#251800=CARTESIAN_POINT('Ctrl Pts',(-2.49634674289376,-2.03953724831737,
10.9484256745151));
#251801=CARTESIAN_POINT('Ctrl Pts',(-2.44945514327004,-2.09562109177532,
10.9526600177757));
#251802=CARTESIAN_POINT('Ctrl Pts',(-2.36556745002752,-2.18928785107805,
10.9600649693526));
#251803=CARTESIAN_POINT('Ctrl Pts',(-2.32948057200955,-2.22764684295282,
10.9632008811682));
#251804=CARTESIAN_POINT('Ctrl Pts',(-2.27710228775061,-2.28065799858243,
10.9676949238489));
#251805=CARTESIAN_POINT('Ctrl Pts',(-2.26157537651787,-2.29605586079043,
10.969020259454));
#251806=CARTESIAN_POINT('Ctrl Pts',(-2.24543561097468,-2.31173893133674,
10.9703913422249));
#251807=CARTESIAN_POINT('Ctrl Pts',(-2.24497783512923,-2.3121834895762,
10.9704302251746));
#251808=CARTESIAN_POINT('Ctrl Pts',(-2.2440463510189,-2.31308754103962,
10.970509333427));
#251809=CARTESIAN_POINT('Ctrl Pts',(-2.24357263360686,-2.3135470247573,
10.9705495591329));
#251810=CARTESIAN_POINT('Ctrl Pts',(-2.24260671782949,-2.31448334219024,
10.9706315681698));
#251811=CARTESIAN_POINT('Ctrl Pts',(-2.24211450846048,-2.31496016446936,
10.9706733519866));
#251812=CARTESIAN_POINT('Ctrl Pts',(-2.24110869553655,-2.31593391270455,
10.9707587231845));
#251813=CARTESIAN_POINT('Ctrl Pts',(-2.24059507873148,-2.3164308248656,
10.970802311151));
#251814=CARTESIAN_POINT('Ctrl Pts',(-2.22695065451891,-2.32962270014803,
10.9719600643232));
#251815=CARTESIAN_POINT('Ctrl Pts',(-2.21371254624232,-2.34220577316728,
10.9730789771653));
#251816=CARTESIAN_POINT('Ctrl Pts',(-2.18579145527427,-2.36829713391313,
10.9754302925374));
#251817=CARTESIAN_POINT('Ctrl Pts',(-2.17108859586833,-2.3817829206279,
10.976663578304));
#251818=CARTESIAN_POINT('Ctrl Pts',(-2.13206592700471,-2.4169138108696,
10.9799246472093));
#251819=CARTESIAN_POINT('Ctrl Pts',(-2.10754218018669,-2.43832797656515,
10.9819618604862));
#251820=CARTESIAN_POINT('Ctrl Pts',(-1.99459936968593,-2.53397288565651,
10.9912923465963));
#251821=CARTESIAN_POINT('Ctrl Pts',(-1.90256428225074,-2.60378364421884,
10.9987585258432));
#251822=CARTESIAN_POINT('Ctrl Pts',(-1.60686238828517,-2.80401992600998,
11.0223174157064));
#251823=CARTESIAN_POINT('Ctrl Pts',(-1.39214644273215,-2.91658137129566,
11.0388993084828));
#251824=CARTESIAN_POINT('Ctrl Pts',(-1.11247204239699,-3.025215768649,11.058860394099));
#251825=CARTESIAN_POINT('Ctrl Pts',(-1.05749636306838,-3.04486890933398,
11.0627064876903));
#251826=CARTESIAN_POINT('Ctrl Pts',(-0.965727649540792,-3.07488947903642,
11.0689677988385));
#251827=CARTESIAN_POINT('Ctrl Pts',(-0.929230969969557,-3.08611491971717,
11.0714171912993));
#251828=CARTESIAN_POINT('Ctrl Pts',(-0.878274144454334,-3.10080192245904,
11.0747727019489));
#251829=CARTESIAN_POINT('Ctrl Pts',(-0.863978054521453,-3.10481561066848,
11.0757071284283));
#251830=CARTESIAN_POINT('Ctrl Pts',(-0.839609409755192,-3.11147586220572,
11.0772874828458));
#251831=CARTESIAN_POINT('Ctrl Pts',(-0.829550927441443,-3.11417264659841,
11.0779361998897));
#251832=CARTESIAN_POINT('Ctrl Pts',(-0.808614791814882,-3.11967720707168,
11.0792787888924));
#251833=CARTESIAN_POINT('Ctrl Pts',(-0.797735310536159,-3.12247692402484,
11.079972212608));
#251834=CARTESIAN_POINT('Ctrl Pts',(-0.768663978538421,-3.12979625650217,
11.0818143329938));
#251835=CARTESIAN_POINT('Ctrl Pts',(-0.750446662236314,-3.13421421798492,
11.0829574366479));
#251836=CARTESIAN_POINT('Ctrl Pts',(-0.667539375151929,-3.1535561069684,
11.0881130361248));
#251837=CARTESIAN_POINT('Ctrl Pts',(-0.602431908669004,-3.16663891719223,
11.0920331898869));
#251838=CARTESIAN_POINT('Ctrl Pts',(-0.352969632080119,-3.20879259113306,
11.1067244289763));
#251839=CARTESIAN_POINT('Ctrl Pts',(-0.166611915149471,-3.22384674457711,
11.1170380060437));
#251840=CARTESIAN_POINT('Ctrl Pts',(0.191030119251093,-3.22162589494382,
11.1371153450664));
#251841=CARTESIAN_POINT('Ctrl Pts',(0.361674210126881,-3.20695318995163,
11.1468223764289));
#251842=CARTESIAN_POINT('Ctrl Pts',(0.574599940630966,-3.17142965872212,
11.1596044219548));
#251843=CARTESIAN_POINT('Ctrl Pts',(0.618700662164427,-3.16312193405382,
11.1622874867997));
#251844=CARTESIAN_POINT('Ctrl Pts',(0.684635589440942,-3.14926945798729,
11.1663593444003));
#251845=CARTESIAN_POINT('Ctrl Pts',(0.706609649338576,-3.14441199168774,
11.1677265123958));
#251846=CARTESIAN_POINT('Ctrl Pts',(0.746012227931751,-3.13526799226979,
11.1701971019172));
#251847=CARTESIAN_POINT('Ctrl Pts',(0.763459363359172,-3.13106521932581,
11.1712978188528));
#251848=CARTESIAN_POINT('Ctrl Pts',(0.800962403960998,-3.12169916308307,
11.1736788276724));
#251849=CARTESIAN_POINT('Ctrl Pts',(0.821005376060777,-3.11648785944851,
11.1749606131778));
#251850=CARTESIAN_POINT('Ctrl Pts',(0.874940178445056,-3.10190806181315,
11.1784355910635));
#251851=CARTESIAN_POINT('Ctrl Pts',(0.908730423779365,-3.09217767940173,
11.1806402816448));
#251852=CARTESIAN_POINT('Ctrl Pts',(1.11595976230474,-3.02881302190786,
11.1943367830342));
#251853=CARTESIAN_POINT('Ctrl Pts',(1.28474293727904,-2.9611639095978,11.2062828778967));
#251854=CARTESIAN_POINT('Ctrl Pts',(1.60869341519044,-2.79839306241365,
11.2306295743778));
#251855=CARTESIAN_POINT('Ctrl Pts',(1.76333549060141,-2.70361741083642,
11.2429831728678));
#251856=CARTESIAN_POINT('Ctrl Pts',(1.95079304533275,-2.56577265987937,
11.2584036064392));
#251857=CARTESIAN_POINT('Ctrl Pts',(1.99164632244395,-2.53419184786923,
11.2617923591158));
#251858=CARTESIAN_POINT('Ctrl Pts',(2.05883684725524,-2.47962260791855,
11.2673912507402));
#251859=CARTESIAN_POINT('Ctrl Pts',(2.08559009919478,-2.45716332519871,
11.2696276203936));
#251860=CARTESIAN_POINT('Ctrl Pts',(2.12280718382041,-2.42487379340251,
11.272742493269));
#251861=CARTESIAN_POINT('Ctrl Pts',(2.13357760105103,-2.4154026355519,11.2736443789634));
#251862=CARTESIAN_POINT('Ctrl Pts',(2.15199523983047,-2.39898743870039,
11.2751868701649));
#251863=CARTESIAN_POINT('Ctrl Pts',(2.15967288048976,-2.39207803060076,
11.275829942411));
#251864=CARTESIAN_POINT('Ctrl Pts',(2.17578671500661,-2.3774357378572,11.2771795818937));
#251865=CARTESIAN_POINT('Ctrl Pts',(2.18421507987119,-2.36969470840714,
11.2778855351453));
#251866=CARTESIAN_POINT('Ctrl Pts',(2.20704155260707,-2.34850448560635,
11.2797981088515));
#251867=CARTESIAN_POINT('Ctrl Pts',(2.22135810699456,-2.33496765247142,
11.2809983649196));
#251868=CARTESIAN_POINT('Ctrl Pts',(2.29127013799473,-2.26763820679431,
11.2868684913453));
#251869=CARTESIAN_POINT('Ctrl Pts',(2.34504474167949,-2.21198304729898,
11.2914119912129));
#251870=CARTESIAN_POINT('Ctrl Pts',(2.51626883581635,-2.02150010581347,
11.3061920222048));
#251871=CARTESIAN_POINT('Ctrl Pts',(2.62450810995535,-1.87883904327364,
11.3160743244534));
#251872=CARTESIAN_POINT('Ctrl Pts',(2.8024391775278,-1.59871379414475,11.3347159627933));
#251873=CARTESIAN_POINT('Ctrl Pts',(2.87519744993961,-1.46382523818974,
11.3434075070993));
#251874=CARTESIAN_POINT('Ctrl Pts',(2.96002656067434,-1.27562127110791,
11.3555621839635));
#251875=CARTESIAN_POINT('Ctrl Pts',(2.98074746116379,-1.22642201455439,
11.3587406408925));
#251876=CARTESIAN_POINT('Ctrl Pts',(3.00902686133688,-1.15431994055603,
11.3634116325884));
#251877=CARTESIAN_POINT('Ctrl Pts',(3.01756589854231,-1.13180969136239,
11.3648716760293));
#251878=CARTESIAN_POINT('Ctrl Pts',(3.03214567893183,-1.09203688032284,
11.3674554531901));
#251879=CARTESIAN_POINT('Ctrl Pts',(3.03829324618058,-1.07481444674469,
11.368575605437));
#251880=CARTESIAN_POINT('Ctrl Pts',(3.0508161701053,-1.03876528796233,11.3709234316049));
#251881=CARTESIAN_POINT('Ctrl Pts',(3.05716457330799,-1.01993008139582,
11.3721519340931));
#251882=CARTESIAN_POINT('Ctrl Pts',(3.0733429909898,-0.970421490271061,
11.3753863142761));
#251883=CARTESIAN_POINT('Ctrl Pts',(3.08288790194672,-0.939657955471732,
11.3774013442109));
#251884=CARTESIAN_POINT('Ctrl Pts',(3.12258902727165,-0.804578247819572,
11.3862747669225));
#251885=CARTESIAN_POINT('Ctrl Pts',(3.14792034208946,-0.698928910227485,
11.3932845998921));
#251886=CARTESIAN_POINT('Ctrl Pts',(3.20576850289787,-0.38948646779044,
11.4140016725154));
#251887=CARTESIAN_POINT('Ctrl Pts',(3.22411671687954,-0.183602133046582,
11.4280455031335));
#251888=CARTESIAN_POINT('Ctrl Pts',(3.22178356804375,0.149118012565971,
11.4504196352041));
#251889=CARTESIAN_POINT('Ctrl Pts',(3.2134463995233,0.275489450037044,11.4588309540877));
#251890=CARTESIAN_POINT('Ctrl Pts',(3.19503744023209,0.422268172084959,
11.4682762805714));
#251891=CARTESIAN_POINT('Ctrl Pts',(3.19216573543396,0.443455327481237,
11.4696316099478));
#251892=CARTESIAN_POINT('Ctrl Pts',(3.18738123633073,0.476295921728712,
11.4717182276112));
#251893=CARTESIAN_POINT('Ctrl Pts',(3.18561494671247,0.487969642843626,
11.4724571607801));
#251894=CARTESIAN_POINT('Ctrl Pts',(3.18219786973034,0.509744072377771,
11.4738299137238));
#251895=CARTESIAN_POINT('Ctrl Pts',(3.18056312012334,0.519846653784449,
11.4744645504747));
#251896=CARTESIAN_POINT('Ctrl Pts',(3.17667381938333,0.543176807411602,
11.4759250784439));
#251897=CARTESIAN_POINT('Ctrl Pts',(3.17438475397495,0.556398281103199,
11.4767490468462));
#251898=CARTESIAN_POINT('Ctrl Pts',(3.16665289061677,0.599455412777923,
11.4794213425896));
#251899=CARTESIAN_POINT('Ctrl Pts',(3.16087134267973,0.629229549086772,
11.4812519201485));
#251900=CARTESIAN_POINT('Ctrl Pts',(3.12173336779103,0.816608322246431,
11.4926879128615));
#251901=CARTESIAN_POINT('Ctrl Pts',(3.07701556476825,0.971625084310848,
11.5017771194138));
#251902=CARTESIAN_POINT('Ctrl Pts',(2.96951831180388,1.26088141462643,11.5190819304013));
#251903=CARTESIAN_POINT('Ctrl Pts',(2.90872596598027,1.39541125665596,11.5272874125494));
#251904=CARTESIAN_POINT('Ctrl Pts',(2.80145664246381,1.59506425538171,11.5402214792416));
#251905=CARTESIAN_POINT('Ctrl Pts',(2.76141796283196,1.66341784472842,11.5447947298266));
#251906=CARTESIAN_POINT('Ctrl Pts',(2.68869185187118,1.77770090206581,11.5527560703656));
#251907=CARTESIAN_POINT('Ctrl Pts',(2.65724246805397,1.8243755854665,11.5561025497488));
#251908=CARTESIAN_POINT('Ctrl Pts',(2.61032939279497,1.89021210205939,11.5609751021571));
#251909=CARTESIAN_POINT('Ctrl Pts',(2.59584206968192,1.91005895932068,11.5624645030511));
#251910=CARTESIAN_POINT('Ctrl Pts',(2.57013566730735,1.94444267386075,11.5650820339151));
#251911=CARTESIAN_POINT('Ctrl Pts',(2.55901654272434,1.95905308059331,11.5662062736578));
#251912=CARTESIAN_POINT('Ctrl Pts',(2.53719221150504,1.98722716186766,11.5683980376107));
#251913=CARTESIAN_POINT('Ctrl Pts',(2.52650154828163,2.00080134424259,11.5694649666015));
#251914=CARTESIAN_POINT('Ctrl Pts',(2.49756892203279,2.0369361235634,11.5723350423054));
#251915=CARTESIAN_POINT('Ctrl Pts',(2.47913093172099,2.0593370359361,11.5741459464324));
#251916=CARTESIAN_POINT('Ctrl Pts',(2.40808546509415,2.14331543121641,11.5810580772105));
#251917=CARTESIAN_POINT('Ctrl Pts',(2.3534694124365,2.20314696155395,11.586239956163));
#251918=CARTESIAN_POINT('Ctrl Pts',(2.13827550878777,2.42174911038901,11.6061848626051));
#251919=CARTESIAN_POINT('Ctrl Pts',(1.96343453316135,2.56553943177328,11.621514370842));
#251920=CARTESIAN_POINT('Ctrl Pts',(1.66755653261322,2.76078887083364,11.6454052219535));
#251921=CARTESIAN_POINT('Ctrl Pts',(1.55591171382705,2.82521588917958,11.6540100002138));
#251922=CARTESIAN_POINT('Ctrl Pts',(1.41466056709349,2.8958074084687,11.664173151145));
#251923=CARTESIAN_POINT('Ctrl Pts',(1.3884433476693,2.90846871620018,11.6660300657538));
#251924=CARTESIAN_POINT('Ctrl Pts',(1.34996461517241,2.92641267243878,11.6687089971135));
#251925=CARTESIAN_POINT('Ctrl Pts',(1.33783694245247,2.93197679418111,11.669546691619));
#251926=CARTESIAN_POINT('Ctrl Pts',(1.31637552493878,2.94166230717733,11.6710169463326));
#251927=CARTESIAN_POINT('Ctrl Pts',(1.30705631863909,2.94581490284486,11.6716513391503));
#251928=CARTESIAN_POINT('Ctrl Pts',(1.28672759425122,2.95475782479119,11.6730263498829));
#251929=CARTESIAN_POINT('Ctrl Pts',(1.27571090610401,2.9595309425171,11.6737659481248));
#251930=CARTESIAN_POINT('Ctrl Pts',(1.24470838960872,2.97275788951337,11.6758324140191));
#251931=CARTESIAN_POINT('Ctrl Pts',(1.22466307480695,2.98107176288728,11.6771512721671));
#251932=CARTESIAN_POINT('Ctrl Pts',(1.08494706701228,3.03737236172377,11.6862345888966));
#251933=CARTESIAN_POINT('Ctrl Pts',(0.96256123432206,3.0783476589196,11.6936407305182));
#251934=CARTESIAN_POINT('Ctrl Pts',(0.797193576542146,3.1228815421372,11.7033246085221));
#251935=CARTESIAN_POINT('Ctrl Pts',(0.756137097401467,3.13307572621057,
11.7057028773094));
#251936=CARTESIAN_POINT('Ctrl Pts',(0.578954736189343,3.17338369697464,
11.7158961203492));
#251937=CARTESIAN_POINT('Ctrl Pts',(0.441155958200194,3.19545505113785,
11.7236535078379));
#251938=CARTESIAN_POINT('Ctrl Pts',(0.217144220371637,3.21656540856973,
11.736452194559));
#251939=CARTESIAN_POINT('Ctrl Pts',(0.131642196141464,3.2211975284276,11.7413791855758));
#251940=CARTESIAN_POINT('Ctrl Pts',(-0.0134855023914868,3.22327197497497,
11.7498927154529));
#251941=CARTESIAN_POINT('Ctrl Pts',(-0.0730412177703081,3.22247240567317,
11.7534290536953));
#251942=CARTESIAN_POINT('Ctrl Pts',(-0.15762821317495,3.21899075722102,
11.7585284125583));
#251943=CARTESIAN_POINT('Ctrl Pts',(-0.182704956213157,3.21766483547543,
11.7600497299663));
#251944=CARTESIAN_POINT('Ctrl Pts',(-0.226171824248095,3.21485678735417,
11.7627044069254));
#251945=CARTESIAN_POINT('Ctrl Pts',(-0.244569674268101,3.21350953159295,
11.763833536507));
#251946=CARTESIAN_POINT('Ctrl Pts',(-0.28003325312058,3.2106062625554,11.7660210750847));
#251947=CARTESIAN_POINT('Ctrl Pts',(-0.297100165231679,3.20907193280222,
11.7670787720217));
#251948=CARTESIAN_POINT('Ctrl Pts',(-0.342262058856747,3.20464848320428,
11.7698910777815));
#251949=CARTESIAN_POINT('Ctrl Pts',(-0.370332198358267,3.20152607359326,
11.771652884546));
#251950=CARTESIAN_POINT('Ctrl Pts',(-0.473215699810164,3.18871059212305,
11.7781628751098));
#251951=CARTESIAN_POINT('Ctrl Pts',(-0.547718533819655,3.1767611265088,
11.7829801384191));
#251952=CARTESIAN_POINT('Ctrl Pts',(-0.848311967222745,3.11766079624425,
11.8028439921008));
#251953=CARTESIAN_POINT('Ctrl Pts',(-1.06942771854834,3.0488916690584,11.818513527782));
#251954=CARTESIAN_POINT('Ctrl Pts',(-1.40108390359436,2.90519084761208,
11.842879498471));
#251955=CARTESIAN_POINT('Ctrl Pts',(-1.51765037326923,2.84603471151077,
11.851610427585));
#251956=CARTESIAN_POINT('Ctrl Pts',(-1.65558789475757,2.76514099505496,
11.8619040408777));
#251957=CARTESIAN_POINT('Ctrl Pts',(-1.68065920282051,2.74997468752692,
11.8637731403095));
#251958=CARTESIAN_POINT('Ctrl Pts',(-1.71687135366568,2.72738872548387,
11.8664662264588));
#251959=CARTESIAN_POINT('Ctrl Pts',(-1.72817758518681,2.72023873100847,
11.8673061167705));
#251960=CARTESIAN_POINT('Ctrl Pts',(-1.74803055190906,2.70751009321934,
11.8687787690944));
#251961=CARTESIAN_POINT('Ctrl Pts',(-1.75659573374236,2.70196098295213,
11.8694133855051));
#251962=CARTESIAN_POINT('Ctrl Pts',(-1.77516006700593,2.68980814873806,
11.8707871946287));
#251963=CARTESIAN_POINT('Ctrl Pts',(-1.78514886414004,2.68318927472652,
11.8715253838606));
#251964=CARTESIAN_POINT('Ctrl Pts',(-1.81303481518356,2.66448656042187,
11.873584060386));
#251965=CARTESIAN_POINT('Ctrl Pts',(-1.83084813357572,2.65227808500167,
11.8748966335251));
#251966=CARTESIAN_POINT('Ctrl Pts',(-1.95060920324415,2.56841747481395,
11.8837139954207));
#251967=CARTESIAN_POINT('Ctrl Pts',(-2.04846102655947,2.49107583799226,
11.890884404987));
#251968=CARTESIAN_POINT('Ctrl Pts',(-2.34760626076273,2.22505378919181,
11.9135482970079));
#251969=CARTESIAN_POINT('Ctrl Pts',(-2.52924695131744,2.01619149584354,
11.9286034010639));
#251970=CARTESIAN_POINT('Ctrl Pts',(-2.71371900606081,1.73928177831334,
11.9481494245084));
#251971=CARTESIAN_POINT('Ctrl Pts',(-2.7440794316737,1.69097588334042,11.9515406965663));
#251972=CARTESIAN_POINT('Ctrl Pts',(-2.78572504242377,1.62063681657417,
11.9564668476198));
#251973=CARTESIAN_POINT('Ctrl Pts',(-2.79806439672783,1.59923834476012,
11.9579638969909));
#251974=CARTESIAN_POINT('Ctrl Pts',(-2.81915445781292,1.56167331596258,
11.960590290173));
#251975=CARTESIAN_POINT('Ctrl Pts',(-2.8280151900197,1.54556962507962,11.9617156627545));
#251976=CARTESIAN_POINT('Ctrl Pts',(-2.84604741517343,1.5121231873291,11.964052332442));
#251977=CARTESIAN_POINT('Ctrl Pts',(-2.8551992512411,1.49477076230871,11.9652642616491));
#251978=CARTESIAN_POINT('Ctrl Pts',(-2.87840484588383,1.44978081437313,
11.9684060529069));
#251979=CARTESIAN_POINT('Ctrl Pts',(-2.89221895643368,1.42202259746327,
11.9703441272816));
#251980=CARTESIAN_POINT('Ctrl Pts',(-2.94834459176881,1.30504115757637,
11.9785126342125));
#251981=CARTESIAN_POINT('Ctrl Pts',(-2.98694080868465,1.21410444187207,
11.9848669111144));
#251982=CARTESIAN_POINT('Ctrl Pts',(-3.10186835549107,0.904504766804046,
12.0065105487312));
#251983=CARTESIAN_POINT('Ctrl Pts',(-3.15880969331165,0.67942462263731,
12.0223187939908));
#251984=CARTESIAN_POINT('Ctrl Pts',(-3.20195534518314,0.373611688638818,
12.043033553281));
#251985=CARTESIAN_POINT('Ctrl Pts',(-3.21000236929912,0.296630968749452,
12.0481782358679));
#251986=CARTESIAN_POINT('Ctrl Pts',(-3.2184370751095,0.173039251601177,
12.056258527319));
#251987=CARTESIAN_POINT('Ctrl Pts',(-3.22059892083219,0.12658153875267,
12.059255362799));
#251988=CARTESIAN_POINT('Ctrl Pts',(-3.22215222671543,0.0640977615092215,
12.063217637612));
#251989=CARTESIAN_POINT('Ctrl Pts',(-3.22243072041141,0.0481016822066572,
12.0642259748981));
#251990=CARTESIAN_POINT('Ctrl Pts',(-3.22269604935966,0.0214678861005913,
12.0658941240438));
#251991=CARTESIAN_POINT('Ctrl Pts',(-3.22274935267479,0.0108312704363253,
12.0665574697344));
#251992=CARTESIAN_POINT('Ctrl Pts',(-3.22274999804659,0.000129566408754178,
12.0672218721387));
#251993=CARTESIAN_POINT('Ctrl Pts',(-3.22275,6.47832063023646E-5,12.0672258940155));
#251994=CARTESIAN_POINT('Ctrl Pts',(-3.22275,-3.23896726357594E-13,12.0672299157825));
#251995=CARTESIAN_POINT('Origin',(0.,0.,-2.31077344927308));
#251996=CARTESIAN_POINT('',(-3.22275,7.83873563209288E-13,13.5633017710267));
#251997=CARTESIAN_POINT('',(-3.22275,-2.24100014615096E-11,13.3128542084224));
#251998=CARTESIAN_POINT('',(-3.22275,-3.50678552687464E-13,-2.31077344927308));
#251999=CARTESIAN_POINT('Ctrl Pts',(-3.22275,7.83873563209288E-13,13.5633017710267));
#252000=CARTESIAN_POINT('Ctrl Pts',(-3.22275,0.0358663401662114,13.5611946398766));
#252001=CARTESIAN_POINT('Ctrl Pts',(-3.22215126056633,0.0717294574829636,
13.5590715766439));
#252002=CARTESIAN_POINT('Ctrl Pts',(-3.21998093223654,0.136712604019992,
13.5551907275807));
#252003=CARTESIAN_POINT('Ctrl Pts',(-3.21861244358439,0.165835447558698,
13.5534391303));
#252004=CARTESIAN_POINT('Ctrl Pts',(-3.21579086853076,0.212397530855393,
13.5506170458497));
#252005=CARTESIAN_POINT('Ctrl Pts',(-3.21459051622025,0.229850855455928,
13.5495543548726));
#252006=CARTESIAN_POINT('Ctrl Pts',(-3.21194561779516,0.264217801727172,
13.5474518433432));
#252007=CARTESIAN_POINT('Ctrl Pts',(-3.2105094232961,0.281131506778595,
13.5464123146483));
#252008=CARTESIAN_POINT('Ctrl Pts',(-3.20716883802595,0.317099815306884,
13.5441911580151));
#252009=CARTESIAN_POINT('Ctrl Pts',(-3.20522810348359,0.336150305702089,
13.5430084345697));
#252010=CARTESIAN_POINT('Ctrl Pts',(-3.1997956045101,0.385141897159354,
13.5399501421897));
#252011=CARTESIAN_POINT('Ctrl Pts',(-3.19605338735088,0.415052813977154,
13.5380668360008));
#252012=CARTESIAN_POINT('Ctrl Pts',(-3.178844011077,0.538518149897557,13.5302239732648));
#252013=CARTESIAN_POINT('Ctrl Pts',(-3.16168512166983,0.631502455369941,
13.524151047291));
#252014=CARTESIAN_POINT('Ctrl Pts',(-3.08775748245068,0.952356580424882,
13.5026131197667));
#252015=CARTESIAN_POINT('Ctrl Pts',(-3.0102117915324,1.17466271469998,13.4865864710136));
#252016=CARTESIAN_POINT('Ctrl Pts',(-2.85870212786544,1.49255903783352,
13.4629476731765));
#252017=CARTESIAN_POINT('Ctrl Pts',(-2.80241117014893,1.59574673381918,
13.4551633074184));
#252018=CARTESIAN_POINT('Ctrl Pts',(-2.72967768614361,1.71330345704064,
13.4463421120735));
#252019=CARTESIAN_POINT('Ctrl Pts',(-2.71857812760522,1.73086164154363,
13.4450259673334));
#252020=CARTESIAN_POINT('Ctrl Pts',(-2.7010600263119,1.75798890667437,13.4429961812286));
#252021=CARTESIAN_POINT('Ctrl Pts',(-2.69475884302119,1.76763261150958,
13.4422753216137));
#252022=CARTESIAN_POINT('Ctrl Pts',(-2.68288689045436,1.785591122116,13.4409346086661));
#252023=CARTESIAN_POINT('Ctrl Pts',(-2.67732909499756,1.79391377782846,
13.44031398658));
#252024=CARTESIAN_POINT('Ctrl Pts',(-2.66439402059305,1.81308970241323,
13.4388855002408));
#252025=CARTESIAN_POINT('Ctrl Pts',(-2.65698912115888,1.82392395393308,
13.4380794802634));
#252026=CARTESIAN_POINT('Ctrl Pts',(-2.63264827627908,1.8590746903839,13.4354668465017));
#252027=CARTESIAN_POINT('Ctrl Pts',(-2.61544257349356,1.88320363623368,
13.4336772327723));
#252028=CARTESIAN_POINT('Ctrl Pts',(-2.49305162417735,2.04992869813666,
13.4213122866347));
#252029=CARTESIAN_POINT('Ctrl Pts',(-2.37658286303402,2.1838916971656,13.4113709393831));
#252030=CARTESIAN_POINT('Ctrl Pts',(-2.15140393087684,2.40341740256482,
13.3937606130911));
#252031=CARTESIAN_POINT('Ctrl Pts',(-2.04711282669549,2.49284602451749,
13.3861041895864));
#252032=CARTESIAN_POINT('Ctrl Pts',(-1.87589041363542,2.62165703698144,
13.3738620427079));
#252033=CARTESIAN_POINT('Ctrl Pts',(-1.81270126910884,2.6657388168922,13.3694085761401));
#252034=CARTESIAN_POINT('Ctrl Pts',(-1.70185613366309,2.73730151183758,
13.3616476746094));
#252035=CARTESIAN_POINT('Ctrl Pts',(-1.65496397457985,2.76590447863094,
13.3583795572725));
#252036=CARTESIAN_POINT('Ctrl Pts',(-1.58654231170114,2.80527685959978,
13.3536198483612));
#252037=CARTESIAN_POINT('Ctrl Pts',(-1.56558587952221,2.81702601550049,
13.3521632300672));
#252038=CARTESIAN_POINT('Ctrl Pts',(-1.52874277563977,2.83714388570301,
13.349603496562));
#252039=CARTESIAN_POINT('Ctrl Pts',(-1.51291371437355,2.84561627327218,
13.3485041049566));
#252040=CARTESIAN_POINT('Ctrl Pts',(-1.47998879469051,2.86288672154734,
13.3462176751596));
#252041=CARTESIAN_POINT('Ctrl Pts',(-1.46288337751684,2.87166491973028,
13.3450299965244));
#252042=CARTESIAN_POINT('Ctrl Pts',(-1.41843803928599,2.89397332320842,
13.3419440006812));
#252043=CARTESIAN_POINT('Ctrl Pts',(-1.39098322232348,2.90726910346661,
13.340037675965));
#252044=CARTESIAN_POINT('Ctrl Pts',(-1.27481875157701,2.96150294767342,
13.3319692947165));
#252045=CARTESIAN_POINT('Ctrl Pts',(-1.184467641818,2.99878238443524,13.3256855580095));
#252046=CARTESIAN_POINT('Ctrl Pts',(-0.893184864502717,3.10374858810872,
13.3054045072757));
#252047=CARTESIAN_POINT('Ctrl Pts',(-0.687212230240054,3.15574988780722,
13.2909909483514));
#252048=CARTESIAN_POINT('Ctrl Pts',(-0.354943453974266,3.2055466186936,
13.2683618758922));
#252049=CARTESIAN_POINT('Ctrl Pts',(-0.231259848256791,3.21683673472798,
13.2600831813729));
#252050=CARTESIAN_POINT('Ctrl Pts',(-0.0788707856187371,3.22190963768195,
13.2502762007257));
#252051=CARTESIAN_POINT('Ctrl Pts',(-0.0505059875189472,3.2224791055765,
13.2484676520801));
#252052=CARTESIAN_POINT('Ctrl Pts',(-0.00910165381677435,3.22276350853609,
13.2458558245503));
#252053=CARTESIAN_POINT('Ctrl Pts',(0.00393366097045205,3.22277396228803,
13.2450376123386));
#252054=CARTESIAN_POINT('Ctrl Pts',(0.0269438792341366,3.22265280352359,
13.2436008913908));
#252055=CARTESIAN_POINT('Ctrl Pts',(0.0369185630251869,3.2225539706236,
13.2429806325191));
#252056=CARTESIAN_POINT('Ctrl Pts',(0.0586145034701227,3.22223824757651,
13.2416371095459));
#252057=CARTESIAN_POINT('Ctrl Pts',(0.0703351560375073,3.2220037181814,
13.2409148133784));
#252058=CARTESIAN_POINT('Ctrl Pts',(0.103171899426244,3.22116739030173,
13.2389003964433));
#252059=CARTESIAN_POINT('Ctrl Pts',(0.124284152143396,3.22042191335284,
13.2376158718731));
#252060=CARTESIAN_POINT('Ctrl Pts',(0.261869204336672,3.21420870237208,
13.2293054000103));
#252061=CARTESIAN_POINT('Ctrl Pts',(0.377991897923247,3.20263032051029,
13.2225730395773));
#252062=CARTESIAN_POINT('Ctrl Pts',(0.544645701192555,3.17681984058416,
13.2130024008611));
#252063=CARTESIAN_POINT('Ctrl Pts',(0.595849692859433,3.16761528325244,
13.2100747340992));
#252064=CARTESIAN_POINT('Ctrl Pts',(0.882804882633464,3.10882688126546,
13.1936399797742));
#252065=CARTESIAN_POINT('Ctrl Pts',(1.11261345672149,3.03417701163737,13.1803029326043));
#252066=CARTESIAN_POINT('Ctrl Pts',(1.37893183780909,2.91330157529856,13.1630634293369));
#252067=CARTESIAN_POINT('Ctrl Pts',(1.42538856681701,2.89085559604023,13.1599888528237));
#252068=CARTESIAN_POINT('Ctrl Pts',(1.49214758121315,2.85659990536123,13.1554614429685));
#252069=CARTESIAN_POINT('Ctrl Pts',(1.51289253948003,2.84566750394746,13.1540389058314));
#252070=CARTESIAN_POINT('Ctrl Pts',(1.54923238495767,2.82600705679663,13.1515183180472));
#252071=CARTESIAN_POINT('Ctrl Pts',(1.56487758611687,2.81737377499035,13.1504236405808));
#252072=CARTESIAN_POINT('Ctrl Pts',(1.59741869759054,2.79906237540298,13.1481264356284));
#252073=CARTESIAN_POINT('Ctrl Pts',(1.61430026898782,2.78936037326888,13.1469230873724));
#252074=CARTESIAN_POINT('Ctrl Pts',(1.6583820652066,2.76349193208171,13.1437496960681));
#252075=CARTESIAN_POINT('Ctrl Pts',(1.68543339541205,2.74707715376231,13.1417707712434));
#252076=CARTESIAN_POINT('Ctrl Pts',(1.80426322779336,2.67255516414074,13.1329341626486));
#252077=CARTESIAN_POINT('Ctrl Pts',(1.89330242268958,2.61023342398971,13.1259239752546));
#252078=CARTESIAN_POINT('Ctrl Pts',(2.14223260359977,2.41655174426798,13.1051712088819));
#252079=CARTESIAN_POINT('Ctrl Pts',(2.29283553839621,2.27415362394656,13.0910872142394));
#252080=CARTESIAN_POINT('Ctrl Pts',(2.50575449385242,2.03003419588436,13.0692981273801));
#252081=CARTESIAN_POINT('Ctrl Pts',(2.57790072315649,1.93759576747014,13.0614993286319));
#252082=CARTESIAN_POINT('Ctrl Pts',(2.66063699322368,1.81876085031963,13.0521924775223));
#252083=CARTESIAN_POINT('Ctrl Pts',(2.67612530448039,1.79589356929337,13.0504327918974));
#252084=CARTESIAN_POINT('Ctrl Pts',(2.6984122254328,1.76205996578632,13.0478778944026));
#252085=CARTESIAN_POINT('Ctrl Pts',(2.70544156284286,1.7512480762753,13.0470686221526));
#252086=CARTESIAN_POINT('Ctrl Pts',(2.7177866054122,1.73200831473337,13.0456415978013));
#252087=CARTESIAN_POINT('Ctrl Pts',(2.72312835127333,1.72359764042373,13.0450221826393));
#252088=CARTESIAN_POINT('Ctrl Pts',(2.7347230950273,1.70515304945076,13.0436734697418));
#252089=CARTESIAN_POINT('Ctrl Pts',(2.74095995180388,1.69510940100128,13.0429452065106));
#252090=CARTESIAN_POINT('Ctrl Pts',(2.75842054246987,1.66664304050818,13.0408977659757));
#252091=CARTESIAN_POINT('Ctrl Pts',(2.76951500334876,1.64814126105842,13.0395865850921));
#252092=CARTESIAN_POINT('Ctrl Pts',(2.85097523481237,1.50914776822978,13.0298708566849));
#252093=CARTESIAN_POINT('Ctrl Pts',(2.91364346287063,1.38429681948049,13.0218891530275));
#252094=CARTESIAN_POINT('Ctrl Pts',(3.04738381157273,1.06819834571415,13.0025347886259));
#252095=CARTESIAN_POINT('Ctrl Pts',(3.10878165776468,0.873539586872534,
12.9913088706737));
#252096=CARTESIAN_POINT('Ctrl Pts',(3.165599608262,0.608031008054314,12.9757109832134));
#252097=CARTESIAN_POINT('Ctrl Pts',(3.17769983394231,0.541244427059038,
12.9717676289282));
#252098=CARTESIAN_POINT('Ctrl Pts',(3.1950345952809,0.424698562499329,12.9648149552288));
#252099=CARTESIAN_POINT('Ctrl Pts',(3.20123565035463,0.375106444609076,
12.9618344360339));
#252100=CARTESIAN_POINT('Ctrl Pts',(3.20861938951724,0.302350091821688,
12.9574203226909));
#252101=CARTESIAN_POINT('Ctrl Pts',(3.21070932288946,0.279284023725336,
12.9560148726176));
#252102=CARTESIAN_POINT('Ctrl Pts',(3.21396788717999,0.238423802997251,
12.953513661383));
#252103=CARTESIAN_POINT('Ctrl Pts',(3.2152377982239,0.220638551757844,12.9524210991844));
#252104=CARTESIAN_POINT('Ctrl Pts',(3.21759426671376,0.183273617033214,
12.9501172531451));
#252105=CARTESIAN_POINT('Ctrl Pts',(3.21864983057021,0.163692776551101,
12.948905050671));
#252106=CARTESIAN_POINT('Ctrl Pts',(3.22097013911627,0.111853116265333,
12.9456823178505));
#252107=CARTESIAN_POINT('Ctrl Pts',(3.22192894167087,0.0795834824832295,
12.9436623971926));
#252108=CARTESIAN_POINT('Ctrl Pts',(3.22410973531638,-0.0689690337821968,
12.9342973552168));
#252109=CARTESIAN_POINT('Ctrl Pts',(3.21952199336371,-0.185238243564716,
12.9267758968677));
#252110=CARTESIAN_POINT('Ctrl Pts',(3.18857647148389,-0.515123457258313,
12.9049121988007));
#252111=CARTESIAN_POINT('Ctrl Pts',(3.14710548087625,-0.726695576877911,
12.8902230967812));
#252112=CARTESIAN_POINT('Ctrl Pts',(3.06305925291084,-1.00472543769805,
12.8707532878309));
#252113=CARTESIAN_POINT('Ctrl Pts',(3.03870811460726,-1.07613174655434,
12.8657428324953));
#252114=CARTESIAN_POINT('Ctrl Pts',(2.99568113575361,-1.18915226412852,
12.8578599058794));
#252115=CARTESIAN_POINT('Ctrl Pts',(2.978589715227,-1.23133763071961,12.8549286438657));
#252116=CARTESIAN_POINT('Ctrl Pts',(2.95442247406637,-1.28753667436181,
12.8510517593429));
#252117=CARTESIAN_POINT('Ctrl Pts',(2.94813047292547,-1.30187924969768,
12.8500648434001));
#252118=CARTESIAN_POINT('Ctrl Pts',(2.93748380060396,-1.32567521985732,
12.848432307294));
#252119=CARTESIAN_POINT('Ctrl Pts',(2.93318750551928,-1.33515427345288,
12.8477832880504));
#252120=CARTESIAN_POINT('Ctrl Pts',(2.92494675392128,-1.35310434121559,
12.8465569650852));
#252121=CARTESIAN_POINT('Ctrl Pts',(2.9210112609994,-1.36157926313022,12.8459791095226));
#252122=CARTESIAN_POINT('Ctrl Pts',(2.91044992670527,-1.38406611667345,
12.8444485851779));
#252123=CARTESIAN_POINT('Ctrl Pts',(2.90375967600479,-1.39804776645132,
12.8434997748723));
#252124=CARTESIAN_POINT('Ctrl Pts',(2.87904855361857,-1.44874770573644,
12.8400675873178));
#252125=CARTESIAN_POINT('Ctrl Pts',(2.86042920244515,-1.48517191280919,
12.8376178685825));
#252126=CARTESIAN_POINT('Ctrl Pts',(2.70114737583583,-1.78265342181489,
12.8176638777577));
#252127=CARTESIAN_POINT('Ctrl Pts',(2.52575118061019,-2.02353037842577,
12.8017313189807));
#252128=CARTESIAN_POINT('Ctrl Pts',(2.26576301680282,-2.29314410800168,
12.7803420927316));
#252129=CARTESIAN_POINT('Ctrl Pts',(2.20964845128471,-2.34726319444911,
12.7758380055377));
#252130=CARTESIAN_POINT('Ctrl Pts',(2.11038564171794,-2.43627977450228,
12.7679975509954));
#252131=CARTESIAN_POINT('Ctrl Pts',(2.06819638864876,-2.47219535168871,
12.7647016432471));
#252132=CARTESIAN_POINT('Ctrl Pts',(2.0063521334228,-2.52215181298464,12.7599086681979));
#252133=CARTESIAN_POINT('Ctrl Pts',(1.98743108663119,-2.53708814959117,
12.7584472734013));
#252134=CARTESIAN_POINT('Ctrl Pts',(1.95411862971046,-2.56278378636093,
12.7558820069196));
#252135=CARTESIAN_POINT('Ctrl Pts',(1.93980133283253,-2.57363772184719,
12.7547819083152));
#252136=CARTESIAN_POINT('Ctrl Pts',(1.91186679139943,-2.59444936274832,
12.7526397918744));
#252137=CARTESIAN_POINT('Ctrl Pts',(1.8982606192465,-2.60442099672753,12.7515983630423));
#252138=CARTESIAN_POINT('Ctrl Pts',(1.86168867002207,-2.63078485859894,
12.7488039069828));
#252139=CARTESIAN_POINT('Ctrl Pts',(1.83858525667503,-2.64698278225353,
12.7470435589161));
#252140=CARTESIAN_POINT('Ctrl Pts',(1.75095070283274,-2.70672295861865,
12.7403830984852));
#252141=CARTESIAN_POINT('Ctrl Pts',(1.6850659004304,-2.74822284581297,12.7354085261731));
#252142=CARTESIAN_POINT('Ctrl Pts',(1.41935142133246,-2.90244371588403,
12.7154655071404));
#252143=CARTESIAN_POINT('Ctrl Pts',(1.20924709610444,-2.99606981572496,
12.6998922332525));
#252144=CARTESIAN_POINT('Ctrl Pts',(0.89837337492101,-3.09653406966299,
12.6778662830106));
#252145=CARTESIAN_POINT('Ctrl Pts',(0.804408848719862,-3.12226306038524,
12.6713430518917));
#252146=CARTESIAN_POINT('Ctrl Pts',(0.673954791905544,-3.15170179833793,
12.6625802457452));
#252147=CARTESIAN_POINT('Ctrl Pts',(0.638356623688517,-3.15910435567473,
12.6602187381818));
#252148=CARTESIAN_POINT('Ctrl Pts',(0.576358239115391,-3.17090593803914,
12.6561656727509));
#252149=CARTESIAN_POINT('Ctrl Pts',(0.550014829495976,-3.17558137701367,
12.6544620957646));
#252150=CARTESIAN_POINT('Ctrl Pts',(0.511051678742976,-3.1819971508875,
12.6519727925185));
#252151=CARTESIAN_POINT('Ctrl Pts',(0.498475668353988,-3.18399147414252,
12.6511739792801));
#252152=CARTESIAN_POINT('Ctrl Pts',(0.476990971310048,-3.18726813630295,
12.6498176091965));
#252153=CARTESIAN_POINT('Ctrl Pts',(0.468088332760631,-3.18858775620315,
12.6492580145221));
#252154=CARTESIAN_POINT('Ctrl Pts',(0.447757694539533,-3.19151433974754,
12.6479857245787));
#252155=CARTESIAN_POINT('Ctrl Pts',(0.436326488107356,-3.19309723296441,
12.6472743736533));
#252156=CARTESIAN_POINT('Ctrl Pts',(0.404753393820786,-3.19729647952879,
12.6453200759619));
#252157=CARTESIAN_POINT('Ctrl Pts',(0.38459451932365,-3.19978392882761,
12.6440840208563));
#252158=CARTESIAN_POINT('Ctrl Pts',(0.271988327922241,-3.21259908011242,
12.6372381695844));
#252159=CARTESIAN_POINT('Ctrl Pts',(0.17914281766099,-3.21911192069469,
12.6318134859512));
#252160=CARTESIAN_POINT('Ctrl Pts',(-0.0820541417697187,-3.22609568725263,
12.6168509453061));
#252161=CARTESIAN_POINT('Ctrl Pts',(-0.250346099388465,-3.21741478542948,
12.6075463005668));
#252162=CARTESIAN_POINT('Ctrl Pts',(-0.593129813908984,-3.17266366030316,
12.5881134168657));
#252163=CARTESIAN_POINT('Ctrl Pts',(-0.766844646278213,-3.13520908200744,
12.5779952479085));
#252164=CARTESIAN_POINT('Ctrl Pts',(-0.969558580437706,-3.0736397602419,
12.5653516299413));
#252165=CARTESIAN_POINT('Ctrl Pts',(-1.00236976531824,-3.06309646168907,
12.5632789548714));
#252166=CARTESIAN_POINT('Ctrl Pts',(-1.05401915463539,-3.0455811128256,
12.5599717030636));
#252167=CARTESIAN_POINT('Ctrl Pts',(-1.07297264065034,-3.03895547472312,
12.5587484554414));
#252168=CARTESIAN_POINT('Ctrl Pts',(-1.10855182729945,-3.02614359433572,
12.5564334887025));
#252169=CARTESIAN_POINT('Ctrl Pts',(-1.12519083083141,-3.01999632147912,
12.5553430914077));
#252170=CARTESIAN_POINT('Ctrl Pts',(-1.16266280694771,-3.00579965110571,
12.5528694460832));
#252171=CARTESIAN_POINT('Ctrl Pts',(-1.18346438730582,-2.99767048710597,
12.5514835872462));
#252172=CARTESIAN_POINT('Ctrl Pts',(-1.24500369056506,-2.97288083146991,
12.5473450454687));
#252173=CARTESIAN_POINT('Ctrl Pts',(-1.28548512443879,-2.95560185374097,
12.5445718733274));
#252174=CARTESIAN_POINT('Ctrl Pts',(-1.53068104161221,-2.84495288642643,
12.527454613147));
#252175=CARTESIAN_POINT('Ctrl Pts',(-1.7254753658575,-2.73119835378743,
12.5124102001004));
#252176=CARTESIAN_POINT('Ctrl Pts',(-2.01632944886312,-2.51773496695751,
12.4880284723794));
#252177=CARTESIAN_POINT('Ctrl Pts',(-2.12066464762074,-2.43050582611848,
12.478830284359));
#252178=CARTESIAN_POINT('Ctrl Pts',(-2.25129371644323,-2.30645932524984,
12.4669508460402));
#252179=CARTESIAN_POINT('Ctrl Pts',(-2.28277062809379,-2.27531023125222,
12.4640581776777));
#252180=CARTESIAN_POINT('Ctrl Pts',(-2.335211470524,-2.22123140567934,12.4592013210175));
#252181=CARTESIAN_POINT('Ctrl Pts',(-2.3565035845879,-2.19862970707747,
12.4572182402297));
#252182=CARTESIAN_POINT('Ctrl Pts',(-2.38658940270406,-2.16575418409494,
12.4544044977161));
#252183=CARTESIAN_POINT('Ctrl Pts',(-2.39564960061816,-2.15572799054074,
12.4535555938201));
#252184=CARTESIAN_POINT('Ctrl Pts',(-2.41132281878493,-2.13816285122721,
12.452084805416));
#252185=CARTESIAN_POINT('Ctrl Pts',(-2.41796411262604,-2.1306495899775,
12.4514608733639));
#252186=CARTESIAN_POINT('Ctrl Pts',(-2.4320976959166,-2.11450914169073,
12.450131660481));
#252187=CARTESIAN_POINT('Ctrl Pts',(-2.43957926818679,-2.10587300573941,
12.4494271429783));
#252188=CARTESIAN_POINT('Ctrl Pts',(-2.45990438737667,-2.08215760532906,
12.4475101193186));
#252189=CARTESIAN_POINT('Ctrl Pts',(-2.47265533060186,-2.06699916518631,
12.4463040833927));
#252190=CARTESIAN_POINT('Ctrl Pts',(-2.54048122110357,-1.98484122956432,
12.4398643901706));
#252191=CARTESIAN_POINT('Ctrl Pts',(-2.59297905393479,-1.91575098536107,
12.4347915702413));
#252192=CARTESIAN_POINT('Ctrl Pts',(-2.74159201450701,-1.70284600077162,
12.4198784977412));
#252193=CARTESIAN_POINT('Ctrl Pts',(-2.82898927922521,-1.55333086609714,
12.4103201763135));
#252194=CARTESIAN_POINT('Ctrl Pts',(-2.97521011732739,-1.24949167868997,
12.3913725737308));
#252195=CARTESIAN_POINT('Ctrl Pts',(-3.03501794846586,-1.09624922720985,
12.3820249483289));
#252196=CARTESIAN_POINT('Ctrl Pts',(-3.09560811580426,-0.897348988973454,
12.3697032977783));
#252197=CARTESIAN_POINT('Ctrl Pts',(-3.10748340485557,-0.855319491042631,
12.3670904620207));
#252198=CARTESIAN_POINT('Ctrl Pts',(-3.12404455585508,-0.791799256289775,
12.3631218490914));
#252199=CARTESIAN_POINT('Ctrl Pts',(-3.1293707795958,-0.770479679372991,
12.3617865514438));
#252200=CARTESIAN_POINT('Ctrl Pts',(-3.13859473982219,-0.731884021168136,
12.3593625396258));
#252201=CARTESIAN_POINT('Ctrl Pts',(-3.14256891921135,-0.714626986368407,
12.3582763146423));
#252202=CARTESIAN_POINT('Ctrl Pts',(-3.15079806254323,-0.677496973424845,
12.355933696335));
#252203=CARTESIAN_POINT('Ctrl Pts',(-3.15500765292982,-0.657614826345666,
12.3546759112392));
#252204=CARTESIAN_POINT('Ctrl Pts',(-3.16589156815588,-0.603697787038005,
12.3512553003437));
#252205=CARTESIAN_POINT('Ctrl Pts',(-3.17220482578302,-0.569593568217683,
12.3490812031752));
#252206=CARTESIAN_POINT('Ctrl Pts',(-3.20777462945284,-0.358460464424845,
12.3355529419085));
#252207=CARTESIAN_POINT('Ctrl Pts',(-3.22275000000872,-0.179374813335885,
12.3237542306299));
#252208=CARTESIAN_POINT('Ctrl Pts',(-3.22275,1.56749301039039E-10,12.3117125106066));
#252209=CARTESIAN_POINT('',(-3.22274905501283,0.00246797769559721,13.3127140476874));
#252210=CARTESIAN_POINT('Ctrl Pts',(-3.22275,-3.23896726357594E-13,12.0672299157825));
#252211=CARTESIAN_POINT('Ctrl Pts',(-3.22275,-0.0108116653985819,12.0679011082235));
#252212=CARTESIAN_POINT('Ctrl Pts',(-3.22269559361987,-0.0216234471182378,
12.06856923911));
#252213=CARTESIAN_POINT('Ctrl Pts',(-3.22241450571572,-0.0495510558761717,
12.070287609666));
#252214=CARTESIAN_POINT('Ctrl Pts',(-3.22210586925214,-0.0666659614557475,
12.0713334426425));
#252215=CARTESIAN_POINT('Ctrl Pts',(-3.2202005696579,-0.139933736446529,
12.0757826669111));
#252216=CARTESIAN_POINT('Ctrl Pts',(-3.21727216450677,-0.196045427098966,
12.0791198911071));
#252217=CARTESIAN_POINT('Ctrl Pts',(-3.20480015512225,-0.355022549124413,
12.0884469850227));
#252218=CARTESIAN_POINT('Ctrl Pts',(-3.19177644294579,-0.45754887858188,
12.0943105410957));
#252219=CARTESIAN_POINT('Ctrl Pts',(-3.13010123346049,-0.807549566361406,
12.1143090446839));
#252220=CARTESIAN_POINT('Ctrl Pts',(-3.05737824815079,-1.04980990205459,
12.1281950979036));
#252221=CARTESIAN_POINT('Ctrl Pts',(-2.93547912218258,-1.33118640648984,
12.1462284142651));
#252222=CARTESIAN_POINT('Ctrl Pts',(-2.91252111456401,-1.38069372805963,
12.1494742179247));
#252223=CARTESIAN_POINT('Ctrl Pts',(-2.8784642380786,-1.44950152486143,
12.1541011009358));
#252224=CARTESIAN_POINT('Ctrl Pts',(-2.86840468768796,-1.46930784746499,
12.1554467177226));
#252225=CARTESIAN_POINT('Ctrl Pts',(-2.84960352252361,-1.50539655882529,
12.1579247050641));
#252226=CARTESIAN_POINT('Ctrl Pts',(-2.84092502346485,-1.52171088706322,
12.1590548447711));
#252227=CARTESIAN_POINT('Ctrl Pts',(-2.82300648447529,-1.55470756187721,
12.1613613364517));
#252228=CARTESIAN_POINT('Ctrl Pts',(-2.81375772580421,-1.57138431012968,
12.1625379633914));
#252229=CARTESIAN_POINT('Ctrl Pts',(-2.79036972352057,-1.61268741928556,
12.1654798759273));
#252230=CARTESIAN_POINT('Ctrl Pts',(-2.77605218521744,-1.63721045962063,
12.1672514651459));
#252231=CARTESIAN_POINT('Ctrl Pts',(-2.718509850971,-1.73284348207593,12.174260547335));
#252232=CARTESIAN_POINT('Ctrl Pts',(-2.67286474218635,-1.80245233546225,
12.1795844814411));
#252233=CARTESIAN_POINT('Ctrl Pts',(-2.54308215496004,-1.98458397715925,
12.1941305601796));
#252234=CARTESIAN_POINT('Ctrl Pts',(-2.45420250009073,-2.09349557860879,
12.2035060361056));
#252235=CARTESIAN_POINT('Ctrl Pts',(-2.21182236916084,-2.35378254601469,
12.2274858429146));
#252236=CARTESIAN_POINT('Ctrl Pts',(-2.04971070038907,-2.49622691209908,
12.2421770468629));
#252237=CARTESIAN_POINT('Ctrl Pts',(-1.85423266076305,-2.63601321068126,
12.2576243171508));
#252238=CARTESIAN_POINT('Ctrl Pts',(-1.83369743965594,-2.65033926004513,
12.2592211010892));
#252239=CARTESIAN_POINT('Ctrl Pts',(-1.8024791572505,-2.67158160734804,
12.2616072363407));
#252240=CARTESIAN_POINT('Ctrl Pts',(-1.79191917100987,-2.67867599647793,
12.2624073559749));
#252241=CARTESIAN_POINT('Ctrl Pts',(-1.77268406442479,-2.6914338352571,
12.2638516898458));
#252242=CARTESIAN_POINT('Ctrl Pts',(-1.76402311780433,-2.69711833870525,
12.2644972572148));
#252243=CARTESIAN_POINT('Ctrl Pts',(-1.74602198009665,-2.70880935362435,
12.2658289445407));
#252244=CARTESIAN_POINT('Ctrl Pts',(-1.73667794416686,-2.71480949536175,
12.2665146581029));
#252245=CARTESIAN_POINT('Ctrl Pts',(-1.71197464127018,-2.73049263773251,
12.2683134833816));
#252246=CARTESIAN_POINT('Ctrl Pts',(-1.69656399656217,-2.74009449787688,
12.2694214562857));
#252247=CARTESIAN_POINT('Ctrl Pts',(-1.62386938675995,-2.78453966664293,
12.2745857500193));
#252248=CARTESIAN_POINT('Ctrl Pts',(-1.56558428644953,-2.81772250728463,
12.2785466805345));
#252249=CARTESIAN_POINT('Ctrl Pts',(-1.38327350089099,-2.91411031461053,
12.2905246266551));
#252250=CARTESIAN_POINT('Ctrl Pts',(-1.25615251529448,-2.97112275763455,
12.2983144308984));
#252251=CARTESIAN_POINT('Ctrl Pts',(-0.92090602837082,-3.09610012212812,
12.3183473134052));
#252252=CARTESIAN_POINT('Ctrl Pts',(-0.708861001783567,-3.15141356978549,
12.3305775561813));
#252253=CARTESIAN_POINT('Ctrl Pts',(-0.44883818415889,-3.19165257520775,
12.3461548236979));
#252254=CARTESIAN_POINT('Ctrl Pts',(-0.40468173066267,-3.19755129544435,
12.3488176651532));
#252255=CARTESIAN_POINT('Ctrl Pts',(-0.33782706892861,-3.20507523806276,
12.3528823069357));
#252256=CARTESIAN_POINT('Ctrl Pts',(-0.315209591367845,-3.20737856872806,
12.3542630655217));
#252257=CARTESIAN_POINT('Ctrl Pts',(-0.274514189483198,-3.21108832739476,
12.3567584265936));
#252258=CARTESIAN_POINT('Ctrl Pts',(-0.256445035621723,-3.21258186031607,
12.3578702696548));
#252259=CARTESIAN_POINT('Ctrl Pts',(-0.217810459464257,-3.21544724101161,
12.3602562510899));
#252260=CARTESIAN_POINT('Ctrl Pts',(-0.197242632622954,-3.21677441990757,
12.3615317276216));
#252261=CARTESIAN_POINT('Ctrl Pts',(-0.141088100996727,-3.21985731977652,
12.3650290063479));
#252262=CARTESIAN_POINT('Ctrl Pts',(-0.105483590736053,-3.22122027530737,
12.3672628404062));
#252263=CARTESIAN_POINT('Ctrl Pts',(0.135150039778801,-3.22643811629139,
12.3824762249249));
#252264=CARTESIAN_POINT('Ctrl Pts',(0.340086804586179,-3.21130558336976,
12.3960463404819));
#252265=CARTESIAN_POINT('Ctrl Pts',(0.759497727149738,-3.13972768514377,
12.4247186045829));
#252266=CARTESIAN_POINT('Ctrl Pts',(0.972462498864557,-3.0804311012453,
12.4397823840852));
#252267=CARTESIAN_POINT('Ctrl Pts',(1.20303459997072,-2.98991057316739,
12.4556962333496));
#252268=CARTESIAN_POINT('Ctrl Pts',(1.22822883655403,-2.97964956350198,
12.4574288926517));
#252269=CARTESIAN_POINT('Ctrl Pts',(1.26525465708179,-2.96402038548086,
12.4599628554394));
#252270=CARTESIAN_POINT('Ctrl Pts',(1.27718786066931,-2.9588980000777,12.4607776162736));
#252271=CARTESIAN_POINT('Ctrl Pts',(1.29841747619625,-2.94963272171546,
12.4622232501823));
#252272=CARTESIAN_POINT('Ctrl Pts',(1.30772557412219,-2.94551777566178,
12.4628557271971));
#252273=CARTESIAN_POINT('Ctrl Pts',(1.32821835710458,-2.93634198500777,
12.4642451676979));
#252274=CARTESIAN_POINT('Ctrl Pts',(1.33939373822714,-2.93126127843539,
12.4650009291463));
#252275=CARTESIAN_POINT('Ctrl Pts',(1.37198439257983,-2.9162191639148,12.4672000207704));
#252276=CARTESIAN_POINT('Ctrl Pts',(1.39332001465352,-2.90608582039925,
12.468633411942));
#252277=CARTESIAN_POINT('Ctrl Pts',(1.5683549204797,-2.8205822053027,12.4803564929219));
#252278=CARTESIAN_POINT('Ctrl Pts',(1.71595641474372,-2.73330012597788,
12.4900182227751));
#252279=CARTESIAN_POINT('Ctrl Pts',(2.05768908746965,-2.49257571272217,
12.5134599421667));
#252280=CARTESIAN_POINT('Ctrl Pts',(2.24242730152477,-2.32777255850444,
12.527153345655));
#252281=CARTESIAN_POINT('Ctrl Pts',(2.43254262309196,-2.1143276402088,12.5440962445621));
#252282=CARTESIAN_POINT('Ctrl Pts',(2.45800305580413,-2.0846740194608,12.5464326937897));
#252283=CARTESIAN_POINT('Ctrl Pts',(2.4978504954696,-2.036518881496,12.5502042128577));
#252284=CARTESIAN_POINT('Ctrl Pts',(2.51258632278443,-2.01831022858024,
12.5516252842279));
#252285=CARTESIAN_POINT('Ctrl Pts',(2.53844879580541,-1.98563048282747,
12.5541677630924));
#252286=CARTESIAN_POINT('Ctrl Pts',(2.54965355446168,-1.9712223197959,12.5552860172622));
#252287=CARTESIAN_POINT('Ctrl Pts',(2.57287431879275,-1.94083359389321,
12.5576393676332));
#252288=CARTESIAN_POINT('Ctrl Pts',(2.5848651747574,-1.92483487584867,12.5588753778602));
#252289=CARTESIAN_POINT('Ctrl Pts',(2.61610534813925,-1.88233450886695,
12.5621516481261));
#252290=CARTESIAN_POINT('Ctrl Pts',(2.63510045191288,-1.85564971861654,
12.5642014980096));
#252291=CARTESIAN_POINT('Ctrl Pts',(2.72858158420027,-1.71999483726189,
12.5745894499862));
#252292=CARTESIAN_POINT('Ctrl Pts',(2.79672122269646,-1.60682375380725,
12.5831588671375));
#252293=CARTESIAN_POINT('Ctrl Pts',(2.92073442302465,-1.36894337336954,
12.6009464482311));
#252294=CARTESIAN_POINT('Ctrl Pts',(2.9760093246865,-1.24421071456987,12.6101592313755));
#252295=CARTESIAN_POINT('Ctrl Pts',(3.03916628701579,-1.07317528191686,
12.6224774611929));
#252296=CARTESIAN_POINT('Ctrl Pts',(3.05418626554493,-1.02965200465071,
12.6255850428885));
#252297=CARTESIAN_POINT('Ctrl Pts',(3.1065133206303,-0.866789382905741,
12.6370866928499));
#252298=CARTESIAN_POINT('Ctrl Pts',(3.13780283494966,-0.745619637495051,
12.6453974488158));
#252299=CARTESIAN_POINT('Ctrl Pts',(3.16614987928917,-0.601730212744978,
12.6547666806572));
#252300=CARTESIAN_POINT('Ctrl Pts',(3.1701126605227,-0.58049124414732,12.6561369635489));
#252301=CARTESIAN_POINT('Ctrl Pts',(3.17594126178828,-0.547410537029383,
12.6582499091828));
#252302=CARTESIAN_POINT('Ctrl Pts',(3.1779550301302,-0.535595959267617,
12.6590003198636));
#252303=CARTESIAN_POINT('Ctrl Pts',(3.18156149502111,-0.5137004638538,12.6603828841193));
#252304=CARTESIAN_POINT('Ctrl Pts',(3.18317222925918,-0.503623148651342,
12.6610159787355));
#252305=CARTESIAN_POINT('Ctrl Pts',(3.1867832007952,-0.480322025424383,
12.6624725607338));
#252306=CARTESIAN_POINT('Ctrl Pts',(3.18874902365361,-0.467093240840651,
12.6632941393678));
#252307=CARTESIAN_POINT('Ctrl Pts',(3.19475606490874,-0.424863071571294,
12.6659008450927));
#252308=CARTESIAN_POINT('Ctrl Pts',(3.19848453792757,-0.395817810729946,
12.6676696519372));
#252309=CARTESIAN_POINT('Ctrl Pts',(3.21665618253989,-0.237163961044718,
12.6772200842411));
#252310=CARTESIAN_POINT('Ctrl Pts',(3.22361951518452,-0.106807994125102,
12.6846655259858));
#252311=CARTESIAN_POINT('Ctrl Pts',(3.22097457393141,0.254016113668192,
12.7050046911416));
#252312=CARTESIAN_POINT('Ctrl Pts',(3.19458544268126,0.483551503888421,
12.7176860567073));
#252313=CARTESIAN_POINT('Ctrl Pts',(3.12725151356476,0.782423885700084,
12.7354822964245));
#252314=CARTESIAN_POINT('Ctrl Pts',(3.10793989867352,0.855919069656302,
12.7399600410749));
#252315=CARTESIAN_POINT('Ctrl Pts',(3.07789030556825,0.955777596185538,
12.7462195377369));
#252316=CARTESIAN_POINT('Ctrl Pts',(3.06937299764526,0.982786279327296,
12.7479303971352));
#252317=CARTESIAN_POINT('Ctrl Pts',(3.05512807243269,1.02596497961939,12.7506958691305));
#252318=CARTESIAN_POINT('Ctrl Pts',(3.0496252524777,1.04220798316683,12.7517431404847));
#252319=CARTESIAN_POINT('Ctrl Pts',(3.03793789795327,1.07582100609374,12.7539251830342));
#252320=CARTESIAN_POINT('Ctrl Pts',(3.03173342818392,1.09318338220801,12.7550605760712));
#252321=CARTESIAN_POINT('Ctrl Pts',(3.01674711674301,1.13401152181053,12.7577505294154));
#252322=CARTESIAN_POINT('Ctrl Pts',(3.00784003044211,1.15742973560635,12.7593091784661));
#252323=CARTESIAN_POINT('Ctrl Pts',(2.97697109858458,1.23582579891384,12.7645813691162));
#252324=CARTESIAN_POINT('Ctrl Pts',(2.95376872060867,1.29029916666848,12.7683357026217));
#252325=CARTESIAN_POINT('Ctrl Pts',(2.89367126342721,1.42126434581914,12.7775903954254));
#252326=CARTESIAN_POINT('Ctrl Pts',(2.85522913879484,1.49699378489056,12.7831380543887));
#252327=CARTESIAN_POINT('Ctrl Pts',(2.74551070657163,1.69349824737261,12.7980408025117));
#252328=CARTESIAN_POINT('Ctrl Pts',(2.66926832270308,1.81128897407097,12.807513174005));
#252329=CARTESIAN_POINT('Ctrl Pts',(2.5631115958955,1.95396944977359,12.8195287745353));
#252330=CARTESIAN_POINT('Ctrl Pts',(2.54008825317846,1.98380678795915,12.8220731677239));
#252331=CARTESIAN_POINT('Ctrl Pts',(2.43294956760782,2.11773039346671,12.8336217887591));
#252332=CARTESIAN_POINT('Ctrl Pts',(2.34291559360804,2.21693021938233,12.8425413711901));
#252333=CARTESIAN_POINT('Ctrl Pts',(2.23133919773066,2.32545008280748,12.8524872643093));
#252334=CARTESIAN_POINT('Ctrl Pts',(2.2155590606225,2.34048943839346,12.853870060507));
#252335=CARTESIAN_POINT('Ctrl Pts',(2.19083653107725,2.36357727235018,12.8559981191068));
#252336=CARTESIAN_POINT('Ctrl Pts',(2.18199994746851,2.37173743664087,12.8567512995002));
#252337=CARTESIAN_POINT('Ctrl Pts',(2.16558558665581,2.38672593045997,12.8581363170549));
#252338=CARTESIAN_POINT('Ctrl Pts',(2.15802102212413,2.39356781235491,12.8587691248359));
#252339=CARTESIAN_POINT('Ctrl Pts',(2.14050900894474,2.40925630513186,12.8602216600435));
#252340=CARTESIAN_POINT('Ctrl Pts',(2.13053910306067,2.41807731593574,12.8610395179291));
#252341=CARTESIAN_POINT('Ctrl Pts',(2.0987203477208,2.44587982210592,12.8636220515042));
#252342=CARTESIAN_POINT('Ctrl Pts',(2.07666967631904,2.46462946261879,12.8653708295544));
#252343=CARTESIAN_POINT('Ctrl Pts',(1.95640680614481,2.56412856777508,12.8747089927733));
#252344=CARTESIAN_POINT('Ctrl Pts',(1.85372413750043,2.63931739258312,12.8819783878121));
#252345=CARTESIAN_POINT('Ctrl Pts',(1.56098937823813,2.82813536626981,12.90163027055));
#252346=CARTESIAN_POINT('Ctrl Pts',(1.36328168961745,2.92856598854802,12.9138040341982));
#252347=CARTESIAN_POINT('Ctrl Pts',(1.07648000843115,3.03886866487142,12.9315655452101));
#252348=CARTESIAN_POINT('Ctrl Pts',(0.99491114224724,3.06654234560991,12.9366214159458));
#252349=CARTESIAN_POINT('Ctrl Pts',(0.883911754314504,3.09930572080196,
12.9435592611539));
#252350=CARTESIAN_POINT('Ctrl Pts',(0.855373062985978,3.10730313545883,
12.9453479159326));
#252351=CARTESIAN_POINT('Ctrl Pts',(0.808048001081882,3.11986370637131,
12.9483238931976));
#252352=CARTESIAN_POINT('Ctrl Pts',(0.789323275947957,3.1246535582669,12.9495039063071));
#252353=CARTESIAN_POINT('Ctrl Pts',(0.752571737535052,3.13370330792907,
12.9518253974347));
#252354=CARTESIAN_POINT('Ctrl Pts',(0.734549023204998,3.13797679280485,
12.9529663900513));
#252355=CARTESIAN_POINT('Ctrl Pts',(0.691578066684137,3.14777544537713,
12.9556933160061));
#252356=CARTESIAN_POINT('Ctrl Pts',(0.666599280645446,3.1531596559746,12.9572836536412));
#252357=CARTESIAN_POINT('Ctrl Pts',(0.58046935611948,3.1706559128626,12.9627864206629));
#252358=CARTESIAN_POINT('Ctrl Pts',(0.51903548494956,3.18128981754247,12.9667446629822));
#252359=CARTESIAN_POINT('Ctrl Pts',(0.367029604247455,3.20308125393506,
12.9766250369327));
#252360=CARTESIAN_POINT('Ctrl Pts',(0.276221976231348,3.21218607373902,
12.9826033785493));
#252361=CARTESIAN_POINT('Ctrl Pts',(0.0524266143072708,3.22506504934053,
12.9974921978879));
#252362=CARTESIAN_POINT('Ctrl Pts',(-0.0806429826780814,3.22448237731509,
13.0064828006704));
#252363=CARTESIAN_POINT('Ctrl Pts',(-0.262392435181865,3.21242735997643,
13.0187879061566));
#252364=CARTESIAN_POINT('Ctrl Pts',(-0.311415627205631,3.20804609746697,
13.0221086069927));
#252365=CARTESIAN_POINT('Ctrl Pts',(-0.47895269091911,3.18919641864129,
13.0334317628747));
#252366=CARTESIAN_POINT('Ctrl Pts',(-0.59676503580555,3.16926596555096,
13.0413532599369));
#252367=CARTESIAN_POINT('Ctrl Pts',(-0.734136456740328,3.13809204692987,
13.0503510009613));
#252368=CARTESIAN_POINT('Ctrl Pts',(-0.755015641236812,3.13313412901258,
13.0517118595416));
#252369=CARTESIAN_POINT('Ctrl Pts',(-0.787444994441657,3.12509052616088,
13.0538134158527));
#252370=CARTESIAN_POINT('Ctrl Pts',(-0.799029731764655,3.12214860542844,
13.0545617344599));
#252371=CARTESIAN_POINT('Ctrl Pts',(-0.820385712246099,3.11659864498664,
13.0559364129018));
#252372=CARTESIAN_POINT('Ctrl Pts',(-0.830161110617933,3.11400905021913,
13.056563744027));
#252373=CARTESIAN_POINT('Ctrl Pts',(-0.852826989807537,3.10789032818082,
13.0580140430726));
#252374=CARTESIAN_POINT('Ctrl Pts',(-0.865707880587451,3.10432698769259,
13.058835060059));
#252375=CARTESIAN_POINT('Ctrl Pts',(-0.906689103639183,3.09271511927801,
13.0614381073684));
#252376=CARTESIAN_POINT('Ctrl Pts',(-0.93470311424843,3.08436414225242,
13.0632038817703));
#252377=CARTESIAN_POINT('Ctrl Pts',(-1.08657964048925,3.03683036332583,
13.0727219313425));
#252378=CARTESIAN_POINT('Ctrl Pts',(-1.20811232344508,2.99056274072579,
13.0801405192197));
#252379=CARTESIAN_POINT('Ctrl Pts',(-1.53516340042591,2.84285028010065,
13.1003710269674));
#252380=CARTESIAN_POINT('Ctrl Pts',(-1.73315211754213,2.72666557733372,
13.1129711417625));
#252381=CARTESIAN_POINT('Ctrl Pts',(-1.97948173744517,2.54436258243106,
13.1307583469665));
#252382=CARTESIAN_POINT('Ctrl Pts',(-2.04011481872142,2.49600862429209,
13.1353253715005));
#252383=CARTESIAN_POINT('Ctrl Pts',(-2.12059934712943,2.42693026424612,
13.1416904261008));
#252384=CARTESIAN_POINT('Ctrl Pts',(-2.14200798631051,2.40805602227281,
13.1434143185947));
#252385=CARTESIAN_POINT('Ctrl Pts',(-2.17590532109481,2.37736179648213,
13.1461953519196));
#252386=CARTESIAN_POINT('Ctrl Pts',(-2.18855529557036,2.36572161891581,
13.1472449918131));
#252387=CARTESIAN_POINT('Ctrl Pts',(-2.21455954665957,2.34140610698522,
13.1494276984574));
#252388=CARTESIAN_POINT('Ctrl Pts',(-2.22789951029634,2.328716447612,13.1505613528939));
#252389=CARTESIAN_POINT('Ctrl Pts',(-2.24159867544874,2.3154596447477,13.1517402787114));
#252390=CARTESIAN_POINT('Ctrl Pts',(-2.2420674178426,2.31500576286028,13.1517806358802));
#252391=CARTESIAN_POINT('Ctrl Pts',(-2.25808350758134,2.2994880029553,13.1531601849085));
#252392=CARTESIAN_POINT('Ctrl Pts',(-2.27347850635729,2.28426829591267,
13.1545061103698));
#252393=CARTESIAN_POINT('Ctrl Pts',(-2.32481767671573,2.23248056523255,
13.159062890899));
#252394=CARTESIAN_POINT('Ctrl Pts',(-2.36004069270859,2.19521164223313,
13.1623044486392));
#252395=CARTESIAN_POINT('Ctrl Pts',(-2.44158482961055,2.10469935224396,
13.1700931062916));
#252396=CARTESIAN_POINT('Ctrl Pts',(-2.48707433785513,2.05074521609687,
13.1746708089397));
#252397=CARTESIAN_POINT('Ctrl Pts',(-2.63738370747775,1.8601034402774,13.1906184533807));
#252398=CARTESIAN_POINT('Ctrl Pts',(-2.73299312892165,1.71654216275024,
13.2022626838592));
#252399=CARTESIAN_POINT('Ctrl Pts',(-2.82960754566598,1.54277274100984,
13.2156920595346));
#252400=CARTESIAN_POINT('Ctrl Pts',(-2.8422579722284,1.51934072146388,13.2174893068008));
#252401=CARTESIAN_POINT('Ctrl Pts',(-2.91868461735447,1.37348204504094,
13.2285843055178));
#252402=CARTESIAN_POINT('Ctrl Pts',(-2.97483747244983,1.24720599821555,
13.2377967686764));
#252403=CARTESIAN_POINT('Ctrl Pts',(-3.03030237718131,1.09720678875932,
13.2480167627886));
#252404=CARTESIAN_POINT('Ctrl Pts',(-3.03767383326058,1.07663038086709,
13.249403310659));
#252405=CARTESIAN_POINT('Ctrl Pts',(-3.04878088649798,1.04460406108585,
13.2515358982324));
#252406=CARTESIAN_POINT('Ctrl Pts',(-3.05266244826398,1.03320594566034,
13.2522899072096));
#252407=CARTESIAN_POINT('Ctrl Pts',(-3.05971353362597,1.01211395635714,
13.2536756646648));
#252408=CARTESIAN_POINT('Ctrl Pts',(-3.06290095363996,1.0024267159078,13.2543083925862));
#252409=CARTESIAN_POINT('Ctrl Pts',(-3.07013731548548,0.980077109436237,
13.2557597436963));
#252410=CARTESIAN_POINT('Ctrl Pts',(-3.07415395166695,0.967404657883401,
13.2565765088654));
#252411=CARTESIAN_POINT('Ctrl Pts',(-3.08663656168474,0.927159215834664,
13.2591519718711));
#252412=CARTESIAN_POINT('Ctrl Pts',(-3.09481110469368,0.899496431827873,
13.2608948946132));
#252413=CARTESIAN_POINT('Ctrl Pts',(-3.13674971870449,0.750230236260733,
13.2701717119449));
#252414=CARTESIAN_POINT('Ctrl Pts',(-3.16372351484846,0.626820695123975,
13.2773902213747));
#252415=CARTESIAN_POINT('Ctrl Pts',(-3.20946250911634,0.33684920937127,
13.2939553016046));
#252416=CARTESIAN_POINT('Ctrl Pts',(-3.22262092036357,0.169789514087309,
13.3032126210189));
#252417=CARTESIAN_POINT('Ctrl Pts',(-3.22274905501283,0.00246797769559721,
13.3127140476874));
#252418=CARTESIAN_POINT('Ctrl Pts',(-3.22274905766543,0.002464511434038,
13.3127142445206));
#252419=CARTESIAN_POINT('Ctrl Pts',(-3.2227496858912,0.00164300417895,13.3127608941841));
#252420=CARTESIAN_POINT('Ctrl Pts',(-3.22275000000001,0.000821500300428959,
13.312807548805));
#252421=CARTESIAN_POINT('Ctrl Pts',(-3.22275,-2.24100014615096E-11,13.3128542084224));
#252422=CARTESIAN_POINT('Origin',(0.,0.,-2.31077344927308));
#252423=CARTESIAN_POINT('',(-3.22275,1.96138700782895E-11,14.8083262771147));
#252424=CARTESIAN_POINT('',(-3.22275,-2.92740584967668E-11,14.5620312016861));
#252425=CARTESIAN_POINT('',(-3.22275,-3.50678552687464E-13,-2.31077344927308));
#252426=CARTESIAN_POINT('',(-3.22274971943303,-0.00134476552198701,13.5633807678595));
#252427=CARTESIAN_POINT('Ctrl Pts',(-3.22274999999999,1.96136509811318E-11,
14.8083262771147));
#252428=CARTESIAN_POINT('Ctrl Pts',(-3.22275,0.148140140194331,14.7997354942855));
#252429=CARTESIAN_POINT('Ctrl Pts',(-3.21253566175653,0.296114577246409,
14.7914703204814));
#252430=CARTESIAN_POINT('Ctrl Pts',(-3.16369340120223,0.64816620807127,
14.7715750645874));
#252431=CARTESIAN_POINT('Ctrl Pts',(-3.11547760387864,0.850213307944121,
14.7599397844463));
#252432=CARTESIAN_POINT('Ctrl Pts',(-3.03356085628352,1.08888020164107,
14.7450014001518));
#252433=CARTESIAN_POINT('Ctrl Pts',(-3.01802653476388,1.13122371791246,
14.742305122163));
#252434=CARTESIAN_POINT('Ctrl Pts',(-2.99350871717841,1.19395069523688,
14.7382350415779));
#252435=CARTESIAN_POINT('Ctrl Pts',(-2.98519381711226,1.21459068770951,
14.7368833542097));
#252436=CARTESIAN_POINT('Ctrl Pts',(-2.96987051709815,1.25151949960226,
14.7344417096045));
#252437=CARTESIAN_POINT('Ctrl Pts',(-2.96294010309425,1.26783984476883,
14.7333544071053));
#252438=CARTESIAN_POINT('Ctrl Pts',(-2.94785415913837,1.30256619407087,
14.7310228085355));
#252439=CARTESIAN_POINT('Ctrl Pts',(-2.93966015860541,1.32095456250108,
14.7297772436186));
#252440=CARTESIAN_POINT('Ctrl Pts',(-2.9168698715098,1.37083644777244,14.7263679274287));
#252441=CARTESIAN_POINT('Ctrl Pts',(-2.9019365236218,1.40217212803042,14.724192761338));
#252442=CARTESIAN_POINT('Ctrl Pts',(-2.80393653046073,1.59953834891227,
14.7102740193285));
#252443=CARTESIAN_POINT('Ctrl Pts',(-2.70717279067632,1.75834545936386,
14.6980515599366));
#252444=CARTESIAN_POINT('Ctrl Pts',(-2.48884107283377,2.05556538518971,
14.6732698896435));
#252445=CARTESIAN_POINT('Ctrl Pts',(-2.367993675611,2.19369239913319,14.6607656120188));
#252446=CARTESIAN_POINT('Ctrl Pts',(-2.18409061269887,2.37088056252323,
14.643866678352));
#252447=CARTESIAN_POINT('Ctrl Pts',(-2.13044502111172,2.41920071877906,
14.6391576703012));
#252448=CARTESIAN_POINT('Ctrl Pts',(-2.06064918224078,2.47794372575322,
14.6333487588759));
#252449=CARTESIAN_POINT('Ctrl Pts',(-2.04597160903183,2.49007637950605,
14.6321442058995));
#252450=CARTESIAN_POINT('Ctrl Pts',(-2.02253469429064,2.50910246298826,
14.630248750036));
#252451=CARTESIAN_POINT('Ctrl Pts',(-2.0138459042662,2.51608156504868,14.6295520420253));
#252452=CARTESIAN_POINT('Ctrl Pts',(-1.99720596174648,2.52930585799812,
14.6282294484163));
#252453=CARTESIAN_POINT('Ctrl Pts',(-1.98926145708896,2.53555884064357,
14.6276030465009));
#252454=CARTESIAN_POINT('Ctrl Pts',(-1.97018230734015,2.5504308456802,14.6261104713961));
#252455=CARTESIAN_POINT('Ctrl Pts',(-1.95902021333611,2.55901458442358,
14.6252467345037));
#252456=CARTESIAN_POINT('Ctrl Pts',(-1.9203538141917,2.588348081423,14.6222858165679));
#252457=CARTESIAN_POINT('Ctrl Pts',(-1.89257225145693,2.60873054360133,
14.6202122222528));
#252458=CARTESIAN_POINT('Ctrl Pts',(-1.82290423879382,2.65814490504265,
14.6151295758977));
#252459=CARTESIAN_POINT('Ctrl Pts',(-1.78064504940145,2.68663691807925,
14.6121488348821));
#252460=CARTESIAN_POINT('Ctrl Pts',(-1.58805790567409,2.80994176387,14.5989330656304));
#252461=CARTESIAN_POINT('Ctrl Pts',(-1.43071132507348,2.89322890819596,
14.5891039821416));
#252462=CARTESIAN_POINT('Ctrl Pts',(-1.09530611526263,3.03667774786743,
14.5686300186313));
#252463=CARTESIAN_POINT('Ctrl Pts',(-0.917264354072286,3.09511248946058,
14.5580002777238));
#252464=CARTESIAN_POINT('Ctrl Pts',(-0.701155773222532,3.14574614331847,
14.5447634677183));
#252465=CARTESIAN_POINT('Ctrl Pts',(-0.667012803188848,3.15316222147736,
14.5426635583024));
#252466=CARTESIAN_POINT('Ctrl Pts',(-0.612773564528106,3.16402298812207,
14.5393109683348));
#252467=CARTESIAN_POINT('Ctrl Pts',(-0.592753011810873,3.16783470974708,
14.5380699078766));
#252468=CARTESIAN_POINT('Ctrl Pts',(-0.555276449089201,3.17460218533928,
14.5357395226645));
#252469=CARTESIAN_POINT('Ctrl Pts',(-0.537829551089867,3.17760449464132,
14.5346517142143));
#252470=CARTESIAN_POINT('Ctrl Pts',(-0.498749808025363,3.18399837494501,
14.5322082039764));
#252471=CARTESIAN_POINT('Ctrl Pts',(-0.477105510850074,3.18731349517535,
14.5308501513789));
#252472=CARTESIAN_POINT('Ctrl Pts',(-0.412589642057926,3.19652311168084,
14.5267873741388));
#252473=CARTESIAN_POINT('Ctrl Pts',(-0.369632688953488,3.20177475811275,
14.5240627883828));
#252474=CARTESIAN_POINT('Ctrl Pts',(-0.16631840047032,3.22248468086062,
14.5110703174464));
#252475=CARTESIAN_POINT('Ctrl Pts',(-0.00507571090419254,3.22676787167101,
14.5004656305962));
#252476=CARTESIAN_POINT('Ctrl Pts',(0.321506716508821,3.21096194663564,
14.4785340216004));
#252477=CARTESIAN_POINT('Ctrl Pts',(0.486351303687658,3.19015749285242,
14.4672278495375));
#252478=CARTESIAN_POINT('Ctrl Pts',(0.743467752234609,3.13730808837392,
14.4496996323184));
#252479=CARTESIAN_POINT('Ctrl Pts',(0.837162800326893,3.11361659398127,
14.4433396759822));
#252480=CARTESIAN_POINT('Ctrl Pts',(0.94913337956593,3.07988263206984,14.4358791424483));
#252481=CARTESIAN_POINT('Ctrl Pts',(0.968551475032696,3.07383136956429,
14.434590570981));
#252482=CARTESIAN_POINT('Ctrl Pts',(0.998901842722178,3.06405711191491,
14.432586194843));
#252483=CARTESIAN_POINT('Ctrl Pts',(1.00987323976845,3.06045861362566,14.4318636208296));
#252484=CARTESIAN_POINT('Ctrl Pts',(1.02936085497042,3.05395068303854,14.4305840159081));
#252485=CARTESIAN_POINT('Ctrl Pts',(1.03788429021441,3.05106452683078,14.4300256882927));
#252486=CARTESIAN_POINT('Ctrl Pts',(1.05843028634901,3.04401129873306,14.4286829474812));
#252487=CARTESIAN_POINT('Ctrl Pts',(1.070440388535,3.03980868560207,14.4279006129375));
#252488=CARTESIAN_POINT('Ctrl Pts',(1.107580020436,3.0265652587633,14.4254883839327));
#252489=CARTESIAN_POINT('Ctrl Pts',(1.13262297856476,3.01728289355477,14.4238718584384));
#252490=CARTESIAN_POINT('Ctrl Pts',(1.36291499676283,2.92865201843427,14.4090742981013));
#252491=CARTESIAN_POINT('Ctrl Pts',(1.55967504224381,2.82877711929414,14.3969045269014));
#252492=CARTESIAN_POINT('Ctrl Pts',(1.90481381243417,2.60653985197629,14.3739101128091));
#252493=CARTESIAN_POINT('Ctrl Pts',(2.05542279027351,2.48949635406364,14.3631685976186));
#252494=CARTESIAN_POINT('Ctrl Pts',(2.22799367889522,2.32899438751498,14.3492186054157));
#252495=CARTESIAN_POINT('Ctrl Pts',(2.26051711321325,2.29744048220432,14.3465099699215));
#252496=CARTESIAN_POINT('Ctrl Pts',(2.30803227647258,2.24935580183815,14.3424248804728));
#252497=CARTESIAN_POINT('Ctrl Pts',(2.32353592335006,2.23333725333107,14.3410707891188));
#252498=CARTESIAN_POINT('Ctrl Pts',(2.35107266358738,2.20428886605547,14.3386265346934));
#252499=CARTESIAN_POINT('Ctrl Pts',(2.3631668379991,2.19131799393622,14.3375390506334));
#252500=CARTESIAN_POINT('Ctrl Pts',(2.38874186333595,2.16343108777896,14.3352089544445));
#252501=CARTESIAN_POINT('Ctrl Pts',(2.40219137197464,2.14848745505957,14.33396509077));
#252502=CARTESIAN_POINT('Ctrl Pts',(2.43839574760883,2.10749613639129,14.3305653340168));
#252503=CARTESIAN_POINT('Ctrl Pts',(2.46087201404647,2.08120699807592,14.328398133837));
#252504=CARTESIAN_POINT('Ctrl Pts',(2.5985491691138,1.91482536472876,14.3147586780835));
#252505=CARTESIAN_POINT('Ctrl Pts',(2.70215743046299,1.76559924611675,14.3028307606079));
#252506=CARTESIAN_POINT('Ctrl Pts',(2.88035914128407,1.45620309563204,14.2788572825919));
#252507=CARTESIAN_POINT('Ctrl Pts',(2.95546096074407,1.29701466453965,14.2668704679057));
#252508=CARTESIAN_POINT('Ctrl Pts',(3.04629389790864,1.05501665610646,14.2496915789419));
#252509=CARTESIAN_POINT('Ctrl Pts',(3.07238339562138,0.9764370435369,14.2442694857146));
#252510=CARTESIAN_POINT('Ctrl Pts',(3.10092882768087,0.877923517333849,
14.2377323375367));
#252511=CARTESIAN_POINT('Ctrl Pts',(3.10626219682884,0.85886233262069,14.2364793897809));
#252512=CARTESIAN_POINT('Ctrl Pts',(3.11436632712284,0.828835216562373,
14.2345255904426));
#252513=CARTESIAN_POINT('Ctrl Pts',(3.11725545327477,0.817902123637985,
14.2338183360548));
#252514=CARTESIAN_POINT('Ctrl Pts',(3.12260542073369,0.797216474897416,
14.2324883001637));
#252515=CARTESIAN_POINT('Ctrl Pts',(3.12507815491088,0.787467618004659,
14.2318648979844));
#252516=CARTESIAN_POINT('Ctrl Pts',(3.13081966461822,0.764378456350037,
14.2303962854714));
#252517=CARTESIAN_POINT('Ctrl Pts',(3.1340488571539,0.7510286103166,14.2295533106254));
#252518=CARTESIAN_POINT('Ctrl Pts',(3.14459650288914,0.706170443545754,
14.2267401257486));
#252519=CARTESIAN_POINT('Ctrl Pts',(3.15152617013043,0.674571596866852,
14.224790456632));
#252520=CARTESIAN_POINT('Ctrl Pts',(3.16731102124927,0.597031749129717,
14.2200723398118));
#252521=CARTESIAN_POINT('Ctrl Pts',(3.17564407235114,0.550991069651247,
14.217327216804));
#252522=CARTESIAN_POINT('Ctrl Pts',(3.20650750855755,0.356377890194215,
14.2058993117215));
#252523=CARTESIAN_POINT('Ctrl Pts',(3.21963660859419,0.206498451853521,
14.1975202337013));
#252524=CARTESIAN_POINT('Ctrl Pts',(3.22584158959593,-0.149003278958,14.1776168000608));
#252525=CARTESIAN_POINT('Ctrl Pts',(3.20980662768336,-0.354098121355896,
14.1660861844325));
#252526=CARTESIAN_POINT('Ctrl Pts',(3.16658984502299,-0.600718857115544,
14.1512638561868));
#252527=CARTESIAN_POINT('Ctrl Pts',(3.15786730819869,-0.645002447521561,
14.1485657463951));
#252528=CARTESIAN_POINT('Ctrl Pts',(3.14345893058849,-0.710829742323324,
14.1444934406876));
#252529=CARTESIAN_POINT('Ctrl Pts',(3.13847475741943,-0.732522443202241,
14.1431413965845));
#252530=CARTESIAN_POINT('Ctrl Pts',(3.12911702190624,-0.771400433149129,
14.1406993650608));
#252531=CARTESIAN_POINT('Ctrl Pts',(3.12482553080471,-0.788604683836959,
14.13961203598));
#252532=CARTESIAN_POINT('Ctrl Pts',(3.11535998098308,-0.825260481470628,
14.1372806621072));
#252533=CARTESIAN_POINT('Ctrl Pts',(3.1101452465862,-0.844700650728657,
14.1360353510475));
#252534=CARTESIAN_POINT('Ctrl Pts',(3.09544705619467,-0.897512477042214,
14.1326274617118));
#252535=CARTESIAN_POINT('Ctrl Pts',(3.08560649843472,-0.930781129536284,
14.1304534847241));
#252536=CARTESIAN_POINT('Ctrl Pts',(3.01990378884756,-1.1404029652338,14.116577911595));
#252537=CARTESIAN_POINT('Ctrl Pts',(2.94949004587681,-1.31180286543515,
14.1044010676474));
#252538=CARTESIAN_POINT('Ctrl Pts',(2.78137757448909,-1.63805047283622,
14.0797418660787));
#252539=CARTESIAN_POINT('Ctrl Pts',(2.68440889589213,-1.79254587073826,
14.0673149180768));
#252540=CARTESIAN_POINT('Ctrl Pts',(2.53056148215358,-1.99695148677586,
14.0503739117438));
#252541=CARTESIAN_POINT('Ctrl Pts',(2.48419784821713,-2.05434161307253,
14.0455589032327));
#252542=CARTESIAN_POINT('Ctrl Pts',(2.42335188153119,-2.12458246095315,
14.0396405341435));
#252543=CARTESIAN_POINT('Ctrl Pts',(2.41067227151651,-2.13895867554608,
14.0384278555955));
#252544=CARTESIAN_POINT('Ctrl Pts',(2.39040046484082,-2.16153371305155,
14.0365225955276));
#252545=CARTESIAN_POINT('Ctrl Pts',(2.38289282614953,-2.16980740224573,
14.0358241101477));
#252546=CARTESIAN_POINT('Ctrl Pts',(2.36851605719503,-2.18548650546368,
14.0345003222121));
#252547=CARTESIAN_POINT('Ctrl Pts',(2.36165499594903,-2.19289882597374,
14.033874483219));
#252548=CARTESIAN_POINT('Ctrl Pts',(2.34518806509989,-2.21052188998329,
14.0323862155953));
#252549=CARTESIAN_POINT('Ctrl Pts',(2.33555008843706,-2.22070256625548,
14.0315261848932));
#252550=CARTESIAN_POINT('Ctrl Pts',(2.30226245470397,-2.25540814277195,
14.0285920720486));
#252551=CARTESIAN_POINT('Ctrl Pts',(2.2782896485405,-2.27962163206156,14.0265410075842));
#252552=CARTESIAN_POINT('Ctrl Pts',(2.21806552820342,-2.33855117074672,
14.0215252406461));
#252553=CARTESIAN_POINT('Ctrl Pts',(2.18137791784707,-2.3728099685099,14.0185878940764));
#252554=CARTESIAN_POINT('Ctrl Pts',(2.01528212106606,-2.52079991441807,
14.0057233377888));
#252555=CARTESIAN_POINT('Ctrl Pts',(1.87767146566831,-2.62490981129512,
13.9961809964709));
#252556=CARTESIAN_POINT('Ctrl Pts',(1.56873640097201,-2.8218523300357,13.9756346998822));
#252557=CARTESIAN_POINT('Ctrl Pts',(1.39601377651298,-2.91117109621544,
13.964628246277));
#252558=CARTESIAN_POINT('Ctrl Pts',(1.18409918400143,-2.99753851965681,
13.950979627456));
#252559=CARTESIAN_POINT('Ctrl Pts',(1.15167061114463,-3.01014662725304,
13.9488882853055));
#252560=CARTESIAN_POINT('Ctrl Pts',(1.09996379568074,-3.02929219925,13.9455463167466));
#252561=CARTESIAN_POINT('Ctrl Pts',(1.08081627325872,-3.03617649921441,
13.9443071840704));
#252562=CARTESIAN_POINT('Ctrl Pts',(1.0448870835615,-3.04871154086945,13.9419785158581));
#252563=CARTESIAN_POINT('Ctrl Pts',(1.02812147535925,-3.05440620891101,
13.9408904758525));
#252564=CARTESIAN_POINT('Ctrl Pts',(0.990477446063168,-3.06684746828097,
13.9384439401889));
#252565=CARTESIAN_POINT('Ctrl Pts',(0.969575495562537,-3.07351952741286,
13.9370830673289));
#252566=CARTESIAN_POINT('Ctrl Pts',(0.907034853582364,-3.09278152484734,
13.9330032110686));
#252567=CARTESIAN_POINT('Ctrl Pts',(0.865209000106622,-3.10474199859709,
13.9302641161829));
#252568=CARTESIAN_POINT('Ctrl Pts',(0.665662568000436,-3.15745879727107,
13.9171407610229));
#252569=CARTESIAN_POINT('Ctrl Pts',(0.505263576687523,-3.18705951855238,
13.9064117530493));
#252570=CARTESIAN_POINT('Ctrl Pts',(0.174391316319274,-3.2225106101127,
13.8840818863798));
#252571=CARTESIAN_POINT('Ctrl Pts',(0.00428405712409704,-3.22722298857725,
13.8724981151371));
#252572=CARTESIAN_POINT('Ctrl Pts',(-0.256217350877482,-3.213835660241,
13.8551114467391));
#252573=CARTESIAN_POINT('Ctrl Pts',(-0.34680433199176,-3.20532631008748,
13.8491355133135));
#252574=CARTESIAN_POINT('Ctrl Pts',(-0.456787553832832,-3.19027661865676,
13.8420559743072));
#252575=CARTESIAN_POINT('Ctrl Pts',(-0.476632347246486,-3.18737218179777,
13.8407856711441));
#252576=CARTESIAN_POINT('Ctrl Pts',(-0.507794408818161,-3.18251382414491,
13.8388034488152));
#252577=CARTESIAN_POINT('Ctrl Pts',(-0.519130187009412,-3.1806844013405,
13.8380849923677));
#252578=CARTESIAN_POINT('Ctrl Pts',(-0.539343246600434,-3.17731137988055,
13.8368088596243));
#252579=CARTESIAN_POINT('Ctrl Pts',(-0.548223884968563,-3.17579113240856,
13.8362499293904));
#252580=CARTESIAN_POINT('Ctrl Pts',(-0.569724312181716,-3.17201766949623,
13.8349008221916));
#252581=CARTESIAN_POINT('Ctrl Pts',(-0.582337175821552,-3.16972637841278,
13.8341127803183));
#252582=CARTESIAN_POINT('Ctrl Pts',(-0.621676285563726,-3.16233717583866,
13.831664553716));
#252583=CARTESIAN_POINT('Ctrl Pts',(-0.648352611273866,-3.15697589773968,
13.8300183177228));
#252584=CARTESIAN_POINT('Ctrl Pts',(-0.785956442394575,-3.12750311188815,
13.8215839228754));
#252585=CARTESIAN_POINT('Ctrl Pts',(-0.895631769467868,-3.09787862839589,
13.8150535391911));
#252586=CARTESIAN_POINT('Ctrl Pts',(-1.18873223666557,-3.00183582955961,
13.7975827537467));
#252587=CARTESIAN_POINT('Ctrl Pts',(-1.36805206936515,-2.92447226222963,
13.7868515234532));
#252588=CARTESIAN_POINT('Ctrl Pts',(-1.64703229867231,-2.77280413373081,
13.7687620686333));
#252589=CARTESIAN_POINT('Ctrl Pts',(-1.75133735728306,-2.70813052545463,
13.7616498210041));
#252590=CARTESIAN_POINT('Ctrl Pts',(-1.8784938655598,-2.61886431594096,
13.7523642688644));
#252591=CARTESIAN_POINT('Ctrl Pts',(-1.90500156491888,-2.59964582746207,
13.7503929506691));
#252592=CARTESIAN_POINT('Ctrl Pts',(-1.94698862946235,-2.5682175218419,
13.7472103146443));
#252593=CARTESIAN_POINT('Ctrl Pts',(-1.96265716147386,-2.5562634454516,
13.7460088792095));
#252594=CARTESIAN_POINT('Ctrl Pts',(-1.99159649625403,-2.5337616878497,
13.7437635842171));
#252595=CARTESIAN_POINT('Ctrl Pts',(-2.00489568420024,-2.52325150805083,
13.7427212246087));
#252596=CARTESIAN_POINT('Ctrl Pts',(-2.01869561671053,-2.51216761613525,
13.741628404508));
#252597=CARTESIAN_POINT('Ctrl Pts',(-2.01927992691387,-2.51169797174067,
13.7415821117042));
#252598=CARTESIAN_POINT('Ctrl Pts',(-2.02042215540262,-2.51077923948155,
13.7414915756762));
#252599=CARTESIAN_POINT('Ctrl Pts',(-2.02098008798839,-2.51033016940132,
13.7414473331644));
#252600=CARTESIAN_POINT('Ctrl Pts',(-2.0220736471648,-2.50944938207923,
13.7413605790553));
#252601=CARTESIAN_POINT('Ctrl Pts',(-2.0226092853375,-2.5090176792206,13.7413180680343));
#252602=CARTESIAN_POINT('Ctrl Pts',(-2.02366175885197,-2.50816887177791,
13.7412345032012));
#252603=CARTESIAN_POINT('Ctrl Pts',(-2.02417860359046,-2.50775177885711,
13.7411934498571));
#252604=CARTESIAN_POINT('Ctrl Pts',(-2.02519653059653,-2.50692979358846,
13.7411125623886));
#252605=CARTESIAN_POINT('Ctrl Pts',(-2.02569762048562,-2.50652491068404,
13.7410727286432));
#252606=CARTESIAN_POINT('Ctrl Pts',(-2.02668670875336,-2.50572523255615,
13.7409940708887));
#252607=CARTESIAN_POINT('Ctrl Pts',(-2.02717471327031,-2.50533044494786,
13.7409552471857));
#252608=CARTESIAN_POINT('Ctrl Pts',(-2.0446127367826,-2.49121494060882,
13.7395674145988));
#252609=CARTESIAN_POINT('Ctrl Pts',(-2.06142282798318,-2.47732295245378,
13.7382115599284));
#252610=CARTESIAN_POINT('Ctrl Pts',(-2.09802724692377,-2.44644223501679,
13.7352187753613));
#252611=CARTESIAN_POINT('Ctrl Pts',(-2.11775876191193,-2.42938175280243,
13.7335789896997));
#252612=CARTESIAN_POINT('Ctrl Pts',(-2.17065512987335,-2.38251175250846,
13.7291096661124));
#252613=CARTESIAN_POINT('Ctrl Pts',(-2.20341096700817,-2.35225120797216,
13.7262619901629));
#252614=CARTESIAN_POINT('Ctrl Pts',(-2.30665749346402,-2.25282061419605,
13.717022720101));
#252615=CARTESIAN_POINT('Ctrl Pts',(-2.37459594228146,-2.18109164809226,
13.7105312047655));
#252616=CARTESIAN_POINT('Ctrl Pts',(-2.5753784215234,-1.94858912772462,
13.6900612606086));
#252617=CARTESIAN_POINT('Ctrl Pts',(-2.6959904761406,-1.77797747682808,
13.6757932781427));
#252618=CARTESIAN_POINT('Ctrl Pts',(-2.84133960572528,-1.52319124252239,
13.6562827180402));
#252619=CARTESIAN_POINT('Ctrl Pts',(-2.88047395406218,-1.44782410792709,
13.6507170529368));
#252620=CARTESIAN_POINT('Ctrl Pts',(-2.92497995215966,-1.35314405807114,
13.644047728717));
#252621=CARTESIAN_POINT('Ctrl Pts',(-2.9332065790361,-1.3352174998084,13.6427988657966));
#252622=CARTESIAN_POINT('Ctrl Pts',(-2.94593054544261,-1.30680560802012,
13.6408426699356));
#252623=CARTESIAN_POINT('Ctrl Pts',(-2.95053752818565,-1.29637030967679,
13.6401290678809));
#252624=CARTESIAN_POINT('Ctrl Pts',(-2.9590920851437,-1.27671149496586,
13.6387941865063));
#252625=CARTESIAN_POINT('Ctrl Pts',(-2.963051998443,-1.26749401054196,13.6381722168549));
#252626=CARTESIAN_POINT('Ctrl Pts',(-2.97225834141134,-1.24578547568564,
13.6367163628319));
#252627=CARTESIAN_POINT('Ctrl Pts',(-2.97746913274882,-1.23327964310522,
13.6358845984754));
#252628=CARTESIAN_POINT('Ctrl Pts',(-2.99443773575078,-1.19182075076126,
13.6331488140221));
#252629=CARTESIAN_POINT('Ctrl Pts',(-3.00585369432996,-1.16272859511286,
13.6312638267463));
#252630=CARTESIAN_POINT('Ctrl Pts',(-3.03255259729587,-1.0916670003113,
13.6267327926392));
#252631=CARTESIAN_POINT('Ctrl Pts',(-3.04739005716418,-1.04953623337256,
13.6241077184834));
#252632=CARTESIAN_POINT('Ctrl Pts',(-3.10446385881446,-0.876046783213798,
13.613495341954));
#252633=CARTESIAN_POINT('Ctrl Pts',(-3.13912199289558,-0.742342228008782,
13.6057694407136));
#252634=CARTESIAN_POINT('Ctrl Pts',(-3.20336795107731,-0.407242692695266,
13.5866687710079));
#252635=CARTESIAN_POINT('Ctrl Pts',(-3.22266494010861,-0.204519623547666,
13.5753149239524));
#252636=CARTESIAN_POINT('Ctrl Pts',(-3.22274971943303,-0.00134476552198701,
13.5633807678595));
#252637=CARTESIAN_POINT('Ctrl Pts',(-3.2227497208408,-0.00134138754393476,
13.5633805694426));
#252638=CARTESIAN_POINT('Ctrl Pts',(-3.22274990694714,-0.000894257881103293,
13.563354305771));
#252639=CARTESIAN_POINT('Ctrl Pts',(-3.22275,-0.000447128689908073,13.5633280396337));
#252640=CARTESIAN_POINT('Ctrl Pts',(-3.22275,7.83873563209288E-13,13.5633017710267));
#252641=CARTESIAN_POINT('Ctrl Pts',(-3.22275,-2.24100014615096E-11,13.3128542084224));
#252642=CARTESIAN_POINT('Ctrl Pts',(-3.22274999999937,-0.0899329648665014,
13.3179622255554));
#252643=CARTESIAN_POINT('Ctrl Pts',(-3.21898558460739,-0.179823228001732,
13.3231316752801));
#252644=CARTESIAN_POINT('Ctrl Pts',(-3.207149078492,-0.320905013689379,
13.3314326182287));
#252645=CARTESIAN_POINT('Ctrl Pts',(-3.20159446116282,-0.372260286167885,
13.3344933286003));
#252646=CARTESIAN_POINT('Ctrl Pts',(-3.19194700081472,-0.445046231040555,
13.3388977292782));
#252647=CARTESIAN_POINT('Ctrl Pts',(-3.18886687955547,-0.466604536510036,
13.3402105684859));
#252648=CARTESIAN_POINT('Ctrl Pts',(-3.18293878851294,-0.505291682551132,
13.3425822717539));
#252649=CARTESIAN_POINT('Ctrl Pts',(-3.18017040715958,-0.522431985199073,
13.3436386364612));
#252650=CARTESIAN_POINT('Ctrl Pts',(-3.17423421164326,-0.557388707507025,
13.3458048548984));
#252651=CARTESIAN_POINT('Ctrl Pts',(-3.17105457333871,-0.575202463141507,
13.3469150437404));
#252652=CARTESIAN_POINT('Ctrl Pts',(-3.16386704210488,-0.613598037790565,
13.3493219526887));
#252653=CARTESIAN_POINT('Ctrl Pts',(-3.15980797773742,-0.634169317271281,
13.3506202430632));
#252654=CARTESIAN_POINT('Ctrl Pts',(-3.14817046930335,-0.69026030657834,
13.3541848074946));
#252655=CARTESIAN_POINT('Ctrl Pts',(-3.14019204928681,-0.725692990679699,
13.3564636014382));
#252656=CARTESIAN_POINT('Ctrl Pts',(-3.09966039951675,-0.892490060864858,
13.3673230058039));
#252657=CARTESIAN_POINT('Ctrl Pts',(-3.05945612483903,-1.0218382299263,
13.3761423260181));
#252658=CARTESIAN_POINT('Ctrl Pts',(-2.91586407907642,-1.3983989610192,
13.4029436732885));
#252659=CARTESIAN_POINT('Ctrl Pts',(-2.78969372900423,-1.63566064835666,
13.4214266917264));
#252660=CARTESIAN_POINT('Ctrl Pts',(-2.61161325015087,-1.88873973878736,
13.4415466202323));
#252661=CARTESIAN_POINT('Ctrl Pts',(-2.58691808649203,-1.92242470805476,
13.4442312792123));
#252662=CARTESIAN_POINT('Ctrl Pts',(-2.55224868566321,-1.96783646783211,
13.4478494861375));
#252663=CARTESIAN_POINT('Ctrl Pts',(-2.54283604782479,-1.97998448815521,
13.4488172750452));
#252664=CARTESIAN_POINT('Ctrl Pts',(-2.52684023747063,-2.0003265818774,
13.4504370113076));
#252665=CARTESIAN_POINT('Ctrl Pts',(-2.52030328791533,-2.00855653846788,
13.4510920812447));
#252666=CARTESIAN_POINT('Ctrl Pts',(-2.50680790624113,-2.02537747043851,
13.4524302246069));
#252667=CARTESIAN_POINT('Ctrl Pts',(-2.49984536031816,-2.03396483734155,
13.4531130006493));
#252668=CARTESIAN_POINT('Ctrl Pts',(-2.48147363890198,-2.05638705049397,
13.4548953143164));
#252669=CARTESIAN_POINT('Ctrl Pts',(-2.46999276728986,-2.07016300928138,
13.4559898824912));
#252670=CARTESIAN_POINT('Ctrl Pts',(-2.42068553041011,-2.1283328361924,
13.4606132857697));
#252671=CARTESIAN_POINT('Ctrl Pts',(-2.38177050360163,-2.17179402347281,
13.4640714943244));
#252672=CARTESIAN_POINT('Ctrl Pts',(-2.16496811612824,-2.40108230138489,
13.4824895727432));
#252673=CARTESIAN_POINT('Ctrl Pts',(-1.96648888556209,-2.56616990062601,
13.4964584098184));
#252674=CARTESIAN_POINT('Ctrl Pts',(-1.67729244903322,-2.75325349678787,
13.5160359146764));
#252675=CARTESIAN_POINT('Ctrl Pts',(-1.60222253511323,-2.79760544157164,
13.5210490350353));
#252676=CARTESIAN_POINT('Ctrl Pts',(-1.47230273643974,-2.86741740154549,
13.529696183272));
#252677=CARTESIAN_POINT('Ctrl Pts',(-1.41836580872615,-2.89447674918599,
13.5332777847565));
#252678=CARTESIAN_POINT('Ctrl Pts',(-1.34083741890371,-2.93068413197448,
13.538431072146));
#252679=CARTESIAN_POINT('Ctrl Pts',(-1.3178471029279,-2.94109391615876,
13.5399598069635));
#252680=CARTESIAN_POINT('Ctrl Pts',(-1.27782517742385,-2.9586519652023,
13.5426231746355));
#252681=CARTESIAN_POINT('Ctrl Pts',(-1.26084978676305,-2.96592589730945,
13.5437534978821));
#252682=CARTESIAN_POINT('Ctrl Pts',(-1.22803297368019,-2.97965521055178,
13.5459402937505));
#252683=CARTESIAN_POINT('Ctrl Pts',(-1.21220079795623,-2.98613117022875,
13.5469960281558));
#252684=CARTESIAN_POINT('Ctrl Pts',(-1.17024692691346,-3.00290326624806,
13.5497959360242));
#252685=CARTESIAN_POINT('Ctrl Pts',(-1.14404138918197,-3.01298442027949,
13.5515471890428));
#252686=CARTESIAN_POINT('Ctrl Pts',(-1.04802570399631,-3.04848802390875,
13.5579739099326));
#252687=CARTESIAN_POINT('Ctrl Pts',(-0.977478103508532,-3.07183532091763,
13.5627161836479));
#252688=CARTESIAN_POINT('Ctrl Pts',(-0.683552096844328,-3.15795786010056,
13.5825642108918));
#252689=CARTESIAN_POINT('Ctrl Pts',(-0.454542326915349,-3.19895389068393,
13.5983048224551));
#252690=CARTESIAN_POINT('Ctrl Pts',(-0.0925098144984718,-3.22408287626044,
13.622770100066));
#252691=CARTESIAN_POINT('Ctrl Pts',(0.0385812291964583,-3.22518003382034,
13.6315272571589));
#252692=CARTESIAN_POINT('Ctrl Pts',(0.198682864991038,-3.21675354740473,
13.6418479676219));
#252693=CARTESIAN_POINT('Ctrl Pts',(0.227958834799953,-3.21481153008997,
13.6437195828405));
#252694=CARTESIAN_POINT('Ctrl Pts',(0.270546634060667,-3.21140175190029,
13.646415590169));
#252695=CARTESIAN_POINT('Ctrl Pts',(0.283881409146017,-3.2102504658608,
13.6472559326816));
#252696=CARTESIAN_POINT('Ctrl Pts',(0.307371579817887,-3.20807488074887,
13.6487290795585));
#252697=CARTESIAN_POINT('Ctrl Pts',(0.317529785492987,-3.20708537052336,
13.6493637428067));
#252698=CARTESIAN_POINT('Ctrl Pts',(0.339599080367137,-3.20482971312209,
13.6507373080323));
#252699=CARTESIAN_POINT('Ctrl Pts',(0.351507947050802,-3.20354541083504,
13.6514752098383));
#252700=CARTESIAN_POINT('Ctrl Pts',(0.384844669861352,-3.19976210405955,
13.6535322986173));
#252701=CARTESIAN_POINT('Ctrl Pts',(0.406255429687084,-3.19711424957678,
13.6548435908077));
#252702=CARTESIAN_POINT('Ctrl Pts',(0.550314258521002,-3.17782800367955,
13.6636093933054));
#252703=CARTESIAN_POINT('Ctrl Pts',(0.671955985320854,-3.15434913428427,
13.6707340651659));
#252704=CARTESIAN_POINT('Ctrl Pts',(0.837618305168215,-3.11235153628912,
13.6804120381007));
#252705=CARTESIAN_POINT('Ctrl Pts',(0.883020986371203,-3.09977589227275,
13.6830615435408));
#252706=CARTESIAN_POINT('Ctrl Pts',(1.05815036124308,-3.04710829521904,
13.6933209861705));
#252707=CARTESIAN_POINT('Ctrl Pts',(1.18556651522669,-2.99983036803342,
13.700876747816));
#252708=CARTESIAN_POINT('Ctrl Pts',(1.39009306170021,-2.90886851641838,
13.7135944144543));
#252709=CARTESIAN_POINT('Ctrl Pts',(1.46906238839584,-2.86979596995303,
13.7186577812724));
#252710=CARTESIAN_POINT('Ctrl Pts',(1.59966322387328,-2.79837281829352,
13.7273827325615));
#252711=CARTESIAN_POINT('Ctrl Pts',(1.65215886781773,-2.76770360358913,
13.7309905676729));
#252712=CARTESIAN_POINT('Ctrl Pts',(1.72523667329897,-2.72218965789974,
13.7361750863304));
#252713=CARTESIAN_POINT('Ctrl Pts',(1.74656096607412,-2.7085573371852,13.7377080869675));
#252714=CARTESIAN_POINT('Ctrl Pts',(1.78317427761115,-2.68453880281972,
13.7403764617772));
#252715=CARTESIAN_POINT('Ctrl Pts',(1.79853878587422,-2.67426948935603,
13.7415074804176));
#252716=CARTESIAN_POINT('Ctrl Pts',(1.8298530804593,-2.65294775503036,13.7438362397307));
#252717=CARTESIAN_POINT('Ctrl Pts',(1.84579303896979,-2.64188230590005,
13.7450344392933));
#252718=CARTESIAN_POINT('Ctrl Pts',(1.88612091926002,-2.61334373670873,
13.7480991436312));
#252719=CARTESIAN_POINT('Ctrl Pts',(1.91036614016374,-2.59567307686122,
13.7499731058671));
#252720=CARTESIAN_POINT('Ctrl Pts',(2.00590438297721,-2.52397824398705,
13.7574860699488));
#252721=CARTESIAN_POINT('Ctrl Pts',(2.07517594631369,-2.4673388316857,13.7632251699227));
#252722=CARTESIAN_POINT('Ctrl Pts',(2.30509618093428,-2.26280817786928,
13.7833120122935));
#252723=CARTESIAN_POINT('Ctrl Pts',(2.45301800569522,-2.101535750111,13.7981452494028));
#252724=CARTESIAN_POINT('Ctrl Pts',(2.65887379114078,-1.82548895909439,
13.8213430445429));
#252725=CARTESIAN_POINT('Ctrl Pts',(2.72826843502348,-1.72005144740038,
13.8297622198412));
#252726=CARTESIAN_POINT('Ctrl Pts',(2.80572110424314,-1.58583667587258,
13.8397330250678));
#252727=CARTESIAN_POINT('Ctrl Pts',(2.8197971124363,-1.56067077057854,13.8415717543002));
#252728=CARTESIAN_POINT('Ctrl Pts',(2.83986608147024,-1.52363212915626,
13.8442295400417));
#252729=CARTESIAN_POINT('Ctrl Pts',(2.84612591274203,-1.51190658736587,
13.8450639399335));
#252730=CARTESIAN_POINT('Ctrl Pts',(2.85706016199703,-1.49111662597587,
13.8465306094882));
#252731=CARTESIAN_POINT('Ctrl Pts',(2.86176432373188,-1.48206832722486,
13.84716467904));
#252732=CARTESIAN_POINT('Ctrl Pts',(2.87192957501705,-1.46228693732336,
13.8485415475877));
#252733=CARTESIAN_POINT('Ctrl Pts',(2.87737352218324,-1.45154545073523,
13.8492833022315));
#252734=CARTESIAN_POINT('Ctrl Pts',(2.89253085031161,-1.42121806255129,
13.8513617087933));
#252735=CARTESIAN_POINT('Ctrl Pts',(2.90210552945349,-1.40156307597027,
13.8526902040262));
#252736=CARTESIAN_POINT('Ctrl Pts',(2.97092565188509,-1.25655894125373,
13.8623669302209));
#252737=CARTESIAN_POINT('Ctrl Pts',(3.02223423380832,-1.12758537439685,
13.8702998978876));
#252738=CARTESIAN_POINT('Ctrl Pts',(3.07526219935315,-0.964347587803793,
13.8799812130817));
#252739=CARTESIAN_POINT('Ctrl Pts',(3.08496379565228,-0.932846334111955,
13.8818332620063));
#252740=CARTESIAN_POINT('Ctrl Pts',(3.13400589721659,-0.764465446248853,
13.8916705845994));
#252741=CARTESIAN_POINT('Ctrl Pts',(3.16472314045262,-0.6252412025472,13.8995948245035));
#252742=CARTESIAN_POINT('Ctrl Pts',(3.1986777825188,-0.401926502558706,
13.9124568517353));
#252743=CARTESIAN_POINT('Ctrl Pts',(3.20801350066146,-0.318955293056436,
13.9172663476996));
#252744=CARTESIAN_POINT('Ctrl Pts',(3.2183949468099,-0.177400366619265,
13.9255970795024));
#252745=CARTESIAN_POINT('Ctrl Pts',(3.22108371457834,-0.1189789984745,13.929071065933));
#252746=CARTESIAN_POINT('Ctrl Pts',(3.22264998953787,-0.0355871182076339,
13.9340960470871));
#252747=CARTESIAN_POINT('Ctrl Pts',(3.22282886677761,-0.0106508416402976,
13.935607026977));
#252748=CARTESIAN_POINT('Ctrl Pts',(3.22263670586035,0.0327025410947999,
13.9382496266437));
#252749=CARTESIAN_POINT('Ctrl Pts',(3.22239718123915,0.0511192578369016,
13.9393771269992));
#252750=CARTESIAN_POINT('Ctrl Pts',(3.22162914835204,0.0867083373539033,
13.941565845018));
#252751=CARTESIAN_POINT('Ctrl Pts',(3.22112115861991,0.103880550126878,
13.9426263876769));
#252752=CARTESIAN_POINT('Ctrl Pts',(3.21940612627436,0.149509041303053,
13.9454565912277));
#252753=CARTESIAN_POINT('Ctrl Pts',(3.21795912865062,0.177954271636137,
13.9472336219981));
#252754=CARTESIAN_POINT('Ctrl Pts',(3.21119705662962,0.283333538447894,
13.9538655899249));
#252755=CARTESIAN_POINT('Ctrl Pts',(3.20349851419942,0.360083475353739,
13.9587930123759));
#252756=CARTESIAN_POINT('Ctrl Pts',(3.16199329879808,0.663714501517062,
13.9786806533261));
#252757=CARTESIAN_POINT('Ctrl Pts',(3.10676522488322,0.886962963958601,
13.9942465054189));
#252758=CARTESIAN_POINT('Ctrl Pts',(2.98384772930271,1.22461386753326,14.0184675935417));
#252759=CARTESIAN_POINT('Ctrl Pts',(2.93200739577582,1.34401088003475,14.0271601626155));
#252760=CARTESIAN_POINT('Ctrl Pts',(2.85984178951104,1.48602746287767,14.0374141278109));
#252761=CARTESIAN_POINT('Ctrl Pts',(2.84623974995362,1.51191669901134,14.0392795369095));
#252762=CARTESIAN_POINT('Ctrl Pts',(2.82590928195695,1.54936534059637,14.0419683372359));
#252763=CARTESIAN_POINT('Ctrl Pts',(2.81945874085534,1.56107291686202,14.0428075635071));
#252764=CARTESIAN_POINT('Ctrl Pts',(2.80800024522166,1.58156708809748,14.0442737591968));
#252765=CARTESIAN_POINT('Ctrl Pts',(2.80302353192458,1.5903706865092,14.0449026254392));
#252766=CARTESIAN_POINT('Ctrl Pts',(2.79207529488783,1.60952661556224,14.0462688078414));
#252767=CARTESIAN_POINT('Ctrl Pts',(2.78608756514042,1.61986927511282,14.047005090751));
#252768=CARTESIAN_POINT('Ctrl Pts',(2.76919139481088,1.64868333841733,14.049053244291));
#252769=CARTESIAN_POINT('Ctrl Pts',(2.75815564052515,1.66707985702906,14.0503573287521));
#252770=CARTESIAN_POINT('Ctrl Pts',(2.68464832256004,1.78688767624556,14.0588359363063));
#252771=CARTESIAN_POINT('Ctrl Pts',(2.61677267848089,1.88489018473704,14.0657053634493));
#252772=CARTESIAN_POINT('Ctrl Pts',(2.51238157905057,2.01907016569537,14.0753462260572));
#252773=CARTESIAN_POINT('Ctrl Pts',(2.48019685688869,2.05847741361839,14.0782087780148));
#252774=CARTESIAN_POINT('Ctrl Pts',(2.36027401084341,2.19841413946955,14.0885489594701));
#252775=CARTESIAN_POINT('Ctrl Pts',(2.2672490782906,2.29423166422355,14.0959738408909));
#252776=CARTESIAN_POINT('Ctrl Pts',(2.10188697793125,2.444649481736,14.1086625235947));
#252777=CARTESIAN_POINT('Ctrl Pts',(2.03270759988753,2.50246640915943,14.1138385631095));
#252778=CARTESIAN_POINT('Ctrl Pts',(1.91216118428086,2.59491353919623,14.1227375873199));
#252779=CARTESIAN_POINT('Ctrl Pts',(1.86205369644798,2.63110090467948,14.126403790174));
#252780=CARTESIAN_POINT('Ctrl Pts',(1.78987219133869,2.68013502063906,14.1316577321123));
#252781=CARTESIAN_POINT('Ctrl Pts',(1.76863677019333,2.69419563299343,14.1332001374005));
#252782=CARTESIAN_POINT('Ctrl Pts',(1.73168572182384,2.71803691314577,14.1358795735217));
#252783=CARTESIAN_POINT('Ctrl Pts',(1.71604817182152,2.72793672032573,14.1370121472487));
#252784=CARTESIAN_POINT('Ctrl Pts',(1.68584079334861,2.74669786435102,14.1391977881598));
#252785=CARTESIAN_POINT('Ctrl Pts',(1.67128416721454,2.75557934984631,14.1402500698036));
#252786=CARTESIAN_POINT('Ctrl Pts',(1.63282583240599,2.77862723713339,14.1430280436932));
#252787=CARTESIAN_POINT('Ctrl Pts',(1.60881061979741,2.79260055049327,14.1447606074511));
#252788=CARTESIAN_POINT('Ctrl Pts',(1.52165677444151,2.84181392265326,14.1510422665374));
#252789=CARTESIAN_POINT('Ctrl Pts',(1.45752093068754,2.87523514329244,14.1556543050729));
#252790=CARTESIAN_POINT('Ctrl Pts',(1.1813842471838,3.00751606002114,14.175475539009));
#252791=CARTESIAN_POINT('Ctrl Pts',(0.960097848557707,3.08528864479673,
14.1913405278997));
#252792=CARTESIAN_POINT('Ctrl Pts',(0.604211141572892,3.16833867826064,
14.21597960179));
#252793=CARTESIAN_POINT('Ctrl Pts',(0.474311635944655,3.19037237932285,
14.224782556928));
#252794=CARTESIAN_POINT('Ctrl Pts',(0.314180600480588,3.20753375138397,
14.2351505608911));
#252795=CARTESIAN_POINT('Ctrl Pts',(0.284900319798646,3.21026699254901,
14.2370265546954));
#252796=CARTESIAN_POINT('Ctrl Pts',(0.242231561340866,3.21366160192668,
14.2397276450768));
#252797=CARTESIAN_POINT('Ctrl Pts',(0.22887077286196,3.21464075832496,14.2405687736708));
#252798=CARTESIAN_POINT('Ctrl Pts',(0.205319522871526,3.21621915382045,
14.2420427808878));
#252799=CARTESIAN_POINT('Ctrl Pts',(0.195131812259069,3.21685332859405,
14.2426775261903));
#252800=CARTESIAN_POINT('Ctrl Pts',(0.17299125468655,3.2181259845369,14.2440506702943));
#252801=CARTESIAN_POINT('Ctrl Pts',(0.161037728247452,3.21874629121891,
14.2447880746575));
#252802=CARTESIAN_POINT('Ctrl Pts',(0.127568428574896,3.22029620271252,
14.2468424165207));
#252803=CARTESIAN_POINT('Ctrl Pts',(0.106045955685324,3.22107678403984,
14.2481514927013));
#252804=CARTESIAN_POINT('Ctrl Pts',(-0.0377753779472141,3.22484979665145,
14.2568288524661));
#252805=CARTESIAN_POINT('Ctrl Pts',(-0.160164806522306,3.22109250585219,
14.2638750152667));
#252806=CARTESIAN_POINT('Ctrl Pts',(-0.330249195292158,3.20614933345786,
14.273547891956));
#252807=CARTESIAN_POINT('Ctrl Pts',(-0.378341771696867,3.20083047518754,
14.2762693100423));
#252808=CARTESIAN_POINT('Ctrl Pts',(-0.563233652342623,3.17615663865755,
14.2867339908872));
#252809=CARTESIAN_POINT('Ctrl Pts',(-0.698852357471505,3.14909629859429,
14.2944210292981));
#252810=CARTESIAN_POINT('Ctrl Pts',(-0.916174401936716,3.09099942372904,
14.3072094492987));
#252811=CARTESIAN_POINT('Ctrl Pts',(-0.999091358457022,3.06520275442988,
14.312203009074));
#252812=CARTESIAN_POINT('Ctrl Pts',(-1.13753594058407,3.01591587017614,
14.3208198397685));
#252813=CARTESIAN_POINT('Ctrl Pts',(-1.19363074620879,2.99415789764203,
14.3243911944309));
#252814=CARTESIAN_POINT('Ctrl Pts',(-1.27231954796944,2.9610734549913,14.3295322780443));
#252815=CARTESIAN_POINT('Ctrl Pts',(-1.29544179754858,2.95103092704319,
14.3310593400453));
#252816=CARTESIAN_POINT('Ctrl Pts',(-1.33529096372843,2.93316492903347,
14.3337207459741));
#252817=CARTESIAN_POINT('Ctrl Pts',(-1.35207305538455,2.92546695238619,
14.3348507982782));
#252818=CARTESIAN_POINT('Ctrl Pts',(-1.3842798294875,2.9103573221763,14.3370377543101));
#252819=CARTESIAN_POINT('Ctrl Pts',(-1.39971347748136,2.90296616448933,
14.3380939256902));
#252820=CARTESIAN_POINT('Ctrl Pts',(-1.44034626643518,2.88310780298086,
14.3408965981759));
#252821=CARTESIAN_POINT('Ctrl Pts',(-1.46544195240657,2.87043337760533,
14.3426502051858));
#252822=CARTESIAN_POINT('Ctrl Pts',(-1.55646496402981,2.82295796739221,
14.3490954114921));
#252823=CARTESIAN_POINT('Ctrl Pts',(-1.62134115476139,2.7862028441973,14.3538543178011));
#252824=CARTESIAN_POINT('Ctrl Pts',(-1.88244431456586,2.62606806139971,
14.3737058245852));
#252825=CARTESIAN_POINT('Ctrl Pts',(-2.06634082897956,2.48395635686017,
14.3894306313799));
#252826=CARTESIAN_POINT('Ctrl Pts',(-2.32773679544921,2.23268627170491,
14.4138738344179));
#252827=CARTESIAN_POINT('Ctrl Pts',(-2.41648738666187,2.1363149538985,14.4226251706268));
#252828=CARTESIAN_POINT('Ctrl Pts',(-2.51765532593124,2.01206098882546,
14.4329398681062));
#252829=CARTESIAN_POINT('Ctrl Pts',(-2.53586282601865,1.98906451107695,
14.4348109255038));
#252830=CARTESIAN_POINT('Ctrl Pts',(-2.56191759893059,1.95521734542149,
14.4375062851637));
#252831=CARTESIAN_POINT('Ctrl Pts',(-2.57001467840759,1.94456196070487,
14.4383465274446));
#252832=CARTESIAN_POINT('Ctrl Pts',(-2.58416958701507,1.92569189414272,
14.4398195646805));
#252833=CARTESIAN_POINT('Ctrl Pts',(-2.59025507355398,1.91749847183039,
14.4404542175249));
#252834=CARTESIAN_POINT('Ctrl Pts',(-2.60339839594501,1.89962571127736,
14.4418278367121));
#252835=CARTESIAN_POINT('Ctrl Pts',(-2.61044127254434,1.88993582541328,
14.4425658021505));
#252836=CARTESIAN_POINT('Ctrl Pts',(-2.63001872586191,1.86268211182718,
14.444623242391));
#252837=CARTESIAN_POINT('Ctrl Pts',(-2.64243142973143,1.84503098722193,
14.4459348181242));
#252838=CARTESIAN_POINT('Ctrl Pts',(-2.72494701578867,1.72515104414752,
14.4547119954144));
#252839=CARTESIAN_POINT('Ctrl Pts',(-2.78928644385263,1.6190646147455,14.4618467594385));
#252840=CARTESIAN_POINT('Ctrl Pts',(-2.9766093496822,1.26572442235873,14.4844926102662));
#252841=CARTESIAN_POINT('Ctrl Pts',(-3.07400709813576,1.00635028865636,
14.4995587974972));
#252842=CARTESIAN_POINT('Ctrl Pts',(-3.15030109991386,0.681915629059473,
14.5191339023975));
#252843=CARTESIAN_POINT('Ctrl Pts',(-3.1619352446837,0.625756232218863,
14.522542394354));
#252844=CARTESIAN_POINT('Ctrl Pts',(-3.17643689682374,0.544957600591357,
14.5274891358243));
#252845=CARTESIAN_POINT('Ctrl Pts',(-3.18052833432557,0.5205474124033,14.5289891059011));
#252846=CARTESIAN_POINT('Ctrl Pts',(-3.18716871191596,0.477923939774208,
14.5316188901645));
#252847=CARTESIAN_POINT('Ctrl Pts',(-3.18984370069301,0.459731262481757,
14.5327447021233));
#252848=CARTESIAN_POINT('Ctrl Pts',(-3.19504790839321,0.422102541666997,
14.5350806298218));
#252849=CARTESIAN_POINT('Ctrl Pts',(-3.19755579717454,0.402664363595528,
14.5362913629958));
#252850=CARTESIAN_POINT('Ctrl Pts',(-3.20356249556793,0.352506462283499,
14.5394264579095));
#252851=CARTESIAN_POINT('Ctrl Pts',(-3.20679674749047,0.321757646781563,
14.5413589654211));
#252852=CARTESIAN_POINT('Ctrl Pts',(-3.21835897682462,0.194217824163122,
14.5494206885913));
#252853=CARTESIAN_POINT('Ctrl Pts',(-3.22275000000088,0.0971299973001183,
14.5556693739565));
#252854=CARTESIAN_POINT('Ctrl Pts',(-3.22275,-2.92740584967668E-11,14.5620312016861));
#252855=CARTESIAN_POINT('Origin',(0.,0.,-2.31077344927308));
#252856=CARTESIAN_POINT('',(-3.22275,1.40950318212534E-10,16.0607604048379));
#252857=CARTESIAN_POINT('',(-3.22275,-2.40695369623669E-12,15.8170600220821));
#252858=CARTESIAN_POINT('',(-3.22275,-3.50678552687464E-13,-2.31077344927308));
#252859=CARTESIAN_POINT('',(-3.22274878243092,0.002869896163636,16.0605665950451));
#252860=CARTESIAN_POINT('Ctrl Pts',(-3.22275,1.40950318212534E-10,16.0607604048379));
#252861=CARTESIAN_POINT('Ctrl Pts',(-3.22274999999996,0.000956430655831547,
16.0606957817113));
#252862=CARTESIAN_POINT('Ctrl Pts',(-3.22274957423342,0.00191286908978262,
16.0606311566737));
#252863=CARTESIAN_POINT('Ctrl Pts',(-3.22274872267921,0.00286931516118902,
16.0605665297975));
#252864=CARTESIAN_POINT('Ctrl Pts',(-3.22274872216818,0.00286988908068463,
16.0605664910178));
#252865=CARTESIAN_POINT('Ctrl Pts',(-3.22260972635913,0.158955561182205,
16.0500198122335));
#252866=CARTESIAN_POINT('Ctrl Pts',(-3.21113152782019,0.314837082433518,
16.0394394156062));
#252867=CARTESIAN_POINT('Ctrl Pts',(-3.18170605861958,0.51475909849832,
16.0262081803247));
#252868=CARTESIAN_POINT('Ctrl Pts',(-3.17404025376148,0.560088659893377,
16.0232319863822));
#252869=CARTESIAN_POINT('Ctrl Pts',(-3.16266995805416,0.619555231068851,
16.0193721379485));
#252870=CARTESIAN_POINT('Ctrl Pts',(-3.15983590497499,0.633850944097037,
16.0184476507336));
#252871=CARTESIAN_POINT('Ctrl Pts',(-3.15426675574805,0.660977214373375,
16.0167005540241));
#252872=CARTESIAN_POINT('Ctrl Pts',(-3.15155010899918,0.673811226303109,
16.0158770090402));
#252873=CARTESIAN_POINT('Ctrl Pts',(-3.14664724261537,0.696294890361333,
16.0144400295048));
#252874=CARTESIAN_POINT('Ctrl Pts',(-3.14449485317703,0.705951536183913,
16.0138247462876));
#252875=CARTESIAN_POINT('Ctrl Pts',(-3.13971572226225,0.726937400389772,
16.0124918147524));
#252876=CARTESIAN_POINT('Ctrl Pts',(-3.13707210484498,0.738262432658298,
16.0117751206014));
#252877=CARTESIAN_POINT('Ctrl Pts',(-3.12955106159701,0.769711948252847,
16.0097915425632));
#252878=CARTESIAN_POINT('Ctrl Pts',(-3.12454080497809,0.789804494042163,
16.0085318896235));
#252879=CARTESIAN_POINT('Ctrl Pts',(-3.09340347988852,0.90973788958046,
16.001051051618));
#252880=CARTESIAN_POINT('Ctrl Pts',(-3.06268400828473,1.00833476375011,
15.9950588056923));
#252881=CARTESIAN_POINT('Ctrl Pts',(-2.98977302668113,1.20802979414192,
15.9829360412511));
#252882=CARTESIAN_POINT('Ctrl Pts',(-2.94705725392159,1.30879098813273,
15.976825690958));
#252883=CARTESIAN_POINT('Ctrl Pts',(-2.83349118563899,1.54277683754517,
15.9622669189802));
#252884=CARTESIAN_POINT('Ctrl Pts',(-2.75825501028418,1.67357642035437,
15.9538196767181));
#252885=CARTESIAN_POINT('Ctrl Pts',(-2.62593432969368,1.87030728632341,
15.9401076233613));
#252886=CARTESIAN_POINT('Ctrl Pts',(-2.57486171042167,1.94001694707925,
15.9350313224493));
#252887=CARTESIAN_POINT('Ctrl Pts',(-2.50468067599009,2.02814769930656,
15.9282714031852));
#252888=CARTESIAN_POINT('Ctrl Pts',(-2.48805711098293,2.04850680493808,
15.926684849749));
#252889=CARTESIAN_POINT('Ctrl Pts',(-2.45883951243787,2.08340966336813,
15.92391995623));
#252890=CARTESIAN_POINT('Ctrl Pts',(-2.44636068320589,2.09804836839196,
15.9227462770801));
#252891=CARTESIAN_POINT('Ctrl Pts',(-2.42198510766311,2.12612979563819,
15.920466956722));
#252892=CARTESIAN_POINT('Ctrl Pts',(-2.41010560004475,2.13958658289417,
15.9193620491992));
#252893=CARTESIAN_POINT('Ctrl Pts',(-2.38235832019316,2.17049364683553,
15.9167944684855));
#252894=CARTESIAN_POINT('Ctrl Pts',(-2.36641031599306,2.18787019861879,
15.9153284677141));
#252895=CARTESIAN_POINT('Ctrl Pts',(-2.3134263507492,2.24434315146159,15.9104885695104));
#252896=CARTESIAN_POINT('Ctrl Pts',(-2.27560264465087,2.2826847593611,15.907081329368));
#252897=CARTESIAN_POINT('Ctrl Pts',(-2.04519299181885,2.5048295533577,15.8865922233264));
#252898=CARTESIAN_POINT('Ctrl Pts',(-1.83141718761829,2.66511726410687,
15.8685296782356));
#252899=CARTESIAN_POINT('Ctrl Pts',(-1.51733543492343,2.84481551581273,
15.8441412764353));
#252900=CARTESIAN_POINT('Ctrl Pts',(-1.43216014884925,2.88863317697712,
15.8377311712224));
#252901=CARTESIAN_POINT('Ctrl Pts',(-1.31246525100365,2.94361116032971,
15.8291034678364));
#252902=CARTESIAN_POINT('Ctrl Pts',(-1.2795241445829,2.9580787476784,15.8267674380387));
#252903=CARTESIAN_POINT('Ctrl Pts',(-1.22187280613736,2.98225563955925,
15.8227534894175));
#252904=CARTESIAN_POINT('Ctrl Pts',(-1.19727247523683,2.99221666640101,
15.8210638453471));
#252905=CARTESIAN_POINT('Ctrl Pts',(-1.16072902758536,3.0064907732883,15.8185908677699));
#252906=CARTESIAN_POINT('Ctrl Pts',(-1.14887963559707,3.01103873121741,
15.8177946841833));
#252907=CARTESIAN_POINT('Ctrl Pts',(-1.12858657003711,3.01869025110008,
15.8164412351724));
#252908=CARTESIAN_POINT('Ctrl Pts',(-1.12015640305096,3.02182860493725,
15.8158819564421));
#252909=CARTESIAN_POINT('Ctrl Pts',(-1.10085459346881,3.0289223420184,15.8146082630671));
#252910=CARTESIAN_POINT('Ctrl Pts',(-1.08997469728975,3.03285452318925,
15.8138952116988));
#252911=CARTESIAN_POINT('Ctrl Pts',(-1.05981679122292,3.04357086038286,
15.8119316098156));
#252912=CARTESIAN_POINT('Ctrl Pts',(-1.04049470115015,3.05023048940808,
15.8106880579799));
#252913=CARTESIAN_POINT('Ctrl Pts',(-0.927820452374565,3.08786996190277,
15.8035134757691));
#252914=CARTESIAN_POINT('Ctrl Pts',(-0.833143814375739,3.11474987712732,
15.7977902180428));
#252915=CARTESIAN_POINT('Ctrl Pts',(-0.54066079439401,3.18349472553782,
15.780622805304));
#252916=CARTESIAN_POINT('Ctrl Pts',(-0.340027393483033,3.21112752891242,
15.7695221294154));
#252917=CARTESIAN_POINT('Ctrl Pts',(0.00279891694355588,3.22583396828578,
15.7500744269696));
#252918=CARTESIAN_POINT('Ctrl Pts',(0.143949010686181,3.22262077444897,
15.7419363219876));
#252919=CARTESIAN_POINT('Ctrl Pts',(0.317151762627454,3.20727482009551,
15.7315449327428));
#252920=CARTESIAN_POINT('Ctrl Pts',(0.349831336743204,3.20387498649939,
15.7295668766696));
#252921=CARTESIAN_POINT('Ctrl Pts',(0.40204543872915,3.19763450077293,15.7263759574915));
#252922=CARTESIAN_POINT('Ctrl Pts',(0.421616262292587,3.19511293006904,
15.7251730703873));
#252923=CARTESIAN_POINT('Ctrl Pts',(0.458795715507767,3.18997506680548,
15.7228742849616));
#252924=CARTESIAN_POINT('Ctrl Pts',(0.476408288283485,3.18739228182276,
15.7217794773664));
#252925=CARTESIAN_POINT('Ctrl Pts',(0.516649413305925,3.18115016387692,
15.7192643172621));
#252926=CARTESIAN_POINT('Ctrl Pts',(0.539261928140943,3.17739508261763,
15.7178410032293));
#252927=CARTESIAN_POINT('Ctrl Pts',(0.598640768329683,3.16688240171998,
15.7140764217167));
#252928=CARTESIAN_POINT('Ctrl Pts',(0.635332063261136,3.15972592139947,
15.711722774622));
#252929=CARTESIAN_POINT('Ctrl Pts',(0.927791534051816,3.09738309549999,
15.6927360979667));
#252930=CARTESIAN_POINT('Ctrl Pts',(1.17605641186558,3.01188008016421,15.6751095270028));
#252931=CARTESIAN_POINT('Ctrl Pts',(1.51228289806673,2.84811490572361,15.6498465504233));
#252932=CARTESIAN_POINT('Ctrl Pts',(1.61072112697769,2.79362458950032,15.6422790304295));
#252933=CARTESIAN_POINT('Ctrl Pts',(1.75613586838751,2.70288379807742,15.6310160485125));
#252934=CARTESIAN_POINT('Ctrl Pts',(1.80529482685637,2.67030065281587,15.6271934841891));
#252935=CARTESIAN_POINT('Ctrl Pts',(1.86757903349072,2.62651115213157,15.6223575882719));
#252936=CARTESIAN_POINT('Ctrl Pts',(1.88154405970112,2.61652522633831,15.621273808906));
#252937=CARTESIAN_POINT('Ctrl Pts',(1.90410881087191,2.60011583991129,15.6195243302889));
#252938=CARTESIAN_POINT('Ctrl Pts',(1.91275721227781,2.59376032033087,15.6188542175049));
#252939=CARTESIAN_POINT('Ctrl Pts',(1.9295609133977,2.58128189760317,15.6175532650286));
#252940=CARTESIAN_POINT('Ctrl Pts',(1.93771913436894,2.57516331780016,15.6169221649739));
#252941=CARTESIAN_POINT('Ctrl Pts',(1.95596751695147,2.56134140274547,15.6155113437579));
#252942=CARTESIAN_POINT('Ctrl Pts',(1.96604159271992,2.55361688135561,15.6147330671847));
#252943=CARTESIAN_POINT('Ctrl Pts',(1.99620871114506,2.53020122962557,15.6124033390887));
#252944=CARTESIAN_POINT('Ctrl Pts',(2.01616197097816,2.51433062197575,15.6108635366975));
#252945=CARTESIAN_POINT('Ctrl Pts',(2.19488250374719,2.3686825010964,15.5970605094616));
#252946=CARTESIAN_POINT('Ctrl Pts',(2.34113429493131,2.22424772385679,15.5856649111666));
#252947=CARTESIAN_POINT('Ctrl Pts',(2.59698092367115,1.91816895056077,15.5633325604899));
#252948=CARTESIAN_POINT('Ctrl Pts',(2.70760218407184,1.75856830394266,15.5524434078279));
#252949=CARTESIAN_POINT('Ctrl Pts',(2.82854479679251,1.54534408081916,15.5379915228506));
#252950=CARTESIAN_POINT('Ctrl Pts',(2.85280534587881,1.50008507146384,15.5349311229411));
#252951=CARTESIAN_POINT('Ctrl Pts',(2.88653540269198,1.43338019057793,15.5304207724012));
#252952=CARTESIAN_POINT('Ctrl Pts',(2.8968692738074,1.41237876224875,15.5290007885634));
#252953=CARTESIAN_POINT('Ctrl Pts',(2.91468482541555,1.37515418177084,15.5264831077506));
#252954=CARTESIAN_POINT('Ctrl Pts',(2.92226216176746,1.35897773820573,15.5253887578686));
#252955=CARTESIAN_POINT('Ctrl Pts',(2.93782523594117,1.3250208818162,15.5230906175132));
#252956=CARTESIAN_POINT('Ctrl Pts',(2.94578491297969,1.30722938850427,15.521885991991));
#252957=CARTESIAN_POINT('Ctrl Pts',(2.9662787527886,1.2602836826764,15.5187054831029));
#252958=CARTESIAN_POINT('Ctrl Pts',(2.97854428562282,1.23101520050028,15.5167206452769));
#252959=CARTESIAN_POINT('Ctrl Pts',(3.03124718854209,1.09985238574996,15.5078145811562));
#252960=CARTESIAN_POINT('Ctrl Pts',(3.06689830851785,0.996125057331645,
15.5007378527394));
#252961=CARTESIAN_POINT('Ctrl Pts',(3.15420020344595,0.692585296934231,
15.4799479270727));
#252962=CARTESIAN_POINT('Ctrl Pts',(3.19204527176955,0.489374328821014,
15.4659004638993));
#252963=CARTESIAN_POINT('Ctrl Pts',(3.22049146510838,0.16779226887119,15.4441870250105));
#252964=CARTESIAN_POINT('Ctrl Pts',(3.22445495720684,0.0511349104559339,
15.4364252064716));
#252965=CARTESIAN_POINT('Ctrl Pts',(3.22152451972878,-0.0930415730923461,
15.4271570369367));
#252966=CARTESIAN_POINT('Ctrl Pts',(3.22061114091543,-0.120585907043692,
15.4254012090784));
#252967=CARTESIAN_POINT('Ctrl Pts',(3.21875235365261,-0.160987145916595,
15.4228508139463));
#252968=CARTESIAN_POINT('Ctrl Pts',(3.21808298931553,-0.173854716253167,
15.4220422542098));
#252969=CARTESIAN_POINT('Ctrl Pts',(3.21675924280161,-0.196664160630129,
15.420615997628));
#252970=CARTESIAN_POINT('Ctrl Pts',(3.21613591126108,-0.206607422912724,
15.4199966446743));
#252971=CARTESIAN_POINT('Ctrl Pts',(3.21467151848355,-0.22835181483957,
15.4186474954993));
#252972=CARTESIAN_POINT('Ctrl Pts',(3.21381158072826,-0.240151320870031,
15.4179187392443));
#252973=CARTESIAN_POINT('Ctrl Pts',(3.21119732532101,-0.273489040244611,
15.4158685615721));
#252974=CARTESIAN_POINT('Ctrl Pts',(3.20929129682661,-0.295015162756862,
15.4145551701727));
#252975=CARTESIAN_POINT('Ctrl Pts',(3.19235287051026,-0.466644754464044,
15.404154966665));
#252976=CARTESIAN_POINT('Ctrl Pts',(3.16701253893829,-0.61556224868986,
15.3955639554509));
#252977=CARTESIAN_POINT('Ctrl Pts',(3.08523970276169,-0.951520070690083,
15.3761122300471));
#252978=CARTESIAN_POINT('Ctrl Pts',(3.022074748761,-1.13629068817429,15.3653427971495));
#252979=CARTESIAN_POINT('Ctrl Pts',(2.91551271530059,-1.3748882260526,15.3503176906445));
#252980=CARTESIAN_POINT('Ctrl Pts',(2.88654996086614,-1.43469877402239,
15.3464536433615));
#252981=CARTESIAN_POINT('Ctrl Pts',(2.83296640255694,-1.53715257184504,
15.3396277231778));
#252982=CARTESIAN_POINT('Ctrl Pts',(2.80917834337105,-1.58020673331712,
15.3366931751038));
#252983=CARTESIAN_POINT('Ctrl Pts',(2.77282587982729,-1.64258454548052,
15.3323345342145));
#252984=CARTESIAN_POINT('Ctrl Pts',(2.76102399011721,-1.66234588243408,
15.3309375621765));
#252985=CARTESIAN_POINT('Ctrl Pts',(2.73971520074275,-1.6971727858827,15.3284458940265));
#252986=CARTESIAN_POINT('Ctrl Pts',(2.73029307683862,-1.71228926905903,
15.3273543107294));
#252987=CARTESIAN_POINT('Ctrl Pts',(2.7101969713993,-1.74394304133163,15.3250468203785));
#252988=CARTESIAN_POINT('Ctrl Pts',(2.69949586384522,-1.76046215778765,
15.3238299440067));
#252989=CARTESIAN_POINT('Ctrl Pts',(2.67065799523871,-1.80409745491183,
15.3205811532836));
#252990=CARTESIAN_POINT('Ctrl Pts',(2.65226005168593,-1.83103747856497,
15.3185395756064));
#252991=CARTESIAN_POINT('Ctrl Pts',(2.56332037546018,-1.95711795759643,
15.3088107924947));
#252992=CARTESIAN_POINT('Ctrl Pts',(2.48761769447146,-2.05248003318512,
15.3009293311116));
#252993=CARTESIAN_POINT('Ctrl Pts',(2.27380501007805,-2.29256755214937,
15.2796752256792));
#252994=CARTESIAN_POINT('Ctrl Pts',(2.12730754000876,-2.42911668537106,
15.2660507554026));
#252995=CARTESIAN_POINT('Ctrl Pts',(1.88177720789917,-2.61862697568247,
15.2452189209509));
#252996=CARTESIAN_POINT('Ctrl Pts',(1.79101527097696,-2.68152222767975,
15.2378915409905));
#252997=CARTESIAN_POINT('Ctrl Pts',(1.67437808777581,-2.75377852587573,
15.2290793815153));
#252998=CARTESIAN_POINT('Ctrl Pts',(1.65138174554023,-2.76763013947763,
15.2273699118184));
#252999=CARTESIAN_POINT('Ctrl Pts',(1.61721102877943,-2.78763495006677,
15.2248737083911));
#253000=CARTESIAN_POINT('Ctrl Pts',(1.60616953977432,-2.79401137233572,
15.2240737869116));
#253001=CARTESIAN_POINT('Ctrl Pts',(1.58726843148564,-2.80477762414213,
15.2227161830266));
#253002=CARTESIAN_POINT('Ctrl Pts',(1.57942790737277,-2.80920025751278,
15.2221564524602));
#253003=CARTESIAN_POINT('Ctrl Pts',(1.56150407913006,-2.8192118531124,15.2208847405414));
#253004=CARTESIAN_POINT('Ctrl Pts',(1.55140922635653,-2.82477961685034,
15.2201740956495));
#253005=CARTESIAN_POINT('Ctrl Pts',(1.52349300814275,-2.83998187063616,
15.21822365771));
#253006=CARTESIAN_POINT('Ctrl Pts',(1.50561000792679,-2.84950285536709,
15.2169907121405));
#253007=CARTESIAN_POINT('Ctrl Pts',(1.40340641488157,-2.90268566709607,
15.2100308374864));
#253008=CARTESIAN_POINT('Ctrl Pts',(1.3172707507851,-2.94277671732208,15.2044973467694));
#253009=CARTESIAN_POINT('Ctrl Pts',(1.07506092857759,-3.0427404457207,15.1895036831677));
#253010=CARTESIAN_POINT('Ctrl Pts',(0.915912046568545,-3.09437151982397,
15.1802642517259));
#253011=CARTESIAN_POINT('Ctrl Pts',(0.581554778721295,-3.17477183297286,
15.1609308371604));
#253012=CARTESIAN_POINT('Ctrl Pts',(0.406547780230568,-3.20188852858029,
15.1508453944993));
#253013=CARTESIAN_POINT('Ctrl Pts',(0.195857889254473,-3.21697739001396,
15.1382390617403));
#253014=CARTESIAN_POINT('Ctrl Pts',(0.16146729386,-3.21888676676952,15.1361675615575));
#253015=CARTESIAN_POINT('Ctrl Pts',(0.106995431247289,-3.22103593569282,
15.1328617541528));
#253016=CARTESIAN_POINT('Ctrl Pts',(0.0869306077220727,-3.22163988716715,
15.1316387587998));
#253017=CARTESIAN_POINT('Ctrl Pts',(0.049126765924715,-3.22242436530274,
15.1293240026776));
#253018=CARTESIAN_POINT('Ctrl Pts',(0.0313892863587283,-3.22264595047502,
15.1282335609304));
#253019=CARTESIAN_POINT('Ctrl Pts',(-0.00868875170015642,-3.22281571743229,
15.125759451026));
#253020=CARTESIAN_POINT('Ctrl Pts',(-0.0310285771806581,-3.22267805254223,
15.1243731680973));
#253021=CARTESIAN_POINT('Ctrl Pts',(-0.097403294180263,-3.22157881916003,
15.120232145332));
#253022=CARTESIAN_POINT('Ctrl Pts',(-0.141420439396597,-3.21994680760062,
15.1174568799119));
#253023=CARTESIAN_POINT('Ctrl Pts',(-0.409190200943396,-3.20451780634388,
15.1003896339542));
#253024=CARTESIAN_POINT('Ctrl Pts',(-0.630999839408173,-3.16830851183655,
15.0854030798675));
#253025=CARTESIAN_POINT('Ctrl Pts',(-0.978859255657224,-3.07352687871825,
15.0610381434794));
#253026=CARTESIAN_POINT('Ctrl Pts',(-1.1080935222725,-3.02933408084008,
15.0517992006517));
#253027=CARTESIAN_POINT('Ctrl Pts',(-1.27514194498351,-2.9600845322329,
15.0398733113168));
#253028=CARTESIAN_POINT('Ctrl Pts',(-1.31578821753152,-2.94224219923064,
15.036973507921));
#253029=CARTESIAN_POINT('Ctrl Pts',(-1.38427122702853,-2.91047731321657,
15.0321059981082));
#253030=CARTESIAN_POINT('Ctrl Pts',(-1.41229793631762,-2.89698113973942,
15.0301192974133));
#253031=CARTESIAN_POINT('Ctrl Pts',(-1.45222334730055,-2.87703802064566,
15.027301390109));
#253032=CARTESIAN_POINT('Ctrl Pts',(-1.46428278359424,-2.87091908062637,
15.0264518695625));
#253033=CARTESIAN_POINT('Ctrl Pts',(-1.48521826956498,-2.86013021228494,
15.0249803860178));
#253034=CARTESIAN_POINT('Ctrl Pts',(-1.49411156481751,-2.85549448989673,
15.0243563695138));
#253035=CARTESIAN_POINT('Ctrl Pts',(-1.51308591807896,-2.84549099370784,
15.0230273956593));
#253036=CARTESIAN_POINT('Ctrl Pts',(-1.52316020871888,-2.84011108561211,
15.022323197854));
#253037=CARTESIAN_POINT('Ctrl Pts',(-1.55060731429737,-2.82526563628965,
15.0204079137619));
#253038=CARTESIAN_POINT('Ctrl Pts',(-1.56792221867907,-2.81569332831976,
15.0192032783224));
#253039=CARTESIAN_POINT('Ctrl Pts',(-1.66031222517607,-2.76350022233958,
15.0127890340651));
#253040=CARTESIAN_POINT('Ctrl Pts',(-1.73374645397744,-2.71803164723146,
15.007738748511));
#253041=CARTESIAN_POINT('Ctrl Pts',(-1.9487327321651,-2.57265433837315,
14.9928295280849));
#253042=CARTESIAN_POINT('Ctrl Pts',(-2.08414691045551,-2.4642335877769,
14.9832556799089));
#253043=CARTESIAN_POINT('Ctrl Pts',(-2.32985279997184,-2.23269669021705,
14.9642850550483));
#253044=CARTESIAN_POINT('Ctrl Pts',(-2.44069163567604,-2.11096293798475,
14.9549302786212));
#253045=CARTESIAN_POINT('Ctrl Pts',(-2.56861352591344,-1.94685664948597,
14.9425998820218));
#253046=CARTESIAN_POINT('Ctrl Pts',(-2.59476838965091,-1.91185851764458,
14.9399860794798));
#253047=CARTESIAN_POINT('Ctrl Pts',(-2.63299878097278,-1.85847195590325,
14.9360162897142));
#253048=CARTESIAN_POINT('Ctrl Pts',(-2.6456113326674,-1.84047309983463,
14.9346808006205));
#253049=CARTESIAN_POINT('Ctrl Pts',(-2.66796033888545,-1.80787528997435,
14.9322665221954));
#253050=CARTESIAN_POINT('Ctrl Pts',(-2.67776359925488,-1.79332303876533,
14.9311903059231));
#253051=CARTESIAN_POINT('Ctrl Pts',(-2.69863006067927,-1.76179564263779,
14.9288616572182));
#253052=CARTESIAN_POINT('Ctrl Pts',(-2.70965293741618,-1.74479483601776,
14.9276077854255));
#253053=CARTESIAN_POINT('Ctrl Pts',(-2.7389612006861,-1.69864449239057,
14.9242083371454));
#253054=CARTESIAN_POINT('Ctrl Pts',(-2.75694083973245,-1.66930483447005,
14.9220517227058));
#253055=CARTESIAN_POINT('Ctrl Pts',(-2.85797542106756,-1.49834805414221,
14.9095074121094));
#253056=CARTESIAN_POINT('Ctrl Pts',(-2.9305701316707,-1.35085719686086,
14.8987520889994));
#253057=CARTESIAN_POINT('Ctrl Pts',(-3.06498357548507,-1.015343676264,14.8745641533478));
#253058=CARTESIAN_POINT('Ctrl Pts',(-3.12138250328075,-0.825843134724053,
14.861072194129));
#253059=CARTESIAN_POINT('Ctrl Pts',(-3.17059709252073,-0.579909243797049,
14.8444311187627));
#253060=CARTESIAN_POINT('Ctrl Pts',(-3.17978879926637,-0.527185401921884,
14.8409150934723));
#253061=CARTESIAN_POINT('Ctrl Pts',(-3.19291800919129,-0.438938468991591,
14.8351405265175));
#253062=CARTESIAN_POINT('Ctrl Pts',(-3.19758525627638,-0.403535827775161,
14.8328533034425));
#253063=CARTESIAN_POINT('Ctrl Pts',(-3.20329412037733,-0.353875999502981,
14.8296927176033));
#253064=CARTESIAN_POINT('Ctrl Pts',(-3.20483059793441,-0.339679703426401,
14.8287946424856));
#253065=CARTESIAN_POINT('Ctrl Pts',(-3.20729702365965,-0.315382681112745,
14.827267424476));
#253066=CARTESIAN_POINT('Ctrl Pts',(-3.20827372351705,-0.30528701214969,
14.8266357581805));
#253067=CARTESIAN_POINT('Ctrl Pts',(-3.21021583315862,-0.284172827007799,
14.825320948772));
#253068=CARTESIAN_POINT('Ctrl Pts',(-3.21117220368781,-0.273153762225458,
14.8246382985928));
#253069=CARTESIAN_POINT('Ctrl Pts',(-3.21358946746526,-0.24353322742016,
14.8228121934577));
#253070=CARTESIAN_POINT('Ctrl Pts',(-3.21494560370638,-0.224923322443813,
14.8216743556143));
#253071=CARTESIAN_POINT('Ctrl Pts',(-3.2205056898234,-0.138244574017291,
14.8164143686205));
#253072=CARTESIAN_POINT('Ctrl Pts',(-3.2227102601513,-0.0700602807453514,
14.8123903960569));
#253073=CARTESIAN_POINT('Ctrl Pts',(-3.22274982252387,-0.00123500483905878,
14.8083979017871));
#253074=CARTESIAN_POINT('Ctrl Pts',(-3.22275,-0.000617500973495014,14.8083620865646));
#253075=CARTESIAN_POINT('Ctrl Pts',(-3.22275,1.96138700782895E-11,14.8083262771147));
#253076=CARTESIAN_POINT('Ctrl Pts',(-3.22275,-2.92740584967668E-11,14.5620312016861));
#253077=CARTESIAN_POINT('Ctrl Pts',(-3.22274999999999,-0.000767382685586242,
14.5620814637719));
#253078=CARTESIAN_POINT('Ctrl Pts',(-3.22274972607258,-0.00153476798980013,
14.5621317326809));
#253079=CARTESIAN_POINT('Ctrl Pts',(-3.22262792044864,-0.172048925614069,
14.5733030758767));
#253080=CARTESIAN_POINT('Ctrl Pts',(-3.20909564308139,-0.341507159977076,
14.5847558065709));
#253081=CARTESIAN_POINT('Ctrl Pts',(-3.15666552162296,-0.669240997370065,
14.6071826385691));
#253082=CARTESIAN_POINT('Ctrl Pts',(-3.11899104670159,-0.827239278373474,
14.6181198783632));
#253083=CARTESIAN_POINT('Ctrl Pts',(-3.06037229256215,-1.01052066348497,
14.6305171017099));
#253084=CARTESIAN_POINT('Ctrl Pts',(-3.05076289908809,-1.03917104696589,
14.6324459323832));
#253085=CARTESIAN_POINT('Ctrl Pts',(-3.03631282695233,-1.08032471510789,
14.6351991464015));
#253086=CARTESIAN_POINT('Ctrl Pts',(-3.03179519261813,-1.09293869815829,
14.6360406527494));
#253087=CARTESIAN_POINT('Ctrl Pts',(-3.02368909401783,-1.11513519884456,
14.6375167664725));
#253088=CARTESIAN_POINT('Ctrl Pts',(-3.02013347537823,-1.12472932323589,
14.6381532311103));
#253089=CARTESIAN_POINT('Ctrl Pts',(-3.0123722909868,-1.14536912080494,
14.6395189697861));
#253090=CARTESIAN_POINT('Ctrl Pts',(-3.00815160885961,-1.15640872996861,
14.6402473546126));
#253091=CARTESIAN_POINT('Ctrl Pts',(-2.99610459724462,-1.18740657319459,
14.6422872906105));
#253092=CARTESIAN_POINT('Ctrl Pts',(-2.98813956500924,-1.20731069876947,
14.6435909772437));
#253093=CARTESIAN_POINT('Ctrl Pts',(-2.9310664369083,-1.34590722029258,
14.6526352805466));
#253094=CARTESIAN_POINT('Ctrl Pts',(-2.87509363803544,-1.46166367253961,
14.660018389446));
#253095=CARTESIAN_POINT('Ctrl Pts',(-2.66912284152672,-1.82973444896855,
14.6838768977901));
#253096=CARTESIAN_POINT('Ctrl Pts',(-2.49163642882076,-2.06491867333873,
14.6998860792243));
#253097=CARTESIAN_POINT('Ctrl Pts',(-2.25721071448654,-2.30057520782022,
14.7195886782357));
#253098=CARTESIAN_POINT('Ctrl Pts',(-2.2291329057991,-2.32779139763092,
14.7219262570076));
#253099=CARTESIAN_POINT('Ctrl Pts',(-2.18345042807594,-2.37048744727025,
14.7256992478237));
#253100=CARTESIAN_POINT('Ctrl Pts',(-2.16615952956548,-2.38629825415869,
14.727120643631));
#253101=CARTESIAN_POINT('Ctrl Pts',(-2.13509420835349,-2.41408853449397,
14.7296634916327));
#253102=CARTESIAN_POINT('Ctrl Pts',(-2.12138738289456,-2.42614226318123,
14.7307817871995));
#253103=CARTESIAN_POINT('Ctrl Pts',(-2.0924557422095,-2.45115200607763,
14.7331350055754));
#253104=CARTESIAN_POINT('Ctrl Pts',(-2.07721132979201,-2.46408405961907,
14.7343708404358));
#253105=CARTESIAN_POINT('Ctrl Pts',(-2.03668415535031,-2.49782049272015,
14.7376461321974));
#253106=CARTESIAN_POINT('Ctrl Pts',(-2.0112034680001,-2.51838242667737,
14.7396951686319));
#253107=CARTESIAN_POINT('Ctrl Pts',(-1.88159835097917,-2.61974725971168,
14.7500698591014));
#253108=CARTESIAN_POINT('Ctrl Pts',(-1.77291187542261,-2.6944877146309,
14.7586261025567));
#253109=CARTESIAN_POINT('Ctrl Pts',(-1.54217406319262,-2.83314355611134,
14.7764741240285));
#253110=CARTESIAN_POINT('Ctrl Pts',(-1.41997959155703,-2.89631790401781,
14.7857640834384));
#253111=CARTESIAN_POINT('Ctrl Pts',(-1.24805070249182,-2.97170303841608,
14.7984471437018));
#253112=CARTESIAN_POINT('Ctrl Pts',(-1.20150000534579,-2.9908272047466,
14.8018431480429));
#253113=CARTESIAN_POINT('Ctrl Pts',(-1.04242728965904,-3.05186461663847,
14.8132879123654));
#253114=CARTESIAN_POINT('Ctrl Pts',(-0.928006460376373,-3.08858255019199,
14.8212562453868));
#253115=CARTESIAN_POINT('Ctrl Pts',(-0.791009219811731,-3.12424122018396,
14.8302987420042));
#253116=CARTESIAN_POINT('Ctrl Pts',(-0.770171365661151,-3.12944322718091,
14.8316607387411));
#253117=CARTESIAN_POINT('Ctrl Pts',(-0.737654004471244,-3.13721645406425,
14.8337636708378));
#253118=CARTESIAN_POINT('Ctrl Pts',(-0.726009976777438,-3.13993153336891,
14.8345122423729));
#253119=CARTESIAN_POINT('Ctrl Pts',(-0.704490228448732,-3.14482326011948,
14.8358871411926));
#253120=CARTESIAN_POINT('Ctrl Pts',(-0.694619309379324,-3.1470182455876,
14.8365144424809));
#253121=CARTESIAN_POINT('Ctrl Pts',(-0.671684335039595,-3.15200510238433,
14.8379643598919));
#253122=CARTESIAN_POINT('Ctrl Pts',(-0.658613079192044,-3.15476224742492,
14.8387850287275));
#253123=CARTESIAN_POINT('Ctrl Pts',(-0.616918582158315,-3.16328651007499,
14.841385810054));
#253124=CARTESIAN_POINT('Ctrl Pts',(-0.588233085062097,-3.16874613265094,
14.8431497064004));
#253125=CARTESIAN_POINT('Ctrl Pts',(-0.43184286827307,-3.19631440646347,
14.8526477448267));
#253126=CARTESIAN_POINT('Ctrl Pts',(-0.302954750400545,-3.21109628466694,
14.8600497376072));
#253127=CARTESIAN_POINT('Ctrl Pts',(0.0542576625291786,-3.23035677095754,
14.8802181176223));
#253128=CARTESIAN_POINT('Ctrl Pts',(0.282678902479633,-3.21842175425126,
14.8927728652563));
#253129=CARTESIAN_POINT('Ctrl Pts',(0.58538006046655,-3.17011037273422,
14.9105566519764));
#253130=CARTESIAN_POINT('Ctrl Pts',(0.66235250231329,-3.15492588422435,
14.9151752055714));
#253131=CARTESIAN_POINT('Ctrl Pts',(0.766592766396783,-3.13037933925601,
14.9216011050474));
#253132=CARTESIAN_POINT('Ctrl Pts',(0.794405547796953,-3.12343705283311,
14.9233324053845));
#253133=CARTESIAN_POINT('Ctrl Pts',(0.838765670823335,-3.11173360490088,
14.9261222914766));
#253134=CARTESIAN_POINT('Ctrl Pts',(0.855374271370775,-3.10720915235227,
14.9271732849796));
#253135=CARTESIAN_POINT('Ctrl Pts',(0.889656632818029,-3.09757438899982,
14.9293564181183));
#253136=CARTESIAN_POINT('Ctrl Pts',(0.907324439732689,-3.09244536874144,
14.9304891263085));
#253137=CARTESIAN_POINT('Ctrl Pts',(0.948709965642377,-3.08004583198981,
14.9331607486942));
#253138=CARTESIAN_POINT('Ctrl Pts',(0.972389308870204,-3.07265225877324,
14.934703595816));
#253139=CARTESIAN_POINT('Ctrl Pts',(1.05084018315465,-3.04715931055071,
14.9398637979903));
#253140=CARTESIAN_POINT('Ctrl Pts',(1.10520840908769,-3.02786371032272,
14.9435196171964));
#253141=CARTESIAN_POINT('Ctrl Pts',(1.41682459348787,-2.90775826472048,
14.9649494238707));
#253142=CARTESIAN_POINT('Ctrl Pts',(1.66074425899616,-2.77566733771619,
14.9837707369428));
#253143=CARTESIAN_POINT('Ctrl Pts',(1.98471372622241,-2.54208720145296,
15.0106153840908));
#253144=CARTESIAN_POINT('Ctrl Pts',(2.080444939307,-2.46435610055872,15.0188001601895));
#253145=CARTESIAN_POINT('Ctrl Pts',(2.18742684176691,-2.36680081505183,
15.0280492950521));
#253146=CARTESIAN_POINT('Ctrl Pts',(2.20321023855988,-2.35211542838452,
15.0294165496566));
#253147=CARTESIAN_POINT('Ctrl Pts',(2.22752976226661,-2.32902814548161,
15.0315258362517));
#253148=CARTESIAN_POINT('Ctrl Pts',(2.23616810642243,-2.32073547711821,
15.0322755752576));
#253149=CARTESIAN_POINT('Ctrl Pts',(2.25208382637645,-2.30528527109465,
15.0336575493209));
#253150=CARTESIAN_POINT('Ctrl Pts',(2.25937346856661,-2.2981412653412,15.0342907182267));
#253151=CARTESIAN_POINT('Ctrl Pts',(2.27614719799126,-2.28154569535308,
15.0357483026882));
#253152=CARTESIAN_POINT('Ctrl Pts',(2.28560645558018,-2.27206953495655,
15.0365707998224));
#253153=CARTESIAN_POINT('Ctrl Pts',(2.31562241257233,-2.24162278668299,
15.0391834957291));
#253154=CARTESIAN_POINT('Ctrl Pts',(2.33595228933482,-2.22042944342507,
15.0409572686508));
#253155=CARTESIAN_POINT('Ctrl Pts',(2.44553006920246,-2.10302659896107,
15.0505609231054));
#253156=CARTESIAN_POINT('Ctrl Pts',(2.52913628919186,-2.00170300407092,
15.0580504976579));
#253157=CARTESIAN_POINT('Ctrl Pts',(2.74323394131785,-1.7073242326538,15.0785640187537));
#253158=CARTESIAN_POINT('Ctrl Pts',(2.8593304076003,-1.50483039954838,15.09137500281));
#253159=CARTESIAN_POINT('Ctrl Pts',(2.98205684632037,-1.22427705960473,
15.1091860068409));
#253160=CARTESIAN_POINT('Ctrl Pts',(3.00919415828918,-1.15597002005049,
15.113521356035));
#253161=CARTESIAN_POINT('Ctrl Pts',(3.0434004154401,-1.06047779841409,15.119612144367));
#253162=CARTESIAN_POINT('Ctrl Pts',(3.05248568779449,-1.03403592843406,
15.1213017080211));
#253163=CARTESIAN_POINT('Ctrl Pts',(3.06656622505557,-0.991252241567517,
15.1240417947097));
#253164=CARTESIAN_POINT('Ctrl Pts',(3.07177767952471,-0.974982712250784,
15.1250852348271));
#253165=CARTESIAN_POINT('Ctrl Pts',(3.08235784674524,-0.94102567389393,
15.1272664441877));
#253166=CARTESIAN_POINT('Ctrl Pts',(3.08770422337394,-0.923331912604987,
15.128404892531));
#253167=CARTESIAN_POINT('Ctrl Pts',(3.10001548794778,-0.881284913735006,
15.1311152056547));
#253168=CARTESIAN_POINT('Ctrl Pts',(3.10684597185512,-0.856893910354364,
15.132691332695));
#253169=CARTESIAN_POINT('Ctrl Pts',(3.12912232057025,-0.773577239534555,
15.1380896817673));
#253170=CARTESIAN_POINT('Ctrl Pts',(3.14318398662438,-0.714298167223327,
15.1419554046626));
#253171=CARTESIAN_POINT('Ctrl Pts',(3.17350006404845,-0.568170087036102,
15.151550005026));
#253172=CARTESIAN_POINT('Ctrl Pts',(3.18787861788167,-0.480986189516279,
15.1573309124744));
#253173=CARTESIAN_POINT('Ctrl Pts',(3.21519197869008,-0.258865712997641,
15.1721747905934));
#253174=CARTESIAN_POINT('Ctrl Pts',(3.22323047421431,-0.123501466520903,
15.1813323999834));
#253175=CARTESIAN_POINT('Ctrl Pts',(3.2225484698029,0.0602889171238125,
15.1937496464241));
#253176=CARTESIAN_POINT('Ctrl Pts',(3.22128196385264,0.108609442932034,
15.1970118086537));
#253177=CARTESIAN_POINT('Ctrl Pts',(3.21296707059381,0.279213865080282,
15.208490706513));
#253178=CARTESIAN_POINT('Ctrl Pts',(3.20003567244147,0.401117954041918,
15.2166254546426));
#253179=CARTESIAN_POINT('Ctrl Pts',(3.17670512328315,0.543255038579436,
15.2258268565323));
#253180=CARTESIAN_POINT('Ctrl Pts',(3.17300332814693,0.564474458401743,
15.2271928970535));
#253181=CARTESIAN_POINT('Ctrl Pts',(3.16691370069047,0.597426527976927,
15.2293007165237));
#253182=CARTESIAN_POINT('Ctrl Pts',(3.16467283983157,0.609185252185454,
15.2300501861064));
#253183=CARTESIAN_POINT('Ctrl Pts',(3.1603997966497,0.630947604235671,15.2314319239441));
#253184=CARTESIAN_POINT('Ctrl Pts',(3.1583855948625,0.640954126186585,15.2320651231602));
#253185=CARTESIAN_POINT('Ctrl Pts',(3.15361816376711,0.664070379874472,
15.2335231120442));
#253186=CARTESIAN_POINT('Ctrl Pts',(3.15083070781573,0.677172694024774,
15.2343459793919));
#253187=CARTESIAN_POINT('Ctrl Pts',(3.14166480165795,0.718974369403137,
15.2369610924942));
#253188=CARTESIAN_POINT('Ctrl Pts',(3.13497511682382,0.747604857574493,
15.2387368696829));
#253189=CARTESIAN_POINT('Ctrl Pts',(3.09621062325606,0.903828087792487,
15.2483620720358));
#253190=CARTESIAN_POINT('Ctrl Pts',(3.05673448154163,1.02946922177239,15.2558695136295));
#253191=CARTESIAN_POINT('Ctrl Pts',(2.92611878125399,1.37060672301495,15.2764538909851));
#253192=CARTESIAN_POINT('Ctrl Pts',(2.81906855047291,1.57910818887085,15.2893176559885));
#253193=CARTESIAN_POINT('Ctrl Pts',(2.65051278262038,1.83470785784223,15.307135252183));
#253194=CARTESIAN_POINT('Ctrl Pts',(2.60858329678742,1.89384872119884,15.311413123281));
#253195=CARTESIAN_POINT('Ctrl Pts',(2.54785766296859,1.9736545538385,15.3174356940224));
#253196=CARTESIAN_POINT('Ctrl Pts',(2.53073197158215,1.99556673244552,15.3191164886264));
#253197=CARTESIAN_POINT('Ctrl Pts',(2.50264863222939,2.03055616094981,15.321846138496));
#253198=CARTESIAN_POINT('Ctrl Pts',(2.49186675303018,2.04377312022222,15.3228880162837));
#253199=CARTESIAN_POINT('Ctrl Pts',(2.46917045085927,2.07114877547519,15.3250689792181));
#253200=CARTESIAN_POINT('Ctrl Pts',(2.45723801238995,2.08529165669815,15.3262087675979));
#253201=CARTESIAN_POINT('Ctrl Pts',(2.42860811102907,2.11863818598469,15.3289278661098));
#253202=CARTESIAN_POINT('Ctrl Pts',(2.41180388185956,2.13774813681059,15.3305115135603));
#253203=CARTESIAN_POINT('Ctrl Pts',(2.35350943979924,2.20247893214203,15.3359649118618));
#253204=CARTESIAN_POINT('Ctrl Pts',(2.31093917566014,2.24710467707102,15.3398793745825));
#253205=CARTESIAN_POINT('Ctrl Pts',(2.20325759252548,2.35368793583731,15.3496241255134));
#253206=CARTESIAN_POINT('Ctrl Pts',(2.1367872393462,2.41419324126008,15.3555086166336));
#253207=CARTESIAN_POINT('Ctrl Pts',(1.96526969834919,2.55768066347925,15.3703518457181));
#253208=CARTESIAN_POINT('Ctrl Pts',(1.85741781148559,2.6370458943435,15.3793966080237));
#253209=CARTESIAN_POINT('Ctrl Pts',(1.70213803905913,2.7370489699189,15.3918745100475));
#253210=CARTESIAN_POINT('Ctrl Pts',(1.65867513142002,2.76360415220034,15.3953113102629));
#253211=CARTESIAN_POINT('Ctrl Pts',(1.51147842547885,2.84881526876242,15.4067338443869));
#253212=CARTESIAN_POINT('Ctrl Pts',(1.40511364272094,2.90275332807333,15.4146397494747));
#253213=CARTESIAN_POINT('Ctrl Pts',(1.27635418013286,2.9593069775233,15.4236225872744));
#253214=CARTESIAN_POINT('Ctrl Pts',(1.2566263008223,2.96773788889347,15.4249830664332));
#253215=CARTESIAN_POINT('Ctrl Pts',(1.22577940705626,2.98055787225596,15.4270841640641));
#253216=CARTESIAN_POINT('Ctrl Pts',(1.21471807378909,2.98508297983287,15.4278323983157));
#253217=CARTESIAN_POINT('Ctrl Pts',(1.19425044427644,2.9933235225987,15.4292070032503));
#253218=CARTESIAN_POINT('Ctrl Pts',(1.18485177272872,2.9970562415297,15.4298343443191));
#253219=CARTESIAN_POINT('Ctrl Pts',(1.16298982712552,3.00561988287328,15.4312847706754));
#253220=CARTESIAN_POINT('Ctrl Pts',(1.15051390417519,3.0104175771992,15.4321059038115));
#253221=CARTESIAN_POINT('Ctrl Pts',(1.11065158094814,3.02546287801877,15.4347097077152));
#253222=CARTESIAN_POINT('Ctrl Pts',(1.08315458504291,3.03541576060018,15.4364761092655));
#253223=CARTESIAN_POINT('Ctrl Pts',(0.932683714788523,3.08757539610112,
15.4460008493636));
#253224=CARTESIAN_POINT('Ctrl Pts',(0.807365070279258,3.12268943643086,
15.4534249855466));
#253225=CARTESIAN_POINT('Ctrl Pts',(0.456150134045896,3.19853249709384,
15.4736803000677));
#253226=CARTESIAN_POINT('Ctrl Pts',(0.227531665699287,3.22287285220127,
15.4862994576544));
#253227=CARTESIAN_POINT('Ctrl Pts',(-0.07891087263912,3.22270802118565,
15.504089336431));
#253228=CARTESIAN_POINT('Ctrl Pts',(-0.156056923781871,3.21989422122287,
15.5086360512408));
#253229=CARTESIAN_POINT('Ctrl Pts',(-0.261439217191516,3.21225447175947,
15.5149771082864));
#253230=CARTESIAN_POINT('Ctrl Pts',(-0.289825591467194,3.2098177991622,
15.5166980578801));
#253231=CARTESIAN_POINT('Ctrl Pts',(-0.33527265443123,3.2053088786997,15.5194755757948));
#253232=CARTESIAN_POINT('Ctrl Pts',(-0.352355945046317,3.20347592950716,
15.5205246793437));
#253233=CARTESIAN_POINT('Ctrl Pts',(-0.387719329030133,3.19939533012292,
15.5227072261354));
#253234=CARTESIAN_POINT('Ctrl Pts',(-0.405996407502154,3.19712740619109,
15.5238412647199));
#253235=CARTESIAN_POINT('Ctrl Pts',(-0.448966159931648,3.19142107427935,
15.5265220272803));
#253236=CARTESIAN_POINT('Ctrl Pts',(-0.473640084332162,3.18785258459176,
15.5280727618363));
#253237=CARTESIAN_POINT('Ctrl Pts',(-0.556004149865956,3.17496328462266,
15.5332886217382));
#253238=CARTESIAN_POINT('Ctrl Pts',(-0.61347906660195,3.16436015697816,
15.5369933591114));
#253239=CARTESIAN_POINT('Ctrl Pts',(-0.752199399764213,3.13484738905813,
15.5460981285163));
#253240=CARTESIAN_POINT('Ctrl Pts',(-0.833057519184828,3.11433547559767,
15.5515434560678));
#253241=CARTESIAN_POINT('Ctrl Pts',(-1.04968617135856,3.05034142511166,
15.5664892216815));
#253242=CARTESIAN_POINT('Ctrl Pts',(-1.18351263293232,3.00095271139991,
15.576118095521));
#253243=CARTESIAN_POINT('Ctrl Pts',(-1.45893570678965,2.87801098793581,
15.5964967507057));
#253244=CARTESIAN_POINT('Ctrl Pts',(-1.5992579213983,2.80246743793846,15.6072194817099));
#253245=CARTESIAN_POINT('Ctrl Pts',(-1.75879094935539,2.70068077691521,
15.6194097825894));
#253246=CARTESIAN_POINT('Ctrl Pts',(-1.783920978429,2.68414760287178,15.6213296248371));
#253247=CARTESIAN_POINT('Ctrl Pts',(-1.81988549782616,2.65975810852582,
15.624072457675));
#253248=CARTESIAN_POINT('Ctrl Pts',(-1.83090753582403,2.65218288037971,
15.6249123989887));
#253249=CARTESIAN_POINT('Ctrl Pts',(-1.84997421598674,2.63890322002242,
15.6263637981408));
#253250=CARTESIAN_POINT('Ctrl Pts',(-1.85804029279344,2.63323016172793,
15.6269772912239));
#253251=CARTESIAN_POINT('Ctrl Pts',(-1.86624909445508,2.62740022126393,
15.6276010601598));
#253252=CARTESIAN_POINT('Ctrl Pts',(-1.8664176600901,2.62728048052659,15.6276138688601));
#253253=CARTESIAN_POINT('Ctrl Pts',(-1.86670813507835,2.62707409931672,
15.6276359406142));
#253254=CARTESIAN_POINT('Ctrl Pts',(-1.86683004989755,2.62698746659895,
15.6276452041946));
#253255=CARTESIAN_POINT('Ctrl Pts',(-1.86713779217371,2.62676875257682,
15.6276685873888));
#253256=CARTESIAN_POINT('Ctrl Pts',(-1.86732361168996,2.62663666000887,
15.6276827062381));
#253257=CARTESIAN_POINT('Ctrl Pts',(-1.86768387906037,2.62638050103607,
15.6277100793555));
#253258=CARTESIAN_POINT('Ctrl Pts',(-1.86785832856042,2.62625643697488,
15.627723333782));
#253259=CARTESIAN_POINT('Ctrl Pts',(-1.86819701832462,2.62601551858567,
15.6277490664731));
#253260=CARTESIAN_POINT('Ctrl Pts',(-1.86836125998449,2.625898666232,15.6277615448717));
#253261=CARTESIAN_POINT('Ctrl Pts',(-1.86868053723207,2.62567146621253,
15.6277858018073));
#253262=CARTESIAN_POINT('Ctrl Pts',(-1.86883557400796,2.62556112022459,
15.6277975804582));
#253263=CARTESIAN_POINT('Ctrl Pts',(-1.86913731257558,2.6253463203299,15.6278205041488));
#253264=CARTESIAN_POINT('Ctrl Pts',(-1.86928401537687,2.62524186786447,
15.6278316492853));
#253265=CARTESIAN_POINT('Ctrl Pts',(-1.86956984662064,2.62503831977431,
15.6278533637931));
#253266=CARTESIAN_POINT('Ctrl Pts',(-1.86970897594874,2.62493922537902,
15.6278639332489));
#253267=CARTESIAN_POINT('Ctrl Pts',(-1.86998032796107,2.62474592330315,
15.6278845471724));
#253268=CARTESIAN_POINT('Ctrl Pts',(-1.87011255139784,2.62465171669732,
15.6278945917123));
#253269=CARTESIAN_POINT('Ctrl Pts',(-1.87037068053567,2.62446777533981,
15.627914200586));
#253270=CARTESIAN_POINT('Ctrl Pts',(-1.87049658689426,2.62437804152175,
15.6279237649827));
#253271=CARTESIAN_POINT('Ctrl Pts',(-1.87074260362601,2.62420267800289,
15.6279424532436));
#253272=CARTESIAN_POINT('Ctrl Pts',(-1.87086271457068,2.62411704912113,
15.6279515771623));
#253273=CARTESIAN_POINT('Ctrl Pts',(-1.87109760463354,2.62394956817173,
15.6279694197596));
#253274=CARTESIAN_POINT('Ctrl Pts',(-1.87121238425372,2.62386771682368,
15.6279781384862));
#253275=CARTESIAN_POINT('Ctrl Pts',(-1.87143702615721,2.62370749852932,
15.6279952022136));
#253276=CARTESIAN_POINT('Ctrl Pts',(-1.87154688889624,2.62362913220865,
15.6280035472578));
#253277=CARTESIAN_POINT('Ctrl Pts',(-1.87176206862088,2.62347562171071,
15.6280198918716));
#253278=CARTESIAN_POINT('Ctrl Pts',(-1.87186738598043,2.62340047810873,
15.6280278914773));
#253279=CARTESIAN_POINT('Ctrl Pts',(-1.87207380899988,2.62325317718014,
15.628043570611));
#253280=CARTESIAN_POINT('Ctrl Pts',(-1.87217491503742,2.62318102033269,
15.6280512501744));
#253281=CARTESIAN_POINT('Ctrl Pts',(-1.8723732168645,2.6230394799792,15.6280663121408));
#253282=CARTESIAN_POINT('Ctrl Pts',(-1.87247041297913,2.62297009690901,
15.6280736945745));
#253283=CARTESIAN_POINT('Ctrl Pts',(-1.87266116776736,2.6228339113356,15.6280881830205));
#253284=CARTESIAN_POINT('Ctrl Pts',(-1.87275472671033,2.62276710923786,
15.6280952890586));
#253285=CARTESIAN_POINT('Ctrl Pts',(-1.87293845464365,2.6226359106621,15.6281092435268));
#253286=CARTESIAN_POINT('Ctrl Pts',(-1.87302862389671,2.6225715145332,15.6281160919817));
#253287=CARTESIAN_POINT('Ctrl Pts',(-1.87320579768508,2.6224449686221,15.628129548405));
#253288=CARTESIAN_POINT('Ctrl Pts',(-1.8732928024416,2.62238281916521,15.6281361563945));
#253289=CARTESIAN_POINT('Ctrl Pts',(-1.87346385268252,2.62226062126964,
15.6281491475035));
#253290=CARTESIAN_POINT('Ctrl Pts',(-1.87354789836182,2.62220057312813,
15.6281555306417));
#253291=CARTESIAN_POINT('Ctrl Pts',(-1.87371321826917,2.622082444959,15.6281680863245));
#253292=CARTESIAN_POINT('Ctrl Pts',(-1.87379449268754,2.6220243651905,15.6281742588871));
#253293=CARTESIAN_POINT('Ctrl Pts',(-1.87395444223003,2.6219100519084,15.6281864065042));
#253294=CARTESIAN_POINT('Ctrl Pts',(-1.87403311752096,2.62185381863419,
15.6281923815745));
#253295=CARTESIAN_POINT('Ctrl Pts',(-1.8741880269229,2.6217430863875,15.6282041462247));
#253296=CARTESIAN_POINT('Ctrl Pts',(-1.8742642611832,2.62168858763453,15.6282099358189));
#253297=CARTESIAN_POINT('Ctrl Pts',(-1.87441443402612,2.62158122137698,
15.6282213405757));
#253298=CARTESIAN_POINT('Ctrl Pts',(-1.8744883727487,2.62152835406979,15.6282269557516));
#253299=CARTESIAN_POINT('Ctrl Pts',(-1.87463408876017,2.62142415559657,
15.6282380218747));
#253300=CARTESIAN_POINT('Ctrl Pts',(-1.87470586615115,2.62137282462936,
15.6282434728321));
#253301=CARTESIAN_POINT('Ctrl Pts',(-1.87484738340222,2.6212716110319,15.6282542199349));
#253302=CARTESIAN_POINT('Ctrl Pts',(-1.87491712340862,2.62122172854588,
15.6282595160937));
#253303=CARTESIAN_POINT('Ctrl Pts',(-1.87505468066352,2.62112333055405,
15.6282699623219));
#253304=CARTESIAN_POINT('Ctrl Pts',(-1.87512249803183,2.62107481519086,
15.6282751124025));
#253305=CARTESIAN_POINT('Ctrl Pts',(-1.87525631643748,2.62097907598431,
15.6282852745625));
#253306=CARTESIAN_POINT('Ctrl Pts',(-1.87532231756739,2.62093185228459,
15.6282902866508));
#253307=CARTESIAN_POINT('Ctrl Pts',(-1.87545260232371,2.62083862631521,
15.6283001803367));
#253308=CARTESIAN_POINT('Ctrl Pts',(-1.87551688603248,2.62079262417987,
15.6283050619422));
#253309=CARTESIAN_POINT('Ctrl Pts',(-1.87564382787277,2.62070177612791,
15.6283147016485));
#253310=CARTESIAN_POINT('Ctrl Pts',(-1.87570648608583,2.62065693033116,
15.6283194597569));
#253311=CARTESIAN_POINT('Ctrl Pts',(-1.87583026254316,2.62056833421241,
15.6283288589745));
#253312=CARTESIAN_POINT('Ctrl Pts',(-1.87589138087947,2.62052458398918,
15.6283335000921));
#253313=CARTESIAN_POINT('Ctrl Pts',(-1.87601215759189,2.62043812223277,
15.6283426714078));
#253314=CARTESIAN_POINT('Ctrl Pts',(-1.87607181600051,2.62039541082867,
15.6283472016098));
#253315=CARTESIAN_POINT('Ctrl Pts',(-1.87618974744126,2.62031097376496,
15.628356156762));
#253316=CARTESIAN_POINT('Ctrl Pts',(-1.87624802056013,2.62026924818443,
15.62836058172));
#253317=CARTESIAN_POINT('Ctrl Pts',(-1.87636325136359,2.62018673310514,
15.6283693316989));
#253318=CARTESIAN_POINT('Ctrl Pts',(-1.87642020909066,2.62014594370697,
15.6283736567242));
#253319=CARTESIAN_POINT('Ctrl Pts',(-1.87653287452234,2.62006525453705,
15.6283822118081));
#253320=CARTESIAN_POINT('Ctrl Pts',(-1.87658858230475,2.62002535483129,
15.6283864418736));
#253321=CARTESIAN_POINT('Ctrl Pts',(-1.87669880930821,2.61994640138662,
15.6283948117082));
#253322=CARTESIAN_POINT('Ctrl Pts',(-1.87675332857785,2.61990734772616,
15.6283989514819));
#253323=CARTESIAN_POINT('Ctrl Pts',(-1.87691024925368,2.61979493369505,
15.628410866767));
#253324=CARTESIAN_POINT('Ctrl Pts',(-1.87701264758681,2.61972156901586,
15.6284186419897));
#253325=CARTESIAN_POINT('Ctrl Pts',(-1.87721724407751,2.61957496492208,
15.6284341770814));
#253326=CARTESIAN_POINT('Ctrl Pts',(-1.87731944226978,2.61950172551658,
15.6284419369535));
#253327=CARTESIAN_POINT('Ctrl Pts',(-1.87752367084564,2.61935534887376,
15.628457443803));
#253328=CARTESIAN_POINT('Ctrl Pts',(-1.87762570123898,2.61928221165763,
15.6284651907815));
#253329=CARTESIAN_POINT('Ctrl Pts',(-1.87782962599359,2.61913601669723,
15.6284806742579));
#253330=CARTESIAN_POINT('Ctrl Pts',(-1.87793152035875,2.61906295897272,
15.6284884107563));
#253331=CARTESIAN_POINT('Ctrl Pts',(-1.87813520429762,2.61891690066106,
15.6285038756457));
#253332=CARTESIAN_POINT('Ctrl Pts',(-1.87823699387892,2.61884390008547,
15.6285116040374));
#253333=CARTESIAN_POINT('Ctrl Pts',(-1.88916629700184,2.6110047515994,15.6293414052162));
#253334=CARTESIAN_POINT('Ctrl Pts',(-1.89994576314816,2.6031713777499,15.6301589802004));
#253335=CARTESIAN_POINT('Ctrl Pts',(-1.92330019800536,2.58597750192634,
15.6319291915597));
#253336=CARTESIAN_POINT('Ctrl Pts',(-1.93585614447994,2.57659160546083,
15.6328801878));
#253337=CARTESIAN_POINT('Ctrl Pts',(-1.97029114301436,2.55045673400706,
15.6354878577077));
#253338=CARTESIAN_POINT('Ctrl Pts',(-1.992025123539,2.53351786041642,15.6371331960816));
#253339=CARTESIAN_POINT('Ctrl Pts',(-2.06270326845192,2.47696134302616,
15.6424918463238));
#253340=CARTESIAN_POINT('Ctrl Pts',(-2.11070594480127,2.43618627518454,
15.6461443635419));
#253341=CARTESIAN_POINT('Ctrl Pts',(-2.26113225222904,2.30062291250157,
15.6577446723567));
#253342=CARTESIAN_POINT('Ctrl Pts',(-2.35860798800838,2.20058094534829,
15.6655086373386));
#253343=CARTESIAN_POINT('Ctrl Pts',(-2.58189276261271,1.93947710011177,
15.6847610400964));
#253344=CARTESIAN_POINT('Ctrl Pts',(-2.69945017098937,1.77220108057633,
15.6962931780687));
#253345=CARTESIAN_POINT('Ctrl Pts',(-2.81790597933807,1.56421679439629,
15.7105634891989));
#253346=CARTESIAN_POINT('Ctrl Pts',(-2.83490093590786,1.53320084301653,
15.7126887227133));
#253347=CARTESIAN_POINT('Ctrl Pts',(-2.86105406119845,1.4835491188399,15.7160896322425));
#253348=CARTESIAN_POINT('Ctrl Pts',(-2.87054876905024,1.46509319244849,
15.7173534962801));
#253349=CARTESIAN_POINT('Ctrl Pts',(-2.88799489422117,1.43036050243356,
15.7197320938652));
#253350=CARTESIAN_POINT('Ctrl Pts',(-2.89598866102847,1.4141058411986,15.7208453003968));
#253351=CARTESIAN_POINT('Ctrl Pts',(-2.91361436388942,1.37748911567723,
15.7233535106355));
#253352=CARTESIAN_POINT('Ctrl Pts',(-2.92317062803156,1.35709187742357,
15.7247510474688));
#253353=CARTESIAN_POINT('Ctrl Pts',(-2.95116611824056,1.29566936795446,
15.7289613414877));
#253354=CARTESIAN_POINT('Ctrl Pts',(-2.96896050363633,1.25435791219073,
15.7317956530741));
#253355=CARTESIAN_POINT('Ctrl Pts',(-3.05056776920302,1.05342446855012,
15.7455996201529));
#253356=CARTESIAN_POINT('Ctrl Pts',(-3.10239654097435,0.889262344481743,
15.7569536220342));
#253357=CARTESIAN_POINT('Ctrl Pts',(-3.16408158506127,0.620831967904263,
15.7754694559997));
#253358=CARTESIAN_POINT('Ctrl Pts',(-3.18239798081183,0.518832589372446,
15.7824886074584));
#253359=CARTESIAN_POINT('Ctrl Pts',(-3.213736755432,0.278159051720678,15.7988503639988));
#253360=CARTESIAN_POINT('Ctrl Pts',(-3.22275000000011,0.139157621639885,
15.8081488051135));
#253361=CARTESIAN_POINT('Ctrl Pts',(-3.22275,-2.40758801783869E-12,15.8170600220821));
#253362=CARTESIAN_POINT('Origin',(0.,0.,-2.31077344927308));
#253363=CARTESIAN_POINT('',(-3.22275,-2.95105326763967E-13,17.3136802073254));
#253364=CARTESIAN_POINT('',(-3.22275,-9.68142638581001E-11,17.0635026513638));
#253365=CARTESIAN_POINT('',(-3.22275,-3.50678552687464E-13,-2.31077344927308));
#253366=CARTESIAN_POINT('Ctrl Pts',(-3.22275,-2.95105326763967E-13,17.3136802073254));
#253367=CARTESIAN_POINT('Ctrl Pts',(-3.22275,0.0221340923676759,17.3123467173463));
#253368=CARTESIAN_POINT('Ctrl Pts',(-3.22252197224614,0.0442671683107299,
17.3110064138654));
#253369=CARTESIAN_POINT('Ctrl Pts',(-3.22172476662145,0.0829541292113185,
17.3086508721571));
#253370=CARTESIAN_POINT('Ctrl Pts',(-3.22125592312253,0.0995094026487866,
17.30763877143));
#253371=CARTESIAN_POINT('Ctrl Pts',(-3.22000437711349,0.134239718201456,
17.3055066188397));
#253372=CARTESIAN_POINT('Ctrl Pts',(-3.21919534889757,0.15241317123072,
17.3043857851612));
#253373=CARTESIAN_POINT('Ctrl Pts',(-3.21688684133087,0.195966805603421,
17.3016869121675));
#253374=CARTESIAN_POINT('Ctrl Pts',(-3.21524081658911,0.221337685758173,
17.3001043773044));
#253375=CARTESIAN_POINT('Ctrl Pts',(-3.20842005984311,0.310183886830126,
17.2945247943625));
#253376=CARTESIAN_POINT('Ctrl Pts',(-3.20166449506103,0.373519576776114,
17.290479341787));
#253377=CARTESIAN_POINT('Ctrl Pts',(-3.18023109811769,0.530267269741759,
17.2802930108338));
#253378=CARTESIAN_POINT('Ctrl Pts',(-3.16331116959225,0.623308208622568,
17.2740903019683));
#253379=CARTESIAN_POINT('Ctrl Pts',(-3.09664976237345,0.916085756411005,
17.2541179036814));
#253380=CARTESIAN_POINT('Ctrl Pts',(-3.03186698205914,1.1118583672275,17.2400466897267));
#253381=CARTESIAN_POINT('Ctrl Pts',(-2.94713543724367,1.30404322042824,
17.2260342330169));
#253382=CARTESIAN_POINT('Ctrl Pts',(-2.94539505726775,1.30796940447217,
17.2257478988381));
#253383=CARTESIAN_POINT('Ctrl Pts',(-2.90711857334532,1.39385485934604,
17.219482928634));
#253384=CARTESIAN_POINT('Ctrl Pts',(-2.86717950771309,1.4742640048828,17.2135885508711));
#253385=CARTESIAN_POINT('Ctrl Pts',(-2.814299379662,1.57042549547647,17.2065902847308));
#253386=CARTESIAN_POINT('Ctrl Pts',(-2.80450308663605,1.58785380897961,
17.2053240717278));
#253387=CARTESIAN_POINT('Ctrl Pts',(-2.78883314886903,1.61513427838849,
17.2033468211409));
#253388=CARTESIAN_POINT('Ctrl Pts',(-2.78306819337775,1.62504784850364,
17.2026292975505));
#253389=CARTESIAN_POINT('Ctrl Pts',(-2.77267824925687,1.64269720661336,
17.2013539539672));
#253390=CARTESIAN_POINT('Ctrl Pts',(-2.76807370477194,1.65044441099464,
17.2007948896313));
#253391=CARTESIAN_POINT('Ctrl Pts',(-2.75682986245909,1.66918289875122,
17.1994443433879));
#253392=CARTESIAN_POINT('Ctrl Pts',(-2.75015730008055,1.68015394466326,
17.1986550094659));
#253393=CARTESIAN_POINT('Ctrl Pts',(-2.72908204504571,1.71434398155703,
17.1961985407646));
#253394=CARTESIAN_POINT('Ctrl Pts',(-2.71444913373042,1.73742053261069,
17.1945454897634));
#253395=CARTESIAN_POINT('Ctrl Pts',(-2.63696352269972,1.85624868133193,
17.1860441248338));
#253396=CARTESIAN_POINT('Ctrl Pts',(-2.56932665281482,1.94879487588652,
17.179458149908));
#253397=CARTESIAN_POINT('Ctrl Pts',(-2.3679877295483,2.195523934105,17.1614261217301));
#253398=CARTESIAN_POINT('Ctrl Pts',(-2.22437756788122,2.34090521190639,
17.1502111179564));
#253399=CARTESIAN_POINT('Ctrl Pts',(-1.98067281953882,2.5448015241628,17.1320534087972));
#253400=CARTESIAN_POINT('Ctrl Pts',(-1.88955072030984,2.61317313269437,
17.1254314875921));
#253401=CARTESIAN_POINT('Ctrl Pts',(-1.76841860602868,2.69440869501883,
17.1167088847139));
#253402=CARTESIAN_POINT('Ctrl Pts',(-1.7415650592748,2.71184321375901,17.1147802616634));
#253403=CARTESIAN_POINT('Ctrl Pts',(-1.69790169758138,2.73927538699542,
17.1116501121912));
#253404=CARTESIAN_POINT('Ctrl Pts',(-1.68125245274873,2.74952541077057,
17.1104578836641));
#253405=CARTESIAN_POINT('Ctrl Pts',(-1.64923023598831,2.76884012785152,
17.1081668247405));
#253406=CARTESIAN_POINT('Ctrl Pts',(-1.63387317535597,2.77792988600331,
17.1070689592419));
#253407=CARTESIAN_POINT('Ctrl Pts',(-1.59831272634414,2.79858103518565,
17.1045283651802));
#253408=CARTESIAN_POINT('Ctrl Pts',(-1.57805817918991,2.81005190690838,
17.1030824623203));
#253409=CARTESIAN_POINT('Ctrl Pts',(-1.51336376426435,2.84577062572734,
17.0984668925374));
#253410=CARTESIAN_POINT('Ctrl Pts',(-1.46847772326269,2.86919031288539,
17.0952684593487));
#253411=CARTESIAN_POINT('Ctrl Pts',(-1.24775096912036,2.9778200847304,17.0795514973403));
#253412=CARTESIAN_POINT('Ctrl Pts',(-1.06498364484869,3.04796391723238,
17.0665362728454));
#253413=CARTESIAN_POINT('Ctrl Pts',(-0.680188839499378,3.15678653021748,
17.0395428911061));
#253414=CARTESIAN_POINT('Ctrl Pts',(-0.478493101586672,3.19358961664113,
17.0256121868813));
#253415=CARTESIAN_POINT('Ctrl Pts',(-0.249236803563963,3.21319926940639,
17.0108140400078));
#253416=CARTESIAN_POINT('Ctrl Pts',(-0.223789751114986,3.2150718137908,
17.0091861445789));
#253417=CARTESIAN_POINT('Ctrl Pts',(-0.185647075553658,3.21742350292292,
17.0067706672793));
#253418=CARTESIAN_POINT('Ctrl Pts',(-0.172967125082773,3.21813008125857,
17.0059717417844));
#253419=CARTESIAN_POINT('Ctrl Pts',(-0.150097049295865,3.21926893113066,
17.0045384888951));
#253420=CARTESIAN_POINT('Ctrl Pts',(-0.13990843234287,3.21972781700876,
17.0039027376001));
#253421=CARTESIAN_POINT('Ctrl Pts',(-0.118995964128202,3.22057023864025,
17.0026037319432));
#253422=CARTESIAN_POINT('Ctrl Pts',(-0.108272104127282,3.22094859641696,
17.0019407630907));
#253423=CARTESIAN_POINT('Ctrl Pts',(-0.0803962523175764,3.22179273099283,
17.0002251719284));
#253424=CARTESIAN_POINT('Ctrl Pts',(-0.0632418268091256,3.22217511313888,
16.9991770382943));
#253425=CARTESIAN_POINT('Ctrl Pts',(0.0127754717451602,3.22326225782861,
16.9945629278761));
#253426=CARTESIAN_POINT('Ctrl Pts',(0.0716517921642314,3.22249123567755,
16.9910703011667));
#253427=CARTESIAN_POINT('Ctrl Pts',(0.242516430491498,3.21556785150419,
16.9810857233447));
#253428=CARTESIAN_POINT('Ctrl Pts',(0.354249598976605,3.20518352056544,
16.974744089558));
#253429=CARTESIAN_POINT('Ctrl Pts',(0.72462013875817,3.15115271151844,16.9537280380013));
#253430=CARTESIAN_POINT('Ctrl Pts',(0.978406290591503,3.08180897347347,
16.9392458621548));
#253431=CARTESIAN_POINT('Ctrl Pts',(1.2555277019743,2.96835993899214,16.9214720426081));
#253432=CARTESIAN_POINT('Ctrl Pts',(1.28981860436541,2.95362122417121,16.9192384434453));
#253433=CARTESIAN_POINT('Ctrl Pts',(1.34472817760542,2.92888175511218,16.9156020385143));
#253434=CARTESIAN_POINT('Ctrl Pts',(1.36551022615871,2.91925058668897,16.9142116914732));
#253435=CARTESIAN_POINT('Ctrl Pts',(1.40225588798655,2.90174306130282,16.9117274353743));
#253436=CARTESIAN_POINT('Ctrl Pts',(1.41826037357369,2.89395436419616,16.9106365718158));
#253437=CARTESIAN_POINT('Ctrl Pts',(1.45187855244221,2.87724798646731,16.9083260286129));
#253438=CARTESIAN_POINT('Ctrl Pts',(1.46947640981608,2.86830025627436,16.9071053388752));
#253439=CARTESIAN_POINT('Ctrl Pts',(1.51617747987021,2.84401225295308,16.903835312422));
#253440=CARTESIAN_POINT('Ctrl Pts',(1.54512927587043,2.82838739185515,16.9017760878545));
#253441=CARTESIAN_POINT('Ctrl Pts',(1.69758866867872,2.74306784674055,16.8907574276256));
#253442=CARTESIAN_POINT('Ctrl Pts',(1.81661903684733,2.66572963972247,16.8815276053146));
#253443=CARTESIAN_POINT('Ctrl Pts',(2.09487014210991,2.45762921491592,16.8584203764023));
#253444=CARTESIAN_POINT('Ctrl Pts',(2.24740047017898,2.31896676001625,16.8443551525489));
#253445=CARTESIAN_POINT('Ctrl Pts',(2.44907765487224,2.09690961777653,16.8243384914274));
#253446=CARTESIAN_POINT('Ctrl Pts',(2.50939325827023,2.02434188957196,16.8181336074175));
#253447=CARTESIAN_POINT('Ctrl Pts',(2.57867747593482,1.93311902359514,16.8108265978599));
#253448=CARTESIAN_POINT('Ctrl Pts',(2.59075974268731,1.91689610776433,16.8095452157002));
#253449=CARTESIAN_POINT('Ctrl Pts',(2.60948318804215,1.89125561195732,16.8075495492701));
#253450=CARTESIAN_POINT('Ctrl Pts',(2.61622773908035,1.8819146434649,16.806828587524));
#253451=CARTESIAN_POINT('Ctrl Pts',(2.62815337945841,1.86521002424517,16.8055503464257));
#253452=CARTESIAN_POINT('Ctrl Pts',(2.63335374223698,1.85786078360184,16.8049917871335));
#253453=CARTESIAN_POINT('Ctrl Pts',(2.64585063360493,1.84004207159366,16.8036465732125));
#253454=CARTESIAN_POINT('Ctrl Pts',(2.65311585941672,1.82955094211429,16.8028620191493));
#253455=CARTESIAN_POINT('Ctrl Pts',(2.67550204160882,1.79681106759752,16.8004358352164));
#253456=CARTESIAN_POINT('Ctrl Pts',(2.69040730192114,1.77441535253602,16.7988077975343));
#253457=CARTESIAN_POINT('Ctrl Pts',(2.7652757898506,1.65880994643778,16.790550097089));
#253458=CARTESIAN_POINT('Ctrl Pts',(2.82068795959516,1.56272991840634,16.7841663816454));
#253459=CARTESIAN_POINT('Ctrl Pts',(2.96196601678823,1.28566585130246,16.7665335636342));
#253460=CARTESIAN_POINT('Ctrl Pts',(3.03607966109708,1.09927335303053,16.7555234523345));
#253461=CARTESIAN_POINT('Ctrl Pts',(3.12644747462702,0.791233951948551,
16.7372244233817));
#253462=CARTESIAN_POINT('Ctrl Pts',(3.15391607491818,0.67344922870197,16.7302110681384));
#253463=CARTESIAN_POINT('Ctrl Pts',(3.18030848583938,0.522318535957917,
16.7210403679275));
#253464=CARTESIAN_POINT('Ctrl Pts',(3.18542539084461,0.490146591868484,
16.7190787806957));
#253465=CARTESIAN_POINT('Ctrl Pts',(3.19284872609865,0.438430806233579,
16.7159081073655));
#253466=CARTESIAN_POINT('Ctrl Pts',(3.19546544593634,0.418933308364208,
16.7147087691225));
#253467=CARTESIAN_POINT('Ctrl Pts',(3.20011134368749,0.38173592766078,16.712412616033));
#253468=CARTESIAN_POINT('Ctrl Pts',(3.20217258339169,0.364040734737923,
16.7113168504109));
#253469=CARTESIAN_POINT('Ctrl Pts',(3.20656255481724,0.323426681658127,
16.7087935246698));
#253470=CARTESIAN_POINT('Ctrl Pts',(3.20879244354722,0.30049833065699,16.7073629346496));
#253471=CARTESIAN_POINT('Ctrl Pts',(3.2150212509779,0.22844135100925,16.7028470770423));
#253472=CARTESIAN_POINT('Ctrl Pts',(3.21813885512107,0.179245578684574,
16.6997347738277));
#253473=CARTESIAN_POINT('Ctrl Pts',(3.2228147469549,0.0634225309152199,
16.6923354388443));
#253474=CARTESIAN_POINT('Ctrl Pts',(3.22343698247599,-0.00321804575677445,
16.68802202482));
#253475=CARTESIAN_POINT('Ctrl Pts',(3.21774612871357,-0.265810141087278,
16.6708117038668));
#253476=CARTESIAN_POINT('Ctrl Pts',(3.19562617229909,-0.46098259338203,
16.6575181695119));
#253477=CARTESIAN_POINT('Ctrl Pts',(3.12565512404511,-0.799194405453589,
16.6342131926274));
#253478=CARTESIAN_POINT('Ctrl Pts',(3.08525434098856,-0.94321086565765,
16.6242113304533));
#253479=CARTESIAN_POINT('Ctrl Pts',(3.0277367250502,-1.10426201086679,16.6132848444565));
#253480=CARTESIAN_POINT('Ctrl Pts',(3.02026621107624,-1.12453383100118,
16.6119145045287));
#253481=CARTESIAN_POINT('Ctrl Pts',(3.00839042980441,-1.1557873998848,16.60981124224));
#253482=CARTESIAN_POINT('Ctrl Pts',(3.00412774671895,-1.16682217308307,
16.6090704714741));
#253483=CARTESIAN_POINT('Ctrl Pts',(2.99616311240045,-1.18710716747405,
16.6077124425826));
#253484=CARTESIAN_POINT('Ctrl Pts',(2.99247899861826,-1.19636376997639,
16.6070942060089));
#253485=CARTESIAN_POINT('Ctrl Pts',(2.98393121763331,-1.21755414941524,
16.6056821758134));
#253486=CARTESIAN_POINT('Ctrl Pts',(2.9790388460684,-1.22947597983675,16.604890093675));
#253487=CARTESIAN_POINT('Ctrl Pts',(2.96345675790082,-1.26680760493885,
16.6024161756487));
#253488=CARTESIAN_POINT('Ctrl Pts',(2.9525121542454,-1.29211050486844,16.6007487099799));
#253489=CARTESIAN_POINT('Ctrl Pts',(2.89354045319857,-1.42378438141158,
16.5921047489965));
#253490=CARTESIAN_POINT('Ctrl Pts',(2.84008144207243,-1.52763905857051,
16.5854004228981));
#253491=CARTESIAN_POINT('Ctrl Pts',(2.67694755225337,-1.80625561236203,
16.5671318092718));
#253492=CARTESIAN_POINT('Ctrl Pts',(2.55597111123807,-1.97373258313,16.5557937671983));
#253493=CARTESIAN_POINT('Ctrl Pts',(2.34742527470843,-2.210820968182,16.5377223823779));
#253494=CARTESIAN_POINT('Ctrl Pts',(2.27087699831267,-2.28937741023895,
16.5313377541164));
#253495=CARTESIAN_POINT('Ctrl Pts',(2.16720384516061,-2.38544589102352,
16.5228826836516));
#253496=CARTESIAN_POINT('Ctrl Pts',(2.14361043998848,-2.40666964488602,
16.5209706780231));
#253497=CARTESIAN_POINT('Ctrl Pts',(2.10502660068808,-2.44036072426009,
16.5178609328343));
#253498=CARTESIAN_POINT('Ctrl Pts',(2.09022938269425,-2.45304679041607,
16.5166722672198));
#253499=CARTESIAN_POINT('Ctrl Pts',(2.06165188942269,-2.47710075296049,
16.5143836203004));
#253500=CARTESIAN_POINT('Ctrl Pts',(2.04789034910675,-2.4884898535557,16.5132845605839));
#253501=CARTESIAN_POINT('Ctrl Pts',(2.01588003747714,-2.51453635297142,
16.5107346518562));
#253502=CARTESIAN_POINT('Ctrl Pts',(1.99756502286316,-2.52911038298497,
16.5092805512584));
#253503=CARTESIAN_POINT('Ctrl Pts',(1.93856974806943,-2.57501481244328,
16.504611085909));
#253504=CARTESIAN_POINT('Ctrl Pts',(1.89730045811374,-2.60557180716549,
16.5013659976067));
#253505=CARTESIAN_POINT('Ctrl Pts',(1.73574744841238,-2.71931678159805,
16.4887373880845));
#253506=CARTESIAN_POINT('Ctrl Pts',(1.61059722078433,-2.79525853746499,
16.4790985113957));
#253507=CARTESIAN_POINT('Ctrl Pts',(1.25750737924223,-2.9779119387294,16.4524457426059));
#253508=CARTESIAN_POINT('Ctrl Pts',(1.02153384805029,-3.06688119368647,
16.4351499102641));
#253509=CARTESIAN_POINT('Ctrl Pts',(0.75205986533862,-3.13388209683342,
16.4172764779589));
#253510=CARTESIAN_POINT('Ctrl Pts',(0.726426171640689,-3.13992295367267,
16.4155951667989));
#253511=CARTESIAN_POINT('Ctrl Pts',(0.688131035205691,-3.1484535248025,
16.413114331227));
#253512=CARTESIAN_POINT('Ctrl Pts',(0.675524691433461,-3.15118236916276,
16.4123026352241));
#253513=CARTESIAN_POINT('Ctrl Pts',(0.653773988568329,-3.15575413129464,
16.4109111015018));
#253514=CARTESIAN_POINT('Ctrl Pts',(0.644637493471649,-3.1576331440656,
16.410329292817));
#253515=CARTESIAN_POINT('Ctrl Pts',(0.625270809779749,-3.16152853759815,
16.4091019555778));
#253516=CARTESIAN_POINT('Ctrl Pts',(0.615038737212195,-3.16353499063816,
16.4084570141463));
#253517=CARTESIAN_POINT('Ctrl Pts',(0.589321173864843,-3.16844857296294,
16.4068443813674));
#253518=CARTESIAN_POINT('Ctrl Pts',(0.573823539471145,-3.17129190932853,
16.4058802064245));
#253519=CARTESIAN_POINT('Ctrl Pts',(0.512749774940117,-3.18203468691038,
16.4021082538866));
#253520=CARTESIAN_POINT('Ctrl Pts',(0.467024373763913,-3.18906660359083,
16.399344807801));
#253521=CARTESIAN_POINT('Ctrl Pts',(0.344584765653447,-3.20520587356563,
16.3920686167063));
#253522=CARTESIAN_POINT('Ctrl Pts',(0.267665652606262,-3.21254414897306,
16.3876258948032));
#253523=CARTESIAN_POINT('Ctrl Pts',(-0.0394683104706741,-3.23073601011831,
16.370143786787));
#253524=CARTESIAN_POINT('Ctrl Pts',(-0.270284306237842,-3.21965260845996,
16.3575299719374));
#253525=CARTESIAN_POINT('Ctrl Pts',(-0.597666587090349,-3.16845371827434,
16.3384995093227));
#253526=CARTESIAN_POINT('Ctrl Pts',(-0.696588235332892,-3.14818460744293,
16.3326035463904));
#253527=CARTESIAN_POINT('Ctrl Pts',(-0.824311183577491,-3.11569925318654,
16.3247137261901));
#253528=CARTESIAN_POINT('Ctrl Pts',(-0.854120780753608,-3.10765962685984,
16.3228524222783));
#253529=CARTESIAN_POINT('Ctrl Pts',(-0.902375066969929,-3.09389875584659,
16.319804923058));
#253530=CARTESIAN_POINT('Ctrl Pts',(-0.920892344947074,-3.08843771780778,
16.31862713244));
#253531=CARTESIAN_POINT('Ctrl Pts',(-0.956504638005302,-3.07758634363401,
16.3163454087994));
#253532=CARTESIAN_POINT('Ctrl Pts',(-0.973605980380738,-3.07221910018391,
16.3152422621458));
#253533=CARTESIAN_POINT('Ctrl Pts',(-1.01333562459316,-3.05938494558483,
16.3126616624615));
#253534=CARTESIAN_POINT('Ctrl Pts',(-1.03592742299457,-3.05180924355685,
16.3111807028089));
#253535=CARTESIAN_POINT('Ctrl Pts',(-1.1092145816413,-3.02632634819424,
16.3063312626484));
#253536=CARTESIAN_POINT('Ctrl Pts',(-1.15954407470954,-3.00740172582723,
16.3029297414502));
#253537=CARTESIAN_POINT('Ctrl Pts',(-1.37334295423957,-2.92084559793913,
16.2881646956274));
#253538=CARTESIAN_POINT('Ctrl Pts',(-1.5315456011658,-2.84108473286912,
16.2764119305378));
#253539=CARTESIAN_POINT('Ctrl Pts',(-1.87041256869448,-2.63368022947694,
16.24963057482));
#253540=CARTESIAN_POINT('Ctrl Pts',(-2.04614434337394,-2.49960409013341,
16.2345667581741));
#253541=CARTESIAN_POINT('Ctrl Pts',(-2.22645035693762,-2.33018496176872,
16.2186749359695));
#253542=CARTESIAN_POINT('Ctrl Pts',(-2.24584962092683,-2.31149361609812,
16.216959430421));
#253543=CARTESIAN_POINT('Ctrl Pts',(-2.274095498464,-2.28358714326564,16.214456160969));
#253544=CARTESIAN_POINT('Ctrl Pts',(-2.28312481337023,-2.27455966649519,
16.2136551057796));
#253545=CARTESIAN_POINT('Ctrl Pts',(-2.29909825237014,-2.25839852230205,
16.212236885685));
#253546=CARTESIAN_POINT('Ctrl Pts',(-2.30606323789365,-2.25128607926038,
16.2116181380409));
#253547=CARTESIAN_POINT('Ctrl Pts',(-2.32129584480191,-2.235586108604,16.2102641719657));
#253548=CARTESIAN_POINT('Ctrl Pts',(-2.32954886105725,-2.22698490396622,
16.2095300525521));
#253549=CARTESIAN_POINT('Ctrl Pts',(-2.35232256966274,-2.20298525546188,
16.2075021070763));
#253550=CARTESIAN_POINT('Ctrl Pts',(-2.3667398666266,-2.18748896332091,
16.2062157823282));
#253551=CARTESIAN_POINT('Ctrl Pts',(-2.47734929976644,-2.06622767400258,
16.1963169852764));
#253552=CARTESIAN_POINT('Ctrl Pts',(-2.56657165419683,-1.95429681063372,
16.1881495374682));
#253553=CARTESIAN_POINT('Ctrl Pts',(-2.73615200715337,-1.70981634247521,
16.1713840028849));
#253554=CARTESIAN_POINT('Ctrl Pts',(-2.81498256581248,-1.57666516886901,
16.1628216381901));
#253555=CARTESIAN_POINT('Ctrl Pts',(-2.94660823852137,-1.31275385016655,
16.1461114078824));
#253556=CARTESIAN_POINT('Ctrl Pts',(-3.0009795661544,-1.18318971804714,
16.1380162340517));
#253557=CARTESIAN_POINT('Ctrl Pts',(-3.05772614337729,-1.01861008598675,
16.1276203509488));
#253558=CARTESIAN_POINT('Ctrl Pts',(-3.06822107645807,-0.986546994701005,
16.1255904250421));
#253559=CARTESIAN_POINT('Ctrl Pts',(-3.08410983781181,-0.935297259735878,
16.1223357334479));
#253560=CARTESIAN_POINT('Ctrl Pts',(-3.08983254843574,-0.916214631412177,
16.1211216765873));
#253561=CARTESIAN_POINT('Ctrl Pts',(-3.10032239091618,-0.880019411052094,
16.1188142289955));
#253562=CARTESIAN_POINT('Ctrl Pts',(-3.10512569364858,-0.862918013593345,
16.1177220571399));
#253563=CARTESIAN_POINT('Ctrl Pts',(-3.11571471317966,-0.823983923748545,
16.1152307279973));
#253564=CARTESIAN_POINT('Ctrl Pts',(-3.12141273010731,-0.802128547994979,
16.1138288097059));
#253565=CARTESIAN_POINT('Ctrl Pts',(-3.13280450001761,-0.756473595440243,
16.1108925583858));
#253566=CARTESIAN_POINT('Ctrl Pts',(-3.13845782726533,-0.73266551019231,
16.1093570354481));
#253567=CARTESIAN_POINT('Ctrl Pts',(-3.15804586205618,-0.645783464476143,
16.1037368946275));
#253568=CARTESIAN_POINT('Ctrl Pts',(-3.17035384394086,-0.58236201985508,
16.099602235878));
#253569=CARTESIAN_POINT('Ctrl Pts',(-3.20870733247854,-0.347134940052192,
16.084146813724));
#253570=CARTESIAN_POINT('Ctrl Pts',(-3.2227500000076,-0.173697287956936,
16.0724966069576));
#253571=CARTESIAN_POINT('Ctrl Pts',(-3.22275,1.40950411064988E-10,16.0607604048379));
#253572=CARTESIAN_POINT('',(-3.22274995225749,-0.000554729076348744,15.8170955430526));
#253573=CARTESIAN_POINT('Ctrl Pts',(-3.22275,-2.40695369623669E-12,15.8170600220821));
#253574=CARTESIAN_POINT('Ctrl Pts',(-3.22275,-0.000184909417959676,15.8170718631003));
#253575=CARTESIAN_POINT('Ctrl Pts',(-3.22274998408588,-0.000369819109989661,
15.817083703424));
#253576=CARTESIAN_POINT('Ctrl Pts',(-3.22274995225749,-0.000554729076422944,
15.8170955430526));
#253577=CARTESIAN_POINT('Ctrl Pts',(-3.22274995179883,-0.000557387331382724,
15.8170957132584));
#253578=CARTESIAN_POINT('Ctrl Pts',(-3.22274622160231,-0.0221249580166652,
15.8184766657508));
#253579=CARTESIAN_POINT('Ctrl Pts',(-3.22252598667833,-0.0436927045790141,
15.8198479352303));
#253580=CARTESIAN_POINT('Ctrl Pts',(-3.22187697376683,-0.075737791702557,
15.8218693625049));
#253581=CARTESIAN_POINT('Ctrl Pts',(-3.22161357567128,-0.0862173026417503,
15.8225278756371));
#253582=CARTESIAN_POINT('Ctrl Pts',(-3.22101093159705,-0.106293693097024,
15.8237843297505));
#253583=CARTESIAN_POINT('Ctrl Pts',(-3.22067991482886,-0.115890747819191,
15.8243827088868));
#253584=CARTESIAN_POINT('Ctrl Pts',(-3.21987769869423,-0.136477688288322,
15.8256613105752));
#253585=CARTESIAN_POINT('Ctrl Pts',(-3.21939312303517,-0.147466883328992,
15.8263407862734));
#253586=CARTESIAN_POINT('Ctrl Pts',(-3.21798302430099,-0.176111864232991,
15.8281045242701));
#253587=CARTESIAN_POINT('Ctrl Pts',(-3.2169684492768,-0.193763159298838,
15.8291840051577));
#253588=CARTESIAN_POINT('Ctrl Pts',(-3.21213045874513,-0.267356513596312,
15.8336573008867));
#253589=CARTESIAN_POINT('Ctrl Pts',(-3.2069924509369,-0.323205552586246,
15.8369860387962));
#253590=CARTESIAN_POINT('Ctrl Pts',(-3.17713258251152,-0.575421495207651,
15.8518325092794));
#253591=CARTESIAN_POINT('Ctrl Pts',(-3.13581152067092,-0.769402875317582,
15.8627585826249));
#253592=CARTESIAN_POINT('Ctrl Pts',(-3.02581556858593,-1.12255294862985,
15.8835199118992));
#253593=CARTESIAN_POINT('Ctrl Pts',(-2.96162936142449,-1.28235233319276,
15.8932765193052));
#253594=CARTESIAN_POINT('Ctrl Pts',(-2.86496036934638,-1.47653082854844,
15.9061192481573));
#253595=CARTESIAN_POINT('Ctrl Pts',(-2.84407206164505,-1.51637561926554,
15.908808834336));
#253596=CARTESIAN_POINT('Ctrl Pts',(-2.81148298794204,-1.57549623809707,
15.9128886266384));
#253597=CARTESIAN_POINT('Ctrl Pts',(-2.80040229238955,-1.59510875775955,
15.9142570789168));
#253598=CARTESIAN_POINT('Ctrl Pts',(-2.78012518211908,-1.63013608690666,
15.9167290501684));
#253599=CARTESIAN_POINT('Ctrl Pts',(-2.77100379326756,-1.6455934028116,
15.9178298513538));
#253600=CARTESIAN_POINT('Ctrl Pts',(-2.75108842276154,-1.67870732844369,
15.9202099781359));
#253601=CARTESIAN_POINT('Ctrl Pts',(-2.74025257742111,-1.69633769771502,
15.921490787352));
#253602=CARTESIAN_POINT('Ctrl Pts',(-2.71058483821589,-1.74358222885284,
15.9249604841978));
#253603=CARTESIAN_POINT('Ctrl Pts',(-2.69143819782519,-1.77299448008669,
15.9271608109834));
#253604=CARTESIAN_POINT('Ctrl Pts',(-2.57221442698824,-1.94975835636564,
15.9406361298049));
#253605=CARTESIAN_POINT('Ctrl Pts',(-2.46055773983435,-2.08889513110084,
15.9523472752103));
#253606=CARTESIAN_POINT('Ctrl Pts',(-2.25174993994693,-2.308991860177,15.9727083442235));
#253607=CARTESIAN_POINT('Ctrl Pts',(-2.16027298165056,-2.39479456253173,
15.9812133661752));
#253608=CARTESIAN_POINT('Ctrl Pts',(-1.96312563952537,-2.55920292059544,
15.9984900944032));
#253609=CARTESIAN_POINT('Ctrl Pts',(-1.85715294909779,-2.63711433568977,
16.0072386647248));
#253610=CARTESIAN_POINT('Ctrl Pts',(-1.72862252117434,-2.72000825678943,
16.0170057584367));
#253611=CARTESIAN_POINT('Ctrl Pts',(-1.71041926112583,-2.7314916705471,
16.0183702550734));
#253612=CARTESIAN_POINT('Ctrl Pts',(-1.68202801344849,-2.74900698954575,
16.0204678640938));
#253613=CARTESIAN_POINT('Ctrl Pts',(-1.67191990156382,-2.75516633249483,
16.0212087458991));
#253614=CARTESIAN_POINT('Ctrl Pts',(-1.65301397657644,-2.76654423063013,
16.022583121127));
#253615=CARTESIAN_POINT('Ctrl Pts',(-1.64422522596628,-2.77177661370795,
16.0232174527754));
#253616=CARTESIAN_POINT('Ctrl Pts',(-1.62389076141627,-2.78375198492425,
16.0246747806862));
#253617=CARTESIAN_POINT('Ctrl Pts',(-1.61232783325735,-2.79046506718093,
16.0254958836393));
#253618=CARTESIAN_POINT('Ctrl Pts',(-1.5746363402173,-2.81203509192934,
16.0281489765303));
#253619=CARTESIAN_POINT('Ctrl Pts',(-1.54834082467919,-2.82659898074328,
16.0299635681521));
#253620=CARTESIAN_POINT('Ctrl Pts',(-1.38271429106032,-2.91532694106923,
16.0411919241792));
#253621=CARTESIAN_POINT('Ctrl Pts',(-1.23828017586229,-2.97954751102875,
16.0501093534808));
#253622=CARTESIAN_POINT('Ctrl Pts',(-0.962038282793848,-3.07879899258903,
16.0665765586549));
#253623=CARTESIAN_POINT('Ctrl Pts',(-0.83160184226044,-3.1165619399603,
16.0741261161211));
#253624=CARTESIAN_POINT('Ctrl Pts',(-0.613107506517491,-3.16512095736399,
16.08684228272));
#253625=CARTESIAN_POINT('Ctrl Pts',(-0.5262938833522,-3.18070820382678,
16.091910869633));
#253626=CARTESIAN_POINT('Ctrl Pts',(-0.378685421786308,-3.20100233218306,
16.1006438979073));
#253627=CARTESIAN_POINT('Ctrl Pts',(-0.318196972275388,-3.20757986127694,
16.1042544513831));
#253628=CARTESIAN_POINT('Ctrl Pts',(-0.232325759855905,-3.21446468807705,
16.1094422049998));
#253629=CARTESIAN_POINT('Ctrl Pts',(-0.207067804046164,-3.2161905040946,
16.1109756460109));
#253630=CARTESIAN_POINT('Ctrl Pts',(-0.163340418892367,-3.21866106363281,
16.1136445378053));
#253631=CARTESIAN_POINT('Ctrl Pts',(-0.144879848093298,-3.21954483466493,
16.1147756283059));
#253632=CARTESIAN_POINT('Ctrl Pts',(-0.109339430121923,-3.22093998814506,
16.1169619951952));
#253633=CARTESIAN_POINT('Ctrl Pts',(-0.0922610748377415,-3.22147441313818,
16.1180165169475));
#253634=CARTESIAN_POINT('Ctrl Pts',(-0.0472124967724841,-3.222525581534,
16.1208087410951));
#253635=CARTESIAN_POINT('Ctrl Pts',(-0.0192388792029165,-3.22281397702412,
16.1225534499698));
#253636=CARTESIAN_POINT('Ctrl Pts',(0.0823263794919396,-3.22253871489787,
16.128929040253));
#253637=CARTESIAN_POINT('Ctrl Pts',(0.155884887511749,-3.2198186154196,
16.1336253518705));
#253638=CARTESIAN_POINT('Ctrl Pts',(0.461355511051301,-3.19803080783324,
16.1534638085808));
#253639=CARTESIAN_POINT('Ctrl Pts',(0.690930735350458,-3.15639631513609,
16.1692481628474));
#253640=CARTESIAN_POINT('Ctrl Pts',(1.03979238434662,-3.05322140805999,
16.1937745719172));
#253641=CARTESIAN_POINT('Ctrl Pts',(1.16322163631314,-3.00836349501601,
16.202547860252));
#253642=CARTESIAN_POINT('Ctrl Pts',(1.31051402350762,-2.94440701197638,
16.212885232079));
#253643=CARTESIAN_POINT('Ctrl Pts',(1.33728616539138,-2.93234471181988,
16.2147583917237));
#253644=CARTESIAN_POINT('Ctrl Pts',(1.37602100144484,-2.91425170713505,
16.2174561922053));
#253645=CARTESIAN_POINT('Ctrl Pts',(1.38811606377214,-2.9085100338793,16.2182968122072));
#253646=CARTESIAN_POINT('Ctrl Pts',(1.40936819328606,-2.89825862074025,
16.2197702632288));
#253647=CARTESIAN_POINT('Ctrl Pts',(1.41854007594948,-2.89378053760286,
16.2204049558762));
#253648=CARTESIAN_POINT('Ctrl Pts',(1.43842646828937,-2.88395392666391,
16.2217783742875));
#253649=CARTESIAN_POINT('Ctrl Pts',(1.44913256573407,-2.87858919843438,
16.2225161018952));
#253650=CARTESIAN_POINT('Ctrl Pts',(1.47902961237556,-2.86339899119203,
16.2245722246131));
#253651=CARTESIAN_POINT('Ctrl Pts',(1.49815261827548,-2.85344023343766,
16.2258827367525));
#253652=CARTESIAN_POINT('Ctrl Pts',(1.62592385741443,-2.78526171305187,
16.2346172787183));
#253653=CARTESIAN_POINT('Ctrl Pts',(1.73126660821293,-2.72103542144094,
16.2417142090766));
#253654=CARTESIAN_POINT('Ctrl Pts',(2.05989203463373,-2.49384474386652,
16.2643414192517));
#253655=CARTESIAN_POINT('Ctrl Pts',(2.26595431378871,-2.30821730218388,
16.2794198053766));
#253656=CARTESIAN_POINT('Ctrl Pts',(2.4833673846921,-2.05483041340132,16.2990259904808));
#253657=CARTESIAN_POINT('Ctrl Pts',(2.51972794221395,-2.01007763326026,
16.3024524410071));
#253658=CARTESIAN_POINT('Ctrl Pts',(2.56998461622273,-1.94471379961092,
16.3074206487033));
#253659=CARTESIAN_POINT('Ctrl Pts',(2.58487432635543,-1.92487852985945,
16.3089236545582));
#253660=CARTESIAN_POINT('Ctrl Pts',(2.61040692230232,-1.89003483897039,
16.3115569687875));
#253661=CARTESIAN_POINT('Ctrl Pts',(2.62115310125099,-1.87510330126874,
16.3126832426938));
#253662=CARTESIAN_POINT('Ctrl Pts',(2.64170677548839,-1.84602254475498,
16.3148729948378));
#253663=CARTESIAN_POINT('Ctrl Pts',(2.65152990908911,-1.83188510732037,
16.3159358271638));
#253664=CARTESIAN_POINT('Ctrl Pts',(2.67741079878549,-1.79399305742347,
16.3187803634508));
#253665=CARTESIAN_POINT('Ctrl Pts',(2.69326531372663,-1.77010212724308,
16.3205695758416));
#253666=CARTESIAN_POINT('Ctrl Pts',(2.75131995214272,-1.68003453780286,
16.3273008251798));
#253667=CARTESIAN_POINT('Ctrl Pts',(2.79141412785753,-1.61253930783438,
16.3323181860534));
#253668=CARTESIAN_POINT('Ctrl Pts',(2.93824792845134,-1.34344168877698,
16.3522257070446));
#253669=CARTESIAN_POINT('Ctrl Pts',(3.02592023151001,-1.13221853590028,
16.3677075295291));
#253670=CARTESIAN_POINT('Ctrl Pts',(3.12729129717424,-0.789277731108036,
16.3918111988924));
#253671=CARTESIAN_POINT('Ctrl Pts',(3.15649968118027,-0.662892249386649,
16.4004726069453));
#253672=CARTESIAN_POINT('Ctrl Pts',(3.18286670129963,-0.506289980585192,
16.4106943510359));
#253673=CARTESIAN_POINT('Ctrl Pts',(3.18732295208164,-0.477433260996854,
16.4125567535897));
#253674=CARTESIAN_POINT('Ctrl Pts',(3.19324569101909,-0.43529066170121,
16.4152420619719));
#253675=CARTESIAN_POINT('Ctrl Pts',(3.19502255949809,-0.42205078166261,
16.4160807470759));
#253676=CARTESIAN_POINT('Ctrl Pts',(3.19801142459324,-0.398678577935066,
16.4175520825572));
#253677=CARTESIAN_POINT('Ctrl Pts',(3.19925769030617,-0.388551053522888,
16.4181865753791));
#253678=CARTESIAN_POINT('Ctrl Pts',(3.20186437669141,-0.366505064229631,
16.4195610396806));
#253679=CARTESIAN_POINT('Ctrl Pts',(3.20320637587783,-0.354584789629988,
16.4202999988224));
#253680=CARTESIAN_POINT('Ctrl Pts',(3.20678394364183,-0.321127868673782,
16.4223629335847));
#253681=CARTESIAN_POINT('Ctrl Pts',(3.20886912132477,-0.299575347016243,
16.4236789429605));
#253682=CARTESIAN_POINT('Ctrl Pts',(3.22168472647574,-0.151564111531097,
16.4326380981155));
#253683=CARTESIAN_POINT('Ctrl Pts',(3.22515540721181,-0.0245743919984683,
16.4399342120575));
#253684=CARTESIAN_POINT('Ctrl Pts',(3.21987394639421,0.141720761726979,
16.449347432257));
#253685=CARTESIAN_POINT('Ctrl Pts',(3.21789849625259,0.181114195381315,
16.4515667027689));
#253686=CARTESIAN_POINT('Ctrl Pts',(3.20642571309684,0.34843243615402,16.4609804148846));
#253687=CARTESIAN_POINT('Ctrl Pts',(3.19001859213704,0.475764498709609,
16.4681185509057));
#253688=CARTESIAN_POINT('Ctrl Pts',(3.14829381116591,0.695286644568743,
16.4807748549173));
#253689=CARTESIAN_POINT('Ctrl Pts',(3.12638749826881,0.787957355092488,
16.4862284074992));
#253690=CARTESIAN_POINT('Ctrl Pts',(3.08288132279225,0.941322171998878,
16.4955538559582));
#253691=CARTESIAN_POINT('Ctrl Pts',(3.0635057862567,1.00258474115839,16.4993611325552));
#253692=CARTESIAN_POINT('Ctrl Pts',(3.03378703663959,1.08762204635964,16.5047825126736));
#253693=CARTESIAN_POINT('Ctrl Pts',(3.02496765374033,1.11191552480378,16.5063471625471));
#253694=CARTESIAN_POINT('Ctrl Pts',(3.00930936095517,1.15348157065268,16.509052873603));
#253695=CARTESIAN_POINT('Ctrl Pts',(3.00261145178311,1.17080613718983,16.510189235546));
#253696=CARTESIAN_POINT('Ctrl Pts',(2.98867094749735,1.20595760955327,16.5125129830378));
#253697=CARTESIAN_POINT('Ctrl Pts',(2.98141771564702,1.22377946047961,16.513700686603));
#253698=CARTESIAN_POINT('Ctrl Pts',(2.96274651106771,1.26850495315987,16.5167060002835));
#253699=CARTESIAN_POINT('Ctrl Pts',(2.9511215314979,1.29531977589778,16.518530502663));
#253700=CARTESIAN_POINT('Ctrl Pts',(2.90525031244094,1.39730502098797,16.5255589108867));
#253701=CARTESIAN_POINT('Ctrl Pts',(2.86848580199242,1.47130145085753,16.5308470023867));
#253702=CARTESIAN_POINT('Ctrl Pts',(2.72147463280352,1.74069087486416,16.5508167466326));
#253703=CARTESIAN_POINT('Ctrl Pts',(2.59377440525216,1.92580913902128,16.5660488785749));
#253704=CARTESIAN_POINT('Ctrl Pts',(2.36449895855361,2.19356116169624,16.5898036897366));
#253705=CARTESIAN_POINT('Ctrl Pts',(2.27533289806995,2.28592041707759,16.5983721715885));
#253706=CARTESIAN_POINT('Ctrl Pts',(2.15949814495306,2.39238994956994,16.6084977425058));
#253707=CARTESIAN_POINT('Ctrl Pts',(2.13783883425448,2.411764325689,16.6103511232412));
#253708=CARTESIAN_POINT('Ctrl Pts',(2.10586298439437,2.4395975932194,16.6130259460462));
#253709=CARTESIAN_POINT('Ctrl Pts',(2.09575194187463,2.4482890226771,16.6138630006887));
#253710=CARTESIAN_POINT('Ctrl Pts',(2.07780974626949,2.46351949288468,16.6153325561184));
#253711=CARTESIAN_POINT('Ctrl Pts',(2.07000111296112,2.470084418722,16.6159668831856));
#253712=CARTESIAN_POINT('Ctrl Pts',(2.05292954398928,2.48429912788716,16.6173422428042));
#253713=CARTESIAN_POINT('Ctrl Pts',(2.04365490896799,2.4919342874903,16.6180822509565));
#253714=CARTESIAN_POINT('Ctrl Pts',(2.0174836024499,2.51323490752009,16.6201509927765));
#253715=CARTESIAN_POINT('Ctrl Pts',(2.00049075089985,2.52678186628411,16.6214716889104));
#253716=CARTESIAN_POINT('Ctrl Pts',(1.88063844739336,2.62036290377296,16.6306406404235));
#253717=CARTESIAN_POINT('Ctrl Pts',(1.77313232798418,2.69427394813547,16.6381226741575));
#253718=CARTESIAN_POINT('Ctrl Pts',(1.63111676052175,2.77971716298425,16.647490780855));
#253719=CARTESIAN_POINT('Ctrl Pts',(1.60050100625079,2.79745705542498,16.649481414978));
#253720=CARTESIAN_POINT('Ctrl Pts',(1.45745246414847,2.87722743925628,16.6586754796325));
#253721=CARTESIAN_POINT('Ctrl Pts',(1.34166887955809,2.93300690710608,16.6658206704963));
#253722=CARTESIAN_POINT('Ctrl Pts',(1.13459312079449,3.01793295285181,16.6784962946494));
#253723=CARTESIAN_POINT('Ctrl Pts',(1.04475825284476,3.05019658122446,16.6839623205248));
#253724=CARTESIAN_POINT('Ctrl Pts',(0.892159887368074,3.09746821841046,
16.6933068648918));
#253725=CARTESIAN_POINT('Ctrl Pts',(0.830137409549292,3.11466365596257,
16.6971203977656));
#253726=CARTESIAN_POINT('Ctrl Pts',(0.742528122999598,3.13615024127863,
16.702549192892));
#253727=CARTESIAN_POINT('Ctrl Pts',(0.717338899430118,3.14200751011786,
16.7041148145031));
#253728=CARTESIAN_POINT('Ctrl Pts',(0.673938702284614,3.15155030094685,
16.7068216774083));
#253729=CARTESIAN_POINT('Ctrl Pts',(0.65576109741242,3.15538270807807,16.7079582088303));
#253730=CARTESIAN_POINT('Ctrl Pts',(0.618695246035927,3.16286322843693,
16.7102818298027));
#253731=CARTESIAN_POINT('Ctrl Pts',(0.599805463360756,3.16649980104512,
16.7114692331996));
#253732=CARTESIAN_POINT('Ctrl Pts',(0.552159498864665,3.1752307455466,16.7144728374886));
#253733=CARTESIAN_POINT('Ctrl Pts',(0.523364987499283,3.18010367758402,
16.7162959145612));
#253734=CARTESIAN_POINT('Ctrl Pts',(0.413053825467058,3.19723302633357,
16.7233120228146));
#253735=CARTESIAN_POINT('Ctrl Pts',(0.331149816409503,3.2067507471146,16.7285888616959));
#253736=CARTESIAN_POINT('Ctrl Pts',(0.0251911439521461,3.23045872347178,
16.7485558893281));
#253737=CARTESIAN_POINT('Ctrl Pts',(-0.199773368623699,3.22437068052218,
16.7637982351436));
#253738=CARTESIAN_POINT('Ctrl Pts',(-0.549444883315904,3.17815831441755,
16.7875673142268));
#253739=CARTESIAN_POINT('Ctrl Pts',(-0.675539618838877,3.15376477163643,
16.7961396045584));
#253740=CARTESIAN_POINT('Ctrl Pts',(-0.828007868655634,3.11470146448752,
16.8062691237319));
#253741=CARTESIAN_POINT('Ctrl Pts',(-0.856064191567081,3.10710741341235,
16.8081228787851));
#253742=CARTESIAN_POINT('Ctrl Pts',(-0.896837468873169,3.09547700837977,
16.8107981390015));
#253743=CARTESIAN_POINT('Ctrl Pts',(-0.909637345366491,3.0917398450466,
16.811635263557));
#253744=CARTESIAN_POINT('Ctrl Pts',(-0.932188832620323,3.08500334161735,
16.8131049011151));
#253745=CARTESIAN_POINT('Ctrl Pts',(-0.941949866683177,3.08203700429875,
16.8137392410099));
#253746=CARTESIAN_POINT('Ctrl Pts',(-0.963173664154548,3.07547693062523,
16.8151145852727));
#253747=CARTESIAN_POINT('Ctrl Pts',(-0.974630549964727,3.07186542021568,
16.8158545656487));
#253748=CARTESIAN_POINT('Ctrl Pts',(-1.0067531555517,3.06154172817584,16.8179231173744));
#253749=CARTESIAN_POINT('Ctrl Pts',(-1.02737199532258,3.05468435529223,
16.8192436538562));
#253750=CARTESIAN_POINT('Ctrl Pts',(-1.17103920688375,3.00528453473384,
16.8284044340231));
#253751=CARTESIAN_POINT('Ctrl Pts',(-1.29149395777692,2.95552346271042,
16.8358792239531));
#253752=CARTESIAN_POINT('Ctrl Pts',(-1.53626769814081,2.83657211369362,
16.8512625298992));
#253753=CARTESIAN_POINT('Ctrl Pts',(-1.65968013394142,2.76617473683709,
16.8591358341182));
#253754=CARTESIAN_POINT('Ctrl Pts',(-1.91472184588331,2.59746228654541,
16.8763708297612));
#253755=CARTESIAN_POINT('Ctrl Pts',(-2.04428201536366,2.4967722862904,16.8857549371368));
#253756=CARTESIAN_POINT('Ctrl Pts',(-2.191117783336,2.36353679077418,16.8975894816669));
#253757=CARTESIAN_POINT('Ctrl Pts',(-2.21624576679139,2.33999099718552,
16.8996607286598));
#253758=CARTESIAN_POINT('Ctrl Pts',(-2.25561912331138,2.30189362390212,
16.9029834003136));
#253759=CARTESIAN_POINT('Ctrl Pts',(-2.27011261066873,2.28760149299407,
16.9042237000457));
#253760=CARTESIAN_POINT('Ctrl Pts',(-2.29728609412987,2.26029297476584,
16.9065825677269));
#253761=CARTESIAN_POINT('Ctrl Pts',(-2.30999332905642,2.24730472533306,
16.9076998755978));
#253762=CARTESIAN_POINT('Ctrl Pts',(-2.33863449835674,2.21753058077326,
16.9102512344071));
#253763=CARTESIAN_POINT('Ctrl Pts',(-2.3544986684942,2.20067925178266,16.9116881944861));
#253764=CARTESIAN_POINT('Ctrl Pts',(-2.39541192476044,2.15627132302239,
16.9154575888654));
#253765=CARTESIAN_POINT('Ctrl Pts',(-2.42016673171305,2.12844946242157,
16.9178020807243));
#253766=CARTESIAN_POINT('Ctrl Pts',(-2.61679113848599,1.899597981639,16.9369569201223));
#253767=CARTESIAN_POINT('Ctrl Pts',(-2.7637706830185,1.67856776028842,16.9547833683786));
#253768=CARTESIAN_POINT('Ctrl Pts',(-2.95343956640391,1.29951634979094,
16.9834035323129));
#253769=CARTESIAN_POINT('Ctrl Pts',(-3.0141236507671,1.151788710399,16.9941110107567));
#253770=CARTESIAN_POINT('Ctrl Pts',(-3.07048166104438,0.979156861753478,
17.0057157522141));
#253771=CARTESIAN_POINT('Ctrl Pts',(-3.07712300845376,0.958081334463621,
17.0071173901006));
#253772=CARTESIAN_POINT('Ctrl Pts',(-3.08702393418855,0.925496514704128,
17.0092594756491));
#253773=CARTESIAN_POINT('Ctrl Pts',(-3.09043694730224,0.914035040027978,
17.0100082057343));
#253774=CARTESIAN_POINT('Ctrl Pts',(-3.09664524104275,0.892754185977941,
17.0113892922575));
#253775=CARTESIAN_POINT('Ctrl Pts',(-3.09945768247206,0.882940464430938,
17.0120225717708));
#253776=CARTESIAN_POINT('Ctrl Pts',(-3.10579629462377,0.860418993414859,
17.0134677836102));
#253777=CARTESIAN_POINT('Ctrl Pts',(-3.10929114913333,0.847702796837297,
17.0142779355073));
#253778=CARTESIAN_POINT('Ctrl Pts',(-3.12023078536697,0.806920390358045,
17.016858540799));
#253779=CARTESIAN_POINT('Ctrl Pts',(-3.12737458536215,0.778774039625884,
17.0186128896932));
#253780=CARTESIAN_POINT('Ctrl Pts',(-3.19278584275539,0.50562467217549,
17.0354148590709));
#253781=CARTESIAN_POINT('Ctrl Pts',(-3.22253397295609,0.254652021912385,
17.0491740595322));
#253782=CARTESIAN_POINT('Ctrl Pts',(-3.22274960926121,0.00183250105543022,
17.0633995295227));
#253783=CARTESIAN_POINT('Ctrl Pts',(-3.22275000000003,0.000916246347937087,
17.0634510886575));
#253784=CARTESIAN_POINT('Ctrl Pts',(-3.22275,-9.68142638581001E-11,17.0635026513638));
#253785=CARTESIAN_POINT('Origin',(0.,0.,-2.31077344927308));
#253786=CARTESIAN_POINT('',(-3.2227491362909,-0.00235945677226465,18.5607734492731));
#253787=CARTESIAN_POINT('',(-3.22274955323411,-0.00169694707575843,18.3142265507618));
#253788=CARTESIAN_POINT('',(-3.22275,-3.50678552687464E-13,-2.31077344927308));
#253789=CARTESIAN_POINT('Ctrl Pts',(-3.22274907157671,-0.00244625253626111,
18.5592428712784));
#253790=CARTESIAN_POINT('Ctrl Pts',(-3.22289265676903,0.186716165640959,
18.5485157862865));
#253791=CARTESIAN_POINT('Ctrl Pts',(-3.20638176666725,0.375530774842403,
18.538092345269));
#253792=CARTESIAN_POINT('Ctrl Pts',(-3.15034419603654,0.692057453392939,
18.5198245147944));
#253793=CARTESIAN_POINT('Ctrl Pts',(-3.11929282742046,0.820742737597622,
18.5121709164876));
#253794=CARTESIAN_POINT('Ctrl Pts',(-3.07092396691331,0.9780536930799,18.5023304837446));
#253795=CARTESIAN_POINT('Ctrl Pts',(-3.06095693997436,1.00881392503395,
18.500383046183));
#253796=CARTESIAN_POINT('Ctrl Pts',(-3.0441992194529,1.05799520194429,18.4972294032883));
#253797=CARTESIAN_POINT('Ctrl Pts',(-3.03769994845516,1.07651369328513,
18.4960327417886));
#253798=CARTESIAN_POINT('Ctrl Pts',(-3.02497181905704,1.1117469146277,18.4937378319867));
#253799=CARTESIAN_POINT('Ctrl Pts',(-3.01877252145473,1.12847159991908,
18.4926405949002));
#253800=CARTESIAN_POINT('Ctrl Pts',(-3.00434360828263,1.16642854819456,
18.4901320169461));
#253801=CARTESIAN_POINT('Ctrl Pts',(-2.9960272208709,1.18762659287769,18.4887178333907));
#253802=CARTESIAN_POINT('Ctrl Pts',(-2.97335059846975,1.24367374548421,
18.4849428155627));
#253803=CARTESIAN_POINT('Ctrl Pts',(-2.95860278808216,1.27836126251055,
18.4825691734736));
#253804=CARTESIAN_POINT('Ctrl Pts',(-2.8375692250755,1.54971809102887,18.4636983257894));
#253805=CARTESIAN_POINT('Ctrl Pts',(-2.70368078570787,1.77298838242029,
18.4462272055401));
#253806=CARTESIAN_POINT('Ctrl Pts',(-2.47456335328253,2.06776451096623,
18.421001454548));
#253807=CARTESIAN_POINT('Ctrl Pts',(-2.39987166523696,2.15400388294558,
18.4133240966872));
#253808=CARTESIAN_POINT('Ctrl Pts',(-2.29299434564181,2.26492741216265,
18.4031990806177));
#253809=CARTESIAN_POINT('Ctrl Pts',(-2.26468996333598,2.29322892615946,
18.4005921272635));
#253810=CARTESIAN_POINT('Ctrl Pts',(-2.21551382074105,2.34060132247369,
18.396198429975));
#253811=CARTESIAN_POINT('Ctrl Pts',(-2.19490534987753,2.35993785306692,
18.3943960646057));
#253812=CARTESIAN_POINT('Ctrl Pts',(-2.16471738561906,2.38752504626452,
18.39181497478));
#253813=CARTESIAN_POINT('Ctrl Pts',(-2.15534011743283,2.39599378060399,
18.3910212753626));
#253814=CARTESIAN_POINT('Ctrl Pts',(-2.14583998281727,2.40447257007618,
18.3902254784126));
#253815=CARTESIAN_POINT('Ctrl Pts',(-2.14576685713346,2.40453782813529,
18.3902193533928));
#253816=CARTESIAN_POINT('Ctrl Pts',(-2.14562004521291,2.40466883246587,
18.3902070573914));
#253817=CARTESIAN_POINT('Ctrl Pts',(-2.14554635892637,2.40473457869055,
18.390200886413));
#253818=CARTESIAN_POINT('Ctrl Pts',(-2.14539840308711,2.40486657934217,
18.3901884966149));
#253819=CARTESIAN_POINT('Ctrl Pts',(-2.14532413348151,2.4049328337206,18.3901822777987));
#253820=CARTESIAN_POINT('Ctrl Pts',(-2.1451749876093,2.40506587126047,18.3901697903902));
#253821=CARTESIAN_POINT('Ctrl Pts',(-2.14510011130034,2.40513265435937,
18.3901635218026));
#253822=CARTESIAN_POINT('Ctrl Pts',(-2.14494972793376,2.40526677052088,
18.3901509328599));
#253823=CARTESIAN_POINT('Ctrl Pts',(-2.1448742208241,2.40533410352476,18.3901446125091));
#253824=CARTESIAN_POINT('Ctrl Pts',(-2.14472255103112,2.40546934131582,
18.3901319179883));
#253825=CARTESIAN_POINT('Ctrl Pts',(-2.14464638829686,2.4055372460382,18.3901255438232));
#253826=CARTESIAN_POINT('Ctrl Pts',(-2.14449338165679,2.40567364975537,
18.3901127395591));
#253827=CARTESIAN_POINT('Ctrl Pts',(-2.1444165376944,2.40574214868507,18.390106309465));
#253828=CARTESIAN_POINT('Ctrl Pts',(-2.14426214219056,2.40587976400727,
18.3900933911624));
#253829=CARTESIAN_POINT('Ctrl Pts',(-2.14418459058588,2.40594888033503,
18.3900869029585));
#253830=CARTESIAN_POINT('Ctrl Pts',(-2.1440287525332,2.40608775438591,18.3900738661858));
#253831=CARTESIAN_POINT('Ctrl Pts',(-2.14395046602077,2.40615751203953,
18.3900673176219));
#253832=CARTESIAN_POINT('Ctrl Pts',(-2.14379312998843,2.40629769345415,
18.3900541578052));
#253833=CARTESIAN_POINT('Ctrl Pts',(-2.14371408040529,2.40636811713845,
18.390047546558));
#253834=CARTESIAN_POINT('Ctrl Pts',(-2.14355518912952,2.40650965613853,
18.390034258974));
#253835=CARTESIAN_POINT('Ctrl Pts',(-2.14347534736779,2.4065807713764,18.390027582643));
#253836=CARTESIAN_POINT('Ctrl Pts',(-2.14331484164867,2.40672371985968,
18.3900141624106));
#253837=CARTESIAN_POINT('Ctrl Pts',(-2.14323417761161,2.40679555302983,
18.3900074185147));
#253838=CARTESIAN_POINT('Ctrl Pts',(-2.14307199621088,2.40693996465833,
18.3899938605866));
#253839=CARTESIAN_POINT('Ctrl Pts',(-2.14299047876653,2.40701254303519,
18.3899870465603));
#253840=CARTESIAN_POINT('Ctrl Pts',(-2.13547016417003,2.41370750757851,
18.389358481527));
#253841=CARTESIAN_POINT('Ctrl Pts',(-2.12800069466802,2.42029539655638,
18.3887392887263));
#253842=CARTESIAN_POINT('Ctrl Pts',(-2.11161461749736,2.43461301049126,
18.3873921436935));
#253843=CARTESIAN_POINT('Ctrl Pts',(-2.10268600934501,2.44232847094139,
18.3866652153393));
#253844=CARTESIAN_POINT('Ctrl Pts',(-2.07737037182655,2.46396269251239,
18.3846234513338));
#253845=CARTESIAN_POINT('Ctrl Pts',(-2.06088581758185,2.47776704208275,
18.3833165590309));
#253846=CARTESIAN_POINT('Ctrl Pts',(-1.93380051263754,2.58204387048164,
18.3734018989864));
#253847=CARTESIAN_POINT('Ctrl Pts',(-1.81741748455037,2.66524640239701,
18.3652389028851));
#253848=CARTESIAN_POINT('Ctrl Pts',(-1.52479823513691,2.84632866918401,
18.3458498945639));
#253849=CARTESIAN_POINT('Ctrl Pts',(-1.34418133543501,2.93594477651714,
18.3347532156109));
#253850=CARTESIAN_POINT('Ctrl Pts',(-1.09342143822162,3.0323419879976,18.319317376898));
#253851=CARTESIAN_POINT('Ctrl Pts',(-1.02971272886994,3.05456367741998,
18.3153966448098));
#253852=CARTESIAN_POINT('Ctrl Pts',(-0.917897780646437,3.08966916607696,
18.3084805638168));
#253853=CARTESIAN_POINT('Ctrl Pts',(-0.870102649171766,3.10346787904315,
18.3055136291425));
#253854=CARTESIAN_POINT('Ctrl Pts',(-0.799668068809054,3.12204778911762,
18.3011166901102));
#253855=CARTESIAN_POINT('Ctrl Pts',(-0.777264718889288,3.12770058222117,
18.2997145608484));
#253856=CARTESIAN_POINT('Ctrl Pts',(-0.737489410724561,3.13728291489456,
18.2972180130621));
#253857=CARTESIAN_POINT('Ctrl Pts',(-0.720141864803557,3.14131029884364,
18.2961267705086));
#253858=CARTESIAN_POINT('Ctrl Pts',(-0.683628100468923,3.14946893473035,
18.2938244559817));
#253859=CARTESIAN_POINT('Ctrl Pts',(-0.664455832561879,3.15356946493662,
18.2926124551757));
#253860=CARTESIAN_POINT('Ctrl Pts',(-0.613578293327099,3.16396650961847,
18.2893873627523));
#253861=CARTESIAN_POINT('Ctrl Pts',(-0.581814301881632,3.16996126044856,
18.287364832157));
#253862=CARTESIAN_POINT('Ctrl Pts',(-0.434557798851252,3.19546487112564,
18.2779439075572));
#253863=CARTESIAN_POINT('Ctrl Pts',(-0.318158166711865,3.20914416131536,
18.2703662463738));
#253864=CARTESIAN_POINT('Ctrl Pts',(0.000583492502514438,3.22909071952589,
18.2492850145463));
#253865=CARTESIAN_POINT('Ctrl Pts',(0.203182023034414,3.22269036192606,
18.2354985925683));
#253866=CARTESIAN_POINT('Ctrl Pts',(0.515746792402945,3.18321375305085,
18.2143245794595));
#253867=CARTESIAN_POINT('Ctrl Pts',(0.626863036132827,3.16320912599812,
18.2068259779797));
#253868=CARTESIAN_POINT('Ctrl Pts',(0.763109223612543,3.13121657159533,
18.1978347342203));
#253869=CARTESIAN_POINT('Ctrl Pts',(0.78943012282361,3.12468447973809,18.1961074641414));
#253870=CARTESIAN_POINT('Ctrl Pts',(0.828043772463393,3.11458259768344,
18.1935909508561));
#253871=CARTESIAN_POINT('Ctrl Pts',(0.840401990859866,3.11127076186023,
18.1927881944016));
#253872=CARTESIAN_POINT('Ctrl Pts',(0.861422044966705,3.1055032874127,18.1914276937007));
#253873=CARTESIAN_POINT('Ctrl Pts',(0.870093711013847,3.10308484392979,
18.1908678724106));
#253874=CARTESIAN_POINT('Ctrl Pts',(0.88981034595826,3.09749691485816,18.1895983618062));
#253875=CARTESIAN_POINT('Ctrl Pts',(0.900848598557094,3.09430467169069,
18.1888899864163));
#253876=CARTESIAN_POINT('Ctrl Pts',(0.931135949951803,3.08536981499655,
18.1869521872327));
#253877=CARTESIAN_POINT('Ctrl Pts',(0.950349154847304,3.07950606147134,
18.1857294649824));
#253878=CARTESIAN_POINT('Ctrl Pts',(1.0567833801761,3.04593197530457,18.1789860516857));
#253879=CARTESIAN_POINT('Ctrl Pts',(1.14285593849067,3.01469336616768,18.1736447628338));
#253880=CARTESIAN_POINT('Ctrl Pts',(1.38422193025158,2.91526684752681,18.1586846372908));
#253881=CARTESIAN_POINT('Ctrl Pts',(1.53562272305683,2.83843602488646,18.1493112682678));
#253882=CARTESIAN_POINT('Ctrl Pts',(1.81914689099172,2.66520251733294,18.1306354007406));
#253883=CARTESIAN_POINT('Ctrl Pts',(1.95137111153841,2.56996934147149,18.1213703445541));
#253884=CARTESIAN_POINT('Ctrl Pts',(2.10909688270586,2.43715390995463,18.109149262779));
#253885=CARTESIAN_POINT('Ctrl Pts',(2.1417909646266,2.40847255271934,18.1065471119432));
#253886=CARTESIAN_POINT('Ctrl Pts',(2.19009365838177,2.36433688115209,18.1025911698138));
#253887=CARTESIAN_POINT('Ctrl Pts',(2.20614181592318,2.34936956895683,18.101257642436));
#253888=CARTESIAN_POINT('Ctrl Pts',(2.23486556242298,2.32202654013214,18.0988350767202));
#253889=CARTESIAN_POINT('Ctrl Pts',(2.24759443710301,2.30970789534828,18.0977485050319));
#253890=CARTESIAN_POINT('Ctrl Pts',(2.27473485807694,2.28300535576677,18.0954031421203));
#253891=CARTESIAN_POINT('Ctrl Pts',(2.2891128756103,2.26858862324514,18.0941429399683));
#253892=CARTESIAN_POINT('Ctrl Pts',(2.3277127063239,2.22914426486944,18.0907106872668));
#253893=CARTESIAN_POINT('Ctrl Pts',(2.35166642512312,2.20385922195507,18.0885272481012));
#253894=CARTESIAN_POINT('Ctrl Pts',(2.50375068066485,2.0380192396147,18.0743081932357));
#253895=CARTESIAN_POINT('Ctrl Pts',(2.61961519151745,1.88676578086715,18.0617689980249));
#253896=CARTESIAN_POINT('Ctrl Pts',(2.79549768026726,1.60947748514098,18.0396857429976));
#253897=CARTESIAN_POINT('Ctrl Pts',(2.86195065340621,1.4881073368923,18.0302902104782));
#253898=CARTESIAN_POINT('Ctrl Pts',(2.95150431113851,1.29620521709324,18.0161055242689));
#253899=CARTESIAN_POINT('Ctrl Pts',(2.98031482430023,1.22851556222435,18.0112240321775));
#253900=CARTESIAN_POINT('Ctrl Pts',(3.02288525410323,1.11816068621147,18.0035182878308));
#253901=CARTESIAN_POINT('Ctrl Pts',(3.0381152030706,1.07609249040335,18.0006382333831));
#253902=CARTESIAN_POINT('Ctrl Pts',(3.057458715557,1.01897307599925,17.996817085121));
#253903=CARTESIAN_POINT('Ctrl Pts',(3.06234548039941,1.00419127077684,17.9958361912822));
#253904=CARTESIAN_POINT('Ctrl Pts',(3.07031540624611,0.979483979114567,
17.9942105995237));
#253905=CARTESIAN_POINT('Ctrl Pts',(3.07345797221054,0.969578084257697,
17.9935625674794));
#253906=CARTESIAN_POINT('Ctrl Pts',(3.07934128880534,0.950716830511556,
17.9923359702249));
#253907=CARTESIAN_POINT('Ctrl Pts',(3.08209100349124,0.941764469582951,
17.9917568711489));
#253908=CARTESIAN_POINT('Ctrl Pts',(3.08931848818855,0.917862932002773,
17.9902186902545));
#253909=CARTESIAN_POINT('Ctrl Pts',(3.09372683225813,0.902892791693413,
17.9892635370282));
#253910=CARTESIAN_POINT('Ctrl Pts',(3.10949988179563,0.847857511358168,
17.9857802691206));
#253911=CARTESIAN_POINT('Ctrl Pts',(3.12019694500608,0.807603405350767,
17.9832871337268));
#253912=CARTESIAN_POINT('Ctrl Pts',(3.20048233435499,0.480024960892568,
17.9633550802903));
#253913=CARTESIAN_POINT('Ctrl Pts',(3.23102057869182,0.184553969359728,
17.947467070587));
#253914=CARTESIAN_POINT('Ctrl Pts',(3.21815755737333,-0.188796176570578,
17.9261325374059));
#253915=CARTESIAN_POINT('Ctrl Pts',(3.21265618676044,-0.266497884558532,
17.9216319260998));
#253916=CARTESIAN_POINT('Ctrl Pts',(3.198437993779,-0.398970354423279,17.9137969797588));
#253917=CARTESIAN_POINT('Ctrl Pts',(3.19111220268402,-0.453856053319911,
17.9105030208264));
#253918=CARTESIAN_POINT('Ctrl Pts',(3.17857384596906,-0.532321984482374,
17.9057123614175));
#253919=CARTESIAN_POINT('Ctrl Pts',(3.17450425545294,-0.556076499646197,
17.9042512814675));
#253920=CARTESIAN_POINT('Ctrl Pts',(3.16693659525158,-0.597455384115182,
17.9016863593282));
#253921=CARTESIAN_POINT('Ctrl Pts',(3.16355681204449,-0.615100488439679,
17.9005862866126));
#253922=CARTESIAN_POINT('Ctrl Pts',(3.15626068666414,-0.651540167683742,
17.8983009871887));
#253923=CARTESIAN_POINT('Ctrl Pts',(3.1523235919564,-0.670329813301026,
17.8971151421686));
#253924=CARTESIAN_POINT('Ctrl Pts',(3.14172541162423,-0.718749814050308,
17.894039479047));
#253925=CARTESIAN_POINT('Ctrl Pts',(3.13481306293851,-0.748322669066041,
17.8921417550143));
#253926=CARTESIAN_POINT('Ctrl Pts',(3.1042159592421,-0.871352828823828,
17.8841639006274));
#253927=CARTESIAN_POINT('Ctrl Pts',(3.07676349182583,-0.963813173747749,
17.8779654979819));
#253928=CARTESIAN_POINT('Ctrl Pts',(2.96818310575658,-1.2772562202947,17.8562486567092));
#253929=CARTESIAN_POINT('Ctrl Pts',(2.86703582966643,-1.4904960917351,17.8401744759062));
#253930=CARTESIAN_POINT('Ctrl Pts',(2.68337422031547,-1.78851827437921,
17.8166894609929));
#253931=CARTESIAN_POINT('Ctrl Pts',(2.61796438130813,-1.88296646264973,
17.8090873496476));
#253932=CARTESIAN_POINT('Ctrl Pts',(2.53498569952396,-1.99007348316253,
17.8004424870812));
#253933=CARTESIAN_POINT('Ctrl Pts',(2.5221670050057,-2.00629474785566,17.7991326313734));
#253934=CARTESIAN_POINT('Ctrl Pts',(2.50197733683822,-2.03134417850028,
17.7971104346578));
#253935=CARTESIAN_POINT('Ctrl Pts',(2.49471396413578,-2.04025782984851,
17.7963909571666));
#253936=CARTESIAN_POINT('Ctrl Pts',(2.48103771707673,-2.05685916504241,
17.7950514651011));
#253937=CARTESIAN_POINT('Ctrl Pts',(2.4746367245951,-2.0645558511334,17.7944306957874));
#253938=CARTESIAN_POINT('Ctrl Pts',(2.4597418607655,-2.08229694391672,17.7930001745159));
#253939=CARTESIAN_POINT('Ctrl Pts',(2.45122224052103,-2.09231931732119,
17.7921922864226));
#253940=CARTESIAN_POINT('Ctrl Pts',(2.42319191719161,-2.12488763291403,
17.7895667518686));
#253941=CARTESIAN_POINT('Ctrl Pts',(2.40342906115388,-2.14721573445124,
17.7877663433793));
#253942=CARTESIAN_POINT('Ctrl Pts',(2.26861571506168,-2.29533419436434,
17.7757947133883));
#253943=CARTESIAN_POINT('Ctrl Pts',(2.14403728381326,-2.4121140214532,17.7662081555279));
#253944=CARTESIAN_POINT('Ctrl Pts',(1.8772630285072,-2.62510884218131,17.7470841331315));
#253945=CARTESIAN_POINT('Ctrl Pts',(1.73547155627702,-2.7209277081484,17.7375714086374));
#253946=CARTESIAN_POINT('Ctrl Pts',(1.53270587971579,-2.83562817915063,
17.724138046052));
#253947=CARTESIAN_POINT('Ctrl Pts',(1.47778100201632,-2.86463560360211,
17.7205170399961));
#253948=CARTESIAN_POINT('Ctrl Pts',(1.38011983398281,-2.91265695079055,
17.7140815238228));
#253949=CARTESIAN_POINT('Ctrl Pts',(1.33774322908415,-2.93236150435328,
17.7112900843765));
#253950=CARTESIAN_POINT('Ctrl Pts',(1.27429577444581,-2.96020215701313,
17.707104649604));
#253951=CARTESIAN_POINT('Ctrl Pts',(1.25354262021145,-2.96904991383025,
17.7057347131584));
#253952=CARTESIAN_POINT('Ctrl Pts',(1.21629062550533,-2.98447148427544,
17.7032732465998));
#253953=CARTESIAN_POINT('Ctrl Pts',(1.1998269723624,-2.99112823910091,17.7021845569713));
#253954=CARTESIAN_POINT('Ctrl Pts',(1.16476870288429,-3.00496734664593,
17.6998641089949));
#253955=CARTESIAN_POINT('Ctrl Pts',(1.14616084572861,-3.01211390438744,
17.698631210315));
#253956=CARTESIAN_POINT('Ctrl Pts',(1.09583018101518,-3.03091005914756,
17.6952924626129));
#253957=CARTESIAN_POINT('Ctrl Pts',(1.06398915215974,-3.04223380393089,
17.6931759802756));
#253958=CARTESIAN_POINT('Ctrl Pts',(0.898003063781035,-3.09833952047665,
17.6821172241117));
#253959=CARTESIAN_POINT('Ctrl Pts',(0.761211314198354,-3.13475126065524,
17.6729074610022));
#253960=CARTESIAN_POINT('Ctrl Pts',(0.359974574203611,-3.21373904878994,
17.6457022911956));
#253961=CARTESIAN_POINT('Ctrl Pts',(0.0920652514683722,-3.23252509157068,
17.6272256620244));
#253962=CARTESIAN_POINT('Ctrl Pts',(-0.216769407828373,-3.21572260629027,
17.6071164595651));
#253963=CARTESIAN_POINT('Ctrl Pts',(-0.258414812413189,-3.21264424075758,
17.6044324806253));
#253964=CARTESIAN_POINT('Ctrl Pts',(-0.315088636555306,-3.20734573300469,
17.6008280514753));
#253965=CARTESIAN_POINT('Ctrl Pts',(-0.33017668287957,-3.20582764337693,
17.5998731244586));
#253966=CARTESIAN_POINT('Ctrl Pts',(-0.355499536651544,-3.20309909868199,
17.5982789058878));
#253967=CARTESIAN_POINT('Ctrl Pts',(-0.36574016072204,-3.20194595547756,
17.5976365334628));
#253968=CARTESIAN_POINT('Ctrl Pts',(-0.386653523051162,-3.19948936744569,
17.5963296839163));
#253969=CARTESIAN_POINT('Ctrl Pts',(-0.397325538418083,-3.19818160579537,
17.5956654458054));
#253970=CARTESIAN_POINT('Ctrl Pts',(-0.425106483149743,-3.19463609069579,
17.59394275232));
#253971=CARTESIAN_POINT('Ctrl Pts',(-0.442204590101602,-3.19231427094593,
17.5928888549849));
#253972=CARTESIAN_POINT('Ctrl Pts',(-0.513038613184772,-3.18211540391633,
17.5885460985855));
#253973=CARTESIAN_POINT('Ctrl Pts',(-0.566592830316869,-3.17301755137519,
17.5853184957343));
#253974=CARTESIAN_POINT('Ctrl Pts',(-0.812597715321352,-3.12479817419771,
17.5706455773933));
#253975=CARTESIAN_POINT('Ctrl Pts',(-1.00146171427537,-3.06948964035161,
17.5597968991057));
#253976=CARTESIAN_POINT('Ctrl Pts',(-1.33861990628245,-2.93629140283928,
17.5394641099352));
#253977=CARTESIAN_POINT('Ctrl Pts',(-1.48814685387385,-2.86341084085395,
17.5300591942345));
#253978=CARTESIAN_POINT('Ctrl Pts',(-1.67602261696069,-2.7531336722922,
17.5172193693333));
#253979=CARTESIAN_POINT('Ctrl Pts',(-1.72002270675444,-2.72586101548764,
17.5141347982859));
#253980=CARTESIAN_POINT('Ctrl Pts',(-1.78299902768415,-2.68469427638844,
17.5095953097727));
#253981=CARTESIAN_POINT('Ctrl Pts',(-1.8025114237413,-2.67163272421818,
17.5081709195013));
#253982=CARTESIAN_POINT('Ctrl Pts',(-1.83662312005357,-2.64825462776954,
17.5056481574118));
#253983=CARTESIAN_POINT('Ctrl Pts',(-1.85128271409607,-2.63802754931779,
17.5045531769896));
#253984=CARTESIAN_POINT('Ctrl Pts',(-1.88172191122941,-2.61641335612001,
17.5022564434706));
#253985=CARTESIAN_POINT('Ctrl Pts',(-1.89748493373297,-2.60500424206966,
17.5010538792809));
#253986=CARTESIAN_POINT('Ctrl Pts',(-1.9385573931954,-2.57470583432497,
17.4978850969095));
#253987=CARTESIAN_POINT('Ctrl Pts',(-1.96369369149169,-2.55558640489592,
17.495910045533));
#253988=CARTESIAN_POINT('Ctrl Pts',(-2.07218293515721,-2.47052053146101,
17.4872252116354));
#253989=CARTESIAN_POINT('Ctrl Pts',(-2.15251780084418,-2.40084920090603,
17.4803700407907));
#253990=CARTESIAN_POINT('Ctrl Pts',(-2.37943224253378,-2.18349799222926,
17.4597123312903));
#253991=CARTESIAN_POINT('Ctrl Pts',(-2.51532219767696,-2.02546329964362,
17.4455528138737));
#253992=CARTESIAN_POINT('Ctrl Pts',(-2.70311051878341,-1.75877642124855,
17.4236083599625));
#253993=CARTESIAN_POINT('Ctrl Pts',(-2.76582600409758,-1.65840666523159,
17.4157341560036));
#253994=CARTESIAN_POINT('Ctrl Pts',(-2.83626884054577,-1.53051168669115,
17.4063484025657));
#253995=CARTESIAN_POINT('Ctrl Pts',(-2.84933726048621,-1.50604258025941,
17.4045808330466));
#253996=CARTESIAN_POINT('Ctrl Pts',(-2.86802715091668,-1.46993357904964,
17.4020166896389));
#253997=CARTESIAN_POINT('Ctrl Pts',(-2.87389676301276,-1.45842444920831,
17.4012059180587));
#253998=CARTESIAN_POINT('Ctrl Pts',(-2.88417141466274,-1.43797501138345,
17.3997772397499));
#253999=CARTESIAN_POINT('Ctrl Pts',(-2.88860438535316,-1.42904919308393,
17.3991576556842));
#254000=CARTESIAN_POINT('Ctrl Pts',(-2.89819853603028,-1.40950423861687,
17.3978097375175));
#254001=CARTESIAN_POINT('Ctrl Pts',(-2.90334282201466,-1.39887720010469,
17.3970824269107));
#254002=CARTESIAN_POINT('Ctrl Pts',(-2.91768982336112,-1.36881916030356,
17.3950403087782));
#254003=CARTESIAN_POINT('Ctrl Pts',(-2.92675685106363,-1.34932360453472,
17.393733432173));
#254004=CARTESIAN_POINT('Ctrl Pts',(-2.99083166330623,-1.20786730980781,
17.3843674630359));
#254005=CARTESIAN_POINT('Ctrl Pts',(-3.03839891047501,-1.08266234440226,
17.3766965786054));
#254006=CARTESIAN_POINT('Ctrl Pts',(-3.08934340044724,-0.918437975359805,
17.3669871660932));
#254007=CARTESIAN_POINT('Ctrl Pts',(-3.09999191628583,-0.881828295867643,
17.3648447110038));
#254008=CARTESIAN_POINT('Ctrl Pts',(-3.14663311000897,-0.710174966302317,
17.3548691720586));
#254009=CARTESIAN_POINT('Ctrl Pts',(-3.17446613581936,-0.573072446619124,
17.3470946691516));
#254010=CARTESIAN_POINT('Ctrl Pts',(-3.20487799820405,-0.349615226686832,
17.3342678168282));
#254011=CARTESIAN_POINT('Ctrl Pts',(-3.21304634824452,-0.264207274741575,
17.329330984468));
#254012=CARTESIAN_POINT('Ctrl Pts',(-3.22109031821581,-0.119263850536278,
17.3208150886266));
#254013=CARTESIAN_POINT('Ctrl Pts',(-3.22274128749274,-0.0598718822926805,
17.3172869848923));
#254014=CARTESIAN_POINT('Ctrl Pts',(-3.22274998853597,-0.000313882066399077,
17.3136991171112));
#254015=CARTESIAN_POINT('Ctrl Pts',(-3.22275,-0.000156941007807153,17.3136896623894));
#254016=CARTESIAN_POINT('Ctrl Pts',(-3.22275,-2.95105326763967E-13,17.3136802073254));
#254017=CARTESIAN_POINT('Ctrl Pts',(-3.22275,-9.68149171942656E-11,17.0635026513638));
#254018=CARTESIAN_POINT('Ctrl Pts',(-3.22274999999488,-0.170393836325402,
17.0730917388645));
#254019=CARTESIAN_POINT('Ctrl Pts',(-3.20923696781612,-0.340500790962171,
17.082824205386));
#254020=CARTESIAN_POINT('Ctrl Pts',(-3.17681918572208,-0.543288175441212,
17.0950718298512));
#254021=CARTESIAN_POINT('Ctrl Pts',(-3.17073276211461,-0.577750628907981,
17.0971752596468));
#254022=CARTESIAN_POINT('Ctrl Pts',(-3.16016034217372,-0.632401363187258,
17.1005491225351));
#254023=CARTESIAN_POINT('Ctrl Pts',(-3.15603904588094,-0.652657936893176,
17.1018080669125));
#254024=CARTESIAN_POINT('Ctrl Pts',(-3.14797543408352,-0.69042772216104,
17.1041717981521));
#254025=CARTESIAN_POINT('Ctrl Pts',(-3.14408109531189,-0.707950435224602,
17.1052750235425));
#254026=CARTESIAN_POINT('Ctrl Pts',(-3.13496294018237,-0.747418069020755,
17.107775237951));
#254027=CARTESIAN_POINT('Ctrl Pts',(-3.12965473120727,-0.769342335082444,
17.1091748672982));
#254028=CARTESIAN_POINT('Ctrl Pts',(-3.11303273091276,-0.83497492524587,
17.113398022427));
#254029=CARTESIAN_POINT('Ctrl Pts',(-3.10103056160646,-0.878501586427535,
17.1162432993291));
#254030=CARTESIAN_POINT('Ctrl Pts',(-3.07122824657916,-0.978346526626052,
17.1228762661628));
#254031=CARTESIAN_POINT('Ctrl Pts',(-3.05278676010583,-1.03445501352186,
17.1266830898872));
#254032=CARTESIAN_POINT('Ctrl Pts',(-2.98047410371263,-1.23565353176753,
17.1406215054443));
#254033=CARTESIAN_POINT('Ctrl Pts',(-2.91771633781987,-1.37731205804534,
17.1509985527858));
#254034=CARTESIAN_POINT('Ctrl Pts',(-2.75462437299016,-1.68380623296778,
17.1744465641999));
#254035=CARTESIAN_POINT('Ctrl Pts',(-2.64916987278993,-1.84528301323793,
17.187517671197));
#254036=CARTESIAN_POINT('Ctrl Pts',(-2.51184634270894,-2.01930618621883,
17.201786218988));
#254037=CARTESIAN_POINT('Ctrl Pts',(-2.49345387167668,-2.04197391013941,
17.203648110753));
#254038=CARTESIAN_POINT('Ctrl Pts',(-2.46629030520907,-2.07453713454269,
17.2063238664436));
#254039=CARTESIAN_POINT('Ctrl Pts',(-2.45776285477622,-2.08463281083364,
17.2071535894951));
#254040=CARTESIAN_POINT('Ctrl Pts',(-2.44253633224151,-2.10243622981725,
17.2086166076807));
#254041=CARTESIAN_POINT('Ctrl Pts',(-2.4358624045583,-2.11016496770706,
17.2092516458132));
#254042=CARTESIAN_POINT('Ctrl Pts',(-2.42130564541515,-2.12686132059507,
17.2106232563471));
#254043=CARTESIAN_POINT('Ctrl Pts',(-2.41340962875784,-2.13581695842871,
17.211358855025));
#254044=CARTESIAN_POINT('Ctrl Pts',(-2.39081957523888,-2.16115329045661,
17.2134403126916));
#254045=CARTESIAN_POINT('Ctrl Pts',(-2.37600697816514,-2.1774279978556,
17.2147777873293));
#254046=CARTESIAN_POINT('Ctrl Pts',(-2.25656255859755,-2.30599203304808,
17.2253591880144));
#254047=CARTESIAN_POINT('Ctrl Pts',(-2.14418411864865,-2.41084215175647,
17.2340913995234));
#254048=CARTESIAN_POINT('Ctrl Pts',(-1.82199512393724,-2.67102370508856,
17.2573818631441));
#254049=CARTESIAN_POINT('Ctrl Pts',(-1.60015208613001,-2.80954403288955,
17.2717444013117));
#254050=CARTESIAN_POINT('Ctrl Pts',(-1.32095529249746,-2.93997580848012,
17.2899573378653));
#254051=CARTESIAN_POINT('Ctrl Pts',(-1.27741603426991,-2.95915335324738,
17.2927978727887));
#254052=CARTESIAN_POINT('Ctrl Pts',(-1.21220155010863,-2.98617061486797,
17.2970609756012));
#254053=CARTESIAN_POINT('Ctrl Pts',(-1.19083987285442,-2.99475339458461,
17.2984586982096));
#254054=CARTESIAN_POINT('Ctrl Pts',(-1.15246842095333,-3.00969496777741,
17.300972558276));
#254055=CARTESIAN_POINT('Ctrl Pts',(-1.13549324915439,-3.01614030183761,
17.3020857611783));
#254056=CARTESIAN_POINT('Ctrl Pts',(-1.09930682502073,-3.02953121042691,
17.3044615381262));
#254057=CARTESIAN_POINT('Ctrl Pts',(-1.08008225251045,-3.03643823382723,
17.3057253283553));
#254058=CARTESIAN_POINT('Ctrl Pts',(-1.0279570095341,-3.0546081929117,17.3091569333583));
#254059=CARTESIAN_POINT('Ctrl Pts',(-0.994938321355894,-3.06552188243654,
17.3113360305214));
#254060=CARTESIAN_POINT('Ctrl Pts',(-0.796946840958239,-3.12742847165649,
17.3244388196282));
#254061=CARTESIAN_POINT('Ctrl Pts',(-0.628293598271117,-3.16562224884237,
17.3357713150107));
#254062=CARTESIAN_POINT('Ctrl Pts',(-0.208374407446207,-3.22583236506848,
17.3642046743258));
#254063=CARTESIAN_POINT('Ctrl Pts',(0.043993330221262,-3.23225712954553,
17.3815152739279));
#254064=CARTESIAN_POINT('Ctrl Pts',(0.323514552051184,-3.20660292339507,
17.399580839431));
#254065=CARTESIAN_POINT('Ctrl Pts',(0.352449781020123,-3.20355166355927,
17.4014365297001));
#254066=CARTESIAN_POINT('Ctrl Pts',(0.394445991978551,-3.19854718669193,
17.4041051128582));
#254067=CARTESIAN_POINT('Ctrl Pts',(0.407541684627146,-3.19690499318935,
17.4049337492644));
#254068=CARTESIAN_POINT('Ctrl Pts',(0.430750181589535,-3.19384972949573,
17.4063956102614));
#254069=CARTESIAN_POINT('Ctrl Pts',(0.440866847708669,-3.19246898906937,
17.4070305667339));
#254070=CARTESIAN_POINT('Ctrl Pts',(0.462812382340604,-3.18936751256247,
17.4084029231252));
#254071=CARTESIAN_POINT('Ctrl Pts',(0.474638375686615,-3.18762903336086,
17.4091393404628));
#254072=CARTESIAN_POINT('Ctrl Pts',(0.508267319334487,-3.18249411323786,
17.4112252692579));
#254073=CARTESIAN_POINT('Ctrl Pts',(0.530045894287881,-3.17893942361998,
17.4125663417633));
#254074=CARTESIAN_POINT('Ctrl Pts',(0.706725246801083,-3.14823567433904,
17.4233785294668));
#254075=CARTESIAN_POINT('Ctrl Pts',(0.859505318591126,-3.11000182259476,
17.4323123378207));
#254076=CARTESIAN_POINT('Ctrl Pts',(1.26278638728043,-2.97707085685767,
17.4561780496207));
#254077=CARTESIAN_POINT('Ctrl Pts',(1.50524980976448,-2.86213060248004,
17.4709263150195));
#254078=CARTESIAN_POINT('Ctrl Pts',(1.76185596040298,-2.69876677822356,
17.4889895270773));
#254079=CARTESIAN_POINT('Ctrl Pts',(1.79263266942669,-2.67842238959554,
17.4911980161354));
#254080=CARTESIAN_POINT('Ctrl Pts',(1.84205388601283,-2.64451999473144,
17.4948173875626));
#254081=CARTESIAN_POINT('Ctrl Pts',(1.86091457434846,-2.63128208794607,
17.4962163750274));
#254082=CARTESIAN_POINT('Ctrl Pts',(1.8943834326313,-2.60725119441303,17.4987316968925));
#254083=CARTESIAN_POINT('Ctrl Pts',(1.90904550758403,-2.59653473103001,
17.4998450845511));
#254084=CARTESIAN_POINT('Ctrl Pts',(1.93999725359777,-2.57350832161721,
17.5022203868674));
#254085=CARTESIAN_POINT('Ctrl Pts',(1.95626202558186,-2.56116639097569,
17.5034835097581));
#254086=CARTESIAN_POINT('Ctrl Pts',(1.99986726422881,-2.52742043922812,
17.5069111082397));
#254087=CARTESIAN_POINT('Ctrl Pts',(2.02698027544262,-2.50572823030897,
17.5090868192187));
#254088=CARTESIAN_POINT('Ctrl Pts',(2.18564816010552,-2.37452284945741,
17.5220908092559));
#254089=CARTESIAN_POINT('Ctrl Pts',(2.30863987473912,-2.25512370250672,
17.5333203396417));
#254090=CARTESIAN_POINT('Ctrl Pts',(2.45318471498812,-2.09052620106113,
17.5479980961817));
#254091=CARTESIAN_POINT('Ctrl Pts',(2.48400486706362,-2.05380980503142,
17.5512249111246));
#254092=CARTESIAN_POINT('Ctrl Pts',(2.64301499665363,-1.85556217976798,
17.5683731689268));
#254093=CARTESIAN_POINT('Ctrl Pts',(2.75630799408501,-1.68268168361495,
17.5824200300711));
#254094=CARTESIAN_POINT('Ctrl Pts',(2.86422989469445,-1.47748452604716,
17.5973317919552));
#254095=CARTESIAN_POINT('Ctrl Pts',(2.87588067932428,-1.45467653613732,
17.5989658731962));
#254096=CARTESIAN_POINT('Ctrl Pts',(2.89297326422821,-1.42020727849262,
17.6013978532029));
#254097=CARTESIAN_POINT('Ctrl Pts',(2.89861885385363,-1.40864891807924,
17.6022070814707));
#254098=CARTESIAN_POINT('Ctrl Pts',(2.90870161678703,-1.38768891788807,
17.603662818071));
#254099=CARTESIAN_POINT('Ctrl Pts',(2.91316278873692,-1.37829902619283,
17.6043107503904));
#254100=CARTESIAN_POINT('Ctrl Pts',(2.9222679433687,-1.35889275292914,17.6056409185257));
#254101=CARTESIAN_POINT('Ctrl Pts',(2.92690601132153,-1.34887384738379,
17.606322801986));
#254102=CARTESIAN_POINT('Ctrl Pts',(2.93891563976133,-1.32257767317141,
17.6081003610918));
#254103=CARTESIAN_POINT('Ctrl Pts',(2.94620358698882,-1.30626233825424,
17.6091911138976));
#254104=CARTESIAN_POINT('Ctrl Pts',(2.9789033759737,-1.23139212052146,17.614145026199));
#254105=CARTESIAN_POINT('Ctrl Pts',(3.00270951209356,-1.17214702216034,
17.6179219690615));
#254106=CARTESIAN_POINT('Ctrl Pts',(3.06878763241124,-0.992445624685405,
17.6290646505522));
#254107=CARTESIAN_POINT('Ctrl Pts',(3.10568223115024,-0.870142540775785,
17.6362381785194));
#254108=CARTESIAN_POINT('Ctrl Pts',(3.18966941857093,-0.517152262960961,
17.6565681261711));
#254109=CARTESIAN_POINT('Ctrl Pts',(3.21889482918857,-0.283091292451115,
17.6696624132014));
#254110=CARTESIAN_POINT('Ctrl Pts',(3.2230447656583,-0.00416058469771298,
17.6861864963438));
#254111=CARTESIAN_POINT('Ctrl Pts',(3.22280377362748,0.0396287285173819,
17.6888050265731));
#254112=CARTESIAN_POINT('Ctrl Pts',(3.22108651637423,0.105966463044588,
17.6928151405759));
#254113=CARTESIAN_POINT('Ctrl Pts',(3.22026518119588,0.128527663682848,
17.6941865318673));
#254114=CARTESIAN_POINT('Ctrl Pts',(3.21835765600317,0.1691736914367,17.6966716616179));
#254115=CARTESIAN_POINT('Ctrl Pts',(3.21735586921932,0.187261660894645,
17.6977827357985));
#254116=CARTESIAN_POINT('Ctrl Pts',(3.21488185213883,0.226011734927106,
17.7001744824493));
#254117=CARTESIAN_POINT('Ctrl Pts',(3.21336280870301,0.246669932122547,
17.701456562589));
#254118=CARTESIAN_POINT('Ctrl Pts',(3.20864859130283,0.303309402027997,
17.7049915723206));
#254119=CARTESIAN_POINT('Ctrl Pts',(3.20504752209932,0.339252985407323,
17.7072569776868));
#254120=CARTESIAN_POINT('Ctrl Pts',(3.17465999247405,0.598540196015575,
17.7237645958112));
#254121=CARTESIAN_POINT('Ctrl Pts',(3.12516304193874,0.818559122455604,
17.7387277352509));
#254122=CARTESIAN_POINT('Ctrl Pts',(2.99019542212305,1.21801893674395,17.7671974048475));
#254123=CARTESIAN_POINT('Ctrl Pts',(2.91026122179156,1.39829543549186,17.7805752354162));
#254124=CARTESIAN_POINT('Ctrl Pts',(2.80018069953023,1.59560468903524,17.7951173219205));
#254125=CARTESIAN_POINT('Ctrl Pts',(2.78564201857704,1.62085315623993,17.7969755961859));
#254126=CARTESIAN_POINT('Ctrl Pts',(2.76401902211784,1.65725397830087,17.7996471012775));
#254127=CARTESIAN_POINT('Ctrl Pts',(2.75720581692301,1.66856465277019,17.8004761261338));
#254128=CARTESIAN_POINT('Ctrl Pts',(2.74500158550529,1.68854614677531,17.8019383218671));
#254129=CARTESIAN_POINT('Ctrl Pts',(2.73963861681907,1.69723364729802,17.8025732295041));
#254130=CARTESIAN_POINT('Ctrl Pts',(2.72791163193,1.71602982574597,17.8039450375322));
#254131=CARTESIAN_POINT('Ctrl Pts',(2.72153263148444,1.72612872659547,17.8046809597432));
#254132=CARTESIAN_POINT('Ctrl Pts',(2.70322765242405,1.75475447758592,17.8067644329155));
#254133=CARTESIAN_POINT('Ctrl Pts',(2.69116737660465,1.77319520321267,17.8081035726699));
#254134=CARTESIAN_POINT('Ctrl Pts',(2.59261650338571,1.92056226395534,17.8187929099076));
#254135=CARTESIAN_POINT('Ctrl Pts',(2.4970907871426,2.04322520949682,17.8276194100026));
#254136=CARTESIAN_POINT('Ctrl Pts',(2.21214419093881,2.35913423244255,17.8515379758648));
#254137=CARTESIAN_POINT('Ctrl Pts',(2.00672256738518,2.53616821985772,17.8664297422117));
#254138=CARTESIAN_POINT('Ctrl Pts',(1.75116489487495,2.70571166991323,17.8846457079835));
#254139=CARTESIAN_POINT('Ctrl Pts',(1.72035965033006,2.72540210677262,17.8868347560242));
#254140=CARTESIAN_POINT('Ctrl Pts',(1.66968715060385,2.75659007136546,17.890428595659));
#254141=CARTESIAN_POINT('Ctrl Pts',(1.65001983023987,2.7684072172705,17.8918217730422));
#254142=CARTESIAN_POINT('Ctrl Pts',(1.61457153500309,2.78919446343336,17.8943306737719));
#254143=CARTESIAN_POINT('Ctrl Pts',(1.59883765729354,2.79824322048986,17.8954435097196));
#254144=CARTESIAN_POINT('Ctrl Pts',(1.56519309686511,2.81721624845205,17.897821968735));
#254145=CARTESIAN_POINT('Ctrl Pts',(1.5472626499982,2.82710365608828,17.8990888401014));
#254146=CARTESIAN_POINT('Ctrl Pts',(1.49843256145489,2.85342641127833,17.9025376496282));
#254147=CARTESIAN_POINT('Ctrl Pts',(1.46735813742212,2.86952999092026,17.904731063632));
#254148=CARTESIAN_POINT('Ctrl Pts',(1.2755355418821,2.96500690746804,17.9182675303777));
#254149=CARTESIAN_POINT('Ctrl Pts',(1.10868202814845,3.03134676820635,17.9300533699625));
#254150=CARTESIAN_POINT('Ctrl Pts',(0.772078383168696,3.13365563484924,
17.9536648232202));
#254151=CARTESIAN_POINT('Ctrl Pts',(0.603191002180882,3.17049889863778,
17.9654310779));
#254152=CARTESIAN_POINT('Ctrl Pts',(0.346826190347902,3.20519039019052,
17.9826451653539));
#254153=CARTESIAN_POINT('Ctrl Pts',(0.261049687578217,3.21331441310618,
17.9882947677988));
#254154=CARTESIAN_POINT('Ctrl Pts',(0.154805113255489,3.21909362352279,
17.9950794848238));
#254155=CARTESIAN_POINT('Ctrl Pts',(0.134555860861409,3.22000359451736,
17.9963630267748));
#254156=CARTESIAN_POINT('Ctrl Pts',(0.102737977576258,3.22113276520516,
17.998363460765));
#254157=CARTESIAN_POINT('Ctrl Pts',(0.0911748333047187,3.22148079966251,
17.9990870495901));
#254158=CARTESIAN_POINT('Ctrl Pts',(0.0693165475858998,3.22202091794257,
18.0004481332105));
#254159=CARTESIAN_POINT('Ctrl Pts',(0.0590223576691214,3.22222592986436,
18.001086271458));
#254160=CARTESIAN_POINT('Ctrl Pts',(0.0346314056356175,3.22259475555631,
18.0025917458571));
#254161=CARTESIAN_POINT('Ctrl Pts',(0.0205342981301641,3.22271541595605,
18.0034567202424));
#254162=CARTESIAN_POINT('Ctrl Pts',(-0.0269631770823556,3.22281027926975,
18.0063551317153));
#254163=CARTESIAN_POINT('Ctrl Pts',(-0.0603633991475908,3.2223577648033,
18.0083667228297));
#254164=CARTESIAN_POINT('Ctrl Pts',(-0.142306577188397,3.21997297284797,
18.0132497434561));
#254165=CARTESIAN_POINT('Ctrl Pts',(-0.190825420876284,3.21746223368574,
18.0160960634046));
#254166=CARTESIAN_POINT('Ctrl Pts',(-0.398940866597498,3.20196805962423,
18.0281808549244));
#254167=CARTESIAN_POINT('Ctrl Pts',(-0.557512702577019,3.17819749897144,
18.0370833854247));
#254168=CARTESIAN_POINT('Ctrl Pts',(-0.899483691786537,3.10054096992262,
18.0567327738122));
#254169=CARTESIAN_POINT('Ctrl Pts',(-1.08117002524418,3.0419543006877,18.0674831467215));
#254170=CARTESIAN_POINT('Ctrl Pts',(-1.29804426104915,2.95012261467738,
18.0814221791403));
#254171=CARTESIAN_POINT('Ctrl Pts',(-1.33910664827585,2.93171203144293,
18.084111453524));
#254172=CARTESIAN_POINT('Ctrl Pts',(-1.40040285689572,2.90267303153688,
18.0882088660067));
#254173=CARTESIAN_POINT('Ctrl Pts',(-1.42093212867533,2.89267881630506,
18.0895954617038));
#254174=CARTESIAN_POINT('Ctrl Pts',(-1.45758354693915,2.87435158989831,
18.0920975995986));
#254175=CARTESIAN_POINT('Ctrl Pts',(-1.47374491415386,2.86609887575268,
18.0932103273759));
#254176=CARTESIAN_POINT('Ctrl Pts',(-1.50806819134597,2.84820481673572,
18.0955941043907));
#254177=CARTESIAN_POINT('Ctrl Pts',(-1.52620918206665,2.83852529482359,
18.0968664540015));
#254178=CARTESIAN_POINT('Ctrl Pts',(-1.57530515822351,2.81172235425866,
18.100344530231));
#254179=CARTESIAN_POINT('Ctrl Pts',(-1.60607210872606,2.79426218562843,
18.1025620552704));
#254180=CARTESIAN_POINT('Ctrl Pts',(-1.80221023428528,2.67864470670798,
18.1169499368491));
#254181=CARTESIAN_POINT('Ctrl Pts',(-1.95877594731079,2.56637377176082,
18.1296345684365));
#254182=CARTESIAN_POINT('Ctrl Pts',(-2.25199018614511,2.31357764317786,
18.1556769105649));
#254183=CARTESIAN_POINT('Ctrl Pts',(-2.38775284644008,2.17318699958612,
18.1689847211067));
#254184=CARTESIAN_POINT('Ctrl Pts',(-2.54469862468332,1.97830395846192,
18.1854026417963));
#254185=CARTESIAN_POINT('Ctrl Pts',(-2.57828274893087,1.93433102609601,
18.1889856346784));
#254186=CARTESIAN_POINT('Ctrl Pts',(-2.62103777781216,1.87525683729302,
18.1936193642435));
#254187=CARTESIAN_POINT('Ctrl Pts',(-2.6312386711322,1.86091652856936,18.1947306589211));
#254188=CARTESIAN_POINT('Ctrl Pts',(-2.64761437313051,1.83749185316269,
18.1965231200787));
#254189=CARTESIAN_POINT('Ctrl Pts',(-2.65386095401943,1.8284584283938,18.1972089183166));
#254190=CARTESIAN_POINT('Ctrl Pts',(-2.66601606803106,1.81068692589094,
18.1985471808549));
#254191=CARTESIAN_POINT('Ctrl Pts',(-2.67192805558701,1.80195152212593,
18.1991998513965));
#254192=CARTESIAN_POINT('Ctrl Pts',(-2.68647385832126,1.78023002569174,
18.2008104893122));
#254193=CARTESIAN_POINT('Ctrl Pts',(-2.69505664827311,1.76720978406804,
18.2017651314263));
#254194=CARTESIAN_POINT('Ctrl Pts',(-2.72721350748557,1.71764810096852,
18.2053603173965));
#254195=CARTESIAN_POINT('Ctrl Pts',(-2.75014276367233,1.68069143605924,
18.2079621638664));
#254196=CARTESIAN_POINT('Ctrl Pts',(-2.80810865319885,1.58289928559105,
18.2146738034993));
#254197=CARTESIAN_POINT('Ctrl Pts',(-2.84191908301163,1.52136170477148,
18.2187269178208));
#254198=CARTESIAN_POINT('Ctrl Pts',(-2.98089375547082,1.2475886256167,18.2362361508487));
#254199=CARTESIAN_POINT('Ctrl Pts',(-3.06448938295378,1.02523947877056,
18.2491745562937));
#254200=CARTESIAN_POINT('Ctrl Pts',(-3.14858394382219,0.695197772479143,
18.268710488841));
#254201=CARTESIAN_POINT('Ctrl Pts',(-3.16932841715508,0.593494019285088,
18.2747641589785));
#254202=CARTESIAN_POINT('Ctrl Pts',(-3.18992542040926,0.459873426055491,
18.2828545129448));
#254203=CARTESIAN_POINT('Ctrl Pts',(-3.1942634608599,0.428705719113672,
18.2847509793399));
#254204=CARTESIAN_POINT('Ctrl Pts',(-3.2005745536457,0.377926382253047,
18.2878581487327));
#254205=CARTESIAN_POINT('Ctrl Pts',(-3.20282537718829,0.358350945811895,
18.2890601425752));
#254206=CARTESIAN_POINT('Ctrl Pts',(-3.20672645333371,0.321443763535929,
18.2913347412043));
#254207=CARTESIAN_POINT('Ctrl Pts',(-3.20841605407078,0.304116827648259,
18.2924060738819));
#254208=CARTESIAN_POINT('Ctrl Pts',(-3.21154891869243,0.269049945751382,
18.2945816062546));
#254209=CARTESIAN_POINT('Ctrl Pts',(-3.21298577170707,0.251310049660437,
18.2956859668293));
#254210=CARTESIAN_POINT('Ctrl Pts',(-3.21670070412515,0.200184663514372,
18.2988799647788));
#254211=CARTESIAN_POINT('Ctrl Pts',(-3.21860578846535,0.166775188916709,
18.3009810583889));
#254212=CARTESIAN_POINT('Ctrl Pts',(-3.22185559410359,0.0882983566951195,
18.3059503638159));
#254213=CARTESIAN_POINT('Ctrl Pts',(-3.2227754459306,0.0432216725679329,
18.3088310051166));
#254214=CARTESIAN_POINT('Ctrl Pts',(-3.22274946474069,-0.00185742123099253,
18.3117384119226));
#254215=CARTESIAN_POINT('Origin',(0.,0.,-2.31077344927308));
#254216=CARTESIAN_POINT('',(-3.22274894448647,-0.00260831580021831,19.564226550678));
#254217=CARTESIAN_POINT('',(-3.22275,-3.50678552687464E-13,-2.31077344927308));
#254218=CARTESIAN_POINT('Ctrl Pts',(-3.2227491362909,-0.00235945677226465,
18.5607734492731));
#254219=CARTESIAN_POINT('Ctrl Pts',(-3.22263491557699,-0.158371938722146,
18.5704359656195));
#254220=CARTESIAN_POINT('Ctrl Pts',(-3.21119034460807,-0.313970114175422,
18.5800984819659));
#254221=CARTESIAN_POINT('Ctrl Pts',(-3.1886034015463,-0.467895191412923,
18.5897609983122));
#254222=CARTESIAN_POINT('Ctrl Pts',(-3.17416265308995,-0.56630573397433,
18.5959386367661));
#254223=CARTESIAN_POINT('Ctrl Pts',(-3.15513682808653,-0.664216922908074,
18.60211627522));
#254224=CARTESIAN_POINT('Ctrl Pts',(-3.13157146815107,-0.761168642524225,
18.6082939136738));
#254225=CARTESIAN_POINT('Ctrl Pts',(-3.10803764030761,-0.85799063399059,
18.6144632860174));
#254226=CARTESIAN_POINT('Ctrl Pts',(-3.07997645292916,-0.953855290442885,
18.6206326583609));
#254227=CARTESIAN_POINT('Ctrl Pts',(-3.04748497176422,-1.0483095484499,
18.6268020307045));
#254228=CARTESIAN_POINT('Ctrl Pts',(-3.01502741669461,-1.14266518170832,
18.6329649612761));
#254229=CARTESIAN_POINT('Ctrl Pts',(-2.97814890538086,-1.23561293679921,
18.6391278918476));
#254230=CARTESIAN_POINT('Ctrl Pts',(-2.9369968944381,-1.326712781487,18.6452908224192));
#254231=CARTESIAN_POINT('Ctrl Pts',(-2.89587431896789,-1.41774746369751,
18.6514493447305));
#254232=CARTESIAN_POINT('Ctrl Pts',(-2.85048449945467,-1.50693646966807,
18.6576078670418));
#254233=CARTESIAN_POINT('Ctrl Pts',(-2.80102346763223,-1.59385855591816,
18.6637663893531));
#254234=CARTESIAN_POINT('Ctrl Pts',(-2.75158067595274,-1.68074858721064,
18.6699226405365));
#254235=CARTESIAN_POINT('Ctrl Pts',(-2.69806986956362,-1.76537298367274,
18.67607889172));
#254236=CARTESIAN_POINT('Ctrl Pts',(-2.64073319146657,-1.8473347758289,
18.6822351429034));
#254237=CARTESIAN_POINT('Ctrl Pts',(-2.58340239936084,-1.929288154062,18.6883907621068));
#254238=CARTESIAN_POINT('Ctrl Pts',(-2.52224676498393,-2.00857911631731,
18.6945463813101));
#254239=CARTESIAN_POINT('Ctrl Pts',(-2.45755138823881,-2.08484021849769,
18.7007020005134));
#254240=CARTESIAN_POINT('Ctrl Pts',(-2.39284543631133,-2.16111378640751,
18.7068586259215));
#254241=CARTESIAN_POINT('Ctrl Pts',(-2.32459887311663,-2.23435617990362,
18.7130152513296));
#254242=CARTESIAN_POINT('Ctrl Pts',(-2.25313599070401,-2.30423431314922,
18.7191718767377));
#254243=CARTESIAN_POINT('Ctrl Pts',(-2.18159729072221,-2.37418658264601,
18.7253350339334));
#254244=CARTESIAN_POINT('Ctrl Pts',(-2.10683576834955,-2.44076716120869,
18.7314981911291));
#254245=CARTESIAN_POINT('Ctrl Pts',(-2.02921127881055,-2.50368111956137,
18.7376613483248));
#254246=CARTESIAN_POINT('Ctrl Pts',(-1.95154310885515,-2.56663048050302,
18.7438279736177));
#254247=CARTESIAN_POINT('Ctrl Pts',(-1.87100911233369,-2.62590885520437,
18.7499945989106));
#254248=CARTESIAN_POINT('Ctrl Pts',(-1.78799912244338,-2.68126401173807,
18.7561612242035));
#254249=CARTESIAN_POINT('Ctrl Pts',(-1.70485344079599,-2.73670965422969,
18.7623379297316));
#254250=CARTESIAN_POINT('Ctrl Pts',(-1.61922405341512,-2.78821904617793,
18.7685146352597));
#254251=CARTESIAN_POINT('Ctrl Pts',(-1.53152651426979,-2.83558531851691,
18.7746913407878));
#254252=CARTESIAN_POINT('Ctrl Pts',(-1.47007477354461,-2.86877598629687,
18.7790195045008));
#254253=CARTESIAN_POINT('Ctrl Pts',(-1.4076080480359,-2.8999333021914,18.7833476682138));
#254254=CARTESIAN_POINT('Ctrl Pts',(-1.34427466814874,-2.9290003719825,
18.7876758319268));
#254255=CARTESIAN_POINT('Ctrl Pts',(-1.25402867214141,-2.97041907834217,
18.7938431870539));
#254256=CARTESIAN_POINT('Ctrl Pts',(-1.16170749812771,-3.00773603028649,
18.800010542181));
#254257=CARTESIAN_POINT('Ctrl Pts',(-1.06772021979529,-3.0407385771783,
18.8061778973081));
#254258=CARTESIAN_POINT('Ctrl Pts',(-0.973859503312663,-3.0736966833388,
18.8123369475679));
#254259=CARTESIAN_POINT('Ctrl Pts',(-0.878337548590659,-3.10235178867337,
18.8184959978276));
#254260=CARTESIAN_POINT('Ctrl Pts',(-0.781585685924161,-3.12653824189925,
18.8246550480874));
#254261=CARTESIAN_POINT('Ctrl Pts',(-0.684935410674578,-3.15069929985894,
18.8308076314742));
#254262=CARTESIAN_POINT('Ctrl Pts',(-0.587058214574734,-3.17040092864544,
18.8369602148611));
#254263=CARTESIAN_POINT('Ctrl Pts',(-0.488402038454336,-3.18552680279631,
18.8431127982479));
#254264=CARTESIAN_POINT('Ctrl Pts',(-0.389816478391465,-3.20064185015821,
18.8492609777423));
#254265=CARTESIAN_POINT('Ctrl Pts',(-0.290453475577518,-3.21118758843733,
18.8554091572367));
#254266=CARTESIAN_POINT('Ctrl Pts',(-0.190771749568043,-3.21709864661728,
18.8615573367311));
#254267=CARTESIAN_POINT('Ctrl Pts',(-0.0911267494434237,-3.22300752697738,
18.8677032510428));
#254268=CARTESIAN_POINT('Ctrl Pts',(0.00883630669787303,-3.22428509431965,
18.8738491653544));
#254269=CARTESIAN_POINT('Ctrl Pts',(0.108653885497284,-3.22091786540209,
18.879995079666));
#254270=CARTESIAN_POINT('Ctrl Pts',(0.208461492104258,-3.21755097288473,
18.8861403799752));
#254271=CARTESIAN_POINT('Ctrl Pts',(0.308123215422906,-3.20954022137823,
18.8922856802843));
#254272=CARTESIAN_POINT('Ctrl Pts',(0.407176852162359,-3.19692423644402,
18.8984309805934));
#254273=CARTESIAN_POINT('Ctrl Pts',(0.506247191523591,-3.18430612417726,
18.9045773171354));
#254274=CARTESIAN_POINT('Ctrl Pts',(0.604708809017923,-3.1670812910456,
18.9107236536773));
#254275=CARTESIAN_POINT('Ctrl Pts',(0.702106957157816,-3.14533994716161,
18.9168699902193));
#254276=CARTESIAN_POINT('Ctrl Pts',(0.799610339987803,-3.12357511265044,
18.9230229676249));
#254277=CARTESIAN_POINT('Ctrl Pts',(0.896047533704754,-3.09728411840606,
18.9291759450304));
#254278=CARTESIAN_POINT('Ctrl Pts',(0.990976416704811,-3.06660778451286,
18.935328922436));
#254279=CARTESIAN_POINT('Ctrl Pts',(1.08595950261818,-3.03591393491092,
18.9414854130959));
#254280=CARTESIAN_POINT('Ctrl Pts',(1.17943215562444,-3.0008299124464,18.9476419037557));
#254281=CARTESIAN_POINT('Ctrl Pts',(1.27097176605301,-2.96154492324464,
18.9537983944155));
#254282=CARTESIAN_POINT('Ctrl Pts',(1.36266388336373,-2.92219448443925,
18.959965141916));
#254283=CARTESIAN_POINT('Ctrl Pts',(1.45241613451464,-2.8786292902949,18.9661318894164));
#254284=CARTESIAN_POINT('Ctrl Pts',(1.53982997182799,-2.83108481334633,
18.9722986369169));
#254285=CARTESIAN_POINT('Ctrl Pts',(1.60263494466419,-2.79692512335855,
18.9767293131251));
#254286=CARTESIAN_POINT('Ctrl Pts',(1.66423333746347,-2.76071224339878,
18.9811599893334));
#254287=CARTESIAN_POINT('Ctrl Pts',(1.72448723673025,-2.72254684676949,
18.9855906655416));
#254288=CARTESIAN_POINT('Ctrl Pts',(1.80863382998711,-2.66924758903294,
18.9917782536194));
#254289=CARTESIAN_POINT('Ctrl Pts',(1.89045070208243,-2.61195262486537,
18.9979658416973));
#254290=CARTESIAN_POINT('Ctrl Pts',(1.96953527651378,-2.55089167881895,
19.0041534297751));
#254291=CARTESIAN_POINT('Ctrl Pts',(2.04851354162897,-2.48991281385427,
19.0103327001973));
#254292=CARTESIAN_POINT('Ctrl Pts',(2.1247664712536,-2.42517829223164,19.0165119706195));
#254293=CARTESIAN_POINT('Ctrl Pts',(2.19791893460797,-2.3569620105958,19.0226912410417));
#254294=CARTESIAN_POINT('Ctrl Pts',(2.27099438078598,-2.2888175491715,19.0288640057368));
#254295=CARTESIAN_POINT('Ctrl Pts',(2.34097553693579,-2.217198909505,19.035036770432));
#254296=CARTESIAN_POINT('Ctrl Pts',(2.40751970038534,-2.14242069975915,
19.0412095351271));
#254297=CARTESIAN_POINT('Ctrl Pts',(2.47401488161133,-2.06769753320262,
19.0473777561369));
#254298=CARTESIAN_POINT('Ctrl Pts',(2.53707781468965,-1.98981974315313,
19.0535459771467));
#254299=CARTESIAN_POINT('Ctrl Pts',(2.59640273859391,-1.90913864910908,
19.0597141981565));
#254300=CARTESIAN_POINT('Ctrl Pts',(2.65570498379905,-1.82848839778907,
19.0658800611822));
#254301=CARTESIAN_POINT('Ctrl Pts',(2.71127180405957,-1.74503731985311,
19.0720459242079));
#254302=CARTESIAN_POINT('Ctrl Pts',(2.76283836520404,-1.65916898785407,
19.0782117872335));
#254303=CARTESIAN_POINT('Ctrl Pts',(2.81439882063367,-1.57331082305517,
19.0843769201931));
#254304=CARTESIAN_POINT('Ctrl Pts',(2.86195973645811,-1.48503634368721,
19.0905420531526));
#254305=CARTESIAN_POINT('Ctrl Pts',(2.9053007100739,-1.39475637533732,19.0967071861121));
#254306=CARTESIAN_POINT('Ctrl Pts',(2.94864798825801,-1.30446327446685,
19.1028732158789));
#254307=CARTESIAN_POINT('Ctrl Pts',(2.98777391800282,-1.21216449463458,
19.1090392456457));
#254308=CARTESIAN_POINT('Ctrl Pts',(3.02250540681059,-1.11829272925329,
19.1152052754126));
#254309=CARTESIAN_POINT('Ctrl Pts',(3.05727241787762,-1.02432495482368,
19.121377611598));
#254310=CARTESIAN_POINT('Ctrl Pts',(3.08763586295672,-0.928781388184056,
19.1275499477835));
#254311=CARTESIAN_POINT('Ctrl Pts',(3.11347195787857,-0.832111729279073,
19.1337222839689));
#254312=CARTESIAN_POINT('Ctrl Pts',(3.13932209911106,-0.73538951397717,
19.1398979758686));
#254313=CARTESIAN_POINT('Ctrl Pts',(3.16063989537245,-0.637540409039791,
19.1460736677683));
#254314=CARTESIAN_POINT('Ctrl Pts',(3.17735274297709,-0.539024219489208,
19.152249359668));
#254315=CARTESIAN_POINT('Ctrl Pts',(3.19409213289811,-0.44035157258716,
19.1584348594216));
#254316=CARTESIAN_POINT('Ctrl Pts',(3.20621191430031,-0.341010153933086,
19.1646203591753));
#254317=CARTESIAN_POINT('Ctrl Pts',(3.213691377452,-0.241464889767976,19.1708058589289));
#254318=CARTESIAN_POINT('Ctrl Pts',(3.21881014957514,-0.173338406240326,
19.175039072338));
#254319=CARTESIAN_POINT('Ctrl Pts',(3.2217566198565,-0.105116506468508,
19.1792722857471));
#254320=CARTESIAN_POINT('Ctrl Pts',(3.22253820001393,-0.0369474214390013,
19.1835054991562));
#254321=CARTESIAN_POINT('Ctrl Pts',(3.2236800145404,0.0626411502551009,
19.1896898226938));
#254322=CARTESIAN_POINT('Ctrl Pts',(3.22020294928591,0.162450337127328,
19.1958741462315));
#254323=CARTESIAN_POINT('Ctrl Pts',(3.2120810071948,0.262017491245266,19.2020584697691));
#254324=CARTESIAN_POINT('Ctrl Pts',(3.20396976937468,0.361453421354353,
19.20823464271));
#254325=CARTESIAN_POINT('Ctrl Pts',(3.19122585870917,0.460647525493929,
19.2144108156509));
#254326=CARTESIAN_POINT('Ctrl Pts',(3.17387527688867,0.559136199199179,
19.2205869885917));
#254327=CARTESIAN_POINT('Ctrl Pts',(3.15654249795328,0.657523816780688,
19.2267568243562));
#254328=CARTESIAN_POINT('Ctrl Pts',(3.13461252095266,0.755207019593721,
19.2329266601207));
#254329=CARTESIAN_POINT('Ctrl Pts',(3.10816314671735,0.851727313104451,
19.2390964958852));
#254330=CARTESIAN_POINT('Ctrl Pts',(3.08173213102797,0.948180611750678,
19.2452620491584));
#254331=CARTESIAN_POINT('Ctrl Pts',(3.05078806917497,1.04347219025267,19.2514276024317));
#254332=CARTESIAN_POINT('Ctrl Pts',(3.01545965903013,1.1371546100957,19.2575931557049));
#254333=CARTESIAN_POINT('Ctrl Pts',(2.98014383587855,1.23080365226953,19.2637565122822));
#254334=CARTESIAN_POINT('Ctrl Pts',(2.94044692111502,1.32284427106072,19.2699198688594));
#254335=CARTESIAN_POINT('Ctrl Pts',(2.89654692491375,1.41284587774914,19.2760832254367));
#254336=CARTESIAN_POINT('Ctrl Pts',(2.85265096692754,1.50283920548822,19.2822460150672));
#254337=CARTESIAN_POINT('Ctrl Pts',(2.80455288589184,1.59079350559452,19.2884088046977));
#254338=CARTESIAN_POINT('Ctrl Pts',(2.7524777063539,1.67630070050834,19.2945715943282));
#254339=CARTESIAN_POINT('Ctrl Pts',(2.70039355390231,1.76182262890334,19.30073544585));
#254340=CARTESIAN_POINT('Ctrl Pts',(2.64433116641951,1.84489624523154,19.3068992973718));
#254341=CARTESIAN_POINT('Ctrl Pts',(2.58455962065447,1.92514132722313,19.3130631488936));
#254342=CARTESIAN_POINT('Ctrl Pts',(2.52472435288427,2.00547195790622,19.3192335716521));
#254343=CARTESIAN_POINT('Ctrl Pts',(2.46117228960451,2.08296768566591,19.3254039944107));
#254344=CARTESIAN_POINT('Ctrl Pts',(2.39421357354202,2.15728044694406,19.3315744171692));
#254345=CARTESIAN_POINT('Ctrl Pts',(2.3272168682355,2.23163536980755,19.3377483407371));
#254346=CARTESIAN_POINT('Ctrl Pts',(2.25680996467729,2.30280342221827,19.3439222643049));
#254347=CARTESIAN_POINT('Ctrl Pts',(2.1833392719104,2.37047404251423,19.3500961878727));
#254348=CARTESIAN_POINT('Ctrl Pts',(2.10974889556082,2.43825489808871,19.3562801687473));
#254349=CARTESIAN_POINT('Ctrl Pts',(2.03308509281522,2.50252666436514,19.3624641496219));
#254350=CARTESIAN_POINT('Ctrl Pts',(1.95372675394799,2.56301957335636,19.3686481304964));
#254351=CARTESIAN_POINT('Ctrl Pts',(1.89909200346803,2.6046662992798,19.3729055312545));
#254352=CARTESIAN_POINT('Ctrl Pts',(1.84318076274415,2.64452283837463,19.3771629320126));
#254353=CARTESIAN_POINT('Ctrl Pts',(1.7861237533846,2.6825136532915,19.3814203327707));
#254354=CARTESIAN_POINT('Ctrl Pts',(1.70423945491699,2.73703545986005,19.3875302617398));
#254355=CARTESIAN_POINT('Ctrl Pts',(1.61969680972089,2.78791060612936,19.3936401907088));
#254356=CARTESIAN_POINT('Ctrl Pts',(1.53285811260511,2.83486570565886,19.3997501196778));
#254357=CARTESIAN_POINT('Ctrl Pts',(1.44613776612968,2.88175681106729,19.4058517215527));
#254358=CARTESIAN_POINT('Ctrl Pts',(1.35712797066862,2.92473827409539,19.4119533234276));
#254359=CARTESIAN_POINT('Ctrl Pts',(1.26622081447294,2.963579324313,19.4180549253025));
#254360=CARTESIAN_POINT('Ctrl Pts',(1.1754093790248,3.00237947682225,19.4241501024918));
#254361=CARTESIAN_POINT('Ctrl Pts',(1.08270495831135,3.03704770620832,19.4302452796812));
#254362=CARTESIAN_POINT('Ctrl Pts',(0.988524154686375,3.06739915206704,
19.4363404568705));
#254363=CARTESIAN_POINT('Ctrl Pts',(0.894407107911653,3.09773005114219,
19.4424315078549));
#254364=CARTESIAN_POINT('Ctrl Pts',(0.798816084730114,3.12374983613484,
19.4485225588393));
#254365=CARTESIAN_POINT('Ctrl Pts',(0.702186646086671,3.14532215783337,
19.4546136098237));
#254366=CARTESIAN_POINT('Ctrl Pts',(0.605590349578068,3.16688708061905,
19.4607025716887));
#254367=CARTESIAN_POINT('Ctrl Pts',(0.507956777553867,3.18400747241715,
19.4667915335537));
#254368=CARTESIAN_POINT('Ctrl Pts',(0.409734566881214,3.19659743277171,
19.4728804954187));
#254369=CARTESIAN_POINT('Ctrl Pts',(0.311518511539175,3.20918660414618,
19.4789690757042));
#254370=CARTESIAN_POINT('Ctrl Pts',(0.212714331128225,3.2172458517047,19.4850576559898));
#254371=CARTESIAN_POINT('Ctrl Pts',(0.11377758964899,3.22074094310512,19.4911462362754));
#254372=CARTESIAN_POINT('Ctrl Pts',(0.0148193130990093,3.22423679526479,
19.4972361418321));
#254373=CARTESIAN_POINT('Ctrl Pts',(-0.084271138243295,3.22316650286517,
19.5033260473889));
#254374=CARTESIAN_POINT('Ctrl Pts',(-0.183037525869199,3.21754795249794,
19.5094159529456));
#254375=CARTESIAN_POINT('Ctrl Pts',(-0.281924322382909,3.21192255239755,
19.5155132828779));
#254376=CARTESIAN_POINT('Ctrl Pts',(-0.380485822456895,3.20173784935418,
19.5216106128101));
#254377=CARTESIAN_POINT('Ctrl Pts',(-0.478270400625576,3.18706369349366,
19.5277079427424));
#254378=CARTESIAN_POINT('Ctrl Pts',(-0.576116712843525,3.17238027344161,
19.533809122084));
#254379=CARTESIAN_POINT('Ctrl Pts',(-0.673184692280438,3.15320184736592,
19.5399103014256));
#254380=CARTESIAN_POINT('Ctrl Pts',(-0.769034697704354,3.12964905320497,
19.5460114807672));
#254381=CARTESIAN_POINT('Ctrl Pts',(-0.865063614285654,3.1060522960036,
19.5521240484134));
#254382=CARTESIAN_POINT('Ctrl Pts',(-0.959869591586191,3.07806499120141,
19.5582366160596));
#254383=CARTESIAN_POINT('Ctrl Pts',(-1.0530297578369,3.04585716861608,19.5643491837058));
#254384=CARTESIAN_POINT('Ctrl Pts',(-1.1291623379385,3.01953621265861,19.5693445112656));
#254385=CARTESIAN_POINT('Ctrl Pts',(-1.20419602804471,2.99039753654828,
19.5743398388255));
#254386=CARTESIAN_POINT('Ctrl Pts',(-1.27791235770485,2.95855666981811,
19.5793351663853));
#254387=CARTESIAN_POINT('Ctrl Pts',(-1.37157794975161,2.91809896326499,
19.5856823396035));
#254388=CARTESIAN_POINT('Ctrl Pts',(-1.46345307865358,2.87313197893506,
19.5920295128216));
#254389=CARTESIAN_POINT('Ctrl Pts',(-1.55308779875617,2.82383353826934,
19.5983766860398));
#254390=CARTESIAN_POINT('Ctrl Pts',(-1.64258957084072,2.77460821804145,
19.604714445003));
#254391=CARTESIAN_POINT('Ctrl Pts',(-1.72985719519464,2.72106442031479,
19.6110522039663));
#254392=CARTESIAN_POINT('Ctrl Pts',(-1.8144617058491,2.66342754369387,19.6173899629296));
#254393=CARTESIAN_POINT('Ctrl Pts',(-1.90337904692538,2.60285254860875,
19.6240507978075));
#254394=CARTESIAN_POINT('Ctrl Pts',(-1.98935416775711,2.53775630464971,
19.6307116326855));
#254395=CARTESIAN_POINT('Ctrl Pts',(-2.07191849325825,2.46845524970466,
19.6373724675634));
#254396=CARTESIAN_POINT('Ctrl Pts',(-2.15028314560458,2.4026792254346,19.6436944959501));
#254397=CARTESIAN_POINT('Ctrl Pts',(-2.22557506805531,2.33311589840458,
19.6500165243368));
#254398=CARTESIAN_POINT('Ctrl Pts',(-2.29742423981357,2.26007951736594,
19.6563385527235));
#254399=CARTESIAN_POINT('Ctrl Pts',(-2.36922414243632,2.18709321956788,
19.6626562459054));
#254400=CARTESIAN_POINT('Ctrl Pts',(-2.43758570973843,2.11063889506989,
19.6689739390873));
#254401=CARTESIAN_POINT('Ctrl Pts',(-2.50217437088175,2.03106892551743,
19.6752916322692));
#254402=CARTESIAN_POINT('Ctrl Pts',(-2.56673232691967,1.95153678310457,
19.6816063220534));
#254403=CARTESIAN_POINT('Ctrl Pts',(-2.62752069280269,1.86889225787235,
19.6879210118376));
#254404=CARTESIAN_POINT('Ctrl Pts',(-2.68424435865614,1.78352173676765,
19.6942357016218));
#254405=CARTESIAN_POINT('Ctrl Pts',(-2.74095298125601,1.69817385613193,
19.700548716735));
#254406=CARTESIAN_POINT('Ctrl Pts',(-2.79359882727932,1.61010175635542,
19.7068617318482));
#254407=CARTESIAN_POINT('Ctrl Pts',(-2.84192976801594,1.51972127581504,
19.7131747469614));
#254408=CARTESIAN_POINT('Ctrl Pts',(-2.89027069290591,1.42932212457295,
19.7194890662104));
#254409=CARTESIAN_POINT('Ctrl Pts',(-2.93429473679977,1.3366139946142,19.7258033854594));
#254410=CARTESIAN_POINT('Ctrl Pts',(-2.97379558060105,1.24203760301276,
19.7321177047084));
#254411=CARTESIAN_POINT('Ctrl Pts',(-3.01330036367614,1.14745177965577,
19.7384326536612));
#254412=CARTESIAN_POINT('Ctrl Pts',(-3.04828089850386,1.05099769957376,
19.7447476026141));
#254413=CARTESIAN_POINT('Ctrl Pts',(-3.07857931707185,0.953135326696814,
19.7510625515669));
#254414=CARTESIAN_POINT('Ctrl Pts',(-3.1088972785572,0.855209831176631,
19.757381573753));
#254415=CARTESIAN_POINT('Ctrl Pts',(-3.13452697951299,0.755874617500144,
19.7637005959391));
#254416=CARTESIAN_POINT('Ctrl Pts',(-3.15536069062618,0.655603900652743,
19.7700196181251));
#254417=CARTESIAN_POINT('Ctrl Pts',(-3.16330684024571,0.617359820459896,
19.7724297454168));
#254418=CARTESIAN_POINT('Ctrl Pts',(-3.17055583629552,0.578979757896498,
19.7748398727084));
#254419=CARTESIAN_POINT('Ctrl Pts',(-3.1771036721075,0.54049035068261,19.77725));
#254420=CARTESIAN_POINT('Ctrl Pts',(-3.22274955323411,-0.00169694707575843,
18.3142265507618));
#254421=CARTESIAN_POINT('Ctrl Pts',(-3.22269119943203,-0.112519312871419,
18.3210373034113));
#254422=CARTESIAN_POINT('Ctrl Pts',(-3.21691235126228,-0.223143969137743,
18.3278480560609));
#254423=CARTESIAN_POINT('Ctrl Pts',(-3.20549873162767,-0.333009675585234,
18.3346588087104));
#254424=CARTESIAN_POINT('Ctrl Pts',(-3.19404741079341,-0.44323828784753,
18.3414920584777));
#254425=CARTESIAN_POINT('Ctrl Pts',(-3.17692415128044,-0.552702677011318,
18.3483253082451));
#254426=CARTESIAN_POINT('Ctrl Pts',(-3.15426565045729,-0.660852304864885,
18.3551585580124));
#254427=CARTESIAN_POINT('Ctrl Pts',(-3.13149845498245,-0.769520735185664,
18.3620245874287));
#254428=CARTESIAN_POINT('Ctrl Pts',(-3.10314290388034,-0.876861513512687,
18.368890616845));
#254429=CARTESIAN_POINT('Ctrl Pts',(-3.06938641079325,-0.982336308876813,
18.3757566462613));
#254430=CARTESIAN_POINT('Ctrl Pts',(-3.04138582663005,-1.06982631789733,
18.3814519308409));
#254431=CARTESIAN_POINT('Ctrl Pts',(-3.00967004785188,-1.15603274305358,
18.3871472154204));
#254432=CARTESIAN_POINT('Ctrl Pts',(-2.97437034114833,-1.24066056445636,
18.3928425));
#254433=CARTESIAN_POINT('Ctrl Pts',(-2.93607974300623,-1.33245877479811,
18.3990203375376));
#254434=CARTESIAN_POINT('Ctrl Pts',(-2.89346925596554,-1.42264127094073,
18.4051981750752));
#254435=CARTESIAN_POINT('Ctrl Pts',(-2.84669655593796,-1.51077340488605,
18.4113760126129));
#254436=CARTESIAN_POINT('Ctrl Pts',(-2.79998654716334,-1.59878741193469,
18.4175455697567));
#254437=CARTESIAN_POINT('Ctrl Pts',(-2.74912561595544,-1.68475613980992,
18.4237151269005));
#254438=CARTESIAN_POINT('Ctrl Pts',(-2.69431962895281,-1.768264488005,18.4298846840443));
#254439=CARTESIAN_POINT('Ctrl Pts',(-2.63957099284961,-1.85168545014719,
18.436047785148));
#254440=CARTESIAN_POINT('Ctrl Pts',(-2.5808857453445,-1.93265079106924,
18.4422108862517));
#254441=CARTESIAN_POINT('Ctrl Pts',(-2.51851537038606,-2.01077047213976,
18.4483739873553));
#254442=CARTESIAN_POINT('Ctrl Pts',(-2.45618985016622,-2.08883397208461,
18.4545326561578));
#254443=CARTESIAN_POINT('Ctrl Pts',(-2.39018474155369,-2.164055543465,18.4606913249603));
#254444=CARTESIAN_POINT('Ctrl Pts',(-2.32079396422091,-2.23607534267873,
18.4668499937628));
#254445=CARTESIAN_POINT('Ctrl Pts',(-2.25142893072578,-2.30806842269304,
18.4730063777116));
#254446=CARTESIAN_POINT('Ctrl Pts',(-2.17868102495851,-2.37686177917559,
18.4791627616604));
#254447=CARTESIAN_POINT('Ctrl Pts',(-2.10288286258792,-2.44213046922846,
18.4853191456092));
#254448=CARTESIAN_POINT('Ctrl Pts',(-2.02709265060043,-2.50739231332263,
18.491474883822));
#254449=CARTESIAN_POINT('Ctrl Pts',(-1.94825314665773,-2.56912994328705,
18.4976306220347));
#254450=CARTESIAN_POINT('Ctrl Pts',(-1.86673131002766,-2.62705762758688,
18.5037863602474));
#254451=CARTESIAN_POINT('Ctrl Pts',(-1.78519633072657,-2.68499465078938,
18.5099430908671));
#254452=CARTESIAN_POINT('Ctrl Pts',(-1.70097851313821,-2.73912025719183,
18.5160998214869));
#254453=CARTESIAN_POINT('Ctrl Pts',(-1.61447431948844,-2.78919168115286,
18.5222565521066));
#254454=CARTESIAN_POINT('Ctrl Pts',(-1.52787882874598,-2.83931595082278,
18.5284197805802));
#254455=CARTESIAN_POINT('Ctrl Pts',(-1.43899251942865,-2.88537727666669,
18.5345830090537));
#254456=CARTESIAN_POINT('Ctrl Pts',(-1.34823689880374,-2.92717864627427,
18.5407462375273));
#254457=CARTESIAN_POINT('Ctrl Pts',(-1.25743037763656,-2.96900346029627,
18.5469129226647));
#254458=CARTESIAN_POINT('Ctrl Pts',(-1.16475285886501,-3.00656339701394,
18.5530796078021));
#254459=CARTESIAN_POINT('Ctrl Pts',(-1.07064436653945,-3.03971021692815,
18.5592462929395));
#254460=CARTESIAN_POINT('Ctrl Pts',(-0.976382816372253,-3.07291094675619,
18.5654230075598));
#254461=CARTESIAN_POINT('Ctrl Pts',(-0.880686059437438,-3.10168409941806,
18.5715997221801));
#254462=CARTESIAN_POINT('Ctrl Pts',(-0.784007844963939,-3.12593174294241,
18.5777764368005));
#254463=CARTESIAN_POINT('Ctrl Pts',(-0.717024589148058,-3.14273166128978,
18.582055957867));
#254464=CARTESIAN_POINT('Ctrl Pts',(-0.649570441744555,-3.15736023489492,
18.5863354789335));
#254465=CARTESIAN_POINT('Ctrl Pts',(-0.581797922398236,-3.16979947946129,
18.5906150000001));
#254466=CARTESIAN_POINT('Ctrl Pts',(-0.483956754347427,-3.18775764642606,
18.5967932171283));
#254467=CARTESIAN_POINT('Ctrl Pts',(-0.385114911041173,-3.2012124448069,
18.6029714342565));
#254468=CARTESIAN_POINT('Ctrl Pts',(-0.285722838716668,-3.21005919290216,
18.6091496513847));
#254469=CARTESIAN_POINT('Ctrl Pts',(-0.18646356636356,-3.21889412065938,
18.6153196136588));
#254470=CARTESIAN_POINT('Ctrl Pts',(-0.0866559543274809,-3.22313319840321,
18.621489575933));
#254471=CARTESIAN_POINT('Ctrl Pts',(0.0132396819434576,-3.22272280429485,
18.6276595382071));
#254472=CARTESIAN_POINT('Ctrl Pts',(0.11303118964346,-3.22231283797046,
18.6338230690756));
#254473=CARTESIAN_POINT('Ctrl Pts',(0.212910108083359,-3.21726303748307,
18.6399865999441));
#254474=CARTESIAN_POINT('Ctrl Pts',(0.312412277492494,-3.20757168764347,
18.6461501308126));
#254475=CARTESIAN_POINT('Ctrl Pts',(0.411843453749759,-3.19788725242166,
18.6523092641038));
#254476=CARTESIAN_POINT('Ctrl Pts',(0.510897985349236,-3.18356789422133,
18.6584683973949));
#254477=CARTESIAN_POINT('Ctrl Pts',(0.609113902321486,-3.16466393421145,
18.6646275306861));
#254478=CARTESIAN_POINT('Ctrl Pts',(0.707293721249057,-3.1457669221181,
18.6707844002641));
#254479=CARTESIAN_POINT('Ctrl Pts',(0.80463511292835,-3.12228873843662,
18.6769412698421));
#254480=CARTESIAN_POINT('Ctrl Pts',(0.900684282413903,-3.09433116939874,
18.6830981394201));
#254481=CARTESIAN_POINT('Ctrl Pts',(0.996723696617756,-3.06637643988526,
18.6892543836725));
#254482=CARTESIAN_POINT('Ctrl Pts',(1.0914707335095,-3.03394335079898,18.695410627925));
#254483=CARTESIAN_POINT('Ctrl Pts',(1.1844857581927,-2.99718385340951,18.7015668721774));
#254484=CARTESIAN_POINT('Ctrl Pts',(1.27751607481518,-2.96041831265226,
18.7077241285343));
#254485=CARTESIAN_POINT('Ctrl Pts',(1.36881341055787,-2.91932511002519,
18.7138813848911));
#254486=CARTESIAN_POINT('Ctrl Pts',(1.45795807544929,-2.8741043496596,18.7200386412479));
#254487=CARTESIAN_POINT('Ctrl Pts',(1.54719720423113,-2.82883567022944,
18.7262024222621));
#254488=CARTESIAN_POINT('Ctrl Pts',(1.63427872009203,-2.7794308958885,18.7323662032762));
#254489=CARTESIAN_POINT('Ctrl Pts',(1.71880764188016,-2.72613606643439,
18.7385299842904));
#254490=CARTESIAN_POINT('Ctrl Pts',(1.80338418411655,-2.67281121265707,
18.7446972377493));
#254491=CARTESIAN_POINT('Ctrl Pts',(1.88540491295446,-2.61559218715906,
18.7508644912082));
#254492=CARTESIAN_POINT('Ctrl Pts',(1.96450564697361,-2.55476713723752,
18.7570317446672));
#254493=CARTESIAN_POINT('Ctrl Pts',(2.04373526782585,-2.49384297890499,
18.7632090470565));
#254494=CARTESIAN_POINT('Ctrl Pts',(2.12003506016258,-2.42930134066297,
18.7693863494458));
#254495=CARTESIAN_POINT('Ctrl Pts',(2.1930755387374,-2.36146929768136,18.7755636518351));
#254496=CARTESIAN_POINT('Ctrl Pts',(2.24361863711628,-2.31453037164257,
18.7798382678901));
#254497=CARTESIAN_POINT('Ctrl Pts',(2.29260178746872,-2.26601663405651,
18.784112883945));
#254498=CARTESIAN_POINT('Ctrl Pts',(2.33992711965106,-2.21604572092308,
18.7883875));
#254499=CARTESIAN_POINT('Ctrl Pts',(2.40821357708754,-2.14394191360905,
18.7945554099509));
#254500=CARTESIAN_POINT('Ctrl Pts',(2.47328428732285,-2.06855195506756,
18.8007233199017));
#254501=CARTESIAN_POINT('Ctrl Pts',(2.53480618406806,-1.99019475723114,
18.8068912298526));
#254502=CARTESIAN_POINT('Ctrl Pts',(2.59624535620559,-1.91194292136816,
18.8130508462046));
#254503=CARTESIAN_POINT('Ctrl Pts',(2.65414493297046,-1.83073211545638,
18.8192104625566));
#254504=CARTESIAN_POINT('Ctrl Pts',(2.70820918384563,-1.74691745054946,
18.8253700789086));
#254505=CARTESIAN_POINT('Ctrl Pts',(2.76221676533419,-1.66319063899427,
18.8315232388375));
#254506=CARTESIAN_POINT('Ctrl Pts',(2.81239677867969,-1.57686575804496,
18.8376763987664));
#254507=CARTESIAN_POINT('Ctrl Pts',(2.85849484813504,-1.48832952187527,
18.8438295586953));
#254508=CARTESIAN_POINT('Ctrl Pts',(2.90456000676338,-1.39985649444264,
18.8499783256944));
#254509=CARTESIAN_POINT('Ctrl Pts',(2.94654881483495,-1.30917563511837,
18.8561270926935));
#254510=CARTESIAN_POINT('Ctrl Pts',(2.98425166953833,-1.21670026520819,
18.8622758596926));
#254511=CARTESIAN_POINT('Ctrl Pts',(3.02194068156101,-1.12425884782043,
18.8684223691592));
#254512=CARTESIAN_POINT('Ctrl Pts',(3.05534670282206,-1.03002463133725,
18.8745688786259));
#254513=CARTESIAN_POINT('Ctrl Pts',(3.08430770680721,-0.9344321977702,18.8807153880925));
#254514=CARTESIAN_POINT('Ctrl Pts',(3.11326585052714,-0.838849205164271,
18.8868612905137));
#254515=CARTESIAN_POINT('Ctrl Pts',(3.13777972369421,-0.741908678491949,
18.8930071929348));
#254516=CARTESIAN_POINT('Ctrl Pts',(3.15773706262155,-0.64406071596259,
18.899153095356));
#254517=CARTESIAN_POINT('Ctrl Pts',(3.17769778682209,-0.546196155925537,
18.9053000402788));
#254518=CARTESIAN_POINT('Ctrl Pts',(3.19310035465664,-0.447424280537048,
18.9114469852016));
#254519=CARTESIAN_POINT('Ctrl Pts',(3.2038837406487,-0.348204737054074,
18.9175939301244));
#254520=CARTESIAN_POINT('Ctrl Pts',(3.21467876505075,-0.248878106824262,
18.9237475093886));
#254521=CARTESIAN_POINT('Ctrl Pts',(3.2208446059332,-0.149103276992905,
18.9299010886529));
#254522=CARTESIAN_POINT('Ctrl Pts',(3.22237221764993,-0.0493442338867971,
18.9360546679172));
#254523=CARTESIAN_POINT('Ctrl Pts',(3.22390070271224,0.0504718421146573,
18.9422117652229));
#254524=CARTESIAN_POINT('Ctrl Pts',(3.2207856918871,0.150271678729752,18.9483688625286));
#254525=CARTESIAN_POINT('Ctrl Pts',(3.21307023060905,0.249594181971336,
18.9545259598343));
#254526=CARTESIAN_POINT('Ctrl Pts',(3.20534195516567,0.349081644238824,
18.9606932831083));
#254527=CARTESIAN_POINT('Ctrl Pts',(3.19299802298441,0.448089758120606,
18.9668606063823));
#254528=CARTESIAN_POINT('Ctrl Pts',(3.17613302734705,0.546165318466194,
18.9730279296563));
#254529=CARTESIAN_POINT('Ctrl Pts',(3.16416282573154,0.615776023154999,
18.9774052864375));
#254530=CARTESIAN_POINT('Ctrl Pts',(3.14991613980794,0.684917140423283,
18.9817826432187));
#254531=CARTESIAN_POINT('Ctrl Pts',(3.13344196559922,0.753431490396909,
18.9861599999999));
#254532=CARTESIAN_POINT('Ctrl Pts',(3.11015303936351,0.85028767404578,18.9923481061771));
#254533=CARTESIAN_POINT('Ctrl Pts',(3.08232946493969,0.946227958167857,
18.9985362123543));
#254534=CARTESIAN_POINT('Ctrl Pts',(3.05005884314237,1.04079710600531,19.0047243185314));
#254535=CARTESIAN_POINT('Ctrl Pts',(3.01783153905458,1.13523931117331,19.0109041182499));
#254536=CARTESIAN_POINT('Ctrl Pts',(2.98116919236648,1.22831363344948,19.0170839179684));
#254537=CARTESIAN_POINT('Ctrl Pts',(2.94021006787556,1.31957656816996,19.023263717687));
#254538=CARTESIAN_POINT('Ctrl Pts',(2.89929399412784,1.41074357952256,19.0294370220281));
#254539=CARTESIAN_POINT('Ctrl Pts',(2.85409029833497,1.50010259697893,19.0356103263692));
#254540=CARTESIAN_POINT('Ctrl Pts',(2.80478624091127,1.587227679098,19.0417836307103));
#254541=CARTESIAN_POINT('Ctrl Pts',(2.75551838527931,1.67428878911737,19.0479524022667));
#254542=CARTESIAN_POINT('Ctrl Pts',(2.70215636711459,1.75911885081006,19.0541211738231));
#254543=CARTESIAN_POINT('Ctrl Pts',(2.64493411252976,1.84131504715419,19.0602899453795));
#254544=CARTESIAN_POINT('Ctrl Pts',(2.58773366141699,1.92347992417188,19.0664563664407));
#254545=CARTESIAN_POINT('Ctrl Pts',(2.52667614353655,2.00301257626303,19.0726227875018));
#254546=CARTESIAN_POINT('Ctrl Pts',(2.46203921655881,2.07953852059212,19.078789208563));
#254547=CARTESIAN_POINT('Ctrl Pts',(2.39740987128964,2.15605548866825,19.0849549063223));
#254548=CARTESIAN_POINT('Ctrl Pts',(2.32920223054317,2.22956612039436,19.0911206040816));
#254549=CARTESIAN_POINT('Ctrl Pts',(2.257734082123,2.29972919643166,19.0972863018409));
#254550=CARTESIAN_POINT('Ctrl Pts',(2.18625546851525,2.36990254655285,19.1034529024526));
#254551=CARTESIAN_POINT('Ctrl Pts',(2.11151570713167,2.43672706475663,19.1096195030642));
#254552=CARTESIAN_POINT('Ctrl Pts',(2.03386854812448,2.49989925626015,19.1157861036759));
#254553=CARTESIAN_POINT('Ctrl Pts',(1.95614206139006,2.5631359872322,19.1219590043559));
#254554=CARTESIAN_POINT('Ctrl Pts',(1.87550258139099,2.62271266746531,19.1281319050359));
#254555=CARTESIAN_POINT('Ctrl Pts',(1.79233586273541,2.67836698711221,19.1343048057159));
#254556=CARTESIAN_POINT('Ctrl Pts',(1.70912387208835,2.73405160231392,19.1404810666284));
#254557=CARTESIAN_POINT('Ctrl Pts',(1.62338227227255,2.78580938069555,19.1466573275408));
#254558=CARTESIAN_POINT('Ctrl Pts',(1.53552289710391,2.83342319376573,19.1528335884533));
#254559=CARTESIAN_POINT('Ctrl Pts',(1.44752442554782,2.88111238762913,19.159019627441));
#254560=CARTESIAN_POINT('Ctrl Pts',(1.35740187087157,2.92464432432897,19.1652056664287));
#254561=CARTESIAN_POINT('Ctrl Pts',(1.26558865316282,2.96384934223815,19.1713917054164));
#254562=CARTESIAN_POINT('Ctrl Pts',(1.20354514381144,2.99034244373238,19.1755719702777));
#254563=CARTESIAN_POINT('Ctrl Pts',(1.14072999841011,3.01486067514458,19.1797522351389));
#254564=CARTESIAN_POINT('Ctrl Pts',(1.07728058697486,3.03736466355739,19.1839325000001));
#254565=CARTESIAN_POINT('Ctrl Pts',(0.983403360390098,3.07066067011604,
19.1901174536928));
#254566=CARTESIAN_POINT('Ctrl Pts',(0.88782340821703,3.09965626757547,19.1963024073856));
#254567=CARTESIAN_POINT('Ctrl Pts',(0.790970226279181,3.12417727788291,
19.2024873610783));
#254568=CARTESIAN_POINT('Ctrl Pts',(0.69424450171438,3.14866601889887,19.2086641754623));
#254569=CARTESIAN_POINT('Ctrl Pts',(0.596249293724536,3.16869177320447,
19.2148409898464));
#254570=CARTESIAN_POINT('Ctrl Pts',(0.497431809052479,3.18412926211277,
19.2210178042304));
#254571=CARTESIAN_POINT('Ctrl Pts',(0.39871554260407,3.19955093848333,19.2271882917363));
#254572=CARTESIAN_POINT('Ctrl Pts',(0.299179099001634,3.21039362789837,
19.2333587792422));
#254573=CARTESIAN_POINT('Ctrl Pts',(0.199281591826288,3.21658272234046,
19.2395292667481));
#254574=CARTESIAN_POINT('Ctrl Pts',(0.0994532499881565,3.2227675316826,
19.2456954820368));
#254575=CARTESIAN_POINT('Ctrl Pts',(-0.000735228215647935,3.224305125701,
19.2518616973255));
#254576=CARTESIAN_POINT('Ctrl Pts',(-0.100818739265824,3.22117263497517,
19.2580279126142));
#254577=CARTESIAN_POINT('Ctrl Pts',(-0.200866711603791,3.21804125656729,
19.264191938338));
#254578=CARTESIAN_POINT('Ctrl Pts',(-0.300809359324772,3.21024310247892,
19.2703559640617));
#254579=CARTESIAN_POINT('Ctrl Pts',(-0.400181583041801,3.19780741494765,
19.2765199897854));
#254580=CARTESIAN_POINT('Ctrl Pts',(-0.499544768059179,3.18537285854176,
19.2826834548417));
#254581=CARTESIAN_POINT('Ctrl Pts',(-0.598337203424098,3.1683016612416,
19.2888469198979));
#254582=CARTESIAN_POINT('Ctrl Pts',(-0.6960998926732,3.14667483256856,19.2950103849541));
#254583=CARTESIAN_POINT('Ctrl Pts',(-0.793879511426865,3.12504425879094,
19.3011749173338));
#254584=CARTESIAN_POINT('Ctrl Pts',(-0.890628607825077,3.09885657975683,
19.3073394497134));
#254585=CARTESIAN_POINT('Ctrl Pts',(-0.985900301681989,3.06824349712394,
19.3135039820931));
#254586=CARTESIAN_POINT('Ctrl Pts',(-1.08127342630268,3.03759782235138,
19.3196750775263));
#254587=CARTESIAN_POINT('Ctrl Pts',(-1.17516559543678,3.0025174686337,19.3258461729595));
#254588=CARTESIAN_POINT('Ctrl Pts',(-1.26714708413827,2.96318339453701,
19.3320172683927));
#254589=CARTESIAN_POINT('Ctrl Pts',(-1.35918080956772,2.92382698243126,
19.3381918684206));
#254590=CARTESIAN_POINT('Ctrl Pts',(-1.4493013044587,2.8802122268692,19.3443664684484));
#254591=CARTESIAN_POINT('Ctrl Pts',(-1.53710260306726,2.83256653057679,
19.3505410684763));
#254592=CARTESIAN_POINT('Ctrl Pts',(-1.62504645148955,2.78484347910583,
19.3567256932771));
#254593=CARTESIAN_POINT('Ctrl Pts',(-1.71066321323486,2.73307663927585,
19.3629103180779));
#254594=CARTESIAN_POINT('Ctrl Pts',(-1.79357502569557,2.67753733675203,
19.3690949428787));
#254595=CARTESIAN_POINT('Ctrl Pts',(-1.84992566537771,2.63979030008943,
19.3732982952525));
#254596=CARTESIAN_POINT('Ctrl Pts',(-1.90502747139949,2.60030158584876,
19.3775016476262));
#254597=CARTESIAN_POINT('Ctrl Pts',(-1.95877093229023,2.55916666071494,
19.381705));
#254598=CARTESIAN_POINT('Ctrl Pts',(-2.03613542261648,2.49995234022197,
19.3877557866198));
#254599=CARTESIAN_POINT('Ctrl Pts',(-2.11097584776025,2.43710122137895,
19.3938065732395));
#254600=CARTESIAN_POINT('Ctrl Pts',(-2.18291996081745,2.37086018296414,
19.3998573598593));
#254601=CARTESIAN_POINT('Ctrl Pts',(-2.25476589126913,2.30470954413128,
19.4058998889307));
#254602=CARTESIAN_POINT('Ctrl Pts',(-2.32372302892345,2.23517847506401,
19.411942418002));
#254603=CARTESIAN_POINT('Ctrl Pts',(-2.38944943747474,2.16255611447464,
19.4179849470734));
#254604=CARTESIAN_POINT('Ctrl Pts',(-2.4557291860714,2.0893223579306,19.4240783472236));
#254605=CARTESIAN_POINT('Ctrl Pts',(-2.51872316734277,2.01294527951245,
19.4301717473738));
#254606=CARTESIAN_POINT('Ctrl Pts',(-2.57811608605867,1.93376188019765,
19.436265147524));
#254607=CARTESIAN_POINT('Ctrl Pts',(-2.63691201497651,1.85537439532161,
19.4422972996702));
#254608=CARTESIAN_POINT('Ctrl Pts',(-2.69217866538471,1.77423711730017,
19.4483294518163));
#254609=CARTESIAN_POINT('Ctrl Pts',(-2.74364938584352,1.69071156915084,
19.4543616039625));
#254610=CARTESIAN_POINT('Ctrl Pts',(-2.79510388599354,1.60721234296029,
19.4603918551566));
#254611=CARTESIAN_POINT('Ctrl Pts',(-2.84276459394218,1.52132672566836,
19.4664221063507));
#254612=CARTESIAN_POINT('Ctrl Pts',(-2.88640833827298,1.43344496484805,
19.4724523575449));
#254613=CARTESIAN_POINT('Ctrl Pts',(-2.93005099255805,1.34556539896172,
19.4784824581275));
#254614=CARTESIAN_POINT('Ctrl Pts',(-2.96967668238611,1.25569019436361,
19.4845125587101));
#254615=CARTESIAN_POINT('Ctrl Pts',(-3.0051089118833,1.16423279039011,19.4905426592928));
#254616=CARTESIAN_POINT('Ctrl Pts',(-3.04118880411217,1.07110364425051,
19.4966829835749));
#254617=CARTESIAN_POINT('Ctrl Pts',(-3.07292022257069,0.976334331643927,
19.502823307857));
#254618=CARTESIAN_POINT('Ctrl Pts',(-3.10016929488618,0.880379409996024,
19.5089636321391));
#254619=CARTESIAN_POINT('Ctrl Pts',(-3.12696636369791,0.786016174123127,
19.5150021016477));
#254620=CARTESIAN_POINT('Ctrl Pts',(-3.14942862080919,0.6905068241316,19.5210405711562));
#254621=CARTESIAN_POINT('Ctrl Pts',(-3.16748039468825,0.594294129001434,
19.5270790406648));
#254622=CARTESIAN_POINT('Ctrl Pts',(-3.18598890499804,0.495647111169271,
19.5332702923337));
#254623=CARTESIAN_POINT('Ctrl Pts',(-3.19986067498097,0.396261184100161,
19.5394615440026));
#254624=CARTESIAN_POINT('Ctrl Pts',(-3.20907084007098,0.296617440326984,
19.5456527956714));
#254625=CARTESIAN_POINT('Ctrl Pts',(-3.21828100516099,0.196973696553792,
19.5518440473403));
#254626=CARTESIAN_POINT('Ctrl Pts',(-3.22282962077333,0.0970726424224399,
19.5580352990092));
#254627=CARTESIAN_POINT('Ctrl Pts',(-3.22274894448647,-0.00260831580023724,
19.564226550678));
#254628=CARTESIAN_POINT('Origin',(0.,0.,0.));
#254629=CARTESIAN_POINT('',(-3.93722999530371,0.00274405186980325,0.404163522034968));
#254630=CARTESIAN_POINT('',(1.75148086551352,3.5285439479163,7.45444598572177E-5));
#254631=CARTESIAN_POINT('Ctrl Pts',(-3.93722999530371,0.00274405186980325,
0.404163522034968));
#254632=CARTESIAN_POINT('Ctrl Pts',(-3.93835497379214,0.1547293111658,0.396451338459333));
#254633=CARTESIAN_POINT('Ctrl Pts',(-3.86157235511925,1.60468070640351,
0.322814988217039));
#254634=CARTESIAN_POINT('Ctrl Pts',(-2.12592865623231,4.06914714944292,
0.188118662358656));
#254635=CARTESIAN_POINT('Ctrl Pts',(0.671429896126083,4.05739230139646,
0.0611345200759264));
#254636=CARTESIAN_POINT('Ctrl Pts',(1.75148086551352,3.5285439479163,7.45444598572177E-5));
#254637=CARTESIAN_POINT('',(-1.74869447533115,3.52286199445086,2.77555756156289E-16));
#254638=CARTESIAN_POINT('Origin',(0.,0.,0.));
#254639=CARTESIAN_POINT('',(-3.93488389043595,0.00402910871532618,0.220836477965015));
#254640=CARTESIAN_POINT('Ctrl Pts',(-1.74869447533115,3.52286199445086,
3.95516952522712E-15));
#254641=CARTESIAN_POINT('Ctrl Pts',(-2.91690893257059,2.9429783173172,0.0659716112048785));
#254642=CARTESIAN_POINT('Ctrl Pts',(-3.86227691191404,1.60239438884148,
0.139583770526549));
#254643=CARTESIAN_POINT('Ctrl Pts',(-3.93787086126692,0.15449063739856,
0.213195929848219));
#254644=CARTESIAN_POINT('Ctrl Pts',(-3.93673266199906,0.00403100175761811,
0.220836477965015));
#254645=CARTESIAN_POINT('',(-3.93299973577035,0.00144167622244941,1.470836477933));
#254646=CARTESIAN_POINT('Ctrl Pts',(-3.93299793819429,0.00402717760202628,
0.220836477965015));
#254647=CARTESIAN_POINT('Ctrl Pts',(-3.93311354600702,-0.108877028281689,
0.226575404348846));
#254648=CARTESIAN_POINT('Ctrl Pts',(-3.92836338289706,-0.222004398198187,
0.232314330732677));
#254649=CARTESIAN_POINT('Ctrl Pts',(-3.91871648337901,-0.334888224477394,
0.238053257116508));
#254650=CARTESIAN_POINT('Ctrl Pts',(-3.909081298676,-0.447634969081591,
0.243785214374049));
#254651=CARTESIAN_POINT('Ctrl Pts',(-3.89456122812118,-0.560138330773846,
0.24951717163159));
#254652=CARTESIAN_POINT('Ctrl Pts',(-3.87517729968192,-0.671929978517044,
0.255249128889131));
#254653=CARTESIAN_POINT('Ctrl Pts',(-3.85536874380315,-0.786170551992133,
0.26110665131997));
#254654=CARTESIAN_POINT('Ctrl Pts',(-3.83048071255231,-0.899667408140772,
0.266964173750808));
#254655=CARTESIAN_POINT('Ctrl Pts',(-3.80059184697523,-1.01192421292574,
0.272821696181647));
#254656=CARTESIAN_POINT('Ctrl Pts',(-3.7713872696243,-1.12161096333307,
0.278545114036871));
#254657=CARTESIAN_POINT('Ctrl Pts',(-3.73740849536641,-1.23011338996449,
0.284268531892095));
#254658=CARTESIAN_POINT('Ctrl Pts',(-3.69878062655764,-1.33697826332438,
0.289991949747319));
#254659=CARTESIAN_POINT('Ctrl Pts',(-3.66016258806189,-1.4438159409008,
0.295713911063759));
#254660=CARTESIAN_POINT('Ctrl Pts',(-3.6168979520197,-1.54901648634995,
0.301435872380199));
#254661=CARTESIAN_POINT('Ctrl Pts',(-3.5691613056908,-1.65214302466812,
0.30715783369664));
#254662=CARTESIAN_POINT('Ctrl Pts',(-3.52142416854057,-1.75527062331854,
0.312879853845464));
#254663=CARTESIAN_POINT('Ctrl Pts',(-3.46921511245753,-1.85632378025581,
0.318601873994288));
#254664=CARTESIAN_POINT('Ctrl Pts',(-3.41275596076645,-1.95488765719493,
0.324323894143112));
#254665=CARTESIAN_POINT('Ctrl Pts',(-3.35396036083763,-2.05753040159275,
0.330282708566958));
#254666=CARTESIAN_POINT('Ctrl Pts',(-3.29055555814702,-2.15747294469517,
0.336241522990803));
#254667=CARTESIAN_POINT('Ctrl Pts',(-3.22284284643409,-2.25427881753536,
0.342200337414648));
#254668=CARTESIAN_POINT('Ctrl Pts',(-3.15773097117648,-2.34736638938298,
0.347930274551024));
#254669=CARTESIAN_POINT('Ctrl Pts',(-3.08863633849219,-2.43755349830048,
0.353660211687401));
#254670=CARTESIAN_POINT('Ctrl Pts',(-3.01586797195248,-2.52448596267661,
0.359390148823777));
#254671=CARTESIAN_POINT('Ctrl Pts',(-2.94305066525653,-2.61147689323235,
0.365123939612942));
#254672=CARTESIAN_POINT('Ctrl Pts',(-2.86655500274261,-2.69520850910087,
0.370857730402108));
#254673=CARTESIAN_POINT('Ctrl Pts',(-2.78672642131459,-2.77536391357011,
0.376591521191273));
#254674=CARTESIAN_POINT('Ctrl Pts',(-2.70678384060799,-2.85563378403786,
0.382333500125608));
#254675=CARTESIAN_POINT('Ctrl Pts',(-2.62349916875116,-2.93231697145337,
0.388075479059943));
#254676=CARTESIAN_POINT('Ctrl Pts',(-2.53725013549212,-3.00513739285664,
0.393817457994278));
#254677=CARTESIAN_POINT('Ctrl Pts',(-2.52717514780255,-3.0136437473219,
0.394488194405937));
#254678=CARTESIAN_POINT('Ctrl Pts',(-2.51705974165276,-3.02209744311984,
0.395158930817596));
#254679=CARTESIAN_POINT('Ctrl Pts',(-2.50690454292716,-3.03049807996164,
0.395829667229255));
#254680=CARTESIAN_POINT('Ctrl Pts',(-2.41781056388444,-3.10419886937527,
0.401714197647443));
#254681=CARTESIAN_POINT('Ctrl Pts',(-2.32531925628814,-3.17408692819413,
0.407598728065632));
#254682=CARTESIAN_POINT('Ctrl Pts',(-2.22979024642192,-3.23983401688446,
0.413483258483821));
#254683=CARTESIAN_POINT('Ctrl Pts',(-2.13438351126278,-3.30549695097063,
0.419360256852487));
#254684=CARTESIAN_POINT('Ctrl Pts',(-2.03594714277588,-3.36702922541343,
0.425237255221152));
#254685=CARTESIAN_POINT('Ctrl Pts',(-1.9348744840283,-3.42414218908273,
0.431114253589818));
#254686=CARTESIAN_POINT('Ctrl Pts',(-1.83390449070715,-3.48119713976569,
0.43698528234661));
#254687=CARTESIAN_POINT('Ctrl Pts',(-1.73030389014374,-3.53384150821365,
0.442856311103402));
#254688=CARTESIAN_POINT('Ctrl Pts',(-1.62449517126266,-3.58182976124554,
0.448727339860194));
#254689=CARTESIAN_POINT('Ctrl Pts',(-1.51559829918762,-3.63121860846703,
0.454769721567848));
#254690=CARTESIAN_POINT('Ctrl Pts',(-1.40436279656774,-3.67567511612874,
0.460812103275502));
#254691=CARTESIAN_POINT('Ctrl Pts',(-1.29127707938659,-3.7149821674203,
0.466854484983155));
#254692=CARTESIAN_POINT('Ctrl Pts',(-1.18152407658287,-3.75313081269703,
0.472718793518591));
#254693=CARTESIAN_POINT('Ctrl Pts',(-1.07002880257866,-3.78642912584396,
0.478583102054027));
#254694=CARTESIAN_POINT('Ctrl Pts',(-0.957257541823985,-3.8147276440948,
0.484447410589463));
#254695=CARTESIAN_POINT('Ctrl Pts',(-0.844503572797165,-3.84302182320575,
0.490310819923927));
#254696=CARTESIAN_POINT('Ctrl Pts',(-0.730474404974104,-3.86631763193849,
0.496174229258391));
#254697=CARTESIAN_POINT('Ctrl Pts',(-0.615649723824761,-3.88451598240431,
0.502037638592855));
#254698=CARTESIAN_POINT('Ctrl Pts',(-0.50081517840818,-3.90271589623952,
0.507901551636417));
#254699=CARTESIAN_POINT('Ctrl Pts',(-0.385185390104271,-3.91581741691315,
0.513765464679979));
#254700=CARTESIAN_POINT('Ctrl Pts',(-0.269247752295546,-3.92377301176862,
0.519629377723542));
#254701=CARTESIAN_POINT('Ctrl Pts',(-0.153272417791312,-3.93173119335643,
0.525495197396811));
#254702=CARTESIAN_POINT('Ctrl Pts',(-0.036989444897966,-3.93454009371325,
0.531361017070082));
#254703=CARTESIAN_POINT('Ctrl Pts',(0.0791118554183913,-3.93220425643586,
0.537226836743351));
#254704=CARTESIAN_POINT('Ctrl Pts',(0.195341224038918,-3.92986584255753,
0.543099126848702));
#254705=CARTESIAN_POINT('Ctrl Pts',(0.311388108615128,-3.92237137231704,
0.548971416954052));
#254706=CARTESIAN_POINT('Ctrl Pts',(0.426766308745078,-3.90977742559856,
0.554843707059402));
#254707=CARTESIAN_POINT('Ctrl Pts',(0.542221028469673,-3.89717512649031,
0.560719891706858));
#254708=CARTESIAN_POINT('Ctrl Pts',(0.657005774981368,-3.87946667824872,
0.566596076354314));
#254709=CARTESIAN_POINT('Ctrl Pts',(0.770644217653579,-3.85675984341741,
0.57247226100177));
#254710=CARTESIAN_POINT('Ctrl Pts',(0.884443379880605,-3.83402089416866,
0.578356756373646));
#254711=CARTESIAN_POINT('Ctrl Pts',(0.997092604841083,-3.80626954806755,
0.584241251745521));
#254712=CARTESIAN_POINT('Ctrl Pts',(1.1081303468093,-3.77366348983058,0.590125747117397));
#254713=CARTESIAN_POINT('Ctrl Pts',(1.13089175721267,-3.7669796374754,0.591331998359559));
#254714=CARTESIAN_POINT('Ctrl Pts',(1.1535855204548,-3.76009195101654,0.59253824960172));
#254715=CARTESIAN_POINT('Ctrl Pts',(1.17620777064543,-3.75300203574063,
0.593744500843882));
#254716=CARTESIAN_POINT('Ctrl Pts',(1.28659360400096,-3.71840661753262,
0.599630433829332));
#254717=CARTESIAN_POINT('Ctrl Pts',(1.39562681385626,-3.67888213448853,
0.605516366814782));
#254718=CARTESIAN_POINT('Ctrl Pts',(1.50283619962322,-3.63455256628681,
0.611402299800233));
#254719=CARTESIAN_POINT('Ctrl Pts',(1.60991159789792,-3.59027840002246,
0.617280876700255));
#254720=CARTESIAN_POINT('Ctrl Pts',(1.71516732886334,-3.54121124835459,
0.623159453600278));
#254721=CARTESIAN_POINT('Ctrl Pts',(1.81814716568986,-3.48752489365939,
0.629038030500301));
#254722=CARTESIAN_POINT('Ctrl Pts',(1.92102546456795,-3.43389147362094,
0.634910811133243));
#254723=CARTESIAN_POINT('Ctrl Pts',(2.02163197087264,-3.37564810000452,
0.640783591766186));
#254724=CARTESIAN_POINT('Ctrl Pts',(2.11953087241314,-3.31301643232985,
0.646656372399129));
#254725=CARTESIAN_POINT('Ctrl Pts',(2.22024715141409,-3.24858232309515,
0.652698162484936));
#254726=CARTESIAN_POINT('Ctrl Pts',(2.31809720859455,-3.17950367824976,
0.658739952570744));
#254727=CARTESIAN_POINT('Ctrl Pts',(2.41263387155287,-3.10607256866864,
0.664781742656551));
#254728=CARTESIAN_POINT('Ctrl Pts',(2.50442748710302,-3.03477211410021,
0.670648225976528));
#254729=CARTESIAN_POINT('Ctrl Pts',(2.59309699683705,-2.95936856719085,
0.676514709296505));
#254730=CARTESIAN_POINT('Ctrl Pts',(2.6782635032127,-2.88017249611179,0.682381192616482));
#254731=CARTESIAN_POINT('Ctrl Pts',(2.76341919202161,-2.80098648425461,
0.688246930795235));
#254732=CARTESIAN_POINT('Ctrl Pts',(2.84507246129512,-2.71800918605741,
0.694112668973988));
#254733=CARTESIAN_POINT('Ctrl Pts',(2.92287945763673,-2.63158976212578,
0.699978407152741));
#254734=CARTESIAN_POINT('Ctrl Pts',(3.00069515605258,-2.54516067289053,
0.70584480136619));
#254735=CARTESIAN_POINT('Ctrl Pts',(3.07466345113915,-2.45528899800045,
0.711711195579639));
#254736=CARTESIAN_POINT('Ctrl Pts',(3.14447961111279,-2.36235835031351,
0.717577589793087));
#254737=CARTESIAN_POINT('Ctrl Pts',(3.21795039442107,-2.26456311950328,
0.723751068515206));
#254738=CARTESIAN_POINT('Ctrl Pts',(3.28682226938243,-2.16338040068169,
0.729924547237324));
#254739=CARTESIAN_POINT('Ctrl Pts',(3.35079154505351,-2.05929235942785,
0.736098025959443));
#254740=CARTESIAN_POINT('Ctrl Pts',(3.41167121663846,-1.96023158844089,
0.741973336461187));
#254741=CARTESIAN_POINT('Ctrl Pts',(3.46811063420051,-1.85853997033719,
0.74784864696293));
#254742=CARTESIAN_POINT('Ctrl Pts',(3.51989560504022,-1.75465778134043,
0.753723957464674));
#254743=CARTESIAN_POINT('Ctrl Pts',(3.57171659929356,-1.65070332830641,
0.759603355035252));
#254744=CARTESIAN_POINT('Ctrl Pts',(3.61887653269448,-1.54455564449925,
0.765482752605829));
#254745=CARTESIAN_POINT('Ctrl Pts',(3.66120966513167,-1.43667421078909,
0.771362150176407));
#254746=CARTESIAN_POINT('Ctrl Pts',(3.7036032251698,-1.32863878383888,0.777249940177917));
#254747=CARTESIAN_POINT('Ctrl Pts',(3.74115610293889,-1.21886505578006,
0.783137730179428));
#254748=CARTESIAN_POINT('Ctrl Pts',(3.77375259322463,-1.10782686604468,
0.789025520180939));
#254749=CARTESIAN_POINT('Ctrl Pts',(3.77861310973372,-1.09126977816137,
0.789903458273462));
#254750=CARTESIAN_POINT('Ctrl Pts',(3.78336351760962,-1.07468459181666,
0.790781396365985));
#254751=CARTESIAN_POINT('Ctrl Pts',(3.78800353131779,-1.05807289291615,
0.791659334458508));
#254752=CARTESIAN_POINT('Ctrl Pts',(3.81901775404746,-0.947038968875929,
0.797527542885656));
#254753=CARTESIAN_POINT('Ctrl Pts',(3.84519837414544,-0.83445237177865,
0.803395751312803));
#254754=CARTESIAN_POINT('Ctrl Pts',(3.86639062477172,-0.720772180843109,
0.809263959739951));
#254755=CARTESIAN_POINT('Ctrl Pts',(3.88755529218587,-0.607239952711398,
0.815124530279044));
#254756=CARTESIAN_POINT('Ctrl Pts',(3.9037444262341,-0.49261736447216,0.820985100818138));
#254757=CARTESIAN_POINT('Ctrl Pts',(3.91485306469716,-0.377378433182414,
0.826845671357231));
#254758=CARTESIAN_POINT('Ctrl Pts',(3.92595022710798,-0.262258552305652,
0.832700187489752));
#254759=CARTESIAN_POINT('Ctrl Pts',(3.93197729373393,-0.146524004434368,
0.838554703622273));
#254760=CARTESIAN_POINT('Ctrl Pts',(3.93288050677404,-0.0306581055645306,
0.844409219754794));
#254761=CARTESIAN_POINT('Ctrl Pts',(3.93381365302187,0.0890476825297482,
0.850457759268059));
#254762=CARTESIAN_POINT('Ctrl Pts',(3.92927733600448,0.208893237457599,
0.856506298781322));
#254763=CARTESIAN_POINT('Ctrl Pts',(3.91927053949092,0.328340430465874,
0.862554838294587));
#254764=CARTESIAN_POINT('Ctrl Pts',(3.90959602720176,0.443821277418104,
0.868402530887642));
#254765=CARTESIAN_POINT('Ctrl Pts',(3.89480861733269,0.558929353772634,
0.874250223480699));
#254766=CARTESIAN_POINT('Ctrl Pts',(3.87496032876677,0.673180102560742,
0.880097916073754));
#254767=CARTESIAN_POINT('Ctrl Pts',(3.85511512250948,0.787413108959298,
0.885944700558626));
#254768=CARTESIAN_POINT('Ctrl Pts',(3.83021067106616,0.900788644716794,
0.891791485043498));
#254769=CARTESIAN_POINT('Ctrl Pts',(3.80035047746741,1.01283031570604,0.89763826952837));
#254770=CARTESIAN_POINT('Ctrl Pts',(3.77048766277349,1.12488182159079,0.903485567237599));
#254771=CARTESIAN_POINT('Ctrl Pts',(3.73566834789256,1.23559882990257,0.909332864946827));
#254772=CARTESIAN_POINT('Ctrl Pts',(3.69604628257231,1.34451882734435,0.915180162656055));
#254773=CARTESIAN_POINT('Ctrl Pts',(3.65641110822163,1.45347486116001,0.921029394954077));
#254774=CARTESIAN_POINT('Ctrl Pts',(3.61197016544886,1.56063231309586,0.926878627252099));
#254775=CARTESIAN_POINT('Ctrl Pts',(3.56292556304311,1.66554808763179,0.932727859550121));
#254776=CARTESIAN_POINT('Ctrl Pts',(3.51382565579645,1.77058216978844,0.938583687698569));
#254777=CARTESIAN_POINT('Ctrl Pts',(3.46011190326251,1.8733691541328,0.944439515847018));
#254778=CARTESIAN_POINT('Ctrl Pts',(3.40203268499144,1.97348995696707,0.950295343995466));
#254779=CARTESIAN_POINT('Ctrl Pts',(3.34391430392436,2.07367827122274,0.956155120726732));
#254780=CARTESIAN_POINT('Ctrl Pts',(3.28142481884333,2.17119647665599,0.962014897457997));
#254781=CARTESIAN_POINT('Ctrl Pts',(3.21485531851645,2.2656553756047,0.967874674189263));
#254782=CARTESIAN_POINT('Ctrl Pts',(3.14818909663982,2.36025151775112,0.97374296482981));
#254783=CARTESIAN_POINT('Ctrl Pts',(3.07743128169455,2.45177915671903,0.979611255470357));
#254784=CARTESIAN_POINT('Ctrl Pts',(3.0029125123752,2.5398829585279,0.985479546110905));
#254785=CARTESIAN_POINT('Ctrl Pts',(2.9855805947781,2.56037454537093,0.986844420098315));
#254786=CARTESIAN_POINT('Ctrl Pts',(2.96804537837472,2.58068107986218,0.988209294085726));
#254787=CARTESIAN_POINT('Ctrl Pts',(2.9503112926361,2.60079839213729,0.989574168073137));
#254788=CARTESIAN_POINT('Ctrl Pts',(2.87394205037106,2.68743065034914,0.995451797951671));
#254789=CARTESIAN_POINT('Ctrl Pts',(2.79362831518194,2.77083868145239,1.0013294278302));
#254790=CARTESIAN_POINT('Ctrl Pts',(2.70967281965614,2.85064242065131,1.00720705770874));
#254791=CARTESIAN_POINT('Ctrl Pts',(2.62582492649507,2.93034387862374,1.01307715446666));
#254792=CARTESIAN_POINT('Ctrl Pts',(2.53834485178755,3.00644995003002,1.01894725122458));
#254793=CARTESIAN_POINT('Ctrl Pts',(2.44757487058002,3.07861433974852,1.0248173479825));
#254794=CARTESIAN_POINT('Ctrl Pts',(2.35689707581916,3.15070543895207,1.03068148304081));
#254795=CARTESIAN_POINT('Ctrl Pts',(2.2629363418411,3.21886256425645,1.03654561809912));
#254796=CARTESIAN_POINT('Ctrl Pts',(2.16607051905588,3.28277740739103,1.04240975315743));
#254797=CARTESIAN_POINT('Ctrl Pts',(2.06621762345819,3.34866320668695,1.04845472184619));
#254798=CARTESIAN_POINT('Ctrl Pts',(1.96327788442577,3.41004052912714,1.05449969053495));
#254799=CARTESIAN_POINT('Ctrl Pts',(1.85770083722228,3.46661745789518,1.06054465922372));
#254800=CARTESIAN_POINT('Ctrl Pts',(1.75539829892882,3.52143963350181,1.06640214110208));
#254801=CARTESIAN_POINT('Ctrl Pts',(1.65062002168364,3.57175458276345,1.07225962298044));
#254802=CARTESIAN_POINT('Ctrl Pts',(1.54380224754594,3.61734206572617,1.0781171048588));
#254803=CARTESIAN_POINT('Ctrl Pts',(1.43700018562714,3.66292284305852,1.08397372513862));
#254804=CARTESIAN_POINT('Ctrl Pts',(1.32815960264227,3.70377737499157,1.08983034541845));
#254805=CARTESIAN_POINT('Ctrl Pts',(1.21773786134816,3.73973307884924,1.09568696569828));
#254806=CARTESIAN_POINT('Ctrl Pts',(1.1073057625578,3.77569215533139,1.10154413532574));
#254807=CARTESIAN_POINT('Ctrl Pts',(0.99529260286013,3.80675136255577,1.1074013049532));
#254808=CARTESIAN_POINT('Ctrl Pts',(0.882171412714956,3.83278783636513,
1.11325847458067));
#254809=CARTESIAN_POINT('Ctrl Pts',(0.76901236190473,3.85883302435274,1.11911760455117));
#254810=CARTESIAN_POINT('Ctrl Pts',(0.654744944964708,3.87985204364202,
1.12497673452167));
#254811=CARTESIAN_POINT('Ctrl Pts',(0.539852207007587,3.8957731703205,1.13083586449217));
#254812=CARTESIAN_POINT('Ctrl Pts',(0.424830350794599,3.91171218941015,
1.13670157904457));
#254813=CARTESIAN_POINT('Ctrl Pts',(0.309182179743551,3.92254182454833,
1.14256729359697));
#254814=CARTESIAN_POINT('Ctrl Pts',(0.193395777696842,3.9282422370787,1.14843300814937));
#254815=CARTESIAN_POINT('Ctrl Pts',(0.0775313268123665,3.93394649212048,
1.15430267663932));
#254816=CARTESIAN_POINT('Ctrl Pts',(-0.0384711291623765,3.93451463764493,
1.16017234512928));
#254817=CARTESIAN_POINT('Ctrl Pts',(-0.154125307541816,3.92997892991491,
1.16604201361923));
#254818=CARTESIAN_POINT('Ctrl Pts',(-0.269945917752929,3.92543669508699,
1.17192012883971));
#254819=CARTESIAN_POINT('Ctrl Pts',(-0.385416840740004,3.91577598371688,
1.17779824406018));
#254820=CARTESIAN_POINT('Ctrl Pts',(-0.500058645391984,3.90108066452986,
1.18367635928065));
#254821=CARTESIAN_POINT('Ctrl Pts',(-0.524844833347922,3.8979034557922,
1.18494724008302));
#254822=CARTESIAN_POINT('Ctrl Pts',(-0.549592310496414,3.8944910933274,
1.18621812088539));
#254823=CARTESIAN_POINT('Ctrl Pts',(-0.574296314742032,3.89084473384299,
1.18748900168776));
#254824=CARTESIAN_POINT('Ctrl Pts',(-0.688538162859492,3.87398241297151,
1.19336609635453));
#254825=CARTESIAN_POINT('Ctrl Pts',(-0.802224297210271,3.85205664271962,
1.19924319102131));
#254826=CARTESIAN_POINT('Ctrl Pts',(-0.914871154585363,3.82511434737677,
1.20512028568808));
#254827=CARTESIAN_POINT('Ctrl Pts',(-1.02737392205874,3.79820651471472,
1.21098986279055));
#254828=CARTESIAN_POINT('Ctrl Pts',(-1.13883965865839,3.76629501342637,
1.21685943989303));
#254829=CARTESIAN_POINT('Ctrl Pts',(-1.2487915917321,3.72947832282468,1.22272901699551));
#254830=CARTESIAN_POINT('Ctrl Pts',(-1.35863214956261,3.69269892549975,
1.22859264854015));
#254831=CARTESIAN_POINT('Ctrl Pts',(-1.46696156508408,3.65102435259494,
1.23445628008479));
#254832=CARTESIAN_POINT('Ctrl Pts',(-1.57331555457698,3.60460360729528,
1.24031991162943));
#254833=CARTESIAN_POINT('Ctrl Pts',(-1.68296215310863,3.55674572394101,
1.2463650751158));
#254834=CARTESIAN_POINT('Ctrl Pts',(-1.79050858428811,3.50384311083602,
1.25241023860217));
#254835=CARTESIAN_POINT('Ctrl Pts',(-1.89546511648441,3.44611389715876,
1.25845540208855));
#254836=CARTESIAN_POINT('Ctrl Pts',(-1.99715512642981,3.39018136785224,
1.26431242424988));
#254837=CARTESIAN_POINT('Ctrl Pts',(-2.09641367033037,3.32971843360438,
1.27016944641122));
#254838=CARTESIAN_POINT('Ctrl Pts',(-2.19281853834584,3.26497103476996,
1.27602646857256));
#254839=CARTESIAN_POINT('Ctrl Pts',(-2.28920950689362,3.20023297109045,
1.28188264627975));
#254840=CARTESIAN_POINT('Ctrl Pts',(-2.38274727528615,3.13121190112845,
1.28773882398695));
#254841=CARTESIAN_POINT('Ctrl Pts',(-2.4730381082637,3.05819742905449,1.29359500169414));
#254842=CARTESIAN_POINT('Ctrl Pts',(-2.56333768435814,2.98517588678256,
1.2994517464716));
#254843=CARTESIAN_POINT('Ctrl Pts',(-2.65038937918525,2.9081604331004,1.30530849124905));
#254844=CARTESIAN_POINT('Ctrl Pts',(-2.7338326307723,2.82748088356484,1.3111652360265));
#254845=CARTESIAN_POINT('Ctrl Pts',(-2.81730407304,2.74677407704477,1.31702395946153));
#254846=CARTESIAN_POINT('Ctrl Pts',(-2.89716435146355,2.66240099972866,
1.32288268289656));
#254847=CARTESIAN_POINT('Ctrl Pts',(-2.97309034837575,2.57472770995206,
1.32874140633159));
#254848=CARTESIAN_POINT('Ctrl Pts',(-3.04910205755941,2.48695544647581,
1.33460674363425));
#254849=CARTESIAN_POINT('Ctrl Pts',(-3.12117035047973,2.39587584669275,
1.34047208093691));
#254850=CARTESIAN_POINT('Ctrl Pts',(-3.18901288686557,2.30188744455617,
1.34633741823958));
#254851=CARTESIAN_POINT('Ctrl Pts',(-3.25690135059727,2.20783541511315,
1.35220672619825));
#254852=CARTESIAN_POINT('Ctrl Pts',(-3.32055813548043,2.11087100616429,
1.35807603415693));
#254853=CARTESIAN_POINT('Ctrl Pts',(-3.37974558077294,2.01141960049259,
1.3639453421156));
#254854=CARTESIAN_POINT('Ctrl Pts',(-3.43901847831361,1.9118246112255,1.36982312392473));
#254855=CARTESIAN_POINT('Ctrl Pts',(-3.49380896468209,1.80973582166201,
1.37570090573386));
#254856=CARTESIAN_POINT('Ctrl Pts',(-3.54392640262637,1.70560096528107,
1.38157868754299));
#254857=CARTESIAN_POINT('Ctrl Pts',(-3.55479822534706,1.68301130898465,
1.38285373679612));
#254858=CARTESIAN_POINT('Ctrl Pts',(-3.56545033110821,1.66032543435367,
1.38412878604925));
#254859=CARTESIAN_POINT('Ctrl Pts',(-3.57588108174667,1.63754801126754,
1.38540383530239));
#254860=CARTESIAN_POINT('Ctrl Pts',(-3.6282167406232,1.52326367200564,1.3918013176194));
#254861=CARTESIAN_POINT('Ctrl Pts',(-3.67512622428012,1.40634521511715,
1.39819879993641));
#254862=CARTESIAN_POINT('Ctrl Pts',(-3.71636016386655,1.28730576493146,
1.40459628225342));
#254863=CARTESIAN_POINT('Ctrl Pts',(-3.75744538515146,1.1686956539024,1.41097069079398));
#254864=CARTESIAN_POINT('Ctrl Pts',(-3.7928957832422,1.0479800797706,1.41734509933454));
#254865=CARTESIAN_POINT('Ctrl Pts',(-3.82251035156653,0.925690883700762,
1.4237195078751));
#254866=CARTESIAN_POINT('Ctrl Pts',(-3.85205662684401,0.803683694165899,
1.43007921663086));
#254867=CARTESIAN_POINT('Ctrl Pts',(-3.8757938214186,0.680110397212712,
1.43643892538663));
#254868=CARTESIAN_POINT('Ctrl Pts',(-3.89356997535806,0.555519438895018,
1.44279863414239));
#254869=CARTESIAN_POINT('Ctrl Pts',(-3.91128399626355,0.431363963656041,
1.44913611379272));
#254870=CARTESIAN_POINT('Ctrl Pts',(-3.92307847021014,0.306198207414769,
1.45547359344305));
#254871=CARTESIAN_POINT('Ctrl Pts',(-3.9288521876697,0.180580971984852,
1.46181107309338));
#254872=CARTESIAN_POINT('Ctrl Pts',(-3.9315930321051,0.120949148444982,
1.46481954137325));
#254873=CARTESIAN_POINT('Ctrl Pts',(-3.9329778250335,0.0612157925789621,
1.46782800965313));
#254874=CARTESIAN_POINT('Ctrl Pts',(-3.93299973577035,0.0014416762224595,
1.470836477933));
#254875=CARTESIAN_POINT('',(-3.93299840952093,-0.00353704761472742,2.72083647800911));
#254876=CARTESIAN_POINT('Ctrl Pts',(-3.93299973577059,0.00144167558636852,
1.47083647796501));
#254877=CARTESIAN_POINT('Ctrl Pts',(-3.93304331884989,-0.117456251947492,
1.47682068426248));
#254878=CARTESIAN_POINT('Ctrl Pts',(-3.92769097363441,-0.236318755341996,
1.48280489055995));
#254879=CARTESIAN_POINT('Ctrl Pts',(-3.91697863997465,-0.354636904428063,
1.48878909685742));
#254880=CARTESIAN_POINT('Ctrl Pts',(-3.90626038729162,-0.473020429360419,
1.49477660968524));
#254881=CARTESIAN_POINT('Ctrl Pts',(-3.89017628169922,-0.590858615918335,
1.50076412251306));
#254882=CARTESIAN_POINT('Ctrl Pts',(-3.86881396591898,-0.707649275496164,
1.50675163534088));
#254883=CARTESIAN_POINT('Ctrl Pts',(-3.84743570814185,-0.824527092119618,
1.5127436164535));
#254884=CARTESIAN_POINT('Ctrl Pts',(-3.82077146341929,-0.940355444834012,
1.51873559756612));
#254885=CARTESIAN_POINT('Ctrl Pts',(-3.78895954349243,-1.05464428969091,
1.52472757867874));
#254886=CARTESIAN_POINT('Ctrl Pts',(-3.7570959412729,-1.16911881053159,
1.53072929448584));
#254887=CARTESIAN_POINT('Ctrl Pts',(-3.72006806543135,-1.28204845581664,
1.53673101029295));
#254888=CARTESIAN_POINT('Ctrl Pts',(-3.6780636878262,-1.39295962191815,
1.54273272610005));
#254889=CARTESIAN_POINT('Ctrl Pts',(-3.63601965285659,-1.50397550197536,
1.54874010827444));
#254890=CARTESIAN_POINT('Ctrl Pts',(-3.58898990357719,-1.61296875038297,
1.55474749044884));
#254891=CARTESIAN_POINT('Ctrl Pts',(-3.53720909265351,-1.71948853873742,
1.56075487262323));
#254892=CARTESIAN_POINT('Ctrl Pts',(-3.48533727340255,-1.826195542927,1.56677281318388));
#254893=CARTESIAN_POINT('Ctrl Pts',(-3.42869789966955,-1.93042006630803,
1.57279075374454));
#254894=CARTESIAN_POINT('Ctrl Pts',(-3.36757026993159,-2.03173804341821,
1.5788086943052));
#254895=CARTESIAN_POINT('Ctrl Pts',(-3.35230014801198,-2.05704800341098,
1.58031201917581));
#254896=CARTESIAN_POINT('Ctrl Pts',(-3.33675014438406,-2.08217673920702,
1.58181534404641));
#254897=CARTESIAN_POINT('Ctrl Pts',(-3.32092500819953,-2.10711795823465,
1.58331866891702));
#254898=CARTESIAN_POINT('Ctrl Pts',(-3.25906702428011,-2.20460928516867,
1.58919493087061));
#254899=CARTESIAN_POINT('Ctrl Pts',(-3.19281041116404,-2.29953508526944,
1.5950711928242));
#254900=CARTESIAN_POINT('Ctrl Pts',(-3.12239447932152,-2.39147270850046,
1.60094745477779));
#254901=CARTESIAN_POINT('Ctrl Pts',(-3.05206887796362,-2.48329239293772,
1.60681617858516));
#254902=CARTESIAN_POINT('Ctrl Pts',(-2.97759481769122,-2.57213119913305,
1.61268490239254));
#254903=CARTESIAN_POINT('Ctrl Pts',(-2.89925595724034,-2.65759362853059,
1.61855362619991));
#254904=CARTESIAN_POINT('Ctrl Pts',(-2.82099672069398,-2.74296919360205,
1.62441638501493));
#254905=CARTESIAN_POINT('Ctrl Pts',(-2.73888077494803,-2.8249749056687,
1.63027914382994));
#254906=CARTESIAN_POINT('Ctrl Pts',(-2.65323286853758,-2.90324720706174,
1.63614190264496));
#254907=CARTESIAN_POINT('Ctrl Pts',(-2.56491557514853,-2.98395902006552,
1.64218738597357));
#254908=CARTESIAN_POINT('Ctrl Pts',(-2.47284282112379,-3.06070053310228,
1.64823286930218));
#254909=CARTESIAN_POINT('Ctrl Pts',(-2.37741309954045,-3.13311282180095,
1.6542783526308));
#254910=CARTESIAN_POINT('Ctrl Pts',(-2.28497274721762,-3.20325677033967,
1.66013445908889));
#254911=CARTESIAN_POINT('Ctrl Pts',(-2.18938295969857,-3.26933841021361,
1.66599056554699));
#254912=CARTESIAN_POINT('Ctrl Pts',(-2.09103996362314,-3.33107203022254,
1.67184667200509));
#254913=CARTESIAN_POINT('Ctrl Pts',(-1.99271139055599,-3.39279659636341,
1.67770191960516));
#254914=CARTESIAN_POINT('Ctrl Pts',(-1.89163076130424,-3.45017419128729,
1.68355716720522));
#254915=CARTESIAN_POINT('Ctrl Pts',(-1.78822262322662,-3.50296286731397,
1.68941241480529));
#254916=CARTESIAN_POINT('Ctrl Pts',(-1.68480470781403,-3.55575653455873,
1.69526821602443));
#254917=CARTESIAN_POINT('Ctrl Pts',(-1.57905921369824,-3.6039602327234,
1.70112401724356));
#254918=CARTESIAN_POINT('Ctrl Pts',(-1.47143394316256,-3.64737866842875,
1.7069798184627));
#254919=CARTESIAN_POINT('Ctrl Pts',(-1.36377253625714,-3.69081168235201,
1.71283758583158));
#254920=CARTESIAN_POINT('Ctrl Pts',(-1.25423048040731,-3.72945608458083,
1.71869535320046));
#254921=CARTESIAN_POINT('Ctrl Pts',(-1.14327346905214,-3.76316552585207,
1.72455312056934));
#254922=CARTESIAN_POINT('Ctrl Pts',(-1.03219143968109,-3.79691294838662,
1.73041748802995));
#254923=CARTESIAN_POINT('Ctrl Pts',(-0.919691667906793,-3.82571419208598,
1.73628185549057));
#254924=CARTESIAN_POINT('Ctrl Pts',(-0.806252939139831,-3.84947336633576,
1.74214622295119));
#254925=CARTESIAN_POINT('Ctrl Pts',(-0.692737581551075,-3.87324859010892,
1.74801455184168));
#254926=CARTESIAN_POINT('Ctrl Pts',(-0.57828241022721,-3.89197489578581,
1.75388288073217));
#254927=CARTESIAN_POINT('Ctrl Pts',(-0.463372574453545,-3.90560812899148,
1.75975120962266));
#254928=CARTESIAN_POINT('Ctrl Pts',(-0.348296927444828,-3.91926103451866,
1.76562800632493));
#254929=CARTESIAN_POINT('Ctrl Pts',(-0.232765716647418,-3.92780617089726,
1.77150480302721));
#254930=CARTESIAN_POINT('Ctrl Pts',(-0.117265391300309,-3.93125143281413,
1.77738159972948));
#254931=CARTESIAN_POINT('Ctrl Pts',(-0.0920307808260116,-3.93200415660251,
1.7786655673302));
#254932=CARTESIAN_POINT('Ctrl Pts',(-0.0667976280864975,-3.93251364043545,
1.77994953493092));
#254933=CARTESIAN_POINT('Ctrl Pts',(-0.0415709710780869,-3.93278029571493,
1.78123350253164));
#254934=CARTESIAN_POINT('Ctrl Pts',(0.0738785598176377,-3.93400064080135,
1.7871095667735));
#254935=CARTESIAN_POINT('Ctrl Pts',(0.189572229615238,-3.93013503998305,
1.79298563101535));
#254936=CARTESIAN_POINT('Ctrl Pts',(0.30502526520211,-3.92115398672233,
1.7988616952572));
#254937=CARTESIAN_POINT('Ctrl Pts',(0.420330200777649,-3.91218445411225,
1.80473022184379));
#254938=CARTESIAN_POINT('Ctrl Pts',(0.535394708215583,-3.89811255072205,
1.81059874843039));
#254939=CARTESIAN_POINT('Ctrl Pts',(0.649732629574102,-3.87896075129238,
1.81646727501698));
#254940=CARTESIAN_POINT('Ctrl Pts',(0.763954347843103,-3.85982841608103,
1.82232983734507));
#254941=CARTESIAN_POINT('Ctrl Pts',(0.877450544192772,-3.8356265220567,
1.82819239967315));
#254942=CARTESIAN_POINT('Ctrl Pts',(0.989739467693193,-3.80642940116987,
1.83405496200124));
#254943=CARTESIAN_POINT('Ctrl Pts',(1.10553339503263,-3.77632091683234,
1.84010051925728));
#254944=CARTESIAN_POINT('Ctrl Pts',(1.22004299834067,-3.74090027531032,
1.84614607651332));
#254945=CARTESIAN_POINT('Ctrl Pts',(1.3327501787942,-3.70030619826576,1.85219163376937));
#254946=CARTESIAN_POINT('Ctrl Pts',(1.44192182779629,-3.66098552399427,
1.858047546872));
#254947=CARTESIAN_POINT('Ctrl Pts',(1.54940202900473,-3.61681128903568,
1.86390345997463));
#254948=CARTESIAN_POINT('Ctrl Pts',(1.65473538768409,-3.56796017308853,
1.86975937307727));
#254949=CARTESIAN_POINT('Ctrl Pts',(1.76005332475921,-3.51911620931603,
1.87561442882972));
#254950=CARTESIAN_POINT('Ctrl Pts',(1.86322466997484,-3.4655968997278,1.88146948458217));
#254951=CARTESIAN_POINT('Ctrl Pts',(1.96381530701981,-3.40762651121197,
1.88732454033462));
#254952=CARTESIAN_POINT('Ctrl Pts',(2.06441548497679,-3.34965062426814,
1.89318015143271));
#254953=CARTESIAN_POINT('Ctrl Pts',(2.16243411054512,-3.2872230252367,1.8990357625308));
#254954=CARTESIAN_POINT('Ctrl Pts',(2.25746352965753,-3.22061289388622,
1.90489137362889));
#254955=CARTESIAN_POINT('Ctrl Pts',(2.35252488857384,-3.15398037457891,
1.91074895282352));
#254956=CARTESIAN_POINT('Ctrl Pts',(2.44459470543798,-3.08316276437169,
1.91660653201814));
#254957=CARTESIAN_POINT('Ctrl Pts',(2.53329663046633,-3.00847090430802,
1.92246411121276));
#254958=CARTESIAN_POINT('Ctrl Pts',(2.62209855956728,-2.93369483535944,
1.9283282943427));
#254959=CARTESIAN_POINT('Ctrl Pts',(2.70752470251825,-2.85503606469215,
1.93419247747264));
#254960=CARTESIAN_POINT('Ctrl Pts',(2.78923389782364,-2.7728438944938,1.94005666060257));
#254961=CARTESIAN_POINT('Ctrl Pts',(2.8709983184397,-2.69059617255348,1.94592480719505));
#254962=CARTESIAN_POINT('Ctrl Pts',(2.94904051192503,-2.60481060020193,
1.95179295378754));
#254963=CARTESIAN_POINT('Ctrl Pts',(3.02305924146376,-2.51586999318338,
1.95766110038002));
#254964=CARTESIAN_POINT('Ctrl Pts',(3.09718483584109,-2.42680097780559,
1.96353771913275));
#254965=CARTESIAN_POINT('Ctrl Pts',(3.16727512500263,-2.33456816467696,
1.96941433788549));
#254966=CARTESIAN_POINT('Ctrl Pts',(3.23307181699572,-2.23958380645779,
1.97529095663822));
#254967=CARTESIAN_POINT('Ctrl Pts',(3.24746800988998,-2.21880140689576,
1.97657674980757));
#254968=CARTESIAN_POINT('Ctrl Pts',(3.26165883164836,-2.19788737725816,
1.97786254297692));
#254969=CARTESIAN_POINT('Ctrl Pts',(3.2756418733088,-2.17684618607425,1.97914833614627));
#254970=CARTESIAN_POINT('Ctrl Pts',(3.33954123599477,-2.08069266386818,
1.98502412240669));
#254971=CARTESIAN_POINT('Ctrl Pts',(3.39930873664199,-1.98156448329821,
1.99089990866711));
#254972=CARTESIAN_POINT('Ctrl Pts',(3.45465558287158,-1.87985206964117,
1.99677569492753));
#254973=CARTESIAN_POINT('Ctrl Pts',(3.50993138150432,-1.7782702220968,2.00264393856317));
#254974=CARTESIAN_POINT('Ctrl Pts',(3.56079761558454,-1.67411109801916,
2.00851218219882));
#254975=CARTESIAN_POINT('Ctrl Pts',(3.6070083295756,-1.5677946008238,2.01438042583447));
#254976=CARTESIAN_POINT('Ctrl Pts',(3.65317204055434,-1.46158624295794,
2.02024270061346));
#254977=CARTESIAN_POINT('Ctrl Pts',(3.69468948707016,-1.3532252532075,2.02610497539245));
#254978=CARTESIAN_POINT('Ctrl Pts',(3.73136060182487,-1.24315608800711,
2.03196725017144));
#254979=CARTESIAN_POINT('Ctrl Pts',(3.76917889277777,-1.12964364797537,
2.03801291348767));
#254980=CARTESIAN_POINT('Ctrl Pts',(3.80184243417943,-1.01431479296164,
2.0440585768039));
#254981=CARTESIAN_POINT('Ctrl Pts',(3.82918532724637,-0.897679636396601,
2.05010424012012));
#254982=CARTESIAN_POINT('Ctrl Pts',(3.85566868752297,-0.784710944141966,
2.05595985603183));
#254983=CARTESIAN_POINT('Ctrl Pts',(3.87716080328516,-0.670517280452859,
2.06181547194353));
#254984=CARTESIAN_POINT('Ctrl Pts',(3.8935617978487,-0.555576751073317,
2.06767108785523));
#254985=CARTESIAN_POINT('Ctrl Pts',(3.90996038245756,-0.440653111002933,
2.07352584334539));
#254986=CARTESIAN_POINT('Ctrl Pts',(3.92126927511692,-0.324983232003589,
2.07938059883555));
#254987=CARTESIAN_POINT('Ctrl Pts',(3.92744009748582,-0.209053296220209,
2.08523535432571));
#254988=CARTESIAN_POINT('Ctrl Pts',(3.93361150227453,-0.0931124186392676,
2.09109066240437));
#254989=CARTESIAN_POINT('Ctrl Pts',(3.93464385080627,0.0230881522979025,
2.09694597048303));
#254990=CARTESIAN_POINT('Ctrl Pts',(3.93054084405488,0.139059962664729,
2.10280127856169));
#254991=CARTESIAN_POINT('Ctrl Pts',(3.92643645990672,0.25507070526025,2.10865855229211));
#254992=CARTESIAN_POINT('Ctrl Pts',(3.91719330699798,0.370852122281178,
2.11451582602253));
#254993=CARTESIAN_POINT('Ctrl Pts',(3.90286707613669,0.485919320472276,
2.12037309975295));
#254994=CARTESIAN_POINT('Ctrl Pts',(3.88852469792352,0.601116212967287,
2.1262369753217));
#254995=CARTESIAN_POINT('Ctrl Pts',(3.86908785786984,0.715596870093928,
2.13210085089045));
#254996=CARTESIAN_POINT('Ctrl Pts',(3.84466366834342,0.828884960244852,
2.1379647264592));
#254997=CARTESIAN_POINT('Ctrl Pts',(3.82022297686574,0.942249592323194,
2.14383256389488));
#254998=CARTESIAN_POINT('Ctrl Pts',(3.7907883305828,1.05441965472114,2.14970040133056));
#254999=CARTESIAN_POINT('Ctrl Pts',(3.7565166938021,1.16493404499403,2.15556823876624));
#255000=CARTESIAN_POINT('Ctrl Pts',(3.72219557451284,1.27560799955317,2.16144454837726));
#255001=CARTESIAN_POINT('Ctrl Pts',(3.68302366650833,1.38462112443565,2.16732085798829));
#255002=CARTESIAN_POINT('Ctrl Pts',(3.63920601205468,1.49153229996037,2.17319716759931));
#255003=CARTESIAN_POINT('Ctrl Pts',(3.62959685494493,1.51497778774868,2.17448583498651));
#255004=CARTESIAN_POINT('Ctrl Pts',(3.61976444921045,1.53832228457782,2.1757745023737));
#255005=CARTESIAN_POINT('Ctrl Pts',(3.60971124706245,1.56156130613909,2.1770631697609));
#255006=CARTESIAN_POINT('Ctrl Pts',(3.56387118189431,1.6675253807822,2.18293916788961));
#255007=CARTESIAN_POINT('Ctrl Pts',(3.51328564673423,1.77164405858943,2.18881516601832));
#255008=CARTESIAN_POINT('Ctrl Pts',(3.45812483112943,1.87346247689299,2.19469116414703));
#255009=CARTESIAN_POINT('Ctrl Pts',(3.40303479650818,1.97515024434029,2.20055962234141));
#255010=CARTESIAN_POINT('Ctrl Pts',(3.3433813518564,2.07454326261412,2.2064280805358));
#255011=CARTESIAN_POINT('Ctrl Pts',(3.27938273845134,2.1712065435484,2.21229653873019));
#255012=CARTESIAN_POINT('Ctrl Pts',(3.21544919223906,2.26777154722322,2.21815903048123));
#255013=CARTESIAN_POINT('Ctrl Pts',(3.14717949124203,2.36161199188648,2.22402152223228));
#255014=CARTESIAN_POINT('Ctrl Pts',(3.07483745964873,2.45231800481523,2.22988401398333));
#255015=CARTESIAN_POINT('Ctrl Pts',(3.00023611825712,2.54585685197964,2.23592959687467));
#255016=CARTESIAN_POINT('Ctrl Pts',(2.921304114022,2.63606187505386,2.24197517976601));
#255017=CARTESIAN_POINT('Ctrl Pts',(2.83837889454358,2.72251616175361,2.24802076265735));
#255018=CARTESIAN_POINT('Ctrl Pts',(2.75805634838872,2.80625701257563,2.25387660016827));
#255019=CARTESIAN_POINT('Ctrl Pts',(2.67398780795631,2.886478728125,2.25973243767919));
#255020=CARTESIAN_POINT('Ctrl Pts',(2.58651988086599,2.96283713792793,2.26558827519011));
#255021=CARTESIAN_POINT('Ctrl Pts',(2.49906478584445,3.03918434549481,2.27144325361459));
#255022=CARTESIAN_POINT('Ctrl Pts',(2.40821160668983,3.11166910294655,2.27729823203907));
#255023=CARTESIAN_POINT('Ctrl Pts',(2.3143417713154,3.17998603228767,2.28315321046355));
#255024=CARTESIAN_POINT('Ctrl Pts',(2.22046305898802,3.24830942212981,2.28900874257355));
#255025=CARTESIAN_POINT('Ctrl Pts',(2.12356745708081,3.31246395746161,2.29486427468355));
#255026=CARTESIAN_POINT('Ctrl Pts',(2.02406666232136,3.37218670101157,2.30071980679354));
#255027=CARTESIAN_POINT('Ctrl Pts',(1.92453245139317,3.43192950174077,2.30657730541495));
#255028=CARTESIAN_POINT('Ctrl Pts',(1.82239166153794,3.48723733879669,2.31243480403637));
#255029=CARTESIAN_POINT('Ctrl Pts',(1.71808131839746,3.53789281682948,2.31829230265778));
#255030=CARTESIAN_POINT('Ctrl Pts',(1.61365340711978,3.58860538862702,2.32415640326305));
#255031=CARTESIAN_POINT('Ctrl Pts',(1.50705143347116,3.63465495520625,2.33002050386832));
#255032=CARTESIAN_POINT('Ctrl Pts',(1.39873324863807,3.67587191005813,2.33588460447359));
#255033=CARTESIAN_POINT('Ctrl Pts',(1.29034187601629,3.7171167141376,2.34175266729958));
#255034=CARTESIAN_POINT('Ctrl Pts',(1.18023237404171,3.75352227524243,2.34762073012557));
#255035=CARTESIAN_POINT('Ctrl Pts',(1.06887697324244,3.78496909050419,2.35348879295156));
#255036=CARTESIAN_POINT('Ctrl Pts',(0.957360822683537,3.81646130157035,
2.35936532676038));
#255037=CARTESIAN_POINT('Ctrl Pts',(0.844595584209227,3.84298038715884,
2.3652418605692));
#255038=CARTESIAN_POINT('Ctrl Pts',(0.731062914969777,3.8644580492426,2.37111839437802));
#255039=CARTESIAN_POINT('Ctrl Pts',(0.706207462988379,3.86916010550686,
2.37240493071052));
#255040=CARTESIAN_POINT('Ctrl Pts',(0.68131524305133,3.87362072737202,2.37369146704302));
#255041=CARTESIAN_POINT('Ctrl Pts',(0.656391326074888,3.87783953085396,
2.37497800337552));
#255042=CARTESIAN_POINT('Ctrl Pts',(0.542557172440594,3.89710792771827,
2.38085395676873));
#255043=CARTESIAN_POINT('Ctrl Pts',(0.427686078346322,3.91139145575735,
2.38672991016195));
#255044=CARTESIAN_POINT('Ctrl Pts',(0.312252207183927,3.92058510417881,
2.39260586355516));
#255045=CARTESIAN_POINT('Ctrl Pts',(0.196966462480855,3.92976695517396,
2.39847427683764));
#255046=CARTESIAN_POINT('Ctrl Pts',(0.0811197846539712,3.93387188323681,
2.40434269012011));
#255047=CARTESIAN_POINT('Ctrl Pts',(-0.0348041591618446,3.93284600137166,
2.41021110340259));
#255048=CARTESIAN_POINT('Ctrl Pts',(-0.150610240190929,3.93182116254638,
2.41607355012182));
#255049=CARTESIAN_POINT('Ctrl Pts',(-0.266493020612717,3.92567589398727,
2.42193599684104));
#255050=CARTESIAN_POINT('Ctrl Pts',(-0.381965069665893,3.91440821651947,
2.42779844356027));
#255051=CARTESIAN_POINT('Ctrl Pts',(-0.501044665878769,3.90278851725783,
2.43384404328651));
#255052=CARTESIAN_POINT('Ctrl Pts',(-0.619686999582292,3.88572104679525,
2.43988964301276));
#255053=CARTESIAN_POINT('Ctrl Pts',(-0.73735862085761,3.86326173902921,
2.445935242739));
#255054=CARTESIAN_POINT('Ctrl Pts',(-0.851335831634707,3.84150756221567,
2.45179103521304));
#255055=CARTESIAN_POINT('Ctrl Pts',(-0.964401936260121,3.81469513307558,
2.45764682768708));
#255056=CARTESIAN_POINT('Ctrl Pts',(-1.07607951783734,3.78292768517863,
2.46350262016112));
#255057=CARTESIAN_POINT('Ctrl Pts',(-1.18774071699334,3.75116489737286,
2.46935755362606));
#255058=CARTESIAN_POINT('Ctrl Pts',(-1.29801340122305,3.71444864907143,
2.475212487091));
#255059=CARTESIAN_POINT('Ctrl Pts',(-1.40643372264266,3.67293250466347,
2.48106742055595));
#255060=CARTESIAN_POINT('Ctrl Pts',(-1.51486429943933,3.63141243328215,
2.48692290783358));
#255061=CARTESIAN_POINT('Ctrl Pts',(-1.62144177963602,3.58509171085717,
2.49277839511122));
#255062=CARTESIAN_POINT('Ctrl Pts',(-1.72572142306456,3.53417240241277,
2.49863388238885));
#255063=CARTESIAN_POINT('Ctrl Pts',(-1.83003609100383,3.48323599164804,
2.504491336355));
#255064=CARTESIAN_POINT('Ctrl Pts',(-1.93205101681309,3.42769810459332,
2.51034879032115));
#255065=CARTESIAN_POINT('Ctrl Pts',(-2.03134585949666,3.36780685299881,
2.5162062442873));
#255066=CARTESIAN_POINT('Ctrl Pts',(-2.13075262648066,3.30784809249594,
2.52207030072564));
#255067=CARTESIAN_POINT('Ctrl Pts',(-2.2274328372074,3.24352638675588,2.52793435716398));
#255068=CARTESIAN_POINT('Ctrl Pts',(-2.32099488704266,3.17513334118771,
2.53379841360232));
#255069=CARTESIAN_POINT('Ctrl Pts',(-2.41462015853048,3.10669408114079,
2.53966643249487));
#255070=CARTESIAN_POINT('Ctrl Pts',(-2.50512275224329,3.03417826059038,
2.54553445138742));
#255071=CARTESIAN_POINT('Ctrl Pts',(-2.59214525227701,2.95791683302586,
2.55140247027998));
#255072=CARTESIAN_POINT('Ctrl Pts',(-2.67929338666174,2.88154530686666,
2.55727896082923));
#255073=CARTESIAN_POINT('Ctrl Pts',(-2.76295110388891,2.80141766650173,
2.56315545137848));
#255074=CARTESIAN_POINT('Ctrl Pts',(-2.84279879779158,2.717900659567,2.56903194192774));
#255075=CARTESIAN_POINT('Ctrl Pts',(-2.86028562741945,2.69961024189912,
2.57031890694854));
#255076=CARTESIAN_POINT('Ctrl Pts',(-2.87758987875138,2.68115738336707,
2.57160587196934));
#255077=CARTESIAN_POINT('Ctrl Pts',(-2.89470846482543,2.66254613174458,
2.57289283699015));
#255078=CARTESIAN_POINT('Ctrl Pts',(-2.97199921562884,2.5785159668074,2.57870350922005));
#255079=CARTESIAN_POINT('Ctrl Pts',(-3.04577010973515,2.49096272657869,
2.58451418144996));
#255080=CARTESIAN_POINT('Ctrl Pts',(-3.11567770475681,2.4002169568773,2.59032485367986));
#255081=CARTESIAN_POINT('Ctrl Pts',(-3.18547304992174,2.30961689666062,
2.59612619577725));
#255082=CARTESIAN_POINT('Ctrl Pts',(-3.251417184205,2.21583483950157,2.60192753787464));
#255083=CARTESIAN_POINT('Ctrl Pts',(-3.3132042719903,2.11923723355013,2.60772887997203));
#255084=CARTESIAN_POINT('Ctrl Pts',(-3.37493450249722,2.02272851796671,
2.61352488359928));
#255085=CARTESIAN_POINT('Ctrl Pts',(-3.43251506141284,1.92340975574695,
2.61932088722654));
#255086=CARTESIAN_POINT('Ctrl Pts',(-3.48568123427798,1.82167926183572,
2.6251168908538));
#255087=CARTESIAN_POINT('Ctrl Pts',(-3.53881202382018,1.7200164719311,2.63090903710602));
#255088=CARTESIAN_POINT('Ctrl Pts',(-3.58753407170129,1.61594551417336,
2.63670118335824));
#255089=CARTESIAN_POINT('Ctrl Pts',(-3.63162720055065,1.50989167698238,
2.64249332961046));
#255090=CARTESIAN_POINT('Ctrl Pts',(-3.67570221153748,1.40388141730318,
2.64828309587033));
#255091=CARTESIAN_POINT('Ctrl Pts',(-3.71515192401547,1.29589028846412,
2.65407286213019));
#255092=CARTESIAN_POINT('Ctrl Pts',(-3.74980351497563,1.18636528905577,
2.65986262839006));
#255093=CARTESIAN_POINT('Ctrl Pts',(-3.78445905022108,1.0768278227496,2.66565305368143));
#255094=CARTESIAN_POINT('Ctrl Pts',(-3.81431523614364,0.965756537495509,
2.67144347897279));
#255095=CARTESIAN_POINT('Ctrl Pts',(-3.83924868942866,0.85361496045954,
2.67723390426415));
#255096=CARTESIAN_POINT('Ctrl Pts',(-3.86418350428454,0.74146725957452,
2.68302464576019));
#255097=CARTESIAN_POINT('Ctrl Pts',(-3.88419496787494,0.628249565364137,
2.68881538725622));
#255098=CARTESIAN_POINT('Ctrl Pts',(-3.89921080241616,0.514435728076061,
2.69460612875226));
#255099=CARTESIAN_POINT('Ctrl Pts',(-3.91423736986617,0.40054053976273,
2.7004010093123));
#255100=CARTESIAN_POINT('Ctrl Pts',(-3.92426113293412,0.286048778251258,
2.70619588987235));
#255101=CARTESIAN_POINT('Ctrl Pts',(-3.92926170845107,0.171439279338812,
2.71199077043239));
#255102=CARTESIAN_POINT('Ctrl Pts',(-3.93180611686232,0.113123317095084,
2.71493933960993));
#255103=CARTESIAN_POINT('Ctrl Pts',(-3.93305085275237,0.0547768964339249,
2.71788790878747));
#255104=CARTESIAN_POINT('Ctrl Pts',(-3.93299840952171,-0.00353704674266808,
2.72083647796501));
#255105=CARTESIAN_POINT('',(-3.93299972773902,0.00146342229266634,3.97083647800159));
#255106=CARTESIAN_POINT('Ctrl Pts',(-3.93299840952093,-0.003537047614731,
2.7208364780091));
#255107=CARTESIAN_POINT('Ctrl Pts',(-3.93286543410983,-0.151398240717296,
2.7283128881572));
#255108=CARTESIAN_POINT('Ctrl Pts',(-3.92439064523477,-0.298892057261803,
2.73578929830529));
#255109=CARTESIAN_POINT('Ctrl Pts',(-3.9077192050117,-0.445218614595948,
2.74326570845338));
#255110=CARTESIAN_POINT('Ctrl Pts',(-3.89069193773564,-0.59466829428622,
2.75090169143706));
#255111=CARTESIAN_POINT('Ctrl Pts',(-3.86511439039472,-0.74290061369427,
2.75853767442075));
#255112=CARTESIAN_POINT('Ctrl Pts',(-3.83118937793492,-0.889087706808858,
2.76617365740444));
#255113=CARTESIAN_POINT('Ctrl Pts',(-3.82432674017123,-0.918659665462114,
2.76771832847122));
#255114=CARTESIAN_POINT('Ctrl Pts',(-3.81712267433492,-0.948148002712915,
2.769262999538));
#255115=CARTESIAN_POINT('Ctrl Pts',(-3.80957909485044,-0.977545968268768,
2.77080767060477));
#255116=CARTESIAN_POINT('Ctrl Pts',(-3.78088320660007,-1.08937626529343,
2.77668362225439));
#255117=CARTESIAN_POINT('Ctrl Pts',(-3.74721163719714,-1.20012642413732,
2.78255957390401));
#255118=CARTESIAN_POINT('Ctrl Pts',(-3.70866130388434,-1.30932056161619,
2.78843552555362));
#255119=CARTESIAN_POINT('Ctrl Pts',(-3.67016044042314,-1.41837457533184,
2.7943039368675));
#255120=CARTESIAN_POINT('Ctrl Pts',(-3.62679340000546,-1.52587615298419,
2.80017234818137));
#255121=CARTESIAN_POINT('Ctrl Pts',(-3.57870766956689,-1.63136152209838,
2.80604075949525));
#255122=CARTESIAN_POINT('Ctrl Pts',(-3.53067083093152,-1.73673963756663,
2.8119032040242));
#255123=CARTESIAN_POINT('Ctrl Pts',(-3.47792501593129,-1.84010524885018,
2.81776564855317));
#255124=CARTESIAN_POINT('Ctrl Pts',(-3.42066666284254,-1.94101225697255,
2.82362809308212));
#255125=CARTESIAN_POINT('Ctrl Pts',(-3.36161943019168,-2.0450718266823,
2.82967369354618));
#255126=CARTESIAN_POINT('Ctrl Pts',(-3.29777320981625,-2.14651622218016,
2.83571929401023));
#255127=CARTESIAN_POINT('Ctrl Pts',(-3.22939606394173,-2.24488085701618,
2.84176489447428));
#255128=CARTESIAN_POINT('Ctrl Pts',(-3.16316572142948,-2.34015718616036,
2.84762068421668));
#255129=CARTESIAN_POINT('Ctrl Pts',(-3.0926849631957,-2.43254388693036,
2.85347647395908));
#255130=CARTESIAN_POINT('Ctrl Pts',(-3.0182422722671,-2.52164680038659,
2.85933226370148));
#255131=CARTESIAN_POINT('Ctrl Pts',(-2.94381050413745,-2.6107366399843,
2.86518719423777));
#255132=CARTESIAN_POINT('Ctrl Pts',(-2.86541822382966,-2.69654333368181,
2.87104212477407));
#255133=CARTESIAN_POINT('Ctrl Pts',(-2.7833943755537,-2.77870558896333,
2.87689705531037));
#255134=CARTESIAN_POINT('Ctrl Pts',(-2.70136277144353,-2.86087561316624,
2.88275253946457));
#255135=CARTESIAN_POINT('Ctrl Pts',(-2.61569920837702,-2.93940022179111,
2.88860802361877));
#255136=CARTESIAN_POINT('Ctrl Pts',(-2.52676916708865,-3.01395530428873,
2.89446350777296));
#255137=CARTESIAN_POINT('Ctrl Pts',(-2.43780925968775,-3.08853542523736,
2.90032095842292));
#255138=CARTESIAN_POINT('Ctrl Pts',(-2.34558100880988,-3.15914310414153,
2.90617840907287));
#255139=CARTESIAN_POINT('Ctrl Pts',(-2.25048203780732,-3.22549524840863,
2.91203585972282));
#255140=CARTESIAN_POINT('Ctrl Pts',(-2.1552758763756,-3.29192218123278,
2.91789991257511));
#255141=CARTESIAN_POINT('Ctrl Pts',(-2.05719287534988,-3.35408376960859,
2.9237639654274));
#255142=CARTESIAN_POINT('Ctrl Pts',(-1.95665870430632,-3.41174086279458,
2.9296280182797));
#255143=CARTESIAN_POINT('Ctrl Pts',(-1.85605660315932,-3.46943691439902,
2.93549603342374));
#255144=CARTESIAN_POINT('Ctrl Pts',(-1.7530003998661,-3.52262222129955,
2.94136404856778));
#255145=CARTESIAN_POINT('Ctrl Pts',(-1.64793780546317,-3.57110486955021,
2.94723206371183));
#255146=CARTESIAN_POINT('Ctrl Pts',(-1.54272353587014,-3.61965751050314,
2.95310855030394));
#255147=CARTESIAN_POINT('Ctrl Pts',(-1.43549747518267,-3.6634937886144,
2.95898503689605));
#255148=CARTESIAN_POINT('Ctrl Pts',(-1.32672465644692,-3.70247088928135,
2.96486152348817));
#255149=CARTESIAN_POINT('Ctrl Pts',(-1.30290261297253,-3.71100715962338,
2.96614851706525));
#255150=CARTESIAN_POINT('Ctrl Pts',(-1.27900642578727,-3.71931055660903,
2.96743551064233));
#255151=CARTESIAN_POINT('Ctrl Pts',(-1.25504104861124,-3.72737990635524,
2.96872250421941));
#255152=CARTESIAN_POINT('Ctrl Pts',(-1.14562388076583,-3.76422161300141,
2.97459844730202));
#255153=CARTESIAN_POINT('Ctrl Pts',(-1.03440259986148,-3.79630210987866,
2.98047439038462));
#255154=CARTESIAN_POINT('Ctrl Pts',(-0.921829096808699,-3.82344348935313,
2.98635033346722));
#255155=CARTESIAN_POINT('Ctrl Pts',(-0.809400055451564,-3.85055003923099,
2.99221873615463));
#255156=CARTESIAN_POINT('Ctrl Pts',(-0.695622640555321,-3.8727299807493,
2.99808713884204));
#255157=CARTESIAN_POINT('Ctrl Pts',(-0.580966128939605,-3.88985441334569,
3.00395554152945));
#255158=CARTESIAN_POINT('Ctrl Pts',(-0.466426196970153,-3.90696143428123,
3.00981797738341));
#255159=CARTESIAN_POINT('Ctrl Pts',(-0.351009352101416,-3.91902311043383,
3.01568041323736));
#255160=CARTESIAN_POINT('Ctrl Pts',(-0.235196710299091,-3.92596122083045,
3.02154284909132));
#255161=CARTESIAN_POINT('Ctrl Pts',(-0.115765580824421,-3.93311610779436,
3.02758845278893));
#255162=CARTESIAN_POINT('Ctrl Pts',(0.00408605061782454,-3.93482189660319,
3.03363405648654));
#255163=CARTESIAN_POINT('Ctrl Pts',(0.123822550277072,-3.93105036549303,
3.03967966018416));
#255164=CARTESIAN_POINT('Ctrl Pts',(0.239799507270431,-3.92739725468215,
3.04553544118688));
#255165=CARTESIAN_POINT('Ctrl Pts',(0.355668011357442,-3.91860565406824,
3.0513912221896));
#255166=CARTESIAN_POINT('Ctrl Pts',(0.470940374846716,-3.90470282650796,
3.05724700319232));
#255167=CARTESIAN_POINT('Ctrl Pts',(0.586195824499152,-3.89080203890026,
3.06310192498021));
#255168=CARTESIAN_POINT('Ctrl Pts',(0.700854897804681,-3.87179156504165,
3.0689568467681));
#255169=CARTESIAN_POINT('Ctrl Pts',(0.814435433910154,-3.84775050178563,
3.07481176855599));
#255170=CARTESIAN_POINT('Ctrl Pts',(0.92802670975107,-3.82370716529981,
3.0806672439626));
#255171=CARTESIAN_POINT('Ctrl Pts',(1.04053884182932,-3.79463237929988,
3.08652271936921));
#255172=CARTESIAN_POINT('Ctrl Pts',(1.15150095299908,-3.76065613360783,
3.09237819477582));
#255173=CARTESIAN_POINT('Ctrl Pts',(1.26250032974675,-3.72666847731429,
3.09823563668859));
#255174=CARTESIAN_POINT('Ctrl Pts',(1.37194825600815,-3.68777620884512,
3.10409307860135));
#255175=CARTESIAN_POINT('Ctrl Pts',(1.47939074860313,-3.64415861522896,
3.10995052051412));
#255176=CARTESIAN_POINT('Ctrl Pts',(1.5869543458508,-3.60049185769824,3.11581456468873));
#255177=CARTESIAN_POINT('Ctrl Pts',(1.6925076152002,-3.55208929986645,3.12167860886333));
#255178=CARTESIAN_POINT('Ctrl Pts',(1.79561815070364,-3.49917768295119,
3.12754265303794));
#255179=CARTESIAN_POINT('Ctrl Pts',(1.89879835767266,-3.44623031382225,
3.13341065952881));
#255180=CARTESIAN_POINT('Ctrl Pts',(1.99953218650402,-3.388768022727,3.13927866601968));
#255181=CARTESIAN_POINT('Ctrl Pts',(2.09741484233863,-3.32706176364937,
3.14514667251055));
#255182=CARTESIAN_POINT('Ctrl Pts',(2.19543880983669,-3.265266420208,3.15102315055086));
#255183=CARTESIAN_POINT('Ctrl Pts',(2.29060305210702,-3.19921511592724,
3.15689962859117));
#255184=CARTESIAN_POINT('Ctrl Pts',(2.38253451786802,-3.12922007394293,
3.16277610663149));
#255185=CARTESIAN_POINT('Ctrl Pts',(2.40266951719116,-3.11388963064682,
3.164063183699));
#255186=CARTESIAN_POINT('Ctrl Pts',(2.42264957578162,-3.09837014727083,
3.16535026076652));
#255187=CARTESIAN_POINT('Ctrl Pts',(2.44247101039903,-3.08266513967384,
3.16663733783403));
#255188=CARTESIAN_POINT('Ctrl Pts',(2.53296252505151,-3.01096649865662,
3.17251327747019));
#255189=CARTESIAN_POINT('Ctrl Pts',(2.62044358809482,-2.93516163647177,
3.17838921710635));
#255190=CARTESIAN_POINT('Ctrl Pts',(2.70451887362864,-2.8555326407146,3.18426515674252));
#255191=CARTESIAN_POINT('Ctrl Pts',(2.78848626707818,-2.7760058312095,3.19013355590622));
#255192=CARTESIAN_POINT('Ctrl Pts',(2.86905627786566,-2.6926649289364,3.19600195506993));
#255193=CARTESIAN_POINT('Ctrl Pts',(2.94586521137948,-2.6058332940509,3.20187035423364));
#255194=CARTESIAN_POINT('Ctrl Pts',(3.02259604664626,-2.5190899483547,3.20773278649134));
#255195=CARTESIAN_POINT('Ctrl Pts',(3.09557313962486,-2.42886323749221,
3.21359521874903));
#255196=CARTESIAN_POINT('Ctrl Pts',(3.16446885071461,-2.33551405323473,
3.21945765100672));
#255197=CARTESIAN_POINT('Ctrl Pts',(3.23551722081132,-2.23924815675953,
3.22550325602513));
#255198=CARTESIAN_POINT('Ctrl Pts',(3.30222464492171,-2.1396617620172,3.23154886104355));
#255199=CARTESIAN_POINT('Ctrl Pts',(3.3642757222787,-2.03718871597261,3.23759446606196));
#255200=CARTESIAN_POINT('Ctrl Pts',(3.42437843919462,-1.93793325192166,
3.24345024331006));
#255201=CARTESIAN_POINT('Ctrl Pts',(3.48011261971374,-1.8359700828469,3.24930602055816));
#255202=CARTESIAN_POINT('Ctrl Pts',(3.53123551057275,-1.73172306356126,
3.25516179780626));
#255203=CARTESIAN_POINT('Ctrl Pts',(3.58235089974168,-1.62749134131413,
3.26101671578711));
#255204=CARTESIAN_POINT('Ctrl Pts',(3.62885616305942,-1.52097680574703,
3.26687163376796));
#255205=CARTESIAN_POINT('Ctrl Pts',(3.67055502879798,-1.41262690777355,
3.2727265517488));
#255206=CARTESIAN_POINT('Ctrl Pts',(3.71225783707682,-1.30426676554451,
3.27858202329986));
#255207=CARTESIAN_POINT('Ctrl Pts',(3.7491531961434,-1.19407130118298,3.28443749485092));
#255208=CARTESIAN_POINT('Ctrl Pts',(3.78109366206613,-1.08250622108299,
3.29029296640198));
#255209=CARTESIAN_POINT('Ctrl Pts',(3.81304485465657,-0.970903673729209,
3.29615040441457));
#255210=CARTESIAN_POINT('Ctrl Pts',(3.84003773168579,-0.857930992604897,
3.30200784242717));
#255211=CARTESIAN_POINT('Ctrl Pts',(3.8619753943248,-0.744066565321826,
3.30786528043976));
#255212=CARTESIAN_POINT('Ctrl Pts',(3.8839377840147,-0.630073795674539,
3.31372932066747));
#255213=CARTESIAN_POINT('Ctrl Pts',(3.90083350862215,-0.515187679243987,
3.31959336089518));
#255214=CARTESIAN_POINT('Ctrl Pts',(3.91261721947705,-0.399894353363076,
3.32545740112289));
#255215=CARTESIAN_POINT('Ctrl Pts',(3.92440889248932,-0.28452312472169,
3.33132540363478));
#255216=CARTESIAN_POINT('Ctrl Pts',(3.93108164995838,-0.168744549773994,
3.33719340614666));
#255217=CARTESIAN_POINT('Ctrl Pts',(3.93264226122829,-0.053045689752066,
3.34306140865855));
#255218=CARTESIAN_POINT('Ctrl Pts',(3.93420512552544,0.0628202026942429,
3.34893788270323));
#255219=CARTESIAN_POINT('Ctrl Pts',(3.93064112771776,0.178605739630143,
3.3548143567479));
#255220=CARTESIAN_POINT('Ctrl Pts',(3.92200893720495,0.293828004935673,
3.36069083079258));
#255221=CARTESIAN_POINT('Ctrl Pts',(3.92011824402597,0.319064930691254,
3.3619779443446));
#255222=CARTESIAN_POINT('Ctrl Pts',(3.91798460763643,0.344274871621692,
3.36326505789663));
#255223=CARTESIAN_POINT('Ctrl Pts',(3.91560897068264,0.369452823388364,
3.36455217144866));
#255224=CARTESIAN_POINT('Ctrl Pts',(3.90476368860647,0.484395465855034,
3.37042811537752));
#255225=CARTESIAN_POINT('Ctrl Pts',(3.88883501953614,0.599049782738696,
3.37630405930639));
#255226=CARTESIAN_POINT('Ctrl Pts',(3.86784422839489,0.712930589098507,
3.38218000323526));
#255227=CARTESIAN_POINT('Ctrl Pts',(3.84688037406965,0.826665255834172,
3.38804840675179));
#255228=CARTESIAN_POINT('Ctrl Pts',(3.82086739068328,0.93962798381804,3.39391681026832));
#255229=CARTESIAN_POINT('Ctrl Pts',(3.78987838490746,1.05133763730365,3.39978521378485));
#255230=CARTESIAN_POINT('Ctrl Pts',(3.75892088800736,1.16293370710045,3.40564765044983));
#255231=CARTESIAN_POINT('Ctrl Pts',(3.72299754243153,1.27327884132832,3.41151008711481));
#255232=CARTESIAN_POINT('Ctrl Pts',(3.68223256855608,1.38190170094146,3.41737252377979));
#255233=CARTESIAN_POINT('Ctrl Pts',(3.64019392861701,1.49391838708925,3.4234181271666));
#255234=CARTESIAN_POINT('Ctrl Pts',(3.59300622314532,1.60410296817546,3.42946373055342));
#255235=CARTESIAN_POINT('Ctrl Pts',(3.54086152279313,1.71195463619896,3.43550933394023));
#255236=CARTESIAN_POINT('Ctrl Pts',(3.49035407699754,1.81641994599784,3.44136511570326));
#255237=CARTESIAN_POINT('Ctrl Pts',(3.4351964574227,1.91869625234109,3.44722089746629));
#255238=CARTESIAN_POINT('Ctrl Pts',(3.37561192235501,2.01834911490919,3.45307667922932));
#255239=CARTESIAN_POINT('Ctrl Pts',(3.31603613029114,2.11798735513682,3.45893160175728));
#255240=CARTESIAN_POINT('Ctrl Pts',(3.25203492615573,2.21500256286955,3.46478652428524));
#255241=CARTESIAN_POINT('Ctrl Pts',(3.18387667346721,2.30898642874994,3.47064144681319));
#255242=CARTESIAN_POINT('Ctrl Pts',(3.11571197624547,2.40297918103984,3.47649692293872));
#255243=CARTESIAN_POINT('Ctrl Pts',(3.04338969143918,2.4939396875457,3.48235239906424));
#255244=CARTESIAN_POINT('Ctrl Pts',(2.96722008668919,2.58149064634142,3.48820787518976));
#255245=CARTESIAN_POINT('Ctrl Pts',(2.89102490138669,2.66907100796659,3.49406531779936));
#255246=CARTESIAN_POINT('Ctrl Pts',(2.81098009764579,2.75323923373456,3.49992276040895));
#255247=CARTESIAN_POINT('Ctrl Pts',(2.7274341076162,2.83365350539049,3.50578020301854));
#255248=CARTESIAN_POINT('Ctrl Pts',(2.64379394859512,2.91415841611672,3.51164424785361));
#255249=CARTESIAN_POINT('Ctrl Pts',(2.5566450243001,2.99090064118381,3.51750829268867));
#255250=CARTESIAN_POINT('Ctrl Pts',(2.46637034291811,3.06357737483061,3.52337233752374));
#255251=CARTESIAN_POINT('Ctrl Pts',(2.3760346635397,3.13630321565863,3.52924034465454));
#255252=CARTESIAN_POINT('Ctrl Pts',(2.28256935324666,3.20495785128986,3.53510835178535));
#255253=CARTESIAN_POINT('Ctrl Pts',(2.18638658096923,3.26928168235129,3.54097635891616));
#255254=CARTESIAN_POINT('Ctrl Pts',(2.09006495170927,3.33369837633271,3.54685283756161));
#255255=CARTESIAN_POINT('Ctrl Pts',(1.99101838274663,3.3937715751451,3.55272931620706));
#255256=CARTESIAN_POINT('Ctrl Pts',(1.889683833842,3.4492874638273,3.55860579485251));
#255257=CARTESIAN_POINT('Ctrl Pts',(1.86748947683889,3.46144658888462,3.55989286492277));
#255258=CARTESIAN_POINT('Ctrl Pts',(1.84518544034691,3.47338728338781,3.56117993499302));
#255259=CARTESIAN_POINT('Ctrl Pts',(1.82277643425848,3.48510761250093,3.56246700506328));
#255260=CARTESIAN_POINT('Ctrl Pts',(1.72047118090115,3.53861517256929,3.56834294749048));
#255261=CARTESIAN_POINT('Ctrl Pts',(1.6156390865796,3.58770243836325,3.57421888991769));
#255262=CARTESIAN_POINT('Ctrl Pts',(1.50869864076134,3.63212298957027,3.58009483234489));
#255263=CARTESIAN_POINT('Ctrl Pts',(1.40189542849687,3.67648653718004,3.58596323434662));
#255264=CARTESIAN_POINT('Ctrl Pts',(1.29298962315551,3.7161951230695,3.59183163634836));
#255265=CARTESIAN_POINT('Ctrl Pts',(1.18242455374738,3.75104801018266,3.59770003835009));
#255266=CARTESIAN_POINT('Ctrl Pts',(1.07197190448255,3.78586545964282,3.60356247348908));
#255267=CARTESIAN_POINT('Ctrl Pts',(0.959863738392177,3.81583690764605,
3.60942490862806));
#255268=CARTESIAN_POINT('Ctrl Pts',(0.84656300726491,3.84080982017212,3.61528734376705));
#255269=CARTESIAN_POINT('Ctrl Pts',(0.729722252198946,3.86656299869719,
3.62133294772167));
#255270=CARTESIAN_POINT('Ctrl Pts',(0.611613597500106,3.8869999823317,3.62737855167629));
#255271=CARTESIAN_POINT('Ctrl Pts',(0.492761664545086,3.90200909045004,
3.63342415563091));
#255272=CARTESIAN_POINT('Ctrl Pts',(0.377641520518336,3.916546933002,3.63927993584988));
#255273=CARTESIAN_POINT('Ctrl Pts',(0.261824515878091,3.92599260394204,
3.64513571606885));
#255274=CARTESIAN_POINT('Ctrl Pts',(0.145796597435225,3.93029672571631,
3.65099149628782));
#255275=CARTESIAN_POINT('Ctrl Pts',(0.0297857041741822,3.93460021593174,
3.65684641726771));
#255276=CARTESIAN_POINT('Ctrl Pts',(-0.0864356289817935,3.93376364185813,
3.66270133824759));
#255277=CARTESIAN_POINT('Ctrl Pts',(-0.202378803930732,3.92778968628917,
3.66855625922747));
#255278=CARTESIAN_POINT('Ctrl Pts',(-0.318332941553371,3.92181516587001,
3.67441173380258));
#255279=CARTESIAN_POINT('Ctrl Pts',(-0.434008456454422,3.9107023195692,
3.68026720837769));
#255280=CARTESIAN_POINT('Ctrl Pts',(-0.54891993244486,3.89450586182185,
3.6861226829528));
#255281=CARTESIAN_POINT('Ctrl Pts',(-0.663869999929264,3.87830396470914,
3.69198012401132));
#255282=CARTESIAN_POINT('Ctrl Pts',(-0.778055109781406,3.8570151188575,
3.69783756506984));
#255283=CARTESIAN_POINT('Ctrl Pts',(-0.890998818565252,3.83074537202818,
3.70369500612837));
#255284=CARTESIAN_POINT('Ctrl Pts',(-1.00406983219014,3.80444601517471,
3.7095590494192));
#255285=CARTESIAN_POINT('Ctrl Pts',(-1.11589624976747,3.77315464549148,
3.71542309271003));
#255286=CARTESIAN_POINT('Ctrl Pts',(-1.22601551456742,3.73702755649995,
3.72128713600086));
#255287=CARTESIAN_POINT('Ctrl Pts',(-1.33620918627586,3.70087605665706,
3.7271551415896));
#255288=CARTESIAN_POINT('Ctrl Pts',(-1.44469302312683,3.65988247666801,
3.73302314717833));
#255289=CARTESIAN_POINT('Ctrl Pts',(-1.55102482179837,3.61425109838336,
3.73889115276707));
#255290=CARTESIAN_POINT('Ctrl Pts',(-1.65751012969131,3.5685538429346,3.74476762988531));
#255291=CARTESIAN_POINT('Ctrl Pts',(-1.76183682894323,3.51820560597106,
3.75064410700355));
#255292=CARTESIAN_POINT('Ctrl Pts',(-1.86358761179898,3.46345639688872,
3.75652058412178));
#255293=CARTESIAN_POINT('Ctrl Pts',(-1.88587339436265,3.45146504964895,
3.75780766897383));
#255294=CARTESIAN_POINT('Ctrl Pts',(-1.90803572050762,3.43926274564896,
3.75909475382587));
#255295=CARTESIAN_POINT('Ctrl Pts',(-1.93007040218111,3.42685238121289,
3.76038183867792));
#255296=CARTESIAN_POINT('Ctrl Pts',(-2.03066556788191,3.37019521296542,
3.76625778078959));
#255297=CARTESIAN_POINT('Ctrl Pts',(-2.12892982139993,3.30901137172813,
3.77213372290126));
#255298=CARTESIAN_POINT('Ctrl Pts',(-2.224428569587,3.24351761808151,3.77800966501293));
#255299=CARTESIAN_POINT('Ctrl Pts',(-2.31980476686566,3.17810791076174,
3.78387806669022));
#255300=CARTESIAN_POINT('Ctrl Pts',(-2.41242217924012,3.10839952159439,
3.78974646836752));
#255301=CARTESIAN_POINT('Ctrl Pts',(-2.50187099775053,3.03465492447078,
3.79561487004482));
#255302=CARTESIAN_POINT('Ctrl Pts',(-2.59122886652548,2.96098530935043,
3.8014773048509));
#255303=CARTESIAN_POINT('Ctrl Pts',(-2.67742423332938,2.88328791058103,
3.80733973965698));
#255304=CARTESIAN_POINT('Ctrl Pts',(-2.76007702793749,2.80186791263467,
3.81320217446306));
#255305=CARTESIAN_POINT('Ctrl Pts',(-2.84531227379063,2.71790398164813,
3.81924777853929));
#255306=CARTESIAN_POINT('Ctrl Pts',(-2.92677956764456,2.62998125818639,
3.82529338261552));
#255307=CARTESIAN_POINT('Ctrl Pts',(-3.00409951337268,2.53847889763812,
3.83133898669175));
#255308=CARTESIAN_POINT('Ctrl Pts',(-3.07899171203542,2.44984959377923,
3.83719476655876));
#255309=CARTESIAN_POINT('Ctrl Pts',(-3.14999282527869,2.35786242231984,
3.84305054642577));
#255310=CARTESIAN_POINT('Ctrl Pts',(-3.21679677247992,2.26289803671371,
3.84890632629278));
#255311=CARTESIAN_POINT('Ctrl Pts',(-3.28359091723009,2.16794758566955,
3.85476124691422));
#255312=CARTESIAN_POINT('Ctrl Pts',(-3.34618888314999,2.07002112666861,
3.86061616753567));
#255313=CARTESIAN_POINT('Ctrl Pts',(-3.404326806816,1.96952989121616,3.86647108815711));
#255314=CARTESIAN_POINT('Ctrl Pts',(-3.46247022748581,1.86902915420832,
3.87232656236765));
#255315=CARTESIAN_POINT('Ctrl Pts',(-3.51615256089043,1.76596351596973,
3.8781820365782));
#255316=CARTESIAN_POINT('Ctrl Pts',(-3.56515531376704,1.66076987831506,
3.88403751078874));
#255317=CARTESIAN_POINT('Ctrl Pts',(-3.61417452352064,1.55554091287465,
3.88989495147694));
#255318=CARTESIAN_POINT('Ctrl Pts',(-3.65851085350462,1.44818290087696,
3.89575239216514));
#255319=CARTESIAN_POINT('Ctrl Pts',(-3.69799374892721,1.33915317753246,
3.90160983285335));
#255320=CARTESIAN_POINT('Ctrl Pts',(-3.73752114757169,1.23000056112453,
3.90747387576715));
#255321=CARTESIAN_POINT('Ctrl Pts',(-3.77218405240381,1.11917286085807,
3.91333791868094));
#255322=CARTESIAN_POINT('Ctrl Pts',(-3.80186161136825,1.00714313183601,
3.91920196159474));
#255323=CARTESIAN_POINT('Ctrl Pts',(-3.83155922325541,0.895037705095614,
3.92506996680205));
#255324=CARTESIAN_POINT('Ctrl Pts',(-3.85626469388085,0.78172903455963,
3.93093797200937));
#255325=CARTESIAN_POINT('Ctrl Pts',(-3.87590850276474,0.667699242320964,
3.93680597721668));
#255326=CARTESIAN_POINT('Ctrl Pts',(-3.89558067103686,0.553504827469349,
3.94268245395));
#255327=CARTESIAN_POINT('Ctrl Pts',(-3.91017654268165,0.438587621137512,
3.94855893068331));
#255328=CARTESIAN_POINT('Ctrl Pts',(-3.91967850662608,0.32343377172702,
3.95443540741663));
#255329=CARTESIAN_POINT('Ctrl Pts',(-3.92175966292067,0.298212337510988,
3.9557224957086));
#255330=CARTESIAN_POINT('Ctrl Pts',(-3.92359665559735,0.272979544951817,
3.95700958400057));
#255331=CARTESIAN_POINT('Ctrl Pts',(-3.92518963269511,0.247740483940024,
3.95829667229254));
#255332=CARTESIAN_POINT('Ctrl Pts',(-3.93036296938364,0.165774358689514,
3.9624766075167));
#255333=CARTESIAN_POINT('Ctrl Pts',(-3.93296914912035,0.0836445127446457,
3.96665654274086));
#255334=CARTESIAN_POINT('Ctrl Pts',(-3.93299972773875,0.00146342301184574,
3.97083647796501));
#255335=CARTESIAN_POINT('',(-3.93299929447449,0.00235577231090492,5.22083647792055));
#255336=CARTESIAN_POINT('Ctrl Pts',(-3.93299972773902,0.00146342229266634,
3.97083647800159));
#255337=CARTESIAN_POINT('Ctrl Pts',(-3.93304230994955,-0.112977790790186,
3.97665724357202));
#255338=CARTESIAN_POINT('Ctrl Pts',(-3.92808569945042,-0.22761977987397,
3.98247800914245));
#255339=CARTESIAN_POINT('Ctrl Pts',(-3.91810353637897,-0.34198490933754,
3.98829877471288));
#255340=CARTESIAN_POINT('Ctrl Pts',(-3.90813370529849,-0.45620875181412,
3.99411234929394));
#255341=CARTESIAN_POINT('Ctrl Pts',(-3.89315070054257,-0.570155998831521,
3.99992592387501));
#255342=CARTESIAN_POINT('Ctrl Pts',(-3.87318016355311,-0.683347949919138,
4.00573949845607));
#255343=CARTESIAN_POINT('Ctrl Pts',(-3.85322872710721,-0.79643164013262,
4.01154751272424));
#255344=CARTESIAN_POINT('Ctrl Pts',(-3.82829931666604,-0.908761058411598,
4.0173555269924));
#255345=CARTESIAN_POINT('Ctrl Pts',(-3.79846940238943,-1.01986234321661,
4.02316354126057));
#255346=CARTESIAN_POINT('Ctrl Pts',(-3.76865832275454,-1.13089347854432,
4.02896788834193));
#255347=CARTESIAN_POINT('Ctrl Pts',(-3.73395300014328,-1.24069761661006,
4.0347722354233));
#255348=CARTESIAN_POINT('Ctrl Pts',(-3.69448189796611,-1.34881151596534,
4.04057658250466));
#255349=CARTESIAN_POINT('Ctrl Pts',(-3.6550233510648,-1.45689102560877,
4.04637908329406));
#255350=CARTESIAN_POINT('Ctrl Pts',(-3.6108021815709,-1.56328096981285,
4.05218158408346));
#255351=CARTESIAN_POINT('Ctrl Pts',(-3.56199635662642,-1.66753439406212,
4.05798408487286));
#255352=CARTESIAN_POINT('Ctrl Pts',(-3.51319373768717,-1.77178097000948,
4.06378620450186));
#255353=CARTESIAN_POINT('Ctrl Pts',(-3.45980724086497,-1.87389092372813,
4.06958832413086));
#255354=CARTESIAN_POINT('Ctrl Pts',(-3.40206217040772,-1.97343912717892,
4.07539044375985));
#255355=CARTESIAN_POINT('Ctrl Pts',(-3.34430631778608,-2.07300591827859,
4.08119364676111));
#255356=CARTESIAN_POINT('Ctrl Pts',(-3.28219048585822,-2.17000964447472,
4.08699684976237));
#255357=CARTESIAN_POINT('Ctrl Pts',(-3.21598451503738,-2.26405225183514,
4.09280005276363));
#255358=CARTESIAN_POINT('Ctrl Pts',(-3.14970989622288,-2.35819237058668,
4.09860927302041));
#255359=CARTESIAN_POINT('Ctrl Pts',(-3.07933691406554,-2.44936489567792,
4.10441849327718));
#255360=CARTESIAN_POINT('Ctrl Pts',(-3.00517711848789,-2.53720308342017,
4.11022771353395));
#255361=CARTESIAN_POINT('Ctrl Pts',(-2.93097562625754,-2.62509065854786,
4.11604020004891));
#255362=CARTESIAN_POINT('Ctrl Pts',(-2.85298336717487,-2.70963985493228,
4.12185268656387));
#255363=CARTESIAN_POINT('Ctrl Pts',(-2.7715490370689,-2.79052054913101,
4.12766517307883));
#255364=CARTESIAN_POINT('Ctrl Pts',(-2.68998837512432,-2.8715267162942,
4.13348667670129));
#255365=CARTESIAN_POINT('Ctrl Pts',(-2.60497529118688,-2.94885273489322,
4.13930818032374));
#255366=CARTESIAN_POINT('Ctrl Pts',(-2.51689200387587,-3.02220840459848,
4.1451296839462));
#255367=CARTESIAN_POINT('Ctrl Pts',(-2.46100018330727,-3.06875505441162,
4.14882362459985));
#255368=CARTESIAN_POINT('Ctrl Pts',(-2.40387282263669,-3.113703957637,4.15251756525351));
#255369=CARTESIAN_POINT('Ctrl Pts',(-2.34561324049977,-3.15699026384184,
4.15621150590716));
#255370=CARTESIAN_POINT('Ctrl Pts',(-2.25293986429195,-3.22584568628788,
4.16208744835867));
#255371=CARTESIAN_POINT('Ctrl Pts',(-2.15707916056136,-3.29073060875942,
4.16796339081019));
#255372=CARTESIAN_POINT('Ctrl Pts',(-2.05840590930094,-3.35133616824021,
4.1738393332617));
#255373=CARTESIAN_POINT('Ctrl Pts',(-1.95985928259052,-3.41186395434676,
4.17970773528498));
#255374=CARTESIAN_POINT('Ctrl Pts',(-1.85850763472646,-3.46812308461244,
4.18557613730827));
#255375=CARTESIAN_POINT('Ctrl Pts',(-1.75475742700522,-3.51984593020348,
4.19144453933155));
#255376=CARTESIAN_POINT('Ctrl Pts',(-1.65111271027363,-3.57151618511265,
4.19730697448932));
#255377=CARTESIAN_POINT('Ctrl Pts',(-1.54507465203718,-3.61865914693874,
4.20316940964708));
#255378=CARTESIAN_POINT('Ctrl Pts',(-1.43707663663068,-3.66105172600037,
4.20903184480485));
#255379=CARTESIAN_POINT('Ctrl Pts',(-1.32570427845713,-3.7047688395175,
4.21507744875139));
#255380=CARTESIAN_POINT('Ctrl Pts',(-1.21224785479972,-3.74343361017472,
4.22112305269793));
#255381=CARTESIAN_POINT('Ctrl Pts',(-1.09720805204918,-3.77685364960286,
4.22716865664447));
#255382=CARTESIAN_POINT('Ctrl Pts',(-0.985780342155254,-3.80922434538819,
4.23302443687515));
#255383=CARTESIAN_POINT('Ctrl Pts',(-0.872867623950878,-3.83667461670365,
4.23888021710584));
#255384=CARTESIAN_POINT('Ctrl Pts',(-0.758942133632789,-3.85907966201747,
4.24473599733652));
#255385=CARTESIAN_POINT('Ctrl Pts',(-0.645033360051377,-3.88148141975061,
4.25059091832547));
#255386=CARTESIAN_POINT('Ctrl Pts',(-0.530112514754661,-3.89883934392723,
4.25644583931442));
#255387=CARTESIAN_POINT('Ctrl Pts',(-0.414662598033087,-3.91107963736261,
4.26230076030336));
#255388=CARTESIAN_POINT('Ctrl Pts',(-0.2992017653294,-3.92332108813815,
4.26815623488485));
#255389=CARTESIAN_POINT('Ctrl Pts',(-0.18321217223457,-3.93044390274308,
4.27401170946634));
#255390=CARTESIAN_POINT('Ctrl Pts',(-0.0671818172790369,-3.93242617266073,
4.27986718404783));
#255391=CARTESIAN_POINT('Ctrl Pts',(0.0488875048780162,-3.93440910829651,
4.28572462511006));
#255392=CARTESIAN_POINT('Ctrl Pts',(0.16499720364775,-3.9312480593145,4.29158206617229));
#255393=CARTESIAN_POINT('Ctrl Pts',(0.280660111039486,-3.92297322219657,
4.29743950723451));
#255394=CARTESIAN_POINT('Ctrl Pts',(0.39645338814494,-3.91468905807682,
4.30330355052499));
#255395=CARTESIAN_POINT('Ctrl Pts',(0.51179845682318,-3.90127963093733,
4.30916759381546));
#255396=CARTESIAN_POINT('Ctrl Pts',(0.626214003219102,-3.88282693693297,
4.31503163710594));
#255397=CARTESIAN_POINT('Ctrl Pts',(0.740706859448634,-3.86436177456441,
4.32089964269197));
#255398=CARTESIAN_POINT('Ctrl Pts',(0.854268539576944,-3.84084664319408,
4.326767648278));
#255399=CARTESIAN_POINT('Ctrl Pts',(0.966430324143622,-3.81241412081317,
4.33263565386403));
#255400=CARTESIAN_POINT('Ctrl Pts',(1.07875403450676,-3.78394055095028,
4.3385121309761));
#255401=CARTESIAN_POINT('Ctrl Pts',(1.18967342243987,-3.7505355412015,4.34438860808817));
#255402=CARTESIAN_POINT('Ctrl Pts',(1.2987372028215,-3.71238072912887,4.35026508520023));
#255403=CARTESIAN_POINT('Ctrl Pts',(1.32262470011469,-3.70402394040471,
4.35155216997408));
#255404=CARTESIAN_POINT('Ctrl Pts',(1.34642326815575,-3.69543947687454,
4.35283925474794));
#255405=CARTESIAN_POINT('Ctrl Pts',(1.37012831730859,-3.68662954392073,
4.35412633952179));
#255406=CARTESIAN_POINT('Ctrl Pts',(1.47834924184469,-3.64640945902591,
4.36000228195433));
#255407=CARTESIAN_POINT('Ctrl Pts',(1.58497621249439,-3.60135375242019,
4.36587822438687));
#255408=CARTESIAN_POINT('Ctrl Pts',(1.6895460737779,-3.55160851792279,4.37175416681941));
#255409=CARTESIAN_POINT('Ctrl Pts',(1.79398174354379,-3.50192712006463,
4.37762256882278));
#255410=CARTESIAN_POINT('Ctrl Pts',(1.89636518444536,-3.44756833804321,
4.38349097082616));
#255411=CARTESIAN_POINT('Ctrl Pts',(1.9962505675709,-3.38872729375984,4.38935937282953));
#255412=CARTESIAN_POINT('Ctrl Pts',(2.09603438936188,-3.32994607779966,
4.39522180796647));
#255413=CARTESIAN_POINT('Ctrl Pts',(2.19332485215691,-3.26669187327245,
4.40108424310342));
#255414=CARTESIAN_POINT('Ctrl Pts',(2.2876988169505,-3.19920663960978,4.40694667824036));
#255415=CARTESIAN_POINT('Ctrl Pts',(2.38502144848215,-3.12961286399652,
4.41299228219436));
#255416=CARTESIAN_POINT('Ctrl Pts',(2.4792419336473,-3.05551951225002,4.41903788614836));
#255417=CARTESIAN_POINT('Ctrl Pts',(2.5699262257194,-2.97724170909244,4.42508349010236));
#255418=CARTESIAN_POINT('Ctrl Pts',(2.65776315428894,-2.90142172254982,
4.43093927031009));
#255419=CARTESIAN_POINT('Ctrl Pts',(2.74228229737723,-2.82167641745144,
4.43679505051782));
#255420=CARTESIAN_POINT('Ctrl Pts',(2.823121786322,-2.73833386927052,4.44265083072554));
#255421=CARTESIAN_POINT('Ctrl Pts',(2.90394941335901,-2.65500355028145,
4.44850575169077));
#255422=CARTESIAN_POINT('Ctrl Pts',(2.98109817257947,-2.56807733400152,
4.45436067265599));
#255423=CARTESIAN_POINT('Ctrl Pts',(3.05424310828056,-2.47792010273147,
4.46021559362122));
#255424=CARTESIAN_POINT('Ctrl Pts',(3.12739495994839,-2.38775434695583,
4.46607106817827));
#255425=CARTESIAN_POINT('Ctrl Pts',(3.19654197547533,-2.29435728944028,
4.47192654273532));
#255426=CARTESIAN_POINT('Ctrl Pts',(3.26139999412125,-2.1981262653328,4.47778201729237));
#255427=CARTESIAN_POINT('Ctrl Pts',(3.32627979443366,-2.10186292336984,
4.48363945832938));
#255428=CARTESIAN_POINT('Ctrl Pts',(3.38686750309089,-2.00276406436294,
4.4894968993664));
#255429=CARTESIAN_POINT('Ctrl Pts',(3.44292311037051,-1.90125470573426,
4.49535434040341));
#255430=CARTESIAN_POINT('Ctrl Pts',(3.49904190084925,-1.7996309306122,4.50121838366777));
#255431=CARTESIAN_POINT('Ctrl Pts',(3.5506181945708,-1.69559159454111,4.50708242693213));
#255432=CARTESIAN_POINT('Ctrl Pts',(3.59745861284973,-1.58958501780599,
4.51294647019649));
#255433=CARTESIAN_POINT('Ctrl Pts',(3.64433068088722,-1.48350681313326,
4.51881447575582));
#255434=CARTESIAN_POINT('Ctrl Pts',(3.68646035188462,-1.37545910450063,
4.52468248131514));
#255435=CARTESIAN_POINT('Ctrl Pts',(3.7237035278962,-1.26590719894209,4.53055048687446));
#255436=CARTESIAN_POINT('Ctrl Pts',(3.7610004711561,-1.15619713542978,4.5364269639592));
#255437=CARTESIAN_POINT('Ctrl Pts',(3.79339672604397,-1.04497893597937,
4.54230344104394));
#255438=CARTESIAN_POINT('Ctrl Pts',(3.82079883474219,-0.932730006182235,
4.54817991812868));
#255439=CARTESIAN_POINT('Ctrl Pts',(3.82680053314686,-0.908144882814232,
4.54946700313126));
#255440=CARTESIAN_POINT('Ctrl Pts',(3.83256285342018,-0.883510338981573,
4.55075408813383));
#255441=CARTESIAN_POINT('Ctrl Pts',(3.83808514540956,-0.858831425011042,
4.55204117313641));
#255442=CARTESIAN_POINT('Ctrl Pts',(3.86329612230202,-0.746164523108877,
4.55791711564744));
#255443=CARTESIAN_POINT('Ctrl Pts',(3.88358348786856,-0.632200709728735,
4.56379305815847));
#255444=CARTESIAN_POINT('Ctrl Pts',(3.89881750983979,-0.517407986956778,
4.56966900066949));
#255445=CARTESIAN_POINT('Ctrl Pts',(3.91403198242897,-0.40276257438288,
4.57553740275257));
#255446=CARTESIAN_POINT('Ctrl Pts',(3.9242059540972,-0.287290773350273,
4.58140580483565));
#255447=CARTESIAN_POINT('Ctrl Pts',(3.92926024759816,-0.171472757733917,
4.58727420691872));
#255448=CARTESIAN_POINT('Ctrl Pts',(3.93430940200193,-0.0557725033907323,
4.59313664213648));
#255449=CARTESIAN_POINT('Ctrl Pts',(3.93424921494047,0.0602728553535137,
4.59899907735424));
#255450=CARTESIAN_POINT('Ctrl Pts',(3.92905214817471,0.176176663958865,
4.604861512572));
#255451=CARTESIAN_POINT('Ctrl Pts',(3.92369270179007,0.295701826130957,
4.61090711649612));
#255452=CARTESIAN_POINT('Ctrl Pts',(3.91287004200091,0.415076004530788,
4.61695272042025));
#255453=CARTESIAN_POINT('Ctrl Pts',(3.89661205092077,0.533763547480533,
4.62299832434438));
#255454=CARTESIAN_POINT('Ctrl Pts',(3.88086453835968,0.648724465113842,
4.62885410463515));
#255455=CARTESIAN_POINT('Ctrl Pts',(3.86001797510522,0.763040782344009,
4.63470988492592));
#255456=CARTESIAN_POINT('Ctrl Pts',(3.83415041616872,0.876230327136198,
4.64056566521669));
#255457=CARTESIAN_POINT('Ctrl Pts',(3.80828665288148,0.9894032631787,4.64642058626565));
#255458=CARTESIAN_POINT('Ctrl Pts',(3.77740345085058,1.10144935326724,4.65227550731462));
#255459=CARTESIAN_POINT('Ctrl Pts',(3.74162983822925,1.21189733627588,4.65813042836358));
#255460=CARTESIAN_POINT('Ctrl Pts',(3.70585284315408,1.32235576232275,4.66398590300495));
#255461=CARTESIAN_POINT('Ctrl Pts',(3.66518464547931,1.43121538821599,4.66984137764632));
#255462=CARTESIAN_POINT('Ctrl Pts',(3.61980370928726,1.53802149082195,4.67569685228768));
#255463=CARTESIAN_POINT('Ctrl Pts',(3.57440753253252,1.64486346278715,4.6815542934096));
#255464=CARTESIAN_POINT('Ctrl Pts',(3.5242956313901,1.74965016043284,4.68741173453152));
#255465=CARTESIAN_POINT('Ctrl Pts',(3.46969373282064,1.85194881150241,4.69326917565344));
#255466=CARTESIAN_POINT('Ctrl Pts',(3.41503028960123,1.9543627687213,4.69913321900299));
#255467=CARTESIAN_POINT('Ctrl Pts',(3.35586694238364,2.05428271775246,4.70499726235254));
#255468=CARTESIAN_POINT('Ctrl Pts',(3.29247435887988,2.15130230235514,4.71086130570208));
#255469=CARTESIAN_POINT('Ctrl Pts',(3.22903894142714,2.2483874424488,4.7167293113469));
#255470=CARTESIAN_POINT('Ctrl Pts',(3.16136883757253,2.34256798137124,4.72259731699172));
#255471=CARTESIAN_POINT('Ctrl Pts',(3.08977580182442,2.43346964116265,4.72846532263654));
#255472=CARTESIAN_POINT('Ctrl Pts',(3.01807940860798,2.52450253390604,4.73434179980657));
#255473=CARTESIAN_POINT('Ctrl Pts',(2.94244904960256,2.61224678938462,4.7402182769766));
#255474=CARTESIAN_POINT('Ctrl Pts',(2.86323420694151,2.69636401032947,4.74609475414663));
#255475=CARTESIAN_POINT('Ctrl Pts',(2.84588432714771,2.7147876241745,4.7473818383481));
#255476=CARTESIAN_POINT('Ctrl Pts',(2.82836262380406,2.73303739673917,4.74866892254958));
#255477=CARTESIAN_POINT('Ctrl Pts',(2.81067297833481,2.75111003212495,4.74995600675105));
#255478=CARTESIAN_POINT('Ctrl Pts',(2.72991420668571,2.83361727268861,4.75583194922262));
#255479=CARTESIAN_POINT('Ctrl Pts',(2.64538613112808,2.91270160876023,4.76170789169419));
#255480=CARTESIAN_POINT('Ctrl Pts',(2.55741059061983,2.98799934253432,4.76758383416576));
#255481=CARTESIAN_POINT('Ctrl Pts',(2.46954794659865,3.06320044888699,4.77345223620894));
#255482=CARTESIAN_POINT('Ctrl Pts',(2.3782469465681,3.13462435063305,4.77932063825213));
#255483=CARTESIAN_POINT('Ctrl Pts',(2.28386717217618,3.20194311939734,4.78518904029531));
#255484=CARTESIAN_POINT('Ctrl Pts',(2.18958336112032,3.26919343987733,4.7910514754728));
#255485=CARTESIAN_POINT('Ctrl Pts',(2.09222733662673,3.33234669175443,4.7969139106503));
#255486=CARTESIAN_POINT('Ctrl Pts',(1.99219224047247,3.39111472483626,4.80277634582779));
#255487=CARTESIAN_POINT('Ctrl Pts',(1.88903159936587,3.45171893478219,4.80882194976687));
#255488=CARTESIAN_POINT('Ctrl Pts',(1.78302206161625,3.50765910302015,4.81486755370595));
#255489=CARTESIAN_POINT('Ctrl Pts',(1.67462804574086,3.55866687235798,4.82091315764503));
#255490=CARTESIAN_POINT('Ctrl Pts',(1.56963745360849,3.60807306755133,4.82676893789484));
#255491=CARTESIAN_POINT('Ctrl Pts',(1.46241028418778,3.65285178513794,4.83262471814466));
#255492=CARTESIAN_POINT('Ctrl Pts',(1.35339343095619,3.69280587372863,4.83848049839448));
#255493=CARTESIAN_POINT('Ctrl Pts',(1.24439257420256,3.73275409969643,4.84433541940229));
#255494=CARTESIAN_POINT('Ctrl Pts',(1.13360294327495,3.76787896237897,4.85019034041011));
#255495=CARTESIAN_POINT('Ctrl Pts',(1.02149004340447,3.79803200239618,4.85604526141792));
#255496=CARTESIAN_POINT('Ctrl Pts',(0.909366543076926,3.82818789343238,
4.86190073601803));
#255497=CARTESIAN_POINT('Ctrl Pts',(0.795919923698388,3.85337092009224,
4.86775621061815));
#255498=CARTESIAN_POINT('Ctrl Pts',(0.681628745774486,3.87348309057028,
4.87361168521827));
#255499=CARTESIAN_POINT('Ctrl Pts',(0.567299184735177,3.89360201544332,
4.87946912629875));
#255500=CARTESIAN_POINT('Ctrl Pts',(0.452124907436328,3.9086466262942,4.88532656737923));
#255501=CARTESIAN_POINT('Ctrl Pts',(0.336591806513044,3.91857052453931,
4.89118400845971));
#255502=CARTESIAN_POINT('Ctrl Pts',(0.220928482197998,3.92850560852841,
4.89704805176794));
#255503=CARTESIAN_POINT('Ctrl Pts',(0.104905938474842,3.93330842463923,
4.90291209507617));
#255504=CARTESIAN_POINT('Ctrl Pts',(-0.0109876093889282,3.93298465194563,
4.9087761383844));
#255505=CARTESIAN_POINT('Ctrl Pts',(-0.126959465756043,3.93266066048097,
4.91464414398789));
#255506=CARTESIAN_POINT('Ctrl Pts',(-0.242801741441477,3.92720320185946,
4.92051214959137));
#255507=CARTESIAN_POINT('Ctrl Pts',(-0.358030746336293,3.91666988456748,
4.92638015519486));
#255508=CARTESIAN_POINT('Ctrl Pts',(-0.473426105103055,3.90612136053032,
4.93225663232384));
#255509=CARTESIAN_POINT('Ctrl Pts',(-0.588206018844008,3.89048240933832,
4.93813310945282));
#255510=CARTESIAN_POINT('Ctrl Pts',(-0.701896341120765,3.86986182263932,
4.9440095865818));
#255511=CARTESIAN_POINT('Ctrl Pts',(-0.726797154847766,3.86534543656484,
4.94529667117642));
#255512=CARTESIAN_POINT('Ctrl Pts',(-0.751645756990695,3.86059026576184,
4.94658375577104));
#255513=CARTESIAN_POINT('Ctrl Pts',(-0.776437269383352,3.85559777034801,
4.94787084036566));
#255514=CARTESIAN_POINT('Ctrl Pts',(-0.889618253164547,3.83280547218116,
4.95374678283829));
#255515=CARTESIAN_POINT('Ctrl Pts',(-1.00198150404016,3.80498771482945,
4.95962272531091));
#255516=CARTESIAN_POINT('Ctrl Pts',(-1.11304671264367,3.77221632670677,
4.96549866778354));
#255517=CARTESIAN_POINT('Ctrl Pts',(-1.22396939445008,3.73948699316666,
4.9713670698277));
#255518=CARTESIAN_POINT('Ctrl Pts',(-1.33359695434867,3.70181678663287,
4.97723547187186));
#255519=CARTESIAN_POINT('Ctrl Pts',(-1.44145852512785,3.65932867071766,
4.98310387391602));
#255520=CARTESIAN_POINT('Ctrl Pts',(-1.54921042456725,3.61688375581058,
4.98896630909441));
#255521=CARTESIAN_POINT('Ctrl Pts',(-1.65519952481822,3.56963082618071,
4.9948287442728));
#255522=CARTESIAN_POINT('Ctrl Pts',(-1.75897004084498,3.51774265622285,
5.00069117945119));
#255523=CARTESIAN_POINT('Ctrl Pts',(-1.86598281306738,3.46423326718497,
5.00673678338991));
#255524=CARTESIAN_POINT('Ctrl Pts',(-1.97063565652213,3.40579435146224,
5.01278238732862));
#255525=CARTESIAN_POINT('Ctrl Pts',(-2.07245056523527,3.3426692409893,5.01882799126733));
#255526=CARTESIAN_POINT('Ctrl Pts',(-2.17106862518289,3.2815261725772,5.02468377151782));
#255527=CARTESIAN_POINT('Ctrl Pts',(-2.26702392365972,3.21598702314574,
5.0305395517683));
#255528=CARTESIAN_POINT('Ctrl Pts',(-2.35990771750162,3.14631920899268,
5.03639533201879));
#255529=CARTESIAN_POINT('Ctrl Pts',(-2.4527778821325,3.07666161747696,5.04225025302719));
#255530=CARTESIAN_POINT('Ctrl Pts',(-2.54257710820565,3.0028768134861,5.0481051740356));
#255531=CARTESIAN_POINT('Ctrl Pts',(-2.62892735203609,2.92527434229962,
5.053960095044));
#255532=CARTESIAN_POINT('Ctrl Pts',(-2.71528576042096,2.8476645336747,5.0598155696446));
#255533=CARTESIAN_POINT('Ctrl Pts',(-2.79819423127799,2.76623661619892,
5.0656710442452));
#255534=CARTESIAN_POINT('Ctrl Pts',(-2.87730993582532,2.68133857116196,
5.0715265188458));
#255535=CARTESIAN_POINT('Ctrl Pts',(-2.95645221028981,2.59641201428862,
5.0773839599267));
#255536=CARTESIAN_POINT('Ctrl Pts',(-3.03179890437162,2.50801331428315,
5.08324140100761));
#255537=CARTESIAN_POINT('Ctrl Pts',(-3.10304646532606,2.41652470172093,
5.08909884208852));
#255538=CARTESIAN_POINT('Ctrl Pts',(-3.1743743331257,2.32493296756762,5.09496288539703));
#255539=CARTESIAN_POINT('Ctrl Pts',(-3.24159359235149,2.2302446953858,5.10082692870555));
#255540=CARTESIAN_POINT('Ctrl Pts',(-3.3044431009817,2.13287242759018,5.10669097201407));
#255541=CARTESIAN_POINT('Ctrl Pts',(-3.36733507660839,2.03543436599851,
5.11255897761779));
#255542=CARTESIAN_POINT('Ctrl Pts',(-3.42585121448078,1.93530905299102,
5.11842698322151));
#255543=CARTESIAN_POINT('Ctrl Pts',(-3.4797763885994,1.83293351907431,5.12429498882523));
#255544=CARTESIAN_POINT('Ctrl Pts',(-3.53377941344132,1.73041018759377,
5.13017146595432));
#255545=CARTESIAN_POINT('Ctrl Pts',(-3.58317807225354,1.6256305239824,5.13604794308341));
#255546=CARTESIAN_POINT('Ctrl Pts',(-3.62780536252005,1.51905143154232,
5.1419244202125));
#255547=CARTESIAN_POINT('Ctrl Pts',(-3.63757977264724,1.49570814194818,
5.14321150480177));
#255548=CARTESIAN_POINT('Ctrl Pts',(-3.64712548538044,1.47227858708217,
5.14449858939103));
#255549=CARTESIAN_POINT('Ctrl Pts',(-3.65644106839263,1.44876765334257,
5.1457856739803));
#255550=CARTESIAN_POINT('Ctrl Pts',(-3.70437574779256,1.32778874416156,
5.15240855384368));
#255551=CARTESIAN_POINT('Ctrl Pts',(-3.74634559922482,1.20431996042898,
5.15903143370706));
#255552=CARTESIAN_POINT('Ctrl Pts',(-3.78211649997361,1.07892714333608,
5.16565431357044));
#255553=CARTESIAN_POINT('Ctrl Pts',(-3.81777367070408,0.9539330002236,5.17225613664653));
#255554=CARTESIAN_POINT('Ctrl Pts',(-3.84727112473125,0.827027227948243,
5.17885795972262));
#255555=CARTESIAN_POINT('Ctrl Pts',(-3.87042347272765,0.698792631442877,
5.18545978279872));
#255556=CARTESIAN_POINT('Ctrl Pts',(-3.89343898965604,0.571315905232001,
5.19202258890329));
#255557=CARTESIAN_POINT('Ctrl Pts',(-3.91018408115724,0.442526219216769,
5.19858539500787));
#255558=CARTESIAN_POINT('Ctrl Pts',(-3.92052425525767,0.313015277480708,
5.20514820111245));
#255559=CARTESIAN_POINT('Ctrl Pts',(-3.92876359226008,0.209817373451253,
5.21037762671515));
#255560=CARTESIAN_POINT('Ctrl Pts',(-3.93293711707552,0.106161927577145,
5.21560705231785));
#255561=CARTESIAN_POINT('Ctrl Pts',(-3.93299929447449,0.00235577231090366,
5.22083647792055));
#255562=CARTESIAN_POINT('',(-3.93299863531357,-0.00327637323301094,6.4708364779999));
#255563=CARTESIAN_POINT('Ctrl Pts',(-3.93299929447502,0.00235577142831299,
5.22083647796501));
#255564=CARTESIAN_POINT('Ctrl Pts',(-3.93306949457354,-0.114844452091178,
5.22674065434008));
#255565=CARTESIAN_POINT('Ctrl Pts',(-3.92789664864031,-0.232061737731447,
5.23264483071515));
#255566=CARTESIAN_POINT('Ctrl Pts',(-3.91750276642645,-0.348799476836041,
5.23854900709023));
#255567=CARTESIAN_POINT('Ctrl Pts',(-3.90710756542916,-0.465552027710973,
5.24445393259154));
#255568=CARTESIAN_POINT('Ctrl Pts',(-3.89149004524592,-0.581824509508502,
5.25035885809286));
#255569=CARTESIAN_POINT('Ctrl Pts',(-3.87072410551644,-0.697125454257667,
5.25626378359418));
#255570=CARTESIAN_POINT('Ctrl Pts',(-3.84995084376558,-0.812467053848058,
5.26217079115831));
#255571=CARTESIAN_POINT('Ctrl Pts',(-3.82402562123884,-0.926836038212441,
5.26807779872244));
#255572=CARTESIAN_POINT('Ctrl Pts',(-3.79307334122479,-1.03975171463663,
5.27398480628656));
#255573=CARTESIAN_POINT('Ctrl Pts',(-3.76208114843012,-1.15281299515265,
5.27989943090174));
#255574=CARTESIAN_POINT('Ctrl Pts',(-3.72604905630204,-1.26441683501574,
5.28581405551692));
#255575=CARTESIAN_POINT('Ctrl Pts',(-3.68515184878624,-1.37409783181088,
5.29172868013209));
#255576=CARTESIAN_POINT('Ctrl Pts',(-3.64422778518474,-1.48385085313846,
5.29764718872066));
#255577=CARTESIAN_POINT('Ctrl Pts',(-3.59843239766944,-1.59167814466311,
5.30356569730922));
#255578=CARTESIAN_POINT('Ctrl Pts',(-3.54798787396473,-1.69713613072117,
5.30948420589778));
#255579=CARTESIAN_POINT('Ctrl Pts',(-3.49745156616804,-1.80278599817254,
5.31541348324571));
#255580=CARTESIAN_POINT('Ctrl Pts',(-3.44224940748687,-1.90605758935708,
5.32134276059362));
#255581=CARTESIAN_POINT('Ctrl Pts',(-3.3826490056056,-2.00653300617644,
5.32727203794154));
#255582=CARTESIAN_POINT('Ctrl Pts',(-3.32760332093607,-2.09932999976544,
5.33274819449267));
#255583=CARTESIAN_POINT('Ctrl Pts',(-3.26880657120879,-2.18974197557187,
5.3382243510438));
#255584=CARTESIAN_POINT('Ctrl Pts',(-3.2065003103526,-2.27746454631212,
5.34370050759492));
#255585=CARTESIAN_POINT('Ctrl Pts',(-3.13964539097391,-2.37159128917778,
5.34957645007164));
#255586=CARTESIAN_POINT('Ctrl Pts',(-3.06853203668357,-2.4629270359288,
5.35545239254837));
#255587=CARTESIAN_POINT('Ctrl Pts',(-2.9934212178758,-2.55106221256381,
5.36132833502509));
#255588=CARTESIAN_POINT('Ctrl Pts',(-2.91840678662658,-2.63908428785559,
5.36719673707344));
#255589=CARTESIAN_POINT('Ctrl Pts',(-2.83940535799492,-2.72391364977943,
5.37306513912178));
#255590=CARTESIAN_POINT('Ctrl Pts',(-2.75672077677496,-2.80517014794063,
5.37893354117013));
#255591=CARTESIAN_POINT('Ctrl Pts',(-2.67412026746886,-2.88634402623229,
5.38479597635278));
#255592=CARTESIAN_POINT('Ctrl Pts',(-2.58784434746087,-2.96395197928577,
5.39065841153543));
#255593=CARTESIAN_POINT('Ctrl Pts',(-2.49823623211291,-3.03764789410463,
5.39652084671807));
#255594=CARTESIAN_POINT('Ctrl Pts',(-2.40582835755744,-3.11364639965725,
5.40256645065522));
#255595=CARTESIAN_POINT('Ctrl Pts',(-2.30987692912422,-3.18548404916728,
5.40861205459237));
#255596=CARTESIAN_POINT('Ctrl Pts',(-2.21079865791848,-3.25282312678477,
5.41465765852951));
#255597=CARTESIAN_POINT('Ctrl Pts',(-2.11483130870848,-3.31804784960798,
5.42051343878446));
#255598=CARTESIAN_POINT('Ctrl Pts',(-2.01593090453599,-3.37905202558977,
5.42636921903941));
#255599=CARTESIAN_POINT('Ctrl Pts',(-1.91450798829165,-3.43557100971111,
5.43222499929437));
#255600=CARTESIAN_POINT('Ctrl Pts',(-1.8130999542368,-3.49208170057624,
5.4380799203073));
#255601=CARTESIAN_POINT('Ctrl Pts',(-1.70917050457927,-3.54410830737973,
5.44393484132023));
#255602=CARTESIAN_POINT('Ctrl Pts',(-1.60315618317904,-3.59143136539386,
5.44978976233316));
#255603=CARTESIAN_POINT('Ctrl Pts',(-1.49713183795337,-3.63875889787961,
5.45564523693834));
#255604=CARTESIAN_POINT('Ctrl Pts',(-1.38902260604292,-3.68138182924245,
5.46150071154352));
#255605=CARTESIAN_POINT('Ctrl Pts',(-1.27928582203951,-3.71912849812005,
5.4673561861487));
#255606=CARTESIAN_POINT('Ctrl Pts',(-1.16951218445099,-3.75688784369568,
5.47321362723424));
#255607=CARTESIAN_POINT('Ctrl Pts',(-1.05811029797793,-3.78976753620867,
5.47907106831979));
#255608=CARTESIAN_POINT('Ctrl Pts',(-0.945552811405881,-3.81764572489937,
5.48492850940534));
#255609=CARTESIAN_POINT('Ctrl Pts',(-0.832868455413806,-3.84555533655213,
5.49079255271857));
#255610=CARTESIAN_POINT('Ctrl Pts',(-0.719026300455215,-3.86845209334975,
5.4966565960318));
#255611=CARTESIAN_POINT('Ctrl Pts',(-0.604509437504849,-3.88626521739929,
5.50252063934503));
#255612=CARTESIAN_POINT('Ctrl Pts',(-0.4899151962689,-3.90409037765874,
5.50838864495347));
#255613=CARTESIAN_POINT('Ctrl Pts',(-0.374645748461646,-3.91682502002907,
5.51425665056191));
#255614=CARTESIAN_POINT('Ctrl Pts',(-0.259187840598699,-3.92445036448237,
5.52012465617036));
#255615=CARTESIAN_POINT('Ctrl Pts',(-0.143563248402915,-3.93208671749693,
5.52600113330421));
#255616=CARTESIAN_POINT('Ctrl Pts',(-0.0277500641979943,-3.93459904335077,
5.53187761043806));
#255617=CARTESIAN_POINT('Ctrl Pts',(0.0877663834234242,-3.93202060802595,
5.53775408757191));
#255618=CARTESIAN_POINT('Ctrl Pts',(0.113067159916258,-3.93145587099328,
5.53904117211779));
#255619=CARTESIAN_POINT('Ctrl Pts',(0.138353728543505,-3.93064712100273,
5.54032825666368));
#255620=CARTESIAN_POINT('Ctrl Pts',(0.163621042766362,-3.92959503694262,
5.54161534120956));
#255621=CARTESIAN_POINT('Ctrl Pts',(0.278974214713604,-3.92479194499473,
5.54749128368696));
#255622=CARTESIAN_POINT('Ctrl Pts',(0.394306017157791,-3.9148973433921,
5.55336722616436));
#255623=CARTESIAN_POINT('Ctrl Pts',(0.509130817813535,-3.89990702586004,
5.55924316864175));
#255624=CARTESIAN_POINT('Ctrl Pts',(0.623808267097234,-3.88493594497236,
5.56511157069077));
#255625=CARTESIAN_POINT('Ctrl Pts',(0.737979602885249,-3.8648822057332,
5.57097997273978));
#255626=CARTESIAN_POINT('Ctrl Pts',(0.851160518054364,-3.83979358462215,
5.5768483747888));
#255627=CARTESIAN_POINT('Ctrl Pts',(0.964226353289277,-3.81473047308454,
5.5827108099721));
#255628=CARTESIAN_POINT('Ctrl Pts',(1.07630337041335,-3.78464275157337,
5.58857324515541));
#255629=CARTESIAN_POINT('Ctrl Pts',(1.18691436524442,-3.74962975366588,
5.59443568033871));
#255630=CARTESIAN_POINT('Ctrl Pts',(1.30098134336964,-3.71352279275741,
5.60048128427561));
#255631=CARTESIAN_POINT('Ctrl Pts',(1.41348874002193,-3.67217777851635,
5.6065268882125));
#255632=CARTESIAN_POINT('Ctrl Pts',(1.52392636419819,-3.62576025634648,
5.61257249214939));
#255633=CARTESIAN_POINT('Ctrl Pts',(1.63089639827218,-3.58080018078186,
5.618428272405));
#255634=CARTESIAN_POINT('Ctrl Pts',(1.7359242839985,-3.53108154589111,5.62428405266061));
#255635=CARTESIAN_POINT('Ctrl Pts',(1.83856447186049,-3.47680452180049,
5.63013983291621));
#255636=CARTESIAN_POINT('Ctrl Pts',(1.94118959891774,-3.42253546199442,
5.63599475392979));
#255637=CARTESIAN_POINT('Ctrl Pts',(2.04142735999498,-3.36370953591843,
5.64184967494337));
#255638=CARTESIAN_POINT('Ctrl Pts',(2.13885593538562,-3.30057332711541,
5.64770459595695));
#255639=CARTESIAN_POINT('Ctrl Pts',(2.23629372280573,-3.23743114868168,
5.65356007056279));
#255640=CARTESIAN_POINT('Ctrl Pts',(2.33092145012147,-3.16997810183942,
5.65941554516862));
#255641=CARTESIAN_POINT('Ctrl Pts',(2.42234606505718,-3.09850424255026,
5.66527101977446));
#255642=CARTESIAN_POINT('Ctrl Pts',(2.51380138368802,-3.02700637975192,
5.67112846086063));
#255643=CARTESIAN_POINT('Ctrl Pts',(2.60205112588368,-2.95148527346462,
5.6769859019468));
#255644=CARTESIAN_POINT('Ctrl Pts',(2.68673567297893,-2.87227095232021,
5.68284334303296));
#255645=CARTESIAN_POINT('Ctrl Pts',(2.77151567244853,-2.79296734457871,
5.68870738634679));
#255646=CARTESIAN_POINT('Ctrl Pts',(2.85272215470362,-2.70996249556236,
5.69457142966062));
#255647=CARTESIAN_POINT('Ctrl Pts',(2.93003264682825,-2.62362300807883,
5.70043547297445));
#255648=CARTESIAN_POINT('Ctrl Pts',(3.00739537714036,-2.53722518157546,
5.70630347858351));
#255649=CARTESIAN_POINT('Ctrl Pts',(3.08085661454114,-2.44748854849365,
5.71217148419256));
#255650=CARTESIAN_POINT('Ctrl Pts',(3.15013550395417,-2.35481109788607,
5.71803948980162));
#255651=CARTESIAN_POINT('Ctrl Pts',(3.2195144099501,-2.26199985064868,5.72391596693605));
#255652=CARTESIAN_POINT('Ctrl Pts',(3.28469868691709,-2.16623965298586,
5.72979244407048));
#255653=CARTESIAN_POINT('Ctrl Pts',(3.34545190124147,-2.06795565147801,
5.73566892120491));
#255654=CARTESIAN_POINT('Ctrl Pts',(3.35875826168645,-2.04642917975824,
5.73695600574466));
#255655=CARTESIAN_POINT('Ctrl Pts',(3.37185223860402,-2.02478172281951,
5.73824309028442));
#255656=CARTESIAN_POINT('Ctrl Pts',(3.38473165277341,-2.00301788277433,
5.73953017482417));
#255657=CARTESIAN_POINT('Ctrl Pts',(3.4435301966768,-1.90365916291552,5.74540611730284));
#255658=CARTESIAN_POINT('Ctrl Pts',(3.49804702800377,-1.80154529067286,
5.7512820597815));
#255659=CARTESIAN_POINT('Ctrl Pts',(3.54801412104477,-1.69708125818031,
5.75715800226016));
#255660=CARTESIAN_POINT('Ctrl Pts',(3.59791709274918,-1.59275128138288,
5.76302640431046));
#255661=CARTESIAN_POINT('Ctrl Pts',(3.64328176091414,-1.48607751112254,
5.76889480636076));
#255662=CARTESIAN_POINT('Ctrl Pts',(3.68388441772059,-1.37749214040422,
5.77476320841106));
#255663=CARTESIAN_POINT('Ctrl Pts',(3.72444579061415,-1.26901717696806,
5.78062564359569));
#255664=CARTESIAN_POINT('Ctrl Pts',(3.76025463963724,-1.15863486366175,
5.78648807878032));
#255665=CARTESIAN_POINT('Ctrl Pts',(3.79113436472628,-1.0467995169045,5.79235051396495));
#255666=CARTESIAN_POINT('Ctrl Pts',(3.82297891083624,-0.931469932646011,
5.79839611790136));
#255667=CARTESIAN_POINT('Ctrl Pts',(3.84958106106959,-0.814595426852911,
5.80444172183777));
#255668=CARTESIAN_POINT('Ctrl Pts',(3.87080177877556,-0.696694042911201,
5.81048732577418));
#255669=CARTESIAN_POINT('Ctrl Pts',(3.89135619502379,-0.582494600867895,
5.81634310603113));
#255670=CARTESIAN_POINT('Ctrl Pts',(3.90686198668723,-0.467332237805583,
5.82219888628808));
#255671=CARTESIAN_POINT('Ctrl Pts',(3.91724436245317,-0.351689642765965,
5.82805466654503));
#255672=CARTESIAN_POINT('Ctrl Pts',(3.92762521477168,-0.236064016425919,
5.83390958755997));
#255673=CARTESIAN_POINT('Ctrl Pts',(3.93288410918128,-0.119958709227479,
5.83976450857491));
#255674=CARTESIAN_POINT('Ctrl Pts',(3.93299810406709,-0.00386178775522389,
5.84561942958985));
#255675=CARTESIAN_POINT('Ctrl Pts',(3.9331121097313,0.112246110868742,5.85147490419704));
#255676=CARTESIAN_POINT('Ctrl Pts',(3.92808024843203,0.228345209412011,
5.85733037880423));
#255677=CARTESIAN_POINT('Ctrl Pts',(3.91793170546246,0.343947890431156,
5.86318585341143));
#255678=CARTESIAN_POINT('Ctrl Pts',(3.9077797542447,0.459589395016366,5.86904329449901));
#255679=CARTESIAN_POINT('Ctrl Pts',(3.89250774048567,0.574733739618474,
5.87490073558659));
#255680=CARTESIAN_POINT('Ctrl Pts',(3.87219658268766,0.688899575425928,
5.88075817667417));
#255681=CARTESIAN_POINT('Ctrl Pts',(3.85186253112331,0.803194093507157,
5.8866222199894));
#255682=CARTESIAN_POINT('Ctrl Pts',(3.82647807142746,0.916507494885766,
5.89248626330463));
#255683=CARTESIAN_POINT('Ctrl Pts',(3.79617502691577,1.02836966360401,5.89835030661986));
#255684=CARTESIAN_POINT('Ctrl Pts',(3.76585150683773,1.14030741684832,5.90421831223029));
#255685=CARTESIAN_POINT('Ctrl Pts',(3.73060290922078,1.25079159258783,5.91008631784073));
#255686=CARTESIAN_POINT('Ctrl Pts',(3.69061004696455,1.35936988389633,5.91595432345117));
#255687=CARTESIAN_POINT('Ctrl Pts',(3.65055944779205,1.46810492756914,5.92183080058701));
#255688=CARTESIAN_POINT('Ctrl Pts',(3.60575107436815,1.57492821668222,5.92770727772284));
#255689=CARTESIAN_POINT('Ctrl Pts',(3.55641270968123,1.67940990780029,5.93358375485868));
#255690=CARTESIAN_POINT('Ctrl Pts',(3.54560646568609,1.70229381679102,5.9348708393854));
#255691=CARTESIAN_POINT('Ctrl Pts',(3.53458308155962,1.72506550124405,5.93615792391211));
#255692=CARTESIAN_POINT('Ctrl Pts',(3.52334523002941,1.74772062699648,5.93744500843882));
#255693=CARTESIAN_POINT('Ctrl Pts',(3.47204093120941,1.85114834521145,5.94332095091657));
#255694=CARTESIAN_POINT('Ctrl Pts',(3.41609396010992,1.95248572342226,5.94919689339432));
#255695=CARTESIAN_POINT('Ctrl Pts',(3.35569799034643,2.05128740004538,5.95507283587207));
#255696=CARTESIAN_POINT('Ctrl Pts',(3.29537952499783,2.14996228731208,5.96094123792146));
#255697=CARTESIAN_POINT('Ctrl Pts',(3.23062362848781,2.24610759526916,5.96680963997084));
#255698=CARTESIAN_POINT('Ctrl Pts',(3.16167092446085,2.33930031535476,5.97267804202023));
#255699=CARTESIAN_POINT('Ctrl Pts',(3.09278833006882,2.43239827907546,5.9785404772039));
#255700=CARTESIAN_POINT('Ctrl Pts',(3.0197176603111,2.52254929668518,5.98440291238758));
#255701=CARTESIAN_POINT('Ctrl Pts',(2.9427437500641,2.60935781782773,5.99026534757125));
#255702=CARTESIAN_POINT('Ctrl Pts',(2.86336482983094,2.69887862628374,5.99631095150801));
#255703=CARTESIAN_POINT('Ctrl Pts',(2.77983498318723,2.7848442544325,6.00235655544476));
#255704=CARTESIAN_POINT('Ctrl Pts',(2.6925129494124,2.86685594637166,6.00840215938152));
#255705=CARTESIAN_POINT('Ctrl Pts',(2.6079327078613,2.94629258354521,6.01425793963753));
#255706=CARTESIAN_POINT('Ctrl Pts',(2.51979518059038,3.0220195650233,6.02011371989354));
#255707=CARTESIAN_POINT('Ctrl Pts',(2.42846444742363,3.09371127088477,6.02596950014955));
#255708=CARTESIAN_POINT('Ctrl Pts',(2.33714711557994,3.16539245713605,6.03182442116354));
#255709=CARTESIAN_POINT('Ctrl Pts',(2.24263783413364,3.23303929037039,6.03767934217754));
#255710=CARTESIAN_POINT('Ctrl Pts',(2.14533343263872,3.29636670636059,6.04353426319153));
#255711=CARTESIAN_POINT('Ctrl Pts',(2.04801983085547,3.35970011006026,6.04938973779777));
#255712=CARTESIAN_POINT('Ctrl Pts',(1.94791092961559,3.41871305948063,6.055245212404));
#255713=CARTESIAN_POINT('Ctrl Pts',(1.84543157254559,3.47316445205981,6.06110068701024));
#255714=CARTESIAN_POINT('Ctrl Pts',(1.74291779919691,3.52763413138819,6.06695812809686));
#255715=CARTESIAN_POINT('Ctrl Pts',(1.63803235131246,3.57753901407749,6.07281556918348));
#255716=CARTESIAN_POINT('Ctrl Pts',(1.531222991558,3.6226847986161,6.07867301027011));
#255717=CARTESIAN_POINT('Ctrl Pts',(1.4242932413981,3.66788146932533,6.08453705358437));
#255718=CARTESIAN_POINT('Ctrl Pts',(1.31543563157924,3.70830817468893,6.09040109689863));
#255719=CARTESIAN_POINT('Ctrl Pts',(1.20511622930149,3.74381942324602,6.0962651402129));
#255720=CARTESIAN_POINT('Ctrl Pts',(1.09472228493422,3.77935466651859,6.10213314582239));
#255721=CARTESIAN_POINT('Ctrl Pts',(0.982864978407684,3.80996773064951,
6.10800115143189));
#255722=CARTESIAN_POINT('Ctrl Pts',(0.870022123119032,3.8355639096857,6.11386915704138));
#255723=CARTESIAN_POINT('Ctrl Pts',(0.757016358798775,3.86119704142686,
6.11974563417625));
#255724=CARTESIAN_POINT('Ctrl Pts',(0.643022610824618,3.88179876088044,
6.12562211131112));
#255725=CARTESIAN_POINT('Ctrl Pts',(0.528525435344543,3.89732598895626,
6.13149858844598));
#255726=CARTESIAN_POINT('Ctrl Pts',(0.503447903249601,3.90072681136767,
6.1327856729818));
#255727=CARTESIAN_POINT('Ctrl Pts',(0.478346225338373,3.90388440309693,
6.13407275751761));
#255728=CARTESIAN_POINT('Ctrl Pts',(0.453225492216509,3.90679864508079,
6.13535984205342));
#255729=CARTESIAN_POINT('Ctrl Pts',(0.338541507815882,3.92010306898418,
6.14123578453135));
#255730=CARTESIAN_POINT('Ctrl Pts',(0.223082003137737,3.92837534667247,
6.14711172700929));
#255731=CARTESIAN_POINT('Ctrl Pts',(0.107325971306983,3.93153534079029,
6.15298766948722));
#255732=CARTESIAN_POINT('Ctrl Pts',(-0.0082815141296696,3.93469127977833,
6.15885607153678));
#255733=CARTESIAN_POINT('Ctrl Pts',(-0.124184361059787,3.93274797094074,
6.16472447358634));
#255734=CARTESIAN_POINT('Ctrl Pts',(-0.239896751886397,3.92567682679488,
6.17059287563589));
#255735=CARTESIAN_POINT('Ctrl Pts',(-0.355491488828726,3.91861287243717,
6.17645531081975));
#255736=CARTESIAN_POINT('Ctrl Pts',(-0.47089574527979,3.9064314788922,6.18231774600361));
#255737=CARTESIAN_POINT('Ctrl Pts',(-0.585622652389425,3.88915609213726,
6.18818018118747));
#255738=CARTESIAN_POINT('Ctrl Pts',(-0.70393414232727,3.87134094486518,
6.19422578512416));
#255739=CARTESIAN_POINT('Ctrl Pts',(-0.821524813649213,3.84810824116936,
6.20027138906086));
#255740=CARTESIAN_POINT('Ctrl Pts',(-0.937864857330161,3.81954166221355,
6.20631699299755));
#255741=CARTESIAN_POINT('Ctrl Pts',(-1.05055198303728,3.79187203469783,
6.21217277325372));
#255742=CARTESIAN_POINT('Ctrl Pts',(-1.16206541246184,3.75919858223408,
6.2180285535099));
#255743=CARTESIAN_POINT('Ctrl Pts',(-1.27193376449624,3.72164929819219,
6.22388433376607));
#255744=CARTESIAN_POINT('Ctrl Pts',(-1.38178599510872,3.68410552390666,
6.22973925478023));
#255745=CARTESIAN_POINT('Ctrl Pts',(-1.48999323784757,3.64168747414375,
6.23559417579439));
#255746=CARTESIAN_POINT('Ctrl Pts',(-1.59610028723417,3.59457269687107,
6.24144909680856));
#255747=CARTESIAN_POINT('Ctrl Pts',(-1.70221736921331,3.54745346482027,
6.24730457141493));
#255748=CARTESIAN_POINT('Ctrl Pts',(-1.80623348582855,3.49563678997855,
6.25316004602132));
#255749=CARTESIAN_POINT('Ctrl Pts',(-1.90771504296155,3.43934765832973,
6.25901552062769));
#255750=CARTESIAN_POINT('Ctrl Pts',(-2.00923068127598,3.38303962275233,
6.26487296171447));
#255751=CARTESIAN_POINT('Ctrl Pts',(-2.10820970676538,3.32225634373593,
6.27073040280124));
#255752=CARTESIAN_POINT('Ctrl Pts',(-2.20424529295946,3.25726751871351,
6.27658784388801));
#255753=CARTESIAN_POINT('Ctrl Pts',(-2.30038912587654,3.19220544139348,
6.28245188720244));
#255754=CARTESIAN_POINT('Ctrl Pts',(-2.39358255570672,3.12292858841028,
6.28831593051687));
#255755=CARTESIAN_POINT('Ctrl Pts',(-2.48344972178239,3.04974859281531,
6.2941799738313));
#255756=CARTESIAN_POINT('Ctrl Pts',(-2.5733776105068,2.97651914998214,6.30004797944094));
#255757=CARTESIAN_POINT('Ctrl Pts',(-2.65997445261805,2.89938158678553,
6.30591598505058));
#255758=CARTESIAN_POINT('Ctrl Pts',(-2.7429005819761,2.81868504757009,6.31178399066022));
#255759=CARTESIAN_POINT('Ctrl Pts',(-2.82594643017179,2.73787200833286,
6.31766046779526));
#255760=CARTESIAN_POINT('Ctrl Pts',(-2.905310708314,2.65349003882839,6.3235369449303));
#255761=CARTESIAN_POINT('Ctrl Pts',(-2.98069337551666,2.56592205671784,
6.32941342206534));
#255762=CARTESIAN_POINT('Ctrl Pts',(-2.99720392475848,2.54674264141861,
6.33070050659958));
#255763=CARTESIAN_POINT('Ctrl Pts',(-3.01352363574769,2.52741050105189,
6.33198759113383));
#255764=CARTESIAN_POINT('Ctrl Pts',(-3.02964963604818,2.50792984008587,
6.33327467566807));
#255765=CARTESIAN_POINT('Ctrl Pts',(-3.10287633135138,2.41946993693054,
6.3391192090466));
#255766=CARTESIAN_POINT('Ctrl Pts',(-3.17235473525013,2.32764397398516,
6.34496374242514));
#255767=CARTESIAN_POINT('Ctrl Pts',(-3.23775741246485,2.23280450062896,
6.35080827580367));
#255768=CARTESIAN_POINT('Ctrl Pts',(-3.30308038054781,2.13808061232829,
6.35664568619121));
#255769=CARTESIAN_POINT('Ctrl Pts',(-3.36433725947034,2.04035085249035,
6.36248309657875));
#255770=CARTESIAN_POINT('Ctrl Pts',(-3.42123975304002,1.94000194644714,
6.36832050696628));
#255771=CARTESIAN_POINT('Ctrl Pts',(-3.47808699042986,1.83975048599639,
6.37415224883249));
#255772=CARTESIAN_POINT('Ctrl Pts',(-3.53058804355407,1.73688529573961,
6.37998399069871));
#255773=CARTESIAN_POINT('Ctrl Pts',(-3.57849741899204,1.63182266875641,
6.38581573256492));
#255774=CARTESIAN_POINT('Ctrl Pts',(-3.6263721341728,1.52683604981215,6.39164325543075));
#255775=CARTESIAN_POINT('Ctrl Pts',(-3.66966160474642,1.41965553356179,
6.39747077829659));
#255776=CARTESIAN_POINT('Ctrl Pts',(-3.7081662451842,1.31072197588828,6.40329830116242));
#255777=CARTESIAN_POINT('Ctrl Pts',(-3.74665800471865,1.20182485960497,
6.40912387455521));
#255778=CARTESIAN_POINT('Ctrl Pts',(-3.78036797210157,1.09117625864008,
6.414949447948));
#255779=CARTESIAN_POINT('Ctrl Pts',(-3.80914491256672,0.979236455135857,
6.42077502134078));
#255780=CARTESIAN_POINT('Ctrl Pts',(-3.83791529183902,0.867322174103,6.42659926649263));
#255781=CARTESIAN_POINT('Ctrl Pts',(-3.86175478097165,0.754117681054901,
6.43242351164447));
#255782=CARTESIAN_POINT('Ctrl Pts',(-3.88056245260592,0.640096907839084,
6.43824775679632));
#255783=CARTESIAN_POINT('Ctrl Pts',(-3.89937772268794,0.526030069331107,
6.44407435498916));
#255784=CARTESIAN_POINT('Ctrl Pts',(-3.91315704387449,0.411146703655898,
6.44990095318201));
#255785=CARTESIAN_POINT('Ctrl Pts',(-3.92185095594521,0.295929179621853,
6.45572755137486));
#255786=CARTESIAN_POINT('Ctrl Pts',(-3.92936567121646,0.196339158428675,
6.46076386023824));
#255787=CARTESIAN_POINT('Ctrl Pts',(-3.93308175351824,0.0964997606865402,
6.46580016910163));
#255788=CARTESIAN_POINT('Ctrl Pts',(-3.93299863531415,-0.00327637254193622,
6.47083647796501));
#255789=CARTESIAN_POINT('',(-3.93299999135599,0.000260756115896825,7.72083647799638));
#255790=CARTESIAN_POINT('Ctrl Pts',(-3.93299863531357,-0.00327637323301801,
6.47083647799989));
#255791=CARTESIAN_POINT('Ctrl Pts',(-3.93288302433106,-0.142057215378997,
6.47784159197612));
#255792=CARTESIAN_POINT('Ctrl Pts',(-3.92541801980143,-0.280523368869989,
6.48484670595235));
#255793=CARTESIAN_POINT('Ctrl Pts',(-3.91072617825782,-0.417982964591799,
6.49185181992859));
#255794=CARTESIAN_POINT('Ctrl Pts',(-3.89585191697551,-0.557149313239084,
6.49894391218167));
#255795=CARTESIAN_POINT('Ctrl Pts',(-3.87357031095842,-0.695283924055693,
6.50603600443474));
#255796=CARTESIAN_POINT('Ctrl Pts',(-3.84405778351081,-0.831690301151798,
6.51312809668782));
#255797=CARTESIAN_POINT('Ctrl Pts',(-3.81900462496335,-0.947485554484084,
6.51914856755278));
#255798=CARTESIAN_POINT('Ctrl Pts',(-3.78874151244498,-1.06203576112651,
6.52516903841774));
#255799=CARTESIAN_POINT('Ctrl Pts',(-3.7534032234113,-1.17492690942272,
6.53118950928269));
#255800=CARTESIAN_POINT('Ctrl Pts',(-3.71891327099915,-1.28510797474763,
6.53706545176065));
#255801=CARTESIAN_POINT('Ctrl Pts',(-3.67951076709477,-1.39395084536786,
6.54294139423859));
#255802=CARTESIAN_POINT('Ctrl Pts',(-3.63531731797249,-1.50098534224998,
6.54881733671654));
#255803=CARTESIAN_POINT('Ctrl Pts',(-3.59118058103526,-1.60788248483379,
6.55468573876613));
#255804=CARTESIAN_POINT('Ctrl Pts',(-3.54226528181998,-1.71297549068377,
6.56055414081572));
#255805=CARTESIAN_POINT('Ctrl Pts',(-3.48874289578739,-1.81580891260424,
6.56642254286531));
#255806=CARTESIAN_POINT('Ctrl Pts',(-3.43527493017229,-1.91853777570049,
6.5722849780492));
#255807=CARTESIAN_POINT('Ctrl Pts',(-3.37720938506593,-2.01901126089608,
6.57814741323308));
#255808=CARTESIAN_POINT('Ctrl Pts',(-3.31476569881553,-2.1167941236587,
6.58400984841696));
#255809=CARTESIAN_POINT('Ctrl Pts',(-3.25037099191042,-2.21763216135384,
6.59005545235365));
#255810=CARTESIAN_POINT('Ctrl Pts',(-3.18132023154694,-2.31560826556371,
6.59610105629033));
#255811=CARTESIAN_POINT('Ctrl Pts',(-3.10790534872448,-2.41027246247593,
6.60214666022701));
#255812=CARTESIAN_POINT('Ctrl Pts',(-3.03679559263627,-2.50196433330534,
6.60800244048321));
#255813=CARTESIAN_POINT('Ctrl Pts',(-2.96159194301872,-2.59054881570634,
6.61385822073942));
#255814=CARTESIAN_POINT('Ctrl Pts',(-2.88260304862656,-2.67564733551507,
6.61971400099562));
#255815=CARTESIAN_POINT('Ctrl Pts',(-2.80362574459031,-2.76073336847813,
6.6255689220098));
#255816=CARTESIAN_POINT('Ctrl Pts',(-2.72086458095177,-2.84233415352404,
6.63142384302398));
#255817=CARTESIAN_POINT('Ctrl Pts',(-2.63466689826601,-2.92010604861902,
6.63727876403816));
#255818=CARTESIAN_POINT('Ctrl Pts',(-2.54846106544974,-2.99788529717264,
6.64313423864461));
#255819=CARTESIAN_POINT('Ctrl Pts',(-2.45881837413144,-3.07183465958274,
6.64898971325106));
#255820=CARTESIAN_POINT('Ctrl Pts',(-2.36612071223765,-3.14164953091843,
6.65484518785751));
#255821=CARTESIAN_POINT('Ctrl Pts',(-2.27339191911294,-3.21148784861552,
6.66070262894432));
#255822=CARTESIAN_POINT('Ctrl Pts',(-2.17760644481216,-3.27718866602247,
6.66656007003113));
#255823=CARTESIAN_POINT('Ctrl Pts',(-2.0791761366056,-3.33849001690432,
6.67241751111794));
#255824=CARTESIAN_POINT('Ctrl Pts',(-1.98063488245983,-3.39986046373916,
6.67828155443241));
#255825=CARTESIAN_POINT('Ctrl Pts',(-1.87944319493971,-3.45682132837217,
6.68414559774688));
#255826=CARTESIAN_POINT('Ctrl Pts',(-1.77603863731821,-3.50915598951555,
6.69000964106134));
#255827=CARTESIAN_POINT('Ctrl Pts',(-1.67256420992241,-3.56152601284264,
6.69587764667101));
#255828=CARTESIAN_POINT('Ctrl Pts',(-1.56687431026887,-3.60926343873527,
6.70174565228068));
#255829=CARTESIAN_POINT('Ctrl Pts',(-1.45942604915193,-3.65219996810919,
6.70761365789035));
#255830=CARTESIAN_POINT('Ctrl Pts',(-1.35182266707329,-3.69519848411425,
6.71349013502542));
#255831=CARTESIAN_POINT('Ctrl Pts',(-1.24245624567729,-3.73338213629185,
6.7193666121605));
#255832=CARTESIAN_POINT('Ctrl Pts',(-1.13179863309566,-3.76663256160231,
6.72524308929557));
#255833=CARTESIAN_POINT('Ctrl Pts',(-1.10756205419988,-3.77391517449766,
6.72653017382948));
#255834=CARTESIAN_POINT('Ctrl Pts',(-1.08326357056531,-3.78096133023377,
6.72781725836339));
#255835=CARTESIAN_POINT('Ctrl Pts',(-1.05890819147291,-3.78777011472866,
6.72910434289731));
#255836=CARTESIAN_POINT('Ctrl Pts',(-0.947718286842929,-3.81885434034308,
6.73498028537528));
#255837=CARTESIAN_POINT('Ctrl Pts',(-0.834975074744924,-3.84508973484664,
6.74085622785326));
#255838=CARTESIAN_POINT('Ctrl Pts',(-0.721139110600009,-3.86632220374389,
6.74673217033124));
#255839=CARTESIAN_POINT('Ctrl Pts',(-0.60744922888121,-3.8875274256231,
6.75260057238086));
#255840=CARTESIAN_POINT('Ctrl Pts',(-0.492669786014068,-3.90374241471174,
6.75846897443047));
#255841=CARTESIAN_POINT('Ctrl Pts',(-0.377276143425831,-3.91486292373076,
6.76433737648009));
#255842=CARTESIAN_POINT('Ctrl Pts',(-0.261999830625348,-3.92597212565404,
6.77019981166401));
#255843=CARTESIAN_POINT('Ctrl Pts',(-0.14611096878662,-3.9319971117745,
6.77606224684794));
#255844=CARTESIAN_POINT('Ctrl Pts',(-0.0300940988899279,-3.93288486294883,
6.78192468203187));
#255845=CARTESIAN_POINT('Ctrl Pts',(0.0895476580527755,-3.93380035144907,
6.78797028596853));
#255846=CARTESIAN_POINT('Ctrl Pts',(0.209325114417832,-3.92925222550942,
6.7940158899052));
#255847=CARTESIAN_POINT('Ctrl Pts',(0.328701893396891,-3.91924024082185,
6.80006149384187));
#255848=CARTESIAN_POINT('Ctrl Pts',(0.444330405076032,-3.90954261873588,
6.80591727409811));
#255849=CARTESIAN_POINT('Ctrl Pts',(0.559582582987395,-3.89471916013571,
6.81177305435435));
#255850=CARTESIAN_POINT('Ctrl Pts',(0.673972825476779,-3.87482252890618,
6.81762883461058));
#255851=CARTESIAN_POINT('Ctrl Pts',(0.788346283029122,-3.85492881718879,
6.8234837556248));
#255852=CARTESIAN_POINT('Ctrl Pts',(0.901857650103256,-3.82996348378381,
6.82933867663902));
#255853=CARTESIAN_POINT('Ctrl Pts',(1.01402954805526,-3.80003066772767,
6.83519359765323));
#255854=CARTESIAN_POINT('Ctrl Pts',(1.12621205204158,-3.77009502147538,
6.8410490722597));
#255855=CARTESIAN_POINT('Ctrl Pts',(1.23705443631635,-3.73519106530982,
6.84690454686617));
#255856=CARTESIAN_POINT('Ctrl Pts',(1.34609324519494,-3.69547317338938,
6.85276002147263));
#255857=CARTESIAN_POINT('Ctrl Pts',(1.4551686732536,-3.65574194276273,6.85861746255948));
#255858=CARTESIAN_POINT('Ctrl Pts',(1.56243893386359,-3.6111937027998,6.86447490364634));
#255859=CARTESIAN_POINT('Ctrl Pts',(1.6674600136861,-3.56203117655615,6.87033234473319));
#255860=CARTESIAN_POINT('Ctrl Pts',(1.77259946825045,-3.51281323666256,
6.87619638804769));
#255861=CARTESIAN_POINT('Ctrl Pts',(1.87548430809016,-3.45897080493629,
6.88206043136219));
#255862=CARTESIAN_POINT('Ctrl Pts',(1.97569454297385,-3.4007528685371,6.88792447467668));
#255863=CARTESIAN_POINT('Ctrl Pts',(2.07597248924917,-3.3424955946641,6.89379248028639));
#255864=CARTESIAN_POINT('Ctrl Pts',(2.17357188544326,-3.27985715133792,
6.89966048589609));
#255865=CARTESIAN_POINT('Ctrl Pts',(2.26810262099788,-3.2131292380828,6.9055284915058));
#255866=CARTESIAN_POINT('Ctrl Pts',(2.36276982873405,-3.1463049910391,6.9114049686409));
#255867=CARTESIAN_POINT('Ctrl Pts',(2.45435920970812,-3.07537974366202,
6.917281445776));
#255868=CARTESIAN_POINT('Ctrl Pts',(2.54251450635903,-3.00068475267794,
6.9231579229111));
#255869=CARTESIAN_POINT('Ctrl Pts',(2.56182255712942,-2.984324820456,6.92444500744472));
#255870=CARTESIAN_POINT('Ctrl Pts',(2.58096601564204,-2.96778418523611,
6.92573209197833));
#255871=CARTESIAN_POINT('Ctrl Pts',(2.59994138699915,-2.95106655027787,
6.92701917651194));
#255872=CARTESIAN_POINT('Ctrl Pts',(2.68656987773229,-2.87474533063978,
6.93289511898994));
#255873=CARTESIAN_POINT('Ctrl Pts',(2.76997782474021,-2.79448050537409,
6.93877106146793));
#255874=CARTESIAN_POINT('Ctrl Pts',(2.84978515425914,-2.71057439937815,
6.94464700394593));
#255875=CARTESIAN_POINT('Ctrl Pts',(2.92949006932228,-2.62677596768023,
6.95051540599556));
#255876=CARTESIAN_POINT('Ctrl Pts',(3.00560327401114,-2.53934584444975,
6.95638380804519));
#255877=CARTESIAN_POINT('Ctrl Pts',(3.0777784356618,-2.44862592099634,6.96225221009482));
#255878=CARTESIAN_POINT('Ctrl Pts',(3.14988021115175,-2.35799823962083,
6.96811464527875));
#255879=CARTESIAN_POINT('Ctrl Pts',(3.21805165285137,-2.26408773279291,
6.97397708046269));
#255880=CARTESIAN_POINT('Ctrl Pts',(3.28198439175556,-2.16727189163541,
6.97983951564663));
#255881=CARTESIAN_POINT('Ctrl Pts',(3.34791467599305,-2.06743108963609,
6.98588511958329));
#255882=CARTESIAN_POINT('Ctrl Pts',(3.40933672327431,-1.96450074129025,
6.99193072351996));
#255883=CARTESIAN_POINT('Ctrl Pts',(3.46595819281448,-1.8589305542871,6.99797632745662));
#255884=CARTESIAN_POINT('Ctrl Pts',(3.52080182578924,-1.75667512651214,
7.00383210771287));
#255885=CARTESIAN_POINT('Ctrl Pts',(3.57114162729818,-1.65194354664113,
7.00968788796912));
#255886=CARTESIAN_POINT('Ctrl Pts',(3.61675728335841,-1.54517175526667,
7.01554366822537));
#255887=CARTESIAN_POINT('Ctrl Pts',(3.66236624605132,-1.43841563094344,
7.0213985892396));
#255888=CARTESIAN_POINT('Ctrl Pts',(3.70325227956609,-1.32962026987251,
7.02725351025383));
#255889=CARTESIAN_POINT('Ctrl Pts',(3.73924271899208,-1.21924275206569,
7.03310843126807));
#255890=CARTESIAN_POINT('Ctrl Pts',(3.77523656137231,-1.10885479788609,
7.03896390587455));
#255891=CARTESIAN_POINT('Ctrl Pts',(3.80633376152611,-0.996884782031934,
7.04481938048103));
#255892=CARTESIAN_POINT('Ctrl Pts',(3.8324113681037,-0.883805468205252,
7.05067485508751));
#255893=CARTESIAN_POINT('Ctrl Pts',(3.85849773248577,-0.770688178250771,
7.05653229617437));
#255894=CARTESIAN_POINT('Ctrl Pts',(3.87956105847857,-0.656461251507195,
7.06238973726123));
#255895=CARTESIAN_POINT('Ctrl Pts',(3.89552953249747,-0.541607479121249,
7.0682471783481));
#255896=CARTESIAN_POINT('Ctrl Pts',(3.9115160054171,-0.426624249052216,
7.07411122166261));
#255897=CARTESIAN_POINT('Ctrl Pts',(3.92239610774169,-0.31101317217588,
7.07997526497712));
#255898=CARTESIAN_POINT('Ctrl Pts',(3.92814991010467,-0.195262089880939,
7.08583930829163));
#255899=CARTESIAN_POINT('Ctrl Pts',(3.93390760027378,-0.0794327953467238,
7.09170731390136));
#255900=CARTESIAN_POINT('Ctrl Pts',(3.93453209092554,0.0365362812697187,
7.09757531951108));
#255901=CARTESIAN_POINT('Ctrl Pts',(3.93005554794925,0.152159094481161,
7.1034433251208));
#255902=CARTESIAN_POINT('Ctrl Pts',(3.92557254227506,0.267948830095802,
7.10931980225592));
#255903=CARTESIAN_POINT('Ctrl Pts',(3.91597384052081,0.383390894991611,
7.11519627939103));
#255904=CARTESIAN_POINT('Ctrl Pts',(3.90134322176381,0.49800609032178,7.12107275652615));
#255905=CARTESIAN_POINT('Ctrl Pts',(3.89813877755612,0.523109471449321,
7.12235984105962));
#255906=CARTESIAN_POINT('Ctrl Pts',(3.89469313932908,0.548173234023334,
7.12364692559309));
#255907=CARTESIAN_POINT('Ctrl Pts',(3.89100750939418,0.573192430025141,
7.12493401012656));
#255908=CARTESIAN_POINT('Ctrl Pts',(3.87418145878955,0.687412866001887,
7.13080995260454));
#255909=CARTESIAN_POINT('Ctrl Pts',(3.85229398329045,0.801080214942577,
7.13668589508252));
#255910=CARTESIAN_POINT('Ctrl Pts',(3.82539162642816,0.913711061798685,
7.1425618375605));
#255911=CARTESIAN_POINT('Ctrl Pts',(3.79852379258844,1.0261973727211,7.14843023961011));
#255912=CARTESIAN_POINT('Ctrl Pts',(3.76665397074647,1.13764942892371,7.15429864165973));
#255913=CARTESIAN_POINT('Ctrl Pts',(3.72988026440124,1.24759056313766,7.16016704370934));
#255914=CARTESIAN_POINT('Ctrl Pts',(3.69314394877411,1.35741991155773,7.16602947889326));
#255915=CARTESIAN_POINT('Ctrl Pts',(3.65151379696037,1.46574100468358,7.17189191407718));
#255916=CARTESIAN_POINT('Ctrl Pts',(3.60513844557973,1.57208962473612,7.1777543492611));
#255917=CARTESIAN_POINT('Ctrl Pts',(3.55731412035048,1.68176105237297,7.18379995319777));
#255918=CARTESIAN_POINT('Ctrl Pts',(3.50444330237383,1.78933428840002,7.18984555713445));
#255919=CARTESIAN_POINT('Ctrl Pts',(3.44674392353413,1.89431922483529,7.19589116107112));
#255920=CARTESIAN_POINT('Ctrl Pts',(3.39085622613519,1.99600777810795,7.20174694132735));
#255921=CARTESIAN_POINT('Ctrl Pts',(3.33043886805119,2.09526775131126,7.20760272158358));
#255922=CARTESIAN_POINT('Ctrl Pts',(3.26573746434136,2.19167694106529,7.21345850183982));
#255923=CARTESIAN_POINT('Ctrl Pts',(3.20104555452681,2.28807198431398,7.21931342285403));
#255924=CARTESIAN_POINT('Ctrl Pts',(3.13207107901831,2.38161673326005,7.22516834386825));
#255925=CARTESIAN_POINT('Ctrl Pts',(3.05910333369062,2.47191743264271,7.23102326488247));
#255926=CARTESIAN_POINT('Ctrl Pts',(2.98612868914464,2.56222667010249,7.23687873948893));
#255927=CARTESIAN_POINT('Ctrl Pts',(2.90916028363934,2.64929092718708,7.2427342140954));
#255928=CARTESIAN_POINT('Ctrl Pts',(2.82852764275017,2.73274959961541,7.24858968870186));
#255929=CARTESIAN_POINT('Ctrl Pts',(2.74786792250078,2.81623630048767,7.25444712978871));
#255930=CARTESIAN_POINT('Ctrl Pts',(2.66354180650745,2.896114712193,7.26030457087555));
#255931=CARTESIAN_POINT('Ctrl Pts',(2.57591508203623,2.97206165651695,7.26616201196239));
#255932=CARTESIAN_POINT('Ctrl Pts',(2.48818958890905,3.04809420460689,7.27202605527689));
#255933=CARTESIAN_POINT('Ctrl Pts',(2.39715637408173,3.12018617032596,7.27789009859139));
#255934=CARTESIAN_POINT('Ctrl Pts',(2.30321371885568,3.18805513836806,7.28375414190588));
#255935=CARTESIAN_POINT('Ctrl Pts',(2.20920758720002,3.25596996502212,7.28962214751559));
#255936=CARTESIAN_POINT('Ctrl Pts',(2.11228844462947,3.31965588594009,7.2954901531253));
#255937=CARTESIAN_POINT('Ctrl Pts',(2.01288143979719,3.37887515444415,7.301358158735));
#255938=CARTESIAN_POINT('Ctrl Pts',(1.91333092300844,3.43817991665259,7.3072346358701));
#255939=CARTESIAN_POINT('Ctrl Pts',(1.81128573836657,3.49300496306484,7.3131111130052));
#255940=CARTESIAN_POINT('Ctrl Pts',(1.70719340343905,3.54315956220634,7.3189875901403));
#255941=CARTESIAN_POINT('Ctrl Pts',(1.6843947723417,3.55414458050243,7.32027467467393));
#255942=CARTESIAN_POINT('Ctrl Pts',(1.66149800241855,3.56490573956675,7.32156175920757));
#255943=CARTESIAN_POINT('Ctrl Pts',(1.63850789823744,3.57544135281415,7.3228488437412));
#255944=CARTESIAN_POINT('Ctrl Pts',(1.53355089953154,3.62353971449461,7.32872478621919));
#255945=CARTESIAN_POINT('Ctrl Pts',(1.42630106718662,3.66709199642041,7.33460072869717));
#255946=CARTESIAN_POINT('Ctrl Pts',(1.3171891745337,3.70587394260669,7.34047667117515));
#255947=CARTESIAN_POINT('Ctrl Pts',(1.20821730204159,3.7446061210343,7.34634507322477));
#255948=CARTESIAN_POINT('Ctrl Pts',(1.09738850678137,3.77858000095999,7.35221347527439));
#255949=CARTESIAN_POINT('Ctrl Pts',(0.985155984923154,3.80761824312392,
7.358081877324));
#255950=CARTESIAN_POINT('Ctrl Pts',(0.87303757869263,3.83662695982432,7.36394431250793));
#255951=CARTESIAN_POINT('Ctrl Pts',(0.759518682182498,3.86070991834644,
7.36980674769186));
#255952=CARTESIAN_POINT('Ctrl Pts',(0.645069573305308,3.87973894039221,
7.37566918287579));
#255953=CARTESIAN_POINT('Ctrl Pts',(0.527044561263792,3.89936251438178,
7.38171478681246));
#255954=CARTESIAN_POINT('Ctrl Pts',(0.408030674305431,3.91361099549031,
7.38776039074913));
#255955=CARTESIAN_POINT('Ctrl Pts',(0.288557645005564,3.92240021995574,
7.3938059946858));
#255956=CARTESIAN_POINT('Ctrl Pts',(0.172835905133741,3.93091347481522,
7.39966177494204));
#255957=CARTESIAN_POINT('Ctrl Pts',(0.0566838666735855,3.93430514103444,
7.40551755519828));
#255958=CARTESIAN_POINT('Ctrl Pts',(-0.0594106094984069,3.93255125579808,
7.41137333545451));
#255959=CARTESIAN_POINT('Ctrl Pts',(-0.175488050664438,3.9307976279163,
7.41722825646874));
#255960=CARTESIAN_POINT('Ctrl Pts',(-0.291507533732658,3.92389995615897,
7.42308317748296));
#255961=CARTESIAN_POINT('Ctrl Pts',(-0.406981265669249,3.91188640548192,
7.42893809849719));
#255962=CARTESIAN_POINT('Ctrl Pts',(-0.522465915833852,3.89987171890424,
7.43479357310366));
#255963=CARTESIAN_POINT('Ctrl Pts',(-0.637404301724936,3.88274023454091,
7.44064904771013));
#255964=CARTESIAN_POINT('Ctrl Pts',(-0.751314521917127,3.86057191218561,
7.4465045223166));
#255965=CARTESIAN_POINT('Ctrl Pts',(-0.86526299728565,3.838396144905,7.45236196340345));
#255966=CARTESIAN_POINT('Ctrl Pts',(-0.978182215408448,3.81118025480984,
7.45821940449031));
#255967=CARTESIAN_POINT('Ctrl Pts',(-1.08960191300048,3.77905499711048,
7.46407684557716));
#255968=CARTESIAN_POINT('Ctrl Pts',(-1.20114719755051,3.74689352935602,
7.46994088889166));
#255969=CARTESIAN_POINT('Ctrl Pts',(-1.31118919133558,3.70981176393342,
7.47580493220616));
#255970=CARTESIAN_POINT('Ctrl Pts',(-1.41927411974641,3.6679899090671,7.48166897552066));
#255971=CARTESIAN_POINT('Ctrl Pts',(-1.52743208042712,3.62613979545058,
7.48753698113037));
#255972=CARTESIAN_POINT('Ctrl Pts',(-1.633629965518,3.57954338011618,7.49340498674008));
#255973=CARTESIAN_POINT('Ctrl Pts',(-1.73743682923334,3.52842773263441,
7.49927299234979));
#255974=CARTESIAN_POINT('Ctrl Pts',(-1.84139355689568,3.4772382904881,7.50514946948489));
#255975=CARTESIAN_POINT('Ctrl Pts',(-1.94295201401711,3.42151679365053,
7.51102594661999));
#255976=CARTESIAN_POINT('Ctrl Pts',(-2.04170850168642,3.36153467840827,
7.51690242375509));
#255977=CARTESIAN_POINT('Ctrl Pts',(-2.06333845870785,3.34839720657869,
7.51818950828867));
#255978=CARTESIAN_POINT('Ctrl Pts',(-2.08483412369737,3.33505550489099,
7.51947659282224));
#255979=CARTESIAN_POINT('Ctrl Pts',(-2.10619146538181,3.32151268417762,
7.52076367735582));
#255980=CARTESIAN_POINT('Ctrl Pts',(-2.20369439385821,3.25968548213652,
7.52663961983381));
#255981=CARTESIAN_POINT('Ctrl Pts',(-2.29863346627671,3.19345935189115,
7.53251556231179));
#255982=CARTESIAN_POINT('Ctrl Pts',(-2.39058598756845,3.12307342789781,
7.53839150478978));
#255983=CARTESIAN_POINT('Ctrl Pts',(-2.48242050882824,3.05277782814097,
7.54425990683939));
#255984=CARTESIAN_POINT('Ctrl Pts',(-2.57127577603329,2.97833329935637,
7.55012830888901));
#255985=CARTESIAN_POINT('Ctrl Pts',(-2.65675622902896,2.9000233343054,7.55599671093863));
#255986=CARTESIAN_POINT('Ctrl Pts',(-2.74214976732823,2.82179299315204,
7.56185914612255));
#255987=CARTESIAN_POINT('Ctrl Pts',(-2.82417501443411,2.73970531080422,
7.56772158130647));
#255988=CARTESIAN_POINT('Ctrl Pts',(-2.90246833628129,2.65408488125089,
7.5735840164904));
#255989=CARTESIAN_POINT('Ctrl Pts',(-2.98320789244257,2.5657892856959,7.57962962042706));
#255990=CARTESIAN_POINT('Ctrl Pts',(-3.05997813090029,2.47373682787979,
7.58567522436373));
#255991=CARTESIAN_POINT('Ctrl Pts',(-3.13241994927456,2.37832593674348,
7.5917208283004));
#255992=CARTESIAN_POINT('Ctrl Pts',(-3.20258719380562,2.28591081686481,
7.59757660855664));
#255993=CARTESIAN_POINT('Ctrl Pts',(-3.26869349911763,2.19034536371258,
7.60343238881288));
#255994=CARTESIAN_POINT('Ctrl Pts',(-3.33045305657604,2.09202567812714,
7.60928816906912));
#255995=CARTESIAN_POINT('Ctrl Pts',(-3.392203551808,1.99372041938172,7.61514309008334));
#255996=CARTESIAN_POINT('Ctrl Pts',(-3.44960834796533,1.89266208125359,
7.62099801109756));
#255997=CARTESIAN_POINT('Ctrl Pts',(-3.50242539112959,1.78927509890758,
7.62685293211179));
#255998=CARTESIAN_POINT('Ctrl Pts',(-3.55524742823067,1.68587834115526,
7.63270840671826));
#255999=CARTESIAN_POINT('Ctrl Pts',(-3.60348066223641,1.58015286908215,
7.63856388132473));
#256000=CARTESIAN_POINT('Ctrl Pts',(-3.64692968661997,1.47254638665475,
7.6444193559312));
#256001=CARTESIAN_POINT('Ctrl Pts',(-3.69039330275907,1.36490376607447,
7.65027679701805));
#256002=CARTESIAN_POINT('Ctrl Pts',(-3.72906935990102,1.25537926151467,
7.6561342381049));
#256003=CARTESIAN_POINT('Ctrl Pts',(-3.7628113905605,1.14443848199376,7.66199167919175));
#256004=CARTESIAN_POINT('Ctrl Pts',(-3.79659145362431,1.03337265532832,
7.66785572250625));
#256005=CARTESIAN_POINT('Ctrl Pts',(-3.8254262700917,0.920887762643375,
7.67371976582075));
#256006=CARTESIAN_POINT('Ctrl Pts',(-3.84921982752044,0.807462518897018,
7.67958380913525));
#256007=CARTESIAN_POINT('Ctrl Pts',(-3.8730294620983,0.693960634464899,
7.68545181474497));
#256008=CARTESIAN_POINT('Ctrl Pts',(-3.89179098811298,0.579517540040464,
7.69131982035469));
#256009=CARTESIAN_POINT('Ctrl Pts',(-3.90546012776368,0.464618327714394,
7.69718782596441));
#256010=CARTESIAN_POINT('Ctrl Pts',(-3.919149001285,0.349553237633885,7.70306430309951));
#256011=CARTESIAN_POINT('Ctrl Pts',(-3.92773078638208,0.234031125519982,
7.70894078023462));
#256012=CARTESIAN_POINT('Ctrl Pts',(-3.93121325401241,0.11853839663663,
7.71481725736972));
#256013=CARTESIAN_POINT('Ctrl Pts',(-3.9319759950429,0.0932428153438174,
7.71610434190329));
#256014=CARTESIAN_POINT('Ctrl Pts',(-3.93249431380678,0.0679486270207419,
7.71739142643687));
#256015=CARTESIAN_POINT('Ctrl Pts',(-3.93276862363217,0.0426609068621461,
7.71867851097045));
#256016=CARTESIAN_POINT('Ctrl Pts',(-3.93292192916729,0.0285281740471575,
7.71939783330197));
#256017=CARTESIAN_POINT('Ctrl Pts',(-3.93299905428545,0.0143946133687574,
7.72011715563349));
#256018=CARTESIAN_POINT('Ctrl Pts',(-3.93299999135595,0.00026075673218739,
7.72083647796501));
#256019=CARTESIAN_POINT('',(-3.9329988040277,0.00306716754010798,8.97083647792409));
#256020=CARTESIAN_POINT('Ctrl Pts',(-3.93299999135599,0.000260756115881105,
7.72083647799638));
#256021=CARTESIAN_POINT('Ctrl Pts',(-3.93300763141371,-0.114974688434713,
7.72670122042153));
#256022=CARTESIAN_POINT('Ctrl Pts',(-3.927946446357,-0.230403984016668,
7.73256596284667));
#256023=CARTESIAN_POINT('Ctrl Pts',(-3.91779128489456,-0.345543699123907,
7.73843070527182));
#256024=CARTESIAN_POINT('Ctrl Pts',(-3.90764915179362,-0.460535698034116,
7.74428792364285));
#256025=CARTESIAN_POINT('Ctrl Pts',(-3.89242607403925,-0.57523844606433,
7.75014514201388));
#256026=CARTESIAN_POINT('Ctrl Pts',(-3.8721488925929,-0.689167580194828,
7.75600236038491));
#256027=CARTESIAN_POINT('Ctrl Pts',(-3.85189226461298,-0.802981232859575,
7.76185364173054));
#256028=CARTESIAN_POINT('Ctrl Pts',(-3.82659179463562,-0.916022425562077,
7.76770492307617));
#256029=CARTESIAN_POINT('Ctrl Pts',(-3.79632613907405,-1.02781167817023,
7.77355620442181));
#256030=CARTESIAN_POINT('Ctrl Pts',(-3.76549875443117,-1.14167573381843,
7.77951608526194));
#256031=CARTESIAN_POINT('Ctrl Pts',(-3.72952007097172,-1.25424047765321,
7.78547596610208));
#256032=CARTESIAN_POINT('Ctrl Pts',(-3.688527897781,-1.3650095044692,7.79143584694221));
#256033=CARTESIAN_POINT('Ctrl Pts',(-3.64832754556203,-1.47363887311081,
7.79728060437534));
#256034=CARTESIAN_POINT('Ctrl Pts',(-3.6033058045945,-1.58054087155183,
7.80312536180847));
#256035=CARTESIAN_POINT('Ctrl Pts',(-3.55364279889051,-1.6852631420326,
7.8089701192416));
#256036=CARTESIAN_POINT('Ctrl Pts',(-3.50398670115038,-1.78997084598345,
7.81481406368783));
#256037=CARTESIAN_POINT('Ctrl Pts',(-3.44969079993109,-1.89249905036668,
7.82065800813405));
#256038=CARTESIAN_POINT('Ctrl Pts',(-3.39098260860229,-1.99241711199157,
7.82650195258028));
#256039=CARTESIAN_POINT('Ctrl Pts',(-3.3322682701429,-2.09234563568928,
7.83234650892561));
#256040=CARTESIAN_POINT('Ctrl Pts',(-3.26914093330697,-2.18966311598395,
7.83819106527095));
#256041=CARTESIAN_POINT('Ctrl Pts',(-3.20187276557864,-2.28396580382583,
7.84403562161628));
#256042=CARTESIAN_POINT('Ctrl Pts',(-3.13228058454925,-2.38152650668836,
7.85008209853034));
#256043=CARTESIAN_POINT('Ctrl Pts',(-3.05825654802452,-2.47585994134154,
7.85612857544441));
#256044=CARTESIAN_POINT('Ctrl Pts',(-2.98014815975296,-2.56655526843298,
7.86217505235848));
#256045=CARTESIAN_POINT('Ctrl Pts',(-2.90453498716516,-2.65435328311519,
7.86802837122177));
#256046=CARTESIAN_POINT('Ctrl Pts',(-2.82509477184531,-2.73874182604679,
7.87388169008506));
#256047=CARTESIAN_POINT('Ctrl Pts',(-2.74218029393698,-2.81938579047702,
7.87973500894835));
#256048=CARTESIAN_POINT('Ctrl Pts',(-2.6551615806433,-2.90402160073174,
7.88587806488781));
#256049=CARTESIAN_POINT('Ctrl Pts',(-2.56431624269091,-2.98453227656997,
7.89202112082726));
#256050=CARTESIAN_POINT('Ctrl Pts',(-2.47009000278943,-3.06057909195624,
7.89816417676671));
#256051=CARTESIAN_POINT('Ctrl Pts',(-2.37586376288796,-3.13662590734251,
7.90430723270616));
#256052=CARTESIAN_POINT('Ctrl Pts',(-2.27825708356548,-3.20820861392727,
7.91045028864561));
#256053=CARTESIAN_POINT('Ctrl Pts',(-2.1777479311858,-3.27504243456722,
7.91659334458507));
#256054=CARTESIAN_POINT('Ctrl Pts',(-2.08160913581824,-3.33897017501681,
7.92246928706305));
#256055=CARTESIAN_POINT('Ctrl Pts',(-1.98249445764508,-3.39876656595813,
7.92834522954104));
#256056=CARTESIAN_POINT('Ctrl Pts',(-1.88079427711241,-3.45414271378315,
7.93422117201903));
#256057=CARTESIAN_POINT('Ctrl Pts',(-1.77922460550304,-3.50944779898672,
7.94008957406865));
#256058=CARTESIAN_POINT('Ctrl Pts',(-1.67507638916764,-3.56034372623259,
7.94595797611827));
#256059=CARTESIAN_POINT('Ctrl Pts',(-1.56876949590573,-3.60658443249506,
7.9518263781679));
#256060=CARTESIAN_POINT('Ctrl Pts',(-1.46257069321916,-3.65277812219641,
7.95768881335183));
#256061=CARTESIAN_POINT('Ctrl Pts',(-1.3542179558431,-3.69432584246097,
7.96355124853576));
#256062=CARTESIAN_POINT('Ctrl Pts',(-1.24415571475198,-3.73102741311961,
7.9694136837197));
#256063=CARTESIAN_POINT('Ctrl Pts',(-1.13065463590979,-3.76887570535554,
7.97545928765636));
#256064=CARTESIAN_POINT('Ctrl Pts',(-1.01533586459138,-3.80156982538415,
7.98150489159303));
#256065=CARTESIAN_POINT('Ctrl Pts',(-0.898709440783336,-3.82894376310842,
7.9875504955297));
#256066=CARTESIAN_POINT('Ctrl Pts',(-0.785744926891016,-3.85545819669366,
7.99340627578594));
#256067=CARTESIAN_POINT('Ctrl Pts',(-0.671554081155232,-3.87698144431913,
7.99926205604218));
#256068=CARTESIAN_POINT('Ctrl Pts',(-0.556615006701356,-3.89341350672066,
8.00511783629842));
#256069=CARTESIAN_POINT('Ctrl Pts',(-0.441692797716789,-3.90984315798006,
8.01097275731265));
#256070=CARTESIAN_POINT('Ctrl Pts',(-0.326022986827634,-3.92118305109915,
8.01682767832687));
#256071=CARTESIAN_POINT('Ctrl Pts',(-0.210091766155291,-3.92738468319488,
8.02268259934109));
#256072=CARTESIAN_POINT('Ctrl Pts',(-0.0941495839985609,-3.93358690166496,
8.02853807394757));
#256073=CARTESIAN_POINT('Ctrl Pts',(0.0220536448866986,-3.9346498712754,
8.03439354855404));
#256074=CARTESIAN_POINT('Ctrl Pts',(0.138029443514754,-3.93057716788807,
8.04024902316051));
#256075=CARTESIAN_POINT('Ctrl Pts',(0.254044191015066,-3.92650309673949,
8.04610646424737));
#256076=CARTESIAN_POINT('Ctrl Pts',(0.369830944103958,-3.91728993744105,
8.05196390533422));
#256077=CARTESIAN_POINT('Ctrl Pts',(0.484904773060254,-3.90299325659978,
8.05782134642107));
#256078=CARTESIAN_POINT('Ctrl Pts',(0.600108307736879,-3.88868046122315,
8.06368538973557));
#256079=CARTESIAN_POINT('Ctrl Pts',(0.714596904617967,-3.86927275895671,
8.06954943305008));
#256080=CARTESIAN_POINT('Ctrl Pts',(0.827894182077904,-3.84487714020638,
8.07541347636458));
#256081=CARTESIAN_POINT('Ctrl Pts',(0.941268013757286,-3.82046503749815,
8.08128148197429));
#256082=CARTESIAN_POINT('Ctrl Pts',(1.05344852485709,-3.79105841155848,
8.08714948758399));
#256083=CARTESIAN_POINT('Ctrl Pts',(1.16397454940685,-3.75681410883385,
8.09301749319369));
#256084=CARTESIAN_POINT('Ctrl Pts',(1.27466013822565,-3.72252036827633,
8.09889397032881));
#256085=CARTESIAN_POINT('Ctrl Pts',(1.3836860868475,-3.68337515209494,8.10477044746393));
#256086=CARTESIAN_POINT('Ctrl Pts',(1.49061119890961,-3.63958339012657,
8.11064692459905));
#256087=CARTESIAN_POINT('Ctrl Pts',(1.514030273777,-3.62999198047235,8.1119340091326));
#256088=CARTESIAN_POINT('Ctrl Pts',(1.53734866471534,-3.62017784468314,
8.11322109366616));
#256089=CARTESIAN_POINT('Ctrl Pts',(1.56056190337424,-3.61014342453828,
8.11450817819971));
#256090=CARTESIAN_POINT('Ctrl Pts',(1.66653758059776,-3.5643331657449,8.12038412067769));
#256091=CARTESIAN_POINT('Ctrl Pts',(1.77066924225063,-3.51377701042851,
8.12626006315568));
#256092=CARTESIAN_POINT('Ctrl Pts',(1.87250198377017,-3.45864501225216,
8.13213600563367));
#256093=CARTESIAN_POINT('Ctrl Pts',(1.97420404625462,-3.40358376338707,
8.13800440768328));
#256094=CARTESIAN_POINT('Ctrl Pts',(2.07361269589383,-3.34395854428528,
8.14387280973289));
#256095=CARTESIAN_POINT('Ctrl Pts',(2.17029288846745,-3.27998746617538,
8.1497412117825));
#256096=CARTESIAN_POINT('Ctrl Pts',(2.266874778689,-3.21608143248953,8.15560364696642));
#256097=CARTESIAN_POINT('Ctrl Pts',(2.36073338795434,-3.1478385557713,8.16146608215034));
#256098=CARTESIAN_POINT('Ctrl Pts',(2.45145877416057,-3.07552253748711,
8.16732851733426));
#256099=CARTESIAN_POINT('Ctrl Pts',(2.54501882809664,-3.00094704264456,
8.17337412127093));
#256100=CARTESIAN_POINT('Ctrl Pts',(2.63524625568776,-2.92203990853658,
8.1794197252076));
#256101=CARTESIAN_POINT('Ctrl Pts',(2.72172403835726,-2.83913847126699,
8.18546532914427));
#256102=CARTESIAN_POINT('Ctrl Pts',(2.80548653713557,-2.75884002554304,
8.19132110940051));
#256103=CARTESIAN_POINT('Ctrl Pts',(2.88573101786577,-2.67479466427583,
8.19717688965675));
#256104=CARTESIAN_POINT('Ctrl Pts',(2.96211321729066,-2.5873488918103,8.20303266991299));
#256105=CARTESIAN_POINT('Ctrl Pts',(3.0384842088505,-2.49991595061205,8.20888759092721));
#256106=CARTESIAN_POINT('Ctrl Pts',(3.11099377455895,-2.40908390115884,
8.21474251194144));
#256107=CARTESIAN_POINT('Ctrl Pts',(3.17933643375411,-2.31523407909518,
8.22059743295566));
#256108=CARTESIAN_POINT('Ctrl Pts',(3.24768555485803,-2.22137538337933,
8.22645290756213));
#256109=CARTESIAN_POINT('Ctrl Pts',(3.31186674324788,-2.12449868151264,
8.23230838216859));
#256110=CARTESIAN_POINT('Ctrl Pts',(3.37161695046699,-2.02501558989645,
8.23816385677505));
#256111=CARTESIAN_POINT('Ctrl Pts',(3.43138722396919,-1.9254990882559,8.2440212978619));
#256112=CARTESIAN_POINT('Ctrl Pts',(3.48672334486547,-1.82337480995101,
8.24987873894876));
#256113=CARTESIAN_POINT('Ctrl Pts',(3.5374077995522,-1.71907971300554,8.25573618003562));
#256114=CARTESIAN_POINT('Ctrl Pts',(3.58814938333396,-1.61466705961125,
8.26160022335013));
#256115=CARTESIAN_POINT('Ctrl Pts',(3.63422865567289,-1.50807907537374,
8.26746426666464));
#256116=CARTESIAN_POINT('Ctrl Pts',(3.67547588602648,-1.39977355712911,
8.27332830997915));
#256117=CARTESIAN_POINT('Ctrl Pts',(3.71675098686027,-1.29139485756354,
8.27919631558887));
#256118=CARTESIAN_POINT('Ctrl Pts',(3.7531874149327,-1.18129670394983,8.28506432119859));
#256119=CARTESIAN_POINT('Ctrl Pts',(3.78466553940226,-1.06995128620932,
8.2909323268083));
#256120=CARTESIAN_POINT('Ctrl Pts',(3.81618910822688,-0.958445121258386,
8.2968088039434));
#256121=CARTESIAN_POINT('Ctrl Pts',(3.84273999392077,-0.845688498873854,
8.3026852810785));
#256122=CARTESIAN_POINT('Ctrl Pts',(3.86424976790761,-0.732163049618011,
8.3085617582136));
#256123=CARTESIAN_POINT('Ctrl Pts',(3.86896090636399,-0.707298348106351,
8.30984884274717));
#256124=CARTESIAN_POINT('Ctrl Pts',(3.87343041490796,-0.682396779669048,
8.31113592728075));
#256125=CARTESIAN_POINT('Ctrl Pts',(3.87765790770314,-0.657463421664869,
8.31242301181432));
#256126=CARTESIAN_POINT('Ctrl Pts',(3.89695773132982,-0.543634862938722,
8.31829895429231));
#256127=CARTESIAN_POINT('Ctrl Pts',(3.91127299793002,-0.428767979368567,
8.32417489677029));
#256128=CARTESIAN_POINT('Ctrl Pts',(3.92049856335526,-0.313336902916516,
8.33005083924827));
#256129=CARTESIAN_POINT('Ctrl Pts',(3.92971228987715,-0.198053955852254,
8.3359192412979));
#256130=CARTESIAN_POINT('Ctrl Pts',(3.93384927191079,-0.0822086635191154,
8.34178764334753));
#256131=CARTESIAN_POINT('Ctrl Pts',(3.93285548640346,0.0337153239081983,
8.34765604539716));
#256132=CARTESIAN_POINT('Ctrl Pts',(3.93186271135597,0.149521442304274,
8.35351848058109));
#256133=CARTESIAN_POINT('Ctrl Pts',(3.92574954930698,0.265405686297156,
8.35938091576501));
#256134=CARTESIAN_POINT('Ctrl Pts',(3.91451388395261,0.380880627417861,
8.36524335094894));
#256135=CARTESIAN_POINT('Ctrl Pts',(3.90292716605019,0.499963523300396,
8.37128895488561));
#256136=CARTESIAN_POINT('Ctrl Pts',(3.88589254737316,0.618610673579545,
8.37733455882228));
#256137=CARTESIAN_POINT('Ctrl Pts',(3.86346581227279,0.7362886101247,8.38338016275894));
#256138=CARTESIAN_POINT('Ctrl Pts',(3.84174324592732,0.850271620694905,
8.38923594301519));
#256139=CARTESIAN_POINT('Ctrl Pts',(3.81496219345816,0.963344936144892,
8.39509172327143));
#256140=CARTESIAN_POINT('Ctrl Pts',(3.78322575425377,1.07503111227119,8.40094750352767));
#256141=CARTESIAN_POINT('Ctrl Pts',(3.75149397186385,1.1867009002388,8.40680242454189));
#256142=CARTESIAN_POINT('Ctrl Pts',(3.71480836139263,1.29698355667858,8.41265734555611));
#256143=CARTESIAN_POINT('Ctrl Pts',(3.67332235685453,1.40541519225911,8.41851226657032));
#256144=CARTESIAN_POINT('Ctrl Pts',(3.6318324297476,1.51385708022616,8.42436774117679));
#256145=CARTESIAN_POINT('Ctrl Pts',(3.58554135379455,1.62044721389172,8.43022321578326));
#256146=CARTESIAN_POINT('Ctrl Pts',(3.53465106900056,1.72474079803698,8.43607869038973));
#256147=CARTESIAN_POINT('Ctrl Pts',(3.48374369340638,1.82906940774389,8.44193613147658));
#256148=CARTESIAN_POINT('Ctrl Pts',(3.42823421850167,1.93109956353574,8.44779357256343));
#256149=CARTESIAN_POINT('Ctrl Pts',(3.36837063784763,2.03041085647363,8.45365101365027));
#256150=CARTESIAN_POINT('Ctrl Pts',(3.30843958182644,2.12983408835467,8.45951505696478));
#256151=CARTESIAN_POINT('Ctrl Pts',(3.24414483793516,2.22653198714789,8.46537910027928));
#256152=CARTESIAN_POINT('Ctrl Pts',(3.17577790141848,2.32011286812992,8.47124314359379));
#256153=CARTESIAN_POINT('Ctrl Pts',(3.1073647698161,2.41375698109275,8.47711114920348));
#256154=CARTESIAN_POINT('Ctrl Pts',(3.03487422388538,2.50427956098514,8.48297915481317));
#256155=CARTESIAN_POINT('Ctrl Pts',(2.95863711649576,2.59132310082971,8.48884716042286));
#256156=CARTESIAN_POINT('Ctrl Pts',(2.88228994707891,2.67849230373757,8.49472363755797));
#256157=CARTESIAN_POINT('Ctrl Pts',(2.8021857063234,2.76217214620715,8.50060011469308));
#256158=CARTESIAN_POINT('Ctrl Pts',(2.71869105178692,2.84204292102243,8.50647659182819));
#256159=CARTESIAN_POINT('Ctrl Pts',(2.70040378953428,2.85953646972297,8.50776367636178));
#256160=CARTESIAN_POINT('Ctrl Pts',(2.68195400531168,2.8768474511919,8.50905076089537));
#256161=CARTESIAN_POINT('Ctrl Pts',(2.66334574718046,2.89397277647454,8.51033784542896));
#256162=CARTESIAN_POINT('Ctrl Pts',(2.57839324286485,2.97215522964777,8.51621378790694));
#256163=CARTESIAN_POINT('Ctrl Pts',(2.48985510842656,3.04672282682729,8.52208973038492));
#256164=CARTESIAN_POINT('Ctrl Pts',(2.39807171558815,3.1173291527999,8.5279656728629));
#256165=CARTESIAN_POINT('Ctrl Pts',(2.30640610574387,3.18784487170056,8.53383407491252));
#256166=CARTESIAN_POINT('Ctrl Pts',(2.21150384384635,3.25440917942465,8.53970247696214));
#256167=CARTESIAN_POINT('Ctrl Pts',(2.1137411271544,3.31671335019716,8.54557087901176));
#256168=CARTESIAN_POINT('Ctrl Pts',(2.01607781350173,3.37895417142145,8.55143331419569));
#256169=CARTESIAN_POINT('Ctrl Pts',(1.91556017639965,3.43694325132007,8.55729574937962));
#256170=CARTESIAN_POINT('Ctrl Pts',(1.81259585267499,3.49041333868432,8.56315818456356));
#256171=CARTESIAN_POINT('Ctrl Pts',(1.70641446195327,3.5455540712504,8.56920378850023));
#256172=CARTESIAN_POINT('Ctrl Pts',(1.59763133453854,3.59588850968678,8.5752493924369));
#256173=CARTESIAN_POINT('Ctrl Pts',(1.48672425454009,3.64117288671689,8.58129499637356));
#256174=CARTESIAN_POINT('Ctrl Pts',(1.37929950489814,3.68503539635306,8.58715077662979));
#256175=CARTESIAN_POINT('Ctrl Pts',(1.2698825971241,3.72416006544192,8.59300655688602));
#256176=CARTESIAN_POINT('Ctrl Pts',(1.15893009997142,3.75837332144908,8.59886233714225));
#256177=CARTESIAN_POINT('Ctrl Pts',(1.04799388332157,3.79258155720862,8.60471725815646));
#256178=CARTESIAN_POINT('Ctrl Pts',(0.935522919670791,3.82187969132178,
8.61057217917068));
#256179=CARTESIAN_POINT('Ctrl Pts',(0.821989824359372,3.84614374778812,
8.61642710018489));
#256180=CARTESIAN_POINT('Ctrl Pts',(0.70844599431038,3.8704100984602,8.62228257479135));
#256181=CARTESIAN_POINT('Ctrl Pts',(0.593840236625425,3.8896413390112,8.6281380493978));
#256182=CARTESIAN_POINT('Ctrl Pts',(0.478655571701212,3.90376457329068,
8.63399352400426));
#256183=CARTESIAN_POINT('Ctrl Pts',(0.363432223596314,3.91789255066356,
8.63985096509108));
#256184=CARTESIAN_POINT('Ctrl Pts',(0.24762999111753,3.92690906040524,8.64570840617791));
#256185=CARTESIAN_POINT('Ctrl Pts',(0.131736525648879,3.93079311180453,
8.65156584726473));
#256186=CARTESIAN_POINT('Ctrl Pts',(0.0157124306043185,3.93468154112095,
8.65742989057923));
#256187=CARTESIAN_POINT('Ctrl Pts',(-0.100402689938917,3.93342595190847,
8.66329393389373));
#256188=CARTESIAN_POINT('Ctrl Pts',(-0.216121581555738,3.92705748137022,
8.66915797720823));
#256189=CARTESIAN_POINT('Ctrl Pts',(-0.331918663660945,3.92068470769863,
8.67502598281794));
#256190=CARTESIAN_POINT('Ctrl Pts',(-0.447318574030938,3.90919221421752,
8.68089398842765));
#256191=CARTESIAN_POINT('Ctrl Pts',(-0.561841285935853,3.8926627608127,
8.68676199403737));
#256192=CARTESIAN_POINT('Ctrl Pts',(-0.676529332048938,3.87610944415801,
8.69263847117247));
#256193=CARTESIAN_POINT('Ctrl Pts',(-0.790337248512992,3.85450473233834,
8.69851494830757));
#256194=CARTESIAN_POINT('Ctrl Pts',(-0.902797209048255,3.82798200091572,
8.70439142544266));
#256195=CARTESIAN_POINT('Ctrl Pts',(-0.927428543865126,3.8221729087302,
8.7056785099763));
#256196=CARTESIAN_POINT('Ctrl Pts',(-0.951995282899111,3.81612808031578,
8.70696559450994));
#256197=CARTESIAN_POINT('Ctrl Pts',(-0.976492630786821,3.80984922825288,
8.70825267904357));
#256198=CARTESIAN_POINT('Ctrl Pts',(-1.08833066728694,3.78118430952744,
8.71412862152157));
#256199=CARTESIAN_POINT('Ctrl Pts',(-1.19908995043581,3.74754342673066,
8.72000456399956));
#256200=CARTESIAN_POINT('Ctrl Pts',(-1.30829457137154,3.70902336397599,
8.72588050647755));
#256201=CARTESIAN_POINT('Ctrl Pts',(-1.41735905315022,3.67055273291274,
8.73174890852714));
#256202=CARTESIAN_POINT('Ctrl Pts',(-1.52487245456459,3.62721550997189,
8.73761731057673));
#256203=CARTESIAN_POINT('Ctrl Pts',(-1.63037096332379,3.57915905234046,
8.74348571262632));
#256204=CARTESIAN_POINT('Ctrl Pts',(-1.73576220345629,3.53115145748704,
8.74934814781025));
#256205=CARTESIAN_POINT('Ctrl Pts',(-1.83914225263862,3.47843434274131,
8.75521058299418));
#256206=CARTESIAN_POINT('Ctrl Pts',(-1.94006495841097,3.4212040215611,8.76107301817811));
#256207=CARTESIAN_POINT('Ctrl Pts',(-2.04414094188438,3.36218556861985,
8.76711862211478));
#256208=CARTESIAN_POINT('Ctrl Pts',(-2.14560307951632,3.29836739620784,
8.77316422605145));
#256209=CARTESIAN_POINT('Ctrl Pts',(-2.24398670852152,3.23001743833973,
8.77920982998812));
#256210=CARTESIAN_POINT('Ctrl Pts',(-2.33928122637291,3.16381357550133,
8.78506561024436));
#256211=CARTESIAN_POINT('Ctrl Pts',(-2.43168730305447,3.09335850875303,
8.7909213905006));
#256212=CARTESIAN_POINT('Ctrl Pts',(-2.52081070056782,3.0189406108605,8.79677717075683));
#256213=CARTESIAN_POINT('Ctrl Pts',(-2.60992102064913,2.94453363260333,
8.80263209177105));
#256214=CARTESIAN_POINT('Ctrl Pts',(-2.69574930261961,2.86616524394409,
8.80848701278526));
#256215=CARTESIAN_POINT('Ctrl Pts',(-2.77793416366369,2.78416428795969,
8.81434193379948));
#256216=CARTESIAN_POINT('Ctrl Pts',(-2.86012679541967,2.70215557865192,
8.82019740840597));
#256217=CARTESIAN_POINT('Ctrl Pts',(-2.93867502922724,2.61651391079365,
8.82605288301246));
#256218=CARTESIAN_POINT('Ctrl Pts',(-3.01325465410107,2.52760467429901,
8.83190835761895));
#256219=CARTESIAN_POINT('Ctrl Pts',(-3.0878593255131,2.4386655788638,8.83776579870582));
#256220=CARTESIAN_POINT('Ctrl Pts',(-3.15849247261472,2.34645704875029,
8.84362323979268));
#256221=CARTESIAN_POINT('Ctrl Pts',(-3.22487089347209,2.25137662785162,
8.84948068087954));
#256222=CARTESIAN_POINT('Ctrl Pts',(-3.29132413291297,2.15618903684676,
8.85534472419405));
#256223=CARTESIAN_POINT('Ctrl Pts',(-3.35351283797005,2.05812343285433,
8.86120876750855));
#256224=CARTESIAN_POINT('Ctrl Pts',(-3.41119774079782,1.95760541815144,
8.86707281082306));
#256225=CARTESIAN_POINT('Ctrl Pts',(-3.46892162093227,1.85701948409192,
8.87294081643279));
#256226=CARTESIAN_POINT('Ctrl Pts',(-3.5221354501389,1.75397820546516,8.87880882204251));
#256227=CARTESIAN_POINT('Ctrl Pts',(-3.57064719127853,1.64892923905629,
8.88467682765224));
#256228=CARTESIAN_POINT('Ctrl Pts',(-3.6192289678737,1.54372861550123,8.89055330478734));
#256229=CARTESIAN_POINT('Ctrl Pts',(-3.66309495360247,1.43651490033964,
8.89642978192244));
#256230=CARTESIAN_POINT('Ctrl Pts',(-3.70210220588523,1.32775308592361,
8.90230625905754));
#256231=CARTESIAN_POINT('Ctrl Pts',(-3.71064569715652,1.30393173072083,
8.9035933435911));
#256232=CARTESIAN_POINT('Ctrl Pts',(-3.71895630268983,1.28003615680195,
8.90488042812465));
#256233=CARTESIAN_POINT('Ctrl Pts',(-3.72703284698822,1.25607131862442,
8.90616751265821));
#256234=CARTESIAN_POINT('Ctrl Pts',(-3.77057278820299,1.12687898005475,
8.9131060723762));
#256235=CARTESIAN_POINT('Ctrl Pts',(-3.8074234076311,0.995326044578603,
8.9200446320942));
#256236=CARTESIAN_POINT('Ctrl Pts',(-3.83736273983174,0.862053480331147,
8.9269831918122));
#256237=CARTESIAN_POINT('Ctrl Pts',(-3.86714814939447,0.729466090506162,
8.93388607934459));
#256238=CARTESIAN_POINT('Ctrl Pts',(-3.89009306797262,0.595176783475139,
8.94078896687699));
#256239=CARTESIAN_POINT('Ctrl Pts',(-3.90602587688562,0.459837850877824,
8.94769185440938));
#256240=CARTESIAN_POINT('Ctrl Pts',(-3.92181433051305,0.325725123299988,
8.95453220003178));
#256241=CARTESIAN_POINT('Ctrl Pts',(-3.93071707851339,0.190581796902268,
8.96137254565419));
#256242=CARTESIAN_POINT('Ctrl Pts',(-3.93261454488523,0.0550621590310676,
8.96821289127659));
#256243=CARTESIAN_POINT('Ctrl Pts',(-3.93285713337963,0.0377361576845521,
8.96908742015909));
#256244=CARTESIAN_POINT('Ctrl Pts',(-3.93298528379372,0.0204040307365112,
8.96996194904159));
#256245=CARTESIAN_POINT('Ctrl Pts',(-3.9329988040277,0.00306716754012942,
8.97083647792409));
#256246=CARTESIAN_POINT('',(-3.93299908398399,-0.00268428409338097,10.2208364780097));
#256247=CARTESIAN_POINT('Ctrl Pts',(-3.93299880402833,0.00306716672873387,
8.97083647796502));
#256248=CARTESIAN_POINT('Ctrl Pts',(-3.93308917252479,-0.112811499136198,
8.97668178221734));
#256249=CARTESIAN_POINT('Ctrl Pts',(-3.9280540123563,-0.228756031444991,
8.98252708646965));
#256250=CARTESIAN_POINT('Ctrl Pts',(-3.91790260917037,-0.344279167327913,
8.98837239072197));
#256251=CARTESIAN_POINT('Ctrl Pts',(-3.90775321798013,-0.459779406666684,
8.99421653644213));
#256252=CARTESIAN_POINT('Ctrl Pts',(-3.89248963587196,-0.574858003416339,
9.0000606821623));
#256253=CARTESIAN_POINT('Ctrl Pts',(-3.87217315440355,-0.689031249158154,
9.00590482788247));
#256254=CARTESIAN_POINT('Ctrl Pts',(-3.85185576317811,-0.803209607493564,
9.01174923529916));
#256255=CARTESIAN_POINT('Ctrl Pts',(-3.82648509527511,-0.916482126613162,
9.01759364271585));
#256256=CARTESIAN_POINT('Ctrl Pts',(-3.79617372817084,-1.02837445784379,
9.02343805013255));
#256257=CARTESIAN_POINT('Ctrl Pts',(-3.76585363871364,-1.1402989870416,
9.02928413932704));
#256258=CARTESIAN_POINT('Ctrl Pts',(-3.73059013125671,-1.25084213917707,
9.03513022852153));
#256259=CARTESIAN_POINT('Ctrl Pts',(-3.69054568544134,-1.35954460892989,
9.04097631771602));
#256260=CARTESIAN_POINT('Ctrl Pts',(-3.65045510954265,-1.46837230089229,
9.04682914144201));
#256261=CARTESIAN_POINT('Ctrl Pts',(-3.60557274235956,-1.57535468796528,
9.052681965168));
#256262=CARTESIAN_POINT('Ctrl Pts',(-3.55610934335194,-1.68005218315533,
9.05853478889398));
#256263=CARTESIAN_POINT('Ctrl Pts',(-3.50661459556593,-1.78481603323892,
9.06439132200666));
#256264=CARTESIAN_POINT('Ctrl Pts',(-3.45253322725666,-1.88729174216262,
9.07024785511933));
#256265=CARTESIAN_POINT('Ctrl Pts',(-3.39412122504588,-1.98706570341623,
9.07610438823201));
#256266=CARTESIAN_POINT('Ctrl Pts',(-3.33561524295534,-2.08700019237866,
9.08197034400196));
#256267=CARTESIAN_POINT('Ctrl Pts',(-3.27276493769432,-2.18422390633897,
9.08783629977193));
#256268=CARTESIAN_POINT('Ctrl Pts',(-3.20586891361158,-2.27835324494226,
9.09370225554188));
#256269=CARTESIAN_POINT('Ctrl Pts',(-3.16641033676859,-2.33387537486531,
9.09716228578553));
#256270=CARTESIAN_POINT('Ctrl Pts',(-3.12554492914801,-2.38832153375116,
9.10062231602918));
#256271=CARTESIAN_POINT('Ctrl Pts',(-3.0833401164466,-2.4416188740897,9.10408234627284));
#256272=CARTESIAN_POINT('Ctrl Pts',(-3.01166645053495,-2.5321302523164,
9.10995828875082));
#256273=CARTESIAN_POINT('Ctrl Pts',(-2.93588572830932,-2.61963230908041,
9.11583423122881));
#256274=CARTESIAN_POINT('Ctrl Pts',(-2.85627992874342,-2.70372964045178,
9.1217101737068));
#256275=CARTESIAN_POINT('Ctrl Pts',(-2.7767762850157,-2.78771905213108,
9.12757857575642));
#256276=CARTESIAN_POINT('Ctrl Pts',(-2.69345760701673,-2.86831213044786,
9.13344697780604));
#256277=CARTESIAN_POINT('Ctrl Pts',(-2.60664715498583,-2.94514509140115,
9.13931537985567));
#256278=CARTESIAN_POINT('Ctrl Pts',(-2.51992496996597,-3.02189993024294,
9.14517781503959));
#256279=CARTESIAN_POINT('Ctrl Pts',(-2.42971838034013,-3.0949019846257,
9.15104025022351));
#256280=CARTESIAN_POINT('Ctrl Pts',(-2.33638818789035,-3.16382351522433,
9.15690268540744));
#256281=CARTESIAN_POINT('Ctrl Pts',(-2.24014194188808,-3.23489846337059,
9.16294828934411));
#256282=CARTESIAN_POINT('Ctrl Pts',(-2.14057400087049,-3.30163338394711,
9.16899389328077));
#256283=CARTESIAN_POINT('Ctrl Pts',(-2.03811812430678,-3.36371275696546,
9.17503949721744));
#256284=CARTESIAN_POINT('Ctrl Pts',(-1.93887922189066,-3.42384292272702,
9.18089527747368));
#256285=CARTESIAN_POINT('Ctrl Pts',(-1.8369314058288,-3.47960529568957,
9.18675105772992));
#256286=CARTESIAN_POINT('Ctrl Pts',(-1.73269846431591,-3.53075700548158,
9.19260683798616));
#256287=CARTESIAN_POINT('Ctrl Pts',(-1.62848081731874,-3.58190120957897,
9.19846175900038));
#256288=CARTESIAN_POINT('Ctrl Pts',(-1.52197908206302,-3.62843591398964,
9.2043166800146));
#256289=CARTESIAN_POINT('Ctrl Pts',(-1.4136406556621,-3.67016472336859,
9.21017160102882));
#256290=CARTESIAN_POINT('Ctrl Pts',(-1.30529198568751,-3.71189747827405,
9.2160270756353));
#256291=CARTESIAN_POINT('Ctrl Pts',(-1.19510666453686,-3.74882328646736,
9.22188255024179));
#256292=CARTESIAN_POINT('Ctrl Pts',(-1.08355035827497,-3.7807945753614,
9.22773802484827));
#256293=CARTESIAN_POINT('Ctrl Pts',(-0.971956587366361,-3.81277660137182,
9.23359546593513));
#256294=CARTESIAN_POINT('Ctrl Pts',(-0.85899131235982,-3.83980068577578,
9.23945290702199));
#256295=CARTESIAN_POINT('Ctrl Pts',(-0.745132894489018,-3.86176979758639,
9.24531034810885));
#256296=CARTESIAN_POINT('Ctrl Pts',(-0.631146140851378,-3.88376367192983,
9.25117439142336));
#256297=CARTESIAN_POINT('Ctrl Pts',(-0.516264640558031,-3.9006911234041,
9.25703843473786));
#256298=CARTESIAN_POINT('Ctrl Pts',(-0.400974518798198,-3.91250666903899,
9.26290247805236));
#256299=CARTESIAN_POINT('Ctrl Pts',(-0.285606496267014,-3.92433019835977,
9.26877048366208));
#256300=CARTESIAN_POINT('Ctrl Pts',(-0.169829713505279,-3.93103492006655,
9.2746384892718));
#256301=CARTESIAN_POINT('Ctrl Pts',(-0.0541312339993148,-3.93262746894563,
9.28050649488151));
#256302=CARTESIAN_POINT('Ctrl Pts',(0.0617342771478512,-3.9342223169565,
9.28638297201663));
#256303=CARTESIAN_POINT('Ctrl Pts',(0.177520848519057,-3.93069027606435,
9.29225944915174));
#256304=CARTESIAN_POINT('Ctrl Pts',(0.292745547399449,-3.92208988225382,
9.29813592628685));
#256305=CARTESIAN_POINT('Ctrl Pts',(0.317982423915861,-3.92020619690947,
9.29942301082039));
#256306=CARTESIAN_POINT('Ctrl Pts',(0.343192383916798,-3.91807957188955,
9.30071009535392));
#256307=CARTESIAN_POINT('Ctrl Pts',(0.368370423145139,-3.91571094839135,
9.30199717988746));
#256308=CARTESIAN_POINT('Ctrl Pts',(0.483316028005758,-3.90489744308944,
9.30787312236544));
#256309=CARTESIAN_POINT('Ctrl Pts',(0.597974713552378,-3.88900047395475,
9.31374906484342));
#256310=CARTESIAN_POINT('Ctrl Pts',(0.71186128919564,-3.86804117156795,
9.31962500732141));
#256311=CARTESIAN_POINT('Ctrl Pts',(0.825601717464484,-3.84710876565245,
9.32549340937103));
#256312=CARTESIAN_POINT('Ctrl Pts',(0.938571604011507,-3.82112701995287,
9.33136181142064));
#256313=CARTESIAN_POINT('Ctrl Pts',(1.0502897930848,-3.79016890791715,9.33723021347026));
#256314=CARTESIAN_POINT('Ctrl Pts',(1.16189438949284,-3.75924227342763,
9.34309264865419));
#256315=CARTESIAN_POINT('Ctrl Pts',(1.27224942454752,-3.7233494469283,9.34895508383811));
#256316=CARTESIAN_POINT('Ctrl Pts',(1.38088352504515,-3.68261451828166,
9.35481751902204));
#256317=CARTESIAN_POINT('Ctrl Pts',(1.49291184178044,-3.64060684787513,
9.36086312295871));
#256318=CARTESIAN_POINT('Ctrl Pts',(1.60310947734438,-3.59344960432805,
9.36690872689538));
#256319=CARTESIAN_POINT('Ctrl Pts',(1.71097557030186,-3.5413347198239,9.37295433083205));
#256320=CARTESIAN_POINT('Ctrl Pts',(1.8154548157296,-3.49085617128971,9.37881011108829));
#256321=CARTESIAN_POINT('Ctrl Pts',(1.91774634485568,-3.43572684599689,
9.38466589134452));
#256322=CARTESIAN_POINT('Ctrl Pts',(2.0174156557983,-3.37616988194313,9.39052167160076));
#256323=CARTESIAN_POINT('Ctrl Pts',(2.11707034186477,-3.31662165692063,
9.39637659261497));
#256324=CARTESIAN_POINT('Ctrl Pts',(2.21410322061805,-3.2526472966825,9.40223151362919));
#256325=CARTESIAN_POINT('Ctrl Pts',(2.30810590865885,-3.18451505168591,
9.4080864346434));
#256326=CARTESIAN_POINT('Ctrl Pts',(2.40211748480592,-3.1163763646753,9.41394190924986));
#256327=CARTESIAN_POINT('Ctrl Pts',(2.49309796646332,-3.04407925363265,
9.41979738385633));
#256328=CARTESIAN_POINT('Ctrl Pts',(2.58066996607157,-2.96793388171235,
9.4256528584628));
#256329=CARTESIAN_POINT('Ctrl Pts',(2.66827137552787,-2.89176293741929,
9.43151029954964));
#256330=CARTESIAN_POINT('Ctrl Pts',(2.75246171542831,-2.81174143304379,
9.43736774063648));
#256331=CARTESIAN_POINT('Ctrl Pts',(2.83289907132974,-2.72821770605996,
9.44322518172332));
#256332=CARTESIAN_POINT('Ctrl Pts',(2.91342709237467,-2.64459983512266,
9.44908922503783));
#256333=CARTESIAN_POINT('Ctrl Pts',(2.9901933999685,-2.5574721601767,9.45495326835233));
#256334=CARTESIAN_POINT('Ctrl Pts',(3.06289508260059,-2.46721760551864,
9.46081731166684));
#256335=CARTESIAN_POINT('Ctrl Pts',(3.1356458892776,-2.37690206645641,9.46668531727654));
#256336=CARTESIAN_POINT('Ctrl Pts',(3.20432635828969,-2.28345577227626,
9.47255332288623));
#256337=CARTESIAN_POINT('Ctrl Pts',(3.26867677645263,-2.18729081995953,
9.47842132849593));
#256338=CARTESIAN_POINT('Ctrl Pts',(3.33312009606093,-2.09098703617414,
9.48429780563103));
#256339=CARTESIAN_POINT('Ctrl Pts',(3.393220676276,-1.99195711301693,9.49017428276613));
#256340=CARTESIAN_POINT('Ctrl Pts',(3.44876458147198,-1.89063795095317,
9.49605075990123));
#256341=CARTESIAN_POINT('Ctrl Pts',(3.46092998255685,-1.86844670891249,
9.49733784443485));
#256342=CARTESIAN_POINT('Ctrl Pts',(3.47287697851214,-1.84614572451827,
9.49862492896847));
#256343=CARTESIAN_POINT('Ctrl Pts',(3.48460363313516,-1.82373970728863,
9.49991201350209));
#256344=CARTESIAN_POINT('Ctrl Pts',(3.53813947031149,-1.72144924775539,
9.50578795598008));
#256345=CARTESIAN_POINT('Ctrl Pts',(3.58725571182295,-1.61663072544782,
9.51166389845806));
#256346=CARTESIAN_POINT('Ctrl Pts',(3.63170582167591,-1.50970256170059,
9.51753984093605));
#256347=CARTESIAN_POINT('Ctrl Pts',(3.67609888997846,-1.40291161579743,
9.52340824298567));
#256348=CARTESIAN_POINT('Ctrl Pts',(3.71583757790152,-1.29401679012507,
9.52927664503529));
#256349=CARTESIAN_POINT('Ctrl Pts',(3.75072102583942,-1.18346135818881,
9.53514504708491));
#256350=CARTESIAN_POINT('Ctrl Pts',(3.78556900503359,-1.07301833665102,
9.54100748226885));
#256351=CARTESIAN_POINT('Ctrl Pts',(3.81557144053061,-0.96091845877266,
9.54686991745278));
#256352=CARTESIAN_POINT('Ctrl Pts',(3.84057567033391,-0.847624634162565,
9.55273235263672));
#256353=CARTESIAN_POINT('Ctrl Pts',(3.86636114435439,-0.730791002647243,
9.55877795657339));
#256354=CARTESIAN_POINT('Ctrl Pts',(3.88683077421347,-0.612688002023787,
9.56482356051005));
#256355=CARTESIAN_POINT('Ctrl Pts',(3.90187273426225,-0.49384022276529,
9.57086916444672));
#256356=CARTESIAN_POINT('Ctrl Pts',(3.91644239737474,-0.378724100940102,
9.57672494470296));
#256357=CARTESIAN_POINT('Ctrl Pts',(3.92592008163983,-0.262909710905088,
9.58258072495921));
#256358=CARTESIAN_POINT('Ctrl Pts',(3.9302562751658,-0.146882985807825,
9.58843650521545));
#256359=CARTESIAN_POINT('Ctrl Pts',(3.93459183242479,-0.0308732857752303,
9.59429142622967));
#256360=CARTESIAN_POINT('Ctrl Pts',(3.93378738369546,0.0853482750012756,
9.60014634724389));
#256361=CARTESIAN_POINT('Ctrl Pts',(3.92784547669866,0.201293097690658,
9.60600126825812));
#256362=CARTESIAN_POINT('Ctrl Pts',(3.92190300788495,0.317248883150332,
9.61185674286458));
#256363=CARTESIAN_POINT('Ctrl Pts',(3.91082213629431,0.432927466269691,
9.61771221747104));
#256364=CARTESIAN_POINT('Ctrl Pts',(3.89465744216663,0.547843415745872,
9.62356769207751));
#256365=CARTESIAN_POINT('Ctrl Pts',(3.87848731934938,0.662797958158712,
9.62942513316436));
#256366=CARTESIAN_POINT('Ctrl Pts',(3.85723003645407,0.776988949130067,
9.6352825742512));
#256367=CARTESIAN_POINT('Ctrl Pts',(3.83099150952541,0.889939915918046,
9.64114001533805));
#256368=CARTESIAN_POINT('Ctrl Pts',(3.80472340778318,1.00301819563767,9.64700405865256));
#256369=CARTESIAN_POINT('Ctrl Pts',(3.77346294928052,1.11485325926834,9.65286810196706));
#256370=CARTESIAN_POINT('Ctrl Pts',(3.73736629965948,1.22498250688309,9.65873214528157));
#256371=CARTESIAN_POINT('Ctrl Pts',(3.70124525977146,1.33518616810079,9.66460015089129));
#256372=CARTESIAN_POINT('Ctrl Pts',(3.66028166719039,1.44368133298243,9.67046815650101));
#256373=CARTESIAN_POINT('Ctrl Pts',(3.61467968151267,1.55002574174092,9.67633616211073));
#256374=CARTESIAN_POINT('Ctrl Pts',(3.56901186113656,1.65652367785073,9.68221263924583));
#256375=CARTESIAN_POINT('Ctrl Pts',(3.51869246263513,1.76086429102316,9.68808911638094));
#256376=CARTESIAN_POINT('Ctrl Pts',(3.46397138003121,1.86263020439503,9.69396559351605));
#256377=CARTESIAN_POINT('Ctrl Pts',(3.45198619614305,1.88491929531337,9.69525267804961));
#256378=CARTESIAN_POINT('Ctrl Pts',(3.43979002147693,1.90708498819124,9.69653976258316));
#256379=CARTESIAN_POINT('Ctrl Pts',(3.42738575119693,1.92912309417835,9.69782684711672));
#256380=CARTESIAN_POINT('Ctrl Pts',(3.37075638712148,2.02973392410271,9.70370278959469));
#256381=CARTESIAN_POINT('Ctrl Pts',(3.30959970541971,2.12801509260485,9.70957873207267));
#256382=CARTESIAN_POINT('Ctrl Pts',(3.24413234661948,2.22353194661493,9.71545467455064));
#256383=CARTESIAN_POINT('Ctrl Pts',(3.17874900020217,2.31892622658718,9.72132307660025));
#256384=CARTESIAN_POINT('Ctrl Pts',(3.109066209097,2.41156290938507,9.72719147864986));
#256385=CARTESIAN_POINT('Ctrl Pts',(3.035346333988,2.50103211349746,9.73305988069947));
#256386=CARTESIAN_POINT('Ctrl Pts',(2.96170141567097,2.59041034723707,9.73892231588341));
#256387=CARTESIAN_POINT('Ctrl Pts',(2.88402783933348,2.67662719185028,9.74478475106736));
#256388=CARTESIAN_POINT('Ctrl Pts',(2.80263068445487,2.75930249276009,9.7506471862513));
#256389=CARTESIAN_POINT('Ctrl Pts',(2.71869031760603,2.84456094065125,9.75669279018797));
#256390=CARTESIAN_POINT('Ctrl Pts',(2.63079011730429,2.92605253095204,9.76273839412464));
#256391=CARTESIAN_POINT('Ctrl Pts',(2.53930913402945,3.00339776284038,9.76878399806131));
#256392=CARTESIAN_POINT('Ctrl Pts',(2.45070052828989,3.07831446041935,9.77463977831754));
#256393=CARTESIAN_POINT('Ctrl Pts',(2.35873297926471,3.14934100027928,9.78049555857378));
#256394=CARTESIAN_POINT('Ctrl Pts',(2.26378705585266,3.2161711965867,9.78635133883001));
#256395=CARTESIAN_POINT('Ctrl Pts',(2.16885506423521,3.28299158663247,9.79220625984422));
#256396=CARTESIAN_POINT('Ctrl Pts',(2.07094590469007,3.34561661999916,9.79806118085843));
#256397=CARTESIAN_POINT('Ctrl Pts',(1.97047073583236,3.40378231960099,9.80391610187263));
#256398=CARTESIAN_POINT('Ctrl Pts',(1.86998606688478,3.46195351886387,9.8097715764791));
#256399=CARTESIAN_POINT('Ctrl Pts',(1.76693526355375,3.51566433938033,9.81562705108557));
#256400=CARTESIAN_POINT('Ctrl Pts',(1.66175516730063,3.56469616712977,9.82148252569204));
#256401=CARTESIAN_POINT('Ctrl Pts',(1.55653974776288,3.61374446154229,9.82733996677889));
#256402=CARTESIAN_POINT('Ctrl Pts',(1.44919398724795,3.65811046423124,9.83319740786574));
#256403=CARTESIAN_POINT('Ctrl Pts',(1.34017517386066,3.69762349399821,9.83905484895259));
#256404=CARTESIAN_POINT('Ctrl Pts',(1.23103347967719,3.73718106096391,9.8449188922671));
#256405=CARTESIAN_POINT('Ctrl Pts',(1.12021535705179,3.77187459668523,9.8507829355816));
#256406=CARTESIAN_POINT('Ctrl Pts',(1.00819382771782,3.80158311835368,9.85664697889611));
#256407=CARTESIAN_POINT('Ctrl Pts',(0.896096606178859,3.83131171387334,
9.86251498450582));
#256408=CARTESIAN_POINT('Ctrl Pts',(0.782794761012432,3.85604850027893,
9.86838299011553));
#256409=CARTESIAN_POINT('Ctrl Pts',(0.668770395129177,3.8757238238294,9.87425099572524));
#256410=CARTESIAN_POINT('Ctrl Pts',(0.554581414489975,3.89542755226122,
9.88012747286034));
#256411=CARTESIAN_POINT('Ctrl Pts',(0.439668239311621,3.91005518341447,
9.88600394999545));
#256412=CARTESIAN_POINT('Ctrl Pts',(0.324517013160983,3.91958897183991,
9.89188042713056));
#256413=CARTESIAN_POINT('Ctrl Pts',(0.299296228872053,3.9216770922132,9.89316751166415));
#256414=CARTESIAN_POINT('Ctrl Pts',(0.274064018824445,3.92352105354648,
9.89445459619775));
#256415=CARTESIAN_POINT('Ctrl Pts',(0.248825472904327,3.92512100247036,
9.89574168073135));
#256416=CARTESIAN_POINT('Ctrl Pts',(0.133603636122442,3.93242526850652,
9.90161762320934));
#256417=CARTESIAN_POINT('Ctrl Pts',(0.0178698172299948,3.93466378666596,
9.90749356568732));
#256418=CARTESIAN_POINT('Ctrl Pts',(-0.0978934626551561,3.93178151350878,
9.91336950816531));
#256419=CARTESIAN_POINT('Ctrl Pts',(-0.213508186844968,3.92890293909004,
9.91923791021493));
#256420=CARTESIAN_POINT('Ctrl Pts',(-0.329151887914362,3.92091665215585,
9.92510631226454));
#256421=CARTESIAN_POINT('Ctrl Pts',(-0.44433791846337,3.90781944493545,
9.93097471431415));
#256422=CARTESIAN_POINT('Ctrl Pts',(-0.559406830319615,3.8947355546753,
9.93683714949805));
#256423=CARTESIAN_POINT('Ctrl Pts',(-0.674018589574355,3.87655112736964,
9.94269958468195));
#256424=CARTESIAN_POINT('Ctrl Pts',(-0.787688213129598,3.85331497270814,
9.94856201986584));
#256425=CARTESIAN_POINT('Ctrl Pts',(-0.90490938523454,3.82935281642185,
9.95460762380252));
#256426=CARTESIAN_POINT('Ctrl Pts',(-1.02112813411794,3.80001807744511,
9.96065322773919));
#256427=CARTESIAN_POINT('Ctrl Pts',(-1.13581973689763,3.7654219584628,9.96669883167586));
#256428=CARTESIAN_POINT('Ctrl Pts',(-1.2469101804907,3.73191211021587,9.97255461193209));
#256429=CARTESIAN_POINT('Ctrl Pts',(-1.35656752040787,3.69346647014502,
9.97841039218833));
#256430=CARTESIAN_POINT('Ctrl Pts',(-1.46432769352019,3.650237445152,9.98426617244456));
#256431=CARTESIAN_POINT('Ctrl Pts',(-1.57207205455225,3.60701476332635,
9.99012109345879));
#256432=CARTESIAN_POINT('Ctrl Pts',(-1.67791941934211,3.55901024589167,
9.99597601447301));
#256433=CARTESIAN_POINT('Ctrl Pts',(-1.7814244631935,3.50642494314876,10.0018309354872));
#256434=CARTESIAN_POINT('Ctrl Pts',(-1.88493929361403,3.4538346683805,10.0076864100937));
#256435=CARTESIAN_POINT('Ctrl Pts',(-1.98611099482549,3.39666293426557,
10.0135418847002));
#256436=CARTESIAN_POINT('Ctrl Pts',(-2.0845182984925,3.33515703726975,10.0193973593066));
#256437=CARTESIAN_POINT('Ctrl Pts',(-2.18295865089524,3.2736304843667,10.0252548003935));
#256438=CARTESIAN_POINT('Ctrl Pts',(-2.27863240985213,3.20776709284905,
10.0311122414804));
#256439=CARTESIAN_POINT('Ctrl Pts',(-2.3711473704363,3.13785741353444,10.0369696825672));
#256440=CARTESIAN_POINT('Ctrl Pts',(-2.46376660946253,3.06786893537045,
10.0428337258817));
#256441=CARTESIAN_POINT('Ctrl Pts',(-2.55321961437504,2.99382531555611,
10.0486977691962));
#256442=CARTESIAN_POINT('Ctrl Pts',(-2.63914729130462,2.91605736822846,
10.0545618125107));
#256443=CARTESIAN_POINT('Ctrl Pts',(-2.72513302899599,2.83823687361423,
10.0604298181205));
#256444=CARTESIAN_POINT('Ctrl Pts',(-2.80758840271163,2.75668732999067,
10.0662978237302));
#256445=CARTESIAN_POINT('Ctrl Pts',(-2.88619242046907,2.67177512377574,
10.0721658293399));
#256446=CARTESIAN_POINT('Ctrl Pts',(-2.96490991731583,2.58674033146271,
10.078042306475));
#256447=CARTESIAN_POINT('Ctrl Pts',(-3.03976469645951,2.49833350218984,
10.0839187836101));
#256448=CARTESIAN_POINT('Ctrl Pts',(-3.11047709888341,2.40695268281739,
10.0897952607452));
#256449=CARTESIAN_POINT('Ctrl Pts',(-3.12596475201316,2.38693816790007,
10.0910823452788));
#256450=CARTESIAN_POINT('Ctrl Pts',(-3.14125386036989,2.36678109016191,
10.0923694298124));
#256451=CARTESIAN_POINT('Ctrl Pts',(-3.15634177473762,2.34648579817697,
10.093656514346));
#256452=CARTESIAN_POINT('Ctrl Pts',(-3.22550845453863,2.25344722916221,
10.0995568238018));
#256453=CARTESIAN_POINT('Ctrl Pts',(-3.290673072617,2.1571930683664,10.1054571332576));
#256454=CARTESIAN_POINT('Ctrl Pts',(-3.35152387932836,2.05810026147701,
10.1113574427134));
#256455=CARTESIAN_POINT('Ctrl Pts',(-3.41229617600891,1.95913530464819,
10.1172501395589));
#256456=CARTESIAN_POINT('Ctrl Pts',(-3.4687655170211,1.85733932833455,10.1231428364044));
#256457=CARTESIAN_POINT('Ctrl Pts',(-3.52066119802542,1.75312113920237,
10.12903553325));
#256458=CARTESIAN_POINT('Ctrl Pts',(-3.57250208611494,1.64901298655582,
10.134922008421));
#256459=CARTESIAN_POINT('Ctrl Pts',(-3.61977873792708,1.54248807032957,
10.140808483592));
#256460=CARTESIAN_POINT('Ctrl Pts',(-3.66226482118138,1.43398234979978,
10.1466949587629));
#256461=CARTESIAN_POINT('Ctrl Pts',(-3.7068583267162,1.32009445808609,10.1528734186965));
#256462=CARTESIAN_POINT('Ctrl Pts',(-3.74617356237532,1.20402459394112,
10.15905187863));
#256463=CARTESIAN_POINT('Ctrl Pts',(-3.78000422930493,1.08630429734804,
10.1652303385635));
#256464=CARTESIAN_POINT('Ctrl Pts',(-3.81219018328193,0.97430709504086,
10.1711084262607));
#256465=CARTESIAN_POINT('Ctrl Pts',(-3.83941215511248,0.860816597138284,
10.176986513958));
#256466=CARTESIAN_POINT('Ctrl Pts',(-3.86154281169423,0.746308323317278,
10.1828646016552));
#256467=CARTESIAN_POINT('Ctrl Pts',(-3.88366644224654,0.631836403523942,
10.1887408231802));
#256468=CARTESIAN_POINT('Ctrl Pts',(-3.90070189906821,0.516347751439844,
10.1946170447052));
#256469=CARTESIAN_POINT('Ctrl Pts',(-3.91257278780409,0.400328839998983,
10.2004932662302));
#256470=CARTESIAN_POINT('Ctrl Pts',(-3.92444388921092,0.28430785004045,
10.2063695930297));
#256471=CARTESIAN_POINT('Ctrl Pts',(-3.93115019501299,0.167756987342149,
10.2122459198291));
#256472=CARTESIAN_POINT('Ctrl Pts',(-3.93266713851748,0.051168130948575,
10.2181222466286));
#256473=CARTESIAN_POINT('Ctrl Pts',(-3.9329006934652,0.0332176244332676,
10.2190269904074));
#256474=CARTESIAN_POINT('Ctrl Pts',(-3.93301133525525,0.0152662207290025,
10.2199317341862));
#256475=CARTESIAN_POINT('Ctrl Pts',(-3.9329990839846,-0.00268428320635572,
10.220836477965));
#256476=CARTESIAN_POINT('',(-3.93299987808706,-0.000979268682662659,11.4708364779372));
#256477=CARTESIAN_POINT('Ctrl Pts',(-3.93299908398399,-0.0026842840933697,
10.2208364780097));
#256478=CARTESIAN_POINT('Ctrl Pts',(-3.93290870171559,-0.135111913380411,
10.227511113673));
#256479=CARTESIAN_POINT('Ctrl Pts',(-3.9261258777171,-0.267278679899612,
10.2341857493362));
#256480=CARTESIAN_POINT('Ctrl Pts',(-3.9127534874604,-0.39855883676877,
10.2408603849995));
#256481=CARTESIAN_POINT('Ctrl Pts',(-3.8993178403376,-0.530460002383905,
10.2475665944148));
#256482=CARTESIAN_POINT('Ctrl Pts',(-3.87923025223139,-0.661465984719606,
10.2542728038301));
#256483=CARTESIAN_POINT('Ctrl Pts',(-3.8526446301691,-0.790960399532857,
10.2609790132454));
#256484=CARTESIAN_POINT('Ctrl Pts',(-3.82590297900647,-0.921214807736393,
10.2677245809206));
#256485=CARTESIAN_POINT('Ctrl Pts',(-3.79258689461957,-1.04993969128303,
10.2744701485958));
#256486=CARTESIAN_POINT('Ctrl Pts',(-3.75290144432354,-1.17652868609069,
10.281215716271));
#256487=CARTESIAN_POINT('Ctrl Pts',(-3.73259339779128,-1.24130746969652,
10.2846675935009));
#256488=CARTESIAN_POINT('Ctrl Pts',(-3.71061822050571,-1.30552729526668,
10.2881194707308));
#256489=CARTESIAN_POINT('Ctrl Pts',(-3.68700813042917,-1.36910921629693,
10.2915713479607));
#256490=CARTESIAN_POINT('Ctrl Pts',(-3.64681796086312,-1.47734125519457,
10.2974472904387));
#256491=CARTESIAN_POINT('Ctrl Pts',(-3.60179172910044,-1.58398067685562,
10.3033232329166));
#256492=CARTESIAN_POINT('Ctrl Pts',(-3.55207540094065,-1.68856428543076,
10.3091991753946));
#256493=CARTESIAN_POINT('Ctrl Pts',(-3.50242287231812,-1.7930136848622,
10.3150675774443));
#256494=CARTESIAN_POINT('Ctrl Pts',(-3.44809239237427,-1.89541214835226,
10.3209359794939));
#256495=CARTESIAN_POINT('Ctrl Pts',(-3.38927895977792,-1.99531379306783,
10.3268043815435));
#256496=CARTESIAN_POINT('Ctrl Pts',(-3.33052532742177,-2.09511385992801,
10.3326668167274));
#256497=CARTESIAN_POINT('Ctrl Pts',(-3.2672980174054,-2.19242180422965,
10.3385292519114));
#256498=CARTESIAN_POINT('Ctrl Pts',(-3.19983887219756,-2.28681442009916,
10.3443916870953));
#256499=CARTESIAN_POINT('Ctrl Pts',(-3.1302720009169,-2.38415628439061,
10.350437291032));
#256500=CARTESIAN_POINT('Ctrl Pts',(-3.0562046962359,-2.47839724618601,
10.3564828949686));
#256501=CARTESIAN_POINT('Ctrl Pts',(-2.97795196288579,-2.56910317168164,
10.3625284989053));
#256502=CARTESIAN_POINT('Ctrl Pts',(-2.90215625814747,-2.65696105539444,
10.3683842791615));
#256503=CARTESIAN_POINT('Ctrl Pts',(-2.82243431786652,-2.7415022387079,
10.3742400594178));
#256504=CARTESIAN_POINT('Ctrl Pts',(-2.73911411748493,-2.82236476228619,
10.380095839674));
#256505=CARTESIAN_POINT('Ctrl Pts',(-2.65580614300898,-2.90321542058356,
10.3859507606882));
#256506=CARTESIAN_POINT('Ctrl Pts',(-2.56890125444077,-2.98038820510011,
10.3918056817024));
#256507=CARTESIAN_POINT('Ctrl Pts',(-2.47876424425139,-3.05355805928442,
10.3976606027167));
#256508=CARTESIAN_POINT('Ctrl Pts',(-2.38861871146198,-3.12673483179673,
10.4035160773231));
#256509=CARTESIAN_POINT('Ctrl Pts',(-2.29524077002123,-3.19590766143401,
10.4093715519296));
#256510=CARTESIAN_POINT('Ctrl Pts',(-2.19902767652229,-3.26079227763575,
10.415227026536));
#256511=CARTESIAN_POINT('Ctrl Pts',(-2.10278227118321,-3.32569868444073,
10.4210844676229));
#256512=CARTESIAN_POINT('Ctrl Pts',(-2.00370016247812,-3.38631378346408,
10.4269419087097));
#256513=CARTESIAN_POINT('Ctrl Pts',(-1.90220630147709,-3.44239744750964,
10.4327993497965));
#256514=CARTESIAN_POINT('Ctrl Pts',(-1.80059804144638,-3.49854432638103,
10.438663393111));
#256515=CARTESIAN_POINT('Ctrl Pts',(-1.69657296491896,-3.55014937629392,
10.4445274364255));
#256516=CARTESIAN_POINT('Ctrl Pts',(-1.59057933871619,-3.59701909464617,
10.45039147974));
#256517=CARTESIAN_POINT('Ctrl Pts',(-1.48451409332259,-3.64392048255652,
10.4562594853497));
#256518=CARTESIAN_POINT('Ctrl Pts',(-1.37647803315502,-3.68608001793417,
10.4621274909594));
#256519=CARTESIAN_POINT('Ctrl Pts',(-1.26693642540508,-3.72335347421942,
10.4679954965691));
#256520=CARTESIAN_POINT('Ctrl Pts',(-1.15723667456969,-3.76068074146748,
10.4738719737042));
#256521=CARTESIAN_POINT('Ctrl Pts',(-1.04602743321664,-3.79310773732621,
10.4797484508393));
#256522=CARTESIAN_POINT('Ctrl Pts',(-0.933786081092086,-3.82054087201782,
10.4856249279744));
#256523=CARTESIAN_POINT('Ctrl Pts',(-0.909202626579218,-3.82654936359487,
10.486912012508));
#256524=CARTESIAN_POINT('Ctrl Pts',(-0.884569685472442,-3.8323184908851,
10.4881990970416));
#256525=CARTESIAN_POINT('Ctrl Pts',(-0.859892307913054,-3.83784760234066,
10.4894861815751));
#256526=CARTESIAN_POINT('Ctrl Pts',(-0.747232379785504,-3.86308972126895,
10.4953621240531));
#256527=CARTESIAN_POINT('Ctrl Pts',(-0.633274179249711,-3.88340858761525,
10.5012380665311));
#256528=CARTESIAN_POINT('Ctrl Pts',(-0.518485672507367,-3.89867433974737,
10.5071140090091));
#256529=CARTESIAN_POINT('Ctrl Pts',(-0.403844470561764,-3.91392050177784,
10.5129824110587));
#256530=CARTESIAN_POINT('Ctrl Pts',(-0.288375486892729,-3.92412639157176,
10.5188508131083));
#256531=CARTESIAN_POINT('Ctrl Pts',(-0.17255887346522,-3.92921269915341,
10.5247192151579));
#256532=CARTESIAN_POINT('Ctrl Pts',(-0.0568600198931209,-3.93429383508629,
10.5305816503419));
#256533=CARTESIAN_POINT('Ctrl Pts',(0.0591853503974699,-3.93426572520224,
10.5364440855258));
#256534=CARTESIAN_POINT('Ctrl Pts',(0.175090590502344,-3.92910069673934,
10.5423065207097));
#256535=CARTESIAN_POINT('Ctrl Pts',(0.294617229838071,-3.92377428963569,
10.5483521246464));
#256536=CARTESIAN_POINT('Ctrl Pts',(0.41399439555861,-3.91298462757559,
10.5543977285831));
#256537=CARTESIAN_POINT('Ctrl Pts',(0.532686428291837,-3.89675944460441,
10.5604433325198));
#256538=CARTESIAN_POINT('Ctrl Pts',(0.647651693819147,-3.88104371014814,
10.566299112776));
#256539=CARTESIAN_POINT('Ctrl Pts',(0.761973768459893,-3.86022874706799,
10.5721548930322));
#256540=CARTESIAN_POINT('Ctrl Pts',(0.875170458626114,-3.83439247708788,
10.5780106732885));
#256541=CARTESIAN_POINT('Ctrl Pts',(0.988350538990038,-3.80855999816683,
10.5838655943027));
#256542=CARTESIAN_POINT('Ctrl Pts',(1.10040516093316,-3.77770776926417,
10.5897205153169));
#256543=CARTESIAN_POINT('Ctrl Pts',(1.21086302768579,-3.74196468825984,
10.5955754363312));
#256544=CARTESIAN_POINT('Ctrl Pts',(1.32133133840838,-3.7062182276894,10.6014309109376));
#256545=CARTESIAN_POINT('Ctrl Pts',(1.43020220108577,-3.66558012281681,
10.6072863855441));
#256546=CARTESIAN_POINT('Ctrl Pts',(1.53702084327476,-3.62022871202068,
10.6131418601506));
#256547=CARTESIAN_POINT('Ctrl Pts',(1.64387535903125,-3.57486207057883,
10.6189993012375));
#256548=CARTESIAN_POINT('Ctrl Pts',(1.74867590409265,-3.52477913685943,
10.6248567423243));
#256549=CARTESIAN_POINT('Ctrl Pts',(1.85098964382749,-3.47020551818526,
10.6307141834112));
#256550=CARTESIAN_POINT('Ctrl Pts',(1.95341870671994,-3.41557038673631,
10.6365782267257));
#256551=CARTESIAN_POINT('Ctrl Pts',(2.05335500541286,-3.35643466211395,
10.6424422700402));
#256552=CARTESIAN_POINT('Ctrl Pts',(2.15039210886709,-3.29306889969253,
10.6483063133547));
#256553=CARTESIAN_POINT('Ctrl Pts',(2.2474947796491,-3.22966032144533,10.6541743189644));
#256554=CARTESIAN_POINT('Ctrl Pts',(2.34169401995645,-3.16201625411257,
10.6600423245741));
#256555=CARTESIAN_POINT('Ctrl Pts',(2.43261546567258,-3.09044834873042,
10.6659103301838));
#256556=CARTESIAN_POINT('Ctrl Pts',(2.52366817290881,-3.01877712215735,
10.6717868073189));
#256557=CARTESIAN_POINT('Ctrl Pts',(2.61143333047028,-2.94317102094232,
10.6776632844541));
#256558=CARTESIAN_POINT('Ctrl Pts',(2.69557244450134,-2.86397943366308,
10.6835397615892));
#256559=CARTESIAN_POINT('Ctrl Pts',(2.71400085830244,-2.84663464275632,
10.6848268461227));
#256560=CARTESIAN_POINT('Ctrl Pts',(2.73225547823554,-2.82911798016423,
10.6861139306563));
#256561=CARTESIAN_POINT('Ctrl Pts',(2.75033300732677,-2.8114333264029,10.6874010151899));
#256562=CARTESIAN_POINT('Ctrl Pts',(2.83286256798328,-2.73069736420806,
10.6932769576679));
#256563=CARTESIAN_POINT('Ctrl Pts',(2.91197026617098,-2.64619115209094,
10.6991529001459));
#256564=CARTESIAN_POINT('Ctrl Pts',(2.98729231513605,-2.55823642846573,
10.7050288426239));
#256565=CARTESIAN_POINT('Ctrl Pts',(3.06251770547715,-2.47039457461337,
10.7108972446735));
#256566=CARTESIAN_POINT('Ctrl Pts',(3.13396684176829,-2.37911332079149,
10.7167656467231));
#256567=CARTESIAN_POINT('Ctrl Pts',(3.2013116962519,-2.28475215799018,10.7226340487727));
#256568=CARTESIAN_POINT('Ctrl Pts',(3.2685880759278,-2.19048693960107,10.7284964839566));
#256569=CARTESIAN_POINT('Ctrl Pts',(3.33176823636123,-2.09314837538507,
10.7343589191406));
#256570=CARTESIAN_POINT('Ctrl Pts',(3.39056391869926,-1.99312952745543,
10.7402213543245));
#256571=CARTESIAN_POINT('Ctrl Pts',(3.4511966416975,-1.88998564239505,10.7462669582611));
#256572=CARTESIAN_POINT('Ctrl Pts',(3.50716611065423,-1.7839915715819,10.7523125621978));
#256573=CARTESIAN_POINT('Ctrl Pts',(3.55820384001509,-1.67561165933575,
10.7583581661345));
#256574=CARTESIAN_POINT('Ctrl Pts',(3.60763905460163,-1.57063472784105,
10.7642139463907));
#256575=CARTESIAN_POINT('Ctrl Pts',(3.65244740997755,-1.46341994002382,
10.7700697266469));
#256576=CARTESIAN_POINT('Ctrl Pts',(3.69243163123173,-1.35441413484922,
10.7759255069032));
#256577=CARTESIAN_POINT('Ctrl Pts',(3.73240998544149,-1.24542432453163,
10.7817804279174));
#256578=CARTESIAN_POINT('Ctrl Pts',(3.76756547098869,-1.1346444068434,10.7876353489316));
#256579=CARTESIAN_POINT('Ctrl Pts',(3.79774949982489,-1.02253984596191,
10.7934902699458));
#256580=CARTESIAN_POINT('Ctrl Pts',(3.82793638260982,-0.910424685412919,
10.7993457445523));
#256581=CARTESIAN_POINT('Ctrl Pts',(3.85315076693146,-0.796985031274626,
10.8052012191588));
#256582=CARTESIAN_POINT('Ctrl Pts',(3.87329452870525,-0.682699416948595,
10.8110566937652));
#256583=CARTESIAN_POINT('Ctrl Pts',(3.89344505548359,-0.568375421375381,
10.8169141348521));
#256584=CARTESIAN_POINT('Ctrl Pts',(3.90852150191746,-0.453205306944438,
10.8227715759389));
#256585=CARTESIAN_POINT('Ctrl Pts',(3.91847733511552,-0.33767495344781,
10.8286290170258));
#256586=CARTESIAN_POINT('Ctrl Pts',(3.92844439005294,-0.222014379658201,
10.8344930603403));
#256587=CARTESIAN_POINT('Ctrl Pts',(3.93327927659204,-0.105993167825182,
10.8403571036548));
#256588=CARTESIAN_POINT('Ctrl Pts',(3.93298753885493,0.0099004652317022,
10.8462211469692));
#256589=CARTESIAN_POINT('Ctrl Pts',(3.93269560399257,0.125872406848457,
10.852089152579));
#256590=CARTESIAN_POINT('Ctrl Pts',(3.92727016634025,0.241716186768103,
10.8579571581887));
#256591=CARTESIAN_POINT('Ctrl Pts',(3.91676870068147,0.356948098975225,
10.8638251637984));
#256592=CARTESIAN_POINT('Ctrl Pts',(3.90625207426127,0.47234636924939,10.8697016409335));
#256593=CARTESIAN_POINT('Ctrl Pts',(3.89064485074995,0.587130601602925,
10.8755781180686));
#256594=CARTESIAN_POINT('Ctrl Pts',(3.87005569072855,0.70082661954263,10.8814545952037));
#256595=CARTESIAN_POINT('Ctrl Pts',(3.86554618804285,0.725728679545069,
10.8827416797373));
#256596=CARTESIAN_POINT('Ctrl Pts',(3.86079788622815,0.750578593974643,
10.8840287642709));
#256597=CARTESIAN_POINT('Ctrl Pts',(3.85581224405347,0.775371484262431,
10.8853158488044));
#256598=CARTESIAN_POINT('Ctrl Pts',(3.83305123196016,0.888558764034425,
10.8911917912824));
#256599=CARTESIAN_POINT('Ctrl Pts',(3.80526453482832,1.00092970005197,10.8970677337604));
#256600=CARTESIAN_POINT('Ctrl Pts',(3.77252384830424,1.11200396311155,10.9029436762384));
#256601=CARTESIAN_POINT('Ctrl Pts',(3.73982517696364,1.22293568775675,10.908812078288));
#256602=CARTESIAN_POINT('Ctrl Pts',(3.70218527481469,1.33257365628167,10.9146804803376));
#256603=CARTESIAN_POINT('Ctrl Pts',(3.65972697531004,1.4404469675028,10.9205488823872));
#256604=CARTESIAN_POINT('Ctrl Pts',(3.61731184649622,1.54821059544829,10.9264113175712));
#256605=CARTESIAN_POINT('Ctrl Pts',(3.5700882158666,1.65421275328576,10.9322737527551));
#256606=CARTESIAN_POINT('Ctrl Pts',(3.5182287318234,1.75799760823851,10.938136187939));
#256607=CARTESIAN_POINT('Ctrl Pts',(3.46474892504538,1.86502516726193,10.9441817918757));
#256608=CARTESIAN_POINT('Ctrl Pts',(3.40633893945029,1.96969416021409,10.9502273958124));
#256609=CARTESIAN_POINT('Ctrl Pts',(3.34324197483432,2.07152651387953,10.956272999749));
#256610=CARTESIAN_POINT('Ctrl Pts',(3.2821261684571,2.17016147116209,10.9621287800053));
#256611=CARTESIAN_POINT('Ctrl Pts',(3.21661354518778,2.26613488222249,10.9679845602615));
#256612=CARTESIAN_POINT('Ctrl Pts',(3.14697140833103,2.35903792999329,10.9738403405178));
#256613=CARTESIAN_POINT('Ctrl Pts',(3.07733949034308,2.45192734572894,10.979695261532));
#256614=CARTESIAN_POINT('Ctrl Pts',(3.00357951117047,2.54174696385068,10.9855501825462));
#256615=CARTESIAN_POINT('Ctrl Pts',(2.92600091158385,2.62811865512394,10.9914051035604));
#256616=CARTESIAN_POINT('Ctrl Pts',(2.84841497681519,2.71449851298027,10.9972605781669));
#256617=CARTESIAN_POINT('Ctrl Pts',(2.76700997971318,2.79742948882504,11.0031160527734));
#256618=CARTESIAN_POINT('Ctrl Pts',(2.68213380679111,2.87656865770108,11.0089715273798));
#256619=CARTESIAN_POINT('Ctrl Pts',(2.59722912937711,2.95573440437538,11.0148289684667));
#256620=CARTESIAN_POINT('Ctrl Pts',(2.50885125979425,3.03110553056513,11.0206864095535));
#256621=CARTESIAN_POINT('Ctrl Pts',(2.41738234469678,3.10237837788176,11.0265438506404));
#256622=CARTESIAN_POINT('Ctrl Pts',(2.32581033020973,3.1737315605456,11.0324078939549));
#256623=CARTESIAN_POINT('Ctrl Pts',(2.23114064211733,3.24097699072152,11.0382719372694));
#256624=CARTESIAN_POINT('Ctrl Pts',(2.13378575063507,3.30385341236362,11.0441359805839));
#256625=CARTESIAN_POINT('Ctrl Pts',(2.03636507709774,3.36677231918718,11.0500039861936));
#256626=CARTESIAN_POINT('Ctrl Pts',(1.93625594268604,3.42531613121839,11.0558719918033));
#256627=CARTESIAN_POINT('Ctrl Pts',(1.83389531842599,3.47926960166286,11.0617399974131));
#256628=CARTESIAN_POINT('Ctrl Pts',(1.73138691812661,3.53330096368164,11.0676164745482));
#256629=CARTESIAN_POINT('Ctrl Pts',(1.62662091305287,3.58272858352748,11.0734929516833));
#256630=CARTESIAN_POINT('Ctrl Pts',(1.52005416032774,3.62738533239444,11.0793694288184));
#256631=CARTESIAN_POINT('Ctrl Pts',(1.49671357445081,3.63716619420415,11.080656513352));
#256632=CARTESIAN_POINT('Ctrl Pts',(1.47328666009692,3.64671838249366,11.0819435978855));
#256633=CARTESIAN_POINT('Ctrl Pts',(1.44977830326759,3.65604046358551,11.0832306824191));
#256634=CARTESIAN_POINT('Ctrl Pts',(1.34245531951811,3.69859867234487,11.0891066248971));
#256635=CARTESIAN_POINT('Ctrl Pts',(1.23307975206688,3.73649739321613,11.0949825673751));
#256636=CARTESIAN_POINT('Ctrl Pts',(1.12209348527102,3.76953514512232,11.1008585098531));
#256637=CARTESIAN_POINT('Ctrl Pts',(1.0112496439664,3.80253050062955,11.1067269119027));
#256638=CARTESIAN_POINT('Ctrl Pts',(0.898799605987272,3.83067717600267,
11.1125953139523));
#256639=CARTESIAN_POINT('Ctrl Pts',(0.785205200775825,3.85382171262172,
11.1184637160019));
#256640=CARTESIAN_POINT('Ctrl Pts',(0.671726295926075,3.87694271637094,
11.1243261511859));
#256641=CARTESIAN_POINT('Ctrl Pts',(0.557105740426479,3.89507161631037,
11.1301885863698));
#256642=CARTESIAN_POINT('Ctrl Pts',(0.441819857916594,3.9081049388611,11.1360510215537));
#256643=CARTESIAN_POINT('Ctrl Pts',(0.32293192768335,3.92154548082847,11.1420966254904));
#256644=CARTESIAN_POINT('Ctrl Pts',(0.203336839629667,3.92956666629365,
11.1481422294271));
#256645=CARTESIAN_POINT('Ctrl Pts',(0.0835679952731944,3.93211207751839,
11.1541878333637));
#256646=CARTESIAN_POINT('Ctrl Pts',(-0.032440271467795,3.93457756631819,
11.16004361362));
#256647=CARTESIAN_POINT('Ctrl Pts',(-0.148611103168792,3.93190599372951,
11.1658993938762));
#256648=CARTESIAN_POINT('Ctrl Pts',(-0.264456053159735,3.92409887693304,
11.1717551741325));
#256649=CARTESIAN_POINT('Ctrl Pts',(-0.380284004758634,3.916292905706,11.1776100951467));
#256650=CARTESIAN_POINT('Ctrl Pts',(-0.495785758013729,3.90335291644478,
11.1834650161609));
#256651=CARTESIAN_POINT('Ctrl Pts',(-0.610475653048774,3.8853324796,11.1893199371751));
#256652=CARTESIAN_POINT('Ctrl Pts',(-0.725176392198759,3.86731033889379,
11.1951754117816));
#256653=CARTESIAN_POINT('Ctrl Pts',(-0.839064712756267,3.84420685975501,
11.2010308863881));
#256654=CARTESIAN_POINT('Ctrl Pts',(-0.951663540110443,3.81612702964989,
11.2068863609945));
#256655=CARTESIAN_POINT('Ctrl Pts',(-1.06430018222756,3.78803776932116,
11.2127438020814));
#256656=CARTESIAN_POINT('Ctrl Pts',(-1.1756460697404,3.75496893461153,11.2186012431682));
#256657=CARTESIAN_POINT('Ctrl Pts',(-1.28523839988161,3.7170756321966,11.2244586842551));
#256658=CARTESIAN_POINT('Ctrl Pts',(-1.39495425725982,3.67913961826215,
11.2303227275696));
#256659=CARTESIAN_POINT('Ctrl Pts',(-1.50291222204019,3.63636841809741,
11.2361867708841));
#256660=CARTESIAN_POINT('Ctrl Pts',(-1.60866853720992,3.58896566400278,
11.2420508141986));
#256661=CARTESIAN_POINT('Ctrl Pts',(-1.71449631122097,3.54153088018134,
11.2479188198083));
#256662=CARTESIAN_POINT('Ctrl Pts',(-1.8181191054644,3.48945849562897,11.253786825418));
#256663=CARTESIAN_POINT('Ctrl Pts',(-1.91911840501449,3.43299774942173,
11.2596548310277));
#256664=CARTESIAN_POINT('Ctrl Pts',(-2.02026351528604,3.37645549193494,
11.2655313081628));
#256665=CARTESIAN_POINT('Ctrl Pts',(-2.1187772227289,3.3155124458296,11.2714077852979));
#256666=CARTESIAN_POINT('Ctrl Pts',(-2.21427053641827,3.25046073527276,
11.277284262433));
#256667=CARTESIAN_POINT('Ctrl Pts',(-2.23518578279538,3.23621290470764,
11.2785713469666));
#256668=CARTESIAN_POINT('Ctrl Pts',(-2.25595626709445,3.2217681271305,11.2798584315002));
#256669=CARTESIAN_POINT('Ctrl Pts',(-2.27657812579469,3.20712971941472,
11.2811455160338));
#256670=CARTESIAN_POINT('Ctrl Pts',(-2.37011177574112,3.14073494273801,
11.2869832882718));
#256671=CARTESIAN_POINT('Ctrl Pts',(-2.46090272053026,3.07012825322945,
11.2928210605097));
#256672=CARTESIAN_POINT('Ctrl Pts',(-2.54854429308361,2.99556521981929,
11.2986588327477));
#256673=CARTESIAN_POINT('Ctrl Pts',(-2.636073061497,2.92109815706108,11.3044890911443));
#256674=CARTESIAN_POINT('Ctrl Pts',(-2.72046020090262,2.84268514339137,
11.3103193495408));
#256675=CARTESIAN_POINT('Ctrl Pts',(-2.80132819023628,2.76062481525243,
11.3161496079374));
#256676=CARTESIAN_POINT('Ctrl Pts',(-2.88211438511873,2.67864748756351,
11.3219739692814));
#256677=CARTESIAN_POINT('Ctrl Pts',(-2.95938821612785,2.59303047806507,
11.3277983306253));
#256678=CARTESIAN_POINT('Ctrl Pts',(-3.03280600594098,2.50411196441539,
11.3336226919693));
#256679=CARTESIAN_POINT('Ctrl Pts',(-3.1061713577615,2.4152569600102,11.3394428933159));
#256680=CARTESIAN_POINT('Ctrl Pts',(-3.17568588015654,2.32310546307272,
11.3452630946624));
#256681=CARTESIAN_POINT('Ctrl Pts',(-3.24104398157485,2.22803117336751,
11.3510832960089));
#256682=CARTESIAN_POINT('Ctrl Pts',(-3.30637760077524,2.13299249714294,
11.3569013171906));
#256683=CARTESIAN_POINT('Ctrl Pts',(-3.36755765655974,2.03503354879621,
11.3627193383723));
#256684=CARTESIAN_POINT('Ctrl Pts',(-3.424320368447,1.9345591265813,11.3685373595539));
#256685=CARTESIAN_POINT('Ctrl Pts',(-3.48107597672475,1.83409727830865,
11.3743546526352));
#256686=CARTESIAN_POINT('Ctrl Pts',(-3.53341513437636,1.7311209466672,11.3801719457165));
#256687=CARTESIAN_POINT('Ctrl Pts',(-3.58111914101488,1.62606109905405,
11.3859892387978));
#256688=CARTESIAN_POINT('Ctrl Pts',(-3.62882907721868,1.52098819259598,
11.3918072549634));
#256689=CARTESIAN_POINT('Ctrl Pts',(-3.67190254461371,1.41383163693878,
11.397625271129));
#256690=CARTESIAN_POINT('Ctrl Pts',(-3.71016859552723,1.30504329152848,
11.4034432872947));
#256691=CARTESIAN_POINT('Ctrl Pts',(-3.74847237718387,1.19614767962433,
11.4092670400876));
#256692=CARTESIAN_POINT('Ctrl Pts',(-3.78195913607339,1.08561746027754,
11.4150907928806));
#256693=CARTESIAN_POINT('Ctrl Pts',(-3.81050750947591,0.973920695040244,
11.4209145456735));
#256694=CARTESIAN_POINT('Ctrl Pts',(-3.83907020804644,0.862167881953742,
11.4267412207428));
#256695=CARTESIAN_POINT('Ctrl Pts',(-3.86268950016671,0.749247767014327,
11.4325678958121));
#256696=CARTESIAN_POINT('Ctrl Pts',(-3.8812953413101,0.63563784777536,11.4383945708815));
#256697=CARTESIAN_POINT('Ctrl Pts',(-3.89993071618738,0.521847591345708,
11.4442304948458));
#256698=CARTESIAN_POINT('Ctrl Pts',(-3.91353669293783,0.407365759236058,
11.4500664188101));
#256699=CARTESIAN_POINT('Ctrl Pts',(-3.92209517684827,0.292674603858209,
11.4559023427744));
#256700=CARTESIAN_POINT('Ctrl Pts',(-3.92939556642889,0.194843010731158,
11.4608803878287));
#256701=CARTESIAN_POINT('Ctrl Pts',(-3.9330242386882,0.0968592949186528,
11.4658584328829));
#256702=CARTESIAN_POINT('Ctrl Pts',(-3.93299987808706,-0.000979268682664797,
11.4708364779372));
#256703=CARTESIAN_POINT('',(-3.93299846730095,0.00347220511500596,12.7208364779205));
#256704=CARTESIAN_POINT('Ctrl Pts',(-3.93299987808693,-0.000979269229120141,
11.470836477965));
#256705=CARTESIAN_POINT('Ctrl Pts',(-3.932986463278,-0.0548566303192047,
11.4735777685261));
#256706=CARTESIAN_POINT('Ctrl Pts',(-3.93186601489811,-0.108718747047242,
11.4763190590872));
#256707=CARTESIAN_POINT('Ctrl Pts',(-3.92964011457576,-0.1625348267819,
11.4790603496483));
#256708=CARTESIAN_POINT('Ctrl Pts',(-3.9248689084726,-0.277889321994402,
11.4849362921262));
#256709=CARTESIAN_POINT('Ctrl Pts',(-3.91500618700124,-0.393223855087732,
11.4908122346041));
#256710=CARTESIAN_POINT('Ctrl Pts',(-3.90004760964988,-0.508052794957657,
11.496688177082));
#256711=CARTESIAN_POINT('Ctrl Pts',(-3.8851082282116,-0.622734378144019,
11.5025565791315));
#256712=CARTESIAN_POINT('Ctrl Pts',(-3.86508604871629,-0.736911252790357,
11.5084249811811));
#256713=CARTESIAN_POINT('Ctrl Pts',(-3.84002871377076,-0.850099098585613,
11.5142933832306));
#256714=CARTESIAN_POINT('Ctrl Pts',(-3.81499685658747,-0.96317185740017,
11.5201558184145));
#256715=CARTESIAN_POINT('Ctrl Pts',(-3.78494011629482,-1.07525718703231,
11.5260182535983));
#256716=CARTESIAN_POINT('Ctrl Pts',(-3.74995769455867,-1.18587785586047,
11.5318806887822));
#256717=CARTESIAN_POINT('Ctrl Pts',(-3.7138822651629,-1.29995481022693,
11.5379262927189));
#256718=CARTESIAN_POINT('Ctrl Pts',(-3.6725683515392,-1.41247363107052,
11.5439718966556));
#256719=CARTESIAN_POINT('Ctrl Pts',(-3.62618135805924,-1.52292408164808,
11.5500175005923));
#256720=CARTESIAN_POINT('Ctrl Pts',(-3.58125085261957,-1.62990653940605,
11.5558732808485));
#256721=CARTESIAN_POINT('Ctrl Pts',(-3.53156125119061,-1.73494816424003,
11.5617290611047));
#256722=CARTESIAN_POINT('Ctrl Pts',(-3.47731260073327,-1.83760335131975,
11.5675848413608));
#256723=CARTESIAN_POINT('Ctrl Pts',(-3.42307191039701,-1.94024347539402,
11.573439762375));
#256724=CARTESIAN_POINT('Ctrl Pts',(-3.364273694054,-2.04049749317739,11.5792946833892));
#256725=CARTESIAN_POINT('Ctrl Pts',(-3.30116441863936,-2.13794351681926,
11.5851496044034));
#256726=CARTESIAN_POINT('Ctrl Pts',(-3.23804917614063,-2.23539875414029,
11.5910050790098));
#256727=CARTESIAN_POINT('Ctrl Pts',(-3.17062228864709,-2.330045123064,11.5968605536162));
#256728=CARTESIAN_POINT('Ctrl Pts',(-3.09917370346276,-2.4214894911531,
11.6027160282227));
#256729=CARTESIAN_POINT('Ctrl Pts',(-3.02770112325666,-2.51296456957184,
11.6085734693095));
#256730=CARTESIAN_POINT('Ctrl Pts',(-2.95220441363665,-2.60123518377285,
11.6144309103963));
#256731=CARTESIAN_POINT('Ctrl Pts',(-2.87301350381704,-2.68594162387885,
11.6202883514831));
#256732=CARTESIAN_POINT('Ctrl Pts',(-2.79373333378863,-2.77074354103578,
11.6261523947976));
#256733=CARTESIAN_POINT('Ctrl Pts',(-2.71075093484285,-2.85197296420257,
11.632016438112));
#256734=CARTESIAN_POINT('Ctrl Pts',(-2.6244328206362,-2.92930731914006,
11.6378804814265));
#256735=CARTESIAN_POINT('Ctrl Pts',(-2.53805638185176,-3.00669392838873,
11.6437484870362));
#256736=CARTESIAN_POINT('Ctrl Pts',(-2.4483400581743,-3.08017996777959,
11.6496164926458));
#256737=CARTESIAN_POINT('Ctrl Pts',(-2.35568176100807,-3.14948447223572,
11.6554844982555));
#256738=CARTESIAN_POINT('Ctrl Pts',(-2.26288969486313,-3.21888903025493,
11.6613609753906));
#256739=CARTESIAN_POINT('Ctrl Pts',(-2.16714751893534,-3.28409977454673,
11.6672374525256));
#256740=CARTESIAN_POINT('Ctrl Pts',(-2.06888031443449,-3.3448801539884,
11.6731139296607));
#256741=CARTESIAN_POINT('Ctrl Pts',(-2.04735752174451,-3.35819246416336,
11.6744010141948));
#256742=CARTESIAN_POINT('Ctrl Pts',(-2.02571368513469,-3.37129242426332,
11.675688098729));
#256743=CARTESIAN_POINT('Ctrl Pts',(-2.00395340611494,-3.38417785379556,
11.6769751832631));
#256744=CARTESIAN_POINT('Ctrl Pts',(-1.90461094302503,-3.44300385995762,
11.6828511257411));
#256745=CARTESIAN_POINT('Ctrl Pts',(-1.80251214411554,-3.49754891528115,
11.6887270682191));
#256746=CARTESIAN_POINT('Ctrl Pts',(-1.69806192741774,-3.5475448821198,
11.6946030106971));
#256747=CARTESIAN_POINT('Ctrl Pts',(-1.59374574868561,-3.59747669056893,
11.7004714127467));
#256748=CARTESIAN_POINT('Ctrl Pts',(-1.48708452211269,-3.64287084351938,
11.7063398147964));
#256749=CARTESIAN_POINT('Ctrl Pts',(-1.37851037885044,-3.68350351369476,
11.712208216846));
#256750=CARTESIAN_POINT('Ctrl Pts',(-1.27004663145496,-3.72409486944012,
11.7180706520299));
#256751=CARTESIAN_POINT('Ctrl Pts',(-1.15967422058035,-3.75993422872318,
11.7239330872139));
#256752=CARTESIAN_POINT('Ctrl Pts',(-1.04784741381294,-3.79084486590595,
11.7297955223978));
#256753=CARTESIAN_POINT('Ctrl Pts',(-0.932526636353501,-3.82272128994709,
11.7358411263345));
#256754=CARTESIAN_POINT('Ctrl Pts',(-0.815659488326674,-3.84935574535524,
11.7418867302711));
#256755=CARTESIAN_POINT('Ctrl Pts',(-0.697763974666621,-3.87060905228847,
11.7479323342078));
#256756=CARTESIAN_POINT('Ctrl Pts',(-0.583570218604554,-3.89119503450356,
11.753788114464));
#256757=CARTESIAN_POINT('Ctrl Pts',(-0.468412146030773,-3.90673265849635,
11.7596438947203));
#256758=CARTESIAN_POINT('Ctrl Pts',(-0.35277242529478,-3.91714699953316,
11.7654996749765));
#256759=CARTESIAN_POINT('Ctrl Pts',(-0.237149672836769,-3.92755981243212,
11.7713545959907));
#256760=CARTESIAN_POINT('Ctrl Pts',(-0.121045823738458,-3.93285080021131,
11.777209517005));
#256761=CARTESIAN_POINT('Ctrl Pts',(-0.00494893822420919,-3.9329968863464,
11.7830644380192));
#256762=CARTESIAN_POINT('Ctrl Pts',(0.111158924438277,-3.93314298629416,
11.7889199126257));
#256763=CARTESIAN_POINT('Ctrl Pts',(0.227259409429624,-3.92814321704365,
11.7947753872321));
#256764=CARTESIAN_POINT('Ctrl Pts',(0.342864891257786,-3.91802662910078,
11.8006308618386));
#256765=CARTESIAN_POINT('Ctrl Pts',(0.458509197592445,-3.90790664364138,
11.8064883029255));
#256766=CARTESIAN_POINT('Ctrl Pts',(0.573657759239503,-3.89266645841358,
11.8123457440123));
#256767=CARTESIAN_POINT('Ctrl Pts',(0.687829205038584,-3.87238685886315,
11.8182031850992));
#256768=CARTESIAN_POINT('Ctrl Pts',(0.802129339434854,-3.85208440111731,
11.8240672284137));
#256769=CARTESIAN_POINT('Ctrl Pts',(0.915449753188868,-3.82673126423591,
11.8299312717282));
#256770=CARTESIAN_POINT('Ctrl Pts',(1.02732029392263,-3.7964591415811,11.8357953150427));
#256771=CARTESIAN_POINT('Ctrl Pts',(1.13926642483947,-3.76616656425362,
11.8416633206524));
#256772=CARTESIAN_POINT('Ctrl Pts',(1.24976033968641,-3.73094850778175,
11.8475313262621));
#256773=CARTESIAN_POINT('Ctrl Pts',(1.35834968157471,-3.69098566003254,
11.8533993318718));
#256774=CARTESIAN_POINT('Ctrl Pts',(1.46709579178068,-3.65096511869848,
11.8592758090069));
#256775=CARTESIAN_POINT('Ctrl Pts',(1.57393146263382,-3.60618627485286,
11.865152286142));
#256776=CARTESIAN_POINT('Ctrl Pts',(1.6784267877521,-3.556876792659,11.8710287632771));
#256777=CARTESIAN_POINT('Ctrl Pts',(1.70131368302734,-3.54607687454046,
11.8723158478106));
#256778=CARTESIAN_POINT('Ctrl Pts',(1.72408841378939,-3.53505978527574,
11.8736029323441));
#256779=CARTESIAN_POINT('Ctrl Pts',(1.74674664513664,-3.52382819639435,
11.8748900168775));
#256780=CARTESIAN_POINT('Ctrl Pts',(1.85018854082262,-3.47255248878723,
11.8807659593555));
#256781=CARTESIAN_POINT('Ctrl Pts',(1.95154137990094,-3.41663353127061,
11.8866419018335));
#256782=CARTESIAN_POINT('Ctrl Pts',(2.05035974727023,-3.35626487434677,
11.8925178443115));
#256783=CARTESIAN_POINT('Ctrl Pts',(2.14905130386437,-3.29597368678803,
11.8983862463611));
#256784=CARTESIAN_POINT('Ctrl Pts',(2.24521450782985,-3.23124436901653,
11.9042546484107));
#256785=CARTESIAN_POINT('Ctrl Pts',(2.33842628410832,-3.16231742774051,
11.9101230504604));
#256786=CARTESIAN_POINT('Ctrl Pts',(2.43154328464627,-3.09346056990418,
11.9159854856443));
#256787=CARTESIAN_POINT('Ctrl Pts',(2.52171449684375,-3.02041482227373,
11.9218479208282));
#256788=CARTESIAN_POINT('Ctrl Pts',(2.60854429162626,-2.94346491037757,
11.9277103560122));
#256789=CARTESIAN_POINT('Ctrl Pts',(2.69808703840084,-2.86411073831598,
11.9337559599488));
#256790=CARTESIAN_POINT('Ctrl Pts',(2.78407575239366,-2.78060465728777,
11.9398015638855));
#256791=CARTESIAN_POINT('Ctrl Pts',(2.86611157855576,-2.69330529633545,
11.9458471678222));
#256792=CARTESIAN_POINT('Ctrl Pts',(2.9455715921751,-2.60874701570664,11.9517029480784));
#256793=CARTESIAN_POINT('Ctrl Pts',(3.02132293353721,-2.5206304240791,11.9575587283347));
#256794=CARTESIAN_POINT('Ctrl Pts',(3.09303988209523,-2.42931951125584,
11.9634145085909));
#256795=CARTESIAN_POINT('Ctrl Pts',(3.16474630733907,-2.33802199684736,
11.9692694296052));
#256796=CARTESIAN_POINT('Ctrl Pts',(3.2324192620312,-2.24353141779136,11.9751243506194));
#256797=CARTESIAN_POINT('Ctrl Pts',(3.2957735722646,-2.14624452482988,11.9809792716336));
#256798=CARTESIAN_POINT('Ctrl Pts',(3.35913387275045,-2.04894843323539,
11.9868347462401));
#256799=CARTESIAN_POINT('Ctrl Pts',(3.41817449179202,-1.94885584804075,
11.9926902208466));
#256800=CARTESIAN_POINT('Ctrl Pts',(3.47265420940231,-1.84639154621126,
11.9985456954531));
#256801=CARTESIAN_POINT('Ctrl Pts',(3.52715222327429,-1.74389283315933,
12.0044031365399));
#256802=CARTESIAN_POINT('Ctrl Pts',(3.57708609625411,-1.63902118387141,
12.0102605776268));
#256803=CARTESIAN_POINT('Ctrl Pts',(3.62226140306803,-1.5322243072878,12.0161180187137));
#256804=CARTESIAN_POINT('Ctrl Pts',(3.66748762932876,-1.425307054369,12.0219820620282));
#256805=CARTESIAN_POINT('Ctrl Pts',(3.70794442332027,-1.31646062336182,
12.0278461053427));
#256806=CARTESIAN_POINT('Ctrl Pts',(3.74348616475801,-1.20615104123213,
12.0337101486572));
#256807=CARTESIAN_POINT('Ctrl Pts',(3.77905192151493,-1.09576692364876,
12.0395781542669));
#256808=CARTESIAN_POINT('Ctrl Pts',(3.80969590381713,-0.983918083384415,
12.0454461598766));
#256809=CARTESIAN_POINT('Ctrl Pts',(3.83532327363904,-0.871082307639612,
12.0513141654864));
#256810=CARTESIAN_POINT('Ctrl Pts',(3.86098764119555,-0.758083633083303,
12.0571906426215));
#256811=CARTESIAN_POINT('Ctrl Pts',(3.88162086975249,-0.64409558413927,
12.0630671197566));
#256812=CARTESIAN_POINT('Ctrl Pts',(3.89717974628138,-0.529602705029176,
12.0689435968917));
#256813=CARTESIAN_POINT('Ctrl Pts',(3.90058750043051,-0.50452611398427,
12.0702306814252));
#256814=CARTESIAN_POINT('Ctrl Pts',(3.90375203058196,-0.479425309890811,
12.0715177659588));
#256815=CARTESIAN_POINT('Ctrl Pts',(3.90667321626538,-0.454305383321326,
12.0728048504923));
#256816=CARTESIAN_POINT('Ctrl Pts',(3.92000934034745,-0.339625080879565,
12.0786807929703));
#256817=CARTESIAN_POINT('Ctrl Pts',(3.92831353277412,-0.224167867215506,
12.0845567354483));
#256818=CARTESIAN_POINT('Ctrl Pts',(3.93150552379089,-0.108412713284382,
12.0904326779263));
#256819=CARTESIAN_POINT('Ctrl Pts',(3.93469341861719,0.00719389537941079,
12.0963010799759));
#256820=CARTESIAN_POINT('Ctrl Pts',(3.93278214745572,0.123097275047859,
12.1021694820255));
#256821=CARTESIAN_POINT('Ctrl Pts',(3.92574298853633,0.238811616044628,
12.1080378840751));
#256822=CARTESIAN_POINT('Ctrl Pts',(3.91871098688318,0.354408301174369,
12.113900319259));
#256823=CARTESIAN_POINT('Ctrl Pts',(3.90656149358598,0.469815920371005,
12.1197627544429));
#256824=CARTESIAN_POINT('Ctrl Pts',(3.88931782004195,0.584547598322071,
12.1256251896269));
#256825=CARTESIAN_POINT('Ctrl Pts',(3.87153537684389,0.702864008162148,
12.1316707935635));
#256826=CARTESIAN_POINT('Ctrl Pts',(3.84833517818206,0.820461096922471,
12.1377163975002));
#256827=CARTESIAN_POINT('Ctrl Pts',(3.81980075876842,0.936809032467246,
12.1437620014369));
#256828=CARTESIAN_POINT('Ctrl Pts',(3.79216228102892,1.04950380224599,12.1496177816931));
#256829=CARTESIAN_POINT('Ctrl Pts',(3.75951965410202,1.16102625893289,12.1554735619493));
#256830=CARTESIAN_POINT('Ctrl Pts',(3.72200074105462,1.27090498605871,12.1613293422055));
#256831=CARTESIAN_POINT('Ctrl Pts',(3.68448733330713,1.38076759024019,12.1671842632198));
#256832=CARTESIAN_POINT('Ctrl Pts',(3.64209919556459,1.48898655394699,12.173039184234));
#256833=CARTESIAN_POINT('Ctrl Pts',(3.59501374996098,1.59510662264047,12.1788941052482));
#256834=CARTESIAN_POINT('Ctrl Pts',(3.54792385235234,1.70123672515805,12.1847495798546));
#256835=CARTESIAN_POINT('Ctrl Pts',(3.49613593138806,1.80526716084839,12.1906050544611));
#256836=CARTESIAN_POINT('Ctrl Pts',(3.43987485319026,1.90676427341957,12.1964605290676));
#256837=CARTESIAN_POINT('Ctrl Pts',(3.38359488048542,2.00829547239596,12.2023179701544));
#256838=CARTESIAN_POINT('Ctrl Pts',(3.32283896334772,2.10729129568078,12.2081754112412));
#256839=CARTESIAN_POINT('Ctrl Pts',(3.25787668674578,2.20334484227012,12.2140328523281));
#256840=CARTESIAN_POINT('Ctrl Pts',(3.19284118777035,2.29950665582656,12.2198968956426));
#256841=CARTESIAN_POINT('Ctrl Pts',(3.12359009774898,2.39271923144746,12.2257609389571));
#256842=CARTESIAN_POINT('Ctrl Pts',(3.05043494582662,2.48260662233866,12.2316249822715));
#256843=CARTESIAN_POINT('Ctrl Pts',(2.97723036345287,2.57255474954424,12.2374929878812));
#256844=CARTESIAN_POINT('Ctrl Pts',(2.90011674010459,2.6591729105376,12.2433609934909));
#256845=CARTESIAN_POINT('Ctrl Pts',(2.81944312622333,2.74212134268198,12.2492289991006));
#256846=CARTESIAN_POINT('Ctrl Pts',(2.73865304541716,2.82518952586208,12.2551054762357));
#256847=CARTESIAN_POINT('Ctrl Pts',(2.65429301682881,2.90457712564489,12.2609819533708));
#256848=CARTESIAN_POINT('Ctrl Pts',(2.56674587516822,2.97998399531053,12.2668584305059));
#256849=CARTESIAN_POINT('Ctrl Pts',(2.54757102441917,2.99649984544414,12.2681455150396));
#256850=CARTESIAN_POINT('Ctrl Pts',(2.52824339585754,3.01282489954851,12.2694325995732));
#256851=CARTESIAN_POINT('Ctrl Pts',(2.50876719315735,3.02895628402547,12.2707196841068));
#256852=CARTESIAN_POINT('Ctrl Pts',(2.41985225108104,3.10260108729945,12.2765956265848));
#256853=CARTESIAN_POINT('Ctrl Pts',(2.32754511504253,3.17244892502778,12.2824715690628));
#256854=CARTESIAN_POINT('Ctrl Pts',(2.23220376281934,3.23817160775262,12.2883475115408));
#256855=CARTESIAN_POINT('Ctrl Pts',(2.1369847594175,3.30380995044472,12.2942159135904));
#256856=CARTESIAN_POINT('Ctrl Pts',(2.03873962015154,3.3653334336578,12.30008431564));
#256857=CARTESIAN_POINT('Ctrl Pts',(1.93786013364157,3.42245337476534,12.3059527176896));
#256858=CARTESIAN_POINT('Ctrl Pts',(1.83708321923592,3.47951523753842,12.3118151528736));
#256859=CARTESIAN_POINT('Ctrl Pts',(1.73367764265923,3.53218226222067,12.3176775880575));
#256860=CARTESIAN_POINT('Ctrl Pts',(1.62806442594008,3.5802088242152,12.3235400232414));
#256861=CARTESIAN_POINT('Ctrl Pts',(1.51915137893325,3.6297359512792,12.3295856271781));
#256862=CARTESIAN_POINT('Ctrl Pts',(1.40789083876213,3.67432761758209,12.3356312311148));
#256863=CARTESIAN_POINT('Ctrl Pts',(1.29477265429651,3.71376530945158,12.3416768350514));
#256864=CARTESIAN_POINT('Ctrl Pts',(1.185206225838,3.75196471183061,12.3475326153077));
#256865=CARTESIAN_POINT('Ctrl Pts',(1.07389748232933,3.78532881015082,12.3533883955639));
#256866=CARTESIAN_POINT('Ctrl Pts',(0.961311424728222,3.81370808330777,
12.3592441758202));
#256867=CARTESIAN_POINT('Ctrl Pts',(0.848741887328872,3.84208319226065,
12.3650990968344));
#256868=CARTESIAN_POINT('Ctrl Pts',(0.734895808662076,3.86547482963971,
12.3709540178486));
#256869=CARTESIAN_POINT('Ctrl Pts',(0.620251627416566,3.88378384036587,
12.3768089388628));
#256870=CARTESIAN_POINT('Ctrl Pts',(0.505596606378347,3.90209458223861,
12.3826644134693));
#256871=CARTESIAN_POINT('Ctrl Pts',(0.390143740363369,3.91532167703186,
12.3885198880758));
#256872=CARTESIAN_POINT('Ctrl Pts',(0.27437919456943,3.92341752272014,12.3943753626822));
#256873=CARTESIAN_POINT('Ctrl Pts',(0.1585757708495,3.93151608728653,12.4002328037691));
#256874=CARTESIAN_POINT('Ctrl Pts',(0.0424608707332888,3.93447994729295,
12.406090244856));
#256875=CARTESIAN_POINT('Ctrl Pts',(-0.0734774233447359,3.93231357705087,
12.4119476859428));
#256876=CARTESIAN_POINT('Ctrl Pts',(-0.189546397526822,3.93014476497979,
12.4178117292573));
#256877=CARTESIAN_POINT('Ctrl Pts',(-0.305437955469581,3.92283418903382,
12.4236757725718));
#256878=CARTESIAN_POINT('Ctrl Pts',(-0.420667130208069,3.91043835977023,
12.4295398158863));
#256879=CARTESIAN_POINT('Ctrl Pts',(-0.535974164536327,3.89803415472696,
12.435407821496));
#256880=CARTESIAN_POINT('Ctrl Pts',(-0.650617517431927,3.88053791636966,
12.4412758271057));
#256881=CARTESIAN_POINT('Ctrl Pts',(-0.76412213248344,3.85805733065865,
12.4471438327155));
#256882=CARTESIAN_POINT('Ctrl Pts',(-0.877790611936774,3.83554429016394,
12.4530203098506));
#256883=CARTESIAN_POINT('Ctrl Pts',(-0.990316673393825,3.80803263961904,
12.4588967869857));
#256884=CARTESIAN_POINT('Ctrl Pts',(-1.10124008445549,3.77567997536715,
12.4647732641208));
#256885=CARTESIAN_POINT('Ctrl Pts',(-1.12553487936497,3.76859399292889,
12.4660603486543));
#256886=CARTESIAN_POINT('Ctrl Pts',(-1.14975287015872,3.76127596456289,
12.4673474331879));
#256887=CARTESIAN_POINT('Ctrl Pts',(-1.17388935733151,3.75372785064978,
12.4686345177215));
#256888=CARTESIAN_POINT('Ctrl Pts',(-1.28407995208228,3.71926835555517,
12.4745104601995));
#256889=CARTESIAN_POINT('Ctrl Pts',(-1.39293371009581,3.67989593925522,
12.4803864026774));
#256890=CARTESIAN_POINT('Ctrl Pts',(-1.49998041874247,3.63573207805377,
12.4862623451554));
#256891=CARTESIAN_POINT('Ctrl Pts',(-1.60688975741978,3.59162489106806,
12.4921307472051));
#256892=CARTESIAN_POINT('Ctrl Pts',(-1.71199628031148,3.54273864329141,
12.4979991492547));
#256893=CARTESIAN_POINT('Ctrl Pts',(-1.81484449284045,3.48924468428436,
12.5038675513043));
#256894=CARTESIAN_POINT('Ctrl Pts',(-1.91758813150674,3.43580511679065,
12.5097299864882));
#256895=CARTESIAN_POINT('Ctrl Pts',(-2.01807766321097,3.37776734655479,
12.5155924216722));
#256896=CARTESIAN_POINT('Ctrl Pts',(-2.11587778278081,3.31535069160633,
12.5214548568561));
#256897=CARTESIAN_POINT('Ctrl Pts',(-2.21673361646199,3.25098386058296,
12.5275004607928));
#256898=CARTESIAN_POINT('Ctrl Pts',(-2.31472880378298,3.18196018518997,
12.5335460647294));
#256899=CARTESIAN_POINT('Ctrl Pts',(-2.40941329025367,3.10857147203486,
12.5395916686661));
#256900=CARTESIAN_POINT('Ctrl Pts',(-2.50112481357806,3.03748706392165,
12.5454474489223));
#256901=CARTESIAN_POINT('Ctrl Pts',(-2.58973008021745,2.96230790349821,
12.5513032291786));
#256902=CARTESIAN_POINT('Ctrl Pts',(-2.67485043070648,2.88334253486286,
12.5571590094348));
#256903=CARTESIAN_POINT('Ctrl Pts',(-2.75995829114658,2.80438875313136,
12.5630139304491));
#256904=CARTESIAN_POINT('Ctrl Pts',(-2.84158194972849,2.72165014855775,
12.5688688514633));
#256905=CARTESIAN_POINT('Ctrl Pts',(-2.9193776684205,2.63547396669511,12.5747237724775));
#256906=CARTESIAN_POINT('Ctrl Pts',(-2.99718074282344,2.5492896367352,12.580579247084));
#256907=CARTESIAN_POINT('Ctrl Pts',(-3.07115488123778,2.4596673897561,12.5864347216904));
#256908=CARTESIAN_POINT('Ctrl Pts',(-3.14099537318366,2.36698902947158,
12.5922901962969));
#256909=CARTESIAN_POINT('Ctrl Pts',(-3.21085932009554,2.27427954443796,
12.5981476373838));
#256910=CARTESIAN_POINT('Ctrl Pts',(-3.27658661179615,2.17851223466658,
12.6040050784706));
#256911=CARTESIAN_POINT('Ctrl Pts',(-3.33791516821867,2.08009887499987,
12.6098625195575));
#256912=CARTESIAN_POINT('Ctrl Pts',(-3.39931285125894,1.98157458849757,
12.615726562872));
#256913=CARTESIAN_POINT('Ctrl Pts',(-3.45630168489255,1.88039864983544,
12.6215906061865));
#256914=CARTESIAN_POINT('Ctrl Pts',(-3.50866492688975,1.77700856239178,
12.627454649501));
#256915=CARTESIAN_POINT('Ctrl Pts',(-3.56106355038251,1.67354861495132,
12.6333226551107));
#256916=CARTESIAN_POINT('Ctrl Pts',(-3.60883018901355,1.56787191480564,
12.6391906607204));
#256917=CARTESIAN_POINT('Ctrl Pts',(-3.65179641735151,1.46043552621082,
12.6450586663301));
#256918=CARTESIAN_POINT('Ctrl Pts',(-3.69482467519638,1.35284403379454,
12.6509351434652));
#256919=CARTESIAN_POINT('Ctrl Pts',(-3.73303855673301,1.24348817121452,
12.6568116206003));
#256920=CARTESIAN_POINT('Ctrl Pts',(-3.76631956849907,1.13283975386679,
12.6626880977354));
#256921=CARTESIAN_POINT('Ctrl Pts',(-3.77360888053423,1.10860518894691,
12.663975182269));
#256922=CARTESIAN_POINT('Ctrl Pts',(-3.78066175253088,1.08430865392967,
12.6652622668025));
#256923=CARTESIAN_POINT('Ctrl Pts',(-3.78747726902243,1.05995515784319,
12.6665493513361));
#256924=CARTESIAN_POINT('Ctrl Pts',(-3.82661172756583,0.920118230712979,
12.6739397459427));
#256925=CARTESIAN_POINT('Ctrl Pts',(-3.85802042500415,0.778031742465942,
12.6813301405493));
#256926=CARTESIAN_POINT('Ctrl Pts',(-3.88148939352243,0.634451801142437,
12.6887205351559));
#256927=CARTESIAN_POINT('Ctrl Pts',(-3.90458226727896,0.493172756161358,
12.6959924972589));
#256928=CARTESIAN_POINT('Ctrl Pts',(-3.91998784976489,0.350447625091903,
12.7032644593619));
#256929=CARTESIAN_POINT('Ctrl Pts',(-3.92754791774603,0.207017762061202,
12.7105364214649));
#256930=CARTESIAN_POINT('Ctrl Pts',(-3.93111729493799,0.139299418386965,
12.7139697736168));
#256931=CARTESIAN_POINT('Ctrl Pts',(-3.93293847653105,0.0714242984524084,
12.7174031257686));
#256932=CARTESIAN_POINT('Ctrl Pts',(-3.93299846730095,0.0034722051150112,
12.7208364779205));
#256933=CARTESIAN_POINT('',(-3.93299957516998,-0.0018280352083959,13.9708364780037));
#256934=CARTESIAN_POINT('Ctrl Pts',(-3.93299846730173,0.00347220423347139,
12.720836477965));
#256935=CARTESIAN_POINT('Ctrl Pts',(-3.93310303389525,-0.114971361987911,
12.7268209657561));
#256936=CARTESIAN_POINT('Ctrl Pts',(-3.92785234975832,-0.23353116451013,
12.7328054535471));
#256937=CARTESIAN_POINT('Ctrl Pts',(-3.91724514225673,-0.35168095692834,
12.7387899413382));
#256938=CARTESIAN_POINT('Ctrl Pts',(-3.90695911630223,-0.466253225939748,
12.7445932214885));
#256939=CARTESIAN_POINT('Ctrl Pts',(-3.89163632232622,-0.580439506551743,
12.7503965016387));
#256940=CARTESIAN_POINT('Ctrl Pts',(-3.87132845003179,-0.69376150943566,
12.7561997817889));
#256941=CARTESIAN_POINT('Ctrl Pts',(-3.85102457356454,-0.80706121480204,
12.7620019200714));
#256942=CARTESIAN_POINT('Ctrl Pts',(-3.82573764262538,-0.919496566210199,
12.7678040583539));
#256943=CARTESIAN_POINT('Ctrl Pts',(-3.79557082352466,-1.03059745953906,
12.7736061966364));
#256944=CARTESIAN_POINT('Ctrl Pts',(-3.76540233153998,-1.14170451390536,
12.7794086566731));
#256945=CARTESIAN_POINT('Ctrl Pts',(-3.73035352440218,-1.25147655692455,
12.7852111167099));
#256946=CARTESIAN_POINT('Ctrl Pts',(-3.69057778123338,-1.35945748027165,
12.7910135767467));
#256947=CARTESIAN_POINT('Ctrl Pts',(-3.650789799573,-1.46747162797899,12.7968178221268));
#256948=CARTESIAN_POINT('Ctrl Pts',(-3.60627213698255,-1.57369316595428,
12.802622067507));
#256949=CARTESIAN_POINT('Ctrl Pts',(-3.5572264497822,-1.6776856037321,12.8084263128871));
#256950=CARTESIAN_POINT('Ctrl Pts',(-3.50812621746861,-1.78179369447795,
12.8142370133347));
#256951=CARTESIAN_POINT('Ctrl Pts',(-3.45448809157378,-1.88366735725365,
12.8200477137823));
#256952=CARTESIAN_POINT('Ctrl Pts',(-3.39655984729305,-1.98289440055607,
12.82585841423));
#256953=CARTESIAN_POINT('Ctrl Pts',(-3.33859279959578,-2.08218791140539,
12.8316730069936));
#256954=CARTESIAN_POINT('Ctrl Pts',(-3.27633014163088,-2.17883092171571,
12.8374875997572));
#256955=CARTESIAN_POINT('Ctrl Pts',(-3.21006212263405,-2.27244145553416,
12.8433021925207));
#256956=CARTESIAN_POINT('Ctrl Pts',(-3.14369783785791,-2.3661879748721,
12.8491252319878));
#256957=CARTESIAN_POINT('Ctrl Pts',(-3.07331684109543,-2.45689289848686,
12.8549482714548));
#256958=CARTESIAN_POINT('Ctrl Pts',(-2.99924858950895,-2.54420850134744,
12.8607713109218));
#256959=CARTESIAN_POINT('Ctrl Pts',(-2.98359097494738,-2.5626665319546,
12.8620022689315));
#256960=CARTESIAN_POINT('Ctrl Pts',(-2.96776871131024,-2.5809732386353,
12.8632332269411));
#256961=CARTESIAN_POINT('Ctrl Pts',(-2.95178510743871,-2.59912556054974,
12.8644641849508));
#256962=CARTESIAN_POINT('Ctrl Pts',(-2.87548783636751,-2.68577514451157,
12.8703401274288));
#256963=CARTESIAN_POINT('Ctrl Pts',(-2.79524606960399,-2.76920527495376,
12.8762160699067));
#256964=CARTESIAN_POINT('Ctrl Pts',(-2.71136202697481,-2.84903579455911,
12.8820920123847));
#256965=CARTESIAN_POINT('Ctrl Pts',(-2.62758563033063,-2.92876386994925,
12.8879604144343));
#256966=CARTESIAN_POINT('Ctrl Pts',(-2.54017654948023,-3.00490123896631,
12.8938288164839));
#256967=CARTESIAN_POINT('Ctrl Pts',(-2.44947657998768,-3.07710147445479,
12.8996972185335));
#256968=CARTESIAN_POINT('Ctrl Pts',(-2.3588688322841,-3.14922829828814,
12.9055596537174));
#256969=CARTESIAN_POINT('Ctrl Pts',(-2.2649771728396,-3.21742569591253,
12.9114220889013));
#256970=CARTESIAN_POINT('Ctrl Pts',(-2.1681790075239,-3.28138519398937,
12.9172845240853));
#256971=CARTESIAN_POINT('Ctrl Pts',(-2.06835643363839,-3.34734307347637,
12.9233301280219));
#256972=CARTESIAN_POINT('Ctrl Pts',(-1.96544306736774,-3.40879357018475,
12.9293757319586));
#256973=CARTESIAN_POINT('Ctrl Pts',(-1.8598885355758,-3.46544421903364,
12.9354213358953));
#256974=CARTESIAN_POINT('Ctrl Pts',(-1.75764827146028,-3.52031611512659,
12.9412771161515));
#256975=CARTESIAN_POINT('Ctrl Pts',(-1.65293061040441,-3.57068486437814,
12.9471328964077));
#256976=CARTESIAN_POINT('Ctrl Pts',(-1.54617143208549,-3.61633003231214,
12.952988676664));
#256977=CARTESIAN_POINT('Ctrl Pts',(-1.43942791896704,-3.6619685025484,
12.9588435976782));
#256978=CARTESIAN_POINT('Ctrl Pts',(-1.33064386367743,-3.70288460746818,
12.9646985186924));
#256979=CARTESIAN_POINT('Ctrl Pts',(-1.22027629848336,-3.73890555582242,
12.9705534397066));
#256980=CARTESIAN_POINT('Ctrl Pts',(-1.10989829785761,-3.77492991001554,
12.9764089143131));
#256981=CARTESIAN_POINT('Ctrl Pts',(-0.997936882098993,-3.80605805947923,
12.9822643889195));
#256982=CARTESIAN_POINT('Ctrl Pts',(-0.884864780905563,-3.83216692218814,
12.988119863526));
#256983=CARTESIAN_POINT('Ctrl Pts',(-0.77175470600656,-3.85828455319848,
12.9939773046128));
#256984=CARTESIAN_POINT('Ctrl Pts',(-0.65753360590397,-3.87937945273476,
12.9998347456997));
#256985=CARTESIAN_POINT('Ctrl Pts',(-0.542684251875529,-3.89537967376305,
13.0056921867865));
#256986=CARTESIAN_POINT('Ctrl Pts',(-0.427705445144124,-3.91139792947579,
13.011556230101));
#256987=CARTESIAN_POINT('Ctrl Pts',(-0.312097380138019,-3.92230998833659,
13.0174202734155));
#256988=CARTESIAN_POINT('Ctrl Pts',(-0.196347892718441,-3.92809578613162,
13.02328431673));
#256989=CARTESIAN_POINT('Ctrl Pts',(-0.080520194137626,-3.93388549335187,
13.0291523223397));
#256990=CARTESIAN_POINT('Ctrl Pts',(0.035448705427454,-3.93454203988918,
13.0350203279494));
#256991=CARTESIAN_POINT('Ctrl Pts',(0.151072751616917,-3.93009745728002,
13.0408883335591));
#256992=CARTESIAN_POINT('Ctrl Pts',(0.266863721990182,-3.92564645811351,
13.0467648106942));
#256993=CARTESIAN_POINT('Ctrl Pts',(0.38230843572701,-3.91607966696002,
13.0526412878293));
#256994=CARTESIAN_POINT('Ctrl Pts',(0.496927670840884,-3.90148073043462,
13.0585177649644));
#256995=CARTESIAN_POINT('Ctrl Pts',(0.522031936778244,-3.89828322536863,
13.059804849498));
#256996=CARTESIAN_POINT('Ctrl Pts',(0.547096650833877,-3.89484451534116,
13.0610919340317));
#256997=CARTESIAN_POINT('Ctrl Pts',(0.572116864656961,-3.89116580129594,
13.0623790185654));
#256998=CARTESIAN_POINT('Ctrl Pts',(0.686341947289151,-3.87437132388793,
13.0682549610434));
#256999=CARTESIAN_POINT('Ctrl Pts',(0.800015341973993,-3.85251526889571,
13.0741309035213));
#257000=CARTESIAN_POINT('Ctrl Pts',(0.912653620815972,-3.82564404622431,
13.0800068459993));
#257001=CARTESIAN_POINT('Ctrl Pts',(1.02514735418691,-3.79880730662188,
13.085875248049));
#257002=CARTESIAN_POINT('Ctrl Pts',(1.13660821551571,-3.76696829332194,
13.0917436500986));
#257003=CARTESIAN_POINT('Ctrl Pts',(1.2465595104342,-3.73022497806044,13.0976120521482));
#257004=CARTESIAN_POINT('Ctrl Pts',(1.35639900922763,-3.69351902261604,
13.1034744873321));
#257005=CARTESIAN_POINT('Ctrl Pts',(1.46473160552755,-3.65191881426347,
13.1093369225161));
#257006=CARTESIAN_POINT('Ctrl Pts',(1.57109304048681,-3.60557286129873,
13.1151993577));
#257007=CARTESIAN_POINT('Ctrl Pts',(1.68077768342519,-3.5577788530238,13.1212449616367));
#257008=CARTESIAN_POINT('Ctrl Pts',(1.78836552977401,-3.50493777221692,
13.1272905655733));
#257009=CARTESIAN_POINT('Ctrl Pts',(1.89336641132977,-3.44726741527956,
13.13333616951));
#257010=CARTESIAN_POINT('Ctrl Pts',(1.99507040906837,-3.39140782853479,
13.1391919497663));
#257011=CARTESIAN_POINT('Ctrl Pts',(2.0943470789089,-3.3310179099754,13.1450477300225));
#257012=CARTESIAN_POINT('Ctrl Pts',(2.19077414959522,-3.26634315794672,
13.1509035102788));
#257013=CARTESIAN_POINT('Ctrl Pts',(2.28718707115254,-3.20167789590257,
13.156758431293));
#257014=CARTESIAN_POINT('Ctrl Pts',(2.38075088229321,-3.13272928045617,
13.1626133523072));
#257015=CARTESIAN_POINT('Ctrl Pts',(2.47107174780495,-3.05978649863029,
13.1684682733215));
#257016=CARTESIAN_POINT('Ctrl Pts',(2.5614011533005,-2.9868368199465,13.1743237479279));
#257017=CARTESIAN_POINT('Ctrl Pts',(2.64848668249115,-2.90989248348584,
13.1801792225344));
#257018=CARTESIAN_POINT('Ctrl Pts',(2.7319676400229,-2.82928291513374,13.1860346971409));
#257019=CARTESIAN_POINT('Ctrl Pts',(2.81547663348299,-2.74864627516978,
13.1918921382278));
#257020=CARTESIAN_POINT('Ctrl Pts',(2.89537835137074,-2.66434224220679,
13.1977495793147));
#257021=CARTESIAN_POINT('Ctrl Pts',(2.97134951437397,-2.57673651416469,
13.2036070204015));
#257022=CARTESIAN_POINT('Ctrl Pts',(3.04740630844109,-2.48903204113306,
13.2094710637161));
#257023=CARTESIAN_POINT('Ctrl Pts',(3.11952343460079,-2.3980187572808,13.2153351070306));
#257024=CARTESIAN_POINT('Ctrl Pts',(3.18741836746576,-2.30409486582951,
13.2211991503451));
#257025=CARTESIAN_POINT('Ctrl Pts',(3.25535917648669,-2.21010751062753,
13.2270671559548));
#257026=CARTESIAN_POINT('Ctrl Pts',(3.31907188514095,-2.11320597567742,
13.2329351615645));
#257027=CARTESIAN_POINT('Ctrl Pts',(3.37831862924121,-2.0138153438987,13.2388031671742));
#257028=CARTESIAN_POINT('Ctrl Pts',(3.43765090671206,-1.91428122380055,
13.2446796443093));
#257029=CARTESIAN_POINT('Ctrl Pts',(3.49250415812827,-1.81225119767171,
13.2505561214444));
#257030=CARTESIAN_POINT('Ctrl Pts',(3.54268752832076,-1.70817273034097,
13.2564325985795));
#257031=CARTESIAN_POINT('Ctrl Pts',(3.55367884814176,-1.6853771365711,13.257719683113));
#257032=CARTESIAN_POINT('Ctrl Pts',(3.56444633586689,-1.66248334210052,
13.2590067676465));
#257033=CARTESIAN_POINT('Ctrl Pts',(3.57498830358303,-1.63949615103072,
13.26029385218));
#257034=CARTESIAN_POINT('Ctrl Pts',(3.62311567540152,-1.53455245157456,
13.266169794658));
#257035=CARTESIAN_POINT('Ctrl Pts',(3.66669760141889,-1.42731466194993,
13.272045737136));
#257036=CARTESIAN_POINT('Ctrl Pts',(3.70550970658548,-1.31821349348304,
13.277921679614));
#257037=CARTESIAN_POINT('Ctrl Pts',(3.74427200529127,-1.20925233141488,
13.2837900816636));
#257038=CARTESIAN_POINT('Ctrl Pts',(3.77827651896329,-1.09843293137146,
13.2896584837132));
#257039=CARTESIAN_POINT('Ctrl Pts',(3.80734578307702,-0.986208440485887,
13.2955268857628));
#257040=CARTESIAN_POINT('Ctrl Pts',(3.83638549018477,-0.874098057062291,
13.3013893209467));
#257041=CARTESIAN_POINT('Ctrl Pts',(3.86049982642276,-0.76058582184569,
13.3072517561307));
#257042=CARTESIAN_POINT('Ctrl Pts',(3.87956048350467,-0.64614197729991,
13.3131141913146));
#257043=CARTESIAN_POINT('Ctrl Pts',(3.89921668095069,-0.528122394071141,
13.3191597952513));
#257044=CARTESIAN_POINT('Ctrl Pts',(3.91349805906358,-0.40911245019233,
13.325205399188));
#257045=CARTESIAN_POINT('Ctrl Pts',(3.92232030765702,-0.289641854954211,
13.3312510031246));
#257046=CARTESIAN_POINT('Ctrl Pts',(3.93086554973213,-0.173922472718091,
13.3371067833809));
#257047=CARTESIAN_POINT('Ctrl Pts',(3.9342893223048,-0.0577713762121623,
13.3429625636371));
#257048=CARTESIAN_POINT('Ctrl Pts',(3.93256752770725,0.058323580329461,
13.3488183438933));
#257049=CARTESIAN_POINT('Ctrl Pts',(3.9308459857555,0.174401501794627,13.3546732649075));
#257050=CARTESIAN_POINT('Ctrl Pts',(3.92398038410408,0.290422887069137,
13.3605281859218));
#257051=CARTESIAN_POINT('Ctrl Pts',(3.91199875287312,0.405899935352512,
13.366383106936));
#257052=CARTESIAN_POINT('Ctrl Pts',(3.90001598875952,0.521387902177801,
13.3722385815425));
#257053=CARTESIAN_POINT('Ctrl Pts',(3.88291627605861,0.636331019124076,
13.3780940561489));
#257054=CARTESIAN_POINT('Ctrl Pts',(3.86077944135489,0.750247362682064,
13.3839495307554));
#257055=CARTESIAN_POINT('Ctrl Pts',(3.83863517230056,0.86420196347287,13.3898069718423));
#257056=CARTESIAN_POINT('Ctrl Pts',(3.81145049611926,0.977128700236576,
13.3956644129291));
#257057=CARTESIAN_POINT('Ctrl Pts',(3.77935603802724,1.08855727356306,13.401521854016));
#257058=CARTESIAN_POINT('Ctrl Pts',(3.74722540459602,1.20011144385162,13.4073858973305));
#257059=CARTESIAN_POINT('Ctrl Pts',(3.71017405814841,1.31016368349018,13.413249940645));
#257060=CARTESIAN_POINT('Ctrl Pts',(3.66838208147061,1.41826016807402,13.4191139839595));
#257061=CARTESIAN_POINT('Ctrl Pts',(3.62656186623101,1.52642969273642,13.4249819895692));
#257062=CARTESIAN_POINT('Ctrl Pts',(3.57999480765519,1.6326404538458,13.4308499951789));
#257063=CARTESIAN_POINT('Ctrl Pts',(3.52890785618393,1.73646144286688,13.4367180007887));
#257064=CARTESIAN_POINT('Ctrl Pts',(3.4777471514762,1.84043231622699,13.4425944779238));
#257065=CARTESIAN_POINT('Ctrl Pts',(3.42205372932586,1.94200617187811,13.4484709550589));
#257066=CARTESIAN_POINT('Ctrl Pts',(3.36209891441958,2.04077923589463,13.4543474321939));
#257067=CARTESIAN_POINT('Ctrl Pts',(3.34896742199554,2.06241282351991,13.4556345167275));
#257068=CARTESIAN_POINT('Ctrl Pts',(3.33563166260049,2.08391217557118,13.4569216012611));
#257069=CARTESIAN_POINT('Ctrl Pts',(3.32209474595243,2.10527325991551,13.4582086857947));
#257070=CARTESIAN_POINT('Ctrl Pts',(3.26029449781206,2.20279327480133,13.4640846282726));
#257071=CARTESIAN_POINT('Ctrl Pts',(3.19409461294023,2.29775064966901,13.4699605707506));
#257072=CARTESIAN_POINT('Ctrl Pts',(3.1237341089437,2.38972262336483,13.4758365132285));
#257073=CARTESIAN_POINT('Ctrl Pts',(3.05346389656304,2.48157657206584,13.4817049152781));
#257074=CARTESIAN_POINT('Ctrl Pts',(2.97904393179451,2.57045241366354,13.4875733173277));
#257075=CARTESIAN_POINT('Ctrl Pts',(2.90075759804885,2.65595450965597,13.4934417193773));
#257076=CARTESIAN_POINT('Ctrl Pts',(2.82255086417264,2.74136966894625,13.4993041545612));
#257077=CARTESIAN_POINT('Ctrl Pts',(2.74048585819392,2.82341760340935,13.5051665897451));
#257078=CARTESIAN_POINT('Ctrl Pts',(2.65488707357435,2.90173458927033,13.511029024929));
#257079=CARTESIAN_POINT('Ctrl Pts',(2.56661379923745,2.98249854881566,13.5170746288656));
#257080=CARTESIAN_POINT('Ctrl Pts',(2.47458256559311,3.05929422927242,13.5231202328023));
#257081=CARTESIAN_POINT('Ctrl Pts',(2.37919170230479,3.13176241814158,13.529165836739));
#257082=CARTESIAN_POINT('Ctrl Pts',(2.28679598142782,3.2019552051696,13.5350216169952));
#257083=CARTESIAN_POINT('Ctrl Pts',(2.19124880488206,3.26808792394175,13.5408773972514));
#257084=CARTESIAN_POINT('Ctrl Pts',(2.09294619449014,3.32987465634508,13.5467331775076));
#257085=CARTESIAN_POINT('Ctrl Pts',(1.99465800843295,3.39165232253433,13.5525880985218));
#257086=CARTESIAN_POINT('Ctrl Pts',(1.89361554186998,3.449085050815,13.558443019536));
#257087=CARTESIAN_POINT('Ctrl Pts',(1.79024316304185,3.50193066995649,13.5642979405501));
#257088=CARTESIAN_POINT('Ctrl Pts',(1.68686101018808,3.55478128573676,13.5701534151566));
#257089=CARTESIAN_POINT('Ctrl Pts',(1.58114887467595,3.60304374229499,13.576008889763));
#257090=CARTESIAN_POINT('Ctrl Pts',(1.47355440644105,3.64652250935849,13.5818643643694));
#257091=CARTESIAN_POINT('Ctrl Pts',(1.36592380408785,3.69001587816629,13.5877218054563));
#257092=CARTESIAN_POINT('Ctrl Pts',(1.25640999446082,3.72872220834599,13.5935792465431));
#257093=CARTESIAN_POINT('Ctrl Pts',(1.14547854607439,3.76249490371526,13.5994366876299));
#257094=CARTESIAN_POINT('Ctrl Pts',(1.03442206106119,3.79630566605262,13.6053007309444));
#257095=CARTESIAN_POINT('Ctrl Pts',(0.921945143128858,3.82517157423755,
13.6111647742588));
#257096=CARTESIAN_POINT('Ctrl Pts',(0.808526480677646,3.84899648350619,
13.6170288175733));
#257097=CARTESIAN_POINT('Ctrl Pts',(0.695031181987774,3.87283749110815,
13.622896823183));
#257098=CARTESIAN_POINT('Ctrl Pts',(0.580593277954821,3.89163065050699,
13.6287648287926));
#257099=CARTESIAN_POINT('Ctrl Pts',(0.465697848411778,3.90533154981554,
13.6346328344023));
#257100=CARTESIAN_POINT('Ctrl Pts',(0.350636546575094,3.91905222884555,
13.6405093115374));
#257101=CARTESIAN_POINT('Ctrl Pts',(0.23511681103267,3.92766594597547,13.6463857886725));
#257102=CARTESIAN_POINT('Ctrl Pts',(0.119625049177905,3.93118033771146,
13.6522622658075));
#257103=CARTESIAN_POINT('Ctrl Pts',(0.0943296796800673,3.93195007086034,
13.6535493503414));
#257104=CARTESIAN_POINT('Ctrl Pts',(0.0690356355892736,3.93247538136678,
13.6548364348754));
#257105=CARTESIAN_POINT('Ctrl Pts',(0.0437479922143117,3.93275668115601,
13.6561235194093));
#257106=CARTESIAN_POINT('Ctrl Pts',(-0.071697989741531,3.93404090246163,
13.6619994618873));
#257107=CARTESIAN_POINT('Ctrl Pts',(-0.187391021699671,3.93023956642023,
13.6678754043654));
#257108=CARTESIAN_POINT('Ctrl Pts',(-0.302846368279034,3.92132287337069,
13.6737513468435));
#257109=CARTESIAN_POINT('Ctrl Pts',(-0.418153554325276,3.91241762285748,
13.6796197488932));
#257110=CARTESIAN_POINT('Ctrl Pts',(-0.533223253743708,3.89841010158475,
13.6854881509429));
#257111=CARTESIAN_POINT('Ctrl Pts',(-0.647569314295453,3.87932249022725,
13.6913565529926));
#257112=CARTESIAN_POINT('Ctrl Pts',(-0.76179911021818,3.86025428674477,
13.6972189881766));
#257113=CARTESIAN_POINT('Ctrl Pts',(-0.875306326089624,3.83611633526808,
13.7030814233607));
#257114=CARTESIAN_POINT('Ctrl Pts',(-0.987609184996774,3.8069826763081,
13.7089438585447));
#257115=CARTESIAN_POINT('Ctrl Pts',(-1.1034208885967,3.77693875125501,13.7149894624813));
#257116=CARTESIAN_POINT('Ctrl Pts',(-1.2179512936038,3.74158184483587,13.7210350664179));
#257117=CARTESIAN_POINT('Ctrl Pts',(-1.3306821919086,3.70105037849221,13.7270806703546));
#257118=CARTESIAN_POINT('Ctrl Pts',(-1.43987349446358,3.66179154465801,
13.7329364506109));
#257119=CARTESIAN_POINT('Ctrl Pts',(-1.54737618777003,3.61767839049213,
13.7387922308672));
#257120=CARTESIAN_POINT('Ctrl Pts',(-1.65273479015303,3.5688873214796,13.7446480111236));
#257121=CARTESIAN_POINT('Ctrl Pts',(-1.75807793284761,3.52010341177544,
13.7505029321379));
#257122=CARTESIAN_POINT('Ctrl Pts',(-1.86127723576311,3.46664312553191,
13.7563578531522));
#257123=CARTESIAN_POINT('Ctrl Pts',(-1.96189846744296,3.40873046799611,
13.7622127741665));
#257124=CARTESIAN_POINT('Ctrl Pts',(-2.06252921302292,3.35081233472491,
13.7680682487731));
#257125=CARTESIAN_POINT('Ctrl Pts',(-2.16058104503836,3.28844119920087,
13.7739237233797));
#257126=CARTESIAN_POINT('Ctrl Pts',(-2.25564616789749,3.22188599507328,
13.7797791979862));
#257127=CARTESIAN_POINT('Ctrl Pts',(-2.35074321706692,3.15530843929838,
13.7856366390732));
#257128=CARTESIAN_POINT('Ctrl Pts',(-2.44285122459867,3.08454425736946,
13.7914940801601));
#257129=CARTESIAN_POINT('Ctrl Pts',(-2.53159367494086,3.00990406242449,
13.7973515212471));
#257130=CARTESIAN_POINT('Ctrl Pts',(-2.62043615153184,2.93517973661902,
13.8032155645617));
#257131=CARTESIAN_POINT('Ctrl Pts',(-2.70590518348767,2.85657094385367,
13.8090796078763));
#257132=CARTESIAN_POINT('Ctrl Pts',(-2.78765942141966,2.77442677866442,
13.8149436511909));
#257133=CARTESIAN_POINT('Ctrl Pts',(-2.86946890014818,2.69222710920737,
13.8208116568007));
#257134=CARTESIAN_POINT('Ctrl Pts',(-2.94755830943711,2.60648761494094,
13.8266796624105));
#257135=CARTESIAN_POINT('Ctrl Pts',(-3.02162620540612,2.51759092681933,
13.8325476680203));
#257136=CARTESIAN_POINT('Ctrl Pts',(-3.09580103175368,2.42856590028081,
13.8384241451554));
#257137=CARTESIAN_POINT('Ctrl Pts',(-3.16594250952575,2.3363749109216,13.8443006222906));
#257138=CARTESIAN_POINT('Ctrl Pts',(-3.2317921229849,2.241430051064,13.8501770994258));
#257139=CARTESIAN_POINT('Ctrl Pts',(-3.24621471274706,2.22063492878737,
13.8514641839585));
#257140=CARTESIAN_POINT('Ctrl Pts',(-3.26043159178119,2.19970779408334,
13.8527512684912));
#257141=CARTESIAN_POINT('Ctrl Pts',(-3.27444034130428,2.17865312779228,
13.8540383530239));
#257142=CARTESIAN_POINT('Ctrl Pts',(-3.33950682555402,2.080860451126,13.8600164787186));
#257143=CARTESIAN_POINT('Ctrl Pts',(-3.40028894269776,1.98000000849237,
13.8659946044133));
#257144=CARTESIAN_POINT('Ctrl Pts',(-3.45649071384092,1.87647567134015,
13.871972730108));
#257145=CARTESIAN_POINT('Ctrl Pts',(-3.51261348722497,1.7730968490086,13.8779424528908));
#257146=CARTESIAN_POINT('Ctrl Pts',(-3.56416853833148,1.66706192514992,
13.8839121756736));
#257147=CARTESIAN_POINT('Ctrl Pts',(-3.61090274354847,1.55880414954353,
13.8898818984564));
#257148=CARTESIAN_POINT('Ctrl Pts',(-3.65758107040856,1.45067581374669,
13.8958444834629));
#257149=CARTESIAN_POINT('Ctrl Pts',(-3.69944986724521,1.34033027461661,
13.9018070684694));
#257150=CARTESIAN_POINT('Ctrl Pts',(-3.7363018239388,1.22822541922549,13.9077696534759));
#257151=CARTESIAN_POINT('Ctrl Pts',(-3.77311019821721,1.11625314296421,
13.9137251869205));
#257152=CARTESIAN_POINT('Ctrl Pts',(-3.80491342872528,1.00252606756105,
13.9196807203651));
#257153=CARTESIAN_POINT('Ctrl Pts',(-3.8315525277421,0.887521395321316,
13.9256362538097));
#257154=CARTESIAN_POINT('Ctrl Pts',(-3.85817311045603,0.772596660520337,
13.9315876476825));
#257155=CARTESIAN_POINT('Ctrl Pts',(-3.87963661635611,0.656396478575151,
13.9375390415554));
#257156=CARTESIAN_POINT('Ctrl Pts',(-3.89583407870534,0.539412487061738,
13.9434904354282));
#257157=CARTESIAN_POINT('Ctrl Pts',(-3.91202327786513,0.422488175321747,
13.9494387931776));
#257158=CARTESIAN_POINT('Ctrl Pts',(-3.92295172834644,0.30478123960899,
13.9553871509271));
#257159=CARTESIAN_POINT('Ctrl Pts',(-3.9285617780135,0.18679228124146,13.9613355086765));
#257160=CARTESIAN_POINT('Ctrl Pts',(-3.93154864777034,0.123973291695202,
13.9645024984393));
#257161=CARTESIAN_POINT('Ctrl Pts',(-3.93302881188282,0.0610744882110394,
13.9676694882022));
#257162=CARTESIAN_POINT('Ctrl Pts',(-3.93299957517034,-0.00182803443963738,
13.970836477965));
#257163=CARTESIAN_POINT('',(-3.93299944805027,-0.00208365934259914,15.2208364779214));
#257164=CARTESIAN_POINT('Ctrl Pts',(-3.93299957516998,-0.00182803520836979,
13.9708364780037));
#257165=CARTESIAN_POINT('Ctrl Pts',(-3.93294033855577,-0.129275021723806,
13.9772531252953));
#257166=CARTESIAN_POINT('Ctrl Pts',(-3.92668218850876,-0.256517553615144,
13.9836697725869));
#257167=CARTESIAN_POINT('Ctrl Pts',(-3.91430926981101,-0.382977728166544,
13.9900864198786));
#257168=CARTESIAN_POINT('Ctrl Pts',(-3.90187435879248,-0.510071509055871,
13.9965352166465));
#257169=CARTESIAN_POINT('Ctrl Pts',(-3.88326334398951,-0.636374811774402,
14.0029840134145));
#257170=CARTESIAN_POINT('Ctrl Pts',(-3.85861196357145,-0.76131643525099,
14.0094328101825));
#257171=CARTESIAN_POINT('Ctrl Pts',(-3.83389603093612,-0.886585231433034,
14.0158984937991));
#257172=CARTESIAN_POINT('Ctrl Pts',(-3.80310818328694,-1.01048496215025,
14.0223641774157));
#257173=CARTESIAN_POINT('Ctrl Pts',(-3.76643400785372,-1.13245921095772,
14.0288298610324));
#257174=CARTESIAN_POINT('Ctrl Pts',(-3.72963590519998,-1.25484562798578,
14.0353173931075));
#257175=CARTESIAN_POINT('Ctrl Pts',(-3.68691176032944,-1.37529328987783,
14.0418049251826));
#257176=CARTESIAN_POINT('Ctrl Pts',(-3.63849613831945,-1.49326315545334,
14.0482924572577));
#257177=CARTESIAN_POINT('Ctrl Pts',(-3.62938961995291,-1.51545216600326,
14.0495127003846));
#257178=CARTESIAN_POINT('Ctrl Pts',(-3.62008187839841,-1.53755358814958,
14.0507329435116));
#257179=CARTESIAN_POINT('Ctrl Pts',(-3.61057465360002,-1.55956393609915,
14.0519531866386));
#257180=CARTESIAN_POINT('Ctrl Pts',(-3.56479369011491,-1.66555227203757,
14.0578291291163));
#257181=CARTESIAN_POINT('Ctrl Pts',(-3.51426632056984,-1.76969790432598,
14.0637050715941));
#257182=CARTESIAN_POINT('Ctrl Pts',(-3.45916247287764,-1.87154588141329,
14.0695810140719));
#257183=CARTESIAN_POINT('Ctrl Pts',(-3.40412933837196,-1.97326315991416,
14.0754494161213));
#257184=CARTESIAN_POINT('Ctrl Pts',(-3.34453159986428,-2.07268828721999,
14.0813178181706));
#257185=CARTESIAN_POINT('Ctrl Pts',(-3.28058724832085,-2.16938615883724,
14.08718622022));
#257186=CARTESIAN_POINT('Ctrl Pts',(-3.21670791402643,-2.26598571012682,
14.0930486554037));
#257187=CARTESIAN_POINT('Ctrl Pts',(-3.14849098410243,-2.35986317934484,
14.0989110905874));
#257188=CARTESIAN_POINT('Ctrl Pts',(-3.07620004668988,-2.45060855151229,
14.1047735257711));
#257189=CARTESIAN_POINT('Ctrl Pts',(-3.00165041635399,-2.54418921586542,
14.1108191297079));
#257190=CARTESIAN_POINT('Ctrl Pts',(-2.92276822572093,-2.63443845134279,
14.1168647336446));
#257191=CARTESIAN_POINT('Ctrl Pts',(-2.83989069561032,-2.72093914613796,
14.1229103375814));
#257192=CARTESIAN_POINT('Ctrl Pts',(-2.7596154063976,-2.8047238376281,14.1287661178374));
#257193=CARTESIAN_POINT('Ctrl Pts',(-2.67559222934242,-2.88499154691874,
14.1346218980934));
#257194=CARTESIAN_POINT('Ctrl Pts',(-2.58816757361598,-2.96139791498589,
14.1404776783494));
#257195=CARTESIAN_POINT('Ctrl Pts',(-2.5007557460584,-3.03779307164153,
14.1463325993634));
#257196=CARTESIAN_POINT('Ctrl Pts',(-2.40994374300934,-3.11032774216744,
14.1521875203774));
#257197=CARTESIAN_POINT('Ctrl Pts',(-2.31611281565845,-3.17869634050544,
14.1580424413914));
#257198=CARTESIAN_POINT('Ctrl Pts',(-2.22227301644156,-3.24707140320504,
14.1638979159976));
#257199=CARTESIAN_POINT('Ctrl Pts',(-2.12541405909878,-3.31127936758053,
14.1697533906038));
#257200=CARTESIAN_POINT('Ctrl Pts',(-2.02594748730443,-3.37105707140726,
14.1756088652101));
#257201=CARTESIAN_POINT('Ctrl Pts',(-1.92644751103389,-3.43085485075129,
14.1814663062967));
#257202=CARTESIAN_POINT('Ctrl Pts',(-1.82433853252037,-3.48621919849487,
14.1873237473833));
#257203=CARTESIAN_POINT('Ctrl Pts',(-1.72005744964628,-3.53693248025974,
14.1931811884699));
#257204=CARTESIAN_POINT('Ctrl Pts',(-1.61565882611948,-3.58770292361208,
14.1990452317842));
#257205=CARTESIAN_POINT('Ctrl Pts',(-1.50908358308714,-3.63381165700011,
14.2049092750985));
#257206=CARTESIAN_POINT('Ctrl Pts',(-1.40078947045128,-3.67508882334466,
14.2107733184127));
#257207=CARTESIAN_POINT('Ctrl Pts',(-1.29242218420112,-3.71639388039698,
14.2166413240222));
#257208=CARTESIAN_POINT('Ctrl Pts',(-1.18233410647362,-3.75286074016077,
14.2225093296317));
#257209=CARTESIAN_POINT('Ctrl Pts',(-1.07099739410399,-3.78436964127746,
14.2283773352412));
#257210=CARTESIAN_POINT('Ctrl Pts',(-0.959499947091306,-3.81592403118095,
14.234253812376));
#257211=CARTESIAN_POINT('Ctrl Pts',(-0.846750668155043,-3.84250608379267,
14.2401302895109));
#257212=CARTESIAN_POINT('Ctrl Pts',(-0.733231168924177,-3.8640472374077,
14.2460067666458));
#257213=CARTESIAN_POINT('Ctrl Pts',(-0.708367770562164,-3.86876524873735,
14.2472938511816));
#257214=CARTESIAN_POINT('Ctrl Pts',(-0.683467438484994,-3.87324164035368,
14.2485809357174));
#257215=CARTESIAN_POINT('Ctrl Pts',(-0.658535249944616,-3.87747602501684,
14.2498680202532));
#257216=CARTESIAN_POINT('Ctrl Pts',(-0.544712030366906,-3.89680731214034,
14.2557439627319));
#257217=CARTESIAN_POINT('Ctrl Pts',(-0.429849108164953,-3.91115432943795,
14.2616199052106));
#257218=CARTESIAN_POINT('Ctrl Pts',(-0.314420586219157,-3.92041180170675,
14.2674958476893));
#257219=CARTESIAN_POINT('Ctrl Pts',(-0.199140190383127,-3.92965739412706,
14.2733642497396));
#257220=CARTESIAN_POINT('Ctrl Pts',(-0.0832960459976697,-3.93382639769409,
14.2792326517899));
#257221=CARTESIAN_POINT('Ctrl Pts',(0.032628211713834,-3.93286465566772,
14.2851010538403));
#257222=CARTESIAN_POINT('Ctrl Pts',(0.148434600119379,-3.93190389152007,
14.2909634890249));
#257223=CARTESIAN_POINT('Ctrl Pts',(0.264320529484257,-3.92582276216068,
14.2968259242096));
#257224=CARTESIAN_POINT('Ctrl Pts',(0.379798571942981,-3.91461901655194,
14.3026883593942));
#257225=CARTESIAN_POINT('Ctrl Pts',(0.498884666043312,-3.903065215713,14.3087339633306));
#257226=CARTESIAN_POINT('Ctrl Pts',(0.617536520453047,-3.88606339386041,
14.314779567267));
#257227=CARTESIAN_POINT('Ctrl Pts',(0.735220651642348,-3.86366918788327,
14.3208251712034));
#257228=CARTESIAN_POINT('Ctrl Pts',(0.849209662372347,-3.84197812928752,
14.3266809514604));
#257229=CARTESIAN_POINT('Ctrl Pts',(0.962290376271785,-3.81522833330441,
14.3325367317173));
#257230=CARTESIAN_POINT('Ctrl Pts',(1.07398532065683,-3.78352276734443,
14.3383925119743));
#257231=CARTESIAN_POINT('Ctrl Pts',(1.18566387559669,-3.75182185366874,
14.3442474329892));
#257232=CARTESIAN_POINT('Ctrl Pts',(1.29595666838717,-3.71516672867222,
14.3501023540042));
#257233=CARTESIAN_POINT('Ctrl Pts',(1.40439976730262,-3.6737106981362,14.3559572750191));
#257234=CARTESIAN_POINT('Ctrl Pts',(1.51285311968827,-3.63225074786552,
14.3618127496263));
#257235=CARTESIAN_POINT('Ctrl Pts',(1.61945604496533,-3.58598913707341,
14.3676682242335));
#257236=CARTESIAN_POINT('Ctrl Pts',(1.72376369211206,-3.53512768280811,
14.3735236988406));
#257237=CARTESIAN_POINT('Ctrl Pts',(1.82810636954325,-3.48424914742497,
14.3793811399282));
#257238=CARTESIAN_POINT('Ctrl Pts',(1.93015186524843,-3.42876787757276,
14.3852385810157));
#257239=CARTESIAN_POINT('Ctrl Pts',(2.02947970175482,-3.36893175059471,
14.3910960221033));
#257240=CARTESIAN_POINT('Ctrl Pts',(2.12891949585127,-3.30902817919414,
14.3969600654185));
#257241=CARTESIAN_POINT('Ctrl Pts',(2.22563516316399,-3.24476016675888,
14.4028241087337));
#257242=CARTESIAN_POINT('Ctrl Pts',(2.31923493841007,-3.17641910025394,
14.4086881520489));
#257243=CARTESIAN_POINT('Ctrl Pts',(2.41289795840394,-3.10803185614329,
14.4145561576593));
#257244=CARTESIAN_POINT('Ctrl Pts',(2.50344057251542,-3.03556633501209,
14.4204241632697));
#257245=CARTESIAN_POINT('Ctrl Pts',(2.59050518232709,-2.95935329089591,
14.4262921688801));
#257246=CARTESIAN_POINT('Ctrl Pts',(2.67769548561984,-2.88303021949265,
14.4321686460159));
#257247=CARTESIAN_POINT('Ctrl Pts',(2.76139746712784,-2.80294911237236,
14.4380451231517));
#257248=CARTESIAN_POINT('Ctrl Pts',(2.84129131829658,-2.71947653870602,
14.4439216002875));
#257249=CARTESIAN_POINT('Ctrl Pts',(2.85878992115806,-2.70119411277405,
14.4452086848142));
#257250=CARTESIAN_POINT('Ctrl Pts',(2.87610600172078,-2.68274911441523,
14.446495769341));
#257251=CARTESIAN_POINT('Ctrl Pts',(2.89323646991126,-2.66414559083684,
14.4477828538678));
#257252=CARTESIAN_POINT('Ctrl Pts',(2.97144240246882,-2.57921470079195,
14.4536587963451));
#257253=CARTESIAN_POINT('Ctrl Pts',(3.04603447030337,-2.49069718155165,
14.4595347388224));
#257254=CARTESIAN_POINT('Ctrl Pts',(3.11666616413018,-2.39893330907011,
14.4654106812997));
#257255=CARTESIAN_POINT('Ctrl Pts',(3.1872072183312,-2.30728719453281,14.4712790833487));
#257256=CARTESIAN_POINT('Ctrl Pts',(3.25379775617551,-2.21240333582628,
14.4771474853976));
#257257=CARTESIAN_POINT('Ctrl Pts',(3.31612894791232,-2.11465784485764,
14.4830158874466));
#257258=CARTESIAN_POINT('Ctrl Pts',(3.37839676262653,-2.0170117394136,14.4888783226298));
#257259=CARTESIAN_POINT('Ctrl Pts',(3.43641362516404,-1.91651013537292,
14.4947407578131));
#257260=CARTESIAN_POINT('Ctrl Pts',(3.48991217164834,-1.81356059567381,
14.5006031929963));
#257261=CARTESIAN_POINT('Ctrl Pts',(3.54508225253357,-1.70739445088026,
14.5066487969333));
#257262=CARTESIAN_POINT('Ctrl Pts',(3.59544675863839,-1.59862524094772,
14.5126944008702));
#257263=CARTESIAN_POINT('Ctrl Pts',(3.64076179062746,-1.48773068258577,
14.5187400048071));
#257264=CARTESIAN_POINT('Ctrl Pts',(3.68465399269227,-1.38031806143427,
14.5245957850627));
#257265=CARTESIAN_POINT('Ctrl Pts',(3.7238089050595,-1.27091197260396,14.5304515653183));
#257266=CARTESIAN_POINT('Ctrl Pts',(3.75805282899773,-1.15996893685224,
14.5363073455739));
#257267=CARTESIAN_POINT('Ctrl Pts',(3.79229172818833,-1.04904218021499,
14.5421622665874));
#257268=CARTESIAN_POINT('Ctrl Pts',(3.82162095015235,-0.936579319396514,
14.548017187601));
#257269=CARTESIAN_POINT('Ctrl Pts',(3.84591638825488,-0.823052935449811,
14.5538721086146));
#257270=CARTESIAN_POINT('Ctrl Pts',(3.87021412353039,-0.709515817399792,
14.5597275832204));
#257271=CARTESIAN_POINT('Ctrl Pts',(3.88947704241376,-0.594915379960817,
14.5655830578263));
#257272=CARTESIAN_POINT('Ctrl Pts',(3.90363211524196,-0.479734623361267,
14.5714385324321));
#257273=CARTESIAN_POINT('Ctrl Pts',(3.91779194185614,-0.364515184893195,
14.5772959735183));
#257274=CARTESIAN_POINT('Ctrl Pts',(3.92684046104926,-0.248715449173139,
14.5831534146045));
#257275=CARTESIAN_POINT('Ctrl Pts',(3.93075654731549,-0.1328230617642,14.5890108556908));
#257276=CARTESIAN_POINT('Ctrl Pts',(3.934677047607,-0.0168000459946449,
14.5948748990047));
#257277=CARTESIAN_POINT('Ctrl Pts',(3.93345355472821,0.0993154171680395,
14.6007389423185));
#257278=CARTESIAN_POINT('Ctrl Pts',(3.92711707119533,0.215036064710605,
14.6066029856324));
#257279=CARTESIAN_POINT('Ctrl Pts',(3.92077630614251,0.330834903928005,
14.6124709912415));
#257280=CARTESIAN_POINT('Ctrl Pts',(3.90931571169151,0.446237986606797,
14.6183389968506));
#257281=CARTESIAN_POINT('Ctrl Pts',(3.89281791503712,0.56076526315925,14.6242070024597));
#257282=CARTESIAN_POINT('Ctrl Pts',(3.87629630083501,0.675457880510334,
14.6300834795943));
#257283=CARTESIAN_POINT('Ctrl Pts',(3.8547230483785,0.789271764541383,14.6359599567288));
#257284=CARTESIAN_POINT('Ctrl Pts',(3.8282314039091,0.901739052123255,14.6418364338633));
#257285=CARTESIAN_POINT('Ctrl Pts',(3.82242912045815,0.926371991851243,
14.643123518403));
#257286=CARTESIAN_POINT('Ctrl Pts',(3.81639108292966,0.950940400959883,
14.6444106029427));
#257287=CARTESIAN_POINT('Ctrl Pts',(3.8101190025785,0.975439483612509,14.6456976874824));
#257288=CARTESIAN_POINT('Ctrl Pts',(3.7814849989708,1.08728543930576,14.6515736299591));
#257289=CARTESIAN_POINT('Ctrl Pts',(3.74787473329744,1.19805401713487,14.6574495724358));
#257290=CARTESIAN_POINT('Ctrl Pts',(3.70938485811833,1.30726928150343,14.6633255149126));
#257291=CARTESIAN_POINT('Ctrl Pts',(3.6709443758916,1.41634439305701,14.6691939169609));
#257292=CARTESIAN_POINT('Ctrl Pts',(3.62763687322898,1.52386976951915,14.6750623190093));
#257293=CARTESIAN_POINT('Ctrl Pts',(3.57960957910569,1.62938155788469,14.6809307210576));
#257294=CARTESIAN_POINT('Ctrl Pts',(3.53163111810794,1.73478606412035,14.6867931562403));
#257295=CARTESIAN_POINT('Ctrl Pts',(3.4789425814707,1.83818068127895,14.692655591423));
#257296=CARTESIAN_POINT('Ctrl Pts',(3.4217401593197,1.93911920265331,14.6985180266056));
#257297=CARTESIAN_POINT('Ctrl Pts',(3.36275047708099,2.04321149590971,14.7045636305428));
#257298=CARTESIAN_POINT('Ctrl Pts',(3.29896035304039,2.1446912701522,14.7106092344799));
#257299=CARTESIAN_POINT('Ctrl Pts',(3.23063759276133,2.24309378855127,14.716654838417));
#257300=CARTESIAN_POINT('Ctrl Pts',(3.16446007356457,2.33840660266718,14.722510618672));
#257301=CARTESIAN_POINT('Ctrl Pts',(3.09403055220544,2.43083215083332,14.7283663989269));
#257302=CARTESIAN_POINT('Ctrl Pts',(3.01963729246406,2.51997611535513,14.7342221791819));
#257303=CARTESIAN_POINT('Ctrl Pts',(2.94525494874276,2.60910699942705,14.7400771001948));
#257304=CARTESIAN_POINT('Ctrl Pts',(2.86691028755852,2.69495694051926,14.7459320212078));
#257305=CARTESIAN_POINT('Ctrl Pts',(2.78493205208289,2.77716446493206,14.7517869422207));
#257306=CARTESIAN_POINT('Ctrl Pts',(2.70294606543257,2.8593797621992,14.7576424168259));
#257307=CARTESIAN_POINT('Ctrl Pts',(2.6173261129955,2.93795166587313,14.7634978914311));
#257308=CARTESIAN_POINT('Ctrl Pts',(2.52843749505405,3.01255586398075,14.7693533660362));
#257309=CARTESIAN_POINT('Ctrl Pts',(2.43951902509637,3.08718511687923,14.7752108071218));
#257310=CARTESIAN_POINT('Ctrl Pts',(2.34733002278658,3.15784374935065,14.7810682482074));
#257311=CARTESIAN_POINT('Ctrl Pts',(2.25226795372043,3.22424844958387,14.7869256892929));
#257312=CARTESIAN_POINT('Ctrl Pts',(2.15709873523312,3.29072799802166,14.7927897326061));
#257313=CARTESIAN_POINT('Ctrl Pts',(2.05905032507611,3.35294380777436,14.7986537759194));
#257314=CARTESIAN_POINT('Ctrl Pts',(1.95854825937223,3.41065649336165,14.8045178192326));
#257315=CARTESIAN_POINT('Ctrl Pts',(1.85797828508849,3.46840817502819,14.810385824841));
#257316=CARTESIAN_POINT('Ctrl Pts',(1.75495171967396,3.52165048464205,14.8162538304495));
#257317=CARTESIAN_POINT('Ctrl Pts',(1.64991616681404,3.5701912613312,14.8221218360579));
#257318=CARTESIAN_POINT('Ctrl Pts',(1.5447289761722,3.61880211539424,14.8279983131917));
#257319=CARTESIAN_POINT('Ctrl Pts',(1.43752739047302,3.66269773522737,14.8338747903256));
#257320=CARTESIAN_POINT('Ctrl Pts',(1.32877636253884,3.70173504972439,14.8397512674594));
#257321=CARTESIAN_POINT('Ctrl Pts',(1.30495736959239,3.71028512540014,14.8410383520053));
#257322=CARTESIAN_POINT('Ctrl Pts',(1.2810640935575,3.71860233585773,14.8423254365511));
#257323=CARTESIAN_POINT('Ctrl Pts',(1.25710148856665,3.72668550423074,14.843612521097));
#257324=CARTESIAN_POINT('Ctrl Pts',(1.14770472118026,3.76358768955593,14.8494884635801));
#257325=CARTESIAN_POINT('Ctrl Pts',(1.03650120846817,3.7957296649438,14.8553644060631));
#257326=CARTESIAN_POINT('Ctrl Pts',(0.923942742723827,3.82293327278517,
14.8612403485462));
#257327=CARTESIAN_POINT('Ctrl Pts',(0.811528720028424,3.85010197101729,
14.8671087506009));
#257328=CARTESIAN_POINT('Ctrl Pts',(0.697763599842017,3.87234480866924,
14.8729771526556));
#257329=CARTESIAN_POINT('Ctrl Pts',(0.583116587485802,3.88953262557327,
14.8788455547103));
#257330=CARTESIAN_POINT('Ctrl Pts',(0.468586145759477,3.90670296627272,
14.8847079898993));
#257331=CARTESIAN_POINT('Ctrl Pts',(0.35317600131364,3.91882844920775,14.8905704250883));
#257332=CARTESIAN_POINT('Ctrl Pts',(0.237367226659337,3.92583058723986,
14.8964328602773));
#257333=CARTESIAN_POINT('Ctrl Pts',(0.11794006692834,3.93305150344172,14.9024784642121));
#257334=CARTESIAN_POINT('Ctrl Pts',(-0.00191060819045115,3.93482355446359,
14.9085240681468));
#257335=CARTESIAN_POINT('Ctrl Pts',(-0.121649180496793,3.93111822219638,
14.9145696720816));
#257336=CARTESIAN_POINT('Ctrl Pts',(-0.237628125825234,3.9275292322814,
14.9204254523429));
#257337=CARTESIAN_POINT('Ctrl Pts',(-0.353501459878626,3.91880169457394,
14.9262812326042));
#257338=CARTESIAN_POINT('Ctrl Pts',(-0.468781480055529,3.90496260212015,
14.9321370128655));
#257339=CARTESIAN_POINT('Ctrl Pts',(-0.584044584734466,3.89112554033168,
14.9379919338848));
#257340=CARTESIAN_POINT('Ctrl Pts',(-0.698714138941152,3.87217846440888,
14.943846854904));
#257341=CARTESIAN_POINT('Ctrl Pts',(-0.812307938231669,3.84820020444439,
14.9497017759233));
#257342=CARTESIAN_POINT('Ctrl Pts',(-0.925912477999098,3.82421967729674,
14.9555572505348));
#257343=CARTESIAN_POINT('Ctrl Pts',(-1.0384406567731,3.79520710570084,14.9614127251463));
#257344=CARTESIAN_POINT('Ctrl Pts',(-1.14942152565754,3.76129221895283,
14.9672681997578));
#257345=CARTESIAN_POINT('Ctrl Pts',(-1.26043966593545,3.72736594235807,
14.9731256408496));
#257346=CARTESIAN_POINT('Ctrl Pts',(-1.3699090685031,3.68853419738089,14.9789830819414));
#257347=CARTESIAN_POINT('Ctrl Pts',(-1.47737565115394,3.64497601986316,
14.9848405230333));
#257348=CARTESIAN_POINT('Ctrl Pts',(-1.58496336499929,3.60136874565003,
14.9907045663527));
#257349=CARTESIAN_POINT('Ctrl Pts',(-1.69054337051291,3.55302456109311,
14.9965686096721));
#257350=CARTESIAN_POINT('Ctrl Pts',(-1.79368313646694,3.50016996815214,
15.0024326529916));
#257351=CARTESIAN_POINT('Ctrl Pts',(-1.89689259327681,3.44727966171324,
15.0083006586062));
#257352=CARTESIAN_POINT('Ctrl Pts',(-1.99765816949556,3.38987308202568,
15.0141686642208));
#257353=CARTESIAN_POINT('Ctrl Pts',(-2.09557492052084,3.32822095908371,
15.0200366698354));
#257354=CARTESIAN_POINT('Ctrl Pts',(-2.1936330320506,3.26647983017382,15.0259131469753));
#257355=CARTESIAN_POINT('Ctrl Pts',(-2.28883377281264,3.2004811604603,15.0317896241152));
#257356=CARTESIAN_POINT('Ctrl Pts',(-2.38080391894879,3.13053696664296,
15.0376661012551));
#257357=CARTESIAN_POINT('Ctrl Pts',(-2.40094750930153,3.11521756956682,
15.0389531857406));
#257358=CARTESIAN_POINT('Ctrl Pts',(-2.4209362616762,3.09970904455408,15.0402402702261));
#257359=CARTESIAN_POINT('Ctrl Pts',(-2.44076649082374,3.08401490548797,
15.0415273547117));
#257360=CARTESIAN_POINT('Ctrl Pts',(-2.53021382122752,3.01322405218999,
15.0473329493106));
#257361=CARTESIAN_POINT('Ctrl Pts',(-2.6167437016043,2.93840781332431,15.0531385439095));
#257362=CARTESIAN_POINT('Ctrl Pts',(-2.69996564784677,2.85983819480183,
15.0589441385085));
#257363=CARTESIAN_POINT('Ctrl Pts',(-2.78308030073049,2.78136987165451,
15.0647422482819));
#257364=CARTESIAN_POINT('Ctrl Pts',(-2.86289519146216,2.69915807542079,
15.0705403580554));
#257365=CARTESIAN_POINT('Ctrl Pts',(-2.93905099343468,2.61351645450925,
15.0763384678288));
#257366=CARTESIAN_POINT('Ctrl Pts',(-3.01813108930501,2.5245862953256,15.0823592182494));
#257367=CARTESIAN_POINT('Ctrl Pts',(-3.09326507449529,2.43195788925591,
15.0883799686699));
#257368=CARTESIAN_POINT('Ctrl Pts',(-3.16409036142845,2.33602679452005,
15.0944007190904));
#257369=CARTESIAN_POINT('Ctrl Pts',(-3.23217814387143,2.24380358172803,
15.1001887583985));
#257370=CARTESIAN_POINT('Ctrl Pts',(-3.29628383170549,2.14852861894465,
15.1059767977066));
#257371=CARTESIAN_POINT('Ctrl Pts',(-3.35612529732445,2.05058820553003,
15.1117648370147));
#257372=CARTESIAN_POINT('Ctrl Pts',(-3.41594578615709,1.95268212408076,
15.1175508473874));
#257373=CARTESIAN_POINT('Ctrl Pts',(-3.47150480282969,1.85211280996971,
15.1233368577602));
#257374=CARTESIAN_POINT('Ctrl Pts',(-3.52256370317595,1.74929527440833,
15.129122868133));
#257375=CARTESIAN_POINT('Ctrl Pts',(-3.57361774512906,1.64648752221494,
15.1349083279511));
#257376=CARTESIAN_POINT('Ctrl Pts',(-3.620172334303,1.54143235359451,15.1406937877693));
#257377=CARTESIAN_POINT('Ctrl Pts',(-3.66203532518342,1.43456832430831,
15.1464792475874));
#257378=CARTESIAN_POINT('Ctrl Pts',(-3.70390502428713,1.32768717088085,
15.1522656344811));
#257379=CARTESIAN_POINT('Ctrl Pts',(-3.74108147791742,1.21899697566816,
15.1580520213748));
#257380=CARTESIAN_POINT('Ctrl Pts',(-3.77342142421475,1.10895435220624,
15.1638384082686));
#257381=CARTESIAN_POINT('Ctrl Pts',(-3.80579112984675,0.998810467127175,
15.1696301198163));
#257382=CARTESIAN_POINT('Ctrl Pts',(-3.83331532668721,0.887312076957398,
15.175421831364));
#257383=CARTESIAN_POINT('Ctrl Pts',(-3.85590123032483,0.774928836719529,
15.1812135429117));
#257384=CARTESIAN_POINT('Ctrl Pts',(-3.87849950850775,0.662484023054278,
15.1870084276686));
#257385=CARTESIAN_POINT('Ctrl Pts',(-3.89615404312042,0.549153812219911,
15.1928033124255));
#257386=CARTESIAN_POINT('Ctrl Pts',(-3.9088238041303,0.435414134203678,
15.1985981971824));
#257387=CARTESIAN_POINT('Ctrl Pts',(-3.92151034391662,0.321523828829201,
15.2044007562021));
#257388=CARTESIAN_POINT('Ctrl Pts',(-3.92919891029343,0.207223395534366,
15.2102033152218));
#257389=CARTESIAN_POINT('Ctrl Pts',(-3.93190054507825,0.0929898038138043,
15.2160058742415));
#257390=CARTESIAN_POINT('Ctrl Pts',(-3.93265024458662,0.0612901573504407,
15.2176160754681));
#257391=CARTESIAN_POINT('Ctrl Pts',(-3.93301623138631,0.0295956320002337,
15.2192262766947));
#257392=CARTESIAN_POINT('Ctrl Pts',(-3.93299944805027,-0.0020836593426039,
15.2208364779214));
#257393=CARTESIAN_POINT('',(-3.93299842594645,0.00351873595700912,16.4708364780091));
#257394=CARTESIAN_POINT('Ctrl Pts',(-3.93299944804982,-0.00208366020134649,
15.220836477965));
#257395=CARTESIAN_POINT('Ctrl Pts',(-3.93293480477982,-0.124100649844272,
15.2270383814188));
#257396=CARTESIAN_POINT('Ctrl Pts',(-3.92719245864474,-0.2459628104,15.2332402848725));
#257397=CARTESIAN_POINT('Ctrl Pts',(-3.9158126229022,-0.367288037267423,
15.2394421883262));
#257398=CARTESIAN_POINT('Ctrl Pts',(-3.9050308910257,-0.482236626643941,
15.245318130798));
#257399=CARTESIAN_POINT('Ctrl Pts',(-3.88916561621277,-0.596899701881591,
15.2511940732698));
#257400=CARTESIAN_POINT('Ctrl Pts',(-3.868237794927,-0.710792066569598,
15.2570700157417));
#257401=CARTESIAN_POINT('Ctrl Pts',(-3.84733682971402,-0.824538276452734,
15.2629384177851));
#257402=CARTESIAN_POINT('Ctrl Pts',(-3.82138631192933,-0.937515340376091,
15.2688068198285));
#257403=CARTESIAN_POINT('Ctrl Pts',(-3.79045908201708,-1.04924208243579,
15.2746752218719));
#257404=CARTESIAN_POINT('Ctrl Pts',(-3.75956329825118,-1.1608552231322,
15.2805376570495));
#257405=CARTESIAN_POINT('Ctrl Pts',(-3.72370097727427,-1.27122017527289,
15.2864000922272));
#257406=CARTESIAN_POINT('Ctrl Pts',(-3.68299607864721,-1.37986553137226,
15.2922625274048));
#257407=CARTESIAN_POINT('Ctrl Pts',(-3.64101937647165,-1.49190545554763,
15.2983081313438));
#257408=CARTESIAN_POINT('Ctrl Pts',(-3.59389259531413,-1.60211612205712,
15.3043537352828));
#257409=CARTESIAN_POINT('Ctrl Pts',(-3.54180752890365,-1.70999661642982,
15.3103993392218));
#257410=CARTESIAN_POINT('Ctrl Pts',(-3.49135786229038,-1.81448981093368,
15.3162551194716));
#257411=CARTESIAN_POINT('Ctrl Pts',(-3.43625681438112,-1.91679657478375,
15.3221108997215));
#257412=CARTESIAN_POINT('Ctrl Pts',(-3.37672740306017,-2.01648234443611,
15.3279666799713));
#257413=CARTESIAN_POINT('Ctrl Pts',(-3.31720672672778,-2.11615348679687,
15.3338216009791));
#257414=CARTESIAN_POINT('Ctrl Pts',(-3.25325919064256,-2.21320404541458,
15.3396765219869));
#257415=CARTESIAN_POINT('Ctrl Pts',(-3.1851529323662,-2.30722556275692,
15.3455314429947));
#257416=CARTESIAN_POINT('Ctrl Pts',(-3.11704023453342,-2.40125596998517,
15.3513869175948));
#257417=CARTESIAN_POINT('Ctrl Pts',(-3.04476827498617,-2.49225643230999,
15.3572423921948));
#257418=CARTESIAN_POINT('Ctrl Pts',(-2.9686471125496,-2.57984947645224,
15.3630978667948));
#257419=CARTESIAN_POINT('Ctrl Pts',(-2.8925003858707,-2.66747193751004,
15.3689553078752));
#257420=CARTESIAN_POINT('Ctrl Pts',(-2.81250215638256,-2.7516843935142,
15.3748127489556));
#257421=CARTESIAN_POINT('Ctrl Pts',(-2.72900066703397,-2.83214483374847,
15.380670190036));
#257422=CARTESIAN_POINT('Ctrl Pts',(-2.64540505879733,-2.91269596514558,
15.386534233344));
#257423=CARTESIAN_POINT('Ctrl Pts',(-2.55829860688726,-2.98948635341672,
15.392398276652));
#257424=CARTESIAN_POINT('Ctrl Pts',(-2.46806415185481,-3.06221298121623,
15.3982623199601));
#257425=CARTESIAN_POINT('Ctrl Pts',(-2.37776872599902,-3.13498874991623,
15.4041303255633));
#257426=CARTESIAN_POINT('Ctrl Pts',(-2.28434142003608,-3.20369504651285,
15.4099983311666));
#257427=CARTESIAN_POINT('Ctrl Pts',(-2.18819425914149,-3.26807204392134,
15.4158663367698));
#257428=CARTESIAN_POINT('Ctrl Pts',(-2.09190829246281,-3.33254198114751,
15.4217428138985));
#257429=CARTESIAN_POINT('Ctrl Pts',(-1.99289498611017,-3.39266993270988,
15.4276192910271));
#257430=CARTESIAN_POINT('Ctrl Pts',(-1.89159118139578,-3.4482418422242,
15.4334957681558));
#257431=CARTESIAN_POINT('Ctrl Pts',(-1.86940330188646,-3.46041337749755,
15.4347828527509));
#257432=CARTESIAN_POINT('Ctrl Pts',(-1.84710561964617,-3.4723665379636,
15.436069937346));
#257433=CARTESIAN_POINT('Ctrl Pts',(-1.82470284365832,-3.48409938611763,
15.437357021941));
#257434=CARTESIAN_POINT('Ctrl Pts',(-1.722427185683,-3.53766349645506,15.4432329644538));
#257435=CARTESIAN_POINT('Ctrl Pts',(-1.61762224335903,-3.58680871003884,
15.4491089069666));
#257436=CARTESIAN_POINT('Ctrl Pts',(-1.51070636986404,-3.6312883752261,
15.4549848494793));
#257437=CARTESIAN_POINT('Ctrl Pts',(-1.40392769843921,-3.67571096093635,
15.4608532515638));
#257438=CARTESIAN_POINT('Ctrl Pts',(-1.2950438607618,-3.71547974793598,
15.4667216536482));
#257439=CARTESIAN_POINT('Ctrl Pts',(-1.18449807480459,-3.75039375409892,
15.4725900557327));
#257440=CARTESIAN_POINT('Ctrl Pts',(-1.07406468943663,-3.78527226044763,
15.4784524909515));
#257441=CARTESIAN_POINT('Ctrl Pts',(-0.961973108392244,-3.81530568121076,
15.4843149261704));
#257442=CARTESIAN_POINT('Ctrl Pts',(-0.848686199069306,-3.8403412264419,
15.4901773613892));
#257443=CARTESIAN_POINT('Ctrl Pts',(-0.731859699853181,-3.86615899411516,
15.4962229653128));
#257444=CARTESIAN_POINT('Ctrl Pts',(-0.613762362204732,-3.88666126873163,
15.5022685692364));
#257445=CARTESIAN_POINT('Ctrl Pts',(-0.494918745659073,-3.90173607964394,
15.50831417316));
#257446=CARTESIAN_POINT('Ctrl Pts',(-0.379806654910923,-3.91633756226612,
15.514169953451));
#257447=CARTESIAN_POINT('Ctrl Pts',(-0.263994888467731,-3.92584725919359,
15.520025733742));
#257448=CARTESIAN_POINT('Ctrl Pts',(-0.147969365777272,-3.93021552421638,
15.525881514033));
#257449=CARTESIAN_POINT('Ctrl Pts',(-0.0319608679768984,-3.93458314826614,
15.5317364350819));
#257450=CARTESIAN_POINT('Ctrl Pts',(0.0842609113420141,-3.93381082503105,
15.5375913561308));
#257451=CARTESIAN_POINT('Ctrl Pts',(0.200207372658188,-3.92790096717487,
15.5434462771797));
#257452=CARTESIAN_POINT('Ctrl Pts',(0.316164796896931,-3.92199055053223,
15.5493017518207));
#257453=CARTESIAN_POINT('Ctrl Pts',(0.431846439140856,-3.91094165463097,
15.5551572264617));
#257454=CARTESIAN_POINT('Ctrl Pts',(0.546766853014029,-3.8948087255275,
15.5610127011027));
#257455=CARTESIAN_POINT('Ctrl Pts',(0.661725861319464,-3.87867037840282,
15.5668701422239));
#257456=CARTESIAN_POINT('Ctrl Pts',(0.775922724378473,-3.85744466028164,
15.5727275833451));
#257457=CARTESIAN_POINT('Ctrl Pts',(0.888880940185533,-3.83123735549951,
15.5785850244663));
#257458=CARTESIAN_POINT('Ctrl Pts',(1.00196647708577,-3.80500051109806,
15.5844490678148));
#257459=CARTESIAN_POINT('Ctrl Pts',(1.11381017790052,-3.7737709664274,15.5903131111632));
#257460=CARTESIAN_POINT('Ctrl Pts',(1.22394939954868,-3.73770475925325,
15.5961771545116));
#257461=CARTESIAN_POINT('Ctrl Pts',(1.33416304153472,-3.70161418238334,
15.602045160155));
#257462=CARTESIAN_POINT('Ctrl Pts',(1.4426695257927,-3.66068058069492,15.6079131657985));
#257463=CARTESIAN_POINT('Ctrl Pts',(1.549026536114,-3.6151079915287,15.6137811714419));
#257464=CARTESIAN_POINT('Ctrl Pts',(1.6555370919682,-3.569469610108,15.6196576486102));
#257465=CARTESIAN_POINT('Ctrl Pts',(1.75989161071668,-3.51917905436695,
15.6255341257784));
#257466=CARTESIAN_POINT('Ctrl Pts',(1.86167264643179,-3.46448610294913,
15.6314106029467));
#257467=CARTESIAN_POINT('Ctrl Pts',(1.8839650436415,-3.45250708358652,15.6326976871496));
#257468=CARTESIAN_POINT('Ctrl Pts',(1.90613410120014,-3.44031703945303,
15.6339847713526));
#257469=CARTESIAN_POINT('Ctrl Pts',(1.92817562946053,-3.42791886455244,
15.6352718555555));
#257470=CARTESIAN_POINT('Ctrl Pts',(2.02880210811891,-3.37131731372989,
15.6411477979834));
#257471=CARTESIAN_POINT('Ctrl Pts',(2.12710017692677,-3.31018780155748,
15.6470237404112));
#257472=CARTESIAN_POINT('Ctrl Pts',(2.22263512295192,-3.24474684840289,
15.652899682839));
#257473=CARTESIAN_POINT('Ctrl Pts',(2.31804747172299,-3.17938987374513,
15.6587680848386));
#257474=CARTESIAN_POINT('Ctrl Pts',(2.41070341192378,-3.10973269237195,
15.6646364868382));
#257475=CARTESIAN_POINT('Ctrl Pts',(2.50019298954164,-3.03603755165295,
15.6705048888378));
#257476=CARTESIAN_POINT('Ctrl Pts',(2.58959157607271,-2.96241734257543,
15.6763673239718));
#257477=CARTESIAN_POINT('Ctrl Pts',(2.6758298872504,-2.88476760181817,15.6822297591059));
#257478=CARTESIAN_POINT('Ctrl Pts',(2.75852768418662,-2.80339330376171,
15.6880921942399));
#257479=CARTESIAN_POINT('Ctrl Pts',(2.84380933197121,-2.71947650691013,
15.6941377981954));
#257480=CARTESIAN_POINT('Ctrl Pts',(2.92532521685751,-2.63159883548661,
15.7001834021508));
#257481=CARTESIAN_POINT('Ctrl Pts',(3.00269573325262,-2.54013923506301,
15.7062290061062));
#257482=CARTESIAN_POINT('Ctrl Pts',(3.07763692057785,-2.45155134180103,
15.7120847863133));
#257483=CARTESIAN_POINT('Ctrl Pts',(3.1486888788664,-2.35960343011601,15.7179405665204));
#257484=CARTESIAN_POINT('Ctrl Pts',(3.21554531710447,-2.26467598425195,
15.7237963467274));
#257485=CARTESIAN_POINT('Ctrl Pts',(3.2823919452343,-2.16976246746553,15.7296512676928));
#257486=CARTESIAN_POINT('Ctrl Pts',(3.34504403985302,-2.07187062323162,
15.7355061886582));
#257487=CARTESIAN_POINT('Ctrl Pts',(3.40323751023743,-1.97141153717658,
15.7413611096237));
#257488=CARTESIAN_POINT('Ctrl Pts',(3.46143648291255,-1.87094295254563,
15.7472165841817));
#257489=CARTESIAN_POINT('Ctrl Pts',(3.5151757864058,-1.7679070007335,15.7530720587398));
#257490=CARTESIAN_POINT('Ctrl Pts',(3.56423668595832,-1.66274046275083,
15.7589275332978));
#257491=CARTESIAN_POINT('Ctrl Pts',(3.61331406194108,-1.55753860602876,
15.7647849743367));
#257492=CARTESIAN_POINT('Ctrl Pts',(3.6577097353157,-1.45020511416891,15.7706424153756));
#257493=CARTESIAN_POINT('Ctrl Pts',(3.69725289849194,-1.34119722807383,
15.7764998564144));
#257494=CARTESIAN_POINT('Ctrl Pts',(3.73684063283831,-1.23206647348149,
15.7823638996819));
#257495=CARTESIAN_POINT('Ctrl Pts',(3.77156479959599,-1.12125794602727,
15.7882279429493));
#257496=CARTESIAN_POINT('Ctrl Pts',(3.8013042852138,-1.00924463397891,15.7940919862167));
#257497=CARTESIAN_POINT('Ctrl Pts',(3.83106386560749,-0.897155635268339,
15.7999599917798));
#257498=CARTESIAN_POINT('Ctrl Pts',(3.85583197013601,-0.783860633166325,
15.8058279973429));
#257499=CARTESIAN_POINT('Ctrl Pts',(3.87553881180354,-0.669841711305314,
15.811696002906));
#257500=CARTESIAN_POINT('Ctrl Pts',(3.8952741038582,-0.555658182526408,
15.8175724799956));
#257501=CARTESIAN_POINT('Ctrl Pts',(3.90993349909001,-0.440749056120797,
15.8234489570851));
#257502=CARTESIAN_POINT('Ctrl Pts',(3.9194991176761,-0.3256004707249,15.8293254341746));
#257503=CARTESIAN_POINT('Ctrl Pts',(3.92159421036448,-0.300380255516758,
15.8306125191732));
#257504=CARTESIAN_POINT('Ctrl Pts',(3.9234451470044,-0.275148547052067,
15.8318996041717));
#257505=CARTESIAN_POINT('Ctrl Pts',(3.92505207281976,-0.249910435262891,
15.8331866891702));
#257506=CARTESIAN_POINT('Ctrl Pts',(3.93238818786376,-0.134690622494353,
15.8390626316252));
#257507=CARTESIAN_POINT('Ctrl Pts',(3.93465869679811,-0.0189574273576847,
15.8449385740802));
#257508=CARTESIAN_POINT('Ctrl Pts',(3.93180842280314,0.0968066442672893,
15.8508145165352));
#257509=CARTESIAN_POINT('Ctrl Pts',(3.92896180648326,0.212422159170078,
15.8566829185614));
#257510=CARTESIAN_POINT('Ctrl Pts',(3.92100748590174,0.328068062832801,
15.8625513205875));
#257511=CARTESIAN_POINT('Ctrl Pts',(3.9079421187654,0.443257708764739,15.8684197226136));
#257512=CARTESIAN_POINT('Ctrl Pts',(3.89489003621609,0.558330232318181,
15.8742821577735));
#257513=CARTESIAN_POINT('Ctrl Pts',(3.8767372904962,0.672947013189608,15.8801445929335));
#257514=CARTESIAN_POINT('Ctrl Pts',(3.85353255723104,0.786623054811122,
15.8860070280934));
#257515=CARTESIAN_POINT('Ctrl Pts',(3.82960280395371,0.90385084616139,15.8920526320389));
#257516=CARTESIAN_POINT('Ctrl Pts',(3.80030019108715,1.02007769942268,15.8980982359843));
#257517=CARTESIAN_POINT('Ctrl Pts',(3.76573577626643,1.13477886098881,15.9041438399298));
#257518=CARTESIAN_POINT('Ctrl Pts',(3.73225663690586,1.24587856259837,15.909999620161));
#257519=CARTESIAN_POINT('Ctrl Pts',(3.69384130981319,1.35554652495435,15.9158554003922));
#257520=CARTESIAN_POINT('Ctrl Pts',(3.65064207360499,1.46331864282018,15.9217111806233));
#257521=CARTESIAN_POINT('Ctrl Pts',(3.60744917619579,1.57107494684637,15.9275661016122));
#257522=CARTESIAN_POINT('Ctrl Pts',(3.55947391903185,1.676935576517,15.933421022601));
#257523=CARTESIAN_POINT('Ctrl Pts',(3.50691722930669,1.78045515158116,15.9392759435898));
#257524=CARTESIAN_POINT('Ctrl Pts',(3.4543555702644,1.88398451458289,15.9451314181705));
#257525=CARTESIAN_POINT('Ctrl Pts',(3.39721180439954,1.98517201489416,15.9509868927512));
#257526=CARTESIAN_POINT('Ctrl Pts',(3.33573311171859,2.08359631584052,15.956842367332));
#257527=CARTESIAN_POINT('Ctrl Pts',(3.27423377226964,2.18205367122606,15.9626998083928));
#257528=CARTESIAN_POINT('Ctrl Pts',(3.20839682966444,2.27774563208528,15.9685572494536));
#257529=CARTESIAN_POINT('Ctrl Pts',(3.13851272629348,2.37027991319462,15.9744146905145));
#257530=CARTESIAN_POINT('Ctrl Pts',(3.06854985290432,2.46291849451896,15.9802787338026));
#257531=CARTESIAN_POINT('Ctrl Pts',(2.99453096284138,2.55239196280046,15.9861427770908));
#257532=CARTESIAN_POINT('Ctrl Pts',(2.91678677096562,2.63834113274231,15.992006820379));
#257533=CARTESIAN_POINT('Ctrl Pts',(2.83899004785703,2.72434837796604,15.9978748259622));
#257534=CARTESIAN_POINT('Ctrl Pts',(2.75746330004798,2.80682629016288,16.0037428315454));
#257535=CARTESIAN_POINT('Ctrl Pts',(2.67257282521114,2.88545377608843,16.0096108371286));
#257536=CARTESIAN_POINT('Ctrl Pts',(2.58755979565011,2.96419477498312,16.0154873142371));
#257537=CARTESIAN_POINT('Ctrl Pts',(2.4991736615527,3.0390739884535,16.0213637913456));
#257538=CARTESIAN_POINT('Ctrl Pts',(2.40781239245791,3.10981164746775,16.0272402684541));
#257539=CARTESIAN_POINT('Ctrl Pts',(2.38780215563081,3.12530483537434,16.028527353231));
#257540=CARTESIAN_POINT('Ctrl Pts',(2.36764930105252,3.14059951784754,16.0298144380079));
#257541=CARTESIAN_POINT('Ctrl Pts',(2.34735817656715,3.15569304446794,16.0311015227848));
#257542=CARTESIAN_POINT('Ctrl Pts',(2.25472287612864,3.2245996925034,16.0369774654948));
#257543=CARTESIAN_POINT('Ctrl Pts',(2.1588980534314,3.28953760282234,16.0428534082048));
#257544=CARTESIAN_POINT('Ctrl Pts',(2.06025831770452,3.35019770526,16.0487293509148));
#257545=CARTESIAN_POINT('Ctrl Pts',(1.96174516350281,3.41077996433943,16.0545977531972));
#257546=CARTESIAN_POINT('Ctrl Pts',(1.86042462856527,3.46709511852478,16.0604661554796));
#257547=CARTESIAN_POINT('Ctrl Pts',(1.75670302621306,3.51887531431477,16.0663345577619));
#257548=CARTESIAN_POINT('Ctrl Pts',(1.65308688575583,3.5706028611151,16.072196993179));
#257549=CARTESIAN_POINT('Ctrl Pts',(1.54707490120607,3.61780443822545,16.0780594285962));
#257550=CARTESIAN_POINT('Ctrl Pts',(1.43910033353993,3.66025671640737,16.0839218640133));
#257551=CARTESIAN_POINT('Ctrl Pts',(1.32775216243419,3.70403539167324,16.0899674678627));
#257552=CARTESIAN_POINT('Ctrl Pts',(1.2143171332307,3.74276287715576,16.0960130717121));
#257553=CARTESIAN_POINT('Ctrl Pts',(1.09929582583472,3.7762465077511,16.1020586755615));
#257554=CARTESIAN_POINT('Ctrl Pts',(0.987886023861116,3.80867879997971,
16.1079144560506));
#257555=CARTESIAN_POINT('Ctrl Pts',(0.874988493563392,3.83619148904333,
16.1137702365396));
#257556=CARTESIAN_POINT('Ctrl Pts',(0.761075402106802,3.85865951235762,
16.1196260170287));
#257557=CARTESIAN_POINT('Ctrl Pts',(0.647179025582752,3.88112423884721,
16.1254809382752));
#257558=CARTESIAN_POINT('Ctrl Pts',(0.532267789068168,3.89854569164663,
16.1313358595217));
#257559=CARTESIAN_POINT('Ctrl Pts',(0.416824652016948,3.91084980656007,
16.1371907807682));
#257560=CARTESIAN_POINT('Ctrl Pts',(0.301370599646478,3.92315508484576,
16.1430462556062));
#257561=CARTESIAN_POINT('Ctrl Pts',(0.185384957217368,3.93034201964616,
16.1489017304441));
#257562=CARTESIAN_POINT('Ctrl Pts',(0.0693557111087275,3.93238843266234,
16.1547572052821));
#257563=CARTESIAN_POINT('Ctrl Pts',(-0.0467125017996223,3.93443553293772,
16.1606146465994));
#257564=CARTESIAN_POINT('Ctrl Pts',(-0.162823935041237,3.93133867128822,
16.1664720879166));
#257565=CARTESIAN_POINT('Ctrl Pts',(-0.27849140397048,3.92312777486466,
16.1723295292339));
#257566=CARTESIAN_POINT('Ctrl Pts',(-0.394289247684611,3.91490762351519,
16.1781935727762));
#257567=CARTESIAN_POINT('Ctrl Pts',(-0.509641716381478,3.90156196173147,
16.1840576163185));
#257568=CARTESIAN_POINT('Ctrl Pts',(-0.624067450912624,3.88317251956585,
16.1899216598607));
#257569=CARTESIAN_POINT('Ctrl Pts',(-0.738570502125945,3.86477065178059,
16.1957896656969));
#257570=CARTESIAN_POINT('Ctrl Pts',(-0.852145169060522,3.84131830056579,
16.2016576715331));
#257571=CARTESIAN_POINT('Ctrl Pts',(-0.964322658995429,3.81294778476548,
16.2075256773693));
#257572=CARTESIAN_POINT('Ctrl Pts',(-1.07666209731249,3.78453631102309,
16.2134021547272));
#257573=CARTESIAN_POINT('Ctrl Pts',(-1.18759993953065,3.75119262138117,
16.2192786320852));
#257574=CARTESIAN_POINT('Ctrl Pts',(-1.29668480014169,3.71309810388596,
16.2251551094432));
#257575=CARTESIAN_POINT('Ctrl Pts',(-1.32057686791984,3.70475453733719,
16.2264421917619));
#257576=CARTESIAN_POINT('Ctrl Pts',(-1.34438013266287,3.69618324772217,
16.2277292740806));
#257577=CARTESIAN_POINT('Ctrl Pts',(-1.36809000354252,3.68738643787263,
16.2290163563994));
#257578=CARTESIAN_POINT('Ctrl Pts',(-1.47633314070521,3.64722618984889,
16.2348922984774));
#257579=CARTESIAN_POINT('Ctrl Pts',(-1.58298499780571,3.6022294401552,16.2407682405554));
#257580=CARTESIAN_POINT('Ctrl Pts',(-1.68758233870674,3.55254202650512,
16.2466441826334));
#257581=CARTESIAN_POINT('Ctrl Pts',(-1.79204545284052,3.50291837528771,
16.2525125842835));
#257582=CARTESIAN_POINT('Ctrl Pts',(-1.89445892456106,3.44861620653612,
16.2583809859336));
#257583=CARTESIAN_POINT('Ctrl Pts',(-1.99437681718968,3.3898303956181,16.2642493875837));
#257584=CARTESIAN_POINT('Ctrl Pts',(-2.09419311545055,3.33110435685035,
16.270111822369));
#257585=CARTESIAN_POINT('Ctrl Pts',(-2.19151852827018,3.26790395220451,
16.2759742571543));
#257586=CARTESIAN_POINT('Ctrl Pts',(-2.28592978297765,3.20047090711597,
16.2818366919396));
#257587=CARTESIAN_POINT('Ctrl Pts',(-2.38329087750043,3.13093094498788,
16.287882296026));
#257588=CARTESIAN_POINT('Ctrl Pts',(-2.47755231355264,3.05688969211424,
16.2939279001124));
#257589=CARTESIAN_POINT('Ctrl Pts',(-2.568279870193,2.97866203325611,16.2999735041989));
#257590=CARTESIAN_POINT('Ctrl Pts',(-2.65615869777351,2.90289062267937,
16.3058292840612));
#257591=CARTESIAN_POINT('Ctrl Pts',(-2.74072191081018,2.82319206033073,
16.3116850639235));
#257592=CARTESIAN_POINT('Ctrl Pts',(-2.82160745935929,2.7398942215509,16.3175408437858));
#257593=CARTESIAN_POINT('Ctrl Pts',(-2.9024811392813,2.65660860536218,16.3233957644085));
#257594=CARTESIAN_POINT('Ctrl Pts',(-2.97967794029489,2.56972505896492,
16.3292506850312));
#257595=CARTESIAN_POINT('Ctrl Pts',(-3.05287270506265,2.47960828492798,
16.3351056056539));
#257596=CARTESIAN_POINT('Ctrl Pts',(-3.12607439054958,2.38948299016025,
16.3409610798717));
#257597=CARTESIAN_POINT('Ctrl Pts',(-3.19527302732344,2.29612418043976,
16.3468165540895));
#257598=CARTESIAN_POINT('Ctrl Pts',(-3.2601842350632,2.19992903372935,16.3526720283073));
#257599=CARTESIAN_POINT('Ctrl Pts',(-3.32511724237395,2.10370158115063,
16.3585294690086));
#257600=CARTESIAN_POINT('Ctrl Pts',(-3.38575972672887,2.00463623941591,
16.36438690971));
#257601=CARTESIAN_POINT('Ctrl Pts',(-3.44187144351535,1.90315789316429,
16.3702443504114));
#257602=CARTESIAN_POINT('Ctrl Pts',(-3.49804640681553,1.80156516524725,
16.3761083933471));
#257603=CARTESIAN_POINT('Ctrl Pts',(-3.54968020995711,1.69755436573442,
16.3819724362829));
#257604=CARTESIAN_POINT('Ctrl Pts',(-3.59657922647575,1.59157370790143,
16.3878364792186));
#257605=CARTESIAN_POINT('Ctrl Pts',(-3.64350993237871,1.48552143957325,
16.393704484453));
#257606=CARTESIAN_POINT('Ctrl Pts',(-3.68569933130791,1.37749704602172,
16.3995724896874));
#257607=CARTESIAN_POINT('Ctrl Pts',(-3.72300306814158,1.26796575450931,
16.4054404949218));
#257608=CARTESIAN_POINT('Ctrl Pts',(-3.76036065970673,1.15827633464857,
16.4113169716894));
#257609=CARTESIAN_POINT('Ctrl Pts',(-3.7928183979578,1.04707606996503,16.417193448457));
#257610=CARTESIAN_POINT('Ctrl Pts',(-3.82028256120574,0.934842314268731,
16.4230699252246));
#257611=CARTESIAN_POINT('Ctrl Pts',(-3.82629786656153,0.91026045078191,
16.4243570134878));
#257612=CARTESIAN_POINT('Ctrl Pts',(-3.83207381993411,0.885629034250463,
16.4256441017509));
#257613=CARTESIAN_POINT('Ctrl Pts',(-3.83760976837449,0.860953114679714,
16.426931190014));
#257614=CARTESIAN_POINT('Ctrl Pts',(-3.8719651963883,0.707817335396848,
16.4349187044658));
#257615=CARTESIAN_POINT('Ctrl Pts',(-3.89716537352266,0.552558641249351,
16.4429062189176));
#257616=CARTESIAN_POINT('Ctrl Pts',(-3.91300312232185,0.39610044773955,
16.4508937333694));
#257617=CARTESIAN_POINT('Ctrl Pts',(-3.92618403448921,0.265888652321806,
16.4575413149013));
#257618=CARTESIAN_POINT('Ctrl Pts',(-3.93288093123125,0.13484612770825,
16.4641888964331));
#257619=CARTESIAN_POINT('Ctrl Pts',(-3.93299842594567,0.00351873682833392,
16.470836477965));
#257620=CARTESIAN_POINT('',(-3.93299991974386,-0.00079454059141139,17.720836478003));
#257621=CARTESIAN_POINT('Ctrl Pts',(-3.93299842594645,0.0035187359570327,
16.4708364780091));
#257622=CARTESIAN_POINT('Ctrl Pts',(-3.93310067614775,-0.110769430492911,
16.476621561376));
#257623=CARTESIAN_POINT('Ctrl Pts',(-3.92821711002783,-0.225203848643301,
16.482406644743));
#257624=CARTESIAN_POINT('Ctrl Pts',(-3.91833624616476,-0.339308210910733,
16.4881917281099));
#257625=CARTESIAN_POINT('Ctrl Pts',(-3.90846305116049,-0.453324013083181,
16.4939723214861));
#257626=CARTESIAN_POINT('Ctrl Pts',(-3.89360030670427,-0.567009847050024,
16.4997529148622));
#257627=CARTESIAN_POINT('Ctrl Pts',(-3.87378859678277,-0.679890364276321,
16.5055335082384));
#257628=CARTESIAN_POINT('Ctrl Pts',(-3.85398502950259,-0.792724487447362,
16.5113117257824));
#257629=CARTESIAN_POINT('Ctrl Pts',(-3.82923661124358,-0.904753533642884,
16.5170899433263));
#257630=CARTESIAN_POINT('Ctrl Pts',(-3.79963558588898,-1.01550894355793,
16.5228681608703));
#257631=CARTESIAN_POINT('Ctrl Pts',(-3.77003912510385,-1.12624727464689,
16.5286454873953));
#257632=CARTESIAN_POINT('Ctrl Pts',(-3.73559165424352,-1.23571194940489,
16.5344228139203));
#257633=CARTESIAN_POINT('Ctrl Pts',(-3.69643597277664,-1.34344709578114,
16.5402001404453));
#257634=CARTESIAN_POINT('Ctrl Pts',(-3.65727627383656,-1.45119329605937,
16.5459780597387));
#257635=CARTESIAN_POINT('Ctrl Pts',(-3.61340755033825,-1.55720921625382,
16.5517559790322));
#257636=CARTESIAN_POINT('Ctrl Pts',(-3.56502136312672,-1.66105739830089,
16.5575338983257));
#257637=CARTESIAN_POINT('Ctrl Pts',(-3.51658769134419,-1.76500749344872,
16.5633174878741));
#257638=CARTESIAN_POINT('Ctrl Pts',(-3.46362788203505,-1.8667852161216,
16.5691010774226));
#257639=CARTESIAN_POINT('Ctrl Pts',(-3.40638025669218,-1.96597623251598,
16.5748846669711));
#257640=CARTESIAN_POINT('Ctrl Pts',(-3.34910430852904,-2.06521632289924,
16.5806711179058));
#257641=CARTESIAN_POINT('Ctrl Pts',(-3.28753654943814,-2.16186680105467,
16.5864575688405));
#257642=CARTESIAN_POINT('Ctrl Pts',(-3.22195851665732,-2.25554257706197,
16.5922440197752));
#257643=CARTESIAN_POINT('Ctrl Pts',(-3.15627465627497,-2.3493695238543,
16.5980398086878));
#257644=CARTESIAN_POINT('Ctrl Pts',(-3.08656785431739,-2.44021184282936,
16.6038355976004));
#257645=CARTESIAN_POINT('Ctrl Pts',(-3.01315999384475,-2.52771751813638,
16.6096313865131));
#257646=CARTESIAN_POINT('Ctrl Pts',(-2.94892519766469,-2.60428846274304,
16.6147029322183));
#257647=CARTESIAN_POINT('Ctrl Pts',(-2.88185724592194,-2.67830497406639,
16.6197744779234));
#257648=CARTESIAN_POINT('Ctrl Pts',(-2.81219345753973,-2.74955577455172,
16.6248460236286));
#257649=CARTESIAN_POINT('Ctrl Pts',(-2.73148029001437,-2.83210767029901,
16.6307219676107));
#257650=CARTESIAN_POINT('Ctrl Pts',(-2.64699592537828,-2.91123874359358,
16.6365979115928));
#257651=CARTESIAN_POINT('Ctrl Pts',(-2.55906200173616,-2.98658511870499,
16.6424738555749));
#257652=CARTESIAN_POINT('Ctrl Pts',(-2.4712409210588,-3.06183480407484,
16.6483422591345));
#257653=CARTESIAN_POINT('Ctrl Pts',(-2.37997939550461,-3.13330918391156,
16.654210662694));
#257654=CARTESIAN_POINT('Ctrl Pts',(-2.28563682562428,-3.20068013105811,
16.6600790662536));
#257655=CARTESIAN_POINT('Ctrl Pts',(-2.19139018116286,-3.26798257692961,
16.6659415029514));
#257656=CARTESIAN_POINT('Ctrl Pts',(-2.09406905775236,-3.33118965085894,
16.6718039396492));
#257657=CARTESIAN_POINT('Ctrl Pts',(-1.99406643804611,-3.39001298532293,
16.6776663763471));
#257658=CARTESIAN_POINT('Ctrl Pts',(-1.89093932453771,-3.45067420307932,
16.6837119797177));
#257659=CARTESIAN_POINT('Ctrl Pts',(-1.78496073760388,-3.5066729555298,
16.6897575830884));
#257660=CARTESIAN_POINT('Ctrl Pts',(-1.67659494708285,-3.55774062902515,
16.6958031864591));
#257661=CARTESIAN_POINT('Ctrl Pts',(-1.57163165694161,-3.60720486496306,
16.7016589682295));
#257662=CARTESIAN_POINT('Ctrl Pts',(-1.46442923095247,-3.65204285809281,
16.70751475));
#257663=CARTESIAN_POINT('Ctrl Pts',(-1.35543445374064,-3.69205720995935,
16.7133705317705));
#257664=CARTESIAN_POINT('Ctrl Pts',(-1.24645566980974,-3.73206569034482,
16.7192254542964));
#257665=CARTESIAN_POINT('Ctrl Pts',(-1.13568544499393,-3.76725179467923,
16.7250803768224));
#257666=CARTESIAN_POINT('Ctrl Pts',(-1.02358920258385,-3.79746680622145,
16.7309352993484));
#257667=CARTESIAN_POINT('Ctrl Pts',(-0.911482361374219,-3.82768467461992,
16.7367907754625));
#257668=CARTESIAN_POINT('Ctrl Pts',(-0.798049651887935,-3.85293040843941,
16.7426462515766));
#257669=CARTESIAN_POINT('Ctrl Pts',(-0.68376958058739,-3.87310575128841,
16.7485017276907));
#257670=CARTESIAN_POINT('Ctrl Pts',(-0.569451130022772,-3.89328786972655,
16.7543591702794));
#257671=CARTESIAN_POINT('Ctrl Pts',(-0.454285158019641,-3.90839613945071,
16.7602166128682));
#257672=CARTESIAN_POINT('Ctrl Pts',(-0.338757531693442,-3.91838389322958,
16.766074055457));
#257673=CARTESIAN_POINT('Ctrl Pts',(-0.223099688497213,-3.92838290469699,
16.7719381002574));
#257674=CARTESIAN_POINT('Ctrl Pts',(-0.107079788808458,-3.93324984519266,
16.7778021450578));
#257675=CARTESIAN_POINT('Ctrl Pts',(0.00881394883159336,-3.93299012385055,
16.7836661898582));
#257676=CARTESIAN_POINT('Ctrl Pts',(0.124785994932083,-3.93273022701684,
16.7895341969462));
#257677=CARTESIAN_POINT('Ctrl Pts',(0.240631297964359,-3.92733678968229,
16.7954022040342));
#257678=CARTESIAN_POINT('Ctrl Pts',(0.355866135827682,-3.91686715288776,
16.8012702111222));
#257679=CARTESIAN_POINT('Ctrl Pts',(0.471267335504422,-3.9063824013259,
16.8071466897135));
#257680=CARTESIAN_POINT('Ctrl Pts',(0.586055903834923,-3.89080688065476,
16.8130231683047));
#257681=CARTESIAN_POINT('Ctrl Pts',(0.699757634082706,-3.87024912034651,
16.818899646896));
#257682=CARTESIAN_POINT('Ctrl Pts',(0.724660660077218,-3.86574654647864,
16.8201867170117));
#257683=CARTESIAN_POINT('Ctrl Pts',(0.749511607663112,-3.86100516442516,
16.8214737871275));
#257684=CARTESIAN_POINT('Ctrl Pts',(0.77430559803329,-3.85602643155546,
16.8227608572433));
#257685=CARTESIAN_POINT('Ctrl Pts',(0.887499108740622,-3.83329671988012,
16.8286367966446));
#257686=CARTESIAN_POINT('Ctrl Pts',(0.999877666872273,-3.8055411024948,
16.8345127360458));
#257687=CARTESIAN_POINT('Ctrl Pts',(1.11096092379942,-3.7728311419663,16.8403886754471));
#257688=CARTESIAN_POINT('Ctrl Pts',(1.22190163071379,-3.74016315720823,
16.846257074421));
#257689=CARTESIAN_POINT('Ctrl Pts',(1.33154994972937,-3.70255358869003,
16.8521254733948));
#257690=CARTESIAN_POINT('Ctrl Pts',(1.43943494607293,-3.66012513939401,
16.8579938723687));
#257691=CARTESIAN_POINT('Ctrl Pts',(1.54721024728521,-3.61773983042772,
16.8638563044814));
#257692=CARTESIAN_POINT('Ctrl Pts',(1.65322541027905,-3.57054553709331,
16.869718736594));
#257693=CARTESIAN_POINT('Ctrl Pts',(1.75702455489567,-3.51871478149248,
16.8755811687067));
#257694=CARTESIAN_POINT('Ctrl Pts',(1.86406692654826,-3.46526456256678,
16.8816267737963));
#257695=CARTESIAN_POINT('Ctrl Pts',(1.96875209481662,-3.40688351012709,
16.887672378886));
#257696=CARTESIAN_POINT('Ctrl Pts',(2.07060191860303,-3.34381469203625,
16.8937179839756));
#257697=CARTESIAN_POINT('Ctrl Pts',(2.16925372742428,-3.28272619179566,
16.8995737611909));
#257698=CARTESIAN_POINT('Ctrl Pts',(2.26524520844887,-3.21724014283959,
16.9054295384062));
#257699=CARTESIAN_POINT('Ctrl Pts',(2.35816747105485,-3.14762373521022,
16.9112853156215));
#257700=CARTESIAN_POINT('Ctrl Pts',(2.45107609905883,-3.07801754248507,
16.9171402336112));
#257701=CARTESIAN_POINT('Ctrl Pts',(2.5409160739004,-3.00428244362256,16.9229951516008));
#257702=CARTESIAN_POINT('Ctrl Pts',(2.62730918114217,-2.92672777461213,
16.9288500695905));
#257703=CARTESIAN_POINT('Ctrl Pts',(2.71371045728507,-2.84916577241917,
16.9347055411919));
#257704=CARTESIAN_POINT('Ctrl Pts',(2.7966639107643,-2.76778375787002,16.9405610127934));
#257705=CARTESIAN_POINT('Ctrl Pts',(2.87582652079642,-2.68292952242208,
16.9464164843949));
#257706=CARTESIAN_POINT('Ctrl Pts',(2.95501571682069,-2.59804678950498,
16.9522739224995));
#257707=CARTESIAN_POINT('Ctrl Pts',(3.03041125641113,-2.50968981853689,
16.9581313606042));
#257708=CARTESIAN_POINT('Ctrl Pts',(3.1017093758898,-2.41824067195912,16.9639887987088));
#257709=CARTESIAN_POINT('Ctrl Pts',(3.17308785983102,-2.32668844746613,
16.9698528390895));
#257710=CARTESIAN_POINT('Ctrl Pts',(3.24035945181504,-2.23203741660605,
16.9757168794701));
#257711=CARTESIAN_POINT('Ctrl Pts',(3.30326278213121,-2.1346999770897,16.9815809198508));
#257712=CARTESIAN_POINT('Ctrl Pts',(3.36620861609834,-2.03729676686562,
16.9874489225515));
#257713=CARTESIAN_POINT('Ctrl Pts',(3.42478010300587,-1.93720388879762,
16.9933169252522));
#257714=CARTESIAN_POINT('Ctrl Pts',(3.47876187563326,-1.83485825410044,
16.9991849279529));
#257715=CARTESIAN_POINT('Ctrl Pts',(3.53282158126532,-1.7323648639214,17.0050614022368));
#257716=CARTESIAN_POINT('Ctrl Pts',(3.58227817363852,-1.62761259844179,
17.0109378765208));
#257717=CARTESIAN_POINT('Ctrl Pts',(3.62696439803191,-1.52105826824912,
17.0168143508047));
#257718=CARTESIAN_POINT('Ctrl Pts',(3.63675193954838,-1.49771986934259,
17.0181014641558));
#257719=CARTESIAN_POINT('Ctrl Pts',(3.64631082119755,-1.47429507487814,
17.0193885775068));
#257720=CARTESIAN_POINT('Ctrl Pts',(3.65563960785821,-1.45078877079272,
17.0206756908579));
#257721=CARTESIAN_POINT('Ctrl Pts',(3.69822748261985,-1.3434775447015,17.0265516342354));
#257722=CARTESIAN_POINT('Ctrl Pts',(3.73615643626882,-1.23411244653244,
17.0324275776128));
#257723=CARTESIAN_POINT('Ctrl Pts',(3.76922486550075,-1.12313530497926,
17.0383035209903));
#257724=CARTESIAN_POINT('Ctrl Pts',(3.80225085884139,-1.01230057762671,
17.044171923916));
#257725=CARTESIAN_POINT('Ctrl Pts',(3.83042861538971,-0.899858312969997,
17.0500403268418));
#257726=CARTESIAN_POINT('Ctrl Pts',(3.85360454877944,-0.78627029806956,
17.0559087297675));
#257727=CARTESIAN_POINT('Ctrl Pts',(3.87675691728429,-0.672797777481723,
17.0617711658035));
#257728=CARTESIAN_POINT('Ctrl Pts',(3.89491749686474,-0.558182226016013,
17.0676336018395));
#257729=CARTESIAN_POINT('Ctrl Pts',(3.90798268218396,-0.442899938756253,
17.0734960378755));
#257730=CARTESIAN_POINT('Ctrl Pts',(3.92145607976527,-0.3240157398426,17.0795416414837));
#257731=CARTESIAN_POINT('Ctrl Pts',(3.92951031765096,-0.204422885091915,
17.0855872450919));
#257732=CARTESIAN_POINT('Ctrl Pts',(3.93208883058094,-0.08465476017675,
17.0916328487001));
#257733=CARTESIAN_POINT('Ctrl Pts',(3.93458638220943,0.0313528316190549,
17.097488629744));
#257734=CARTESIAN_POINT('Ctrl Pts',(3.93194691662088,0.147524408656614,
17.1033444107879));
#257735=CARTESIAN_POINT('Ctrl Pts',(3.92417181586921,0.263371523779159,
17.1092001918318));
#257736=CARTESIAN_POINT('Ctrl Pts',(3.91639785602221,0.379201639698823,
17.1150551136086));
#257737=CARTESIAN_POINT('Ctrl Pts',(3.90348978714195,0.494706976650673,
17.1209100353854));
#257738=CARTESIAN_POINT('Ctrl Pts',(3.88550104532099,0.609401859867114,
17.1267649571623));
#257739=CARTESIAN_POINT('Ctrl Pts',(3.86751060271479,0.724107587164066,
17.1326204325056));
#257740=CARTESIAN_POINT('Ctrl Pts',(3.84443859620843,0.838002300606692,
17.1384759078489));
#257741=CARTESIAN_POINT('Ctrl Pts',(3.81638988128393,0.950608896462505,
17.1443313831922));
#257742=CARTESIAN_POINT('Ctrl Pts',(3.78833174671346,1.06325330917618,17.1501888249894));
#257743=CARTESIAN_POINT('Ctrl Pts',(3.75529368000615,1.17460834380498,17.1560462667867));
#257744=CARTESIAN_POINT('Ctrl Pts',(3.71743065980171,1.28421115458722,17.1619037085839));
#257745=CARTESIAN_POINT('Ctrl Pts',(3.67952496248891,1.39393750361356,17.1677677525665));
#257746=CARTESIAN_POINT('Ctrl Pts',(3.63678359202403,1.50190729655567,17.173631796549));
#257747=CARTESIAN_POINT('Ctrl Pts',(3.58941005794056,1.60767671997674,17.1794958405316));
#257748=CARTESIAN_POINT('Ctrl Pts',(3.54200451407092,1.71351761065672,17.1853638467855));
#257749=CARTESIAN_POINT('Ctrl Pts',(3.48996075889787,1.81715480334818,17.1912318530394));
#257750=CARTESIAN_POINT('Ctrl Pts',(3.43352791571731,1.9181697140738,17.1970998592932));
#257751=CARTESIAN_POINT('Ctrl Pts',(3.37701360192753,2.01933045736522,17.2029763370332));
#257752=CARTESIAN_POINT('Ctrl Pts',(3.31609777103728,2.11786101402561,17.2088528147731));
#257753=CARTESIAN_POINT('Ctrl Pts',(3.25107243960499,2.21337231220616,17.2147292925131));
#257754=CARTESIAN_POINT('Ctrl Pts',(3.23683046796727,2.23429137820409,17.2160163698329));
#257755=CARTESIAN_POINT('Ctrl Pts',(3.22239151149396,2.25506573819467,17.2173034471527));
#257756=CARTESIAN_POINT('Ctrl Pts',(3.20775888593271,2.27569152780418,17.2185905244726));
#257757=CARTESIAN_POINT('Ctrl Pts',(3.14095590324228,2.36985537150351,17.2244664763692));
#257758=CARTESIAN_POINT('Ctrl Pts',(3.06989293192811,2.46123056080213,17.2303424282658));
#257759=CARTESIAN_POINT('Ctrl Pts',(2.99483071752197,2.54940737689896,17.2362183801624));
#257760=CARTESIAN_POINT('Ctrl Pts',(2.91986482756885,2.63747103907879,17.2420867916759));
#257761=CARTESIAN_POINT('Ctrl Pts',(2.84091016594796,2.72234417899121,17.2479552031894));
#257762=CARTESIAN_POINT('Ctrl Pts',(2.75827036878138,2.80364647783964,17.2538236147029));
#257763=CARTESIAN_POINT('Ctrl Pts',(2.67571459738447,2.88486611084824,17.2596860593843));
#257764=CARTESIAN_POINT('Ctrl Pts',(2.58948143612544,2.96252183701393,17.2655485040657));
#257765=CARTESIAN_POINT('Ctrl Pts',(2.49991391043687,3.03626735324876,17.2714109487471));
#257766=CARTESIAN_POINT('Ctrl Pts',(2.40754809760837,3.11231684213573,17.2774565491362));
#257767=CARTESIAN_POINT('Ctrl Pts',(2.31163643951869,3.18420743762803,17.2835021495254));
#257768=CARTESIAN_POINT('Ctrl Pts',(2.21259545924414,3.25160119537009,17.2895477499146));
#257769=CARTESIAN_POINT('Ctrl Pts',(2.11666401779078,3.31687902589269,17.2954035396915));
#257770=CARTESIAN_POINT('Ctrl Pts',(2.01779718218882,3.37793791755644,17.3012593294684));
#257771=CARTESIAN_POINT('Ctrl Pts',(1.9164053502428,3.4345129980189,17.3071151192452));
#257772=CARTESIAN_POINT('Ctrl Pts',(1.81502839603622,3.49107977693191,17.3129700497723));
#257773=CARTESIAN_POINT('Ctrl Pts',(1.71112754257285,3.54316385185117,17.3188249802993));
#257774=CARTESIAN_POINT('Ctrl Pts',(1.60513921357111,3.59054551636048,17.3246799108264));
#257775=CARTESIAN_POINT('Ctrl Pts',(1.49914086354589,3.63793166072881,17.3305353949276));
#257776=CARTESIAN_POINT('Ctrl Pts',(1.39105502246991,3.68061434239041,17.3363908790287));
#257777=CARTESIAN_POINT('Ctrl Pts',(1.28133893120599,3.71842164679799,17.3422463631299));
#257778=CARTESIAN_POINT('Ctrl Pts',(1.17158599389743,3.75624164806352,17.3481038136831));
#257779=CARTESIAN_POINT('Ctrl Pts',(1.06020210774935,3.78918288192592,17.3539612642363));
#257780=CARTESIAN_POINT('Ctrl Pts',(0.947659855360323,3.81712323596428,
17.3598187147895));
#257781=CARTESIAN_POINT('Ctrl Pts',(0.83499075264517,3.84509508255719,17.365682767481));
#257782=CARTESIAN_POINT('Ctrl Pts',(0.72116107858175,3.86805469964639,17.3715468201724));
#257783=CARTESIAN_POINT('Ctrl Pts',(0.606653886206962,3.88593104189331,
17.3774108728639));
#257784=CARTESIAN_POINT('Ctrl Pts',(0.492069323007804,3.90381946292155,
17.3832788878095));
#257785=CARTESIAN_POINT('Ctrl Pts',(0.376806739120909,3.91661772430358,
17.389146902755));
#257786=CARTESIAN_POINT('Ctrl Pts',(0.261352871919692,3.92430677653255,
17.3950149177006));
#257787=CARTESIAN_POINT('Ctrl Pts',(0.145732329050413,3.93200692910791,
17.4008914040411));
#257788=CARTESIAN_POINT('Ctrl Pts',(0.0299203627822675,3.93458314356511,
17.4067678903817));
#257789=CARTESIAN_POINT('Ctrl Pts',(-0.0855976786094879,3.9320684171841,
17.4126443767222));
#257790=CARTESIAN_POINT('Ctrl Pts',(-0.110896980453302,3.93151767358594,
17.4139313705105));
#257791=CARTESIAN_POINT('Ctrl Pts',(-0.136182211232252,3.93072294360493,
17.4152183642988));
#257792=CARTESIAN_POINT('Ctrl Pts',(-0.161448325108427,3.92968490318495,
17.4165053580872));
#257793=CARTESIAN_POINT('Ctrl Pts',(-0.276803700559333,3.9249456091658,
17.4223812776046));
#257794=CARTESIAN_POINT('Ctrl Pts',(-0.392140530454384,3.91511483242535,
17.428257197122));
#257795=CARTESIAN_POINT('Ctrl Pts',(-0.50697318805222,3.90018809630974,
17.4341331166395));
#257796=CARTESIAN_POINT('Ctrl Pts',(-0.62165848345037,3.88528051534314,
17.4400014957199));
#257797=CARTESIAN_POINT('Ctrl Pts',(-0.735840487596784,3.86529003304004,
17.4458698748003));
#257798=CARTESIAN_POINT('Ctrl Pts',(-0.849034869944904,3.84026415622905,
17.4517382538807));
#257799=CARTESIAN_POINT('Ctrl Pts',(-0.962114158566661,3.81526372521633,
17.4576006661136));
#257800=CARTESIAN_POINT('Ctrl Pts',(-1.07420742218651,3.7852381724168,17.4634630783465));
#257801=CARTESIAN_POINT('Ctrl Pts',(-1.18483740451374,3.75028656569937,
17.4693254905794));
#257802=CARTESIAN_POINT('Ctrl Pts',(-1.29892457249747,3.71424272167995,
17.4753711031262));
#257803=CARTESIAN_POINT('Ctrl Pts',(-1.41145505743273,3.67295994118316,
17.4814167156729));
#257804=CARTESIAN_POINT('Ctrl Pts',(-1.52191857161317,3.62660348830403,
17.4874623282197));
#257805=CARTESIAN_POINT('Ctrl Pts',(-1.62891311449737,3.58170280302043,
17.493318085713));
#257806=CARTESIAN_POINT('Ctrl Pts',(-1.73396815795937,3.53204251637407,
17.4991738432063));
#257807=CARTESIAN_POINT('Ctrl Pts',(-1.83663804450311,3.47782255060315,
17.5050296006995));
#257808=CARTESIAN_POINT('Ctrl Pts',(-1.93929286772474,3.42361053977244,
17.5108844990591));
#257809=CARTESIAN_POINT('Ctrl Pts',(-2.03956286497587,3.36484037276013,
17.5167393974187));
#257810=CARTESIAN_POINT('Ctrl Pts',(-2.13702608290057,3.30175839833908,
17.5225942957782));
#257811=CARTESIAN_POINT('Ctrl Pts',(-2.23449851836854,3.23867045796655,
17.5284497478624));
#257812=CARTESIAN_POINT('Ctrl Pts',(-2.32916330028911,3.17127012383021,
17.5343051999465));
#257813=CARTESIAN_POINT('Ctrl Pts',(-2.42062721873252,3.09984723299895,
17.5401606520306));
#257814=CARTESIAN_POINT('Ctrl Pts',(-2.51212185663276,3.0284003537748,17.5460180707516));
#257815=CARTESIAN_POINT('Ctrl Pts',(-2.6004131681809,2.95292848524702,17.5518754894725));
#257816=CARTESIAN_POINT('Ctrl Pts',(-2.68514135502035,2.8737614555769,17.5577329081934));
#257817=CARTESIAN_POINT('Ctrl Pts',(-2.76996504873149,2.79450518765412,
17.5635969294838));
#257818=CARTESIAN_POINT('Ctrl Pts',(-2.85121729967337,2.71154572716617,
17.5694609507742));
#257819=CARTESIAN_POINT('Ctrl Pts',(-2.92857543508125,2.62524949691238,
17.5753249720646));
#257820=CARTESIAN_POINT('Ctrl Pts',(-3.00598584335641,2.53889495409239,
17.5811929558239));
#257821=CARTESIAN_POINT('Ctrl Pts',(-3.0794966354121,2.44919947017301,17.5870609395832));
#257822=CARTESIAN_POINT('Ctrl Pts',(-3.14882673908066,2.35656087705169,
17.5929289233425));
#257823=CARTESIAN_POINT('Ctrl Pts',(-3.21825693856327,2.26378853632436,
17.5988053790437));
#257824=CARTESIAN_POINT('Ctrl Pts',(-3.2834941725723,2.16806494631924,17.6046818347449));
#257825=CARTESIAN_POINT('Ctrl Pts',(-3.34430177547875,2.06981512085734,
17.6105582904461));
#257826=CARTESIAN_POINT('Ctrl Pts',(-3.35762233069981,2.04829244666907,
17.6118455908647));
#257827=CARTESIAN_POINT('Ctrl Pts',(-3.37073049823953,2.02664862920047,
17.6131328912832));
#257828=CARTESIAN_POINT('Ctrl Pts',(-3.3836240952532,2.00488827170543,17.6144201917018));
#257829=CARTESIAN_POINT('Ctrl Pts',(-3.44454128761214,1.90207911131986,
17.6205021816334));
#257830=CARTESIAN_POINT('Ctrl Pts',(-3.50085414675206,1.79634782237633,
17.6265841715651));
#257831=CARTESIAN_POINT('Ctrl Pts',(-3.55228244957488,1.68812866762055,
17.6326661614968));
#257832=CARTESIAN_POINT('Ctrl Pts',(-3.60362884969778,1.58008185845017,
17.6387384654896));
#257833=CARTESIAN_POINT('Ctrl Pts',(-3.65010602275546,1.46955540601067,
17.6448107694824));
#257834=CARTESIAN_POINT('Ctrl Pts',(-3.69147830432186,1.35701029057301,
17.6508830734753));
#257835=CARTESIAN_POINT('Ctrl Pts',(-3.73277151972813,1.24468025899781,
17.6569437727477));
#257836=CARTESIAN_POINT('Ctrl Pts',(-3.76897915975207,1.13033960097184,
17.6630044720201));
#257837=CARTESIAN_POINT('Ctrl Pts',(-3.7999129418847,1.01447061766085,17.6690651712925));
#257838=CARTESIAN_POINT('Ctrl Pts',(-3.83081195534235,0.898731867730426,
17.6751190585146));
#257839=CARTESIAN_POINT('Ctrl Pts',(-3.85644881503235,0.781468569978592,
17.6811729457366));
#257840=CARTESIAN_POINT('Ctrl Pts',(-3.87668426530563,0.66318029760524,
17.6872268329586));
#257841=CARTESIAN_POINT('Ctrl Pts',(-3.89689414166229,0.545041520023117,
17.6932730691719));
#257842=CARTESIAN_POINT('Ctrl Pts',(-3.91171614982977,0.425880715184696,
17.6993193053852));
#257843=CARTESIAN_POINT('Ctrl Pts',(-3.92106171204903,0.306209161037272,
17.7053655415984));
#257844=CARTESIAN_POINT('Ctrl Pts',(-3.92903276452442,0.204138443883995,
17.7105225203873));
#257845=CARTESIAN_POINT('Ctrl Pts',(-3.93302062486231,0.101696518362754,
17.7156794991761));
#257846=CARTESIAN_POINT('Ctrl Pts',(-3.93299991974402,-0.000794539836274554,
17.720836477965));
#257847=CARTESIAN_POINT('',(-3.93299894594177,-0.00287944802932865,18.970836477928));
#257848=CARTESIAN_POINT('Ctrl Pts',(-3.93299991974386,-0.000794540591381787,
17.720836478003));
#257849=CARTESIAN_POINT('Ctrl Pts',(-3.93297488581434,-0.124713247691418,
17.7270716184659));
#257850=CARTESIAN_POINT('Ctrl Pts',(-3.92708906524364,-0.248483679099339,
17.7333067589288));
#257851=CARTESIAN_POINT('Ctrl Pts',(-3.91540977936332,-0.371557881986174,
17.7395418993916));
#257852=CARTESIAN_POINT('Ctrl Pts',(-3.90369131069854,-0.495044985971108,
17.7457979580996));
#257853=CARTESIAN_POINT('Ctrl Pts',(-3.88614052210331,-0.617830863470176,
17.7520540168076));
#257854=CARTESIAN_POINT('Ctrl Pts',(-3.8628763889649,-0.739374738260309,
17.7583100755156));
#257855=CARTESIAN_POINT('Ctrl Pts',(-3.83957308099714,-0.86112328263881,
17.7645766688965));
#257856=CARTESIAN_POINT('Ctrl Pts',(-3.8105372973786,-0.98162533375304,
17.7708432622774));
#257857=CARTESIAN_POINT('Ctrl Pts',(-3.77593807307681,-1.1003547920053,
17.7771098556582));
#257858=CARTESIAN_POINT('Ctrl Pts',(-3.74123648688048,-1.21943551166669,
17.7833949887718));
#257859=CARTESIAN_POINT('Ctrl Pts',(-3.70093863710898,-1.33673283863354,
17.7896801218854));
#257860=CARTESIAN_POINT('Ctrl Pts',(-3.65526274537066,-1.45173801434877,
17.795965254999));
#257861=CARTESIAN_POINT('Ctrl Pts',(-3.61560811683237,-1.5515825351541,
17.8014218451048));
#257862=CARTESIAN_POINT('Ctrl Pts',(-3.57190073260232,-1.64969963998605,
17.8068784352106));
#257863=CARTESIAN_POINT('Ctrl Pts',(-3.52431099124079,-1.74577233252775,
17.8123350253164));
#257864=CARTESIAN_POINT('Ctrl Pts',(-3.47306336887225,-1.84922944169551,
17.8182110242431));
#257865=CARTESIAN_POINT('Ctrl Pts',(-3.41717183874442,-1.95059870997914,
17.8240870231698));
#257866=CARTESIAN_POINT('Ctrl Pts',(-3.35682983759973,-2.04943466385249,
17.8299630220965));
#257867=CARTESIAN_POINT('Ctrl Pts',(-3.2965652673676,-2.14814379133698,
17.8358314809358));
#257868=CARTESIAN_POINT('Ctrl Pts',(-3.23186179656452,-2.24432572013498,
17.8416999397752));
#257869=CARTESIAN_POINT('Ctrl Pts',(-3.16295982397821,-2.33755730451678,
17.8475683986145));
#257870=CARTESIAN_POINT('Ctrl Pts',(-3.09412790559635,-2.43069409822382,
17.8534308908582));
#257871=CARTESIAN_POINT('Ctrl Pts',(-3.02110622035992,-2.52088618428527,
17.8592933831018));
#257872=CARTESIAN_POINT('Ctrl Pts',(-2.94417939310716,-2.60773785131926,
17.8651558753454));
#257873=CARTESIAN_POINT('Ctrl Pts',(-2.86485007840845,-2.69730196662597,
17.8712014579948));
#257874=CARTESIAN_POINT('Ctrl Pts',(-2.78136792497248,-2.7833132051691,
17.8772470406442));
#257875=CARTESIAN_POINT('Ctrl Pts',(-2.69409144613518,-2.86537262495845,
17.8832926232936));
#257876=CARTESIAN_POINT('Ctrl Pts',(-2.60955420333167,-2.94485654992269,
17.889148460916));
#257877=CARTESIAN_POINT('Ctrl Pts',(-2.52145757372515,-3.0206327066666,
17.8950042985383));
#257878=CARTESIAN_POINT('Ctrl Pts',(-2.43016546459566,-3.09237527067569,
17.9008601361607));
#257879=CARTESIAN_POINT('Ctrl Pts',(-2.33888675076927,-3.16410730788899,
17.9067151145552));
#257880=CARTESIAN_POINT('Ctrl Pts',(-2.24441381420525,-3.23180667427304,
17.9125700929497));
#257881=CARTESIAN_POINT('Ctrl Pts',(-2.14714333413732,-3.29518808304923,
17.9184250713442));
#257882=CARTESIAN_POINT('Ctrl Pts',(-2.04986365787679,-3.35857548406112,
17.9242806032829));
#257883=CARTESIAN_POINT('Ctrl Pts',(-1.94978625816811,-3.4176438905975,
17.9301361352217));
#257884=CARTESIAN_POINT('Ctrl Pts',(-1.84733585251232,-3.47215196211551,
17.9359916671604));
#257885=CARTESIAN_POINT('Ctrl Pts',(-1.74485104256939,-3.52667833821056,
17.9418491654691));
#257886=CARTESIAN_POINT('Ctrl Pts',(-1.63999200626029,-3.57664114030922,
17.9477066637778));
#257887=CARTESIAN_POINT('Ctrl Pts',(-1.53320640599483,-3.62184581624017,
17.9535641620865));
#257888=CARTESIAN_POINT('Ctrl Pts',(-1.42630045149718,-3.66710144074518,
17.9594282621721));
#257889=CARTESIAN_POINT('Ctrl Pts',(-1.31746397952908,-3.70758807470327,
17.9652923622577));
#257890=CARTESIAN_POINT('Ctrl Pts',(-1.20716298407007,-3.74315996584317,
17.9711564623433));
#257891=CARTESIAN_POINT('Ctrl Pts',(-1.0967874633723,-3.77875589125102,
17.9770245245279));
#257892=CARTESIAN_POINT('Ctrl Pts',(-0.984945845856242,-3.80943035263879,
17.9828925867125));
#257893=CARTESIAN_POINT('Ctrl Pts',(-0.872115900019499,-3.83508837667832,
17.988760648897));
#257894=CARTESIAN_POINT('Ctrl Pts',(-0.759123079087412,-3.86078343922817,
17.994637181893));
#257895=CARTESIAN_POINT('Ctrl Pts',(-0.645139487153175,-3.88144753966241,
18.0005137148889));
#257896=CARTESIAN_POINT('Ctrl Pts',(-0.530649664272131,-3.89703732774115,
18.0063902478849));
#257897=CARTESIAN_POINT('Ctrl Pts',(-0.505584648024338,-3.90045036727305,
18.0076767849003));
#257898=CARTESIAN_POINT('Ctrl Pts',(-0.480495372701463,-3.90362039622428,
18.0089633219157));
#257899=CARTESIAN_POINT('Ctrl Pts',(-0.45538692229026,-3.90654729281587,
18.0102498589311));
#257900=CARTESIAN_POINT('Ctrl Pts',(-0.340713484564884,-3.91991479612761,
18.0161256346122));
#257901=CARTESIAN_POINT('Ctrl Pts',(-0.225261720292381,-3.92825086847855,
18.0220014102934));
#257902=CARTESIAN_POINT('Ctrl Pts',(-0.109510553206871,-3.93147509705153,
18.0278771859746));
#257903=CARTESIAN_POINT('Ctrl Pts',(0.00609206620409948,-3.93469518785494,
18.0337454210595));
#257904=CARTESIAN_POINT('Ctrl Pts',(0.12199291537467,-3.93281646991857,
18.0396136561444));
#257905=CARTESIAN_POINT('Ctrl Pts',(0.237706215873664,-3.92581007626898,
18.0454818912294));
#257906=CARTESIAN_POINT('Ctrl Pts',(0.353301858790676,-3.91881080673849,
18.0513441594777));
#257907=CARTESIAN_POINT('Ctrl Pts',(0.468709922737927,-3.90669425729709,
18.0572064277261));
#257908=CARTESIAN_POINT('Ctrl Pts',(0.58344354785797,-3.88948359380303,
18.0630686959745));
#257909=CARTESIAN_POINT('Ctrl Pts',(0.70176655989913,-3.87173450288295,
18.0691143624983));
#257910=CARTESIAN_POINT('Ctrl Pts',(0.819371792889485,-3.84856730564004,
18.0751600290221));
#257911=CARTESIAN_POINT('Ctrl Pts',(0.935729352959446,-3.82006538923224,
18.0812056955459));
#257912=CARTESIAN_POINT('Ctrl Pts',(1.04842908682777,-3.79245946150426,
18.0870613099802));
#257913=CARTESIAN_POINT('Ctrl Pts',(1.15995798684355,-3.75984930431401,
18.0929169244146));
#257914=CARTESIAN_POINT('Ctrl Pts',(1.26984462171162,-3.72236264175189,
18.0987725388489));
#257915=CARTESIAN_POINT('Ctrl Pts',(1.37971514505317,-3.68488147546653,
18.1046272947358));
#257916=CARTESIAN_POINT('Ctrl Pts',(1.48794349146881,-3.642525358783,18.1104820506227));
#257917=CARTESIAN_POINT('Ctrl Pts',(1.59407437776438,-3.59547157938359,
18.1163368065096));
#257918=CARTESIAN_POINT('Ctrl Pts',(1.70021531495974,-3.5484133438561,18.1221921168587));
#257919=CARTESIAN_POINT('Ctrl Pts',(1.80425801978836,-3.49665672854094,
18.1280474272078));
#257920=CARTESIAN_POINT('Ctrl Pts',(1.90576879438018,-3.44042647100134,
18.1339027375569));
#257921=CARTESIAN_POINT('Ctrl Pts',(2.00731367905753,-3.38417731872961,
18.1397600154325));
#257922=CARTESIAN_POINT('Ctrl Pts',(2.1063245808304,-3.32345173494806,18.1456172933081));
#257923=CARTESIAN_POINT('Ctrl Pts',(2.20239454523198,-3.25851918317698,
18.1514745711837));
#257924=CARTESIAN_POINT('Ctrl Pts',(2.29857283674299,-3.19351341439491,
18.1573384536415));
#257925=CARTESIAN_POINT('Ctrl Pts',(2.39180323002588,-3.12429144095205,
18.1632023360993));
#257926=CARTESIAN_POINT('Ctrl Pts',(2.48170971374509,-3.0511646787257,18.1690662185571));
#257927=CARTESIAN_POINT('Ctrl Pts',(2.57167696652274,-2.97798848909095,
18.1749340644957));
#257928=CARTESIAN_POINT('Ctrl Pts',(2.6583155284195,-2.90090252884139,18.1808019104342));
#257929=CARTESIAN_POINT('Ctrl Pts',(2.74128556283274,-2.82025574425526,
18.1866697563728));
#257930=CARTESIAN_POINT('Ctrl Pts',(2.82437542406964,-2.73949248812487,
18.1925460767606));
#257931=CARTESIAN_POINT('Ctrl Pts',(2.90378590270158,-2.65515844412652,
18.1984223971483));
#257932=CARTESIAN_POINT('Ctrl Pts',(2.97921676953516,-2.56763635278061,
18.204298717536));
#257933=CARTESIAN_POINT('Ctrl Pts',(2.99575851827648,-2.54844303703158,
18.2055873758726));
#257934=CARTESIAN_POINT('Ctrl Pts',(3.0121090476354,-2.52909651654374,18.2068760342091));
#257935=CARTESIAN_POINT('Ctrl Pts',(3.02826547238151,-2.50960100987826,
18.2081646925457));
#257936=CARTESIAN_POINT('Ctrl Pts',(3.10193627915747,-2.42070450417717,
18.2140407759492));
#257937=CARTESIAN_POINT('Ctrl Pts',(3.17181087799,-2.32841464196013,18.2199168593528));
#257938=CARTESIAN_POINT('Ctrl Pts',(3.23756097330368,-2.23308932739846,
18.2257929427563));
#257939=CARTESIAN_POINT('Ctrl Pts',(3.30322668534541,-2.13788635276503,
18.2316614848303));
#257940=CARTESIAN_POINT('Ctrl Pts',(3.36477818866503,-2.03965600993005,
18.2375300269042));
#257941=CARTESIAN_POINT('Ctrl Pts',(3.42192668560722,-1.93879002430103,
18.2433985689781));
#257942=CARTESIAN_POINT('Ctrl Pts',(3.47901706632259,-1.83802661268206,
18.2492611431343));
#257943=CARTESIAN_POINT('Ctrl Pts',(3.53171314487032,-1.73463324670722,
18.2551237172906));
#257944=CARTESIAN_POINT('Ctrl Pts',(3.57976917376844,-1.62903089674114,
18.2609862914469));
#257945=CARTESIAN_POINT('Ctrl Pts',(3.62932508338567,-1.52013258303776,
18.2670318428933));
#257946=CARTESIAN_POINT('Ctrl Pts',(3.67394629137763,-1.40888549915709,
18.2730773943397));
#257947=CARTESIAN_POINT('Ctrl Pts',(3.71341416183815,-1.29577940354826,
18.2791229457861));
#257948=CARTESIAN_POINT('Ctrl Pts',(3.75164401190339,-1.18622119769277,
18.2849788615642));
#257949=CARTESIAN_POINT('Ctrl Pts',(3.78503884728929,-1.0749192827355,18.2908347773422));
#257950=CARTESIAN_POINT('Ctrl Pts',(3.81344901027675,-0.962338633755953,
18.2966906931203));
#257951=CARTESIAN_POINT('Ctrl Pts',(3.84185499733292,-0.849774532694668,
18.3025457481536));
#257952=CARTESIAN_POINT('Ctrl Pts',(3.86527766794579,-0.7359324714477,18.3084008031868));
#257953=CARTESIAN_POINT('Ctrl Pts',(3.88361772652158,-0.621290877325088,
18.31425585822));
#257954=CARTESIAN_POINT('Ctrl Pts',(3.90195951400109,-0.506638476024428,
18.3201114652049));
#257955=CARTESIAN_POINT('Ctrl Pts',(3.91521767176824,-0.39118679959254,
18.3259670721898));
#257956=CARTESIAN_POINT('Ctrl Pts',(3.92334445499873,-0.275422016967966,
18.3318226791747));
#257957=CARTESIAN_POINT('Ctrl Pts',(3.93147396496573,-0.159618392399321,
18.3376802508604));
#257958=CARTESIAN_POINT('Ctrl Pts',(3.93446864792641,-0.0435018642342749,
18.3435378225461));
#257959=CARTESIAN_POINT('Ctrl Pts',(3.93233283481887,0.0724394657999363,
18.3493953942318));
#257960=CARTESIAN_POINT('Ctrl Pts',(3.93019461556805,0.188511411874933,
18.3552595648829));
#257961=CARTESIAN_POINT('Ctrl Pts',(3.92291437187116,0.304407353006746,
18.361123735534));
#257962=CARTESIAN_POINT('Ctrl Pts',(3.91054847183753,0.419642287441569,
18.3669879061851));
#257963=CARTESIAN_POINT('Ctrl Pts',(3.89817422013104,0.534955049165209,
18.3728560373756));
#257964=CARTESIAN_POINT('Ctrl Pts',(3.88070753460741,0.649605508229467,
18.3787241685661));
#257965=CARTESIAN_POINT('Ctrl Pts',(3.85825596185029,0.763118557530013,
18.3845922997566));
#257966=CARTESIAN_POINT('Ctrl Pts',(3.83577199021616,0.876795412518599,
18.3904688989891));
#257967=CARTESIAN_POINT('Ctrl Pts',(3.80828887319298,0.989331182825753,
18.3963454982216));
#257968=CARTESIAN_POINT('Ctrl Pts',(3.77596407233751,1.10026556994951,18.4022220974541));
#257969=CARTESIAN_POINT('Ctrl Pts',(3.76889135279296,1.1245381961439,18.4035079070228));
#257970=CARTESIAN_POINT('Ctrl Pts',(3.76158702439922,1.14873423410985,18.4047937165915));
#257971=CARTESIAN_POINT('Ctrl Pts',(3.75405304017374,1.17284899776666,18.4060795261603));
#257972=CARTESIAN_POINT('Ctrl Pts',(3.71962208134895,1.28305555112387,18.4119557869796));
#257973=CARTESIAN_POINT('Ctrl Pts',(3.68027731276114,1.39192630389124,18.4178320477989));
#257974=CARTESIAN_POINT('Ctrl Pts',(3.63614013207501,1.49899097392663,18.4237083086182));
#257975=CARTESIAN_POINT('Ctrl Pts',(3.59205956952264,1.60591830392999,18.4295770315088));
#257976=CARTESIAN_POINT('Ctrl Pts',(3.54319897664802,1.71104378055194,18.4354457543994));
#257977=CARTESIAN_POINT('Ctrl Pts',(3.48972962711575,1.81391183072126,18.44131447729));
#257978=CARTESIAN_POINT('Ctrl Pts',(3.43631462206099,1.9166753292084,18.4471772354048));
#257979=CARTESIAN_POINT('Ctrl Pts',(3.37830036708313,2.01718560101243,18.4530399935197));
#257980=CARTESIAN_POINT('Ctrl Pts',(3.31590610828367,2.11500725319018,18.4589027516345));
#257981=CARTESIAN_POINT('Ctrl Pts',(3.25156719723852,2.21587772907773,18.464948235307));
#257982=CARTESIAN_POINT('Ctrl Pts',(3.18257095061507,2.31388883067095,18.4709937189796));
#257983=CARTESIAN_POINT('Ctrl Pts',(3.10920903409692,2.40859049701066,18.4770392026521));
#257984=CARTESIAN_POINT('Ctrl Pts',(3.03814521112503,2.50032559297483,18.4828953089518));
#257985=CARTESIAN_POINT('Ctrl Pts',(2.96298542301897,2.58895514989585,18.4887514152515));
#257986=CARTESIAN_POINT('Ctrl Pts',(2.88403815099348,2.67410039894057,18.4946075215513));
#257987=CARTESIAN_POINT('Ctrl Pts',(2.80510245468572,2.75923316348337,18.500462769194));
#257988=CARTESIAN_POINT('Ctrl Pts',(2.72238065927654,2.84088233348448,18.5063180168366));
#257989=CARTESIAN_POINT('Ctrl Pts',(2.63621995589132,2.91870405217116,18.5121732644793));
#257990=CARTESIAN_POINT('Ctrl Pts',(2.55005110297565,2.99653313164346,18.5180290659419));
#257991=CARTESIAN_POINT('Ctrl Pts',(2.4604430017628,3.07053376349345,18.5238848674046));
#257992=CARTESIAN_POINT('Ctrl Pts',(2.36777741151076,3.14040110965771,18.5297406688672));
#257993=CARTESIAN_POINT('Ctrl Pts',(2.27508070458647,3.21029191695038,18.5355984366807));
#257994=CARTESIAN_POINT('Ctrl Pts',(2.17932479641105,3.27604643033228,18.5414562044941));
#257995=CARTESIAN_POINT('Ctrl Pts',(2.08092142884035,3.33740243407849,18.5473139723075));
#257996=CARTESIAN_POINT('Ctrl Pts',(1.98240718282173,3.39882757223172,18.5531783405068));
#257997=CARTESIAN_POINT('Ctrl Pts',(1.88123987386353,3.45584409037383,18.5590427087062));
#257998=CARTESIAN_POINT('Ctrl Pts',(1.77785698489317,3.50823510347676,18.5649070769056));
#257999=CARTESIAN_POINT('Ctrl Pts',(1.67440425686416,3.56066150869411,18.5707754067078));
#258000=CARTESIAN_POINT('Ctrl Pts',(1.56873334356251,3.60845601710389,18.5766437365101));
#258001=CARTESIAN_POINT('Ctrl Pts',(1.46130130311543,3.65145005463763,18.5825120663124));
#258002=CARTESIAN_POINT('Ctrl Pts',(1.35371423721524,3.69450613297523,18.5883888641702));
#258003=CARTESIAN_POINT('Ctrl Pts',(1.24436136058433,3.73274778058609,18.594265662028));
#258004=CARTESIAN_POINT('Ctrl Pts',(1.13371449742192,3.76605635092405,18.6001424598859));
#258005=CARTESIAN_POINT('Ctrl Pts',(1.10954029857822,3.77333362910018,18.6014264265155));
#258006=CARTESIAN_POINT('Ctrl Pts',(1.08530436796868,3.78037562719454,18.6027103931452));
#258007=CARTESIAN_POINT('Ctrl Pts',(1.06101167767463,3.78718143476624,18.6039943597749));
#258008=CARTESIAN_POINT('Ctrl Pts',(0.949861003344788,3.81832125879547,
18.6098691210705));
#258009=CARTESIAN_POINT('Ctrl Pts',(0.837154478092364,3.84461515798849,
18.6157438823661));
#258010=CARTESIAN_POINT('Ctrl Pts',(0.723352382783124,3.86590873279776,
18.6216186436618));
#258011=CARTESIAN_POINT('Ctrl Pts',(0.609696392508168,3.88717496981093,
18.627485862634));
#258012=CARTESIAN_POINT('Ctrl Pts',(0.494948031629236,3.90345357400914,
18.6333530816063));
#258013=CARTESIAN_POINT('Ctrl Pts',(0.379582426893661,3.91463998104468,
18.6392203005786));
#258014=CARTESIAN_POINT('Ctrl Pts',(0.264334156778507,3.92581501074791,
18.6450815521924));
#258015=CARTESIAN_POINT('Ctrl Pts',(0.148470300141058,3.93190810551321,
18.6509428038063));
#258016=CARTESIAN_POINT('Ctrl Pts',(0.0324752019179193,3.93286592210571,
18.6568040554202));
#258017=CARTESIAN_POINT('Ctrl Pts',(-0.0871770345004511,3.93385393710916,
18.6628501028356));
#258018=CARTESIAN_POINT('Ctrl Pts',(-0.206968485783391,3.92937740804405,
18.668896150251));
#258019=CARTESIAN_POINT('Ctrl Pts',(-0.326362506474011,3.91943573928289,
18.6749421976664));
#258020=CARTESIAN_POINT('Ctrl Pts',(-0.441975985118381,3.90980886766604,
18.6807968005158));
#258021=CARTESIAN_POINT('Ctrl Pts',(-0.557216380231496,3.89505777357661,
18.6866514033652));
#258022=CARTESIAN_POINT('Ctrl Pts',(-0.671598214632129,3.8752348107054,
18.6925060062147));
#258023=CARTESIAN_POINT('Ctrl Pts',(-0.785963345652738,3.85541474261626,
18.6983597541062));
#258024=CARTESIAN_POINT('Ctrl Pts',(-0.89946975849245,3.83052434898566,
18.7042135019977));
#258025=CARTESIAN_POINT('Ctrl Pts',(-1.01164016905407,3.80066746353272,
18.7100672498892));
#258026=CARTESIAN_POINT('Ctrl Pts',(-1.12382129359438,3.77080772629353,
18.7159215569026));
#258027=CARTESIAN_POINT('Ctrl Pts',(-1.23466576311504,3.73598066043904,
18.721775863916));
#258028=CARTESIAN_POINT('Ctrl Pts',(-1.34371018966508,3.69634034231025,
18.7276301709294));
#258029=CARTESIAN_POINT('Ctrl Pts',(-1.45279137087877,3.65668666296157,
18.7334864512035));
#258030=CARTESIAN_POINT('Ctrl Pts',(-1.56007091479021,3.61221664632338,
18.7393427314777));
#258031=CARTESIAN_POINT('Ctrl Pts',(-1.66510485227562,3.56313272709959,
18.7451990117518));
#258032=CARTESIAN_POINT('Ctrl Pts',(-1.77025748546047,3.51399333961228,
18.7510619100324));
#258033=CARTESIAN_POINT('Ctrl Pts',(-1.87315907298071,3.4602298178422,18.7569248083131));
#258034=CARTESIAN_POINT('Ctrl Pts',(-1.97338964691929,3.40209087201265,
18.7627877065937));
#258035=CARTESIAN_POINT('Ctrl Pts',(-2.07368809359793,3.34391255646383,
18.7686545750299));
#258036=CARTESIAN_POINT('Ctrl Pts',(-2.17131157832395,3.28135313929512,
18.7745214434662));
#258037=CARTESIAN_POINT('Ctrl Pts',(-2.2658699964757,3.2147040546637,18.7803883119024));
#258038=CARTESIAN_POINT('Ctrl Pts',(-2.36056527542287,3.14795850430331,
18.7862636718542));
#258039=CARTESIAN_POINT('Ctrl Pts',(-2.45218630920164,3.07711172534182,
18.7921390318059));
#258040=CARTESIAN_POINT('Ctrl Pts',(-2.54037683090483,3.00249472222716,
18.7980143917577));
#258041=CARTESIAN_POINT('Ctrl Pts',(-2.55986412420316,2.98600674373859,
18.7993126589683));
#258042=CARTESIAN_POINT('Ctrl Pts',(-2.57918406329377,2.96933481511489,
18.800610926179));
#258043=CARTESIAN_POINT('Ctrl Pts',(-2.59833305960692,2.95248273684263,
18.8019091933896));
#258044=CARTESIAN_POINT('Ctrl Pts',(-2.68376370729919,2.87729947719728,
18.8077012363179));
#258045=CARTESIAN_POINT('Ctrl Pts',(-2.76608902957665,2.79826365860864,
18.8134932792462));
#258046=CARTESIAN_POINT('Ctrl Pts',(-2.84493415261627,2.71566541887574,
18.8192853221745));
#258047=CARTESIAN_POINT('Ctrl Pts',(-2.92367726215477,2.63317404860156,
18.8250698710873));
#258048=CARTESIAN_POINT('Ctrl Pts',(-2.99894883105194,2.54712972324905,
18.8308544200001));
#258049=CARTESIAN_POINT('Ctrl Pts',(-3.07040720799903,2.45786260337465,
18.8366389689128));
#258050=CARTESIAN_POINT('Ctrl Pts',(-3.14178558698597,2.36869541842465,
18.8424170419982));
#258051=CARTESIAN_POINT('Ctrl Pts',(-3.20935900137614,2.27631294623772,
18.8481951150836));
#258052=CARTESIAN_POINT('Ctrl Pts',(-3.27282351652875,2.18108120657082,
18.853973188169));
#258053=CARTESIAN_POINT('Ctrl Pts',(-3.33624872740734,2.08590844497033,
18.8597476828301));
#258054=CARTESIAN_POINT('Ctrl Pts',(-3.39556985957282,1.9878902747605,18.8655221774911));
#258055=CARTESIAN_POINT('Ctrl Pts',(-3.45052439071638,1.88742428432808,
18.8712966721521));
#258056=CARTESIAN_POINT('Ctrl Pts',(-3.50545905190921,1.78699461945858,
18.8770690789248));
#258057=CARTESIAN_POINT('Ctrl Pts',(-3.55603004609453,1.68411926648386,
18.8828414856975));
#258058=CARTESIAN_POINT('Ctrl Pts',(-3.60201964944105,1.57922241785019,
18.8886138924702));
#258059=CARTESIAN_POINT('Ctrl Pts',(-3.64800447626287,1.47433646390469,
18.8943856997151));
#258060=CARTESIAN_POINT('Ctrl Pts',(-3.68940868866779,1.36742982206938,
18.9001575069601));
#258061=CARTESIAN_POINT('Ctrl Pts',(-3.72606213610041,1.2589479567952,18.905929314205));
#258062=CARTESIAN_POINT('Ctrl Pts',(-3.76273881891724,1.15039732260583,
18.9117047803189));
#258063=CARTESIAN_POINT('Ctrl Pts',(-3.79465858306969,1.04026987371933,
18.9174802464327));
#258064=CARTESIAN_POINT('Ctrl Pts',(-3.82170081340551,0.929027390777956,
18.9232557125466));
#258065=CARTESIAN_POINT('Ctrl Pts',(-3.84875170762517,0.81774926758282,
18.9290330290243));
#258066=CARTESIAN_POINT('Ctrl Pts',(-3.87092187129608,0.705355816281533,
18.9348103455021));
#258067=CARTESIAN_POINT('Ctrl Pts',(-3.8881419432584,0.592318519949188,
18.9405876619799));
#258068=CARTESIAN_POINT('Ctrl Pts',(-3.90538360762339,0.479139485137241,
18.9463722226866));
#258069=CARTESIAN_POINT('Ctrl Pts',(-3.9176627359606,0.365315416113108,
18.9521567833933));
#258070=CARTESIAN_POINT('Ctrl Pts',(-3.92496191163897,0.251322486426023,
18.9579413441));
#258071=CARTESIAN_POINT('Ctrl Pts',(-3.930385766159,0.166616884837634,18.9622397220427));
#258072=CARTESIAN_POINT('Ctrl Pts',(-3.93306095518726,0.0818181379921459,
18.9665380999854));
#258073=CARTESIAN_POINT('Ctrl Pts',(-3.93299894594177,-0.00287944802935699,
18.970836477928));
#258074=CARTESIAN_POINT('Ctrl Pts',(-3.93299894594123,-0.00287944875768067,
18.970836477965));
#258075=CARTESIAN_POINT('Ctrl Pts',(-3.93285955254499,-0.193274946860016,
18.9804989943114));
#258076=CARTESIAN_POINT('Ctrl Pts',(-3.91889275474165,-0.383164830983256,
18.9901615106578));
#258077=CARTESIAN_POINT('Ctrl Pts',(-3.89132795850799,-0.571012888938626,
18.9998240270042));
#258078=CARTESIAN_POINT('Ctrl Pts',(-3.87179907361845,-0.704097968524874,
19.0066696487847));
#258079=CARTESIAN_POINT('Ctrl Pts',(-3.84542340013612,-0.836284199472048,
19.0135152705652));
#258080=CARTESIAN_POINT('Ctrl Pts',(-3.81229009242283,-0.966919464699496,
19.0203608923457));
#258081=CARTESIAN_POINT('Ctrl Pts',(-3.77930457041597,-1.09697205266679,
19.0271759803485));
#258082=CARTESIAN_POINT('Ctrl Pts',(-3.73962153078669,-1.22548733640384,
19.0339910683513));
#258083=CARTESIAN_POINT('Ctrl Pts',(-3.6933803811278,-1.35182482604081,
19.0408061563541));
#258084=CARTESIAN_POINT('Ctrl Pts',(-3.64750954796444,-1.47715055760599,
19.0475666665724));
#258085=CARTESIAN_POINT('Ctrl Pts',(-3.59518520759239,-1.60033308325736,
19.0543271767906));
#258086=CARTESIAN_POINT('Ctrl Pts',(-3.53659449190347,-1.72075227730143,
19.0610876870088));
#258087=CARTESIAN_POINT('Ctrl Pts',(-3.51951458529148,-1.75585593774284,
19.0630584580059));
#258088=CARTESIAN_POINT('Ctrl Pts',(-3.50190250031843,-1.79072481372021,
19.0650292290029));
#258089=CARTESIAN_POINT('Ctrl Pts',(-3.48376370290062,-1.82534365595966,
19.067));
#258090=CARTESIAN_POINT('',(-3.56066877200036,1.66757030866008,19.0681870665394));
#258091=CARTESIAN_POINT('Origin',(0.,0.,19.067));
#258092=CARTESIAN_POINT('',(-3.93115504418186,-0.00207051908275006,17.9041635502338));
#258093=CARTESIAN_POINT('Ctrl Pts',(-3.56174364677249,1.66807409747762,
19.0669999597496));
#258094=CARTESIAN_POINT('Ctrl Pts',(-3.5099739625514,1.77861495663293,19.0608645385329));
#258095=CARTESIAN_POINT('Ctrl Pts',(-3.45310794955396,1.88662946387192,
19.0547291173162));
#258096=CARTESIAN_POINT('Ctrl Pts',(-3.39142665006682,1.99166118534668,
19.0485936960995));
#258097=CARTESIAN_POINT('Ctrl Pts',(-3.32695834632604,2.10143865402443,
19.0421810523669));
#258098=CARTESIAN_POINT('Ctrl Pts',(-3.25722971012385,2.2079571269901,19.0357684086343));
#258099=CARTESIAN_POINT('Ctrl Pts',(-3.18260936614508,2.31073291890812,
19.0293557649017));
#258100=CARTESIAN_POINT('Ctrl Pts',(-3.11090557499978,2.40949169601291,
19.0231937607835));
#258101=CARTESIAN_POINT('Ctrl Pts',(-3.03468553378717,2.50479464386839,
19.0170317566654));
#258102=CARTESIAN_POINT('Ctrl Pts',(-2.95431481317474,2.59624979242297,
19.0108697525473));
#258103=CARTESIAN_POINT('Ctrl Pts',(-2.87382287672716,2.68784287444543,
19.0046984548398));
#258104=CARTESIAN_POINT('Ctrl Pts',(-2.78916801121425,2.77557632717908,
18.9985271571323));
#258105=CARTESIAN_POINT('Ctrl Pts',(-2.70075115349836,2.85909639691936,
18.9923558594248));
#258106=CARTESIAN_POINT('Ctrl Pts',(-2.61213074260116,2.94280874646168,
18.9861703541633));
#258107=CARTESIAN_POINT('Ctrl Pts',(-2.51973129512467,3.02228810083865,
18.9799848489018));
#258108=CARTESIAN_POINT('Ctrl Pts',(-2.42398602642619,3.09722145538393,
18.9737993436403));
#258109=CARTESIAN_POINT('Ctrl Pts',(-2.41285472375999,3.10593317409939,
18.9730802195296));
#258110=CARTESIAN_POINT('Ctrl Pts',(-2.40167822774746,3.11458349748398,
18.9723610954189));
#258111=CARTESIAN_POINT('Ctrl Pts',(-2.39045724201333,3.12317197318784,
18.9716419713081));
#258112=CARTESIAN_POINT('Ctrl Pts',(-2.29862762614441,3.19345781468798,
18.9657568474505));
#258113=CARTESIAN_POINT('Ctrl Pts',(-2.20354696592246,3.25980387280755,
18.9598717235929));
#258114=CARTESIAN_POINT('Ctrl Pts',(-2.10558719971127,3.32189577566968,
18.9539865997352));
#258115=CARTESIAN_POINT('Ctrl Pts',(-2.00775261843656,3.38390832992557,
18.9481089966066));
#258116=CARTESIAN_POINT('Ctrl Pts',(-1.90704659310603,3.44167732316943,
18.942231393478));
#258117=CARTESIAN_POINT('Ctrl Pts',(-1.80387324554285,3.49492922875624,
18.9363537903493));
#258118=CARTESIAN_POINT('Ctrl Pts',(-1.70080450276349,3.54812714361576,
18.9304821463702));
#258119=CARTESIAN_POINT('Ctrl Pts',(-1.59527377741334,3.59681689371709,
18.9246105023911));
#258120=CARTESIAN_POINT('Ctrl Pts',(-1.48771267368374,3.64076914958375,
18.918738858412));
#258121=CARTESIAN_POINT('Ctrl Pts',(-1.37713666330677,3.6859533744781,18.9127026339494));
#258122=CARTESIAN_POINT('Ctrl Pts',(-1.26441514053429,3.72613035403407,
18.9066664094867));
#258123=CARTESIAN_POINT('Ctrl Pts',(-1.15004282740772,3.76110229788131,
18.900630185024));
#258124=CARTESIAN_POINT('Ctrl Pts',(-1.03891586331661,3.79508190222671,
18.8947652402592));
#258125=CARTESIAN_POINT('Ctrl Pts',(-0.926230951465942,3.8241477588249,
18.8889002954944));
#258126=CARTESIAN_POINT('Ctrl Pts',(-0.812459787741505,3.8481681477429,
18.8830353507297));
#258127=CARTESIAN_POINT('Ctrl Pts',(-0.698705966307203,3.872184875201,18.8771712999662));
#258128=CARTESIAN_POINT('Ctrl Pts',(-0.583866624546522,3.89115757953955,
18.8713072492028));
#258129=CARTESIAN_POINT('Ctrl Pts',(-0.468424941049874,3.90500538726932,
18.8654431984393));
#258130=CARTESIAN_POINT('Ctrl Pts',(-0.352973253377511,3.91885439505004,
18.8595786394973));
#258131=CARTESIAN_POINT('Ctrl Pts',(-0.23691952853528,3.92757757438164,
18.8537140805552));
#258132=CARTESIAN_POINT('Ctrl Pts',(-0.120752695437392,3.93114586177422,
18.8478495216132));
#258133=CARTESIAN_POINT('Ctrl Pts',(0.00136544168213387,3.93489695490011,
18.8416845174211));
#258134=CARTESIAN_POINT('Ctrl Pts',(0.123608077433709,3.93295095848204,
18.835519513229));
#258135=CARTESIAN_POINT('Ctrl Pts',(0.245407968231507,3.92533615492081,
18.8293545090369));
#258136=CARTESIAN_POINT('Ctrl Pts',(0.361440802866056,3.91808190176338,
18.8234814092561));
#258137=CARTESIAN_POINT('Ctrl Pts',(0.477071446451001,3.90568346212199,
18.8176083094753));
#258138=CARTESIAN_POINT('Ctrl Pts',(0.591816564619008,3.88821837784898,
18.8117352096945));
#258139=CARTESIAN_POINT('Ctrl Pts',(0.706639073366195,3.87074151413813,
18.805858148764));
#258140=CARTESIAN_POINT('Ctrl Pts',(0.82057446491756,3.84819128021455,18.7999810878335));
#258141=CARTESIAN_POINT('Ctrl Pts',(0.933151490277918,3.82069591778672,
18.794104026903));
#258142=CARTESIAN_POINT('Ctrl Pts',(1.04588576594911,3.79316214917189,18.7882187567517));
#258143=CARTESIAN_POINT('Ctrl Pts',(1.15725749601787,3.76066958284886,18.7823334866004));
#258144=CARTESIAN_POINT('Ctrl Pts',(1.26681240886458,3.72339567072138,18.7764482164491));
#258145=CARTESIAN_POINT('Ctrl Pts',(1.28281361141082,3.71795157513366,18.7755886347354));
#258146=CARTESIAN_POINT('Ctrl Pts',(1.29877609546574,3.71240556355235,18.7747290530217));
#258147=CARTESIAN_POINT('Ctrl Pts',(1.31469848687477,3.70675827221161,18.773869471308));
#258148=CARTESIAN_POINT('Ctrl Pts',(1.42373525580808,3.66808553862523,18.7679830431773));
#258149=CARTESIAN_POINT('Ctrl Pts',(1.53123667264062,3.62453649152885,18.7620966150467));
#258150=CARTESIAN_POINT('Ctrl Pts',(1.63673641344779,3.57625263549628,18.7562101869161));
#258151=CARTESIAN_POINT('Ctrl Pts',(1.74210449190753,3.52802903710775,18.7503311049736));
#258152=CARTESIAN_POINT('Ctrl Pts',(1.8454754922307,3.47508255194167,18.7444520230311));
#258153=CARTESIAN_POINT('Ctrl Pts',(1.9463999146736,3.41760389339646,18.7385729410886));
#258154=CARTESIAN_POINT('Ctrl Pts',(2.04722499176466,3.36018181419465,18.7326996462435));
#258155=CARTESIAN_POINT('Ctrl Pts',(2.14560792669137,3.29823663887568,18.7268263513984));
#258156=CARTESIAN_POINT('Ctrl Pts',(2.24112140797721,3.2320061625415,18.7209530565534));
#258157=CARTESIAN_POINT('Ctrl Pts',(2.33927549178774,3.16394465292631,18.7149173863348));
#258158=CARTESIAN_POINT('Ctrl Pts',(2.43439874195802,3.09135761886026,18.7088817161163));
#258159=CARTESIAN_POINT('Ctrl Pts',(2.52605653718554,3.01455259880172,18.7028460458977));
#258160=CARTESIAN_POINT('Ctrl Pts',(2.6151531417599,2.93989373880519,18.6969790302067));
#258161=CARTESIAN_POINT('Ctrl Pts',(2.7009750644671,2.8612497813171,18.6911120145157));
#258162=CARTESIAN_POINT('Ctrl Pts',(2.7831551469449,2.77894520061733,18.6852449988246));
#258163=CARTESIAN_POINT('Ctrl Pts',(2.86532485412331,2.69665101093495,18.6793787238489));
#258164=CARTESIAN_POINT('Ctrl Pts',(2.94385334506628,2.61069740788989,18.6735124488732));
#258165=CARTESIAN_POINT('Ctrl Pts',(3.01840991512097,2.52144612956522,18.6676461738975));
#258166=CARTESIAN_POINT('Ctrl Pts',(3.09297487133345,2.43218481221512,18.6617792390804));
#258167=CARTESIAN_POINT('Ctrl Pts',(3.16356675484448,2.33962539751845,18.6559123042634));
#258168=CARTESIAN_POINT('Ctrl Pts',(3.22989523474795,2.2441625994015,18.6500453694463));
#258169=CARTESIAN_POINT('Ctrl Pts',(3.29956371003566,2.14389273642279,18.6438830029348));
#258170=CARTESIAN_POINT('Ctrl Pts',(3.36452792857829,2.04041987981295,18.6377206364233));
#258171=CARTESIAN_POINT('Ctrl Pts',(3.4245038148658,1.93423437617307,18.6315582699117));
#258172=CARTESIAN_POINT('Ctrl Pts',(3.48169104609249,1.83298610248407,18.6256824304634));
#258173=CARTESIAN_POINT('Ctrl Pts',(3.53434325267981,1.72927216476109,18.619806591015));
#258174=CARTESIAN_POINT('Ctrl Pts',(3.58226258738736,1.62354049995828,18.6139307515667));
#258175=CARTESIAN_POINT('Ctrl Pts',(3.6302152500197,1.51773529872195,18.6080508254686));
#258176=CARTESIAN_POINT('Ctrl Pts',(3.67342833320686,1.40990995629303,18.6021708993706));
#258177=CARTESIAN_POINT('Ctrl Pts',(3.71175311641914,1.30052981617216,18.5962909732725));
#258178=CARTESIAN_POINT('Ctrl Pts',(3.75013246205207,1.19099395318178,18.5904026760116));
#258179=CARTESIAN_POINT('Ctrl Pts',(3.78360950228262,1.07989926721846,18.5845143787507));
#258180=CARTESIAN_POINT('Ctrl Pts',(3.81208604666243,0.967723603536469,
18.5786260814898));
#258181=CARTESIAN_POINT('Ctrl Pts',(3.81616307805429,0.951663238341362,
18.5777830447626));
#258182=CARTESIAN_POINT('Ctrl Pts',(3.82013769526064,0.935580726698167,
18.5769400080353));
#258183=CARTESIAN_POINT('Ctrl Pts',(3.82400969690509,0.919477480950912,
18.5760969713081));
#258184=CARTESIAN_POINT('Ctrl Pts',(3.85096434828551,0.807375933723437,
18.5702282338512));
#258185=CARTESIAN_POINT('Ctrl Pts',(3.87303090986046,0.693898836985092,
18.5643594963943));
#258186=CARTESIAN_POINT('Ctrl Pts',(3.89007150739674,0.579510713740539,
18.5584907589374));
#258187=CARTESIAN_POINT('Ctrl Pts',(3.90708995623147,0.465271267700331,
18.5526296494357));
#258188=CARTESIAN_POINT('Ctrl Pts',(3.91909537116961,0.350123555482149,
18.546768539934));
#258189=CARTESIAN_POINT('Ctrl Pts',(3.92600019717784,0.234545201953788,
18.5409074304324));
#258190=CARTESIAN_POINT('Ctrl Pts',(3.93289790151264,0.119086056539917,
18.5350523661095));
#258191=CARTESIAN_POINT('Ctrl Pts',(3.93470545608126,0.00319756395961585,
18.5291973017866));
#258192=CARTESIAN_POINT('Ctrl Pts',(3.93138681688566,-0.112635234352483,
18.5233422374637));
#258193=CARTESIAN_POINT('Ctrl Pts',(3.9279619922646,-0.232174297264666,
18.5172998305405));
#258194=CARTESIAN_POINT('Ctrl Pts',(3.91907734655091,-0.351653598483055,
18.5112574236174));
#258195=CARTESIAN_POINT('Ctrl Pts',(3.90475145217433,-0.470537030150045,
18.5052150166942));
#258196=CARTESIAN_POINT('Ctrl Pts',(3.89088586043468,-0.585600640475025,
18.4993667572195));
#258197=CARTESIAN_POINT('Ctrl Pts',(3.87192338100028,-0.700105644022471,
18.4935184977448));
#258198=CARTESIAN_POINT('Ctrl Pts',(3.8479336621843,-0.813569622975753,
18.4876702382701));
#258199=CARTESIAN_POINT('Ctrl Pts',(3.82394764991499,-0.927016071105226,
18.4818228823845));
#258200=CARTESIAN_POINT('Ctrl Pts',(3.79493602828602,-1.03942140959071,
18.4759755264988));
#258201=CARTESIAN_POINT('Ctrl Pts',(3.76101959801277,-1.15031325445021,
18.4701281706132));
#258202=CARTESIAN_POINT('Ctrl Pts',(3.72710016811007,-1.26121490678183,
18.4642802975769));
#258203=CARTESIAN_POINT('Ctrl Pts',(3.68827518840264,-1.37060240357491,
18.4584324245407));
#258204=CARTESIAN_POINT('Ctrl Pts',(3.64471516728602,-1.47801906258182,
18.4525845515045));
#258205=CARTESIAN_POINT('Ctrl Pts',(3.6011407108324,-1.58547131834998,18.4467347405441));
#258206=CARTESIAN_POINT('Ctrl Pts',(3.55282824846559,-1.69095105434521,
18.4408849295837));
#258207=CARTESIAN_POINT('Ctrl Pts',(3.49999590859855,-1.79402275342131,
18.4350351186233));
#258208=CARTESIAN_POINT('Ctrl Pts',(3.44710407083485,-1.89721052816843,
18.4291787198144));
#258209=CARTESIAN_POINT('Ctrl Pts',(3.38968238537155,-1.99798448502726,
18.4233223210056));
#258210=CARTESIAN_POINT('Ctrl Pts',(3.32799434560108,-2.09593478802352,
18.4174659221967));
#258211=CARTESIAN_POINT('Ctrl Pts',(3.26626468939241,-2.19395117097219,
18.4116055725011));
#258212=CARTESIAN_POINT('Ctrl Pts',(3.20026318330507,-2.28913976787733,
18.4057452228055));
#258213=CARTESIAN_POINT('Ctrl Pts',(3.13029491473867,-2.38112216124273,
18.3998848731099));
#258214=CARTESIAN_POINT('Ctrl Pts',(3.06022529354294,-2.47323779582747,
18.3940160343969));
#258215=CARTESIAN_POINT('Ctrl Pts',(2.98617770693884,-2.56213764191437,
18.3881471956839));
#258216=CARTESIAN_POINT('Ctrl Pts',(2.90849553066704,-2.64747856423614,
18.3822783569709));
#258217=CARTESIAN_POINT('Ctrl Pts',(2.89105048699147,-2.66664352830727,
18.3809603950833));
#258218=CARTESIAN_POINT('Ctrl Pts',(2.87342228256386,-2.68562916758781,
18.3796424331956));
#258219=CARTESIAN_POINT('Ctrl Pts',(2.85561503733998,-2.70443187352128,
18.378324471308));
#258220=CARTESIAN_POINT('Ctrl Pts',(2.77619379146872,-2.78829292626762,
18.3724462922967));
#258221=CARTESIAN_POINT('Ctrl Pts',(2.69294508776773,-2.86878994417562,
18.3665681132853));
#258222=CARTESIAN_POINT('Ctrl Pts',(2.60618517272479,-2.94555391148583,
18.3606899342739));
#258223=CARTESIAN_POINT('Ctrl Pts',(2.5195362893618,-3.02221963950839,18.3548192779081));
#258224=CARTESIAN_POINT('Ctrl Pts',(2.42938543727218,-3.09516154721246,
18.3489486215423));
#258225=CARTESIAN_POINT('Ctrl Pts',(2.33608716590236,-3.16404578874994,
18.3430779651765));
#258226=CARTESIAN_POINT('Ctrl Pts',(2.24288348542366,-3.23286019167526,
18.3372132608033));
#258227=CARTESIAN_POINT('Ctrl Pts',(2.14653906301677,-3.29762486813221,
18.33134855643));
#258228=CARTESIAN_POINT('Ctrl Pts',(2.04744263576382,-3.35804521310486,
18.3254838520568));
#258229=CARTESIAN_POINT('Ctrl Pts',(1.94540402006663,-3.42025944758195,
18.3194450236922));
#258230=CARTESIAN_POINT('Ctrl Pts',(1.84044776017657,-3.47786705033665,
18.3134061953277));
#258231=CARTESIAN_POINT('Ctrl Pts',(1.73303209652776,-3.53059325785407,
18.3073673669632));
#258232=CARTESIAN_POINT('Ctrl Pts',(1.62883166012331,-3.581741234291,18.3015092962724));
#258233=CARTESIAN_POINT('Ctrl Pts',(1.52231735461547,-3.62829569046279,
18.2956512255816));
#258234=CARTESIAN_POINT('Ctrl Pts',(1.41393308472613,-3.67005207482358,
18.2897931548907));
#258235=CARTESIAN_POINT('Ctrl Pts',(1.30556466749011,-3.71180235175304,
18.2839359410213));
#258236=CARTESIAN_POINT('Ctrl Pts',(1.1953272144696,-3.74875580416738,18.2780787271519));
#258237=CARTESIAN_POINT('Ctrl Pts',(1.08368403454574,-3.78075626208179,
18.2722215132825));
#258238=CARTESIAN_POINT('Ctrl Pts',(0.97203030496013,-3.81275974386212,
18.2663637459389));
#258239=CARTESIAN_POINT('Ctrl Pts',(0.858970980853819,-3.83980918710216,
18.2605059785952));
#258240=CARTESIAN_POINT('Ctrl Pts',(0.744983253302858,-3.86179866801705,
18.2546482112516));
#258241=CARTESIAN_POINT('Ctrl Pts',(0.630957311268464,-3.88379552092428,
18.2487884800864));
#258242=CARTESIAN_POINT('Ctrl Pts',(0.516002751566652,-3.90072896020009,
18.2429287489213));
#258243=CARTESIAN_POINT('Ctrl Pts',(0.400604948507621,-3.91254452693272,
18.2370690177561));
#258244=CARTESIAN_POINT('Ctrl Pts',(0.285077628217789,-3.92437335491854,
18.2312027098959));
#258245=CARTESIAN_POINT('Ctrl Pts',(0.169106482113305,-3.9310728038183,
18.2253364020358));
#258246=CARTESIAN_POINT('Ctrl Pts',(0.05318006704996,-3.93264044637551,
18.2194700941756));
#258247=CARTESIAN_POINT('Ctrl Pts',(-0.0628245292563574,-3.93420914615719,
18.2135998300537));
#258248=CARTESIAN_POINT('Ctrl Pts',(-0.178783923287657,-3.93063916050815,
18.2077295659318));
#258249=CARTESIAN_POINT('Ctrl Pts',(-0.294213214673637,-3.9219800591425,
18.2018593018099));
#258250=CARTESIAN_POINT('Ctrl Pts',(-0.409808110012898,-3.91330853474799,
18.1959806157447));
#258251=CARTESIAN_POINT('Ctrl Pts',(-0.524870977130521,-3.89953337277573,
18.1901019296795));
#258252=CARTESIAN_POINT('Ctrl Pts',(-0.638925607187836,-3.88075547651223,
18.1842232436143));
#258253=CARTESIAN_POINT('Ctrl Pts',(-0.662668191845239,-3.87684650945407,
18.1829994861789));
#258254=CARTESIAN_POINT('Ctrl Pts',(-0.68636713462133,-3.87272092654932,
18.1817757287435));
#258255=CARTESIAN_POINT('Ctrl Pts',(-0.710018223193508,-3.8683799093074,
18.180551971308));
#258256=CARTESIAN_POINT('Ctrl Pts',(-0.823612685446079,-3.84753031848538,
18.1746743531434));
#258257=CARTESIAN_POINT('Ctrl Pts',(-0.93647409787697,-3.82163880661589,
18.1687967349788));
#258258=CARTESIAN_POINT('Ctrl Pts',(-1.04812076214779,-3.79076929764325,
18.1629191168142));
#258259=CARTESIAN_POINT('Ctrl Pts',(-1.15962482068919,-3.75993921814102,
18.1570490061021));
#258260=CARTESIAN_POINT('Ctrl Pts',(-1.26991682277623,-3.72414389573843,
18.15117889539));
#258261=CARTESIAN_POINT('Ctrl Pts',(-1.37852367281272,-3.68349853854931,
18.1453087846778));
#258262=CARTESIAN_POINT('Ctrl Pts',(-1.48702069364622,-3.64289428417447,
18.1394446101436));
#258263=CARTESIAN_POINT('Ctrl Pts',(-1.5938355681219,-3.59744989487158,
18.1335804356094));
#258264=CARTESIAN_POINT('Ctrl Pts',(-1.69850946074777,-3.54733063186255,
18.1277162610751));
#258265=CARTESIAN_POINT('Ctrl Pts',(-1.80630452693748,-3.49571690910983,
18.1216772281681));
#258266=CARTESIAN_POINT('Ctrl Pts',(-1.911828495614,-3.43914525844542,18.1156381952612));
#258267=CARTESIAN_POINT('Ctrl Pts',(-2.01460110954849,-3.37785011055938,
18.1095991623542));
#258268=CARTESIAN_POINT('Ctrl Pts',(-2.11428581510268,-3.31839663813125,
18.1037415783723));
#258269=CARTESIAN_POINT('Ctrl Pts',(-2.21138176076628,-3.25449968645423,
18.0978839943904));
#258270=CARTESIAN_POINT('Ctrl Pts',(-2.30547553699735,-3.18641986378236,
18.0920264104085));
#258271=CARTESIAN_POINT('Ctrl Pts',(-2.39955582200104,-3.11834980244013,
18.0861696662908));
#258272=CARTESIAN_POINT('Ctrl Pts',(-2.49063445943363,-3.04609830442356,
18.0803129221731));
#258273=CARTESIAN_POINT('Ctrl Pts',(-2.57832802573415,-2.96996861796784,
18.0744561780554));
#258274=CARTESIAN_POINT('Ctrl Pts',(-2.66603014227994,-2.89383150876131,
18.068598862897));
#258275=CARTESIAN_POINT('Ctrl Pts',(-2.75034622007518,-2.81381572982717,
18.0627415477386));
#258276=CARTESIAN_POINT('Ctrl Pts',(-2.8309273955115,-2.73026355528957,
18.0568842325802));
#258277=CARTESIAN_POINT('Ctrl Pts',(-2.91153583817867,-2.64668310818809,
18.0510249354109));
#258278=CARTESIAN_POINT('Ctrl Pts',(-2.9884065791666,-2.55956418264079,
18.0451656382416));
#258279=CARTESIAN_POINT('Ctrl Pts',(-3.06122944348281,-2.46928396389599,
18.0393063410724));
#258280=CARTESIAN_POINT('Ctrl Pts',(-3.13413441001506,-2.37890196110175,
18.0334404379932));
#258281=CARTESIAN_POINT('Ctrl Pts',(-3.20298213222088,-2.28535187275344,
18.027574534914));
#258282=CARTESIAN_POINT('Ctrl Pts',(-3.26750432365938,-2.18904191254239,
18.0217086318348));
#258283=CARTESIAN_POINT('Ctrl Pts',(-3.3320702153965,-2.09266672246349,
18.0158387558323));
#258284=CARTESIAN_POINT('Ctrl Pts',(-3.39230452897062,-1.99352828995328,
18.0099688798298));
#258285=CARTESIAN_POINT('Ctrl Pts',(-3.44798456722994,-1.89206010056345,
18.0040990038274));
#258286=CARTESIAN_POINT('Ctrl Pts',(-3.5037447516381,-1.79044585731188,
17.9982206786935));
#258287=CARTESIAN_POINT('Ctrl Pts',(-3.5549373969427,-1.68649553343672,
17.9923423535597));
#258288=CARTESIAN_POINT('Ctrl Pts',(-3.60138758242706,-1.580663304167,17.9864640284259));
#258289=CARTESIAN_POINT('Ctrl Pts',(-3.61109263489564,-1.55855128615849,
17.98523584272));
#258290=CARTESIAN_POINT('Ctrl Pts',(-3.62059083489173,-1.53635716961777,
17.984007657014));
#258291=CARTESIAN_POINT('Ctrl Pts',(-3.62988086315592,-1.51408517570659,
17.9827794713081));
#258292=CARTESIAN_POINT('Ctrl Pts',(-3.67943525765663,-1.39528304279522,
17.9762281458156));
#258293=CARTESIAN_POINT('Ctrl Pts',(-3.72320130331636,-1.27393123983944,
17.9696768203231));
#258294=CARTESIAN_POINT('Ctrl Pts',(-3.76093818682342,-1.15057939964759,
17.9631254948306));
#258295=CARTESIAN_POINT('Ctrl Pts',(-3.79845718965327,-1.02793975346797,
17.956611994593));
#258296=CARTESIAN_POINT('Ctrl Pts',(-3.8300163393861,-0.903323327055673,
17.9500984943553));
#258297=CARTESIAN_POINT('Ctrl Pts',(-3.85542529309697,-0.777293258267532,
17.9435849941176));
#258298=CARTESIAN_POINT('Ctrl Pts',(-3.88105557945092,-0.65016536512386,
17.9370147559977));
#258299=CARTESIAN_POINT('Ctrl Pts',(-3.90042783164738,-0.521599290631718,
17.9304445178778));
#258300=CARTESIAN_POINT('Ctrl Pts',(-3.91339665537872,-0.392193342205873,
17.9238742797579));
#258301=CARTESIAN_POINT('Ctrl Pts',(-3.92636547911007,-0.262787393780027,
17.917304041638));
#258302=CARTESIAN_POINT('Ctrl Pts',(-3.93293072645011,-0.132541816141693,
17.9107338035181));
#258303=CARTESIAN_POINT('Ctrl Pts',(-3.93299945431987,-0.00207179139282337,
17.9041635653982));
#258304=CARTESIAN_POINT('',(-3.93113584355659,0.00341903309056729,16.654163522035));
#258305=CARTESIAN_POINT('Ctrl Pts',(-3.92772530458877,-0.00206815318150977,
17.904163522035));
#258306=CARTESIAN_POINT('Ctrl Pts',(-3.92400119087583,0.785602615821928,
17.8644446717927));
#258307=CARTESIAN_POINT('Ctrl Pts',(-3.31313291637687,2.88598162922864,
17.7588016548837));
#258308=CARTESIAN_POINT('Ctrl Pts',(0.103372134188801,4.64201135434511,
17.587234471308));
#258309=CARTESIAN_POINT('Ctrl Pts',(3.94766405912961,2.44442860147959,17.3894619713081));
#258310=CARTESIAN_POINT('Ctrl Pts',(4.20154746985927,-1.97643607916758,
17.191689471308));
#258311=CARTESIAN_POINT('Ctrl Pts',(0.634085622619158,-4.59968875606274,
16.993916971308));
#258312=CARTESIAN_POINT('Ctrl Pts',(-3.12038746571605,-3.18621803741959,
16.8147416548837));
#258313=CARTESIAN_POINT('Ctrl Pts',(-3.92323046052567,-0.9330686808722,
16.701490505126));
#258314=CARTESIAN_POINT('Ctrl Pts',(-3.93113584355659,0.00341903309056729,
16.654163522035));
#258315=CARTESIAN_POINT('',(-3.93909859392385,-0.000902565702873282,15.404163522035));
#258316=CARTESIAN_POINT('Ctrl Pts',(-3.93113584355659,0.00341903309056729,
16.654163522035));
#258317=CARTESIAN_POINT('Ctrl Pts',(-3.93424227143049,0.371412782013792,
16.6355663384593));
#258318=CARTESIAN_POINT('Ctrl Pts',(-3.71846148902814,2.04031595755692,
16.5510449882172));
#258319=CARTESIAN_POINT('Ctrl Pts',(-1.35548843458597,4.44093334314415,
16.4005994713079));
#258320=CARTESIAN_POINT('Ctrl Pts',(2.98365116613823,3.55767782069685,16.2028269713081));
#258321=CARTESIAN_POINT('Ctrl Pts',(4.60914037559767,-0.561310729341494,
16.005054471308));
#258322=CARTESIAN_POINT('Ctrl Pts',(2.04258527805945,-4.16978279364218,
15.807281971308));
#258323=CARTESIAN_POINT('Ctrl Pts',(-2.38171473979766,-3.98580973400276,
15.609509471308));
#258324=CARTESIAN_POINT('Ctrl Pts',(-3.91594831015911,-1.3977922893583,
15.4751366548837));
#258325=CARTESIAN_POINT('Ctrl Pts',(-3.93925372265761,-0.0505946126246084,
15.406688005126));
#258326=CARTESIAN_POINT('Ctrl Pts',(-3.93909859392385,-0.000902565702873282,
15.404163522035));
#258327=CARTESIAN_POINT('',(-3.93161494696421,-0.00266436291445193,14.1541639891901));
#258328=CARTESIAN_POINT('Ctrl Pts',(-3.93909859392385,-0.000902565702873282,
15.404163522035));
#258329=CARTESIAN_POINT('Ctrl Pts',(-3.93520270225845,1.24705986361814,
15.3407638384593));
#258330=CARTESIAN_POINT('Ctrl Pts',(-2.62185579271932,3.79973940462817,
15.2114399882171));
#258331=CARTESIAN_POINT('Ctrl Pts',(1.71950142291712,4.31306839047415,15.016191971308));
#258332=CARTESIAN_POINT('Ctrl Pts',(4.55309266773441,0.910269848327174,
14.818419471308));
#258333=CARTESIAN_POINT('Ctrl Pts',(3.24561556297038,-3.32042521907114,
14.620646971308));
#258334=CARTESIAN_POINT('Ctrl Pts',(-1.01377068166446,-4.53117126656537,
14.422874471308));
#258335=CARTESIAN_POINT('Ctrl Pts',(-3.63768788039038,-2.24294951629792,
14.267380475811));
#258336=CARTESIAN_POINT('Ctrl Pts',(-3.93159311262421,-0.471316921337659,
14.1778106469806));
#258337=CARTESIAN_POINT('Ctrl Pts',(-3.92866495709156,-0.00268210302728455,
14.1541649848169));
#258338=CARTESIAN_POINT('',(-3.93299876508478,0.00311670364493707,12.9041635219956));
#258339=CARTESIAN_POINT('Ctrl Pts',(-3.93299910315985,-0.00265603912754121,
14.154163522035));
#258340=CARTESIAN_POINT('Ctrl Pts',(-3.9330778785801,0.113992715771548,
14.148284295995));
#258341=CARTESIAN_POINT('Ctrl Pts',(-3.92796280482098,0.230678078603042,
14.142405069955));
#258342=CARTESIAN_POINT('Ctrl Pts',(-3.91767077265389,0.346907360967524,
14.136525843915));
#258343=CARTESIAN_POINT('Ctrl Pts',(-3.90737884254069,0.463135490823962,
14.1306466761723));
#258344=CARTESIAN_POINT('Ctrl Pts',(-3.8919100916819,0.578907143014563,
14.1247675084296));
#258345=CARTESIAN_POINT('Ctrl Pts',(-3.87133335419905,0.693734142641077,
14.118888340687));
#258346=CARTESIAN_POINT('Ctrl Pts',(-3.85075201344031,0.808586830516746,
14.1130078577002));
#258347=CARTESIAN_POINT('Ctrl Pts',(-3.82506048462843,0.922494044084642,
14.1071273747135));
#258348=CARTESIAN_POINT('Ctrl Pts',(-3.79437872290933,1.03497782929536,
14.1012468917268));
#258349=CARTESIAN_POINT('Ctrl Pts',(-3.76223968652257,1.1528041946425,14.0950871066919));
#258350=CARTESIAN_POINT('Ctrl Pts',(-3.72462484474384,1.26906810645793,
14.088927321657));
#258351=CARTESIAN_POINT('Ctrl Pts',(-3.68173017534728,1.38323964515817,
14.0827675366221));
#258352=CARTESIAN_POINT('Ctrl Pts',(-3.64070817178212,1.49242676172739,
14.0768766712252));
#258353=CARTESIAN_POINT('Ctrl Pts',(-3.59485785034093,1.59969999551068,
14.0709858058282));
#258354=CARTESIAN_POINT('Ctrl Pts',(-3.54439896097547,1.70461872729242,
14.0650949404312));
#258355=CARTESIAN_POINT('Ctrl Pts',(-3.49390086133653,1.8096189886563,14.059199497398));
#258356=CARTESIAN_POINT('Ctrl Pts',(-3.43878725398647,1.91226074630146,
14.0533040543647));
#258357=CARTESIAN_POINT('Ctrl Pts',(-3.37932260894418,2.01213014108896,
14.0474086113315));
#258358=CARTESIAN_POINT('Ctrl Pts',(-3.31976746413456,2.11215152798851,
14.0415041959715));
#258359=CARTESIAN_POINT('Ctrl Pts',(-3.25584828985909,2.20939179302548,
14.0355997806116));
#258360=CARTESIAN_POINT('Ctrl Pts',(-3.18787143305446,2.30346797813977,
14.0296953652516));
#258361=CARTESIAN_POINT('Ctrl Pts',(-3.17879201118603,2.31603339249659,
14.0289067339371));
#258362=CARTESIAN_POINT('Ctrl Pts',(-3.16964025615249,2.3285424115323,14.0281181026225));
#258363=CARTESIAN_POINT('Ctrl Pts',(-3.16041694862804,2.34099417146319,
14.027329471308));
#258364=CARTESIAN_POINT('Ctrl Pts',(-3.09168960483071,2.43377828208552,
14.0214529963733));
#258365=CARTESIAN_POINT('Ctrl Pts',(-3.01875971553102,2.52368598879652,
14.0155765214385));
#258366=CARTESIAN_POINT('Ctrl Pts',(-2.94189651046244,2.61031299305828,
14.0097000465037));
#258367=CARTESIAN_POINT('Ctrl Pts',(-2.8651317994684,2.69682899171461,14.0038311018035));
#258368=CARTESIAN_POINT('Ctrl Pts',(-2.78444406782172,2.78007234256194,
13.9979621571032));
#258369=CARTESIAN_POINT('Ctrl Pts',(-2.70014481638619,2.85966903164384,
13.992093212403));
#258370=CARTESIAN_POINT('Ctrl Pts',(-2.61593113489753,2.93918492422589,
13.9862302251137));
#258371=CARTESIAN_POINT('Ctrl Pts',(-2.52811352405206,3.01506123645907,
13.9803672378245));
#258372=CARTESIAN_POINT('Ctrl Pts',(-2.43704216015887,3.08695878003063,
13.9745042505352));
#258373=CARTESIAN_POINT('Ctrl Pts',(-2.34322944318998,3.16102052257517,
13.9684647805674));
#258374=CARTESIAN_POINT('Ctrl Pts',(-2.24596427876282,3.23085983307217,
13.9624253105996));
#258375=CARTESIAN_POINT('Ctrl Pts',(-2.14566873027637,3.29614846448308,
13.9563858406318));
#258376=CARTESIAN_POINT('Ctrl Pts',(-2.0484141738828,3.35945752436892,13.9505294892639));
#258377=CARTESIAN_POINT('Ctrl Pts',(-1.94831071920802,3.4184876422181,13.9446731378961));
#258378=CARTESIAN_POINT('Ctrl Pts',(-1.84577418286868,3.47298238778366,
13.9388167865282));
#258379=CARTESIAN_POINT('Ctrl Pts',(-1.74325260953445,3.52746918101158,
13.932961289769));
#258380=CARTESIAN_POINT('Ctrl Pts',(-1.63829902486732,3.57742172440048,
13.9271057930098));
#258381=CARTESIAN_POINT('Ctrl Pts',(-1.53135433771683,3.6226292789017,13.9212502962506));
#258382=CARTESIAN_POINT('Ctrl Pts',(-1.42439946656333,3.6678411383748,13.9153942418911));
#258383=CARTESIAN_POINT('Ctrl Pts',(-1.315453496126,3.70830695004004,13.9095381875316));
#258384=CARTESIAN_POINT('Ctrl Pts',(-1.20497716694659,3.74386418385301,
13.903682133172));
#258385=CARTESIAN_POINT('Ctrl Pts',(-1.0944636756262,3.77943337844478,13.8978241089469));
#258386=CARTESIAN_POINT('Ctrl Pts',(-0.982419194522758,3.81009058551966,
13.8919660847218));
#258387=CARTESIAN_POINT('Ctrl Pts',(-0.869318781506862,3.83572338107422,
13.8861080604966));
#258388=CARTESIAN_POINT('Ctrl Pts',(-0.756091053279677,3.86138503103076,
13.8802434419933));
#258389=CARTESIAN_POINT('Ctrl Pts',(-0.64180542340723,3.88201088972378,
13.8743788234899));
#258390=CARTESIAN_POINT('Ctrl Pts',(-0.526946369473274,3.89753980399161,
13.8685142049866));
#258391=CARTESIAN_POINT('Ctrl Pts',(-0.412009668866924,3.91307921606938,
13.8626456219014));
#258392=CARTESIAN_POINT('Ctrl Pts',(-0.296499182246349,3.92351478552903,
13.8567770388163));
#258393=CARTESIAN_POINT('Ctrl Pts',(-0.180902007055634,3.92883741886111,
13.8509084557312));
#258394=CARTESIAN_POINT('Ctrl Pts',(-0.0651384508610817,3.93416771315096,
13.8450314258934));
#258395=CARTESIAN_POINT('Ctrl Pts',(0.050711631895831,3.93437038447231,
13.8391543960556));
#258396=CARTESIAN_POINT('Ctrl Pts',(0.166163602504942,3.92948834547229,
13.8332773662179));
#258397=CARTESIAN_POINT('Ctrl Pts',(0.190525507278744,3.92845817016569,
13.8320372345813));
#258398=CARTESIAN_POINT('Ctrl Pts',(0.214869714223744,3.9272017725209,13.8307971029446));
#258399=CARTESIAN_POINT('Ctrl Pts',(0.23919172235873,3.92571984735985,13.829556971308));
#258400=CARTESIAN_POINT('Ctrl Pts',(0.354443738328614,3.91869761213242,
13.8236804963725));
#258401=CARTESIAN_POINT('Ctrl Pts',(0.46957595871394,3.90658413568195,13.817804021437));
#258402=CARTESIAN_POINT('Ctrl Pts',(0.584102673278668,3.88938466432271,
13.8119275465015));
#258403=CARTESIAN_POINT('Ctrl Pts',(0.698482630981103,3.87220723271603,
13.8060586018005));
#258404=CARTESIAN_POINT('Ctrl Pts',(0.812258221494294,3.84995682811163,
13.8001896570996));
#258405=CARTESIAN_POINT('Ctrl Pts',(0.924946073218048,3.82269064425027,
13.7943207123986));
#258406=CARTESIAN_POINT('Ctrl Pts',(1.03751953847568,3.79545213757298,13.7884577251086));
#258407=CARTESIAN_POINT('Ctrl Pts',(1.14900706246548,3.76320807563182,13.7825947378186));
#258408=CARTESIAN_POINT('Ctrl Pts',(1.25893337942031,3.72606706141762,13.7767317505286));
#258409=CARTESIAN_POINT('Ctrl Pts',(1.37216860526202,3.68780805985148,13.7706922805611));
#258410=CARTESIAN_POINT('Ctrl Pts',(1.48374670444182,3.64435268868069,13.7646528105936));
#258411=CARTESIAN_POINT('Ctrl Pts',(1.59316238680228,3.59587577778744,13.7586133406261));
#258412=CARTESIAN_POINT('Ctrl Pts',(1.69926055180413,3.54886870183842,13.7527569892575));
#258413=CARTESIAN_POINT('Ctrl Pts',(1.80332513603157,3.49714038499151,13.7469006378889));
#258414=CARTESIAN_POINT('Ctrl Pts',(1.90491445763304,3.44089957846791,13.7410442865203));
#258415=CARTESIAN_POINT('Ctrl Pts',(2.00648895445501,3.38466697908205,13.7351887897603));
#258416=CARTESIAN_POINT('Ctrl Pts',(2.10558854597426,3.32392339926162,13.7293332930004));
#258417=CARTESIAN_POINT('Ctrl Pts',(2.20179617070332,3.25892353740866,13.7234777962405));
#258418=CARTESIAN_POINT('Ctrl Pts',(2.29801295697871,3.19391748582545,13.7176217418803));
#258419=CARTESIAN_POINT('Ctrl Pts',(2.39133688705236,3.12465457751915,13.71176568752));
#258420=CARTESIAN_POINT('Ctrl Pts',(2.48138049870848,3.05143242111459,13.7059096331598));
#258421=CARTESIAN_POINT('Ctrl Pts',(2.57145439932694,2.97818563416605,13.700051608934));
#258422=CARTESIAN_POINT('Ctrl Pts',(2.65824546736195,2.9009772110248,13.6941935847082));
#258423=CARTESIAN_POINT('Ctrl Pts',(2.74140043679727,2.82014408233475,13.6883355604823));
#258424=CARTESIAN_POINT('Ctrl Pts',(2.82464901236726,2.73921996116667,13.6824709419783));
#258425=CARTESIAN_POINT('Ctrl Pts',(2.90425302396592,2.65466327850392,13.6766063234742));
#258426=CARTESIAN_POINT('Ctrl Pts',(2.97989704860918,2.56684681656119,13.6707417049702));
#258427=CARTESIAN_POINT('Ctrl Pts',(3.05559220989862,2.47897098919779,13.6648731218844));
#258428=CARTESIAN_POINT('Ctrl Pts',(3.12732179899887,2.38783131792171,13.6590045387986));
#258429=CARTESIAN_POINT('Ctrl Pts',(3.19481260479563,2.29383116646343,13.6531359557127));
#258430=CARTESIAN_POINT('Ctrl Pts',(3.26240055127037,2.19969571896985,13.6472589258743));
#258431=CARTESIAN_POINT('Ctrl Pts',(3.32573731448605,2.10269191915057,13.6413818960359));
#258432=CARTESIAN_POINT('Ctrl Pts',(3.3845946194405,2.00324942582156,13.6355048661975));
#258433=CARTESIAN_POINT('Ctrl Pts',(3.39701429528465,1.98226573427747,13.6342647345677));
#258434=CARTESIAN_POINT('Ctrl Pts',(3.40923468476728,1.96117353142325,13.6330246029378));
#258435=CARTESIAN_POINT('Ctrl Pts',(3.42125391619583,1.9399769691712,13.631784471308));
#258436=CARTESIAN_POINT('Ctrl Pts',(3.47820812214531,1.83953515813686,13.6259079963713));
#258437=CARTESIAN_POINT('Ctrl Pts',(3.53082914630815,1.73641778663748,13.6200315214345));
#258438=CARTESIAN_POINT('Ctrl Pts',(3.57885655466612,1.63103487428178,13.6141550464978));
#258439=CARTESIAN_POINT('Ctrl Pts',(3.62682241972617,1.52578700173337,13.6082861017955));
#258440=CARTESIAN_POINT('Ctrl Pts',(3.67020620576742,1.41827973399494,13.6024171570933));
#258441=CARTESIAN_POINT('Ctrl Pts',(3.70879230016866,1.3089494544136,13.596548212391));
#258442=CARTESIAN_POINT('Ctrl Pts',(3.74733922684326,1.19973015311524,13.5906852250997));
#258443=CARTESIAN_POINT('Ctrl Pts',(3.78109801249512,1.08869190775323,13.5848222378084));
#258444=CARTESIAN_POINT('Ctrl Pts',(3.80990055930484,0.976292337473103,
13.5789592505172));
#258445=CARTESIAN_POINT('Ctrl Pts',(3.83957009597436,0.860509410564029,
13.5729197805501));
#258446=CARTESIAN_POINT('Ctrl Pts',(3.86398009968608,0.743282309532098,
13.5668803105831));
#258447=CARTESIAN_POINT('Ctrl Pts',(3.88300161831438,0.625129932228423,
13.560840840616));
#258448=CARTESIAN_POINT('Ctrl Pts',(3.90144639861543,0.510559971543423,
13.5549844892461));
#258449=CARTESIAN_POINT('Ctrl Pts',(3.91482467444911,0.395120471390472,
13.5491281378762));
#258450=CARTESIAN_POINT('Ctrl Pts',(3.9230706113381,0.279295503822177,13.5432717865062));
#258451=CARTESIAN_POINT('Ctrl Pts',(3.93131534490975,0.163487438419818,
13.537416289745));
#258452=CARTESIAN_POINT('Ctrl Pts',(3.93442919952694,0.0472944289759187,
13.5315607929837));
#258453=CARTESIAN_POINT('Ctrl Pts',(3.93239828128702,-0.0687950385629423,
13.5257052962225));
#258454=CARTESIAN_POINT('Ctrl Pts',(3.93036716964921,-0.184895560933151,
13.5198492418609));
#258455=CARTESIAN_POINT('Ctrl Pts',(3.92319031845648,-0.300892109174371,
13.5139931874993));
#258456=CARTESIAN_POINT('Ctrl Pts',(3.91090594330545,-0.416297613034404,
13.5081371331377));
#258457=CARTESIAN_POINT('Ctrl Pts',(3.89861743592375,-0.531741937115748,
13.5022791089105));
#258458=CARTESIAN_POINT('Ctrl Pts',(3.88121803186177,-0.646594411352283,
13.4964210846833));
#258459=CARTESIAN_POINT('Ctrl Pts',(3.85879755477098,-0.760375191134925,
13.4905630604562));
#258460=CARTESIAN_POINT('Ctrl Pts',(3.83635183933042,-0.874284052006421,
13.4846984419508));
#258461=CARTESIAN_POINT('Ctrl Pts',(3.80887384969728,-0.987118405537053,
13.4788338234453));
#258462=CARTESIAN_POINT('Ctrl Pts',(3.77650409680879,-1.09841058206228,
13.4729692049399));
#258463=CARTESIAN_POINT('Ctrl Pts',(3.74411246141731,-1.20977799398997,
13.4671006218528));
#258464=CARTESIAN_POINT('Ctrl Pts',(3.70682261015782,-1.31960076317401,
13.4612320387656));
#258465=CARTESIAN_POINT('Ctrl Pts',(3.66482370558852,-1.42742993066436,
13.4553634556784));
#258466=CARTESIAN_POINT('Ctrl Pts',(3.62276435127318,-1.53541429853093,
13.4494864258386));
#258467=CARTESIAN_POINT('Ctrl Pts',(3.57598258358747,-1.64139896238258,
13.4436093959988));
#258468=CARTESIAN_POINT('Ctrl Pts',(3.52471410888429,-1.74495829481166,
13.437732366159));
#258469=CARTESIAN_POINT('Ctrl Pts',(3.51389577748777,-1.76681069404737,
13.436492234542));
#258470=CARTESIAN_POINT('Ctrl Pts',(3.50287782348456,-1.78855520180486,
13.435252102925));
#258471=CARTESIAN_POINT('Ctrl Pts',(3.49166270678754,-1.81018798527365,
13.434011971308));
#258472=CARTESIAN_POINT('Ctrl Pts',(3.4385188700611,-1.91269687070594,13.4281354963722));
#258473=CARTESIAN_POINT('Ctrl Pts',(3.38076952327136,-2.01303219564053,
13.4222590214364));
#258474=CARTESIAN_POINT('Ctrl Pts',(3.31861637510571,-2.11075208276107,
13.4163825465005));
#258475=CARTESIAN_POINT('Ctrl Pts',(3.25654287124843,-2.20834674963047,
13.4105136017992));
#258476=CARTESIAN_POINT('Ctrl Pts',(3.19007700817169,-2.30333229878898,
13.4046446570979));
#258477=CARTESIAN_POINT('Ctrl Pts',(3.11946703335963,-2.39529005086701,
13.3987757123966));
#258478=CARTESIAN_POINT('Ctrl Pts',(3.04892873287071,-2.48715445905622,
13.3929127251062));
#258479=CARTESIAN_POINT('Ctrl Pts',(2.97425493800888,-2.57599685827205,
13.3870497378159));
#258480=CARTESIAN_POINT('Ctrl Pts',(2.89573760499766,-2.66142682089935,
13.3811867505256));
#258481=CARTESIAN_POINT('Ctrl Pts',(2.81485680973775,-2.74942832389657,
13.3751472805582));
#258482=CARTESIAN_POINT('Ctrl Pts',(2.72989765575555,-2.83380831947677,
13.3691078105908));
#258483=CARTESIAN_POINT('Ctrl Pts',(2.6412248117809,-2.91417578289865,13.3630683406234));
#258484=CARTESIAN_POINT('Ctrl Pts',(2.55524055587679,-2.99210647995857,
13.3572119892544));
#258485=CARTESIAN_POINT('Ctrl Pts',(2.46576489163852,-3.06626416307308,
13.3513556378854));
#258486=CARTESIAN_POINT('Ctrl Pts',(2.37316770886201,-3.13632970613975,
13.3454992865164));
#258487=CARTESIAN_POINT('Ctrl Pts',(2.28058403865545,-3.20638502464533,
13.3396437897562));
#258488=CARTESIAN_POINT('Ctrl Pts',(2.18488008469697,-3.27234914160957,
13.3337882929959));
#258489=CARTESIAN_POINT('Ctrl Pts',(2.08645775726643,-3.33394406478914,
13.3279327962356));
#258490=CARTESIAN_POINT('Ctrl Pts',(1.98802605738985,-3.39554485345786,
13.3220767418749));
#258491=CARTESIAN_POINT('Ctrl Pts',(1.88687581927528,-3.45277540231397,
13.3162206875143));
#258492=CARTESIAN_POINT('Ctrl Pts',(1.78343617899,-3.50540217314213,13.3103646331536));
#258493=CARTESIAN_POINT('Ctrl Pts',(1.67996174357306,-3.55804664661711,
13.3045066089274));
#258494=CARTESIAN_POINT('Ctrl Pts',(1.57419674222064,-3.60608407561705,
13.2986485847012));
#258495=CARTESIAN_POINT('Ctrl Pts',(1.46659239303793,-3.64932812346098,
13.292790560475));
#258496=CARTESIAN_POINT('Ctrl Pts',(1.35886691546933,-3.69262085039414,
13.2869259419706));
#258497=CARTESIAN_POINT('Ctrl Pts',(1.24929834064817,-3.73110927279107,
13.2810613234661));
#258498=CARTESIAN_POINT('Ctrl Pts',(1.1383553177923,-3.76465618223683,13.2751967049617));
#258499=CARTESIAN_POINT('Ctrl Pts',(1.0273372955672,-3.7982257699636,13.2693281218754));
#258500=CARTESIAN_POINT('Ctrl Pts',(0.914943374010366,-3.82684709123545,
13.2634595387892));
#258501=CARTESIAN_POINT('Ctrl Pts',(0.8016530447359,-3.85043392306187,13.257590955703));
#258502=CARTESIAN_POINT('Ctrl Pts',(0.688199654741695,-3.87405470382108,
13.2517139258641));
#258503=CARTESIAN_POINT('Ctrl Pts',(0.573847687929116,-3.89262646845106,
13.2458368960253));
#258504=CARTESIAN_POINT('Ctrl Pts',(0.459082455495839,-3.90611473193708,
13.2399598661865));
#258505=CARTESIAN_POINT('Ctrl Pts',(0.434865461839885,-3.90896093530674,
13.2387197345603));
#258506=CARTESIAN_POINT('Ctrl Pts',(0.410630067428487,-3.91158097243245,
13.2374796029342));
#258507=CARTESIAN_POINT('Ctrl Pts',(0.386380826472741,-3.9139748155723,
13.236239471308));
#258508=CARTESIAN_POINT('Ctrl Pts',(0.271473623326335,-3.92531825599066,
13.230362996372));
#258509=CARTESIAN_POINT('Ctrl Pts',(0.155877324156971,-3.93161588281209,
13.224486521436));
#258510=CARTESIAN_POINT('Ctrl Pts',(0.0400723249525348,-3.93279585139795,
13.2186100465));
#258511=CARTESIAN_POINT('Ctrl Pts',(-0.0755842793700643,-3.93397430794806,
13.2127411017985));
#258512=CARTESIAN_POINT('Ctrl Pts',(-0.191448642919037,-3.93004814395898,
13.206872157097));
#258513=CARTESIAN_POINT('Ctrl Pts',(-0.307034440858103,-3.92099717573565,
13.2010032123955));
#258514=CARTESIAN_POINT('Ctrl Pts',(-0.422502910702303,-3.91195539491144,
13.195140225105));
#258515=CARTESIAN_POINT('Ctrl Pts',(-0.537692968378007,-3.89779918952418,
13.1892772378144));
#258516=CARTESIAN_POINT('Ctrl Pts',(-0.652118139763882,-3.87856042002582,
13.1834142505239));
#258517=CARTESIAN_POINT('Ctrl Pts',(-0.769987640727734,-3.85874254138545,
13.1773747805566));
#258518=CARTESIAN_POINT('Ctrl Pts',(-0.887045031542341,-3.83353125909403,
13.1713353105893));
#258519=CARTESIAN_POINT('Ctrl Pts',(-1.00276369128009,-3.80301906114738,
13.1652958406219));
#258520=CARTESIAN_POINT('Ctrl Pts',(-1.1149737254482,-3.77343200248375,
13.1594394892528));
#258521=CARTESIAN_POINT('Ctrl Pts',(-1.22592461250148,-3.73886095797199,
13.1535831378836));
#258522=CARTESIAN_POINT('Ctrl Pts',(-1.33514715562305,-3.69944199479214,
13.1477267865145));
#258523=CARTESIAN_POINT('Ctrl Pts',(-1.44435376006093,-3.66002878396312,
13.141871289754));
#258524=CARTESIAN_POINT('Ctrl Pts',(-1.55183213403117,-3.61576920127481,
13.1360157929935));
#258525=CARTESIAN_POINT('Ctrl Pts',(-1.65713010316883,-3.56684858399844,
13.130160296233));
#258526=CARTESIAN_POINT('Ctrl Pts',(-1.76243809949759,-3.51792330816709,
13.1243042418722));
#258527=CARTESIAN_POINT('Ctrl Pts',(-1.86556490397208,-3.46433628928523,
13.1184481875114));
#258528=CARTESIAN_POINT('Ctrl Pts',(-1.96608076218818,-3.40631992574883,
13.1125921331505));
#258529=CARTESIAN_POINT('Ctrl Pts',(-2.06663043203135,-3.3482840466088,
13.1067341089241));
#258530=CARTESIAN_POINT('Ctrl Pts',(-2.16456705197183,-3.28581606623922,
13.1008760846977));
#258531=CARTESIAN_POINT('Ctrl Pts',(-2.25948839534632,-3.21919263034931,
13.0950180604714));
#258532=CARTESIAN_POINT('Ctrl Pts',(-2.35451659006255,-3.1524941975908,
13.0891534419667));
#258533=CARTESIAN_POINT('Ctrl Pts',(-2.44652239576883,-3.08163121032613,
13.0832888234621));
#258534=CARTESIAN_POINT('Ctrl Pts',(-2.53513526457622,-3.00692171336436,
13.0774242049575));
#258535=CARTESIAN_POINT('Ctrl Pts',(-2.62380803718929,-2.93216171151263,
13.0715556218711));
#258536=CARTESIAN_POINT('Ctrl Pts',(-2.70908300292042,-2.85355030105153,
13.0656870387847));
#258537=CARTESIAN_POINT('Ctrl Pts',(-2.7906264419413,-2.77144241533863,
13.0598184556982));
#258538=CARTESIAN_POINT('Ctrl Pts',(-2.87228724783648,-2.68921635033361,
13.0539414258592));
#258539=CARTESIAN_POINT('Ctrl Pts',(-2.95020553235073,-2.60348407114684,
13.0480643960202));
#258540=CARTESIAN_POINT('Ctrl Pts',(-3.02408777323364,-2.51463359950884,
13.0421873661812));
#258541=CARTESIAN_POINT('Ctrl Pts',(-3.03967791075394,-2.49588496580436,
13.0409472345568));
#258542=CARTESIAN_POINT('Ctrl Pts',(-3.05508849156538,-2.47699759080929,
13.0397071029324));
#258543=CARTESIAN_POINT('Ctrl Pts',(-3.07031700924428,-2.45797527708178,
13.038466971308));
#258544=CARTESIAN_POINT('Ctrl Pts',(-3.14227544215279,-2.36809023935273,
13.0326070491426));
#258545=CARTESIAN_POINT('Ctrl Pts',(-3.21040812691704,-2.27488676098109,
13.0267471269773));
#258546=CARTESIAN_POINT('Ctrl Pts',(-3.27439259146059,-2.17872489245154,
13.0208872048119));
#258547=CARTESIAN_POINT('Ctrl Pts',(-3.33829802090321,-2.08268180530181,
13.0150345209588));
#258548=CARTESIAN_POINT('Ctrl Pts',(-3.39806518766487,-1.98368793322563,
13.0091818371058));
#258549=CARTESIAN_POINT('Ctrl Pts',(-3.45341137449383,-1.88213678528332,
13.0033291532528));
#258550=CARTESIAN_POINT('Ctrl Pts',(-3.50870271804399,-1.78068626573544,
12.9974822689027));
#258551=CARTESIAN_POINT('Ctrl Pts',(-3.55958159431877,-1.67668387017918,
12.9916353845526));
#258552=CARTESIAN_POINT('Ctrl Pts',(-3.60580860118161,-1.57055191943619,
12.9857885002025));
#258553=CARTESIAN_POINT('Ctrl Pts',(-3.65200109233267,-1.46449921284228,
12.9799459814687));
#258554=CARTESIAN_POINT('Ctrl Pts',(-3.6935484568733,-1.35632049214502,
12.9741034627349));
#258555=CARTESIAN_POINT('Ctrl Pts',(-3.73025760894366,-1.24646186099611,
12.9682609440011));
#258556=CARTESIAN_POINT('Ctrl Pts',(-3.7669519298529,-1.13664761472043,
12.9624207857505));
#258557=CARTESIAN_POINT('Ctrl Pts',(-3.79881179126718,-1.02515519938419,
12.9565806274999));
#258558=CARTESIAN_POINT('Ctrl Pts',(-3.82569278444555,-0.912449296696138,
12.9507404692493));
#258559=CARTESIAN_POINT('Ctrl Pts',(-3.85256701909957,-0.79977173096654,
12.9449017793541));
#258560=CARTESIAN_POINT('Ctrl Pts',(-3.87446478275368,-0.685881688865453,
12.9390630894589));
#258561=CARTESIAN_POINT('Ctrl Pts',(-3.8912921706179,-0.57125672240054,
12.9332243995637));
#258562=CARTESIAN_POINT('Ctrl Pts',(-3.90812426445964,-0.456599699711643,
12.92738407681));
#258563=CARTESIAN_POINT('Ctrl Pts',(-3.91988308810419,-0.341207752495339,
12.9215437540563));
#258564=CARTESIAN_POINT('Ctrl Pts',(-3.92652632663352,-0.225565968740512,
12.9157034313026));
#258565=CARTESIAN_POINT('Ctrl Pts',(-3.93090179086183,-0.149400332675666,
12.9118567948801));
#258566=CARTESIAN_POINT('Ctrl Pts',(-3.933059183935,-0.0731264525454888,
12.9080101584575));
#258567=CARTESIAN_POINT('Ctrl Pts',(-3.9329987650854,0.00311670286490963,
12.904163522035));
#258568=CARTESIAN_POINT('',(-3.93299999997998,1.25478604955714E-5,11.6541635220815));
#258569=CARTESIAN_POINT('Ctrl Pts',(-3.93299876508478,0.00311670364493542,
12.9041635219957));
#258570=CARTESIAN_POINT('Ctrl Pts',(-3.93289051723057,0.13971572794475,
12.8972717980195));
#258571=CARTESIAN_POINT('Ctrl Pts',(-3.92566195699015,0.276017078558251,
12.8903800740433));
#258572=CARTESIAN_POINT('Ctrl Pts',(-3.91142917386115,0.411352425382229,
12.8834883500672));
#258573=CARTESIAN_POINT('Ctrl Pts',(-3.89669952620131,0.551412310829302,
12.8763560369407));
#258574=CARTESIAN_POINT('Ctrl Pts',(-3.874467964418,0.690437391631793,12.8692237238141));
#258575=CARTESIAN_POINT('Ctrl Pts',(-3.84491697545102,0.827709158997629,
12.8620914106876));
#258576=CARTESIAN_POINT('Ctrl Pts',(-3.81536598648405,0.964980926363465,
12.8549590975611));
#258577=CARTESIAN_POINT('Ctrl Pts',(-3.77849571199835,1.10049933560846,
12.8478267844346));
#258578=CARTESIAN_POINT('Ctrl Pts',(-3.73454091440123,1.23356927598867,
12.8406944713081));
#258579=CARTESIAN_POINT('Ctrl Pts',(-3.69832555736119,1.34320862517502,
12.8348179963721));
#258580=CARTESIAN_POINT('Ctrl Pts',(-3.65721828267301,1.45143226609062,
12.828941521436));
#258581=CARTESIAN_POINT('Ctrl Pts',(-3.61134817310259,1.55777192574156,
12.8230650465));
#258582=CARTESIAN_POINT('Ctrl Pts',(-3.56553684242359,1.66397531958963,
12.8171961017985));
#258583=CARTESIAN_POINT('Ctrl Pts',(-3.51497497647907,1.76829915778894,
12.8113271570969));
#258584=CARTESIAN_POINT('Ctrl Pts',(-3.45984128668686,1.87029069156027,
12.8054582123954));
#258585=CARTESIAN_POINT('Ctrl Pts',(-3.40476356164893,1.97217869641585,
12.7995952251049));
#258586=CARTESIAN_POINT('Ctrl Pts',(-3.34512343896653,2.07173874515476,
12.7937322378143));
#258587=CARTESIAN_POINT('Ctrl Pts',(-3.28114726590327,2.16853905186315,
12.7878692505237));
#258588=CARTESIAN_POINT('Ctrl Pts',(-3.215245336274,2.26825315940252,12.7818297805564));
#258589=CARTESIAN_POINT('Ctrl Pts',(-3.14474235240354,2.36503833783608,
12.7757903105891));
#258590=CARTESIAN_POINT('Ctrl Pts',(-3.0699363592589,2.45845068083544,12.7697508406218));
#258591=CARTESIAN_POINT('Ctrl Pts',(-2.9973985069728,2.5490307326915,12.7638944892526));
#258592=CARTESIAN_POINT('Ctrl Pts',(-2.92081509741286,2.63643918672693,
12.7580381378834));
#258593=CARTESIAN_POINT('Ctrl Pts',(-2.84050073232488,2.72030229747759,
12.7521817865142));
#258594=CARTESIAN_POINT('Ctrl Pts',(-2.76019808739336,2.80415317020857,
12.7463262897537));
#258595=CARTESIAN_POINT('Ctrl Pts',(-2.67616585492461,2.88445943047131,
12.7404707929932));
#258596=CARTESIAN_POINT('Ctrl Pts',(-2.5887567750199,2.96088286829935,12.7346152962327));
#258597=CARTESIAN_POINT('Ctrl Pts',(-2.50133937142617,3.03731358368861,
12.7287592418719));
#258598=CARTESIAN_POINT('Ctrl Pts',(-2.41054479183504,3.10986046998059,
12.722903187511));
#258599=CARTESIAN_POINT('Ctrl Pts',(-2.31675970719597,3.17822489121101,
12.7170471331502));
#258600=CARTESIAN_POINT('Ctrl Pts',(-2.22294307503436,3.24661230893526,
12.7111891089238));
#258601=CARTESIAN_POINT('Ctrl Pts',(-2.12613427078891,3.31081422103607,
12.7053310846974));
#258602=CARTESIAN_POINT('Ctrl Pts',(-2.02674925330031,3.37057509399311,
12.699473060471));
#258603=CARTESIAN_POINT('Ctrl Pts',(-1.92725235978758,3.43040323874858,
12.6936084419663));
#258604=CARTESIAN_POINT('Ctrl Pts',(-1.82517381881096,3.48578015379365,
12.6877438234617));
#258605=CARTESIAN_POINT('Ctrl Pts',(-1.7209545905739,3.53649604795235,12.681879204957));
#258606=CARTESIAN_POINT('Ctrl Pts',(-1.61666490836746,3.58724622691737,
12.6760106218706));
#258607=CARTESIAN_POINT('Ctrl Pts',(-1.51023203498892,3.63332894710027,
12.6701420387842));
#258608=CARTESIAN_POINT('Ctrl Pts',(-1.40211572117287,3.67458303817452,
12.6642734556977));
#258609=CARTESIAN_POINT('Ctrl Pts',(-1.29384379368602,3.7158965069719,12.6583964258587));
#258610=CARTESIAN_POINT('Ctrl Pts',(-1.18388398044833,3.75236734777742,
12.6525193960197));
#258611=CARTESIAN_POINT('Ctrl Pts',(-1.07270998281249,3.78388455066674,
12.6466423661806));
#258612=CARTESIAN_POINT('Ctrl Pts',(-1.04925078760107,3.79053510053291,
12.6454022345564));
#258613=CARTESIAN_POINT('Ctrl Pts',(-1.02573755873963,3.79696526409723,
12.6441621029322));
#258614=CARTESIAN_POINT('Ctrl Pts',(-1.00217478841056,3.80317429175606,
12.642921971308));
#258615=CARTESIAN_POINT('Ctrl Pts',(-0.890520487721301,3.83259632624208,
12.637045496372));
#258616=CARTESIAN_POINT('Ctrl Pts',(-0.777385639151944,3.85714567500466,
12.6311690214359));
#258617=CARTESIAN_POINT('Ctrl Pts',(-0.663233166504726,3.87667522070757,
12.6252925464998));
#258618=CARTESIAN_POINT('Ctrl Pts',(-0.549226971157995,3.89617974085336,
12.6194236017983));
#258619=CARTESIAN_POINT('Ctrl Pts',(-0.43420614817201,3.91067718146114,
12.6135546570967));
#258620=CARTESIAN_POINT('Ctrl Pts',(-0.318647667633408,3.92007049221207,
12.6076857123952));
#258621=CARTESIAN_POINT('Ctrl Pts',(-0.203206487460461,3.92945426806101,
12.6018227251046));
#258622=CARTESIAN_POINT('Ctrl Pts',(-0.0872291442570081,3.93374418671206,
12.595959737814));
#258623=CARTESIAN_POINT('Ctrl Pts',(0.0287989912652807,3.93289455974885,
12.5900967505234));
#258624=CARTESIAN_POINT('Ctrl Pts',(0.148319707432526,3.93201935803453,
12.5840572805561));
#258625=CARTESIAN_POINT('Ctrl Pts',(0.267893882975228,3.92569021573269,
12.5780178105888));
#258626=CARTESIAN_POINT('Ctrl Pts',(0.386986894000942,3.91391493825192,
12.5719783406215));
#258627=CARTESIAN_POINT('Ctrl Pts',(0.502468968083502,3.90249669082778,
12.5661219892523));
#258628=CARTESIAN_POINT('Ctrl Pts',(0.617498195405212,3.88595784810588,
12.5602656378831));
#258629=CARTESIAN_POINT('Ctrl Pts',(0.73158973869103,3.86435834961537,12.5544092865139));
#258630=CARTESIAN_POINT('Ctrl Pts',(0.845664632766857,3.84276200310769,
12.5485537897533));
#258631=CARTESIAN_POINT('Ctrl Pts',(0.9588017095401,3.81610654606005,12.5426982929928));
#258632=CARTESIAN_POINT('Ctrl Pts',(1.07052512546853,3.7845032640679,12.5368427962323));
#258633=CARTESIAN_POINT('Ctrl Pts',(1.18225918046291,3.75289697259561,12.5309867418714));
#258634=CARTESIAN_POINT('Ctrl Pts',(1.29257890989874,3.71634203187436,12.5251306875105));
#258635=CARTESIAN_POINT('Ctrl Pts',(1.40102314347583,3.67499974849592,12.5192746331496));
#258636=CARTESIAN_POINT('Ctrl Pts',(1.50950385563515,3.63364355835791,12.5134166089232));
#258637=CARTESIAN_POINT('Ctrl Pts',(1.6161074320524,3.58749697027091,12.5075585846968));
#258638=CARTESIAN_POINT('Ctrl Pts',(1.72039286503307,3.53676934361619,12.5017005604703));
#258639=CARTESIAN_POINT('Ctrl Pts',(1.82479569035204,3.48598461373488,12.4958359419656));
#258640=CARTESIAN_POINT('Ctrl Pts',(1.92687479272097,3.4306087335386,12.489971323461));
#258641=CARTESIAN_POINT('Ctrl Pts',(2.02621387723058,3.37089696130247,12.4841067049563));
#258642=CARTESIAN_POINT('Ctrl Pts',(2.12562011664947,3.31114482289358,12.4782381218698));
#258643=CARTESIAN_POINT('Ctrl Pts',(2.22228230672707,3.24705118323557,12.4723695387834));
#258644=CARTESIAN_POINT('Ctrl Pts',(2.31581466475513,3.1789135626036,12.4665009556969));
#258645=CARTESIAN_POINT('Ctrl Pts',(2.40948164551545,3.11067787032185,12.4606239258579));
#258646=CARTESIAN_POINT('Ctrl Pts',(2.50000948309522,3.03838683782404,12.4547468960188));
#258647=CARTESIAN_POINT('Ctrl Pts',(2.5870468365032,2.96237702964001,12.4488698661797));
#258648=CARTESIAN_POINT('Ctrl Pts',(2.60541287808837,2.94633794706996,12.4476297345558));
#258649=CARTESIAN_POINT('Ctrl Pts',(2.62362363686524,2.9301334045145,12.4463896029319));
#258650=CARTESIAN_POINT('Ctrl Pts',(2.64167603511197,2.91376675894195,12.445149471308));
#258651=CARTESIAN_POINT('Ctrl Pts',(2.72721894345236,2.83621194085533,12.439272996372));
#258652=CARTESIAN_POINT('Ctrl Pts',(2.80948446166904,2.75475919996778,12.4333965214359));
#258653=CARTESIAN_POINT('Ctrl Pts',(2.88809685722913,2.66971637880566,12.4275200464998));
#258654=CARTESIAN_POINT('Ctrl Pts',(2.96660851726647,2.58478253324447,12.4216511017982));
#258655=CARTESIAN_POINT('Ctrl Pts',(3.04147608666776,2.49626805670776,12.4157821570967));
#258656=CARTESIAN_POINT('Ctrl Pts',(3.11235814417319,2.40451986525352,12.4099132123951));
#258657=CARTESIAN_POINT('Ctrl Pts',(3.18316825117169,2.31286480496842,12.4040502251045));
#258658=CARTESIAN_POINT('Ctrl Pts',(3.25000064271123,2.21798288372013,12.3981872378139));
#258659=CARTESIAN_POINT('Ctrl Pts',(3.31255237255257,2.12025606451115,12.3923242505233));
#258660=CARTESIAN_POINT('Ctrl Pts',(3.37698698157607,2.01958755537781,12.386284780556));
#258661=CARTESIAN_POINT('Ctrl Pts',(3.43687883344845,1.9159004897512,12.3802453105887));
#258662=CARTESIAN_POINT('Ctrl Pts',(3.49194296937092,1.80964728570542,12.3742058406214));
#258663=CARTESIAN_POINT('Ctrl Pts',(3.54533754365489,1.70661571168199,12.3683494892522));
#258664=CARTESIAN_POINT('Ctrl Pts',(3.59419273431216,1.60117176068095,12.3624931378829));
#258665=CARTESIAN_POINT('Ctrl Pts',(3.63829443129475,1.49375454182059,12.3566367865137));
#258666=CARTESIAN_POINT('Ctrl Pts',(3.68238969258198,1.38635299819595,12.3507812897532));
#258667=CARTESIAN_POINT('Ctrl Pts',(3.72173268285892,1.27697914095696,12.3449257929926));
#258668=CARTESIAN_POINT('Ctrl Pts',(3.75615723803829,1.16609253626485,12.3390702962321));
#258669=CARTESIAN_POINT('Ctrl Pts',(3.7905850713587,1.05519537219359,12.3332142418712));
#258670=CARTESIAN_POINT('Ctrl Pts',(3.82009341615424,0.942785568433326,
12.3273581875103));
#258671=CARTESIAN_POINT('Ctrl Pts',(3.84456604025781,0.829337664703831,
12.3215021331494));
#258672=CARTESIAN_POINT('Ctrl Pts',(3.8690468964877,0.715851599252443,12.3156441089229));
#258673=CARTESIAN_POINT('Ctrl Pts',(3.88848857670796,0.601327142618534,
12.3097860846965));
#258674=CARTESIAN_POINT('Ctrl Pts',(3.90282612382881,0.486248133322302,
12.30392806047));
#258675=CARTESIAN_POINT('Ctrl Pts',(3.9171798104826,0.371039581542509,12.2980634419653));
#258676=CARTESIAN_POINT('Ctrl Pts',(3.92641784539432,0.255275640874513,
12.2921988234606));
#258677=CARTESIAN_POINT('Ctrl Pts',(3.93052722196335,0.13944445992978,12.2863342049559));
#258678=CARTESIAN_POINT('Ctrl Pts',(3.93463937654077,0.0235349751381991,
12.2804656218695));
#258679=CARTESIAN_POINT('Ctrl Pts',(3.93361597255984,-0.092441428839417,
12.274597038783));
#258680=CARTESIAN_POINT('Ctrl Pts',(3.9274960673015,-0.207999137813684,
12.2687284556965));
#258681=CARTESIAN_POINT('Ctrl Pts',(3.92136735355823,-0.323723170986733,
12.2628514258574));
#258682=CARTESIAN_POINT('Ctrl Pts',(3.91012753949836,-0.439026897450485,
12.2569743960184));
#258683=CARTESIAN_POINT('Ctrl Pts',(3.89386719148217,-0.553432285920135,
12.2510973661793));
#258684=CARTESIAN_POINT('Ctrl Pts',(3.89043604133658,-0.577573347655859,
12.2498572345555));
#258685=CARTESIAN_POINT('Ctrl Pts',(3.88678152268101,-0.601674456093228,
12.2486171029318));
#258686=CARTESIAN_POINT('Ctrl Pts',(3.88290477146283,-0.625731200877199,
12.247376971308));
#258687=CARTESIAN_POINT('Ctrl Pts',(3.86453443807978,-0.739726243870756,
12.241500496372));
#258688=CARTESIAN_POINT('Ctrl Pts',(3.84110958488746,-0.853099259789004,
12.2356240214359));
#258689=CARTESIAN_POINT('Ctrl Pts',(3.81268340188325,-0.965367431087237,
12.2297475464998));
#258690=CARTESIAN_POINT('Ctrl Pts',(3.78429364476817,-1.07749173966707,
12.2238786017983));
#258691=CARTESIAN_POINT('Ctrl Pts',(3.75091540363758,-1.18851362275136,
12.2180096570967));
#258692=CARTESIAN_POINT('Ctrl Pts',(3.71265333098622,-1.29795772038883,
12.2121407123952));
#258693=CARTESIAN_POINT('Ctrl Pts',(3.67443009715556,-1.40729072420958,
12.2062777251046));
#258694=CARTESIAN_POINT('Ctrl Pts',(3.63133302828834,-1.51504874105127,
12.200414737814));
#258695=CARTESIAN_POINT('Ctrl Pts',(3.58351713425597,-1.62076955440737,
12.1945517505234));
#258696=CARTESIAN_POINT('Ctrl Pts',(3.53426192668763,-1.72967268612805,
12.1885122805561));
#258697=CARTESIAN_POINT('Ctrl Pts',(3.4799994135655,-1.83641359285394,12.1824728105888));
#258698=CARTESIAN_POINT('Ctrl Pts',(3.42095347312482,-1.94050672112087,
12.1764333406215));
#258699=CARTESIAN_POINT('Ctrl Pts',(3.36369782386785,-2.04144371353101,
12.1705769892523));
#258700=CARTESIAN_POINT('Ctrl Pts',(3.30194485399917,-2.13989079154352,
12.1647206378831));
#258701=CARTESIAN_POINT('Ctrl Pts',(3.23594591522378,-2.23542904914169,
12.1588642865139));
#258702=CARTESIAN_POINT('Ctrl Pts',(3.1699566075758,-2.3309533649834,12.1530087897533));
#258703=CARTESIAN_POINT('Ctrl Pts',(3.09972279759509,-2.42356936504171,
12.1471532929928));
#258704=CARTESIAN_POINT('Ctrl Pts',(3.02553912800216,-2.51288718109826,
12.1412977962323));
#258705=CARTESIAN_POINT('Ctrl Pts',(2.95134839413403,-2.60221350260669,
12.1354417418714));
#258706=CARTESIAN_POINT('Ctrl Pts',(2.87320731661203,-2.68824069829287,
12.1295856875105));
#258707=CARTESIAN_POINT('Ctrl Pts',(2.79145031533835,-2.77061259236968,
12.1237296331496));
#258708=CARTESIAN_POINT('Ctrl Pts',(2.70966581256091,-2.85301219478851,
12.1178716089232));
#258709=CARTESIAN_POINT('Ctrl Pts',(2.62426325791441,-2.93175375787231,
12.1120135846968));
#258710=CARTESIAN_POINT('Ctrl Pts',(2.53561282382302,-3.00651901834402,
12.1061555604703));
#258711=CARTESIAN_POINT('Ctrl Pts',(2.44686259744573,-3.08136844079782,
12.1002909419656));
#258712=CARTESIAN_POINT('Ctrl Pts',(2.35485751013449,-3.15223236079099,
12.094426323461));
#258713=CARTESIAN_POINT('Ctrl Pts',(2.25999967318794,-3.21883371381474,
12.0885617049563));
#258714=CARTESIAN_POINT('Ctrl Pts',(2.16507771073154,-3.285480090485,12.0826931218698));
#258715=CARTESIAN_POINT('Ctrl Pts',(2.06729950548291,-3.3478579408293,12.0768245387834));
#258716=CARTESIAN_POINT('Ctrl Pts',(1.96709343185303,-3.40573522610914,
12.0709559556969));
#258717=CARTESIAN_POINT('Ctrl Pts',(1.86674312989721,-3.46369581516153,
12.0650789258578));
#258718=CARTESIAN_POINT('Ctrl Pts',(1.76395835053689,-3.51714272235285,
12.0592018960188));
#258719=CARTESIAN_POINT('Ctrl Pts',(1.65918919677122,-3.56589122230582,
12.0533248661797));
#258720=CARTESIAN_POINT('Ctrl Pts',(1.63708150898486,-3.57617780550591,
12.0520847345558));
#258721=CARTESIAN_POINT('Ctrl Pts',(1.61488552214605,-3.58625535991692,
12.0508446029319));
#258722=CARTESIAN_POINT('Ctrl Pts',(1.5926055527196,-3.59612243304461,12.049604471308));
#258723=CARTESIAN_POINT('Ctrl Pts',(1.48702991914283,-3.64287844410842,
12.043727996372));
#258724=CARTESIAN_POINT('Ctrl Pts',(1.37921975576809,-3.68505821602127,
12.0378515214359));
#258725=CARTESIAN_POINT('Ctrl Pts',(1.26960879846334,-3.72244308201811,
12.0319750464998));
#258726=CARTESIAN_POINT('Ctrl Pts',(1.16013829886895,-3.75978004228718,
12.0261061017983));
#258727=CARTESIAN_POINT('Ctrl Pts',(1.04887198157874,-3.7923341839783,12.0202371570967));
#258728=CARTESIAN_POINT('Ctrl Pts',(0.93626539069549,-3.8199340463136,12.0143682123951));
#258729=CARTESIAN_POINT('Ctrl Pts',(0.823773103792509,-3.84750589275663,
12.0085052251046));
#258730=CARTESIAN_POINT('Ctrl Pts',(0.709943647958522,-3.8701333655085,
12.002642237814));
#258731=CARTESIAN_POINT('Ctrl Pts',(0.595249006656992,-3.88769438357413,
11.9967792505234));
#258732=CARTESIAN_POINT('Ctrl Pts',(0.47710192442408,-3.90578400852915,
11.9907397805561));
#258733=CARTESIAN_POINT('Ctrl Pts',(0.358037166249289,-3.9184971851488,
11.9847003105888));
#258734=CARTESIAN_POINT('Ctrl Pts',(0.238583828644082,-3.92575683871397,
11.9786608406215));
#258735=CARTESIAN_POINT('Ctrl Pts',(0.122752353195335,-3.93279637733683,
11.9728044892523));
#258736=CARTESIAN_POINT('Ctrl Pts',(0.00655596343611999,-3.93470830404591,
11.966948137883));
#258737=CARTESIAN_POINT('Ctrl Pts',(-0.109517133238559,-3.93147491376038,
11.9610917865138));
#258738=CARTESIAN_POINT('Ctrl Pts',(-0.225573291538121,-3.92824199531871,
11.9552362897533));
#258739=CARTESIAN_POINT('Ctrl Pts',(-0.341505780128436,-3.91986526442406,
11.9493807929928));
#258740=CARTESIAN_POINT('Ctrl Pts',(-0.456827129013423,-3.90637913856263,
11.9435252962322));
#258741=CARTESIAN_POINT('Ctrl Pts',(-0.57215945958413,-3.89289172846029,
11.9376692418713));
#258742=CARTESIAN_POINT('Ctrl Pts',(-0.686880124866386,-3.87429400410638,
11.9318131875105));
#258743=CARTESIAN_POINT('Ctrl Pts',(-0.800508210034658,-3.85067209791578,
11.9259571331496));
#258744=CARTESIAN_POINT('Ctrl Pts',(-0.914174517534386,-3.82704224576423,
11.9200991089231));
#258745=CARTESIAN_POINT('Ctrl Pts',(-1.02674711030018,-3.79838493509126,
11.9142410846967));
#258746=CARTESIAN_POINT('Ctrl Pts',(-1.13775736069864,-3.76483694044989,
11.9083830604702));
#258747=CARTESIAN_POINT('Ctrl Pts',(-1.24889257344802,-3.7312511814015,
11.9025184419656));
#258748=CARTESIAN_POINT('Ctrl Pts',(-1.35846153845435,-3.69276386978575,
11.8966538234609));
#258749=CARTESIAN_POINT('Ctrl Pts',(-1.46601274944517,-3.64956101722717,
11.8907892049562));
#258750=CARTESIAN_POINT('Ctrl Pts',(-1.57363666688249,-3.60632895880601,
11.8849206218697));
#258751=CARTESIAN_POINT('Ctrl Pts',(-1.67923973935278,-3.55837518189441,
11.8790520387833));
#258752=CARTESIAN_POINT('Ctrl Pts',(-1.78239388471749,-3.50593226399508,
11.8731834556968));
#258753=CARTESIAN_POINT('Ctrl Pts',(-1.88569650161834,-3.45341386410176,
11.8673064258577));
#258754=CARTESIAN_POINT('Ctrl Pts',(-1.98654279946989,-3.39639363114801,
11.8614293960187));
#258755=CARTESIAN_POINT('Ctrl Pts',(-2.08453251033331,-3.33514815463474,
11.8555523661796));
#258756=CARTESIAN_POINT('Ctrl Pts',(-2.10520964531166,-3.32222454282366,
11.8543122345558));
#258757=CARTESIAN_POINT('Ctrl Pts',(-2.12575970130394,-3.30911293981966,
11.8530721029319));
#258758=CARTESIAN_POINT('Ctrl Pts',(-2.14617910718161,-3.29581617204254,
11.851831971308));
#258759=CARTESIAN_POINT('Ctrl Pts',(-2.24292913726319,-3.23281420763031,
11.8459560524575));
#258760=CARTESIAN_POINT('Ctrl Pts',(-2.33706204953458,-3.16544462936648,
11.840080133607));
#258761=CARTESIAN_POINT('Ctrl Pts',(-2.42815809443204,-3.09395172367705,
11.8342042147565));
#258762=CARTESIAN_POINT('Ctrl Pts',(-2.51913739990764,-3.02255043602093,
11.8283358258856));
#258763=CARTESIAN_POINT('Ctrl Pts',(-2.60708725581871,-2.94703658198866,
11.8224674370148));
#258764=CARTESIAN_POINT('Ctrl Pts',(-2.6916155892492,-2.86769847084918,
11.816599048144));
#258765=CARTESIAN_POINT('Ctrl Pts',(-2.77605812574587,-2.78844088852641,
11.8107366157348));
#258766=CARTESIAN_POINT('Ctrl Pts',(-2.85708574857717,-2.70536705107285,
11.8048741833256));
#258767=CARTESIAN_POINT('Ctrl Pts',(-2.93433881231637,-2.61880597496908,
11.7990117509163));
#258768=CARTESIAN_POINT('Ctrl Pts',(-3.01387042901268,-2.52969180923521,
11.7929764080482));
#258769=CARTESIAN_POINT('Ctrl Pts',(-3.08940101458313,-2.43688177027347,
11.7869410651801));
#258770=CARTESIAN_POINT('Ctrl Pts',(-3.1605781230071,-2.34077656523832,
11.780905722312));
#258771=CARTESIAN_POINT('Ctrl Pts',(-3.22963783539814,-2.24753032405252,
11.7750499204695));
#258772=CARTESIAN_POINT('Ctrl Pts',(-3.2945991648606,-2.15118255228048,
11.769194118627));
#258773=CARTESIAN_POINT('Ctrl Pts',(-3.35518108726665,-2.05213276170139,
11.7633383167844));
#258774=CARTESIAN_POINT('Ctrl Pts',(-3.41575418820649,-1.95309739397891,
11.7574833676181));
#258775=CARTESIAN_POINT('Ctrl Pts',(-3.47194893482579,-1.8513611418387,
11.7516284184517));
#258776=CARTESIAN_POINT('Ctrl Pts',(-3.5235283962209,-1.74735132157932,
11.7457734692853));
#258777=CARTESIAN_POINT('Ctrl Pts',(-3.57511279231883,-1.64333155050736,
11.739917959965));
#258778=CARTESIAN_POINT('Ctrl Pts',(-3.62208084204468,-1.53703814871761,
11.7340624506448));
#258779=CARTESIAN_POINT('Ctrl Pts',(-3.66424253896638,-1.42892113695236,
11.7282069413245));
#258780=CARTESIAN_POINT('Ctrl Pts',(-3.70641844247636,-1.32076769463558,
11.722349458962));
#258781=CARTESIAN_POINT('Ctrl Pts',(-3.74378462291302,-1.21078980480763,
11.7164919765995));
#258782=CARTESIAN_POINT('Ctrl Pts',(-3.7762002249795,-1.09945480164708,
11.710634494237));
#258783=CARTESIAN_POINT('Ctrl Pts',(-3.80865232096792,-0.987994456038543,
11.7047704174418));
#258784=CARTESIAN_POINT('Ctrl Pts',(-3.83614259932708,-0.875174344191746,
11.6989063406467));
#258785=CARTESIAN_POINT('Ctrl Pts',(-3.85858081435279,-0.761474293137025,
11.6930422638515));
#258786=CARTESIAN_POINT('Ctrl Pts',(-3.88103421481454,-0.647697293677529,
11.6871742184446));
#258787=CARTESIAN_POINT('Ctrl Pts',(-3.89842868196084,-0.533039576235783,
11.6813061730378));
#258788=CARTESIAN_POINT('Ctrl Pts',(-3.91072577682643,-0.417986720441329,
11.6754381276309));
#258789=CARTESIAN_POINT('Ctrl Pts',(-3.92304055730816,-0.302768396244369,
11.6695616428325));
#258790=CARTESIAN_POINT('Ctrl Pts',(-3.93024331012025,-0.187154209903649,
11.6636851580341));
#258791=CARTESIAN_POINT('Ctrl Pts',(-3.93234765545738,-0.071630416854992,
11.6578086732356));
#258792=CARTESIAN_POINT('Ctrl Pts',(-3.93278276006484,-0.047744159338664,
11.6565936228509));
#258793=CARTESIAN_POINT('Ctrl Pts',(-3.93300007614865,-0.0238617492305318,
11.6553785724662));
#258794=CARTESIAN_POINT('Ctrl Pts',(-3.93299999997998,1.25478604846101E-5,
11.6541635220815));
#258795=CARTESIAN_POINT('',(-3.93299875665656,-0.00312732120702944,10.4041635220741));
#258796=CARTESIAN_POINT('Ctrl Pts',(-3.93299999997998,1.254881375347E-5,
11.654163522033));
#258797=CARTESIAN_POINT('Ctrl Pts',(-3.93299963153457,0.115489264304682,
11.648286489212));
#258798=CARTESIAN_POINT('Ctrl Pts',(-3.92790919375625,0.231155856959505,
11.642409456391));
#258799=CARTESIAN_POINT('Ctrl Pts',(-3.91770442456459,0.346527115457176,
11.63653242357));
#258800=CARTESIAN_POINT('Ctrl Pts',(-3.90751273112395,0.461750544462173,
11.6306629212101));
#258801=CARTESIAN_POINT('Ctrl Pts',(-3.89221977489077,0.576678984593512,
11.6247934188503));
#258802=CARTESIAN_POINT('Ctrl Pts',(-3.87185328733267,0.690826404656908,
11.6189239164904));
#258803=CARTESIAN_POINT('Ctrl Pts',(-3.85150747450685,0.804857949690607,
11.6130603724672));
#258804=CARTESIAN_POINT('Ctrl Pts',(-3.82609844717892,0.918109647932914,
11.607196828444));
#258805=CARTESIAN_POINT('Ctrl Pts',(-3.7957057434686,1.03010043636505,11.6013332844209));
#258806=CARTESIAN_POINT('Ctrl Pts',(-3.76437976836089,1.14553013568222,
11.5952896880412));
#258807=CARTESIAN_POINT('Ctrl Pts',(-3.72775913984388,1.25961979118295,
11.5892460916615));
#258808=CARTESIAN_POINT('Ctrl Pts',(-3.6859879483633,1.37185343405209,11.5832024952818));
#258809=CARTESIAN_POINT('Ctrl Pts',(-3.64550711673329,1.48062005140654,
11.5773455925023));
#258810=CARTESIAN_POINT('Ctrl Pts',(-3.60018941256176,1.58764322468082,
11.5714886897227));
#258811=CARTESIAN_POINT('Ctrl Pts',(-3.55021640761558,1.69246933771254,
11.5656317869432));
#258812=CARTESIAN_POINT('Ctrl Pts',(-3.50025071090823,1.79728012058209,
11.559775740699));
#258813=CARTESIAN_POINT('Ctrl Pts',(-3.4456312447062,1.89989410979751,11.5539196944549));
#258814=CARTESIAN_POINT('Ctrl Pts',(-3.38658693868387,1.99987947305227,
11.5480636482107));
#258815=CARTESIAN_POINT('Ctrl Pts',(-3.32753703631444,2.09987431313613,
11.5422070469178));
#258816=CARTESIAN_POINT('Ctrl Pts',(-3.26406167019856,2.19723967670041,
11.5363504456248));
#258817=CARTESIAN_POINT('Ctrl Pts',(-3.196434399675,2.29157066846613,11.5304938443319));
#258818=CARTESIAN_POINT('Ctrl Pts',(-3.12878441945234,2.38593333722283,
11.5246352763523));
#258819=CARTESIAN_POINT('Ctrl Pts',(-3.05698000263036,2.47725927284569,
11.5187767083727));
#258820=CARTESIAN_POINT('Ctrl Pts',(-2.98133603676951,2.56517532263575,
11.5129181403931));
#258821=CARTESIAN_POINT('Ctrl Pts',(-2.90560692994552,2.65319032621639,
11.5070529783102));
#258822=CARTESIAN_POINT('Ctrl Pts',(-2.82602991785966,2.73778747083878,
11.5011878162274));
#258823=CARTESIAN_POINT('Ctrl Pts',(-2.7429579755543,2.81862919596442,11.4953226541445));
#258824=CARTESIAN_POINT('Ctrl Pts',(-2.65982993761201,2.89952551073773,
11.4894535315186));
#258825=CARTESIAN_POINT('Ctrl Pts',(-2.57320257736082,2.97666108262849,
11.4835844088927));
#258826=CARTESIAN_POINT('Ctrl Pts',(-2.48346196311381,3.04973862449996,
11.4777152862668));
#258827=CARTESIAN_POINT('Ctrl Pts',(-2.39359208342735,3.12292142975348,
11.4718377095566));
#258828=CARTESIAN_POINT('Ctrl Pts',(-2.30060033017896,3.19203429461456,
11.4659601328465));
#258829=CARTESIAN_POINT('Ctrl Pts',(-2.20490175587179,3.25682318324982,
11.4600825561363));
#258830=CARTESIAN_POINT('Ctrl Pts',(-2.18430187973036,3.27076950471688,
11.4588173611936));
#258831=CARTESIAN_POINT('Ctrl Pts',(-2.16357666935699,3.28451564075698,
11.4575521662508));
#258832=CARTESIAN_POINT('Ctrl Pts',(-2.1427304044802,3.29805934053894,11.4562869713081));
#258833=CARTESIAN_POINT('Ctrl Pts',(-2.04590536280434,3.36096601967711,
11.450410496372));
#258834=CARTESIAN_POINT('Ctrl Pts',(-1.94614836124524,3.41970872241911,
11.4445340214359));
#258835=CARTESIAN_POINT('Ctrl Pts',(-1.84385297068083,3.47400276662404,
11.4386575464999));
#258836=CARTESIAN_POINT('Ctrl Pts',(-1.74168866351076,3.52822723733629,
11.4327886017983));
#258837=CARTESIAN_POINT('Ctrl Pts',(-1.6369927974258,3.57801419475766,11.4269196570968));
#258838=CARTESIAN_POINT('Ctrl Pts',(-1.53018796156289,3.62312210700771,
11.4210507123952));
#258839=CARTESIAN_POINT('Ctrl Pts',(-1.42349154047165,3.66818423140586,
11.4151877251046));
#258840=CARTESIAN_POINT('Ctrl Pts',(-1.31469078583114,3.70857659860889,
11.409324737814));
#258841=CARTESIAN_POINT('Ctrl Pts',(-1.20423234882466,3.74410382468812,
11.4034617505234));
#258842=CARTESIAN_POINT('Ctrl Pts',(-1.09044898551991,3.78070046123066,
11.3974222805561));
#258843=CARTESIAN_POINT('Ctrl Pts',(-0.974906954394349,3.81213420969258,
11.3913828105888));
#258844=CARTESIAN_POINT('Ctrl Pts',(-0.858116434120484,3.83824506584615,
11.3853433406215));
#258845=CARTESIAN_POINT('Ctrl Pts',(-0.744867038557684,3.86356423276215,
11.3794869892523));
#258846=CARTESIAN_POINT('Ctrl Pts',(-0.630444202922027,3.88387854155951,
11.3736306378831));
#258847=CARTESIAN_POINT('Ctrl Pts',(-0.515327149098713,3.89909309063041,
11.3677742865139));
#258848=CARTESIAN_POINT('Ctrl Pts',(-0.400226894136644,3.91430541946469,
11.3619187897533));
#258849=CARTESIAN_POINT('Ctrl Pts',(-0.284433031437971,3.9244194143499,
11.3560632929928));
#258850=CARTESIAN_POINT('Ctrl Pts',(-0.168432320485068,3.92939175361989,
11.3502077962323));
#258851=CARTESIAN_POINT('Ctrl Pts',(-0.0524205631529066,3.93436456638996,
11.3443517418714));
#258852=CARTESIAN_POINT('Ctrl Pts',(0.0637976692825216,3.93419473254505,
11.3384956875105));
#258853=CARTESIAN_POINT('Ctrl Pts',(0.179733888538592,3.9288910304704,11.3326396331496));
#258854=CARTESIAN_POINT('Ctrl Pts',(0.295709106538668,3.92358554433103,
11.3267816089231));
#258855=CARTESIAN_POINT('Ctrl Pts',(0.411401710717966,3.9131427748111,11.3209235846967));
#258856=CARTESIAN_POINT('Ctrl Pts',(0.526327313606261,3.89762345012342,
11.3150655604703));
#258857=CARTESIAN_POINT('Ctrl Pts',(0.641382286291133,3.88208665559589,
11.3092009419656));
#258858=CARTESIAN_POINT('Ctrl Pts',(0.755668125284889,3.86146195551416,
11.3033363234609));
#258859=CARTESIAN_POINT('Ctrl Pts',(0.868709539743867,3.83586140724062,
11.2974717049562));
#258860=CARTESIAN_POINT('Ctrl Pts',(0.981827372120121,3.81024355256138,
11.2916031218697));
#258861=CARTESIAN_POINT('Ctrl Pts',(1.09369870776683,3.77964326014677,11.2857345387833));
#258862=CARTESIAN_POINT('Ctrl Pts',(1.20386399908539,3.7442222786189,11.2798659556968));
#258863=CARTESIAN_POINT('Ctrl Pts',(1.31418785320323,3.70875031506288,11.2739889258577));
#258864=CARTESIAN_POINT('Ctrl Pts',(1.42280037731297,3.66844395870327,11.2681118960187));
#258865=CARTESIAN_POINT('Ctrl Pts',(1.52926250657235,3.62351282404134,11.2622348661796));
#258866=CARTESIAN_POINT('Ctrl Pts',(1.55172743475087,3.61403175579499,11.2609947345557));
#258867=CARTESIAN_POINT('Ctrl Pts',(1.57409670390057,3.60434492285895,11.2597546029319));
#258868=CARTESIAN_POINT('Ctrl Pts',(1.59636633986488,3.59445454957305,11.258514471308));
#258869=CARTESIAN_POINT('Ctrl Pts',(1.7018930074074,3.54758812861831,11.252637996372));
#258870=CARTESIAN_POINT('Ctrl Pts',(1.80552775613501,3.49599352287628,11.2467615214359));
#258871=CARTESIAN_POINT('Ctrl Pts',(1.90681735073534,3.43984543125628,11.2408850464998));
#258872=CARTESIAN_POINT('Ctrl Pts',(2.00797715078876,3.383769288943,11.2350161017982));
#258873=CARTESIAN_POINT('Ctrl Pts',(2.10679741541973,3.32315146315843,11.2291471570967));
#258874=CARTESIAN_POINT('Ctrl Pts',(2.20284525902097,3.25821450564704,11.2232782123951));
#258875=CARTESIAN_POINT('Ctrl Pts',(2.29879560698957,3.19334346392843,11.2174152251045));
#258876=CARTESIAN_POINT('Ctrl Pts',(2.3919787919248,3.12416224115855,11.211552237814));
#258877=CARTESIAN_POINT('Ctrl Pts',(2.48198749317454,3.05093872172569,11.2056892505234));
#258878=CARTESIAN_POINT('Ctrl Pts',(2.57470556010034,2.97551108994061,11.1996497805561));
#258879=CARTESIAN_POINT('Ctrl Pts',(2.66405461129145,2.89579416231397,11.1936103105888));
#258880=CARTESIAN_POINT('Ctrl Pts',(2.749622345888,2.8121283674458,11.1875708406214));
#258881=CARTESIAN_POINT('Ctrl Pts',(2.83259564029596,2.73099934536517,11.1817144892522));
#258882=CARTESIAN_POINT('Ctrl Pts',(2.91201329817608,2.64615777493143,11.175858137883));
#258883=CARTESIAN_POINT('Ctrl Pts',(2.98753447169513,2.55795363140799,11.1700017865138));
#258884=CARTESIAN_POINT('Ctrl Pts',(3.06304462452115,2.4697623593846,11.1641462897533));
#258885=CARTESIAN_POINT('Ctrl Pts',(3.1346591553342,2.37820980339812,11.1582907929927));
#258886=CARTESIAN_POINT('Ctrl Pts',(3.20207634466161,2.28368038108632,11.1524352962322));
#258887=CARTESIAN_POINT('Ctrl Pts',(3.2694999539138,2.18914195703792,11.1465792418713));
#258888=CARTESIAN_POINT('Ctrl Pts',(3.33272518749005,2.09162643912829,11.1407231875104));
#258889=CARTESIAN_POINT('Ctrl Pts',(3.39149305750062,1.99154810158457,11.1348671331495));
#258890=CARTESIAN_POINT('Ctrl Pts',(3.45028069590743,1.89143609958726,11.1290091089231));
#258891=CARTESIAN_POINT('Ctrl Pts',(3.50460778041299,1.78875991935942,11.1231510846966));
#258892=CARTESIAN_POINT('Ctrl Pts',(3.55426110735821,1.68395872298605,11.1172930604702));
#258893=CARTESIAN_POINT('Ctrl Pts',(3.60397032820906,1.57903955368837,11.1114284419655));
#258894=CARTESIAN_POINT('Ctrl Pts',(3.64899511406278,1.47199096702418,11.1055638234608));
#258895=CARTESIAN_POINT('Ctrl Pts',(3.68917024914258,1.36327248664427,11.0996992049561));
#258896=CARTESIAN_POINT('Ctrl Pts',(3.72937254329648,1.25448051072396,11.0938306218697));
#258897=CARTESIAN_POINT('Ctrl Pts',(3.76471853296518,1.14401678523187,11.0879620387832));
#258898=CARTESIAN_POINT('Ctrl Pts',(3.79509324129745,1.03235473063208,11.0820934556968));
#258899=CARTESIAN_POINT('Ctrl Pts',(3.82551166847004,0.920531958915893,
11.0762164258577));
#258900=CARTESIAN_POINT('Ctrl Pts',(3.85094444483676,0.807507817057756,
11.0703393960186));
#258901=CARTESIAN_POINT('Ctrl Pts',(3.87132788650239,0.693764654035434,
11.0644623661795));
#258902=CARTESIAN_POINT('Ctrl Pts',(3.87562906435998,0.669763330693276,
11.0632222345557));
#258903=CARTESIAN_POINT('Ctrl Pts',(3.87970559692021,0.645730003481113,
11.0619821029319));
#258904=CARTESIAN_POINT('Ctrl Pts',(3.88355718189753,0.621669216651523,
11.060741971308));
#258905=CARTESIAN_POINT('Ctrl Pts',(3.90180826278956,0.507655020070562,
11.054865496372));
#258906=CARTESIAN_POINT('Ctrl Pts',(3.91506425903091,0.392648746114955,
11.0489890214359));
#258907=CARTESIAN_POINT('Ctrl Pts',(3.92322449143385,0.277125584913448,
11.0431125464998));
#258908=CARTESIAN_POINT('Ctrl Pts',(3.931374267149,0.161750457440614,11.0372436017983));
#258909=CARTESIAN_POINT('Ctrl Pts',(3.93444123627607,0.0458601679209655,
11.0313746570967));
#258910=CARTESIAN_POINT('Ctrl Pts',(3.93237592910319,-0.0700610605816664,
11.0255057123952));
#258911=CARTESIAN_POINT('Ctrl Pts',(3.93031271836915,-0.185864620502874,
11.0196427251046));
#258912=CARTESIAN_POINT('Ctrl Pts',(3.92312760137356,-0.301698646731676,
11.013779737814));
#258913=CARTESIAN_POINT('Ctrl Pts',(3.91082304886289,-0.417075629212228,
11.0079167505234));
#258914=CARTESIAN_POINT('Ctrl Pts',(3.89814811513608,-0.535925591880217,
11.0018772805561));
#258915=CARTESIAN_POINT('Ctrl Pts',(3.88004062454556,-0.654290114789306,
10.9958378105888));
#258916=CARTESIAN_POINT('Ctrl Pts',(3.85656114444387,-0.771637958608704,
10.9897983406215));
#258917=CARTESIAN_POINT('Ctrl Pts',(3.83379356944368,-0.885427779494729,
10.9839419892522));
#258918=CARTESIAN_POINT('Ctrl Pts',(3.80597515660557,-0.998261251319322,
10.978085637883));
#258919=CARTESIAN_POINT('Ctrl Pts',(3.77321343554066,-1.10966182679925,
10.9722292865138));
#258920=CARTESIAN_POINT('Ctrl Pts',(3.74045649534521,-1.2210461457581,10.9663737897533));
#258921=CARTESIAN_POINT('Ctrl Pts',(3.70275779775884,-1.33099758836577,
10.9605182929928));
#258922=CARTESIAN_POINT('Ctrl Pts',(3.66027507920438,-1.43905362810264,
10.9546627962322));
#258923=CARTESIAN_POINT('Ctrl Pts',(3.61778831515557,-1.54711995767296,
10.9488067418713));
#258924=CARTESIAN_POINT('Ctrl Pts',(3.57051677551205,-1.65329014149911,
10.9429506875105));
#258925=CARTESIAN_POINT('Ctrl Pts',(3.51866652400122,-1.75712119470262,
10.9370946331496));
#258926=CARTESIAN_POINT('Ctrl Pts',(3.46679883104976,-1.860987174702,10.9312366089231));
#258927=CARTESIAN_POINT('Ctrl Pts',(3.41034954783291,-1.9625120904682,10.9253785846967));
#258928=CARTESIAN_POINT('Ctrl Pts',(3.34957056466185,-2.0612777669084,10.9195205604702));
#258929=CARTESIAN_POINT('Ctrl Pts',(3.28872316362313,-2.16015462219082,
10.9136559419656));
#258930=CARTESIAN_POINT('Ctrl Pts',(3.22353655135716,-2.25626568726273,
10.9077913234609));
#258931=CARTESIAN_POINT('Ctrl Pts',(3.15430585201212,-2.34922191203004,
10.9019267049562));
#258932=CARTESIAN_POINT('Ctrl Pts',(3.08502835153775,-2.44224097678508,
10.8960581218697));
#258933=CARTESIAN_POINT('Ctrl Pts',(3.01170158035158,-2.53210063549052,
10.8901895387833));
#258934=CARTESIAN_POINT('Ctrl Pts',(2.93465970456777,-2.61844637493041,
10.8843209556968));
#258935=CARTESIAN_POINT('Ctrl Pts',(2.85750694108657,-2.70491639327873,
10.8784439258577));
#258936=CARTESIAN_POINT('Ctrl Pts',(2.77662868887771,-2.78786210489861,
10.8725668960186));
#258937=CARTESIAN_POINT('Ctrl Pts',(2.69239456592323,-2.86696712596902,
10.8666898661796));
#258938=CARTESIAN_POINT('Ctrl Pts',(2.67462004332537,-2.88365933970976,
10.8654497345557));
#258939=CARTESIAN_POINT('Ctrl Pts',(2.65669620556759,-2.90018068876621,
10.8642096029319));
#258940=CARTESIAN_POINT('Ctrl Pts',(2.63862669716608,-2.91652844200128,
10.862969471308));
#258941=CARTESIAN_POINT('Ctrl Pts',(2.55300271081917,-2.99399373705519,
10.857092996372));
#258942=CARTESIAN_POINT('Ctrl Pts',(2.46382353700696,-3.06781270103919,
10.8512165214359));
#258943=CARTESIAN_POINT('Ctrl Pts',(2.37143262106348,-3.13764184121706,
10.8453400464998));
#258944=CARTESIAN_POINT('Ctrl Pts',(2.27916009671913,-3.20738150091423,
10.8394711017983));
#258945=CARTESIAN_POINT('Ctrl Pts',(2.18368434133317,-3.27314125789395,
10.8336021570967));
#258946=CARTESIAN_POINT('Ctrl Pts',(2.08538429412416,-3.33461562190011,
10.8277332123952));
#258947=CARTESIAN_POINT('Ctrl Pts',(1.98718402870016,-3.39602758490092,
10.8218702251046));
#258948=CARTESIAN_POINT('Ctrl Pts',(1.88616552191402,-3.45316259015437,
10.816007237814));
#258949=CARTESIAN_POINT('Ctrl Pts',(1.78273878875029,-3.50575689560545,
10.8101442505234));
#258950=CARTESIAN_POINT('Ctrl Pts',(1.67619879168062,-3.55993435028507,
10.8041047805561));
#258951=CARTESIAN_POINT('Ctrl Pts',(1.56710364355383,-3.60929314032474,
10.7980653105888));
#258952=CARTESIAN_POINT('Ctrl Pts',(1.45593169352115,-3.65359438140041,
10.7920258406215));
#258953=CARTESIAN_POINT('Ctrl Pts',(1.3481305114114,-3.69655239513933,10.7861694892523));
#258954=CARTESIAN_POINT('Ctrl Pts',(1.23837706107286,-3.73475496829349,
10.780313137883));
#258955=CARTESIAN_POINT('Ctrl Pts',(1.12712945065788,-3.76803240451295,
10.7744567865138));
#258956=CARTESIAN_POINT('Ctrl Pts',(1.01589807444195,-3.80130498460542,
10.7686012897533));
#258957=CARTESIAN_POINT('Ctrl Pts',(0.903173366977586,-3.82965373869254,
10.7627457929928));
#258958=CARTESIAN_POINT('Ctrl Pts',(0.789429058247675,-3.85295870234735,
10.7568902962322));
#258959=CARTESIAN_POINT('Ctrl Pts',(0.675673918008615,-3.87626588525981,
10.7510342418714));
#258960=CARTESIAN_POINT('Ctrl Pts',(0.560899387779055,-3.89452824010562,
10.7451781875105));
#258961=CARTESIAN_POINT('Ctrl Pts',(0.445589166560199,-3.90767696907564,
10.7393221331496));
#258962=CARTESIAN_POINT('Ctrl Pts',(0.330240157171288,-3.92083012102855,
10.7334641089232));
#258963=CARTESIAN_POINT('Ctrl Pts',(0.214355508254845,-3.92886617991995,
10.7276060846967));
#258964=CARTESIAN_POINT('Ctrl Pts',(0.0984231081634105,-3.93176829070324,
10.7217480604703));
#258965=CARTESIAN_POINT('Ctrl Pts',(-0.0176397950592482,-3.93467366834328,
10.7158834419656));
#258966=CARTESIAN_POINT('Ctrl Pts',(-0.133750143999501,-3.93243355295864,
10.7100188234609));
#258967=CARTESIAN_POINT('Ctrl Pts',(-0.249420891978136,-3.92508321168416,
10.7041542049562));
#258968=CARTESIAN_POINT('Ctrl Pts',(-0.365169835348115,-3.91772790145407,
10.6982856218698));
#258969=CARTESIAN_POINT('Ctrl Pts',(-0.480478176761877,-3.90525553056381,
10.6924170387833));
#258970=CARTESIAN_POINT('Ctrl Pts',(-0.594866533463926,-3.8877529251953,
10.6865484556969));
#258971=CARTESIAN_POINT('Ctrl Pts',(-0.709419531295986,-3.87022512802572,
10.6806714258578));
#258972=CARTESIAN_POINT('Ctrl Pts',(-0.823049498770957,-3.84765272788506,
10.6747943960187));
#258973=CARTESIAN_POINT('Ctrl Pts',(-0.935289686065408,-3.82017305931808,
10.6689173661797));
#258974=CARTESIAN_POINT('Ctrl Pts',(-0.958973861498471,-3.81437448300713,
10.6676772345558));
#258975=CARTESIAN_POINT('Ctrl Pts',(-0.982596218813739,-3.80835757603493,
10.6664371029319));
#258976=CARTESIAN_POINT('Ctrl Pts',(-1.00615248140522,-3.80212390436742,
10.665196971308));
#258977=CARTESIAN_POINT('Ctrl Pts',(-1.11777594462562,-3.77258509202802,
10.659320496372));
#258978=CARTESIAN_POINT('Ctrl Pts',(-1.22828123126072,-3.73807790275959,
10.6534440214359));
#258979=CARTESIAN_POINT('Ctrl Pts',(-1.33719313729155,-3.69870295016785,
10.6475675464998));
#258980=CARTESIAN_POINT('Ctrl Pts',(-1.44596548139053,-3.65937845344133,
10.6416986017983));
#258981=CARTESIAN_POINT('Ctrl Pts',(-1.55314812084941,-3.61519873747118,
10.6358296570967));
#258982=CARTESIAN_POINT('Ctrl Pts',(-1.65827835528228,-3.56631489024768,
10.6299607123951));
#258983=CARTESIAN_POINT('Ctrl Pts',(-1.76330187478718,-3.51748066372809,
10.6240977251046));
#258984=CARTESIAN_POINT('Ctrl Pts',(-1.86627676131745,-3.46395197718809,
10.618234737814));
#258985=CARTESIAN_POINT('Ctrl Pts',(-1.96675836703128,-3.40592873174299,
10.6123717505234));
#258986=CARTESIAN_POINT('Ctrl Pts',(-2.0702645849194,-3.3461589197167,10.6063322805561));
#258987=CARTESIAN_POINT('Ctrl Pts',(-2.17112462101919,-3.28161982600654,
10.6002928105888));
#258988=CARTESIAN_POINT('Ctrl Pts',(-2.26887740614487,-3.21258218819151,
10.5942533406215));
#258989=CARTESIAN_POINT('Ctrl Pts',(-2.36366629657974,-3.14563779291604,
10.5883969892522));
#258990=CARTESIAN_POINT('Ctrl Pts',(-2.45553328457484,-3.074463970667,10.582540637883));
#258991=CARTESIAN_POINT('Ctrl Pts',(-2.5440863358764,-2.99935221599714,
10.5766842865138));
#258992=CARTESIAN_POINT('Ctrl Pts',(-2.63262646476228,-2.92425142227446,
10.5708287897533));
#258993=CARTESIAN_POINT('Ctrl Pts',(-2.71785330395911,-2.84521410569714,
10.5649732929927));
#258994=CARTESIAN_POINT('Ctrl Pts',(-2.79940799052347,-2.76257197238251,
10.5591177962322));
#258995=CARTESIAN_POINT('Ctrl Pts',(-2.88097044328147,-2.67992196932013,
10.5532617418713));
#258996=CARTESIAN_POINT('Ctrl Pts',(-2.95885975838638,-2.59366676086053,
10.5474056875104));
#258997=CARTESIAN_POINT('Ctrl Pts',(-3.03275452905179,-2.50417430833315,
10.5415496331496));
#258998=CARTESIAN_POINT('Ctrl Pts',(-3.10667415651591,-2.41465175224286,
10.5356916089231));
#258999=CARTESIAN_POINT('Ctrl Pts',(-3.17659630502371,-2.32189010475253,
10.5298335846967));
#259000=CARTESIAN_POINT('Ctrl Pts',(-3.24224082591309,-2.22628916063984,
10.5239755604702));
#259001=CARTESIAN_POINT('Ctrl Pts',(-3.3079592417231,-2.13058060017039,
10.5181109419655));
#259002=CARTESIAN_POINT('Ctrl Pts',(-3.36939018554241,-2.03202670430909,
10.5122463234609));
#259003=CARTESIAN_POINT('Ctrl Pts',(-3.42629766038499,-1.93105498172381,
10.5063817049562));
#259004=CARTESIAN_POINT('Ctrl Pts',(-3.48324360564761,-1.83001500053821,
10.5005131218697));
#259005=CARTESIAN_POINT('Ctrl Pts',(-3.53565980672289,-1.72655430510248,
10.4946445387833));
#259006=CARTESIAN_POINT('Ctrl Pts',(-3.58335766604816,-1.62112209200107,
10.4887759556968));
#259007=CARTESIAN_POINT('Ctrl Pts',(-3.63112417772309,-1.51553812850115,
10.4828989258577));
#259008=CARTESIAN_POINT('Ctrl Pts',(-3.67415864226214,-1.40797736605348,
10.4770218960187));
#259009=CARTESIAN_POINT('Ctrl Pts',(-3.71232169009813,-1.29890595087826,
10.4711448661796));
#259010=CARTESIAN_POINT('Ctrl Pts',(-3.72037460182053,-1.27589042859561,
10.4699047345557));
#259011=CARTESIAN_POINT('Ctrl Pts',(-3.72821078614053,-1.2528076828768,
10.4686646029319));
#259012=CARTESIAN_POINT('Ctrl Pts',(-3.73582922396418,-1.22966215253425,
10.467424471308));
#259013=CARTESIAN_POINT('Ctrl Pts',(-3.77875150432028,-1.0992602295483,
10.4604375694694));
#259014=CARTESIAN_POINT('Ctrl Pts',(-3.81487274743111,-0.966516379801271,
10.4534506676308));
#259015=CARTESIAN_POINT('Ctrl Pts',(-3.84397267993236,-0.832083551053413,
10.4464637657922));
#259016=CARTESIAN_POINT('Ctrl Pts',(-3.87333558081508,-0.696435888443252,
10.4394137251725));
#259017=CARTESIAN_POINT('Ctrl Pts',(-3.8955494943805,-0.559068587730943,
10.4323636845529));
#259018=CARTESIAN_POINT('Ctrl Pts',(-3.91043755570927,-0.420674604532453,
10.4253136439332));
#259019=CARTESIAN_POINT('Ctrl Pts',(-3.92532561703803,-0.282280621333972,
10.4182636033135));
#259020=CARTESIAN_POINT('Ctrl Pts',(-3.93288764831246,-0.142860003044011,
10.4112135626938));
#259021=CARTESIAN_POINT('Ctrl Pts',(-3.93299875665656,-0.00312732120702682,
10.4041635220741));
#259022=CARTESIAN_POINT('',(-3.93299911320432,0.00264112363370479,9.15416352198993));
#259023=CARTESIAN_POINT('Ctrl Pts',(-3.93299875665718,-0.00312732043226372,
10.404163522035));
#259024=CARTESIAN_POINT('Ctrl Pts',(-3.93309078967956,0.112615779917745,
10.398323846247));
#259025=CARTESIAN_POINT('Ctrl Pts',(-3.92806927566635,0.228430631313712,
10.3924841704591));
#259026=CARTESIAN_POINT('Ctrl Pts',(-3.91794197275038,0.343830915074334,
10.3866444946711));
#259027=CARTESIAN_POINT('Ctrl Pts',(-3.90781704942902,0.459204083432567,
10.3808061910215));
#259028=CARTESIAN_POINT('Ctrl Pts',(-3.8925887583352,0.574162464627012,
10.3749678873719));
#259029=CARTESIAN_POINT('Ctrl Pts',(-3.87231687339564,0.688223097560241,
10.3691295837223));
#259030=CARTESIAN_POINT('Ctrl Pts',(-3.85204479682467,0.802284808715876,
10.3632912248829));
#259031=CARTESIAN_POINT('Ctrl Pts',(-3.82672910434552,0.915448346124159,
10.3574528660435));
#259032=CARTESIAN_POINT('Ctrl Pts',(-3.79648088756923,1.02723992831351,
10.351614507204));
#259033=CARTESIAN_POINT('Ctrl Pts',(-3.7662249914741,1.13905989178595,10.345774666141));
#259034=CARTESIAN_POINT('Ctrl Pts',(-3.73103418970762,1.24950680701535,
10.3399348250781));
#259035=CARTESIAN_POINT('Ctrl Pts',(-3.69106952592704,1.35812177464789,
10.3340949840151));
#259036=CARTESIAN_POINT('Ctrl Pts',(-3.65105991031265,1.46685891125452,
10.3282485743603));
#259037=CARTESIAN_POINT('Ctrl Pts',(-3.60626585456031,1.57375959587137,
10.3224021647054));
#259038=CARTESIAN_POINT('Ctrl Pts',(-3.55689674711794,1.67838450014942,
10.3165557550506));
#259039=CARTESIAN_POINT('Ctrl Pts',(-3.50749770353745,1.78307284623849,
10.3107058002856));
#259040=CARTESIAN_POINT('Ctrl Pts',(-3.45351827707842,1.88548229723389,
10.3048558455205));
#259041=CARTESIAN_POINT('Ctrl Pts',(-3.39521316212138,1.98519938136141,
10.2990058907555));
#259042=CARTESIAN_POINT('Ctrl Pts',(-3.33681352420546,2.08507812461354,
10.2931464521736));
#259043=CARTESIAN_POINT('Ctrl Pts',(-3.27407441730308,2.18225543563252,
10.2872870135916));
#259044=CARTESIAN_POINT('Ctrl Pts',(-3.20729327165033,2.27634770402646,
10.2814275750097));
#259045=CARTESIAN_POINT('Ctrl Pts',(-3.16255700013714,2.3393795257333,10.2775023737758));
#259046=CARTESIAN_POINT('Ctrl Pts',(-3.11600768858825,2.40102757864677,
10.273577172542));
#259047=CARTESIAN_POINT('Ctrl Pts',(-3.06774420917845,2.46118558159519,
10.2696519713081));
#259048=CARTESIAN_POINT('Ctrl Pts',(-2.99548826351334,2.55124898865822,
10.263775496372));
#259049=CARTESIAN_POINT('Ctrl Pts',(-2.91914387804605,2.63827599189948,
10.2578990214359));
#259050=CARTESIAN_POINT('Ctrl Pts',(-2.838995680598,2.72187298115579,10.2520225464998));
#259051=CARTESIAN_POINT('Ctrl Pts',(-2.75895018668055,2.80536284752952,
10.2461536017983));
#259052=CARTESIAN_POINT('Ctrl Pts',(-2.67511085747126,2.88543114576499,
10.2402846570967));
#259053=CARTESIAN_POINT('Ctrl Pts',(-2.58780339201678,2.96171615862602,
10.2344157123952));
#259054=CARTESIAN_POINT('Ctrl Pts',(-2.50058455006753,3.03792373658269,
10.2285527251046));
#259055=CARTESIAN_POINT('Ctrl Pts',(-2.40990488344022,3.11035539816109,
10.222689737814));
#259056=CARTESIAN_POINT('Ctrl Pts',(-2.31612739419673,3.17868571800539,
10.2168267505234));
#259057=CARTESIAN_POINT('Ctrl Pts',(-2.21952709441381,3.24907285925295,
10.2107872805561));
#259058=CARTESIAN_POINT('Ctrl Pts',(-2.11963982650347,3.31510751082604,
10.2047478105888));
#259059=CARTESIAN_POINT('Ctrl Pts',(-2.01690000395989,3.37647795402644,
10.1987083406214));
#259060=CARTESIAN_POINT('Ctrl Pts',(-1.91727528462475,3.43598762640026,
10.1928519892522));
#259061=CARTESIAN_POINT('Ctrl Pts',(-1.8149688772172,3.49111162716366,10.186995637883));
#259062=CARTESIAN_POINT('Ctrl Pts',(-1.71040618228331,3.54160975992655,
10.1811392865138));
#259063=CARTESIAN_POINT('Ctrl Pts',(-1.60585874602865,3.59210052357171,
10.1752837897533));
#259064=CARTESIAN_POINT('Ctrl Pts',(-1.49905604847651,3.63796658212048,
10.1694282929927));
#259065=CARTESIAN_POINT('Ctrl Pts',(-1.39044680087717,3.67901436446373,
10.1635727962322));
#259066=CARTESIAN_POINT('Ctrl Pts',(-1.28182721076438,3.72006605565682,
10.1577167418713));
#259067=CARTESIAN_POINT('Ctrl Pts',(-1.17140111465654,3.7562984126361,10.1518606875105));
#259068=CARTESIAN_POINT('Ctrl Pts',(-1.05963518074281,3.78756680254384,
10.1460046331496));
#259069=CARTESIAN_POINT('Ctrl Pts',(-0.947831650889574,3.81884571054465,
10.1401466089231));
#259070=CARTESIAN_POINT('Ctrl Pts',(-0.834687784210151,3.84515722000133,
10.1342885846967));
#259071=CARTESIAN_POINT('Ctrl Pts',(-0.720682622384007,3.86640731917806,
10.1284305604702));
#259072=CARTESIAN_POINT('Ctrl Pts',(-0.606549126886282,3.88768133923,10.1225659419655));
#259073=CARTESIAN_POINT('Ctrl Pts',(-0.491552807025955,3.90388250173589,
10.1167013234609));
#259074=CARTESIAN_POINT('Ctrl Pts',(-0.376180139063614,3.91496839105683,
10.1108367049562));
#259075=CARTESIAN_POINT('Ctrl Pts',(-0.260729477216973,3.92606177462735,
10.1049681218697));
#259076=CARTESIAN_POINT('Ctrl Pts',(-0.144902371729417,3.93203297799127,
10.0990995387833));
#259077=CARTESIAN_POINT('Ctrl Pts',(-0.0291859082189477,3.93289170747955,
10.0932309556968));
#259078=CARTESIAN_POINT('Ctrl Pts',(0.0866971079884395,3.93375167295196,
10.0873539258577));
#259079=CARTESIAN_POINT('Ctrl Pts',(0.202468753687625,3.92948449489353,
10.0814768960187));
#259080=CARTESIAN_POINT('Ctrl Pts',(0.317646406652164,3.92015175220819,
10.0755998661796));
#259081=CARTESIAN_POINT('Ctrl Pts',(0.341950426491008,3.91818241911677,
10.0743597345557));
#259082=CARTESIAN_POINT('Ctrl Pts',(0.366228033625769,3.9159877149394,10.0731196029319));
#259083=CARTESIAN_POINT('Ctrl Pts',(0.390474757234038,3.91356850763635,
10.071879471308));
#259084=CARTESIAN_POINT('Ctrl Pts',(0.505370031917421,3.90210487683449,
10.066002996372));
#259085=CARTESIAN_POINT('Ctrl Pts',(0.619949171234503,3.88555841742889,
10.0601265214359));
#259086=CARTESIAN_POINT('Ctrl Pts',(0.73372702899801,3.86395311137671,10.0542500464998));
#259087=CARTESIAN_POINT('Ctrl Pts',(0.847359089500328,3.84237549080316,
10.0483811017982));
#259088=CARTESIAN_POINT('Ctrl Pts',(0.960191508640707,3.81575199186813,
10.0425121570967));
#259089=CARTESIAN_POINT('Ctrl Pts',(1.0717434813489,3.784158415049,10.0366432123951));
#259090=CARTESIAN_POINT('Ctrl Pts',(1.18318222059205,3.75259690803634,10.0307802251045));
#259091=CARTESIAN_POINT('Ctrl Pts',(1.29334270404577,3.71607547016882,10.0249172378139));
#259092=CARTESIAN_POINT('Ctrl Pts',(1.40175420989629,3.67472096015984,10.0190542505233));
#259093=CARTESIAN_POINT('Ctrl Pts',(1.51342902705711,3.63212163172327,10.013014780556));
#259094=CARTESIAN_POINT('Ctrl Pts',(1.62324746636208,3.58439373749369,10.0069753105887));
#259095=CARTESIAN_POINT('Ctrl Pts',(1.73071135911118,3.53173147215973,10.0009358406214));
#259096=CARTESIAN_POINT('Ctrl Pts',(1.83491691338163,3.48066594300497,9.9950794892522));
#259097=CARTESIAN_POINT('Ctrl Pts',(1.93690824726824,3.42496114726119,9.98922313788299));
#259098=CARTESIAN_POINT('Ctrl Pts',(2.03625206176144,3.36484272158036,9.98336678651377));
#259099=CARTESIAN_POINT('Ctrl Pts',(2.13558137915908,3.30473306889225,9.97751128975323));
#259100=CARTESIAN_POINT('Ctrl Pts',(2.23226359244968,3.24021128059932,9.97165579299268));
#259101=CARTESIAN_POINT('Ctrl Pts',(2.32589177737904,3.17154795642768,9.96580029623214));
#259102=CARTESIAN_POINT('Ctrl Pts',(2.41952887822285,3.10287809366592,9.95994424187125));
#259103=CARTESIAN_POINT('Ctrl Pts',(2.51011103978352,3.03006615507781,9.95408818751037));
#259104=CARTESIAN_POINT('Ctrl Pts',(2.59726257059164,2.95342447667174,9.94823213314948));
#259105=CARTESIAN_POINT('Ctrl Pts',(2.68444341752092,2.87675701745942,9.94237410892303));
#259106=CARTESIAN_POINT('Ctrl Pts',(2.76819102926681,2.79625752911366,9.93651608469658));
#259107=CARTESIAN_POINT('Ctrl Pts',(2.84816540221072,2.7122763210355,9.93065806047013));
#259108=CARTESIAN_POINT('Ctrl Pts',(2.92822980094584,2.62820057673997,9.92479344196546));
#259109=CARTESIAN_POINT('Ctrl Pts',(3.00451219871417,2.54063558922418,9.91892882346079));
#259110=CARTESIAN_POINT('Ctrl Pts',(3.07671178996934,2.4499660327163,9.91306420495611));
#259111=CARTESIAN_POINT('Ctrl Pts',(3.14896018937547,2.35923518204699,9.90719562186964));
#259112=CARTESIAN_POINT('Ctrl Pts',(3.2171200443725,2.26539591626727,9.90132703878317));
#259113=CARTESIAN_POINT('Ctrl Pts',(3.28093390974316,2.16886183974393,9.8954584556967));
#259114=CARTESIAN_POINT('Ctrl Pts',(3.34483962350809,2.0721888200635,9.88958142585763));
#259115=CARTESIAN_POINT('Ctrl Pts',(3.40438665320248,1.97281360176912,9.88370439601856));
#259116=CARTESIAN_POINT('Ctrl Pts',(3.45936347077419,1.87117433102134,9.87782736617949));
#259117=CARTESIAN_POINT('Ctrl Pts',(3.47096431200072,1.84972709026777,9.87658723455569));
#259118=CARTESIAN_POINT('Ctrl Pts',(3.48236182869111,1.82817910781322,9.87534710293188));
#259119=CARTESIAN_POINT('Ctrl Pts',(3.49355431073443,1.80653460469178,9.87410697130808));
#259120=CARTESIAN_POINT('Ctrl Pts',(3.54659089083413,1.70397018519341,9.86823049637202));
#259121=CARTESIAN_POINT('Ctrl Pts',(3.5951942876369,1.5988993790448,9.86235402143594));
#259122=CARTESIAN_POINT('Ctrl Pts',(3.63912008030365,1.49174194857245,9.85647754649988));
#259123=CARTESIAN_POINT('Ctrl Pts',(3.68298958556625,1.38472183181104,9.85060860179832));
#259124=CARTESIAN_POINT('Ctrl Pts',(3.72219325199971,1.27562078670707,9.84473965709676));
#259125=CARTESIAN_POINT('Ctrl Pts',(3.75653246394915,1.16488319040843,9.8388707123952));
#259126=CARTESIAN_POINT('Ctrl Pts',(3.79083681907021,1.05425800092319,9.83300772510461));
#259127=CARTESIAN_POINT('Ctrl Pts',(3.82028642015564,0.941999956514412,
9.82714473781403));
#259128=CARTESIAN_POINT('Ctrl Pts',(3.84473095028929,0.828572821113264,
9.82128175052345));
#259129=CARTESIAN_POINT('Ctrl Pts',(3.8699112889614,0.711731398169494,9.81524228055614));
#259130=CARTESIAN_POINT('Ctrl Pts',(3.88978029191589,0.593649798330309,
9.80920281058883));
#259131=CARTESIAN_POINT('Ctrl Pts',(3.90422912302375,0.474851508298298,
9.80316334062152));
#259132=CARTESIAN_POINT('Ctrl Pts',(3.91823986110178,0.359655219177676,
9.79730698925231));
#259133=CARTESIAN_POINT('Ctrl Pts',(3.9271543186426,0.24378551259495,9.79145063788309));
#259134=CARTESIAN_POINT('Ctrl Pts',(3.93092538653102,0.12772864019454,9.78559428651388));
#259135=CARTESIAN_POINT('Ctrl Pts',(3.9346959041131,0.0116887038014935,
9.77973878975334));
#259136=CARTESIAN_POINT('Ctrl Pts',(3.93332451113864,-0.104537931754083,
9.7738832929928));
#259137=CARTESIAN_POINT('Ctrl Pts',(3.92681617069035,-0.220462608178249,
9.76802779623226));
#259138=CARTESIAN_POINT('Ctrl Pts',(3.92030721047351,-0.336398323740624,
9.76217174187139));
#259139=CARTESIAN_POINT('Ctrl Pts',(3.90866035348079,-0.452031610972567,
9.75631568751052));
#259140=CARTESIAN_POINT('Ctrl Pts',(3.89193257887595,-0.566877236695884,
9.75045963314965));
#259141=CARTESIAN_POINT('Ctrl Pts',(3.87519917736507,-0.681761494309081,
9.74460160892318));
#259142=CARTESIAN_POINT('Ctrl Pts',(3.85338151910736,-0.795857155424221,
9.7387435846967));
#259143=CARTESIAN_POINT('Ctrl Pts',(3.82658787411862,-0.908688198255243,
9.73288556047023));
#259144=CARTESIAN_POINT('Ctrl Pts',(3.79976406797954,-1.0216462530716,9.72702094196555));
#259145=CARTESIAN_POINT('Ctrl Pts',(3.76795319081166,-1.13333644665078,
9.72115632346087));
#259146=CARTESIAN_POINT('Ctrl Pts',(3.73131369244653,-1.2432968786903,9.7152917049562));
#259147=CARTESIAN_POINT('Ctrl Pts',(3.69464942515776,-1.35333164585084,
9.70942312186973));
#259148=CARTESIAN_POINT('Ctrl Pts',(3.65315018399584,-1.46163393861627,
9.70355453878326));
#259149=CARTESIAN_POINT('Ctrl Pts',(3.60702231229754,-1.56776243053204,
9.69768595569679));
#259150=CARTESIAN_POINT('Ctrl Pts',(3.56082804795985,-1.67404367501221,
9.69180892585772));
#259151=CARTESIAN_POINT('Ctrl Pts',(3.50999203841075,-1.77814450541052,
9.68593189601864));
#259152=CARTESIAN_POINT('Ctrl Pts',(3.45476623595575,-1.87964870518407,
9.68005486617957));
#259153=CARTESIAN_POINT('Ctrl Pts',(3.44311285560011,-1.90106744416246,
9.67881473455573));
#259154=CARTESIAN_POINT('Ctrl Pts',(3.43126416390677,-1.92237067020355,
9.6775746029319));
#259155=CARTESIAN_POINT('Ctrl Pts',(3.41922276683365,-1.9435546482583,9.67633447130806));
#259156=CARTESIAN_POINT('Ctrl Pts',(3.3621635267212,-2.0439368284175,9.67045799637199));
#259157=CARTESIAN_POINT('Ctrl Pts',(3.30058606534913,-2.14196937778998,
9.66458152143592));
#259158=CARTESIAN_POINT('Ctrl Pts',(3.23470898962048,-2.2372185303337,9.65870504649985));
#259159=CARTESIAN_POINT('Ctrl Pts',(3.16891633011683,-2.33234562867565,
9.6528361017983));
#259160=CARTESIAN_POINT('Ctrl Pts',(3.09883524605315,-2.42469608704472,
9.64696715709676));
#259161=CARTESIAN_POINT('Ctrl Pts',(3.02472995346133,-2.51386111562151,
9.64109821239522));
#259162=CARTESIAN_POINT('Ctrl Pts',(2.95069988319724,-2.60293563512983,
9.63523522510463));
#259163=CARTESIAN_POINT('Ctrl Pts',(2.87265399203605,-2.68883084111629,
9.62937223781404));
#259164=CARTESIAN_POINT('Ctrl Pts',(2.79089908220354,-2.77116786084052,
9.62350925052345));
#259165=CARTESIAN_POINT('Ctrl Pts',(2.70668325533213,-2.8559833197825,9.61746978055614));
#259166=CARTESIAN_POINT('Ctrl Pts',(2.61853183037083,-2.93702261751076,
9.61143031058884));
#259167=CARTESIAN_POINT('Ctrl Pts',(2.52682429095157,-3.01390908997884,
9.60539084062153));
#259168=CARTESIAN_POINT('Ctrl Pts',(2.43789735250282,-3.08846434081218,
9.59953448925231));
#259169=CARTESIAN_POINT('Ctrl Pts',(2.34562717472276,-3.15911468227834,
9.59367813788309));
#259170=CARTESIAN_POINT('Ctrl Pts',(2.25039568444709,-3.22555549687521,
9.58782178651387));
#259171=CARTESIAN_POINT('Ctrl Pts',(2.15517809116175,-3.29198661586242,
9.58196628975332));
#259172=CARTESIAN_POINT('Ctrl Pts',(2.05700038303853,-3.35420919342828,
9.57611079299279));
#259173=CARTESIAN_POINT('Ctrl Pts',(1.95627489654002,-3.41196095070963,
9.57025529623225));
#259174=CARTESIAN_POINT('Ctrl Pts',(1.85553981827368,-3.4697182075072,9.56439924187137));
#259175=CARTESIAN_POINT('Ctrl Pts',(1.75225683734641,-3.52300359241427,
9.55854318751049));
#259176=CARTESIAN_POINT('Ctrl Pts',(1.6468637806232,-3.57160029791569,9.55268713314961));
#259177=CARTESIAN_POINT('Ctrl Pts',(1.54143527167537,-3.62021335042681,
9.54682910892315));
#259178=CARTESIAN_POINT('Ctrl Pts',(1.43389565005852,-3.66413441461709,
9.54097108469669));
#259179=CARTESIAN_POINT('Ctrl Pts',(1.32470298711665,-3.70319470132536,
9.53511306047024));
#259180=CARTESIAN_POINT('Ctrl Pts',(1.21538740785142,-3.74229895753398,
9.52924844196555));
#259181=CARTESIAN_POINT('Ctrl Pts',(1.10441546207365,-3.77653137635416,
9.52338382346086));
#259182=CARTESIAN_POINT('Ctrl Pts',(0.992260743807369,-3.80577293283491,
9.51751920495618));
#259183=CARTESIAN_POINT('Ctrl Pts',(0.880030207045497,-3.8350342571048,
9.51165062186972));
#259184=CARTESIAN_POINT('Ctrl Pts',(0.766615708140619,-3.8592979145663,
9.50578203878325));
#259185=CARTESIAN_POINT('Ctrl Pts',(0.65249970833359,-3.87849624605008,
9.49991345569679));
#259186=CARTESIAN_POINT('Ctrl Pts',(0.538219459404579,-3.89772221002269,
9.49403642585771));
#259187=CARTESIAN_POINT('Ctrl Pts',(0.423236102552506,-3.91186824846193,
9.48815939601864));
#259188=CARTESIAN_POINT('Ctrl Pts',(0.308035918127367,-3.92091862618232,
9.48228236617957));
#259189=CARTESIAN_POINT('Ctrl Pts',(0.2837271438504,-3.9228283765028,9.48104223455574));
#259190=CARTESIAN_POINT('Ctrl Pts',(0.259408708406923,-3.92451141903962,
9.4798021029319));
#259191=CARTESIAN_POINT('Ctrl Pts',(0.235085163687484,-3.92596790178091,
9.47856197130807));
#259192=CARTESIAN_POINT('Ctrl Pts',(0.119825865276744,-3.9328695758932,
9.472685496372));
#259193=CARTESIAN_POINT('Ctrl Pts',(0.00407266020957847,-3.93470260675513,
9.46680902143594));
#259194=CARTESIAN_POINT('Ctrl Pts',(-0.111691641314658,-3.93141373773614,
9.46093254649988));
#259195=CARTESIAN_POINT('Ctrl Pts',(-0.227307600108367,-3.9281290831408,
9.45506360179832));
#259196=CARTESIAN_POINT('Ctrl Pts',(-0.34293421826802,-3.91973559295167,
9.44919465709676));
#259197=CARTESIAN_POINT('Ctrl Pts',(-0.458084754329627,-3.90623186176279,
9.4433257123952));
#259198=CARTESIAN_POINT('Ctrl Pts',(-0.573118404118721,-3.89274183785532,
9.43746272510464));
#259199=CARTESIAN_POINT('Ctrl Pts',(-0.687676525602775,-3.8741519389711,
9.43159973781408));
#259200=CARTESIAN_POINT('Ctrl Pts',(-0.80127423609795,-3.85051277086126,
9.42573675052352));
#259201=CARTESIAN_POINT('Ctrl Pts',(-0.918291368643197,-3.82616203653826,
9.41969728055621));
#259202=CARTESIAN_POINT('Ctrl Pts',(-1.03428890876868,-3.79645324686516,
9.4136578105889));
#259203=CARTESIAN_POINT('Ctrl Pts',(-1.14874419599218,-3.76149913893042,
9.40761834062159));
#259204=CARTESIAN_POINT('Ctrl Pts',(-1.2597291634933,-3.72760485036346,
9.40176198925237));
#259205=CARTESIAN_POINT('Ctrl Pts',(-1.36926363050524,-3.68877886688265,
9.39590563788315));
#259206=CARTESIAN_POINT('Ctrl Pts',(-1.47688399926232,-3.64517525679122,
9.39004928651393));
#259207=CARTESIAN_POINT('Ctrl Pts',(-1.58448866313818,-3.60157800971012,
9.3841937897534));
#259208=CARTESIAN_POINT('Ctrl Pts',(-1.69017940181734,-3.55320467729791,
9.37833829299287));
#259209=CARTESIAN_POINT('Ctrl Pts',(-1.79351152823802,-3.50025790450894,
9.37248279623235));
#259210=CARTESIAN_POINT('Ctrl Pts',(-1.89685349464887,-3.44730608976698,
9.36662674187146));
#259211=CARTESIAN_POINT('Ctrl Pts',(-1.99783603503181,-3.38978015707795,
9.36077068751058));
#259212=CARTESIAN_POINT('Ctrl Pts',(-2.09603868129343,-3.32792891248021,
9.35491463314969));
#259213=CARTESIAN_POINT('Ctrl Pts',(-2.19427436106121,-3.26605686229781,
9.34905660892328));
#259214=CARTESIAN_POINT('Ctrl Pts',(-2.28972793827619,-3.19985682684637,
9.34319858469686));
#259215=CARTESIAN_POINT('Ctrl Pts',(-2.38200815922846,-3.12962076446477,
9.33734056047045));
#259216=CARTESIAN_POINT('Ctrl Pts',(-2.47439225845652,-3.05930563854188,
9.33147594196576));
#259217=CARTESIAN_POINT('Ctrl Pts',(-2.5635955432187,-2.98494566788812,
9.32561132346107));
#259218=CARTESIAN_POINT('Ctrl Pts',(-2.64926001224255,-2.90687295689588,
9.31974670495638));
#259219=CARTESIAN_POINT('Ctrl Pts',(-2.73498239190311,-2.82874746742437,
9.31387812186992));
#259220=CARTESIAN_POINT('Ctrl Pts',(-2.81716090045971,-2.74690453024212,
9.30800953878347));
#259221=CARTESIAN_POINT('Ctrl Pts',(-2.89547576050465,-2.66171168993375,
9.30214095569702));
#259222=CARTESIAN_POINT('Ctrl Pts',(-2.97390334047536,-2.57639623010427,
9.29626392585794));
#259223=CARTESIAN_POINT('Ctrl Pts',(-3.04845590970486,-2.48772155966338,
9.29038689601886));
#259224=CARTESIAN_POINT('Ctrl Pts',(-3.11885513504136,-2.39608673603986,
9.28450986617978));
#259225=CARTESIAN_POINT('Ctrl Pts',(-3.13371030985389,-2.37675056696504,
9.28326973455588));
#259226=CARTESIAN_POINT('Ctrl Pts',(-3.14838070876592,-2.35728268751127,
9.28202960293198));
#259227=CARTESIAN_POINT('Ctrl Pts',(-3.16286397392929,-2.33768699410769,
9.28078947130807));
#259228=CARTESIAN_POINT('Ctrl Pts',(-3.23181323616237,-2.24439942477283,
9.27488568099729));
#259229=CARTESIAN_POINT('Ctrl Pts',(-3.29674593639203,-2.14790444279783,
9.26898189068651));
#259230=CARTESIAN_POINT('Ctrl Pts',(-3.357351231072,-2.04858041365707,9.26307810037573));
#259231=CARTESIAN_POINT('Ctrl Pts',(-3.41787820237606,-1.94938474612748,
9.25718193984038));
#259232=CARTESIAN_POINT('Ctrl Pts',(-3.47408867880547,-1.8473676458361,
9.25128577930502));
#259233=CARTESIAN_POINT('Ctrl Pts',(-3.5257129685583,-1.74293920242212,
9.24538961876966));
#259234=CARTESIAN_POINT('Ctrl Pts',(-3.57728259270084,-1.63862133960143,
9.23949970175292));
#259235=CARTESIAN_POINT('Ctrl Pts',(-3.62427550994493,-1.53189757501787,
9.23360978473617));
#259236=CARTESIAN_POINT('Ctrl Pts',(-3.66646648705797,-1.4232050095755,
9.22771986771942));
#259237=CARTESIAN_POINT('Ctrl Pts',(-3.71037505838516,-1.31008757098965,
9.22159017224572));
#259238=CARTESIAN_POINT('Ctrl Pts',(-3.74908218615332,-1.1948380113328,
9.21546047677202));
#259239=CARTESIAN_POINT('Ctrl Pts',(-3.78238784457942,-1.07797550676157,
9.20933078129831));
#259240=CARTESIAN_POINT('Ctrl Pts',(-3.81434471613369,-0.965845609783869,
9.20344932150509));
#259241=CARTESIAN_POINT('Ctrl Pts',(-3.84132894942371,-0.852231291647644,
9.19756786171186));
#259242=CARTESIAN_POINT('Ctrl Pts',(-3.86321398196001,-0.737608791696994,
9.19168640191864));
#259243=CARTESIAN_POINT('Ctrl Pts',(-3.88509192118417,-0.623023442852632,
9.1858068484068));
#259244=CARTESIAN_POINT('Ctrl Pts',(-3.90187387451445,-0.507430962637488,
9.17992729489496));
#259245=CARTESIAN_POINT('Ctrl Pts',(-3.91348423597454,-0.391318456987147,
9.17404774138312));
#259246=CARTESIAN_POINT('Ctrl Pts',(-3.9250946136188,-0.275205789482569,
9.16816817967552));
#259247=CARTESIAN_POINT('Ctrl Pts',(-3.93153334311241,-0.158573500149906,
9.16228861796792));
#259248=CARTESIAN_POINT('Ctrl Pts',(-3.9327766547239,-0.0419140079057827,
9.15640905626031));
#259249=CARTESIAN_POINT('Ctrl Pts',(-3.9329349374279,-0.0270623973281688,
9.15566054485186));
#259250=CARTESIAN_POINT('Ctrl Pts',(-3.93300908639746,-0.0122103481301702,
9.15491203344342));
#259251=CARTESIAN_POINT('Ctrl Pts',(-3.93299911320492,0.00264112274000227,
9.15416352203497));
#259252=CARTESIAN_POINT('',(-3.93424124989278,0.000925550842382836,7.90416352203497));
#259253=CARTESIAN_POINT('Ctrl Pts',(-3.93299911320432,0.00264112363370051,
9.15416352198993));
#259254=CARTESIAN_POINT('Ctrl Pts',(-3.93291035429015,0.134815447560986,
9.14750196030159));
#259255=CARTESIAN_POINT('Ctrl Pts',(-3.92615470656503,0.26673201376134,
9.14084039861325));
#259256=CARTESIAN_POINT('Ctrl Pts',(-3.91283401044963,0.397767528424178,
9.13417883692491));
#259257=CARTESIAN_POINT('Ctrl Pts',(-3.89945202944097,0.529405901785881,
9.12748662720636));
#259258=CARTESIAN_POINT('Ctrl Pts',(-3.87944456837661,0.660154926868483,
9.12079441748782));
#259259=CARTESIAN_POINT('Ctrl Pts',(-3.85296449477469,0.789400786676568,
9.11410220776927));
#259260=CARTESIAN_POINT('Ctrl Pts',(-3.82633163095001,0.919392396062604,
9.10737138395058));
#259261=CARTESIAN_POINT('Ctrl Pts',(-3.79315134365712,1.04786327566221,
9.10064056013189));
#259262=CARTESIAN_POINT('Ctrl Pts',(-3.75362763403148,1.17420977045638,
9.0939097363132));
#259263=CARTESIAN_POINT('Ctrl Pts',(-3.73230669359977,1.24236698835868,
9.09027881464482));
#259264=CARTESIAN_POINT('Ctrl Pts',(-3.70914062135989,1.30990637709726,
9.08664789297644));
#259265=CARTESIAN_POINT('Ctrl Pts',(-3.68416709535157,1.37673592730371,
9.08301697130806));
#259266=CARTESIAN_POINT('Ctrl Pts',(-3.64374862504109,1.48489639250922,
9.07714049637199));
#259267=CARTESIAN_POINT('Ctrl Pts',(-3.59849649986989,1.59145346478966,
9.07126402143592));
#259268=CARTESIAN_POINT('Ctrl Pts',(-3.54855777328464,1.6959442000435,9.06538754649985));
#259269=CARTESIAN_POINT('Ctrl Pts',(-3.49868303919946,1.80030103874369,
9.0595186017983));
#259270=CARTESIAN_POINT('Ctrl Pts',(-3.44413382341125,1.90259643727877,
9.05364965709675));
#259271=CARTESIAN_POINT('Ctrl Pts',(-3.38510617211613,2.0023848789634,9.04778071239519));
#259272=CARTESIAN_POINT('Ctrl Pts',(-3.32613843823298,2.10207202803281,
9.04191772510462));
#259273=CARTESIAN_POINT('Ctrl Pts',(-3.26270152026241,2.19925692900491,
9.03605473781404));
#259274=CARTESIAN_POINT('Ctrl Pts',(-3.19503825599498,2.29351685032583,
9.03019175052346));
#259275=CARTESIAN_POINT('Ctrl Pts',(-3.12533824946592,2.39061410394828,
9.02415228055615));
#259276=CARTESIAN_POINT('Ctrl Pts',(-3.05115361762181,2.4846070925014,9.01811281058884));
#259277=CARTESIAN_POINT('Ctrl Pts',(-2.97279931020066,2.57506373926365,
9.01207334062154));
#259278=CARTESIAN_POINT('Ctrl Pts',(-2.89682072962432,2.66277771250764,
9.00621698925232));
#259279=CARTESIAN_POINT('Ctrl Pts',(-2.81692196968616,2.74716636468995,
9.00036063788311));
#259280=CARTESIAN_POINT('Ctrl Pts',(-2.73343181764692,2.82786836650426,
8.9945042865139));
#259281=CARTESIAN_POINT('Ctrl Pts',(-2.6499538492019,2.90855859159498,8.98864878975337));
#259282=CARTESIAN_POINT('Ctrl Pts',(-2.56288582743188,2.98556294936955,
8.98279329299284));
#259283=CARTESIAN_POINT('Ctrl Pts',(-2.4725932785355,3.05855709100567,8.97693779623231));
#259284=CARTESIAN_POINT('Ctrl Pts',(-2.3822921313666,3.13155818364195,8.97108174187143));
#259285=CARTESIAN_POINT('Ctrl Pts',(-2.28876616759336,3.20054804155024,
8.96522568751055));
#259286=CARTESIAN_POINT('Ctrl Pts',(-2.19241329216521,3.2652431695568,8.95936963314967));
#259287=CARTESIAN_POINT('Ctrl Pts',(-2.0960280054582,3.32996005977673,8.95351160892323));
#259288=CARTESIAN_POINT('Ctrl Pts',(-1.99681425861177,3.39037911747974,
8.94765358469679));
#259289=CARTESIAN_POINT('Ctrl Pts',(-1.89519755969265,3.44626104782197,
8.94179556047035));
#259290=CARTESIAN_POINT('Ctrl Pts',(-1.79346647258389,3.50220588350274,
8.93593094196567));
#259291=CARTESIAN_POINT('Ctrl Pts',(-1.68932739639763,3.5536031991818,8.93006632346099));
#259292=CARTESIAN_POINT('Ctrl Pts',(-1.58322905712907,3.60026037289835,
8.92420170495631));
#259293=CARTESIAN_POINT('Ctrl Pts',(-1.47705899358003,3.64694908765727,
8.91833312186986));
#259294=CARTESIAN_POINT('Ctrl Pts',(-1.36892741328657,3.68889113074596,
8.9124645387834));
#259295=CARTESIAN_POINT('Ctrl Pts',(-1.25929994290721,3.72594318982374,
8.90659595569695));
#259296=CARTESIAN_POINT('Ctrl Pts',(-1.14951468382348,3.76304857856766,
8.90071892585788));
#259297=CARTESIAN_POINT('Ctrl Pts',(-1.03822963275164,3.79524982333243,
8.89484189601882));
#259298=CARTESIAN_POINT('Ctrl Pts',(-0.925922421305458,3.82245427307167,
8.88896486617975));
#259299=CARTESIAN_POINT('Ctrl Pts',(-0.902224102882769,3.82819477454199,
8.88772473455586));
#259300=CARTESIAN_POINT('Ctrl Pts',(-0.8784802939293,3.83371296908723,8.88648460293196));
#259301=CARTESIAN_POINT('Ctrl Pts',(-0.854695512203774,3.83900828097814,
8.88524447130806));
#259302=CARTESIAN_POINT('Ctrl Pts',(-0.741989190570715,3.86410059134748,
8.87936799637199));
#259303=CARTESIAN_POINT('Ctrl Pts',(-0.62799142012608,3.88426672184273,
8.87349152143592));
#259304=CARTESIAN_POINT('Ctrl Pts',(-0.513170456044613,3.89937752507281,
8.86761504649985));
#259305=CARTESIAN_POINT('Ctrl Pts',(-0.398496625882081,3.91446896501226,
8.86174610179829));
#259306=CARTESIAN_POINT('Ctrl Pts',(-0.283002105394635,3.9245179073427,
8.85587715709674));
#259307=CARTESIAN_POINT('Ctrl Pts',(-0.167167253910271,3.92944577634303,
8.85000821239518));
#259308=CARTESIAN_POINT('Ctrl Pts',(-0.0514499833282893,3.93436864319353,
8.84414522510459));
#259309=CARTESIAN_POINT('Ctrl Pts',(0.0646065211783655,3.93418075938562,
8.838282237814));
#259310=CARTESIAN_POINT('Ctrl Pts',(0.180515487543246,3.92885519696985,
8.8324192505234));
#259311=CARTESIAN_POINT('Ctrl Pts',(0.299913447423724,3.92336932898568,
8.8263797805561));
#259312=CARTESIAN_POINT('Ctrl Pts',(0.419154404326305,3.91243151860435,
8.82034031058879));
#259313=CARTESIAN_POINT('Ctrl Pts',(0.537704433560517,3.8960701921461,8.81430084062148));
#259314=CARTESIAN_POINT('Ctrl Pts',(0.652659989227609,3.88020494616845,
8.80844448925227));
#259315=CARTESIAN_POINT('Ctrl Pts',(0.766965473795392,3.85924038906495,
8.80258813788305));
#259316=CARTESIAN_POINT('Ctrl Pts',(0.880138723547427,3.83325512160518,
8.79673178651384));
#259317=CARTESIAN_POINT('Ctrl Pts',(0.993295458094677,3.80727364613701,
8.79087628975331));
#259318=CARTESIAN_POINT('Ctrl Pts',(1.10531988427633,3.77627300953238,8.78502079299278));
#259319=CARTESIAN_POINT('Ctrl Pts',(1.21574080643334,3.74038277340339,8.77916529623225));
#259320=CARTESIAN_POINT('Ctrl Pts',(1.32617224362404,3.7044891195612,8.77330924187136));
#259321=CARTESIAN_POINT('Ctrl Pts',(1.43499948076815,3.66370506814976,8.76745318751047));
#259322=CARTESIAN_POINT('Ctrl Pts',(1.54176791442105,3.6182095984149,8.76159713314958));
#259323=CARTESIAN_POINT('Ctrl Pts',(1.64857226294889,3.5726988248674,8.75573910892314));
#259324=CARTESIAN_POINT('Ctrl Pts',(1.75331605144466,3.52247364324909,8.7498810846967));
#259325=CARTESIAN_POINT('Ctrl Pts',(1.85556667801781,3.46776027190894,8.74402306047025));
#259326=CARTESIAN_POINT('Ctrl Pts',(1.95793240638224,3.41298531065722,8.73815844196557));
#259327=CARTESIAN_POINT('Ctrl Pts',(2.05779900733597,3.35371227073252,8.73229382346089));
#259328=CARTESIAN_POINT('Ctrl Pts',(2.15476034423315,3.29021228174114,8.7264292049562));
#259329=CARTESIAN_POINT('Ctrl Pts',(2.25178722864191,3.22666936567803,8.72056062186974));
#259330=CARTESIAN_POINT('Ctrl Pts',(2.34590460410072,3.15889405105692,8.71469203878328));
#259331=CARTESIAN_POINT('Ctrl Pts',(2.43673845398853,3.08719852080387,8.70882345569682));
#259332=CARTESIAN_POINT('Ctrl Pts',(2.52770304259934,3.01539979794056,8.70294642585775));
#259333=CARTESIAN_POINT('Ctrl Pts',(2.61537436318139,2.93966986790048,8.69706939601868));
#259334=CARTESIAN_POINT('Ctrl Pts',(2.69941432158252,2.86035859997224,8.69119236617961));
#259335=CARTESIAN_POINT('Ctrl Pts',(2.71714787287179,2.84362286539573,8.68995223455576));
#259336=CARTESIAN_POINT('Ctrl Pts',(2.7347198732339,2.82672778510936,8.68871210293192));
#259337=CARTESIAN_POINT('Ctrl Pts',(2.75212737675622,2.8096768323259,8.68747197130808));
#259338=CARTESIAN_POINT('Ctrl Pts',(2.83461439360333,2.72887936313655,8.681595496372));
#259339=CARTESIAN_POINT('Ctrl Pts',(2.9136760718494,2.64431332078843,8.67571902143593));
#259340=CARTESIAN_POINT('Ctrl Pts',(2.98894883581638,2.55630081501999,8.66984254649985));
#259341=CARTESIAN_POINT('Ctrl Pts',(3.06412514373247,2.46840109026675,8.6639736017983));
#259342=CARTESIAN_POINT('Ctrl Pts',(3.13552192723564,2.37706399588563,8.65810465709674));
#259343=CARTESIAN_POINT('Ctrl Pts',(3.20281140389944,2.28264936226563,8.65223571239519));
#259344=CARTESIAN_POINT('Ctrl Pts',(3.27003257679035,2.18833056644988,8.64637272510459));
#259345=CARTESIAN_POINT('Ctrl Pts',(3.33315449791145,2.0909407794463,8.640509737814));
#259346=CARTESIAN_POINT('Ctrl Pts',(3.39188918338247,1.99087336806062,8.63464675052341));
#259347=CARTESIAN_POINT('Ctrl Pts',(3.45239185059966,1.88779381222744,8.6286072805561));
#259348=CARTESIAN_POINT('Ctrl Pts',(3.50823868180835,1.78187321487768,8.6225678105888));
#259349=CARTESIAN_POINT('Ctrl Pts',(3.55916238545576,1.67357465144429,8.61652834062149));
#259350=CARTESIAN_POINT('Ctrl Pts',(3.60854206665222,1.56855973396298,8.61067198925227));
#259351=CARTESIAN_POINT('Ctrl Pts',(3.65329267031689,1.46130937299166,8.60481563788305));
#259352=CARTESIAN_POINT('Ctrl Pts',(3.69321718741445,1.35227061144822,8.59895928651384));
#259353=CARTESIAN_POINT('Ctrl Pts',(3.73313587838633,1.2432477617698,8.5931037897533));
#259354=CARTESIAN_POINT('Ctrl Pts',(3.76822974136158,1.13243741788122,8.58724829299277));
#259355=CARTESIAN_POINT('Ctrl Pts',(3.79835046683571,1.02030521467303,8.58139279623224));
#259356=CARTESIAN_POINT('Ctrl Pts',(3.82847406061084,0.908162333471344,
8.57553674187135));
#259357=CARTESIAN_POINT('Ctrl Pts',(3.85362346839962,0.794697741277012,
8.56968068751046));
#259358=CARTESIAN_POINT('Ctrl Pts',(3.87370085314682,0.680390108929896,
8.56382463314957));
#259359=CARTESIAN_POINT('Ctrl Pts',(3.89378499154524,0.566044025664439,
8.55796660892313));
#259360=CARTESIAN_POINT('Ctrl Pts',(3.90879364292156,0.450854744561919,
8.55210858469668));
#259361=CARTESIAN_POINT('Ctrl Pts',(3.91868056588485,0.335308250057171,
8.54625056047023));
#259362=CARTESIAN_POINT('Ctrl Pts',(3.92857861838916,0.219631686828761,
8.54038594196555));
#259363=CARTESIAN_POINT('Ctrl Pts',(3.93334340015094,0.103597519004202,
8.53452132346087));
#259364=CARTESIAN_POINT('Ctrl Pts',(3.9329807478794,-0.0123059664400662,
8.52865670495618));
#259365=CARTESIAN_POINT('Ctrl Pts',(3.93261785044875,-0.128287804610262,
8.52278812186971));
#259366=CARTESIAN_POINT('Ctrl Pts',(3.92712063629491,-0.244138373326166,
8.51691953878325));
#259367=CARTESIAN_POINT('Ctrl Pts',(3.91654686946191,-0.35937392686186,
8.51105095569678));
#259368=CARTESIAN_POINT('Ctrl Pts',(3.90595788362437,-0.474775340912462,
8.50517392585771));
#259369=CARTESIAN_POINT('Ctrl Pts',(3.89027781912066,-0.589559566020484,
8.49929689601864));
#259370=CARTESIAN_POINT('Ctrl Pts',(3.86961561816118,-0.703252421028928,
8.49341986617956));
#259371=CARTESIAN_POINT('Ctrl Pts',(3.86525561837737,-0.727243128709607,
8.49217973455573));
#259372=CARTESIAN_POINT('Ctrl Pts',(3.86067395786117,-0.751185294892164,
8.4909396029319));
#259373=CARTESIAN_POINT('Ctrl Pts',(3.8558719418734,-0.775074556332128,
8.48969947130807));
#259374=CARTESIAN_POINT('Ctrl Pts',(3.83311715838715,-0.888275964469223,
8.48382299637199));
#259375=CARTESIAN_POINT('Ctrl Pts',(3.80533561733877,-1.00066079646393,
8.47794652143592));
#259376=CARTESIAN_POINT('Ctrl Pts',(3.77259909706671,-1.11174864641762,
8.47207004649985));
#259377=CARTESIAN_POINT('Ctrl Pts',(3.73990452603765,-1.22269414614068,
8.4662011017983));
#259378=CARTESIAN_POINT('Ctrl Pts',(3.70226771868287,-1.33234557675928,
8.46033215709674));
#259379=CARTESIAN_POINT('Ctrl Pts',(3.65981158979467,-1.44023196992867,
8.45446321239519));
#259380=CARTESIAN_POINT('Ctrl Pts',(3.61739855700303,-1.54800885046608,
8.4486002251046));
#259381=CARTESIAN_POINT('Ctrl Pts',(3.57017608374951,-1.65402387562024,
8.44273723781401));
#259382=CARTESIAN_POINT('Ctrl Pts',(3.51831689761231,-1.75782115358067,
8.43687425052341));
#259383=CARTESIAN_POINT('Ctrl Pts',(3.46489669018543,-1.86474284927257,
8.43083478055611));
#259384=CARTESIAN_POINT('Ctrl Pts',(3.40655632782321,-1.96931073926958,
8.4247953105888));
#259385=CARTESIAN_POINT('Ctrl Pts',(3.34353825557212,-2.0710482692409,8.4187558406215));
#259386=CARTESIAN_POINT('Ctrl Pts',(3.28243091077021,-2.1697010858247,8.41289948925228));
#259387=CARTESIAN_POINT('Ctrl Pts',(3.21692565909362,-2.26569232740226,
8.40704313788307));
#259388=CARTESIAN_POINT('Ctrl Pts',(3.14728982722824,-2.35861309744214,
8.40118678651385));
#259389=CARTESIAN_POINT('Ctrl Pts',(3.07766415721673,-2.45152030769161,
8.39533128975332));
#259390=CARTESIAN_POINT('Ctrl Pts',(3.00390935302893,-2.54135760724159,
8.38947579299279));
#259391=CARTESIAN_POINT('Ctrl Pts',(2.92633487980487,-2.62774678598175,
8.38362029623227));
#259392=CARTESIAN_POINT('Ctrl Pts',(2.84875301941015,-2.71414419128897,
8.37776424187138));
#259393=CARTESIAN_POINT('Ctrl Pts',(2.76735104263499,-2.79709251599194,
8.3719081875105));
#259394=CARTESIAN_POINT('Ctrl Pts',(2.68247686227203,-2.87624875199889,
8.36605213314961));
#259395=CARTESIAN_POINT('Ctrl Pts',(2.59757413184547,-2.95543161466148,
8.36019410892317));
#259396=CARTESIAN_POINT('Ctrl Pts',(2.50919717692449,-3.03081957083429,
8.35433608469673));
#259397=CARTESIAN_POINT('Ctrl Pts',(2.41772817347323,-3.10210887610248,
8.3484780604703));
#259398=CARTESIAN_POINT('Ctrl Pts',(2.32615620492044,-3.17347843052916,
8.34261344196561));
#259399=CARTESIAN_POINT('Ctrl Pts',(2.23148556649261,-3.24073987169441,
8.33674882346093));
#259400=CARTESIAN_POINT('Ctrl Pts',(2.13412875972782,-3.30363185553454,
8.33088420495625));
#259401=CARTESIAN_POINT('Ctrl Pts',(2.03670613810714,-3.36656635542455,
8.32501562186979));
#259402=CARTESIAN_POINT('Ctrl Pts',(1.9365940875158,-3.42512530829786,8.31914703878333));
#259403=CARTESIAN_POINT('Ctrl Pts',(1.83422961587707,-3.47909337561374,
8.31327845569688));
#259404=CARTESIAN_POINT('Ctrl Pts',(1.73171780929298,-3.53313912009752,
8.3074014258578));
#259405=CARTESIAN_POINT('Ctrl Pts',(1.62694748362794,-3.58258061700573,
8.30152439601873));
#259406=CARTESIAN_POINT('Ctrl Pts',(1.52037553378327,-3.62725064425844,
8.29564736617966));
#259407=CARTESIAN_POINT('Ctrl Pts',(1.49788743199745,-3.63667661536151,
8.2944072345558));
#259408=CARTESIAN_POINT('Ctrl Pts',(1.47531916159813,-3.64589030657686,
8.29316710293194));
#259409=CARTESIAN_POINT('Ctrl Pts',(1.45267509187603,-3.65489043302846,
8.29192697130807));
#259410=CARTESIAN_POINT('Ctrl Pts',(1.34537413638719,-3.69753833950591,
8.286050496372));
#259411=CARTESIAN_POINT('Ctrl Pts',(1.23601687412186,-3.73552720202288,
8.28017402143592));
#259412=CARTESIAN_POINT('Ctrl Pts',(1.12504515455434,-3.7686552509103,8.27429754649985));
#259413=CARTESIAN_POINT('Ctrl Pts',(1.01421563640559,-3.80174084884201,
8.26842860179829));
#259414=CARTESIAN_POINT('Ctrl Pts',(0.901776167133158,-3.82997790347437,
8.26255965709674));
#259415=CARTESIAN_POINT('Ctrl Pts',(0.788188566919396,-3.85321265737794,
8.25669071239519));
#259416=CARTESIAN_POINT('Ctrl Pts',(0.674716266482581,-3.87642382629567,
8.2508277251046));
#259417=CARTESIAN_POINT('Ctrl Pts',(0.560098555277048,-3.89464271255726,
8.24496473781401));
#259418=CARTESIAN_POINT('Ctrl Pts',(0.444811775447612,-3.90776553600944,
8.23910175052342));
#259419=CARTESIAN_POINT('Ctrl Pts',(0.326054730634482,-3.92128337157646,
8.23306228055611));
#259420=CARTESIAN_POINT('Ctrl Pts',(0.206588125901247,-3.92939335631743,
8.22702281058881));
#259421=CARTESIAN_POINT('Ctrl Pts',(0.0869436374963476,-3.93203888636658,
8.2209833406215));
#259422=CARTESIAN_POINT('Ctrl Pts',(-0.0290731930007671,-3.93460420312608,
8.21512698925228));
#259423=CARTESIAN_POINT('Ctrl Pts',(-0.145256833890354,-3.93203164671809,
8.20927063788307));
#259424=CARTESIAN_POINT('Ctrl Pts',(-0.261118758180631,-3.92432236113781,
8.20341428651385));
#259425=CARTESIAN_POINT('Ctrl Pts',(-0.376963774911809,-3.91661420056216,
8.19755878975332));
#259426=CARTESIAN_POINT('Ctrl Pts',(-0.492486756747227,-3.90377082876646,
8.19170329299278));
#259427=CARTESIAN_POINT('Ctrl Pts',(-0.607201924524633,-3.88584544505486,
8.18584779623225));
#259428=CARTESIAN_POINT('Ctrl Pts',(-0.721928016263048,-3.8679183543659,
8.17999174187137));
#259429=CARTESIAN_POINT('Ctrl Pts',(-0.835845733284041,-3.8449083534386,
8.17413568751048));
#259430=CARTESIAN_POINT('Ctrl Pts',(-0.948477841967473,-3.81692006509132,
8.16827963314959));
#259431=CARTESIAN_POINT('Ctrl Pts',(-1.06114783795495,-3.78892236201495,
8.16242160892314));
#259432=CARTESIAN_POINT('Ctrl Pts',(-1.17253096540947,-3.75594314104913,
8.15656358469669));
#259433=CARTESIAN_POINT('Ctrl Pts',(-1.28216422261669,-3.71813715538329,
8.15070556047024));
#259434=CARTESIAN_POINT('Ctrl Pts',(-1.39192089211684,-3.68028861216242,
8.14484094196556));
#259435=CARTESIAN_POINT('Ctrl Pts',(-1.4999233695722,-3.63760259441104,
8.13897632346088));
#259436=CARTESIAN_POINT('Ctrl Pts',(-1.6057276615338,-3.59028239515852,
8.13311170495619));
#259437=CARTESIAN_POINT('Ctrl Pts',(-1.71160347899483,-3.54293020664713,
8.12724312186974));
#259438=CARTESIAN_POINT('Ctrl Pts',(-1.81527778397138,-3.4909377829408,
8.12137453878328));
#259439=CARTESIAN_POINT('Ctrl Pts',(-1.91633178630073,-3.43455404453234,
8.11550595569682));
#259440=CARTESIAN_POINT('Ctrl Pts',(-2.01753123739441,-3.37808915203902,
8.10962892585775));
#259441=CARTESIAN_POINT('Ctrl Pts',(-2.11610250971854,-3.31722054741486,
8.10375189601868));
#259442=CARTESIAN_POINT('Ctrl Pts',(-2.21165630466072,-3.25224005726122,
8.09787486617961));
#259443=CARTESIAN_POINT('Ctrl Pts',(-2.23181942891412,-3.23852830779269,
8.09663473455576));
#259444=CARTESIAN_POINT('Ctrl Pts',(-2.25184831577001,-3.22463361002975,
8.09539460293191));
#259445=CARTESIAN_POINT('Ctrl Pts',(-2.27173950580696,-3.21055892606816,
8.09415447130807));
#259446=CARTESIAN_POINT('Ctrl Pts',(-2.36541204959047,-3.144277750976,8.08831438413299));
#259447=CARTESIAN_POINT('Ctrl Pts',(-2.45634508284629,-3.07377766099405,
8.08247429695792));
#259448=CARTESIAN_POINT('Ctrl Pts',(-2.54413139898459,-2.99931399234903,
8.07663420978283));
#259449=CARTESIAN_POINT('Ctrl Pts',(-2.63180489291161,-2.92494602376442,
8.07080162823709));
#259450=CARTESIAN_POINT('Ctrl Pts',(-2.71633939417977,-2.84662487243111,
8.06496904669133));
#259451=CARTESIAN_POINT('Ctrl Pts',(-2.79735680083598,-2.76464897027031,
8.05913646514558));
#259452=CARTESIAN_POINT('Ctrl Pts',(-2.87829237462163,-2.68275586912311,
8.05330977488802));
#259453=CARTESIAN_POINT('Ctrl Pts',(-2.95571762607744,-2.59721565412246,
8.04748308463046));
#259454=CARTESIAN_POINT('Ctrl Pts',(-3.02928825524465,-2.50836633421771,
8.0416563943729));
#259455=CARTESIAN_POINT('Ctrl Pts',(-3.10280642452256,-2.41958036874584,
8.03583385886471));
#259456=CARTESIAN_POINT('Ctrl Pts',(-3.17247517203039,-2.32749031240236,
8.03001132335653));
#259457=CARTESIAN_POINT('Ctrl Pts',(-3.23798824238765,-2.23246974048011,
8.02418878784835));
#259458=CARTESIAN_POINT('Ctrl Pts',(-3.30347679317533,-2.13748473189679,
8.01836843153988));
#259459=CARTESIAN_POINT('Ctrl Pts',(-3.36481252099727,-2.03957173170653,
8.01254807523142));
#259460=CARTESIAN_POINT('Ctrl Pts',(-3.4217309428114,-1.93913546587313,
8.00672771892296));
#259461=CARTESIAN_POINT('Ctrl Pts',(-3.47864223314819,-1.8387117839964,
8.00090809186414));
#259462=CARTESIAN_POINT('Ctrl Pts',(-3.53113711173155,-1.73576582906683,
7.99508846480533));
#259463=CARTESIAN_POINT('Ctrl Pts',(-3.57899614054457,-1.63072855680126,
7.98926883774651));
#259464=CARTESIAN_POINT('Ctrl Pts',(-3.62686108896054,-1.52567829265173,
7.98344849086779));
#259465=CARTESIAN_POINT('Ctrl Pts',(-3.67008887487706,-1.41853657797749,
7.97762814398907));
#259466=CARTESIAN_POINT('Ctrl Pts',(-3.70850778308308,-1.30975532936966,
7.97180779711035));
#259467=CARTESIAN_POINT('Ctrl Pts',(-3.74696460218192,-1.20086673793379,
7.96598170684753));
#259468=CARTESIAN_POINT('Ctrl Pts',(-3.78060292647502,-1.09033577653945,
7.9601556165847));
#259469=CARTESIAN_POINT('Ctrl Pts',(-3.80930060036575,-0.978630643324191,
7.95432952632187));
#259470=CARTESIAN_POINT('Ctrl Pts',(-3.83801263407408,-0.866869614800349,
7.94850052078467));
#259471=CARTESIAN_POINT('Ctrl Pts',(-3.86177900736688,-0.753933653675194,
7.94267151524746));
#259472=CARTESIAN_POINT('Ctrl Pts',(-3.88052886830953,-0.640300478069776,
7.93684250971026));
#259473=CARTESIAN_POINT('Ctrl Pts',(-3.89930857883885,-0.5264863996121,
7.93100422445591));
#259474=CARTESIAN_POINT('Ctrl Pts',(-3.91305577257815,-0.411973304872136,
7.92516593920156));
#259475=CARTESIAN_POINT('Ctrl Pts',(-3.92175154018954,-0.297243767001051,
7.91932765394721));
#259476=CARTESIAN_POINT('Ctrl Pts',(-3.92928022149421,-0.197912441065812,
7.9142729433098));
#259477=CARTESIAN_POINT('Ctrl Pts',(-3.93302326243764,-0.0984190716634967,
7.90921823267238));
#259478=CARTESIAN_POINT('Ctrl Pts',(-3.93299989116401,0.000925258806245537,
7.90416352203497));
#259479=CARTESIAN_POINT('',(-3.93117425036855,-0.0034247740854032,6.65416352203497));
#259480=CARTESIAN_POINT('Ctrl Pts',(-3.93908469165526,0.000926690287404459,
7.90416352203497));
#259481=CARTESIAN_POINT('Ctrl Pts',(-3.93924795559323,0.0519846458656478,
7.90156967179267));
#259482=CARTESIAN_POINT('Ctrl Pts',(-3.91527744507353,1.40055255217221,
7.83305165488378));
#259483=CARTESIAN_POINT('Ctrl Pts',(-2.37754416811895,3.98829885572659,
7.69860947130798));
#259484=CARTESIAN_POINT('Ctrl Pts',(2.04694591492513,4.16764399334989,7.50083697130812));
#259485=CARTESIAN_POINT('Ctrl Pts',(4.60972494745586,0.556488942156041,
7.30306447130803));
#259486=CARTESIAN_POINT('Ctrl Pts',(2.97992819577477,-3.56079653756905,
7.1052919713081));
#259487=CARTESIAN_POINT('Ctrl Pts',(-1.36013325384479,-4.43951366319872,
6.90751947130804));
#259488=CARTESIAN_POINT('Ctrl Pts',(-3.71950508566899,-2.0375324526334,
6.75714332155038));
#259489=CARTESIAN_POINT('Ctrl Pts',(-3.93427653238721,-0.370036660280284,
6.67269133845934));
#259490=CARTESIAN_POINT('Ctrl Pts',(-3.93117425036855,-0.0034247740854032,
6.65416352203497));
#259491=CARTESIAN_POINT('',(-3.92771320559034,0.00202021301316996,5.40416352203497));
#259492=CARTESIAN_POINT('Ctrl Pts',(-3.93117425036855,-0.0034247740854032,
6.65416352203497));
#259493=CARTESIAN_POINT('Ctrl Pts',(-3.92323824529709,0.934411879900014,
6.60676717179267));
#259494=CARTESIAN_POINT('Ctrl Pts',(-3.11850751936548,3.1889329285567,6.49344665488371));
#259495=CARTESIAN_POINT('Ctrl Pts',(0.638898125826581,4.5990274209643,6.31420197130807));
#259496=CARTESIAN_POINT('Ctrl Pts',(4.2036098479625,1.97203151090957,6.11642947130806));
#259497=CARTESIAN_POINT('Ctrl Pts',(3.94511019507904,-2.44854029629629,
5.91865697130807));
#259498=CARTESIAN_POINT('Ctrl Pts',(0.0985063367380218,-4.64214826731606,
5.72088447130805));
#259499=CARTESIAN_POINT('Ctrl Pts',(-3.31475397322523,-2.88317796999455,
5.54938665488371));
#259500=CARTESIAN_POINT('Ctrl Pts',(-3.92402635340491,-0.784273446107112,
5.443813005126));
#259501=CARTESIAN_POINT('Ctrl Pts',(-3.92771320559034,0.00202021301316996,
5.40416352203497));
#259502=CARTESIAN_POINT('',(-3.93835609680327,0.00176884156033657,4.15416352203497));
#259503=CARTESIAN_POINT('Ctrl Pts',(-3.92771320559034,0.00202021301316996,
5.40416352203497));
#259504=CARTESIAN_POINT('Ctrl Pts',(-3.93015638686309,0.523076617291602,
5.37788883845933));
#259505=CARTESIAN_POINT('Ctrl Pts',(-3.59181156520463,2.34843854388582,
5.28568998821704));
#259506=CARTESIAN_POINT('Ctrl Pts',(-0.833417785374429,4.56778489316098,
5.12756697130806));
#259507=CARTESIAN_POINT('Ctrl Pts',(3.37464468803266,3.18920323300653,4.92979447130806));
#259508=CARTESIAN_POINT('Ctrl Pts',(4.51344516429205,-1.0899801753418,4.73202197130807));
#259509=CARTESIAN_POINT('Ctrl Pts',(1.54723696509406,-4.37781929912556,
4.53424947130806));
#259510=CARTESIAN_POINT('Ctrl Pts',(-2.71224270174677,-3.70207996991296,
4.34162998821703));
#259511=CARTESIAN_POINT('Ctrl Pts',(-3.93161373910733,-1.19505393419467,
4.21493467179267));
#259512=CARTESIAN_POINT('Ctrl Pts',(-3.93835609680327,0.00176884156033657,
4.15416352203497));
#259513=CARTESIAN_POINT('',(-3.93264116285329,-0.00353165188606064,2.90416352203497));
#259514=CARTESIAN_POINT('Ctrl Pts',(-3.93835609680327,0.00176884156033657,
4.15416352203497));
#259515=CARTESIAN_POINT('Ctrl Pts',(-3.93892780695442,0.103251996397657,
4.149010505126));
#259516=CARTESIAN_POINT('Ctrl Pts',(-3.88947668791503,1.50247512506948,
4.07793332155035));
#259517=CARTESIAN_POINT('Ctrl Pts',(-2.22189842665676,4.07705916880626,
3.94093197130807));
#259518=CARTESIAN_POINT('Ctrl Pts',(2.20621683484524,4.08556620217308,3.74315947130806));
#259519=CARTESIAN_POINT('Ctrl Pts',(4.62776308396295,0.378223395423315,
3.54538697130807));
#259520=CARTESIAN_POINT('Ctrl Pts',(2.84032772545949,-3.6731162177948,3.34761447130806));
#259521=CARTESIAN_POINT('Ctrl Pts',(-1.53040473322048,-4.38373180256663,
3.14984197130807));
#259522=CARTESIAN_POINT('Ctrl Pts',(-3.75680152222125,-1.93490720171295,
3.00202498821703));
#259523=CARTESIAN_POINT('Ctrl Pts',(-3.93548612495526,-0.319204885198335,
2.92013217179267));
#259524=CARTESIAN_POINT('Ctrl Pts',(-3.93264116285329,-0.00353165188606064,
2.90416352203497));
#259525=CARTESIAN_POINT('',(-3.92706270663355,0.00129905399659486,1.65416352203497));
#259526=CARTESIAN_POINT('Ctrl Pts',(-3.93264116285329,-0.00353165188606064,
2.90416352203497));
#259527=CARTESIAN_POINT('Ctrl Pts',(-3.92374112718673,0.984004538319144,
2.854208005126));
#259528=CARTESIAN_POINT('Ctrl Pts',(-3.04753415908209,3.28882845637856,
2.73832832155037));
#259529=CARTESIAN_POINT('Ctrl Pts',(0.815860814369345,4.57095274380756,
2.55652447130806));
#259530=CARTESIAN_POINT('Ctrl Pts',(4.27656469796981,1.8083818743231,2.35875197130806));
#259531=CARTESIAN_POINT('Ctrl Pts',(3.84770343210594,-2.59892886654929,
2.16097947130807));
#259532=CARTESIAN_POINT('Ctrl Pts',(-0.0806683086839,-4.64248789480798,
1.96320697130806));
#259533=CARTESIAN_POINT('Ctrl Pts',(-3.37364175399093,-2.78134286902773,
1.79426832155037));
#259534=CARTESIAN_POINT('Ctrl Pts',(-3.92487363956869,-0.734550070664457,
1.69125383845933));
#259535=CARTESIAN_POINT('Ctrl Pts',(-3.92706270663355,0.00129905399659486,
1.65416352203497));
#259536=CARTESIAN_POINT('Ctrl Pts',(-3.92706270663355,0.00129905399659486,
1.65416352203497));
#259537=CARTESIAN_POINT('Ctrl Pts',(-3.92876447782353,0.573344954566663,
1.62532967179267));
#259538=CARTESIAN_POINT('Ctrl Pts',(-3.54452519170164,2.45110582699664,
1.5305716548837));
#259539=CARTESIAN_POINT('Ctrl Pts',(-0.656570351814675,4.59650634559706,
1.36988947130806));
#259540=CARTESIAN_POINT('Ctrl Pts',(3.49518900507133,3.0566909045963,1.17211697130807));
#259541=CARTESIAN_POINT('Ctrl Pts',(4.46800855191978,-1.26342377815173,
0.974344471308062));
#259542=CARTESIAN_POINT('Ctrl Pts',(1.37722468627986,-4.43402775821398,
0.776571971308065));
#259543=CARTESIAN_POINT('Ctrl Pts',(-2.79693116634906,-3.60624455861583,
0.586511654883699));
#259544=CARTESIAN_POINT('Ctrl Pts',(-3.92873859619418,-1.14444899111955,
0.462375505126));
#259545=CARTESIAN_POINT('Ctrl Pts',(-3.93722999530371,0.00274405186980325,
0.404163522034968));
#259546=CARTESIAN_POINT('Origin',(0.,0.,-2.31077344927308));
#259547=CARTESIAN_POINT('Ctrl Pts',(-3.22274894448584,-0.00260831658724833,
19.5642265507269));
#259548=CARTESIAN_POINT('Ctrl Pts',(-3.22268270099715,-0.0844565608860859,
19.5693102004846));
#259549=CARTESIAN_POINT('Ctrl Pts',(-3.21949864137641,-0.166205662479208,
19.5743938502423));
#259550=CARTESIAN_POINT('Ctrl Pts',(-3.21321799883013,-0.24768458671075,
19.5794774999999));
#259551=CARTESIAN_POINT('Ctrl Pts',(-3.20537591739532,-0.349420094556691,
19.5858250026785));
#259552=CARTESIAN_POINT('Ctrl Pts',(-3.19268680426057,-0.450926465041492,
19.5921725053571));
#259553=CARTESIAN_POINT('Ctrl Pts',(-3.17517278854975,-0.551720332553758,
19.5985200080356));
#259554=CARTESIAN_POINT('Ctrl Pts',(-3.15768470707801,-0.65236494747302,
19.604858111519));
#259555=CARTESIAN_POINT('Ctrl Pts',(-3.13538601009322,-0.752298763341892,
19.6111962150024));
#259556=CARTESIAN_POINT('Ctrl Pts',(-3.10835063807583,-0.851042815182392,
19.6175343184858));
#259557=CARTESIAN_POINT('Ctrl Pts',(-3.07996430191294,-0.954721131420382,
19.6241891385489));
#259558=CARTESIAN_POINT('Ctrl Pts',(-3.04635564880892,-1.05708724839055,
19.630843958612));
#259559=CARTESIAN_POINT('Ctrl Pts',(-3.00767141738148,-1.15759673788694,
19.637498778675));
#259560=CARTESIAN_POINT('Ctrl Pts',(-2.97091947693275,-1.25308574299826,
19.6438211881331));
#259561=CARTESIAN_POINT('Ctrl Pts',(-2.92958690288105,-1.34689867276782,
19.6501435975912));
#259562=CARTESIAN_POINT('Ctrl Pts',(-2.88385076064012,-1.43858345355958,
19.6564660070493));
#259563=CARTESIAN_POINT('Ctrl Pts',(-2.83814591721452,-1.53020549130214,
19.6627840898651));
#259564=CARTESIAN_POINT('Ctrl Pts',(-2.78804368302485,-1.61970191747214,
19.669102172681));
#259565=CARTESIAN_POINT('Ctrl Pts',(-2.73376870195253,-1.70664180387238,
19.6754202554968));
#259566=CARTESIAN_POINT('Ctrl Pts',(-2.67951945686945,-1.79354046531157,
19.6817353424182));
#259567=CARTESIAN_POINT('Ctrl Pts',(-2.62110161771166,-1.87788465763653,
19.6880504293396));
#259568=CARTESIAN_POINT('Ctrl Pts',(-2.55878480582845,-1.95926973129314,
19.6943655162611));
#259569=CARTESIAN_POINT('Ctrl Pts',(-2.49648445582225,-2.04063330591869,
19.700678934962));
#259570=CARTESIAN_POINT('Ctrl Pts',(-2.43028743041509,-2.11903899800435,
19.7069923536629));
#259571=CARTESIAN_POINT('Ctrl Pts',(-2.3605051650532,-2.19411324417342,
19.7133057723638));
#259572=CARTESIAN_POINT('Ctrl Pts',(-2.29070847910578,-2.26920300452192,
19.7196204957399));
#259573=CARTESIAN_POINT('Ctrl Pts',(-2.21732534519101,-2.34095964406943,
19.7259352191161));
#259574=CARTESIAN_POINT('Ctrl Pts',(-2.14070560633903,-2.40904484588574,
19.7322499424923));
#259575=CARTESIAN_POINT('Ctrl Pts',(-2.06407817695149,-2.47713688160247,
19.7385652996947));
#259576=CARTESIAN_POINT('Ctrl Pts',(-1.98421380250134,-2.54155648191869,
19.7448806568971));
#259577=CARTESIAN_POINT('Ctrl Pts',(-1.9014962663222,-2.60200490231336,
19.7511960140996));
#259578=CARTESIAN_POINT('Ctrl Pts',(-1.81872555031785,-2.66249218552453,
19.7575154315002));
#259579=CARTESIAN_POINT('Ctrl Pts',(-1.73309834020476,-2.71900295700267,
19.7638348489009));
#259580=CARTESIAN_POINT('Ctrl Pts',(-1.6450281803835,-2.77128126473011,
19.7701542663016));
#259581=CARTESIAN_POINT('Ctrl Pts',(-1.61206509949341,-2.79084809746795,
19.7725195108677));
#259582=CARTESIAN_POINT('Ctrl Pts',(-1.57876005794138,-2.80982246879779,
19.7748847554338));
#259583=CARTESIAN_POINT('Ctrl Pts',(-1.54513563095214,-2.82819261091994,
19.77725));
#259584=CARTESIAN_POINT('Origin',(0.,0.,19.5));
#259585=CARTESIAN_POINT('Ctrl Pts',(-3.55851891020094,1.66656297071707,
19.0705612398686));
#259586=CARTESIAN_POINT('Ctrl Pts',(-3.59687330580814,1.55040695638482,
19.0850916788804));
#259587=CARTESIAN_POINT('Ctrl Pts',(-3.6298262220845,1.43277962313427,19.099504081714));
#259588=CARTESIAN_POINT('Ctrl Pts',(-3.65724210796529,1.31411610773058,
19.1138295224127));
#259589=CARTESIAN_POINT('Ctrl Pts',(-3.68417457330094,1.19754496977377,
19.1279023645857));
#259590=CARTESIAN_POINT('Ctrl Pts',(-3.70576340599889,1.07997411133984,
19.1418913836265));
#259591=CARTESIAN_POINT('Ctrl Pts',(-3.72187102178874,0.961821544164156,
19.15585840718));
#259592=CARTESIAN_POINT('Ctrl Pts',(-3.73769233592671,0.845769056577946,
19.1695771766176));
#259593=CARTESIAN_POINT('Ctrl Pts',(-3.74822573132689,0.729155654508635,
19.1832748790167));
#259594=CARTESIAN_POINT('Ctrl Pts',(-3.75333170678875,0.61237871638476,
19.1970397591525));
#259595=CARTESIAN_POINT('Ctrl Pts',(-3.75558091286343,0.560937928904781,
19.203103253239));
#259596=CARTESIAN_POINT('Ctrl Pts',(-3.75677682158521,0.509465397590146,
19.2091801600778));
#259597=CARTESIAN_POINT('Ctrl Pts',(-3.7569066961667,0.457994939495345,
19.2152797608931));
#259598=CARTESIAN_POINT('Ctrl Pts',(-3.75697600074545,0.430528915151644,
19.2185346723643));
#259599=CARTESIAN_POINT('Ctrl Pts',(-3.75674173389767,0.40306347870438,
19.221796063762));
#259600=CARTESIAN_POINT('Ctrl Pts',(-3.75620188182415,0.375603748088969,
19.2250654637997));
#259601=CARTESIAN_POINT('Ctrl Pts',(-3.75585189969696,0.357801806771246,
19.2271849917889));
#259602=CARTESIAN_POINT('Ctrl Pts',(-3.75537348402805,0.340002263203687,
19.2293078873353));
#259603=CARTESIAN_POINT('Ctrl Pts',(-3.75476607182455,0.32220650793041,
19.2314345849014));
#259604=CARTESIAN_POINT('Ctrl Pts',(-3.75432939366825,0.309412860456961,
19.2329635011247));
#259605=CARTESIAN_POINT('Ctrl Pts',(-3.75382607099664,0.296622655712598,
19.2344942061387));
#259606=CARTESIAN_POINT('Ctrl Pts',(-3.75325632212278,0.283843398119468,
19.236026023707));
#259607=CARTESIAN_POINT('Ctrl Pts',(-3.7489693790417,0.187688842255025,
19.2475518292456));
#259608=CARTESIAN_POINT('Ctrl Pts',(-3.74091892861043,0.0920269731287933,
19.2591552753384));
#259609=CARTESIAN_POINT('Ctrl Pts',(-3.72908658133375,-0.00295912595350346,
19.2709122445952));
#259610=CARTESIAN_POINT('Ctrl Pts',(2.28383702403548,-3.20593235360934,
-0.412058650086213));
#259611=CARTESIAN_POINT('Ctrl Pts',(3.3469402646796,-2.44868256130438,-0.34609107865597));
#259612=CARTESIAN_POINT('Ctrl Pts',(4.64210938897443,0.19229506283688,-0.214199340559059));
#259613=CARTESIAN_POINT('Ctrl Pts',(2.36472936830208,4.00381224408868,-0.0163834357954821));
#259614=CARTESIAN_POINT('Ctrl Pts',(-2.06494558101047,4.16156058203527,
0.181389064204519));
#259615=CARTESIAN_POINT('Ctrl Pts',(-4.61545750661852,0.540050558253595,
0.379161564204519));
#259616=CARTESIAN_POINT('Ctrl Pts',(-2.96874505650394,-3.57559009225921,
0.57693406420452));
#259617=CARTESIAN_POINT('Ctrl Pts',(1.37835608349618,-4.43767033499375,
0.774706564204519));
#259618=CARTESIAN_POINT('Ctrl Pts',(4.47167904409764,-1.26446168733233,
0.97247906420452));
#259619=CARTESIAN_POINT('Ctrl Pts',(3.49806032095048,3.05920199201367,1.17025156420451));
#259620=CARTESIAN_POINT('Ctrl Pts',(-0.657109727760937,4.60028239937832,
1.36802406420452));
#259621=CARTESIAN_POINT('Ctrl Pts',(-4.21461215365385,1.95748915205319,
1.56579656420451));
#259622=CARTESIAN_POINT('Ctrl Pts',(-3.93890797286949,-2.46571316296779,
1.76356906420452));
#259623=CARTESIAN_POINT('Ctrl Pts',(-0.0807345781174718,-4.64630172267007,
1.96134156420452));
#259624=CARTESIAN_POINT('Ctrl Pts',(3.85086434041363,-2.60106390008049,
2.15911406420451));
#259625=CARTESIAN_POINT('Ctrl Pts',(4.2800779180295,1.80986746940371,2.35688656420452));
#259626=CARTESIAN_POINT('Ctrl Pts',(0.816531048256037,4.57470780517246,
2.55465906420451));
#259627=CARTESIAN_POINT('Ctrl Pts',(-3.38965584783304,3.17882299039181,
2.75243156420452));
#259628=CARTESIAN_POINT('Ctrl Pts',(-4.51292822741089,-1.10822387779583,
2.95020406420452));
#259629=CARTESIAN_POINT('Ctrl Pts',(-1.53166196863923,-4.38733306095833,
3.14797656420451));
#259630=CARTESIAN_POINT('Ctrl Pts',(2.84266106940413,-3.67613370180096,
3.34574906420452));
#259631=CARTESIAN_POINT('Ctrl Pts',(4.63156481531668,0.378534107902338,
3.54352156420453));
#259632=CARTESIAN_POINT('Ctrl Pts',(2.20802925340745,4.08892251597919,3.74129406420452));
#259633=CARTESIAN_POINT('Ctrl Pts',(-2.22372372772789,4.08040849403945,
3.93906656420452));
#259634=CARTESIAN_POINT('Ctrl Pts',(-4.63298505560038,0.360735531134475,
4.13683906420452));
#259635=CARTESIAN_POINT('Ctrl Pts',(-2.8285153723176,-3.68702880618816,
4.33461156420452));
#259636=CARTESIAN_POINT('Ctrl Pts',(1.54850802827834,-4.38141570036494,
4.53238406420451));
#259637=CARTESIAN_POINT('Ctrl Pts',(4.51715298288247,-1.09087559970398,
4.73015656420452));
#259638=CARTESIAN_POINT('Ctrl Pts',(3.37741697613064,3.1918231799883,4.92792906420452));
#259639=CARTESIAN_POINT('Ctrl Pts',(-0.834102442403632,4.57153735212035,
5.12570156420453));
#259640=CARTESIAN_POINT('Ctrl Pts',(-4.28700009044229,1.79340761385376,
5.32347406420452));
#259641=CARTESIAN_POINT('Ctrl Pts',(-3.84084237808476,-2.61583838787399,
5.52124656420452));
#259642=CARTESIAN_POINT('Ctrl Pts',(0.0985872602042438,-4.64596181617238,
5.71901906420452));
#259643=CARTESIAN_POINT('Ctrl Pts',(3.94835112354715,-2.45055178483769,
5.91679156420453));
#259644=CARTESIAN_POINT('Ctrl Pts',(4.20706313523509,1.97365154501452,6.11456406420452));
#259645=CARTESIAN_POINT('Ctrl Pts',(0.639422983947544,4.60280554582189,
6.31233656420453));
#259646=CARTESIAN_POINT('Ctrl Pts',(-3.50977666360783,3.04567700464268,
6.51010906420451));
#259647=CARTESIAN_POINT('Ctrl Pts',(-4.46681087492398,-1.28151521749841,
6.70788156420452));
#259648=CARTESIAN_POINT('Ctrl Pts',(-1.36125061036072,-4.44316074667783,
6.90565406420451));
#259649=CARTESIAN_POINT('Ctrl Pts',(2.98237622222907,-3.5637217503761,7.10342656420454));
#259650=CARTESIAN_POINT('Ctrl Pts',(4.61351186038695,0.556946100705404,
7.30119906420452));
#259651=CARTESIAN_POINT('Ctrl Pts',(2.04862749160126,4.17106773448699,7.49897156420452));
#259652=CARTESIAN_POINT('Ctrl Pts',(-2.37949733297311,3.99157526390221,
7.69674406420453));
#259653=CARTESIAN_POINT('Ctrl Pts',(-4.64345335994372,0.181718295858487,
7.89451656420453));
#259654=CARTESIAN_POINT('Ctrl Pts',(-2.6841573851303,-3.79341268212052,
8.09228906420453));
#259655=CARTESIAN_POINT('Ctrl Pts',(1.71639774986823,-4.31840936101126,
8.29006156420452));
#259656=CARTESIAN_POINT('Ctrl Pts',(4.55587760940055,-0.915783737126305,
8.48783406420454));
#259657=CARTESIAN_POINT('Ctrl Pts',(3.25175620015281,3.31975334321544,8.68560656420453));
#259658=CARTESIAN_POINT('Ctrl Pts',(-1.0098593017621,4.53595247281834,8.88337906420453));
#259659=CARTESIAN_POINT('Ctrl Pts',(-4.35300098966657,1.62667237911762,
9.08115156420452));
#259660=CARTESIAN_POINT('Ctrl Pts',(-3.73705905632412,-2.76207716303657,
9.27892406420453));
#259661=CARTESIAN_POINT('Ctrl Pts',(0.277763175149986,-4.63869898393428,
9.47669656420453));
#259662=CARTESIAN_POINT('Ctrl Pts',(4.03995793423611,-2.29639293994407,
9.67446906420453));
#259663=CARTESIAN_POINT('Ctrl Pts',(4.12778383240777,2.13449789832069,9.87224156420453));
#259664=CARTESIAN_POINT('Ctrl Pts',(0.461362625713666,4.6240485694483,10.0700140642046));
#259665=CARTESIAN_POINT('Ctrl Pts',(-3.62467098613596,2.9079960260094,10.2677865642046));
#259666=CARTESIAN_POINT('Ctrl Pts',(-4.41404200413699,-1.45289842409465,
10.4655590642046));
#259667=CARTESIAN_POINT('Ctrl Pts',(-1.18881218846961,-4.49237200436122,
10.6633315642046));
#259668=CARTESIAN_POINT('Ctrl Pts',(3.11765029295676,-3.44600308993607,
10.8611040642046));
#259669=CARTESIAN_POINT('Ctrl Pts',(4.58858890454678,0.734528767368906,
11.0588765642046));
#259670=CARTESIAN_POINT('Ctrl Pts',(1.88617510483447,4.24700177995311,11.2566490642046));
#259671=CARTESIAN_POINT('Ctrl Pts',(-2.5317276143798,3.89679816408415,11.4544215642046));
#259672=CARTESIAN_POINT('Ctrl Pts',(-4.64700707314824,0.00243045926715866,
11.6521940642046));
#259673=CARTESIAN_POINT('Ctrl Pts',(-2.53580240411764,-3.8941477645683,
11.8499665642046));
#259674=CARTESIAN_POINT('Ctrl Pts',(1.88173157397906,-4.24897245560811,
12.0477390642046));
#259675=CARTESIAN_POINT('Ctrl Pts',(4.58781805371527,-0.739328175456174,
12.2455115642046));
#259676=CARTESIAN_POINT('Ctrl Pts',(3.12125321615583,3.44274004328707,12.4432840642046));
#259677=CARTESIAN_POINT('Ctrl Pts',(-1.18411237407708,4.4936130819872,12.6410565642046));
#259678=CARTESIAN_POINT('Ctrl Pts',(-4.41251981128717,1.45751485755395,
12.8388290642046));
#259679=CARTESIAN_POINT('Ctrl Pts',(-3.62771085945,-2.90420291391904,13.0366015642046));
#259680=CARTESIAN_POINT('Ctrl Pts',(0.456525471432565,-4.62452863967124,
13.2343740642046));
#259681=CARTESIAN_POINT('Ctrl Pts',(4.12554882142769,-2.13881452369848,
13.4321465642046));
#259682=CARTESIAN_POINT('Ctrl Pts',(4.04235782408847,2.29216575903919,13.6299190642046));
#259683=CARTESIAN_POINT('Ctrl Pts',(0.282615249824077,4.63840589716145,
13.8276915642046));
#259684=CARTESIAN_POINT('Ctrl Pts',(-3.73416779116287,2.76598473430493,
14.0254640642046));
#259685=CARTESIAN_POINT('Ctrl Pts',(-4.35470015938386,-1.62211811119156,
14.2232365642046));
#259686=CARTESIAN_POINT('Ctrl Pts',(-1.01460349953272,-4.53489364724057,
14.4210090642046));
#259687=CARTESIAN_POINT('Ctrl Pts',(3.24828185297365,-3.32315296559463,
14.6187815642046));
#259688=CARTESIAN_POINT('Ctrl Pts',(4.55683305695415,0.911017639724529,
14.8165540642046));
#259689=CARTESIAN_POINT('Ctrl Pts',(1.72091400224631,4.31661159850661,15.0143265642046));
#259690=CARTESIAN_POINT('Ctrl Pts',(-2.68018788222611,3.79621830794186,
15.2120990642046));
#259691=CARTESIAN_POINT('Ctrl Pts',(-4.64364091052774,-0.17686097194712,
15.4098715642046));
#259692=CARTESIAN_POINT('Ctrl Pts',(-2.38367133079787,-3.98908409735304,
15.6076440642046));
#259693=CARTESIAN_POINT('Ctrl Pts',(2.04426327244963,-4.17320829181426,
15.8054165642046));
#259694=CARTESIAN_POINT('Ctrl Pts',(4.61292680830011,-0.561771849014371,
16.0031890642046));
#259695=CARTESIAN_POINT('Ctrl Pts',(2.98610225103185,3.56060047146191,16.2009615642046));
#259696=CARTESIAN_POINT('Ctrl Pts',(-1.35660197535887,4.44458159289761,
16.3987340642046));
#259697=CARTESIAN_POINT('Ctrl Pts',(-4.46546831401767,1.28618815797446,
16.5965065642045));
#259698=CARTESIAN_POINT('Ctrl Pts',(-3.51295987415327,-3.04200632858649,
16.7942790642046));
#259699=CARTESIAN_POINT('Ctrl Pts',(0.634606527243763,-4.60346742421083,
16.9920515642045));
#259700=CARTESIAN_POINT('Ctrl Pts',(4.20499906287745,-1.97805973164798,
17.1898240642046));
#259701=CARTESIAN_POINT('Ctrl Pts',(3.95090708561034,2.44643671224224,17.3875965642045));
#259702=CARTESIAN_POINT('Ctrl Pts',(0.103457054932767,4.6458247907269,17.5853690642046));
#259703=CARTESIAN_POINT('Ctrl Pts',(-3.83812323138877,2.61991467372935,
17.7831415642046));
#259704=CARTESIAN_POINT('Ctrl Pts',(-4.28883691552302,-1.78903737920712,
17.9809140642046));
#259705=CARTESIAN_POINT('Ctrl Pts',(-0.838954441256415,-4.57044187584642,
18.1786865642046));
#259706=CARTESIAN_POINT('Ctrl Pts',(3.37421140880478,-3.19577675801525,
18.3764590642046));
#259707=CARTESIAN_POINT('Ctrl Pts',(4.51803287068356,1.08695978779998,18.5742315642046));
#259708=CARTESIAN_POINT('Ctrl Pts',(1.55358642717095,4.3782366249204,18.7720040642046));
#259709=CARTESIAN_POINT('Ctrl Pts',(-2.82561198434755,3.6930169760152,18.9697765642046));
#259710=CARTESIAN_POINT('Ctrl Pts',(-4.63188723191833,-0.363030295585548,
19.1675926032154));
#259711=CARTESIAN_POINT('Ctrl Pts',(-3.03081717849875,-2.83058498061266,
19.2994844755598));
#259712=CARTESIAN_POINT('Ctrl Pts',(-1.88494306520931,-3.45556123458669,
19.3654521812374));
#259713=CARTESIAN_POINT('Ctrl Pts',(2.14474796587059,-3.01068632383087,
-0.273654916792053));
#259714=CARTESIAN_POINT('Ctrl Pts',(3.14310664422014,-2.29955416570856,
-0.207687345361809));
#259715=CARTESIAN_POINT('Ctrl Pts',(4.35939805011098,0.180584008633708,
-0.075795607264898));
#259716=CARTESIAN_POINT('Ctrl Pts',(2.22071384653295,3.75997414695711,0.122020297498679));
#259717=CARTESIAN_POINT('Ctrl Pts',(-1.93918733600355,3.9081153774257,0.319792797498679));
#259718=CARTESIAN_POINT('Ctrl Pts',(-4.3343693068741,0.507160679195471,
0.51756529749868));
#259719=CARTESIAN_POINT('Ctrl Pts',(-2.78794408450143,-3.35783135856578,
0.715337797498679));
#259720=CARTESIAN_POINT('Ctrl Pts',(1.29441215603915,-4.16740963738492,
0.913110297498681));
#259721=CARTESIAN_POINT('Ctrl Pts',(4.19934716572204,-1.18745409733102,
1.11088279749868));
#259722=CARTESIAN_POINT('Ctrl Pts',(3.28502326518657,2.8728920586308,1.30865529749868));
#259723=CARTESIAN_POINT('Ctrl Pts',(-0.617090771862006,4.32011838614606,
1.50642779749868));
#259724=CARTESIAN_POINT('Ctrl Pts',(-3.95793602973923,1.83827516276157,
1.70420029749868));
#259725=CARTESIAN_POINT('Ctrl Pts',(-3.69902264200789,-2.31554757850064,
1.90197279749868));
#259726=CARTESIAN_POINT('Ctrl Pts',(-0.0758177227054686,-4.3633350644738,
2.09974529749868));
#259727=CARTESIAN_POINT('Ctrl Pts',(3.61634099720126,-2.44265525520715,
2.29751779749868));
#259728=CARTESIAN_POINT('Ctrl Pts',(4.01941483207982,1.69964385928032,2.49529029749868));
#259729=CARTESIAN_POINT('Ctrl Pts',(0.766803097763436,4.29610132261495,
2.69306279749868));
#259730=CARTESIAN_POINT('Ctrl Pts',(-3.18322078507834,2.98522796099457,
2.89083529749868));
#259731=CARTESIAN_POINT('Ctrl Pts',(-4.23808421266269,-1.04073140185459,
3.08860779749868));
#259732=CARTESIAN_POINT('Ctrl Pts',(-1.43838148566121,-4.12013797791067,
3.28638029749868));
#259733=CARTESIAN_POINT('Ctrl Pts',(2.66953879900375,-3.45225171333561,
3.48415279749868));
#259734=CARTESIAN_POINT('Ctrl Pts',(4.3494956566103,0.355480819949967,3.68192529749868));
#259735=CARTESIAN_POINT('Ctrl Pts',(2.07355700077952,3.83990107720247,3.87969779749868));
#259736=CARTESIAN_POINT('Ctrl Pts',(-2.08829565836325,3.83190557181197,
4.07747029749868));
#259737=CARTESIAN_POINT('Ctrl Pts',(-4.35082940215671,0.338766202875003,
4.27524279749868));
#259738=CARTESIAN_POINT('Ctrl Pts',(-2.65625459582596,-3.46248328972505,
4.47301529749868));
#259739=CARTESIAN_POINT('Ctrl Pts',(1.45420159531167,-4.1145809933437,4.67078779749869));
#259740=CARTESIAN_POINT('Ctrl Pts',(4.24205167426729,-1.02443965959917,
4.86856029749868));
#259741=CARTESIAN_POINT('Ctrl Pts',(3.17172727879392,2.99743641978549,5.06633279749868));
#259742=CARTESIAN_POINT('Ctrl Pts',(-0.783304367976271,4.29312395485058,
5.26410529749868));
#259743=CARTESIAN_POINT('Ctrl Pts',(-4.0259154339378,1.68418643331785,5.46187779749868));
#259744=CARTESIAN_POINT('Ctrl Pts',(-3.60692938722528,-2.45652995480633,
5.65965029749867));
#259745=CARTESIAN_POINT('Ctrl Pts',(0.0925831500052695,-4.36301585878538,
5.85742279749869));
#259746=CARTESIAN_POINT('Ctrl Pts',(3.70789069081969,-2.30130955075952,
6.05519529749868));
#259747=CARTESIAN_POINT('Ctrl Pts',(3.95084675772568,1.85345324204774,6.25296779749868));
#259748=CARTESIAN_POINT('Ctrl Pts',(0.600481176948914,4.32248786923329,
6.45074029749868));
#259749=CARTESIAN_POINT('Ctrl Pts',(-3.29602606521889,2.86019076302732,
6.64851279749868));
#259750=CARTESIAN_POINT('Ctrl Pts',(-4.194775475263,-1.20346904224601,6.84628529749869));
#259751=CARTESIAN_POINT('Ctrl Pts',(-1.27834843155858,-4.17256567486365,
7.04405779749867));
#259752=CARTESIAN_POINT('Ctrl Pts',(2.80074509203999,-3.34668581628575,
7.24183029749869));
#259753=CARTESIAN_POINT('Ctrl Pts',(4.33254215338042,0.523027258082037,
7.43960279749867));
#259754=CARTESIAN_POINT('Ctrl Pts',(1.92386304241383,3.91704353020872,7.6373752974987));
#259755=CARTESIAN_POINT('Ctrl Pts',(-2.23458242027749,3.7484824169925,7.83514779749867));
#259756=CARTESIAN_POINT('Ctrl Pts',(-4.36066017125721,0.170651382433251,
8.0329202974987));
#259757=CARTESIAN_POINT('Ctrl Pts',(-2.5206882239182,-3.56238823001025,
8.23069279749867));
#259758=CARTESIAN_POINT('Ctrl Pts',(1.61186658413571,-4.05541183339768,
8.42846529749869));
#259759=CARTESIAN_POINT('Ctrl Pts',(4.27841791366164,-0.860011150843142,
8.62623779749867));
#259760=CARTESIAN_POINT('Ctrl Pts',(3.05371943023388,3.11757544654935,8.82401029749869));
#259761=CARTESIAN_POINT('Ctrl Pts',(-0.948357374223968,4.25970624741547,
9.02178279749868));
#259762=CARTESIAN_POINT('Ctrl Pts',(-4.08789678062198,1.52760562138784,
9.21955529749868));
#259763=CARTESIAN_POINT('Ctrl Pts',(-3.50946662351017,-2.59386257191539,
9.41732779749867));
#259764=CARTESIAN_POINT('Ctrl Pts',(0.260846986289807,-4.35619534379014,
9.61510029749869));
#259765=CARTESIAN_POINT('Ctrl Pts',(3.79391851102637,-2.15653920789927,
9.81287279749867));
#259766=CARTESIAN_POINT('Ctrl Pts',(3.87639568188924,2.00450381415097,10.0106452974987));
#259767=CARTESIAN_POINT('Ctrl Pts',(0.433264958319839,4.34243716125028,
10.2084177974987));
#259768=CARTESIAN_POINT('Ctrl Pts',(-3.40392315329433,2.73089475996095,
10.4061902974987));
#259769=CARTESIAN_POINT('Ctrl Pts',(-4.14522030688164,-1.36441475766407,
10.6039627974987));
#259770=CARTESIAN_POINT('Ctrl Pts',(-1.11641176502036,-4.21877989404988,
10.8017352974987));
#259771=CARTESIAN_POINT('Ctrl Pts',(2.92778077145794,-3.23613639666138,
10.9995077974987));
#259772=CARTESIAN_POINT('Ctrl Pts',(4.30913704247314,0.689794877265052,
11.1972802974987));
#259773=CARTESIAN_POINT('Ctrl Pts',(1.771304246667,3.9883530798131,11.3950527974987));
#259774=CARTESIAN_POINT('Ctrl Pts',(-2.37754165202425,3.65947738296135,
11.5928252974987));
#259775=CARTESIAN_POINT('Ctrl Pts',(-4.3639974580629,0.0022824406971417,
11.7905977974987));
#259776=CARTESIAN_POINT('Ctrl Pts',(-2.38136828103039,-3.65698839670247,
11.9883702974987));
#259777=CARTESIAN_POINT('Ctrl Pts',(1.76713133342362,-3.99020373840124,
12.1861427974987));
#259778=CARTESIAN_POINT('Ctrl Pts',(4.30841313759926,-0.694301994289642,
12.3839152974987));
#259779=CARTESIAN_POINT('Ctrl Pts',(2.93116427129658,3.23307207438738,12.5816877974987));
#259780=CARTESIAN_POINT('Ctrl Pts',(-1.11199817628692,4.21994538820984,
12.7794602974987));
#259781=CARTESIAN_POINT('Ctrl Pts',(-4.14379081783146,1.36875004348661,
12.9772327974987));
#259782=CARTESIAN_POINT('Ctrl Pts',(-3.40677789382007,-2.72733265401625,
13.1750052974987));
#259783=CARTESIAN_POINT('Ctrl Pts',(0.428722393900526,-4.34288799448544,
13.3727777974987));
#259784=CARTESIAN_POINT('Ctrl Pts',(3.87429678638894,-2.00855755064833,
13.5705502974987));
#259785=CARTESIAN_POINT('Ctrl Pts',(3.79617224403135,2.15256946857392,13.7683227974987));
#259786=CARTESIAN_POINT('Ctrl Pts',(0.265403562428066,4.35592010643597,
13.9660952974987));
#259787=CARTESIAN_POINT('Ctrl Pts',(-3.50675144068053,2.59753216630456,
14.1638677974987));
#259788=CARTESIAN_POINT('Ctrl Pts',(-4.08949246838623,-1.52332871512547,
14.3616402974987));
#259789=CARTESIAN_POINT('Ctrl Pts',(-0.952812643321995,-4.25871190588399,
14.5594127974987));
#259790=CARTESIAN_POINT('Ctrl Pts',(3.05045667594506,-3.12076802688922,
14.7571852974987));
#259791=CARTESIAN_POINT('Ctrl Pts',(4.27931517304376,0.855535315833938,
14.9549577974987));
#259792=CARTESIAN_POINT('Ctrl Pts',(1.6161077900533,4.0537235572929,15.1527302974987));
#259793=CARTESIAN_POINT('Ctrl Pts',(-2.51696046962155,3.56502298906262,
15.3505027974987));
#259794=CARTESIAN_POINT('Ctrl Pts',(-4.36083629973281,-0.166089876744038,
15.5482752974987));
#259795=CARTESIAN_POINT('Ctrl Pts',(-2.23850221545109,-3.74614296617676,
15.7460477974987));
#259796=CARTESIAN_POINT('Ctrl Pts',(1.91976461067398,-3.91905372442359,
15.9438202974987));
#259797=CARTESIAN_POINT('Ctrl Pts',(4.3319927318324,-0.52755911116981,16.1415927974987));
#259798=CARTESIAN_POINT('Ctrl Pts',(2.80424420016869,3.34375462788149,16.3393652974987));
#259799=CARTESIAN_POINT('Ctrl Pts',(-1.27398290531514,4.17389998944372,
16.5371377974987));
#259800=CARTESIAN_POINT('Ctrl Pts',(-4.19351467830484,1.20785739372427,
16.7349102974987));
#259801=CARTESIAN_POINT('Ctrl Pts',(-3.2990154135263,-2.85674363658093,
16.9326827974987));
#259802=CARTESIAN_POINT('Ctrl Pts',(0.595958049593802,-4.3231094382478,
17.1304552974987));
#259803=CARTESIAN_POINT('Ctrl Pts',(3.94890839043248,-1.85759296358465,
17.3282277974988));
#259804=CARTESIAN_POINT('Ctrl Pts',(3.71029099100666,2.29744509218147,17.5260002974987));
#259805=CARTESIAN_POINT('Ctrl Pts',(0.0971563670203983,4.36288717839253,
17.7237727974988));
#259806=CARTESIAN_POINT('Ctrl Pts',(-3.60437584059141,2.46035798881423,
17.9215452974987));
#259807=CARTESIAN_POINT('Ctrl Pts',(-4.02764039364993,-1.68008235243554,
18.1193177974987));
#259808=CARTESIAN_POINT('Ctrl Pts',(-0.787860872910852,-4.29209519470465,
18.3170902974987));
#259809=CARTESIAN_POINT('Ctrl Pts',(3.16871693526713,-3.00114921905351,
18.5148627974987));
#259810=CARTESIAN_POINT('Ctrl Pts',(4.24287797559777,1.02076232644127,18.7126352974987));
#259811=CARTESIAN_POINT('Ctrl Pts',(1.45897071218826,4.11159552830341,18.9104077974987));
#259812=CARTESIAN_POINT('Ctrl Pts',(-2.65352802848456,3.46810677113839,
19.1081802974987));
#259813=CARTESIAN_POINT('Ctrl Pts',(-4.34979843756326,-0.340921212771463,
19.3059963365096));
#259814=CARTESIAN_POINT('Ctrl Pts',(-2.84623592230972,-2.65819816190986,
19.4378882088539));
#259815=CARTESIAN_POINT('Ctrl Pts',(-1.77014724008023,-3.24511243614284,
19.5038559145315));
#259816=CARTESIAN_POINT('Ctrl Pts',(2.00565890770568,-2.81544029405241,
-0.135251183497891));
#259817=CARTESIAN_POINT('Ctrl Pts',(2.93927302376069,-2.15042577011275,
-0.0692836120676477));
#259818=CARTESIAN_POINT('Ctrl Pts',(4.07668671124753,0.168872954430536,
0.0626081260292637));
#259819=CARTESIAN_POINT('Ctrl Pts',(2.07669832476383,3.51613604982555,0.26042403079284));
#259820=CARTESIAN_POINT('Ctrl Pts',(-1.81342909099665,3.65467017281614,
0.45819653079284));
#259821=CARTESIAN_POINT('Ctrl Pts',(-4.05328110712969,0.474270800137351,
0.655969030792841));
#259822=CARTESIAN_POINT('Ctrl Pts',(-2.60714311249892,-3.14007262487236,
0.853741530792841));
#259823=CARTESIAN_POINT('Ctrl Pts',(1.21046822858213,-3.89714893977609,
1.05151403079284));
#259824=CARTESIAN_POINT('Ctrl Pts',(3.92701528734643,-1.1104465073297,1.24928653079284));
#259825=CARTESIAN_POINT('Ctrl Pts',(3.07198620942266,2.68658212524793,1.44705903079284));
#259826=CARTESIAN_POINT('Ctrl Pts',(-0.577071815963079,4.03995437291379,
1.64483153079285));
#259827=CARTESIAN_POINT('Ctrl Pts',(-3.70125990582461,1.71906117346994,
1.84260403079284));
#259828=CARTESIAN_POINT('Ctrl Pts',(-3.45913731114628,-2.1653819940335,
2.04037653079284));
#259829=CARTESIAN_POINT('Ctrl Pts',(-0.0709008672934647,-4.08036840627753,
2.23814903079284));
#259830=CARTESIAN_POINT('Ctrl Pts',(3.38181765398889,-2.28424661033382,
2.43592153079284));
#259831=CARTESIAN_POINT('Ctrl Pts',(3.75875174613015,1.58942024915694,2.63369403079284));
#259832=CARTESIAN_POINT('Ctrl Pts',(0.717075147270833,4.01749484005744,
2.83146653079284));
#259833=CARTESIAN_POINT('Ctrl Pts',(-2.97678572232363,2.79163293159735,
3.02923903079284));
#259834=CARTESIAN_POINT('Ctrl Pts',(-3.96324019791451,-0.973238925913344,
3.22701153079285));
#259835=CARTESIAN_POINT('Ctrl Pts',(-1.34510100268319,-3.85294289486299,
3.42478403079284));
#259836=CARTESIAN_POINT('Ctrl Pts',(2.49641652860337,-3.22836972487026,
3.62255653079285));
#259837=CARTESIAN_POINT('Ctrl Pts',(4.06742649790391,0.332427531997598,
3.82032903079284));
#259838=CARTESIAN_POINT('Ctrl Pts',(1.93908474815161,3.59087963842575,4.01810153079285));
#259839=CARTESIAN_POINT('Ctrl Pts',(-1.95286758899861,3.5834026495845,4.21587403079284));
#259840=CARTESIAN_POINT('Ctrl Pts',(-4.06867374871303,0.316796874615529,
4.41364653079285));
#259841=CARTESIAN_POINT('Ctrl Pts',(-2.48399381933433,-3.23793777326195,
4.61141903079284));
#259842=CARTESIAN_POINT('Ctrl Pts',(1.359895162345,-3.84774628632246,4.80919153079285));
#259843=CARTESIAN_POINT('Ctrl Pts',(3.9669503656521,-0.958003719494359,
5.00696403079284));
#259844=CARTESIAN_POINT('Ctrl Pts',(2.96603758145719,2.80304965958268,5.20473653079285));
#259845=CARTESIAN_POINT('Ctrl Pts',(-0.732506293548905,4.01471055758082,
5.40250903079284));
#259846=CARTESIAN_POINT('Ctrl Pts',(-3.76483077743333,1.57496525278195,
5.60028153079285));
#259847=CARTESIAN_POINT('Ctrl Pts',(-3.3730163963658,-2.29722152173868,
5.79805403079284));
#259848=CARTESIAN_POINT('Ctrl Pts',(0.0865790398062952,-4.08006990139837,
5.99582653079285));
#259849=CARTESIAN_POINT('Ctrl Pts',(3.46743025809225,-2.15206731668136,
6.19359903079284));
#259850=CARTESIAN_POINT('Ctrl Pts',(3.69463038021628,1.73325493908096,6.39137153079286));
#259851=CARTESIAN_POINT('Ctrl Pts',(0.561539369950281,4.0421701926447,6.58914403079284));
#259852=CARTESIAN_POINT('Ctrl Pts',(-3.08227546682996,2.67470452141197,
6.78691653079286));
#259853=CARTESIAN_POINT('Ctrl Pts',(-3.92274007560203,-1.1254228669936,
6.98468903079284));
#259854=CARTESIAN_POINT('Ctrl Pts',(-1.19544625275643,-3.90197060304948,
7.18246153079285));
#259855=CARTESIAN_POINT('Ctrl Pts',(2.6191139618509,-3.12964988219538,7.38023403079285));
#259856=CARTESIAN_POINT('Ctrl Pts',(4.05157244637388,0.489108415458669,
7.57800653079284));
#259857=CARTESIAN_POINT('Ctrl Pts',(1.79909859322641,3.66301932593045,7.77577903079285));
#259858=CARTESIAN_POINT('Ctrl Pts',(-2.08966750758188,3.50538957008279,
7.97355153079285));
#259859=CARTESIAN_POINT('Ctrl Pts',(-4.0778669825707,0.159584469008015,
8.17132403079285));
#259860=CARTESIAN_POINT('Ctrl Pts',(-2.35721906270609,-3.33136377789996,
8.36909653079284));
#259861=CARTESIAN_POINT('Ctrl Pts',(1.50733541840319,-3.79241430578413,
8.56686903079285));
#259862=CARTESIAN_POINT('Ctrl Pts',(4.00095821792272,-0.804238564559976,
8.76464153079284));
#259863=CARTESIAN_POINT('Ctrl Pts',(2.85568266031496,2.91539754988326,8.96241403079285));
#259864=CARTESIAN_POINT('Ctrl Pts',(-0.886855446685837,3.98346002201258,
9.16018653079284));
#259865=CARTESIAN_POINT('Ctrl Pts',(-3.82279257157741,1.42853886365807,
9.35795903079284));
#259866=CARTESIAN_POINT('Ctrl Pts',(-3.28187419069619,-2.42564798079422,
9.55573153079285));
#259867=CARTESIAN_POINT('Ctrl Pts',(0.243930797429626,-4.07369170364599,
9.75350403079284));
#259868=CARTESIAN_POINT('Ctrl Pts',(3.54787908781661,-2.01668547585448,
9.95127653079285));
#259869=CARTESIAN_POINT('Ctrl Pts',(3.62500753137072,1.87450972998126,10.1490490307928));
#259870=CARTESIAN_POINT('Ctrl Pts',(0.405167290926007,4.06082575305226,
10.3468215307929));
#259871=CARTESIAN_POINT('Ctrl Pts',(-3.18317532045269,2.55379349391248,
10.5445940307928));
#259872=CARTESIAN_POINT('Ctrl Pts',(-3.87639860962629,-1.27593109123349,
10.7423665307929));
#259873=CARTESIAN_POINT('Ctrl Pts',(-1.04401134157109,-3.94518778373853,
10.9401390307929));
#259874=CARTESIAN_POINT('Ctrl Pts',(2.73791124995913,-3.02626970338668,
11.1379115307928));
#259875=CARTESIAN_POINT('Ctrl Pts',(4.0296851803995,0.645060987161196,11.3356840307929));
#259876=CARTESIAN_POINT('Ctrl Pts',(1.65643338849953,3.7297043796731,11.5334565307928));
#259877=CARTESIAN_POINT('Ctrl Pts',(-2.2233556896687,3.42215660183855,11.7312290307929));
#259878=CARTESIAN_POINT('Ctrl Pts',(-4.08098784297757,0.00213442212713404,
11.9290015307929));
#259879=CARTESIAN_POINT('Ctrl Pts',(-2.22693415794315,-3.41982902883666,
12.1267740307928));
#259880=CARTESIAN_POINT('Ctrl Pts',(1.65253109286818,-3.73143502119435,
12.3245465307929));
#259881=CARTESIAN_POINT('Ctrl Pts',(4.02900822148325,-0.649275813123116,
12.5223190307928));
#259882=CARTESIAN_POINT('Ctrl Pts',(2.74107532643733,3.0234041054877,12.7200915307929));
#259883=CARTESIAN_POINT('Ctrl Pts',(-1.03988397849677,3.94627769443245,
12.9178640307928));
#259884=CARTESIAN_POINT('Ctrl Pts',(-3.87506182437573,1.27998522941927,
13.1156365307929));
#259885=CARTESIAN_POINT('Ctrl Pts',(-3.18584492819014,-2.55046239411347,
13.3134090307928));
#259886=CARTESIAN_POINT('Ctrl Pts',(0.400919316368492,-4.06124734929963,
13.5111815307929));
#259887=CARTESIAN_POINT('Ctrl Pts',(3.6230447513502,-1.87830057759819,13.7089540307929));
#259888=CARTESIAN_POINT('Ctrl Pts',(3.54998666397424,2.01297317810865,13.9067265307929));
#259889=CARTESIAN_POINT('Ctrl Pts',(0.248191875032054,4.07343431571049,
14.1044990307928));
#259890=CARTESIAN_POINT('Ctrl Pts',(-3.27933509019819,2.42907959830422,
14.3022715307929));
#259891=CARTESIAN_POINT('Ctrl Pts',(-3.8242847773886,-1.42453931905938,
14.5000440307929));
#259892=CARTESIAN_POINT('Ctrl Pts',(-0.891021787111275,-3.9825301645274,
14.6978165307929));
#259893=CARTESIAN_POINT('Ctrl Pts',(2.85263149891647,-2.91838308818382,
14.8955890307928));
#259894=CARTESIAN_POINT('Ctrl Pts',(4.00179728913336,0.800052991943351,
15.0933615307929));
#259895=CARTESIAN_POINT('Ctrl Pts',(1.51130157786028,3.79083551607919,15.2911340307928));
#259896=CARTESIAN_POINT('Ctrl Pts',(-2.35373305701698,3.33382767018338,
15.4889065307929));
#259897=CARTESIAN_POINT('Ctrl Pts',(-4.07803168893789,-0.155318781540962,
15.6866790307929));
#259898=CARTESIAN_POINT('Ctrl Pts',(-2.09333310010432,-3.50320183500046,
15.8844515307929));
#259899=CARTESIAN_POINT('Ctrl Pts',(1.79526594889833,-3.66489915703294,
16.0822240307929));
#259900=CARTESIAN_POINT('Ctrl Pts',(4.0510586553647,-0.493346373325246,
16.2799965307929));
#259901=CARTESIAN_POINT('Ctrl Pts',(2.62238614930553,3.12690878430107,16.4777690307929));
#259902=CARTESIAN_POINT('Ctrl Pts',(-1.19136383527139,3.90321838598983,
16.6755415307929));
#259903=CARTESIAN_POINT('Ctrl Pts',(-3.92156104259203,1.12952662947407,
16.8733140307929));
#259904=CARTESIAN_POINT('Ctrl Pts',(-3.08507095289933,-2.67148094457537,
17.0710865307928));
#259905=CARTESIAN_POINT('Ctrl Pts',(0.557309571943842,-4.04275145228477,
17.2688590307928));
#259906=CARTESIAN_POINT('Ctrl Pts',(3.6928177179875,-1.73712619552131,17.4666315307929));
#259907=CARTESIAN_POINT('Ctrl Pts',(3.46967489640299,2.14845347212071,17.6644040307928));
#259908=CARTESIAN_POINT('Ctrl Pts',(0.0908556791080224,4.07994956605816,
17.8621765307929));
#259909=CARTESIAN_POINT('Ctrl Pts',(-3.37062844979403,2.3008013038991,18.0599490307929));
#259910=CARTESIAN_POINT('Ctrl Pts',(-3.76644387177684,-1.57112732566396,
18.2577215307929));
#259911=CARTESIAN_POINT('Ctrl Pts',(-0.736767304565286,-4.01374851356288,
18.4554940307928));
#259912=CARTESIAN_POINT('Ctrl Pts',(2.9632224617295,-2.80652168009177,18.6532665307929));
#259913=CARTESIAN_POINT('Ctrl Pts',(3.96772308051197,0.954564865082551,
18.8510390307928));
#259914=CARTESIAN_POINT('Ctrl Pts',(1.36435499720556,3.84495443168642,19.0488115307929));
#259915=CARTESIAN_POINT('Ctrl Pts',(-2.48144407262158,3.24319656626158,
19.2465840307929));
#259916=CARTESIAN_POINT('Ctrl Pts',(-4.06770964320818,-0.31881212995738,
19.4444000698038));
#259917=CARTESIAN_POINT('Ctrl Pts',(-2.66165466612069,-2.48581134320706,
19.5762919421481));
#259918=CARTESIAN_POINT('Ctrl Pts',(-1.65535141495114,-3.03466363769899,
19.6422596478257));
#259919=CARTESIAN_POINT('Ctrl Pts',(1.86656984954077,-2.62019426427394,
0.00315254979626938));
#259920=CARTESIAN_POINT('Ctrl Pts',(2.73543940330123,-2.00129737451693,
0.0691201212265132));
#259921=CARTESIAN_POINT('Ctrl Pts',(3.79397537238408,0.157161900227365,
0.201011859323424));
#259922=CARTESIAN_POINT('Ctrl Pts',(1.9326828029947,3.27229795269397,0.398827764087002));
#259923=CARTESIAN_POINT('Ctrl Pts',(-1.68767084598974,3.40122496820657,
0.596600264087));
#259924=CARTESIAN_POINT('Ctrl Pts',(-3.77219290738527,0.441380921079229,
0.794372764087002));
#259925=CARTESIAN_POINT('Ctrl Pts',(-2.4263421404964,-2.92231389117894,
0.992145264087002));
#259926=CARTESIAN_POINT('Ctrl Pts',(1.12652430112509,-3.62688824216726,
1.18991776408701));
#259927=CARTESIAN_POINT('Ctrl Pts',(3.65468340897082,-1.0334389173284,1.38769026408701));
#259928=CARTESIAN_POINT('Ctrl Pts',(2.85894915365876,2.50027219186506,1.58546276408701));
#259929=CARTESIAN_POINT('Ctrl Pts',(-0.537052860064148,3.75979035968154,
1.78323526408701));
#259930=CARTESIAN_POINT('Ctrl Pts',(-3.44458378191,1.59984718417832,1.98100776408701));
#259931=CARTESIAN_POINT('Ctrl Pts',(-3.21925198028467,-2.01521640956636,
2.17878026408701));
#259932=CARTESIAN_POINT('Ctrl Pts',(-0.0659840118814633,-3.79740174808127,
2.37655276408701));
#259933=CARTESIAN_POINT('Ctrl Pts',(3.14729431077653,-2.12583796546047,
2.57432526408699));
#259934=CARTESIAN_POINT('Ctrl Pts',(3.49808866018047,1.47919663903355,2.77209776408701));
#259935=CARTESIAN_POINT('Ctrl Pts',(0.667347196778231,3.73888835749994,
2.969870264087));
#259936=CARTESIAN_POINT('Ctrl Pts',(-2.77035065956893,2.59803790220012,
3.167642764087));
#259937=CARTESIAN_POINT('Ctrl Pts',(-3.68839618316631,-0.905746449972094,
3.36541526408701));
#259938=CARTESIAN_POINT('Ctrl Pts',(-1.25182051970517,-3.58574781181533,
3.56318776408701));
#259939=CARTESIAN_POINT('Ctrl Pts',(2.32329425820301,-3.00448773640491,
3.76096026408701));
#259940=CARTESIAN_POINT('Ctrl Pts',(3.78535733919753,0.309374244045226,
3.95873276408701));
#259941=CARTESIAN_POINT('Ctrl Pts',(1.8046124955237,3.34185819964903,4.156505264087));
#259942=CARTESIAN_POINT('Ctrl Pts',(-1.81743951963397,3.33489972735703,
4.354277764087));
#259943=CARTESIAN_POINT('Ctrl Pts',(-3.78651809526935,0.294827546356054,
4.55205026408701));
#259944=CARTESIAN_POINT('Ctrl Pts',(-2.31173304284269,-3.01339225679884,
4.74982276408699));
#259945=CARTESIAN_POINT('Ctrl Pts',(1.26558872937833,-3.58091157930122,
4.94759526408702));
#259946=CARTESIAN_POINT('Ctrl Pts',(3.69184905703692,-0.891567779389545,
5.145367764087));
#259947=CARTESIAN_POINT('Ctrl Pts',(2.76034788412047,2.60866289937987,5.34314026408701));
#259948=CARTESIAN_POINT('Ctrl Pts',(-0.681708219121542,3.73629716031106,
5.54091276408699));
#259949=CARTESIAN_POINT('Ctrl Pts',(-3.50374612092884,1.46574407224603,
5.73868526408701));
#259950=CARTESIAN_POINT('Ctrl Pts',(-3.13910340550632,-2.13791308867103,
5.93645776408699));
#259951=CARTESIAN_POINT('Ctrl Pts',(0.080574929607317,-3.79712394401137,
6.134230264087));
#259952=CARTESIAN_POINT('Ctrl Pts',(3.2269698253648,-2.00282508260319,6.332002764087));
#259953=CARTESIAN_POINT('Ctrl Pts',(3.43841400270688,1.61305663611419,6.52977526408701));
#259954=CARTESIAN_POINT('Ctrl Pts',(0.522597562951646,3.76185251605611,
6.727547764087));
#259955=CARTESIAN_POINT('Ctrl Pts',(-2.86852486844103,2.4892182797966,6.925320264087));
#259956=CARTESIAN_POINT('Ctrl Pts',(-3.65070467594106,-1.04737669174119,
7.12309276408701));
#259957=CARTESIAN_POINT('Ctrl Pts',(-1.11254407395429,-3.63137553123531,
7.320865264087));
#259958=CARTESIAN_POINT('Ctrl Pts',(2.43748283166181,-2.91261394810503,
7.51863776408702));
#259959=CARTESIAN_POINT('Ctrl Pts',(3.77060273936735,0.4551895728353,7.71641026408699));
#259960=CARTESIAN_POINT('Ctrl Pts',(1.67433414403899,3.40899512165219,7.91418276408701));
#259961=CARTESIAN_POINT('Ctrl Pts',(-1.94475259488627,3.26229672317309,
8.11195526408701));
#259962=CARTESIAN_POINT('Ctrl Pts',(-3.79507379388419,0.14851755558278,
8.309727764087));
#259963=CARTESIAN_POINT('Ctrl Pts',(-2.19374990149398,-3.10033932578968,
8.507500264087));
#259964=CARTESIAN_POINT('Ctrl Pts',(1.40280425267068,-3.52941677817056,
8.70527276408699));
#259965=CARTESIAN_POINT('Ctrl Pts',(3.7234985221838,-0.748465978276811,
8.90304526408702));
#259966=CARTESIAN_POINT('Ctrl Pts',(2.65764589039604,2.71321965321718,9.10081776408701));
#259967=CARTESIAN_POINT('Ctrl Pts',(-0.825353519147718,3.7072137966097,
9.29859026408701));
#259968=CARTESIAN_POINT('Ctrl Pts',(-3.55768836253281,1.32947210592829,
9.49636276408701));
#259969=CARTESIAN_POINT('Ctrl Pts',(-3.05428175788224,-2.25743338967303,
9.69413526408699));
#259970=CARTESIAN_POINT('Ctrl Pts',(0.227014608569453,-3.79118806350185,
9.89190776408703));
#259971=CARTESIAN_POINT('Ctrl Pts',(3.30183966460686,-1.87683174380968,
10.089680264087));
#259972=CARTESIAN_POINT('Ctrl Pts',(3.3736193808522,1.74451564581155,10.287452764087));
#259973=CARTESIAN_POINT('Ctrl Pts',(0.377069623532174,3.77921434485424,
10.485225264087));
#259974=CARTESIAN_POINT('Ctrl Pts',(-2.96242748761104,2.37669222786403,
10.682997764087));
#259975=CARTESIAN_POINT('Ctrl Pts',(-3.60757691237093,-1.18744742480291,
10.880770264087));
#259976=CARTESIAN_POINT('Ctrl Pts',(-0.97161091812183,-3.67159567342719,
11.078542764087));
#259977=CARTESIAN_POINT('Ctrl Pts',(2.54804172846031,-2.81640301011199,
11.276315264087));
#259978=CARTESIAN_POINT('Ctrl Pts',(3.75023331832587,0.60032709705734,11.474087764087));
#259979=CARTESIAN_POINT('Ctrl Pts',(1.54156253033206,3.47105567953309,11.671860264087));
#259980=CARTESIAN_POINT('Ctrl Pts',(-2.06916972731314,3.18483582071574,
11.869632764087));
#259981=CARTESIAN_POINT('Ctrl Pts',(-3.79797822789224,0.00198640355712319,
12.067405264087));
#259982=CARTESIAN_POINT('Ctrl Pts',(-2.07250003485589,-3.18266966097084,
12.265177764087));
#259983=CARTESIAN_POINT('Ctrl Pts',(1.53793085231274,-3.47266630398747,
12.462950264087));
#259984=CARTESIAN_POINT('Ctrl Pts',(3.74960330536725,-0.60424963195659,
12.660722764087));
#259985=CARTESIAN_POINT('Ctrl Pts',(2.55098638157809,2.81373613658802,12.858495264087));
#259986=CARTESIAN_POINT('Ctrl Pts',(-0.967769780706639,3.67261000065507,
13.056267764087));
#259987=CARTESIAN_POINT('Ctrl Pts',(-3.60633283092,1.19122041535194,13.254040264087));
#259988=CARTESIAN_POINT('Ctrl Pts',(-2.96491196256021,-2.37359213421067,
13.451812764087));
#259989=CARTESIAN_POINT('Ctrl Pts',(0.373116238836454,-3.77960670411384,
13.649585264087));
#259990=CARTESIAN_POINT('Ctrl Pts',(3.37179271631145,-1.74804360454804,
13.847357764087));
#259991=CARTESIAN_POINT('Ctrl Pts',(3.30380108391712,1.87337688764339,14.045130264087));
#259992=CARTESIAN_POINT('Ctrl Pts',(0.230980187636045,3.790948524985,14.242902764087));
#259993=CARTESIAN_POINT('Ctrl Pts',(-3.05191873971586,2.26062703030387,
14.440675264087));
#259994=CARTESIAN_POINT('Ctrl Pts',(-3.55907708639098,-1.32574992299329,
14.638447764087));
#259995=CARTESIAN_POINT('Ctrl Pts',(-0.829230930900554,-3.70634842317082,
14.836220264087));
#259996=CARTESIAN_POINT('Ctrl Pts',(2.65480632188787,-2.71599814947841,
15.033992764087));
#259997=CARTESIAN_POINT('Ctrl Pts',(3.72427940522297,0.74457066805276,15.231765264087));
#259998=CARTESIAN_POINT('Ctrl Pts',(1.40649536566728,3.52794747486548,15.429537764087));
#259999=CARTESIAN_POINT('Ctrl Pts',(-2.19050564441242,3.10263235130414,
15.627310264087));
#260000=CARTESIAN_POINT('Ctrl Pts',(-3.79522707814296,-0.144547686337884,
15.825082764087));
#260001=CARTESIAN_POINT('Ctrl Pts',(-1.94816398475754,-3.26026070382418,
16.022855264087));
#260002=CARTESIAN_POINT('Ctrl Pts',(1.67076728712268,-3.41074458964229,
16.220627764087));
#260003=CARTESIAN_POINT('Ctrl Pts',(3.77012457889698,-0.459133635480682,
16.418400264087));
#260004=CARTESIAN_POINT('Ctrl Pts',(2.44052809844237,2.91006294072064,16.616172764087));
#260005=CARTESIAN_POINT('Ctrl Pts',(-1.10874476522764,3.63253678253595,
16.813945264087));
#260006=CARTESIAN_POINT('Ctrl Pts',(-3.6496074068792,1.05119586522387,17.011717764087));
#260007=CARTESIAN_POINT('Ctrl Pts',(-2.87112649227236,-2.48621825256981,
17.209490264087));
#260008=CARTESIAN_POINT('Ctrl Pts',(0.51866109429388,-3.76239346632174,
17.407262764087));
#260009=CARTESIAN_POINT('Ctrl Pts',(3.43672704554254,-1.61665942745799,
17.605035264087));
#260010=CARTESIAN_POINT('Ctrl Pts',(3.22905880179933,1.99946185205994,17.802807764087));
#260011=CARTESIAN_POINT('Ctrl Pts',(0.0845549911956499,3.79701195372378,
18.000580264087));
#260012=CARTESIAN_POINT('Ctrl Pts',(-3.13688105899666,2.14124461898399,
18.198352764087));
#260013=CARTESIAN_POINT('Ctrl Pts',(-3.50524734990374,-1.4621722988924,
18.396125264087));
#260014=CARTESIAN_POINT('Ctrl Pts',(-0.685673736219726,-3.73540183242111,
18.593897764087));
#260015=CARTESIAN_POINT('Ctrl Pts',(2.75772798819186,-2.61189414113004,
18.791670264087));
#260016=CARTESIAN_POINT('Ctrl Pts',(3.69256818542617,0.88836740372384,18.989442764087));
#260017=CARTESIAN_POINT('Ctrl Pts',(1.26973928222288,3.57831333506942,19.187215264087));
#260018=CARTESIAN_POINT('Ctrl Pts',(-2.3093601167586,3.01828636138478,19.384987764087));
#260019=CARTESIAN_POINT('Ctrl Pts',(-3.78562084885311,-0.296703047143297,
19.582803803098));
#260020=CARTESIAN_POINT('Ctrl Pts',(-2.47707340993165,-2.31342452450426,
19.7146956754422));
#260021=CARTESIAN_POINT('Ctrl Pts',(-1.54055558982206,-2.82421483925514,
19.7806633811199));
#260022=CARTESIAN_POINT('Ctrl Pts',(1.75279930320746,3.52789804876769,2.86229373536173E-16));
#260023=CARTESIAN_POINT('Ctrl Pts',(1.83447079285969,3.47853779768125,-2.03614959547088E-15));
#260024=CARTESIAN_POINT('Ctrl Pts',(1.9140947383689,3.42607984753856,-1.70822902311683E-16));
#260025=CARTESIAN_POINT('Ctrl Pts',(1.99146917849576,3.3705151092053,8.74300631892311E-16));
#260026=CARTESIAN_POINT('Ctrl Pts',(2.09010694656004,3.29968058344612,2.05149679631144E-15));
#260027=CARTESIAN_POINT('Ctrl Pts',(2.18509043883734,3.22379765720304,-9.10996029650036E-16));
#260028=CARTESIAN_POINT('Ctrl Pts',(2.27623490042508,3.1432744471131,8.11850586757146E-16));
#260029=CARTESIAN_POINT('Ctrl Pts',(2.35348132939542,3.07502970332593,2.2719914056588E-15));
#260030=CARTESIAN_POINT('Ctrl Pts',(2.4279697040414,3.00345097986864,1.81605216791664E-15));
#260031=CARTESIAN_POINT('Ctrl Pts',(2.49956303211591,2.92877198870791,2.2065682614425E-15));
#260032=CARTESIAN_POINT('Ctrl Pts',(2.5242255442793,2.90304652549249,2.34109347720781E-15));
#260033=CARTESIAN_POINT('Ctrl Pts',(2.54854878077249,2.87694774894346,2.37550202059879E-15));
#260034=CARTESIAN_POINT('Ctrl Pts',(2.57249452004371,2.85052138616924,2.06779038336435E-15));
#260035=CARTESIAN_POINT('Ctrl Pts',(2.65366236625338,2.7609450767789,1.02475343365563E-15));
#260036=CARTESIAN_POINT('Ctrl Pts',(2.73057055546618,2.66753281357049,2.79320129631381E-15));
#260037=CARTESIAN_POINT('Ctrl Pts',(2.8030366800126,2.57068789639114,3.66373598126302E-15));
#260038=CARTESIAN_POINT('Ctrl Pts',(2.87558533260316,2.47373268738027,4.53526207461651E-15));
#260039=CARTESIAN_POINT('Ctrl Pts',(2.94368213761813,2.37333611107257,6.88960740750642E-16));
#260040=CARTESIAN_POINT('Ctrl Pts',(3.007096443202,2.26988275097777,4.34374758384592E-15));
#260041=CARTESIAN_POINT('Ctrl Pts',(3.02439282495162,2.24166563509191,5.34059818198255E-15));
#260042=CARTESIAN_POINT('Ctrl Pts',(3.04134056895315,2.21322104129718,6.55777160202515E-15));
#260043=CARTESIAN_POINT('Ctrl Pts',(3.05793432949856,2.18455664797758,5.21804821573824E-15));
#260044=CARTESIAN_POINT('Ctrl Pts',(3.0719333338598,2.16037448830406,3.74557415333203E-15));
#260045=CARTESIAN_POINT('Ctrl Pts',(3.08568039890931,2.13603589347975,7.06947186048359E-15));
#260046=CARTESIAN_POINT('Ctrl Pts',(3.09917214976624,2.11154546334535,6.63358257213531E-15));
#260047=CARTESIAN_POINT('Ctrl Pts',(3.10952920728848,2.09274517594482,6.49618977517167E-15));
#260048=CARTESIAN_POINT('Ctrl Pts',(3.11973673264636,2.07385347610629,4.30040482780213E-15));
#260049=CARTESIAN_POINT('Ctrl Pts',(3.12978288789371,2.05489234507567,4.13558076672871E-15));
#260050=CARTESIAN_POINT('Ctrl Pts',(3.18543717352967,1.94985034877193,4.71724120995002E-15));
#260051=CARTESIAN_POINT('Ctrl Pts',(3.23621623074516,1.84254873547601,4.73048287775305E-15));
#260052=CARTESIAN_POINT('Ctrl Pts',(3.28194760804037,1.7333657774407,4.74620343027254E-15));
#260053=CARTESIAN_POINT('Ctrl Pts',(3.32735401483942,1.62495868145335,4.71586595529493E-15));
#260054=CARTESIAN_POINT('Ctrl Pts',(3.36778445351152,1.51469601660824,5.7165044333348E-15));
#260055=CARTESIAN_POINT('Ctrl Pts',(3.40302049110049,1.40293613231933,6.38378239159465E-15));
#260056=CARTESIAN_POINT('Ctrl Pts',(3.43721763530565,1.29447135759175,7.65246346190412E-15));
#260057=CARTESIAN_POINT('Ctrl Pts',(3.46652217571582,1.18459561281048,5.23326451904315E-15));
#260058=CARTESIAN_POINT('Ctrl Pts',(3.4906860815092,1.07363693774357,5.10702591327572E-15));
#260059=CARTESIAN_POINT('Ctrl Pts',(3.50717437800193,0.997924031535933,
5.33424237539366E-15));
#260060=CARTESIAN_POINT('Ctrl Pts',(3.52126818188651,0.921706923658275,
5.80367298533689E-15));
#260061=CARTESIAN_POINT('Ctrl Pts',(3.53287506570147,0.845092524005051,
7.07767178198537E-15));
#260062=CARTESIAN_POINT('Ctrl Pts',(3.53714290814536,0.816921466909462,
7.04204661411027E-15));
#260063=CARTESIAN_POINT('Ctrl Pts',(3.54107426600386,0.788697812530836,
5.43860166991208E-15));
#260064=CARTESIAN_POINT('Ctrl Pts',(3.54466460187288,0.76042337864298,4.44089209850063E-15));
#260065=CARTESIAN_POINT('Ctrl Pts',(3.54781671197229,0.735600038469682,
3.56496000438575E-15));
#260066=CARTESIAN_POINT('Ctrl Pts',(3.55070529414814,0.710740908665674,
3.35794494782224E-15));
#260067=CARTESIAN_POINT('Ctrl Pts',(3.55332435291955,0.685880474621733,
3.91353616180368E-15));
#260068=CARTESIAN_POINT('Ctrl Pts',(3.56503933400909,0.57468040615398,6.39868106818853E-15));
#260069=CARTESIAN_POINT('Ctrl Pts',(3.57138461782529,0.463318188425493,
1.67998447934304E-15));
#260070=CARTESIAN_POINT('Ctrl Pts',(3.57216496053255,0.352111263492755,
1.99840144432528E-15));
#260071=CARTESIAN_POINT('Ctrl Pts',(3.57263270387297,0.285452988786406,
2.18926298946545E-15));
#260072=CARTESIAN_POINT('Ctrl Pts',(3.57110006250948,0.218850497592311,
5.55435765969798E-15));
#260073=CARTESIAN_POINT('Ctrl Pts',(3.56751601518668,0.152373241746208,
5.10702591327572E-15));
#260074=CARTESIAN_POINT('Ctrl Pts',(3.56141928221821,0.0392904499003424,
4.04931262847179E-15));
#260075=CARTESIAN_POINT('Ctrl Pts',(3.54938889023284,-0.0734312531627452,
3.16088255514917E-15));
#260076=CARTESIAN_POINT('Ctrl Pts',(3.53163824840077,-0.185433964967349,
1.60982338570648E-15));
#260077=CARTESIAN_POINT('Ctrl Pts',(3.51910644172461,-0.264506955387629,
5.14788409583811E-16));
#260078=CARTESIAN_POINT('Ctrl Pts',(3.50372242082101,-0.343221283764593,
9.58919127278865E-16));
#260079=CARTESIAN_POINT('Ctrl Pts',(3.4855479178701,-0.421443262011223,
6.66133814775094E-16));
#260080=CARTESIAN_POINT('Ctrl Pts',(3.47646066639465,-0.460554251134538,
5.19741158523209E-16));
#260081=CARTESIAN_POINT('Ctrl Pts',(3.46667563378722,-0.499542035897557,
2.2271828927908E-15));
#260082=CARTESIAN_POINT('Ctrl Pts',(3.45619963468214,-0.538389119328871,
1.49880108324396E-15));
#260083=CARTESIAN_POINT('Ctrl Pts',(3.44942611035294,-0.563506691610151,
1.02784725264275E-15));
#260084=CARTESIAN_POINT('Ctrl Pts',(3.44236353288121,-0.588566040585249,
-1.81790838627316E-15));
#260085=CARTESIAN_POINT('Ctrl Pts',(3.43501403463685,-0.613560869415645,
-1.88737914186277E-15));
#260086=CARTESIAN_POINT('Ctrl Pts',(3.43099672687466,-0.627223287792596,
-1.92535253765069E-15));
#260087=CARTESIAN_POINT('Ctrl Pts',(3.42689421896722,-0.640864516596422,
-1.22266932942972E-15));
#260088=CARTESIAN_POINT('Ctrl Pts',(3.42270950093411,-0.654475540993858,
-1.22124532708767E-15));
#260089=CARTESIAN_POINT('Ctrl Pts',(3.38999385410531,-0.760884972559132,
-1.58862401117716E-15));
#260090=CARTESIAN_POINT('Ctrl Pts',(3.35221828589833,-0.865585500186228,
3.4290659176697E-16));
#260091=CARTESIAN_POINT('Ctrl Pts',(3.30961957687026,-0.968251586859118,
-9.99200722162641E-16));
#260092=CARTESIAN_POINT('Ctrl Pts',(3.266944521034,-1.07110167507115,-2.34371340498723E-15));
#260093=CARTESIAN_POINT('Ctrl Pts',(3.21942843768939,-1.17191077813822,
-6.00747044203194E-15));
#260094=CARTESIAN_POINT('Ctrl Pts',(3.16726458926213,-1.27032445089415,
-4.38538094726937E-15));
#260095=CARTESIAN_POINT('Ctrl Pts',(3.11601107760244,-1.36702065863472,
-2.79159932763245E-15));
#260096=CARTESIAN_POINT('Ctrl Pts',(3.06026996439313,-1.46140489503514,
-2.78742529000394E-15));
#260097=CARTESIAN_POINT('Ctrl Pts',(3.00019063179608,-1.55310502918845,
-1.72084568816899E-15));
#260098=CARTESIAN_POINT('Ctrl Pts',(2.94705920041998,-1.63420046041805,
-7.77611160214002E-16));
#260099=CARTESIAN_POINT('Ctrl Pts',(2.89053421382684,-1.71319648990997,
-5.06270758738262E-15));
#260100=CARTESIAN_POINT('Ctrl Pts',(2.830702015742,-1.78980623133405,-2.38697950294409E-15));
#260101=CARTESIAN_POINT('Ctrl Pts',(2.82029713655003,-1.80312874212189,
-1.13314336364148E-15));
#260102=CARTESIAN_POINT('Ctrl Pts',(2.80979659776632,-1.81637333173455,
-3.50715845124803E-15));
#260103=CARTESIAN_POINT('Ctrl Pts',(2.79920599239979,-1.82953264244366,
-3.27515792264421E-15));
#260104=CARTESIAN_POINT('Ctrl Pts',(2.73180388711991,-1.9132828356696,-2.89142751403143E-15));
#260105=CARTESIAN_POINT('Ctrl Pts',(2.66069563561445,-1.9936599364221,-1.01197196229115E-15));
#260106=CARTESIAN_POINT('Ctrl Pts',(2.58605721113782,-2.07034386466854,
-1.83186799063151E-15));
#260107=CARTESIAN_POINT('Ctrl Pts',(2.51246520689647,-2.14595269500396,
-2.15041636385202E-15));
#260108=CARTESIAN_POINT('Ctrl Pts',(2.43544073059348,-2.21797169194816,
-2.64088159904353E-15));
#260109=CARTESIAN_POINT('Ctrl Pts',(2.3551241205076,-2.28605318007106,-3.77475828372553E-15));
#260110=CARTESIAN_POINT('Ctrl Pts',(2.27727340703588,-2.3520444167395,-4.19887348472418E-15));
#260111=CARTESIAN_POINT('Ctrl Pts',(2.19632906523751,-2.41433649943972,
-1.81897112986788E-15));
#260112=CARTESIAN_POINT('Ctrl Pts',(2.11240041152739,-2.47256856817298,
-3.60822483003176E-15));
#260113=CARTESIAN_POINT('Ctrl Pts',(2.03466386030107,-2.52650438143806,
-3.18302953207866E-15));
#260114=CARTESIAN_POINT('Ctrl Pts',(1.95436666507115,-2.57695701945168,
-1.65126864917111E-15));
#260115=CARTESIAN_POINT('Ctrl Pts',(1.87158653173908,-2.62360084935054,
-8.32667268468867E-16));
#260116=CARTESIAN_POINT('Ctrl Pts',(-1.43037430634624,2.88158472091696,
-0.413345808225853));
#260117=CARTESIAN_POINT('Ctrl Pts',(-2.38593513615963,2.4072590315855,-0.347374197020977));
#260118=CARTESIAN_POINT('Ctrl Pts',(-3.77197008027487,0.441785045807912,
-0.215430974611227));
#260119=CARTESIAN_POINT('Ctrl Pts',(-2.42248806046208,-2.92946651123822,
-0.0175161409965988));
#260120=CARTESIAN_POINT('Ctrl Pts',(1.13632421357434,-3.62384868015713,
0.180398692618027));
#260121=CARTESIAN_POINT('Ctrl Pts',(3.65866024061303,-1.02244510071097,
0.378313526232654));
#260122=CARTESIAN_POINT('Ctrl Pts',(2.84987228722314,2.5124186827546,0.576228359847282));
#260123=CARTESIAN_POINT('Ctrl Pts',(-0.554751695607484,3.75800204913211,
0.774143193461907));
#260124=CARTESIAN_POINT('Ctrl Pts',(-3.4539307032892,1.58177692684051,0.972058027076536));
#260125=CARTESIAN_POINT('Ctrl Pts',(-3.20771217175408,-2.03531056509857,
1.16997286069116));
#260126=CARTESIAN_POINT('Ctrl Pts',(-0.0401470203663782,-3.79865643127254,
1.36788769430579));
#260127=CARTESIAN_POINT('Ctrl Pts',(3.163947729481,-2.10263059238148,1.56580252792041));
#260128=CARTESIAN_POINT('Ctrl Pts',(3.48663178432909,1.50832114879186,1.76371736153505));
#260129=CARTESIAN_POINT('Ctrl Pts',(0.634008830268578,3.74561072927655,
1.96163219514967));
#260130=CARTESIAN_POINT('Ctrl Pts',(-2.79600544339863,2.57176105983533,
2.1595470287643));
#260131=CARTESIAN_POINT('Ctrl Pts',(-3.67968187030208,-0.944214684454183,
2.35746186237892));
#260132=CARTESIAN_POINT('Ctrl Pts',(-1.21224693115205,-3.60028454405826,
2.55537669599355));
#260133=CARTESIAN_POINT('Ctrl Pts',(2.35918847985848,-2.97755376163462,
2.75329152960818));
#260134=CARTESIAN_POINT('Ctrl Pts',(3.78209600952429,0.356855453303921,
2.9512063632228));
#260135=CARTESIAN_POINT('Ctrl Pts',(1.76062403462141,3.36627360473104,3.14912119683744));
#260136=CARTESIAN_POINT('Ctrl Pts',(-1.86425955536149,3.31000484381239,
3.34703603045206));
#260137=CARTESIAN_POINT('Ctrl Pts',(-3.7913499457688,0.239293105077073,
3.54495086406669));
#260138=CARTESIAN_POINT('Ctrl Pts',(-2.26563336564454,-3.04934434403637,
3.74286569768131));
#260139=CARTESIAN_POINT('Ctrl Pts',(1.32341017753202,-3.560924190624,3.94078053129594));
#260140=CARTESIAN_POINT('Ctrl Pts',(3.70721550972523,-0.829547300363254,
4.13869536491057));
#260141=CARTESIAN_POINT('Ctrl Pts',(2.71483566892025,2.65730367782625,4.33661019852519));
#260142=CARTESIAN_POINT('Ctrl Pts',(-0.749962592571982,3.7241309954383,
4.53452503213983));
#260143=CARTESIAN_POINT('Ctrl Pts',(-3.53176506589602,1.39936809859862,
4.73243986575444));
#260144=CARTESIAN_POINT('Ctrl Pts',(-3.09716622458576,-2.19980838530159,
4.93035469936908));
#260145=CARTESIAN_POINT('Ctrl Pts',(0.158041951713996,-3.79560512941772,
5.1282695329837));
#260146=CARTESIAN_POINT('Ctrl Pts',(3.26932029938714,-1.93471970478396,
5.32618436659833));
#260147=CARTESIAN_POINT('Ctrl Pts',(3.40320748108887,1.68812748234117,5.52409920021295));
#260148=CARTESIAN_POINT('Ctrl Pts',(0.43777157361897,3.77358604057225,5.72201403382758));
#260149=CARTESIAN_POINT('Ctrl Pts',(-2.92634574058982,2.42241535717116,
5.9199288674422));
#260150=CARTESIAN_POINT('Ctrl Pts',(-3.62542104038862,-1.13486467741114,
6.11784370105684));
#260151=CARTESIAN_POINT('Ctrl Pts',(-1.02280192366893,-3.65861610190322,
6.31575853467146));
#260152=CARTESIAN_POINT('Ctrl Pts',(2.51128952770567,-2.85044215240023,
6.5136733682861));
#260153=CARTESIAN_POINT('Ctrl Pts',(3.75833334529226,0.553647922249075,
6.71158820190071));
#260154=CARTESIAN_POINT('Ctrl Pts',(1.58263864965663,3.45352724917065,6.90950303551535));
#260155=CARTESIAN_POINT('Ctrl Pts',(-2.03437531199935,3.20825694826264,
7.10741786912997));
#260156=CARTESIAN_POINT('Ctrl Pts',(-3.79867050418984,0.0412062707186327,
7.30533270274459));
#260157=CARTESIAN_POINT('Ctrl Pts',(-2.10349187136144,-3.16337122438474,
7.50324753635922));
#260158=CARTESIAN_POINT('Ctrl Pts',(1.50735042908147,-3.48704606222752,
7.70116236997385));
#260159=CARTESIAN_POINT('Ctrl Pts',(3.74543893348258,-0.635045472152602,
7.89907720358848));
#260160=CARTESIAN_POINT('Ctrl Pts',(2.57253194898869,2.79529514140836,8.0969920372031));
#260161=CARTESIAN_POINT('Ctrl Pts',(-0.943196538906329,3.67994236981285,
8.29490687081774));
#260162=CARTESIAN_POINT('Ctrl Pts',(-3.59994983150709,1.21324225395456,
8.49282170443235));
#260163=CARTESIAN_POINT('Ctrl Pts',(-2.97820550244154,-2.35836543847123,
8.69073653804698));
#260164=CARTESIAN_POINT('Ctrl Pts',(0.355809861940216,-3.78219445537836,
8.8886513716616));
#260165=CARTESIAN_POINT('Ctrl Pts',(3.36578688114091,-1.7615544916035,9.08656620527623));
#260166=CARTESIAN_POINT('Ctrl Pts',(3.31051999380733,1.86334455395415,9.28448103889086));
#260167=CARTESIAN_POINT('Ctrl Pts',(0.240341112094004,3.79128364884325,
9.48239587250549));
#260168=CARTESIAN_POINT('Ctrl Pts',(-3.04871797664126,2.26647617570826,
9.68031070612012));
#260169=CARTESIAN_POINT('Ctrl Pts',(-3.56128986322979,-1.32242582635301,
9.87822553973474));
#260170=CARTESIAN_POINT('Ctrl Pts',(-0.83057201159013,-3.70698606548661,
10.0761403733494));
#260171=CARTESIAN_POINT('Ctrl Pts',(2.65655314905942,-2.71557009159609,
10.274055206964));
#260172=CARTESIAN_POINT('Ctrl Pts',(3.72433815535594,0.748933148357456,
10.4719700405786));
#260173=CARTESIAN_POINT('Ctrl Pts',(1.40034428802749,3.53137812066868,10.6698848741933));
#260174=CARTESIAN_POINT('Ctrl Pts',(-2.19895218980709,3.0977741723843,10.8677997078079));
#260175=CARTESIAN_POINT('Ctrl Pts',(-3.79564866990161,-0.156992773154816,
11.0657145414225));
#260176=CARTESIAN_POINT('Ctrl Pts',(-1.93562332903015,-3.26878538363457,
11.2636293750371));
#260177=CARTESIAN_POINT('Ctrl Pts',(1.68718671098545,-3.40367397945556,
11.4615442086518));
#260178=CARTESIAN_POINT('Ctrl Pts',(3.7734648885675,-0.43881464298359,11.6594590422664));
#260179=CARTESIAN_POINT('Ctrl Pts',(2.42322415848731,2.92567603023173,11.857373875881));
#260180=CARTESIAN_POINT('Ctrl Pts',(-1.13386250339844,3.62573459860695,
12.0552887094957));
#260181=CARTESIAN_POINT('Ctrl Pts',(-3.65833324154142,1.02381319095868,
12.2532035431103));
#260182=CARTESIAN_POINT('Ctrl Pts',(-2.85113620846061,-2.51050151901093,
12.4511183767249));
#260183=CARTESIAN_POINT('Ctrl Pts',(0.552609031119811,-3.758486239814,12.6490332103395));
#260184=CARTESIAN_POINT('Ctrl Pts',(3.45308964784694,-1.58359320536449,
12.8469480439542));
#260185=CARTESIAN_POINT('Ctrl Pts',(3.20881916310805,2.03348841517158,13.0448628775688));
#260186=CARTESIAN_POINT('Ctrl Pts',(0.0422562890258594,3.79865896892123,
13.2427777111834));
#260187=CARTESIAN_POINT('Ctrl Pts',(-3.1627896610741,2.10436620290518,13.440692544798));
#260188=CARTESIAN_POINT('Ctrl Pts',(-3.48746258741064,-1.5063864901418,
13.6386073784127));
#260189=CARTESIAN_POINT('Ctrl Pts',(-0.636080753601478,-3.74526325254614,
13.8365222120273));
#260190=CARTESIAN_POINT('Ctrl Pts',(2.79458394112346,-2.57330451988858,
14.0344370456419));
#260191=CARTESIAN_POINT('Ctrl Pts',(3.68020294556761,0.94217930161899,14.2323518792566));
#260192=CARTESIAN_POINT('Ctrl Pts',(1.21423729739401,3.59961433217161,14.4302667128712));
#260193=CARTESIAN_POINT('Ctrl Pts',(-2.35754211922225,2.97885728294461,
14.6281815464858));
#260194=CARTESIAN_POINT('Ctrl Pts',(-3.78229266369463,-0.354764383222645,
14.8260963801005));
#260195=CARTESIAN_POINT('Ctrl Pts',(-1.76248478622916,-3.36529982672292,
15.024011213715));
#260196=CARTESIAN_POINT('Ctrl Pts',(1.86242939393929,-3.31103493060374,
15.2219260473297));
#260197=CARTESIAN_POINT('Ctrl Pts',(3.79121707405805,-0.241389077501906,
15.4198408809443));
#260198=CARTESIAN_POINT('Ctrl Pts',(2.26731880001602,3.04809135937923,15.6177557145589));
#260199=CARTESIAN_POINT('Ctrl Pts',(-1.32144135527743,3.56165528174486,
15.8156705481736));
#260200=CARTESIAN_POINT('Ctrl Pts',(-3.70675637139401,0.831596632357296,
16.0135853817882));
#260201=CARTESIAN_POINT('Ctrl Pts',(-2.71630424424639,-2.65580236950805,
16.2115002154028));
#260202=CARTESIAN_POINT('Ctrl Pts',(0.747903527837983,-3.72454512026097,
16.4094150490174));
#260203=CARTESIAN_POINT('Ctrl Pts',(3.53099113340195,-1.40132019993944,
16.6073298826321));
#260204=CARTESIAN_POINT('Ctrl Pts',(3.09838144724328,2.19809550012073,16.8052447162467));
#260205=CARTESIAN_POINT('Ctrl Pts',(-0.155942746811587,3.79569254506809,
17.0031595498613));
#260206=CARTESIAN_POINT('Ctrl Pts',(-3.26825181952199,1.93652560855552,
17.201074383476));
#260207=CARTESIAN_POINT('Ctrl Pts',(-3.40413714935415,-1.68624351756118,
17.3989892170906));
#260208=CARTESIAN_POINT('Ctrl Pts',(-0.439863558166481,-3.77334784211365,
17.5969040507052));
#260209=CARTESIAN_POINT('Ctrl Pts',(2.92501736172631,-2.42402435559258,
17.7948188843198));
#260210=CARTESIAN_POINT('Ctrl Pts',(3.62602629419879,1.1328441110195,17.9927337179345));
#260211=CARTESIAN_POINT('Ctrl Pts',(1.02486574019099,3.65808101165132,18.1906485515491));
#260212=CARTESIAN_POINT('Ctrl Pts',(-2.50979256920917,2.85177081985058,
18.3885633851637));
#260213=CARTESIAN_POINT('Ctrl Pts',(-3.75848698963855,-0.551456610966241,
18.5864782187783));
#260214=CARTESIAN_POINT('Ctrl Pts',(-1.58483866315692,-3.45286925653142,
18.784393052393));
#260215=CARTESIAN_POINT('Ctrl Pts',(2.03315943800767,-3.20896423162532,
18.9823078860076));
#260216=CARTESIAN_POINT('Ctrl Pts',(3.79757377187795,-0.0441069402319698,
19.1802227196223));
#260217=CARTESIAN_POINT('Ctrl Pts',(2.10733370637857,3.16375838102537,19.3781375532368));
#260218=CARTESIAN_POINT('Ctrl Pts',(-1.51055995362578,3.48482947278868,
19.5760959260673));
#260219=CARTESIAN_POINT('Ctrl Pts',(-2.99356127193463,1.58998577181604,
19.7080826876928));
#260220=CARTESIAN_POINT('Ctrl Pts',(-3.17185176654334,0.537454353407991,
19.7740978381135));
#260221=CARTESIAN_POINT('Ctrl Pts',(-1.53694980720768,3.09628819646456,
-0.274955153680968));
#260222=CARTESIAN_POINT('Ctrl Pts',(-2.56370834631237,2.5866210600114,-0.208983542476093));
#260223=CARTESIAN_POINT('Ctrl Pts',(-4.05301511775646,0.474701927998286,
-0.0770403200663413));
#260224=CARTESIAN_POINT('Ctrl Pts',(-2.60298478585014,-3.14773760245323,
0.120874513548287));
#260225=CARTESIAN_POINT('Ctrl Pts',(1.2209903891798,-3.89385736698855,0.318789347162913));
#260226=CARTESIAN_POINT('Ctrl Pts',(3.93126269571537,-1.09862627806308,
0.51670418077754));
#260227=CARTESIAN_POINT('Ctrl Pts',(3.06221290677602,2.69961603263725,0.714619014392168));
#260228=CARTESIAN_POINT('Ctrl Pts',(-0.59608558950558,4.03800634510397,
0.912533848006791));
#260229=CARTESIAN_POINT('Ctrl Pts',(-3.71127900226987,1.69963325820862,
1.11044868162142));
#260230=CARTESIAN_POINT('Ctrl Pts',(-3.44671501863647,-2.18695915241001,
1.30836351523604));
#260231=CARTESIAN_POINT('Ctrl Pts',(-0.0431383274562087,-4.08168983726099,
1.50627834885068));
#260232=CARTESIAN_POINT('Ctrl Pts',(3.39968973943801,-2.25929511544758,
1.7041931824653));
#260233=CARTESIAN_POINT('Ctrl Pts',(3.74641660225106,1.62070437685965,1.90210801607993));
#260234=CARTESIAN_POINT('Ctrl Pts',(0.681248079699113,4.02469176263519,
2.10002284969455));
#260235=CARTESIAN_POINT('Ctrl Pts',(-3.00433250801347,2.76337994017454,
2.29793768330918));
#260236=CARTESIAN_POINT('Ctrl Pts',(-3.95385062221435,-1.01456700585002,
2.49585251692381));
#260237=CARTESIAN_POINT('Ctrl Pts',(-1.3025700188097,-3.86853749492883,
2.69376735053843));
#260238=CARTESIAN_POINT('Ctrl Pts',(2.53496882822741,-3.19940777710475,
2.89168218415307));
#260239=CARTESIAN_POINT('Ctrl Pts',(4.06389551803955,0.383444331824902,
3.08959701776769));
#260240=CARTESIAN_POINT('Ctrl Pts',(1.89180605284284,3.61709067678639,3.28751185138232));
#260241=CARTESIAN_POINT('Ctrl Pts',(-2.00316333388078,3.55662939692278,
3.48542668499694));
#260242=CARTESIAN_POINT('Ctrl Pts',(-4.07383895414842,0.257122551826211,
3.68334151861157));
#260243=CARTESIAN_POINT('Ctrl Pts',(-2.43444303290489,-3.27654739104502,
3.88125635222619));
#260244=CARTESIAN_POINT('Ctrl Pts',(1.42201590743771,-3.82624444802916,
4.07917118584083));
#260245=CARTESIAN_POINT('Ctrl Pts',(3.98343576060461,-0.89135589034721,
4.27708601945545));
#260246=CARTESIAN_POINT('Ctrl Pts',(2.91711486946803,2.85529623764002,4.47500085307008));
#260247=CARTESIAN_POINT('Ctrl Pts',(-0.805841419936308,4.00161159918771,
4.6729156866847));
#260248=CARTESIAN_POINT('Ctrl Pts',(-3.79491271134303,1.50363336352689,
4.87083052029933));
#260249=CARTESIAN_POINT('Ctrl Pts',(-3.32793242345554,-2.36371351098971,
5.06874535391395));
#260250=CARTESIAN_POINT('Ctrl Pts',(0.169817470951354,-4.07841118650735,
5.26666018752859));
#260251=CARTESIAN_POINT('Ctrl Pts',(3.51291349512468,-2.07887338585129,
5.4645750211432));
#260252=CARTESIAN_POINT('Ctrl Pts',(3.65677645266742,1.8139078680418,5.66248985475784));
#260253=CARTESIAN_POINT('Ctrl Pts',(0.470389416734859,4.0547514813478,5.86040468837246));
#260254=CARTESIAN_POINT('Ctrl Pts',(-3.1443843068682,2.60290666552285,6.05831952198709));
#260255=CARTESIAN_POINT('Ctrl Pts',(-3.89554688192456,-1.21942210470022,
6.25623435560171));
#260256=CARTESIAN_POINT('Ctrl Pts',(-1.09900968747838,-3.93121526828241,
6.45414918921635));
#260257=CARTESIAN_POINT('Ctrl Pts',(2.69840274557872,-3.06282523193468,
6.65206402283097));
#260258=CARTESIAN_POINT('Ctrl Pts',(4.03836232574987,0.594899575297352,
6.84997885644559));
#260259=CARTESIAN_POINT('Ctrl Pts',(1.70055918697444,3.71084548726127,7.04789369006024));
#260260=CARTESIAN_POINT('Ctrl Pts',(-2.18595421470653,3.44730038579951,
7.24580852367484));
#260261=CARTESIAN_POINT('Ctrl Pts',(-4.08170495873475,0.0442765013016559,
7.44372335728949));
#260262=CARTESIAN_POINT('Ctrl Pts',(-2.26022056730752,-3.39907027962765,
7.6416381909041));
#260263=CARTESIAN_POINT('Ctrl Pts',(1.61966132996968,-3.74686174750661,
7.83955302451875));
#260264=CARTESIAN_POINT('Ctrl Pts',(4.02450716653944,-0.682361960546052,
8.03746785813335));
#260265=CARTESIAN_POINT('Ctrl Pts',(2.76420826736859,3.00356928226049,8.23538269174799));
#260266=CARTESIAN_POINT('Ctrl Pts',(-1.01347299947942,3.95413053123613,
8.4332975253626));
#260267=CARTESIAN_POINT('Ctrl Pts',(-3.86817784334064,1.30363950193914,
8.63121235897725));
#260268=CARTESIAN_POINT('Ctrl Pts',(-3.20010807834974,-2.53408446299809,
8.82912719259186));
#260269=CARTESIAN_POINT('Ctrl Pts',(0.382320834683111,-4.064001298978,9.0270420262065));
#260270=CARTESIAN_POINT('Ctrl Pts',(3.61656768799618,-1.89280583707616,
9.22495685982112));
#260271=CARTESIAN_POINT('Ctrl Pts',(3.55718293013567,2.00218015679883,9.42287169343575));
#260272=CARTESIAN_POINT('Ctrl Pts',(0.258248644608689,4.0737677175172,9.62078652705038));
#260273=CARTESIAN_POINT('Ctrl Pts',(-3.27587435375479,2.43534863975144,
9.81870136066499));
#260274=CARTESIAN_POINT('Ctrl Pts',(-3.82663736646909,-1.42095821341447,
10.0166161942796));
#260275=CARTESIAN_POINT('Ctrl Pts',(-0.892456951597825,-3.98318922074665,
10.2145310278942));
#260276=CARTESIAN_POINT('Ctrl Pts',(2.85448978786086,-2.91790401311039,
10.4124458615089));
#260277=CARTESIAN_POINT('Ctrl Pts',(4.00183419434623,0.804735273048721,
10.6103606951235));
#260278=CARTESIAN_POINT('Ctrl Pts',(1.5046822876776,3.79449693528363,10.8082755287381));
#260279=CARTESIAN_POINT('Ctrl Pts',(-2.36279352137976,3.3285856687268,11.0061903623527));
#260280=CARTESIAN_POINT('Ctrl Pts',(-4.07845797114128,-0.168690119336393,
11.2041051959674));
#260281=CARTESIAN_POINT('Ctrl Pts',(-2.07984433807326,-3.5123387234309,
11.402020029582));
#260282=CARTESIAN_POINT('Ctrl Pts',(1.81289700092304,-3.65727770927665,
11.5999348631966));
#260283=CARTESIAN_POINT('Ctrl Pts',(4.0546213024502,-0.471510203966385,
11.7978496968113));
#260284=CARTESIAN_POINT('Ctrl Pts',(2.60377572967019,3.143664697182,11.9957645304259));
#260285=CARTESIAN_POINT('Ctrl Pts',(-1.21834525988501,3.89588380299556,
12.1936793640405));
#260286=CARTESIAN_POINT('Ctrl Pts',(-3.93091133232899,1.10009630309998,
12.3915941976551));
#260287=CARTESIAN_POINT('Ctrl Pts',(-3.06357100129271,-2.69755602328645,
12.5895090312698));
#260288=CARTESIAN_POINT('Ctrl Pts',(0.593783277616569,-4.03852661226194,
12.7874238648844));
#260289=CARTESIAN_POINT('Ctrl Pts',(3.71037528077956,-1.70158486550113,
12.985338698499));
#260290=CARTESIAN_POINT('Ctrl Pts',(3.4479044906093,2.1850012362432,13.1832535321136));
#260291=CARTESIAN_POINT('Ctrl Pts',(0.0454047552332988,4.08169256398689,
13.3811683657283));
#260292=CARTESIAN_POINT('Ctrl Pts',(-3.39844538472134,2.26116004426235,
13.5790831993429));
#260293=CARTESIAN_POINT('Ctrl Pts',(-3.74730930748937,-1.61862556907763,
13.7769980329575));
#260294=CARTESIAN_POINT('Ctrl Pts',(-0.683474379593425,-4.02431839582384,
13.9749128665721));
#260295=CARTESIAN_POINT('Ctrl Pts',(3.00280509128201,-2.76503840161413,
14.1728277001868));
#260296=CARTESIAN_POINT('Ctrl Pts',(3.95441052218274,1.01237996904276,14.3707425338014));
#260297=CARTESIAN_POINT('Ctrl Pts',(1.30470868489051,3.86781734634577,14.568657367416));
#260298=CARTESIAN_POINT('Ctrl Pts',(-2.53319979920386,3.2008084222486,14.7665722010306));
#260299=CARTESIAN_POINT('Ctrl Pts',(-4.06410682467997,-0.381197458580596,
14.9644870346453));
#260300=CARTESIAN_POINT('Ctrl Pts',(-1.89380544685607,-3.61604434372852,
15.1624018682599));
#260301=CARTESIAN_POINT('Ctrl Pts',(2.00119680929171,-3.55773623426484,
15.3603167018745));
#260302=CARTESIAN_POINT('Ctrl Pts',(4.07369618232338,-0.259374692681903,
15.5582315354892));
#260303=CARTESIAN_POINT('Ctrl Pts',(2.43625404700157,3.27520104798036,15.7561463691038));
#260304=CARTESIAN_POINT('Ctrl Pts',(-1.41990039056132,3.8270300118863,15.9540612027184));
#260305=CARTESIAN_POINT('Ctrl Pts',(-3.98294241241839,0.893557915648685,
16.1519760363331));
#260306=CARTESIAN_POINT('Ctrl Pts',(-2.91869286660792,-2.85368306861148,
16.3498908699477));
#260307=CARTESIAN_POINT('Ctrl Pts',(0.803628936719916,-4.00205657996199,
16.5478057035623));
#260308=CARTESIAN_POINT('Ctrl Pts',(3.79408111405252,-1.50573091363394,
16.7457205371769));
#260309=CARTESIAN_POINT('Ctrl Pts',(3.32923819091856,2.36187300075628,16.9436353707915));
#260310=CARTESIAN_POINT('Ctrl Pts',(-0.167561856769994,4.07850511539461,
17.1415502044062));
#260311=CARTESIAN_POINT('Ctrl Pts',(-3.51176540408623,2.08081384538083,
17.3394650380208));
#260312=CARTESIAN_POINT('Ctrl Pts',(-3.65777538941758,-1.81188353127027,
17.5373798716354));
#260313=CARTESIAN_POINT('Ctrl Pts',(-0.472637272581203,-4.05449553500327,
17.7352947052501));
#260314=CARTESIAN_POINT('Ctrl Pts',(3.14295695206386,-2.60463554851707,
17.9332095388647));
#260315=CARTESIAN_POINT('Ctrl Pts',(3.89619723248157,1.21725098829224,18.1311243724793));
#260316=CARTESIAN_POINT('Ctrl Pts',(1.10122727653295,3.93064030908756,18.3290392060939));
#260317=CARTESIAN_POINT('Ctrl Pts',(-2.69679425047197,3.06425289682812,
18.5269540397085));
#260318=CARTESIAN_POINT('Ctrl Pts',(-4.03852741795501,-0.592544991997906,
18.7248688733232));
#260319=CARTESIAN_POINT('Ctrl Pts',(-1.70292312088329,-3.71013846836731,
18.9227837069378));
#260320=CARTESIAN_POINT('Ctrl Pts',(2.1846477473792,-3.44806036801054,19.1206985405524));
#260321=CARTESIAN_POINT('Ctrl Pts',(4.08052651019308,-0.0473932962758928,
19.3186133741671));
#260322=CARTESIAN_POINT('Ctrl Pts',(2.26434865291609,3.3994862828525,19.5165282077817));
#260323=CARTESIAN_POINT('Ctrl Pts',(-1.6231099923986,3.74448000260561,19.7144865806121));
#260324=CARTESIAN_POINT('Ctrl Pts',(-3.21660798809866,1.7084537345319,19.8464733422378));
#260325=CARTESIAN_POINT('Ctrl Pts',(-3.40818269697037,0.577499442760154,
19.9124884926585));
#260326=CARTESIAN_POINT('Ctrl Pts',(-1.64352530806914,3.31099167201216,
-0.136564499136082));
#260327=CARTESIAN_POINT('Ctrl Pts',(-2.74148155646512,2.76598308843731,
-0.0705928879312071));
#260328=CARTESIAN_POINT('Ctrl Pts',(-4.33406015523805,0.507618810188653,
0.0613503344785438));
#260329=CARTESIAN_POINT('Ctrl Pts',(-2.78348151123821,-3.36600869366824,
0.259265168093171));
#260330=CARTESIAN_POINT('Ctrl Pts',(1.30565656478528,-4.16386605381997,
0.457180001707797));
#260331=CARTESIAN_POINT('Ctrl Pts',(4.20386515081771,-1.1748074554152,0.655094835322425));
#260332=CARTESIAN_POINT('Ctrl Pts',(3.27455352632889,2.88681338251992,0.853009668937051));
#260333=CARTESIAN_POINT('Ctrl Pts',(-0.637419483403673,4.31801064107583,
1.05092450255168));
#260334=CARTESIAN_POINT('Ctrl Pts',(-3.96862730125054,1.81748958957675,
1.24883933616631));
#260335=CARTESIAN_POINT('Ctrl Pts',(-3.68571786551885,-2.33860773972145,
1.44675416978093));
#260336=CARTESIAN_POINT('Ctrl Pts',(-0.0461296345460419,-4.36472324324944,
1.64466900339556));
#260337=CARTESIAN_POINT('Ctrl Pts',(3.63543174939503,-2.41595963851369,
1.84258383701018));
#260338=CARTESIAN_POINT('Ctrl Pts',(4.00620142017303,1.73308760492743,2.04049867062481));
#260339=CARTESIAN_POINT('Ctrl Pts',(0.728487329129644,4.30377279599383,
2.23841350423944));
#260340=CARTESIAN_POINT('Ctrl Pts',(-3.21265957262829,2.95499882051374,
2.43632833785407));
#260341=CARTESIAN_POINT('Ctrl Pts',(-4.22801937412663,-1.08491932724587,
2.63424317146869));
#260342=CARTESIAN_POINT('Ctrl Pts',(-1.39289310646734,-4.13679044579939,
2.83215800508332));
#260343=CARTESIAN_POINT('Ctrl Pts',(2.71074917659634,-3.42126179257488,
3.03007283869794));
#260344=CARTESIAN_POINT('Ctrl Pts',(4.34569502655482,0.410033210345885,
3.22798767231258));
#260345=CARTESIAN_POINT('Ctrl Pts',(2.02298807106426,3.86790774884172,3.4259025059272));
#260346=CARTESIAN_POINT('Ctrl Pts',(-2.14206711240008,3.80325395003319,
3.62381733954183));
#260347=CARTESIAN_POINT('Ctrl Pts',(-4.35632796252803,0.274951998575345,
3.82173217315645));
#260348=CARTESIAN_POINT('Ctrl Pts',(-2.60325270016525,-3.50375043805368,
4.01964700677108));
#260349=CARTESIAN_POINT('Ctrl Pts',(1.52062163734339,-4.09156470543431,
4.2175618403857));
#260350=CARTESIAN_POINT('Ctrl Pts',(4.259656011484,-0.953164480331169,4.41547667400034));
#260351=CARTESIAN_POINT('Ctrl Pts',(3.11939407001581,3.0532887974538,4.61339150761496));
#260352=CARTESIAN_POINT('Ctrl Pts',(-0.861720247300632,4.27909220293711,
4.81130634122959));
#260353=CARTESIAN_POINT('Ctrl Pts',(-4.05806035679004,1.60789862845514,
5.00922117484421));
#260354=CARTESIAN_POINT('Ctrl Pts',(-3.5586986223253,-2.52761863667785,
5.20713600845884));
#260355=CARTESIAN_POINT('Ctrl Pts',(0.181592990188709,-4.36121724359697,
5.40505084207346));
#260356=CARTESIAN_POINT('Ctrl Pts',(3.75650669086223,-2.22302706691864,
5.6029656756881));
#260357=CARTESIAN_POINT('Ctrl Pts',(3.91034542424596,1.93968825374242,5.80088050930272));
#260358=CARTESIAN_POINT('Ctrl Pts',(0.503007259850752,4.33591692212334,
5.99879534291735));
#260359=CARTESIAN_POINT('Ctrl Pts',(-3.3624228731466,2.78339797387454,6.19671017653197));
#260360=CARTESIAN_POINT('Ctrl Pts',(-4.1656727234605,-1.30397953198931,
6.39462501014661));
#260361=CARTESIAN_POINT('Ctrl Pts',(-1.17521745128784,-4.20381443466159,
6.59253984376122));
#260362=CARTESIAN_POINT('Ctrl Pts',(2.88551596345178,-3.2752083114691,6.79045467737586));
#260363=CARTESIAN_POINT('Ctrl Pts',(4.3183913062075,0.636151228345629,6.98836951099048));
#260364=CARTESIAN_POINT('Ctrl Pts',(1.81847972429224,3.96816372535188,7.18628434460512));
#260365=CARTESIAN_POINT('Ctrl Pts',(-2.33753311741372,3.68634382333638,
7.38419917821973));
#260366=CARTESIAN_POINT('Ctrl Pts',(-4.36473941327965,0.0473467318846832,
7.58211401183438));
#260367=CARTESIAN_POINT('Ctrl Pts',(-2.4169492632536,-3.63476933487058,
7.78002884544898));
#260368=CARTESIAN_POINT('Ctrl Pts',(1.73197223085787,-4.0066774327857,7.97794367906362));
#260369=CARTESIAN_POINT('Ctrl Pts',(4.3035753995963,-0.729678448939505,
8.17585851267824));
#260370=CARTESIAN_POINT('Ctrl Pts',(2.95588458574849,3.21184342311262,8.37377334629287));
#260371=CARTESIAN_POINT('Ctrl Pts',(-1.08374946005252,4.22831869265942,
8.5716881799075));
#260372=CARTESIAN_POINT('Ctrl Pts',(-4.13640585517419,1.39403674992373,
8.76960301352212));
#260373=CARTESIAN_POINT('Ctrl Pts',(-3.42201065425794,-2.70980348752494,
8.96751784713675));
#260374=CARTESIAN_POINT('Ctrl Pts',(0.40883180742601,-4.34580814257763,
9.16543268075137));
#260375=CARTESIAN_POINT('Ctrl Pts',(3.86734849485145,-2.02405718254882,
9.36334751436601));
#260376=CARTESIAN_POINT('Ctrl Pts',(3.803845866464,2.14101575964352,9.56126234798063));
#260377=CARTESIAN_POINT('Ctrl Pts',(0.276156177123374,4.35625178619118,
9.75917718159526));
#260378=CARTESIAN_POINT('Ctrl Pts',(-3.50303073086834,2.60422110379462,
9.95709201520989));
#260379=CARTESIAN_POINT('Ctrl Pts',(-4.0919848697084,-1.51949060047594,
10.1550068488245));
#260380=CARTESIAN_POINT('Ctrl Pts',(-0.954341891605521,-4.2593923760067,
10.3529216824392));
#260381=CARTESIAN_POINT('Ctrl Pts',(3.05242642666228,-3.12023793462469,
10.5508365160538));
#260382=CARTESIAN_POINT('Ctrl Pts',(4.27933023333652,0.860537397739989,
10.7487513496684));
#260383=CARTESIAN_POINT('Ctrl Pts',(1.60902028732771,4.05761574989858,10.9466661832831));
#260384=CARTESIAN_POINT('Ctrl Pts',(-2.52663485295242,3.55939716506929,
11.1445810168977));
#260385=CARTESIAN_POINT('Ctrl Pts',(-4.36126727238094,-0.18038746551797,
11.3424958505123));
#260386=CARTESIAN_POINT('Ctrl Pts',(-2.22406534711636,-3.75589206322724,
11.5404106841269));
#260387=CARTESIAN_POINT('Ctrl Pts',(1.93860729086062,-3.91088143909774,
11.7383255177416));
#260388=CARTESIAN_POINT('Ctrl Pts',(4.33577771633291,-0.504205764949182,
11.9362403513562));
#260389=CARTESIAN_POINT('Ctrl Pts',(2.78432730085307,3.36165336413227,12.1341551849708));
#260390=CARTESIAN_POINT('Ctrl Pts',(-1.30282801637157,4.16603300738415,
12.3320700185855));
#260391=CARTESIAN_POINT('Ctrl Pts',(-4.20348942311656,1.17637941524129,
12.5299848522001));
#260392=CARTESIAN_POINT('Ctrl Pts',(-3.27600579412479,-2.88461052756198,
12.7278996858147));
#260393=CARTESIAN_POINT('Ctrl Pts',(0.634957524113322,-4.31856698470986,
12.9258145194293));
#260394=CARTESIAN_POINT('Ctrl Pts',(3.96766091371217,-1.81957652563777,
13.123729353044));
#260395=CARTESIAN_POINT('Ctrl Pts',(3.68698981811055,2.33651405731482,13.3216441866586));
#260396=CARTESIAN_POINT('Ctrl Pts',(0.0485532214407396,4.36472615905254,
13.5195590202732));
#260397=CARTESIAN_POINT('Ctrl Pts',(-3.63410110836858,2.41795388561951,
13.7174738538878));
#260398=CARTESIAN_POINT('Ctrl Pts',(-4.0071560275681,-1.73086464801346,
13.9153886875025));
#260399=CARTESIAN_POINT('Ctrl Pts',(-0.730868005585374,-4.30337353910152,
14.1133035211171));
#260400=CARTESIAN_POINT('Ctrl Pts',(3.21102624144054,-2.95677228333969,
14.3112183547317));
#260401=CARTESIAN_POINT('Ctrl Pts',(4.22861809879787,1.08258063646653,14.5091331883463));
#260402=CARTESIAN_POINT('Ctrl Pts',(1.39518007238701,4.13602036051992,14.707048021961));
#260403=CARTESIAN_POINT('Ctrl Pts',(-2.70885747918549,3.42275956155259,
14.9049628555756));
#260404=CARTESIAN_POINT('Ctrl Pts',(-4.3459209856653,-0.407630533938537,
15.1028776891902));
#260405=CARTESIAN_POINT('Ctrl Pts',(-2.02512610748298,-3.86678886073412,
15.3007925228048));
#260406=CARTESIAN_POINT('Ctrl Pts',(2.13996422464412,-3.80443753792594,
15.4987073564195));
#260407=CARTESIAN_POINT('Ctrl Pts',(4.35617529058869,-0.277360307861903,
15.6966221900341));
#260408=CARTESIAN_POINT('Ctrl Pts',(2.60518929398711,3.50231073658149,15.8945370236487));
#260409=CARTESIAN_POINT('Ctrl Pts',(-1.51835942584521,4.09240474202774,
16.0924518572633));
#260410=CARTESIAN_POINT('Ctrl Pts',(-4.25912845344279,0.955519198940071,
16.290366690878));
#260411=CARTESIAN_POINT('Ctrl Pts',(-3.12108148896944,-3.05156376771492,
16.4882815244926));
#260412=CARTESIAN_POINT('Ctrl Pts',(0.859354345601846,-4.279568039663,16.6861963581073));
#260413=CARTESIAN_POINT('Ctrl Pts',(4.05717109470311,-1.61014162732844,
16.8841111917219));
#260414=CARTESIAN_POINT('Ctrl Pts',(3.56009493459384,2.52565050139181,17.0820260253365));
#260415=CARTESIAN_POINT('Ctrl Pts',(-0.1791809667284,4.36131768572114,17.2799408589511));
#260416=CARTESIAN_POINT('Ctrl Pts',(-3.75527898865047,2.22510208220613,
17.4778556925657));
#260417=CARTESIAN_POINT('Ctrl Pts',(-3.91141362948099,-1.93752354497935,
17.6757705261804));
#260418=CARTESIAN_POINT('Ctrl Pts',(-0.505410986995922,-4.33564322789287,
17.873685359795));
#260419=CARTESIAN_POINT('Ctrl Pts',(3.36089654240142,-2.78524674144156,
18.0716001934096));
#260420=CARTESIAN_POINT('Ctrl Pts',(4.16636817076433,1.30165786556497,18.2695150270243));
#260421=CARTESIAN_POINT('Ctrl Pts',(1.17758881287491,4.20319960652379,18.4674298606389));
#260422=CARTESIAN_POINT('Ctrl Pts',(-2.88379593173475,3.27673497380564,
18.6653446942535));
#260423=CARTESIAN_POINT('Ctrl Pts',(-4.31856784627148,-0.633633373029566,
18.8632595278681));
#260424=CARTESIAN_POINT('Ctrl Pts',(-1.82100757860965,-3.9674076802032,
19.0611743614828));
#260425=CARTESIAN_POINT('Ctrl Pts',(2.33613605675073,-3.68715650439574,
19.2590891950974));
#260426=CARTESIAN_POINT('Ctrl Pts',(4.36347924850822,-0.050679652319815,
19.457004028712));
#260427=CARTESIAN_POINT('Ctrl Pts',(2.42136359945361,3.63521418467965,19.6549188623266));
#260428=CARTESIAN_POINT('Ctrl Pts',(-1.73566003117141,4.00413053242251,
19.8528772351571));
#260429=CARTESIAN_POINT('Ctrl Pts',(-3.4396547042627,1.82692169724777,19.9848639967826));
#260430=CARTESIAN_POINT('Ctrl Pts',(-3.64451362739738,0.617544532112318,
20.0508791472033));
#260431=CARTESIAN_POINT('Ctrl Pts',(-1.75010080893059,3.52569514755975,
0.00182615540880226));
#260432=CARTESIAN_POINT('Ctrl Pts',(-2.91925476661787,2.94534511686322,
0.0677977666136779));
#260433=CARTESIAN_POINT('Ctrl Pts',(-4.61510519271965,0.540535692379026,
0.199740989023429));
#260434=CARTESIAN_POINT('Ctrl Pts',(-2.96397823662627,-3.58427978488325,
0.397655822638056));
#260435=CARTESIAN_POINT('Ctrl Pts',(1.39032274039075,-4.43387474065139,
0.595570656252683));
#260436=CARTESIAN_POINT('Ctrl Pts',(4.47646760592004,-1.25098863276732,
0.79348548986731));
#260437=CARTESIAN_POINT('Ctrl Pts',(3.48689414588177,3.07401073240257,0.991400323481937));
#260438=CARTESIAN_POINT('Ctrl Pts',(-0.678753377301771,4.59801493704769,
1.18931515709656));
#260439=CARTESIAN_POINT('Ctrl Pts',(-4.2259756002312,1.93534592094488,1.38722999071119));
#260440=CARTESIAN_POINT('Ctrl Pts',(-3.92472071240123,-2.4902563270329,
1.58514482432581));
#260441=CARTESIAN_POINT('Ctrl Pts',(-0.0491209416358709,-4.64775664923788,
1.78305965794044));
#260442=CARTESIAN_POINT('Ctrl Pts',(3.87117375935205,-2.57262416157981,
1.98097449155507));
#260443=CARTESIAN_POINT('Ctrl Pts',(4.26598623809502,1.84547083299521,2.17888932516969));
#260444=CARTESIAN_POINT('Ctrl Pts',(0.775726578560172,4.58285382935247,
2.37680415878432));
#260445=CARTESIAN_POINT('Ctrl Pts',(-3.42098663724313,3.14661770085293,
2.57471899239895));
#260446=CARTESIAN_POINT('Ctrl Pts',(-4.50218812603891,-1.1552716486417,
2.77263382601358));
#260447=CARTESIAN_POINT('Ctrl Pts',(-1.48321619412499,-4.40504339666996,
2.9705486596282));
#260448=CARTESIAN_POINT('Ctrl Pts',(2.88652952496526,-3.643115808045,3.16846349324284));
#260449=CARTESIAN_POINT('Ctrl Pts',(4.6274945350701,0.436622088866865,3.36637832685745));
#260450=CARTESIAN_POINT('Ctrl Pts',(2.15417008928569,4.11872482089706,3.56429316047209));
#260451=CARTESIAN_POINT('Ctrl Pts',(-2.28097089091936,4.04987850314359,
3.76220799408671));
#260452=CARTESIAN_POINT('Ctrl Pts',(-4.63881697090765,0.292781445324475,
3.96012282770134));
#260453=CARTESIAN_POINT('Ctrl Pts',(-2.77206236742561,-3.73095348506232,
4.15803766131596));
#260454=CARTESIAN_POINT('Ctrl Pts',(1.61922736724908,-4.35688496283948,
4.35595249493059));
#260455=CARTESIAN_POINT('Ctrl Pts',(4.53587626236338,-1.01497307031512,
4.55386732854522));
#260456=CARTESIAN_POINT('Ctrl Pts',(3.32167327056359,3.25128135726756,4.75178216215984));
#260457=CARTESIAN_POINT('Ctrl Pts',(-0.917599074664954,4.55657280668652,
4.94969699577447));
#260458=CARTESIAN_POINT('Ctrl Pts',(-4.32120800223705,1.71216389338339,
5.1476118293891));
#260459=CARTESIAN_POINT('Ctrl Pts',(-3.78946482119506,-2.69152376236598,
5.34552666300372));
#260460=CARTESIAN_POINT('Ctrl Pts',(0.193368509426066,-4.64402330068658,
5.54344149661836));
#260461=CARTESIAN_POINT('Ctrl Pts',(4.00009988659977,-2.36718074798598,
5.74135633023296));
#260462=CARTESIAN_POINT('Ctrl Pts',(4.16391439582449,2.06546863944303,5.93927116384762));
#260463=CARTESIAN_POINT('Ctrl Pts',(0.535625102966643,4.61708236289889,
6.13718599746222));
#260464=CARTESIAN_POINT('Ctrl Pts',(-3.58046143942498,2.96388928222623,
6.33510083107687));
#260465=CARTESIAN_POINT('Ctrl Pts',(-4.43579856499644,-1.3885369592784,
6.53301566469148));
#260466=CARTESIAN_POINT('Ctrl Pts',(-1.25142521509729,-4.47641360104077,
6.73093049830612));
#260467=CARTESIAN_POINT('Ctrl Pts',(3.07262918132483,-3.48759139100354,
6.92884533192075));
#260468=CARTESIAN_POINT('Ctrl Pts',(4.59842028666512,0.677402881393908,
7.12676016553538));
#260469=CARTESIAN_POINT('Ctrl Pts',(1.93640026161004,4.22548196344249,7.32467499914999));
#260470=CARTESIAN_POINT('Ctrl Pts',(-2.4891120201209,3.92538726087325,7.52258983276462));
#260471=CARTESIAN_POINT('Ctrl Pts',(-4.64777386782454,0.0504169624677064,
7.72050466637926));
#260472=CARTESIAN_POINT('Ctrl Pts',(-2.57367795919968,-3.8704683901135,
7.91841949999387));
#260473=CARTESIAN_POINT('Ctrl Pts',(1.84428313174606,-4.26649311806479,
8.11633433360852));
#260474=CARTESIAN_POINT('Ctrl Pts',(4.58264363265316,-0.776994937332951,
8.31424916722312));
#260475=CARTESIAN_POINT('Ctrl Pts',(3.14756090412839,3.42011756396473,8.51216400083777));
#260476=CARTESIAN_POINT('Ctrl Pts',(-1.15402592062561,4.5025068540827,8.71007883445239));
#260477=CARTESIAN_POINT('Ctrl Pts',(-4.40463386700773,1.48443399790831,
8.90799366806701));
#260478=CARTESIAN_POINT('Ctrl Pts',(-3.64391323016614,-2.88552251205178,
9.10590850168166));
#260479=CARTESIAN_POINT('Ctrl Pts',(0.43534278016891,-4.62761498617725,
9.30382333529625));
#260480=CARTESIAN_POINT('Ctrl Pts',(4.11812930170671,-2.15530852802148,
9.5017381689109));
#260481=CARTESIAN_POINT('Ctrl Pts',(4.05050880279234,2.2798513624882,9.69965300252552));
#260482=CARTESIAN_POINT('Ctrl Pts',(0.294063709638058,4.63873585486514,
9.89756783614015));
#260483=CARTESIAN_POINT('Ctrl Pts',(-3.73018710798186,2.7730935678378,10.0954826697548));
#260484=CARTESIAN_POINT('Ctrl Pts',(-4.3573323729477,-1.61802298753741,
10.2933975033694));
#260485=CARTESIAN_POINT('Ctrl Pts',(-1.01622683161321,-4.53559553126675,
10.491312336984));
#260486=CARTESIAN_POINT('Ctrl Pts',(3.25036306546372,-3.32257185613898,
10.6892271705987));
#260487=CARTESIAN_POINT('Ctrl Pts',(4.55682627232683,0.916339522431252,
10.8871420042133));
#260488=CARTESIAN_POINT('Ctrl Pts',(1.71335828697782,4.32073456451352,11.0850568378279));
#260489=CARTESIAN_POINT('Ctrl Pts',(-2.69047618452508,3.79020866141177,
11.2829716714425));
#260490=CARTESIAN_POINT('Ctrl Pts',(-4.64407657362062,-0.192084811699544,
11.4808865050572));
#260491=CARTESIAN_POINT('Ctrl Pts',(-2.36828635615946,-3.99944540302358,
11.6788013386718));
#260492=CARTESIAN_POINT('Ctrl Pts',(2.06431758079821,-4.16448516891884,
11.8767161722864));
#260493=CARTESIAN_POINT('Ctrl Pts',(4.61693413021561,-0.536901325931978,
12.074631005901));
#260494=CARTESIAN_POINT('Ctrl Pts',(2.96487887203597,3.57964203108254,12.2725458395157));
#260495=CARTESIAN_POINT('Ctrl Pts',(-1.38731077285814,4.43618221177274,
12.4704606731303));
#260496=CARTESIAN_POINT('Ctrl Pts',(-4.47606751390413,1.25266252738259,
12.6683755067449));
#260497=CARTESIAN_POINT('Ctrl Pts',(-3.48844058695688,-3.07166503183752,
12.8662903403595));
#260498=CARTESIAN_POINT('Ctrl Pts',(0.676131770610078,-4.59860735715779,
13.0642051739742));
#260499=CARTESIAN_POINT('Ctrl Pts',(4.22494654664478,-1.93756818577441,
13.2621200075888));
#260500=CARTESIAN_POINT('Ctrl Pts',(3.9260751456118,2.48802687838644,13.4600348412034));
#260501=CARTESIAN_POINT('Ctrl Pts',(0.0517016876481762,4.64775975411819,
13.657949674818));
#260502=CARTESIAN_POINT('Ctrl Pts',(-3.86975683201582,2.57474772697667,
13.8558645084327));
#260503=CARTESIAN_POINT('Ctrl Pts',(-4.26700274764684,-1.84310372694929,
14.0537793420473));
#260504=CARTESIAN_POINT('Ctrl Pts',(-0.778261631577316,-4.58242868237922,
14.2516941756619));
#260505=CARTESIAN_POINT('Ctrl Pts',(3.41924739159908,-3.14850616506524,
14.4496090092766));
#260506=CARTESIAN_POINT('Ctrl Pts',(4.50282567541301,1.15278130389029,14.6475238428912));
#260507=CARTESIAN_POINT('Ctrl Pts',(1.48565145988351,4.40422337469407,14.8454386765058));
#260508=CARTESIAN_POINT('Ctrl Pts',(-2.8845151591671,3.64471070085658,15.0433535101204));
#260509=CARTESIAN_POINT('Ctrl Pts',(-4.62773514665064,-0.434063609296485,
15.2412683437351));
#260510=CARTESIAN_POINT('Ctrl Pts',(-2.15644676810989,-4.11753337773972,
15.4391831773497));
#260511=CARTESIAN_POINT('Ctrl Pts',(2.27873163999654,-4.05113884158703,
15.6370980109643));
#260512=CARTESIAN_POINT('Ctrl Pts',(4.63865439885401,-0.2953459230419,15.8350128445789));
#260513=CARTESIAN_POINT('Ctrl Pts',(2.77412454097265,3.72942042518262,16.0329276781936));
#260514=CARTESIAN_POINT('Ctrl Pts',(-1.61681846112911,4.35777947216919,
16.2308425118082));
#260515=CARTESIAN_POINT('Ctrl Pts',(-4.53531449446717,1.01748048223146,
16.4287573454228));
#260516=CARTESIAN_POINT('Ctrl Pts',(-3.32347011133097,-3.24944446681835,
16.6266721790375));
#260517=CARTESIAN_POINT('Ctrl Pts',(0.91507975448378,-4.55707949936403,
16.8245870126521));
#260518=CARTESIAN_POINT('Ctrl Pts',(4.32026107535369,-1.71455234102294,
17.0225018462667));
#260519=CARTESIAN_POINT('Ctrl Pts',(3.79095167826912,2.68942800202735,17.2204166798813));
#260520=CARTESIAN_POINT('Ctrl Pts',(-0.190800076686807,4.64413025604767,
17.4183315134959));
#260521=CARTESIAN_POINT('Ctrl Pts',(-3.99879257321471,2.36939031903143,
17.6162463471106));
#260522=CARTESIAN_POINT('Ctrl Pts',(-4.16505186954441,-2.06316355868843,
17.8141611807252));
#260523=CARTESIAN_POINT('Ctrl Pts',(-0.538184701410647,-4.61679092078249,
18.0120760143399));
#260524=CARTESIAN_POINT('Ctrl Pts',(3.57883613273897,-2.96585793436604,
18.2099908479544));
#260525=CARTESIAN_POINT('Ctrl Pts',(4.43653910904709,1.3860647428377,18.4079056815691));
#260526=CARTESIAN_POINT('Ctrl Pts',(1.25395034921688,4.47575890396004,18.6058205151837));
#260527=CARTESIAN_POINT('Ctrl Pts',(-3.07079761299755,3.48921705078318,
18.8037353487984));
#260528=CARTESIAN_POINT('Ctrl Pts',(-4.59860827458794,-0.674721754061232,
19.001650182413));
#260529=CARTESIAN_POINT('Ctrl Pts',(-1.93909203633601,-4.22467689203909,
19.1995650160276));
#260530=CARTESIAN_POINT('Ctrl Pts',(2.48762436612226,-3.92625264078095,
19.3974798496422));
#260531=CARTESIAN_POINT('Ctrl Pts',(4.64643198682337,-0.0539660083637359,
19.5953946832569));
#260532=CARTESIAN_POINT('Ctrl Pts',(2.57837854599114,3.87094208650678,19.7933095168715));
#260533=CARTESIAN_POINT('Ctrl Pts',(-1.84821006994423,4.26378106223944,
19.9912678897019));
#260534=CARTESIAN_POINT('Ctrl Pts',(-3.66270142042672,1.94538965996362,
20.1232546513276));
#260535=CARTESIAN_POINT('Ctrl Pts',(-3.88084455782439,0.657589621464481,
20.1892698017482));
#260536=CARTESIAN_POINT('Ctrl Pts',(-1.87556942017163,-2.62718932281027,
2.51101223147643E-16));
#260537=CARTESIAN_POINT('Ctrl Pts',(-1.94321685966309,-2.58955705721538,
-2.98696319824802E-15));
#260538=CARTESIAN_POINT('Ctrl Pts',(-2.00929342641587,-2.54939743639506,
-3.18303088817132E-15));
#260539=CARTESIAN_POINT('Ctrl Pts',(-2.07363931685561,-2.5067408274455,
-3.47291639890557E-15));
#260540=CARTESIAN_POINT('Ctrl Pts',(-2.15991597834028,-2.44954572477035,
-4.04153294977544E-15));
#260541=CARTESIAN_POINT('Ctrl Pts',(-2.24308257138536,-2.38786373783807,
-3.13550384268977E-15));
#260542=CARTESIAN_POINT('Ctrl Pts',(-2.32304487609101,-2.32209391940347,
-2.33840724561674E-15));
#260543=CARTESIAN_POINT('Ctrl Pts',(-2.39668046934978,-2.26152788623596,
-1.60437786732316E-15));
#260544=CARTESIAN_POINT('Ctrl Pts',(-2.46759885376822,-2.19749435520736,
-1.58516999870415E-15));
#260545=CARTESIAN_POINT('Ctrl Pts',(-2.53570984456099,-2.13026962439171,
-1.08940634291343E-15));
#260546=CARTESIAN_POINT('Ctrl Pts',(-2.54906783404081,-2.11708544902489,
-1.04875430384881E-15));
#260547=CARTESIAN_POINT('Ctrl Pts',(-2.56231717356686,-2.10377893194792,
4.2212099467669E-16));
#260548=CARTESIAN_POINT('Ctrl Pts',(-2.57544805121062,-2.09036165114785,
5.759281940243E-16));
#260549=CARTESIAN_POINT('Ctrl Pts',(-2.6498106779512,-2.01437706953205,
-5.81331574431158E-17));
#260550=CARTESIAN_POINT('Ctrl Pts',(-2.72045456846015,-1.93476701230077,
-1.89288485759184E-15));
#260551=CARTESIAN_POINT('Ctrl Pts',(-2.78728141151529,-1.85194311734714,
-1.5404344466674E-15));
#260552=CARTESIAN_POINT('Ctrl Pts',(-2.85581727251888,-1.76700109864913,
-1.17897053082972E-15));
#260553=CARTESIAN_POINT('Ctrl Pts',(-2.9203389474257,-1.67867826627061,
1.37094499452068E-15));
#260554=CARTESIAN_POINT('Ctrl Pts',(-2.98071257569894,-1.58737132139589,
2.22044604925031E-15));
#260555=CARTESIAN_POINT('Ctrl Pts',(-3.01428701700591,-1.53659452117212,
2.69286296567517E-15));
#260556=CARTESIAN_POINT('Ctrl Pts',(-3.04657809338566,-1.48489406210769,
5.92055426793446E-15));
#260557=CARTESIAN_POINT('Ctrl Pts',(-3.07755815354105,-1.43233300373666,
3.56659146660832E-15));
#260558=CARTESIAN_POINT('Ctrl Pts',(-3.08697793780036,-1.41635131009848,
2.90579300526694E-15));
#260559=CARTESIAN_POINT('Ctrl Pts',(-3.0962717941836,-1.40029795380699,
4.94759990803286E-15));
#260560=CARTESIAN_POINT('Ctrl Pts',(-3.10543719647879,-1.38417861149924,
4.6074255521944E-15));
#260561=CARTESIAN_POINT('Ctrl Pts',(-3.16080948827413,-1.28679445998392,
2.67287859025293E-15));
#260562=CARTESIAN_POINT('Ctrl Pts',(-3.21152045425685,-1.18696368226749,
5.82879830159953E-15));
#260563=CARTESIAN_POINT('Ctrl Pts',(-3.25746102236525,-1.08512302646891,
4.46864767411626E-15));
#260564=CARTESIAN_POINT('Ctrl Pts',(-3.30388770314436,-0.982204760287715,
3.09410483336006E-15));
#260565=CARTESIAN_POINT('Ctrl Pts',(-3.34544306335798,-0.877233138262983,
2.6696688988621E-15));
#260566=CARTESIAN_POINT('Ctrl Pts',(-3.38197996308487,-0.770617372601717,
3.30291349825984E-15));
#260567=CARTESIAN_POINT('Ctrl Pts',(-3.41753428813729,-0.666868789214298,
3.91912846157006E-15));
#260568=CARTESIAN_POINT('Ctrl Pts',(-3.44833674489485,-0.561562436895271,
3.88870334882072E-15));
#260569=CARTESIAN_POINT('Ctrl Pts',(-3.47421314506653,-0.455048337768718,
3.66373598126302E-15));
#260570=CARTESIAN_POINT('Ctrl Pts',(-3.48715134515238,-0.401791288205442,
3.55125229748417E-15));
#260571=CARTESIAN_POINT('Ctrl Pts',(-3.49885739233011,-0.348231952880776,
3.07635813663633E-15));
#260572=CARTESIAN_POINT('Ctrl Pts',(-3.50930537873547,-0.294412451083064,
3.33066907387547E-15));
#260573=CARTESIAN_POINT('Ctrl Pts',(-3.51491240797328,-0.265529611037486,
3.4671478943173E-15));
#260574=CARTESIAN_POINT('Ctrl Pts',(-3.52015705948641,-0.236571826863691,
4.32442325837932E-15));
#260575=CARTESIAN_POINT('Ctrl Pts',(-3.52503497038303,-0.207545526731505,
4.30211422042248E-15));
#260576=CARTESIAN_POINT('Ctrl Pts',(-3.52881969857847,-0.185024275554966,
4.28480483393351E-15));
#260577=CARTESIAN_POINT('Ctrl Pts',(-3.53238441234349,-0.162456043358417,
2.9467404425913E-15));
#260578=CARTESIAN_POINT('Ctrl Pts',(-3.53572297498661,-0.139872357824409,
3.13638004456607E-15));
#260579=CARTESIAN_POINT('Ctrl Pts',(-3.53609939778504,-0.137326048224713,
3.15776190175956E-15));
#260580=CARTESIAN_POINT('Ctrl Pts',(-3.53647294545778,-0.134779558926291,
3.14642742435836E-15));
#260581=CARTESIAN_POINT('Ctrl Pts',(-3.53684361068852,-0.132232937888745,
3.1641356201817E-15));
#260582=CARTESIAN_POINT('Ctrl Pts',(-3.55353020233728,-0.0175892599457696,
5.186219913102E-15));
#260583=CARTESIAN_POINT('Ctrl Pts',(-3.56440026289145,0.0974665540390713,
5.07191696097025E-15));
#260584=CARTESIAN_POINT('Ctrl Pts',(-3.56931023113663,0.212509296148271,
3.83026943495679E-15));
#260585=CARTESIAN_POINT('Ctrl Pts',(-3.57218292020646,0.279817680096528,
1.70301208742856E-15));
#260586=CARTESIAN_POINT('Ctrl Pts',(-3.57301463943239,0.347122208748641,
5.48449796780725E-15));
#260587=CARTESIAN_POINT('Ctrl Pts',(-3.57176938301271,0.41434171205851,
4.19109191795997E-15));
#260588=CARTESIAN_POINT('Ctrl Pts',(-3.5697177817538,0.525088073558945,
2.14805900299604E-15));
#260589=CARTESIAN_POINT('Ctrl Pts',(-3.56203156872923,0.635603442404429,
5.535809693293E-15));
#260590=CARTESIAN_POINT('Ctrl Pts',(-3.54897252034833,0.745605368646729,
5.13478148889135E-15));
#260591=CARTESIAN_POINT('Ctrl Pts',(-3.53562561329751,0.858032051062244,
4.72491347915652E-15));
#260592=CARTESIAN_POINT('Ctrl Pts',(-3.5166663209495,0.969923083623129,
3.47522615189797E-15));
#260593=CARTESIAN_POINT('Ctrl Pts',(-3.49231997030835,1.0809798264328,2.1094237467878E-15));
#260594=CARTESIAN_POINT('Ctrl Pts',(-3.48394443529913,1.1191851267311,1.63956581907238E-15));
#260595=CARTESIAN_POINT('Ctrl Pts',(-3.47493090089764,1.1572916683045,1.00344127597866E-16));
#260596=CARTESIAN_POINT('Ctrl Pts',(-3.46528713442918,1.19528713766673,
4.44089209850063E-16));
#260597=CARTESIAN_POINT('Ctrl Pts',(-3.46131507764283,1.21093664166752,
3.61845925886729E-16));
#260598=CARTESIAN_POINT('Ctrl Pts',(-3.45723619243246,1.22656668453369,
-1.56589949516286E-16));
#260599=CARTESIAN_POINT('Ctrl Pts',(-3.45305468210887,1.2421634091862,5.55111512312578E-17));
#260600=CARTESIAN_POINT('Ctrl Pts',(-3.42263513893302,1.35562605838552,
3.11615268497786E-15));
#260601=CARTESIAN_POINT('Ctrl Pts',(-3.38674446557073,1.46750384585196,
-5.69849959668556E-16));
#260602=CARTESIAN_POINT('Ctrl Pts',(-3.34571175820367,1.57747597390746,
-7.7715611723761E-16));
#260603=CARTESIAN_POINT('Ctrl Pts',(-3.30470986567157,1.68736551484662,
-9.84306591561689E-16));
#260604=CARTESIAN_POINT('Ctrl Pts',(-3.25857332074224,1.79535300088055,
6.45103697825085E-16));
#260605=CARTESIAN_POINT('Ctrl Pts',(-3.20757486876686,1.90112149564073,
3.33066907387547E-16));
#260606=CARTESIAN_POINT('Ctrl Pts',(-3.15595880640236,2.00817088655903,
1.72512343350343E-17));
#260607=CARTESIAN_POINT('Ctrl Pts',(-3.09936212517733,2.11294801982453,
2.74834656774289E-15));
#260608=CARTESIAN_POINT('Ctrl Pts',(-3.03801481501982,2.21511582858276,
-7.21644966006352E-16));
#260609=CARTESIAN_POINT('Ctrl Pts',(-2.97799894244694,2.3150662612218,-4.11632631688848E-15));
#260610=CARTESIAN_POINT('Ctrl Pts',(-2.91343592049529,2.41252009783622,
1.82683910698455E-15));
#260611=CARTESIAN_POINT('Ctrl Pts',(-2.84449674836446,2.50714265484644,
-2.38697950294409E-15));
#260612=CARTESIAN_POINT('Ctrl Pts',(-2.83448523320077,2.52088397396958,
-2.89070916018422E-15));
#260613=CARTESIAN_POINT('Ctrl Pts',(-2.82438675889958,2.53455810077557,
-1.50365065139371E-15));
#260614=CARTESIAN_POINT('Ctrl Pts',(-2.81420395125994,2.54816172130323,
-1.22124532708767E-15));
#260615=CARTESIAN_POINT('Ctrl Pts',(-2.74076732429818,2.64626865225709,
1.88643940676309E-16));
#260616=CARTESIAN_POINT('Ctrl Pts',(-2.66291885988769,2.74075040032154,
-7.7831521150718E-16));
#260617=CARTESIAN_POINT('Ctrl Pts',(-2.58094817198274,2.83127269698007,
-4.9960036108132E-16));
#260618=CARTESIAN_POINT('Ctrl Pts',(-2.49883747965016,2.92194960405673,
-3.19828665886133E-16));
#260619=CARTESIAN_POINT('Ctrl Pts',(-2.41259008723588,3.00865435231219,
-9.23807423859023E-16));
#260620=CARTESIAN_POINT('Ctrl Pts',(-2.32244725468202,3.09103471217502,
-3.88578058618805E-16));
#260621=CARTESIAN_POINT('Ctrl Pts',(-2.23400471151706,3.17186119972475,
-1.22638691089234E-15));
#260622=CARTESIAN_POINT('Ctrl Pts',(-2.14181179126767,3.24852559953772,
-1.07853142926365E-15));
#260623=CARTESIAN_POINT('Ctrl Pts',(-2.04605523770132,3.32066838036946,
-8.32667268468867E-16));
#260624=CARTESIAN_POINT('Ctrl Pts',(-1.95043831892495,3.39270596065171,
-1.12437181343088E-15));
#260625=CARTESIAN_POINT('Ctrl Pts',(-1.85126778116324,3.46023588193575,
4.8784508495953E-17));
#260626=CARTESIAN_POINT('Ctrl Pts',(-1.74869447533115,3.52286199445086,
-4.9960036108132E-16));
#260627=CARTESIAN_POINT('Origin',(-1.73205080756888,-3.,-8.));
#260628=CARTESIAN_POINT('',(-1.73205080756888,-3.,-8.));
#260629=CARTESIAN_POINT('',(1.73205080756888,-3.,-8.));
#260630=CARTESIAN_POINT('',(-0.86602540378444,-3.,-8.));
#260631=CARTESIAN_POINT('',(-1.73205080756888,-3.,-4.));
#260632=CARTESIAN_POINT('',(-1.73205080756888,-3.,-8.));
#260633=CARTESIAN_POINT('',(1.73205080756888,-3.,-4.));
#260634=CARTESIAN_POINT('',(-1.73205080756888,-3.,-4.));
#260635=CARTESIAN_POINT('',(1.73205080756888,-3.,-8.));
#260636=CARTESIAN_POINT('Origin',(-3.46410161513775,4.24230095489963E-16,
-8.));
#260637=CARTESIAN_POINT('',(-3.46410161513775,4.24230095489963E-16,-8.));
#260638=CARTESIAN_POINT('',(-3.03108891324554,-0.749999999999999,-8.));
#260639=CARTESIAN_POINT('',(-3.46410161513775,5.55111512312578E-16,-4.));
#260640=CARTESIAN_POINT('',(-3.46410161513775,4.24230095489963E-16,-8.));
#260641=CARTESIAN_POINT('',(-3.46410161513775,4.24230095489963E-16,-4.));
#260642=CARTESIAN_POINT('Origin',(-1.73205080756888,3.,-8.));
#260643=CARTESIAN_POINT('',(-1.73205080756888,3.,-8.));
#260644=CARTESIAN_POINT('',(-2.1650635094611,2.25,-8.));
#260645=CARTESIAN_POINT('',(-1.73205080756888,3.,-4.));
#260646=CARTESIAN_POINT('',(-1.73205080756888,3.,-8.));
#260647=CARTESIAN_POINT('',(-1.73205080756888,3.,-4.));
#260648=CARTESIAN_POINT('Origin',(1.73205080756888,3.,-8.));
#260649=CARTESIAN_POINT('',(1.73205080756888,3.,-8.));
#260650=CARTESIAN_POINT('',(0.866025403784439,3.,-8.));
#260651=CARTESIAN_POINT('',(1.73205080756888,3.,-4.));
#260652=CARTESIAN_POINT('',(1.73205080756888,3.,-8.));
#260653=CARTESIAN_POINT('',(1.73205080756888,3.,-4.));
#260654=CARTESIAN_POINT('Origin',(3.46410161513775,0.,-8.));
#260655=CARTESIAN_POINT('',(3.46410161513775,0.,-8.));
#260656=CARTESIAN_POINT('',(3.03108891324554,0.75,-8.));
#260657=CARTESIAN_POINT('',(3.46410161513775,0.,-4.));
#260658=CARTESIAN_POINT('',(3.46410161513775,0.,-8.));
#260659=CARTESIAN_POINT('',(3.46410161513775,0.,-4.));
#260660=CARTESIAN_POINT('Origin',(1.73205080756888,-3.,-8.));
#260661=CARTESIAN_POINT('',(2.1650635094611,-2.25,-8.));
#260662=CARTESIAN_POINT('',(1.73205080756888,-3.,-4.));
#260663=CARTESIAN_POINT('Origin',(0.,5.55111512312578E-16,-4.));
#260664=CARTESIAN_POINT('Origin',(0.,0.,0.));
#260665=CARTESIAN_POINT('',(-6.5,-7.9602041944578E-16,0.));
#260666=CARTESIAN_POINT('Origin',(0.,0.,0.));
#260667=CARTESIAN_POINT('Origin',(0.,0.,-8.));
#260668=CARTESIAN_POINT('',(-6.5,-7.9602041944578E-16,-8.));
#260669=CARTESIAN_POINT('',(-6.5,-7.9602041944578E-16,-8.));
#260670=CARTESIAN_POINT('Origin',(0.,0.,-8.));
#260671=CARTESIAN_POINT('Origin',(0.,0.,-8.));
#260672=CARTESIAN_POINT('Origin',(0.,0.,20.));
#260673=CARTESIAN_POINT('',(0.,0.,0.));
#260674=CARTESIAN_POINT('Origin',(0.,0.,19.5));
#260675=CARTESIAN_POINT('',(-1.954,2.39295984553393E-16,19.046));
#260676=CARTESIAN_POINT('',(-1.76525906551972,0.00187739100781801,19.2347399361577));
#260677=CARTESIAN_POINT('',(-1.5,1.83697019872103E-16,19.5));
#260678=CARTESIAN_POINT('',(-1.91639047105473,-0.379636187408775,19.0463684911581));
#260679=CARTESIAN_POINT('Origin',(0.,0.,19.046));
#260680=CARTESIAN_POINT('',(-1.40413430885517,0.669318379170786,19.4445));
#260681=CARTESIAN_POINT('Ctrl Pts',(-1.40413430885493,0.669318379171303,
19.4445));
#260682=CARTESIAN_POINT('Ctrl Pts',(-1.38217147333919,0.721346567327714,
19.4419383467048));
#260683=CARTESIAN_POINT('Ctrl Pts',(-1.35733080539739,0.771980546116191,
19.4395076811575));
#260684=CARTESIAN_POINT('Ctrl Pts',(-1.32979496729222,0.821092768858667,
19.4371346858709));
#260685=CARTESIAN_POINT('Ctrl Pts',(-1.32816523228221,0.823999522904693,
19.4369942378671));
#260686=CARTESIAN_POINT('Ctrl Pts',(-1.32652604274719,0.826900953081449,
19.4368539918808));
#260687=CARTESIAN_POINT('Ctrl Pts',(-1.3248774314762,0.829797035270251,
19.4367139327115));
#260688=CARTESIAN_POINT('Ctrl Pts',(-1.29585145900179,0.880786376041457,
19.4342480065928));
#260689=CARTESIAN_POINT('Ctrl Pts',(-1.26390831139223,0.930115053534165,
19.4318396036553));
#260690=CARTESIAN_POINT('Ctrl Pts',(-1.22923552529087,0.977600394819607,
19.4294196905002));
#260691=CARTESIAN_POINT('Ctrl Pts',(-1.21062500144787,1.00308802288625,
19.4281208086814));
#260692=CARTESIAN_POINT('Ctrl Pts',(-1.19122789539636,1.02804396868633,
19.4268188866479));
#260693=CARTESIAN_POINT('Ctrl Pts',(-1.17107268993615,1.05243613342277,
19.42550545887));
#260694=CARTESIAN_POINT('Ctrl Pts',(-1.16329639586048,1.06184713379721,
19.4249987113368));
#260695=CARTESIAN_POINT('Ctrl Pts',(-1.15540926681824,1.07117162708454,
19.4244904029669));
#260696=CARTESIAN_POINT('Ctrl Pts',(-1.14741992670891,1.08040030926175,
19.4239805469279));
#260697=CARTESIAN_POINT('Ctrl Pts',(-1.10629043233698,1.1279099942262,19.4213557843321));
#260698=CARTESIAN_POINT('Ctrl Pts',(-1.06240353091898,1.17294124127734,
19.4186842000219));
#260699=CARTESIAN_POINT('Ctrl Pts',(-1.01605870517633,1.21527920720128,
19.4159296594468));
#260700=CARTESIAN_POINT('Ctrl Pts',(-0.969336626725759,1.25796180949049,
19.4131526965651));
#260701=CARTESIAN_POINT('Ctrl Pts',(-0.92011662502485,1.2979067796946,19.4102913361356));
#260702=CARTESIAN_POINT('Ctrl Pts',(-0.86869609931806,1.33488789533211,
19.4073422821979));
#260703=CARTESIAN_POINT('Ctrl Pts',(-0.855531220514918,1.34435594138338,
19.4065872541787));
#260704=CARTESIAN_POINT('Ctrl Pts',(-0.842222042258913,1.3536296915388,
19.4058266516426));
#260705=CARTESIAN_POINT('Ctrl Pts',(-0.828773418670833,1.36270530490215,
19.4050607762351));
#260706=CARTESIAN_POINT('Ctrl Pts',(-0.819370051506753,1.36905103419823,
19.4045252710504));
#260707=CARTESIAN_POINT('Ctrl Pts',(-0.809900124623619,1.37529870996624,
19.4039872839289));
#260708=CARTESIAN_POINT('Ctrl Pts',(-0.80037510752539,1.38144110703308,
19.4034475126238));
#260709=CARTESIAN_POINT('Ctrl Pts',(-0.746541592567262,1.41615672181531,
19.4003968318404));
#260710=CARTESIAN_POINT('Ctrl Pts',(-0.690868048765296,1.44756602956533,
19.3972819523276));
#260711=CARTESIAN_POINT('Ctrl Pts',(-0.633694512627027,1.47552898535086,
19.3941499067646));
#260712=CARTESIAN_POINT('Ctrl Pts',(-0.576880995505364,1.50331585974414,
19.3910375835424));
#260713=CARTESIAN_POINT('Ctrl Pts',(-0.518586721712705,1.52770092579246,
19.3879087670402));
#260714=CARTESIAN_POINT('Ctrl Pts',(-0.459095719137883,1.54854391708141,
19.3848352584146));
#260715=CARTESIAN_POINT('Ctrl Pts',(-0.418361167794408,1.56281548525247,
19.3827307721983));
#260716=CARTESIAN_POINT('Ctrl Pts',(-0.377064475020572,1.5754263952828,
19.3806527559442));
#260717=CARTESIAN_POINT('Ctrl Pts',(-0.33528224562359,1.58632535588287,
19.3786294936236));
#260718=CARTESIAN_POINT('Ctrl Pts',(-0.310052201624067,1.59290665275136,
19.3774077541878));
#260719=CARTESIAN_POINT('Ctrl Pts',(-0.284644882455448,1.59886359739272,
19.3762060545926));
#260720=CARTESIAN_POINT('Ctrl Pts',(-0.259075039617233,1.60418323521717,
19.3750311608205));
#260721=CARTESIAN_POINT('Ctrl Pts',(-0.248347253480673,1.60641508064797,
19.3745382360418));
#260722=CARTESIAN_POINT('Ctrl Pts',(-0.237590851597929,1.60853462095232,
19.3740500399615));
#260723=CARTESIAN_POINT('Ctrl Pts',(-0.226821249685733,1.61053844914986,
19.3735677156736));
#260724=CARTESIAN_POINT('Ctrl Pts',(-0.220750353363047,1.61166802045017,
19.3732958262603));
#260725=CARTESIAN_POINT('Ctrl Pts',(-0.214674129358586,1.61276106547953,
19.3730257502935));
#260726=CARTESIAN_POINT('Ctrl Pts',(-0.208592782959594,1.61381751167616,
19.3727575748846));
#260727=CARTESIAN_POINT('Ctrl Pts',(-0.148510985974506,1.62425486908805,
19.3701080858705));
#260728=CARTESIAN_POINT('Ctrl Pts',(-0.0879270076695866,1.63112400483074,
19.3676429980082));
#260729=CARTESIAN_POINT('Ctrl Pts',(-0.0270872981813738,1.63451635283288,
19.3652592164502));
#260730=CARTESIAN_POINT('Ctrl Pts',(0.0364354134851305,1.63805830176435,
19.3627703112623));
#260731=CARTESIAN_POINT('Ctrl Pts',(0.100237386887145,1.63780868765977,
19.3603694038062));
#260732=CARTESIAN_POINT('Ctrl Pts',(0.164005042467492,1.63382964290583,
19.3579595145087));
#260733=CARTESIAN_POINT('Ctrl Pts',(0.217259240175272,1.63050662853301,
19.3559469468529));
#260734=CARTESIAN_POINT('Ctrl Pts',(0.270488824308838,1.62458148559031,
19.3539283785832));
#260735=CARTESIAN_POINT('Ctrl Pts',(0.323492638541354,1.61607910238884,
19.3518619134404));
#260736=CARTESIAN_POINT('Ctrl Pts',(0.338458321045913,1.61367844558012,
19.3512784448414));
#260737=CARTESIAN_POINT('Ctrl Pts',(0.353405905971691,1.61107229073373,
19.3506912477853));
#260738=CARTESIAN_POINT('Ctrl Pts',(0.368330639185305,1.60826113415862,
19.350099598337));
#260739=CARTESIAN_POINT('Ctrl Pts',(0.38115751140529,1.60584512137882,19.3495911127403));
#260740=CARTESIAN_POINT('Ctrl Pts',(0.393969332268037,1.60327717012554,
19.3490792625555));
#260741=CARTESIAN_POINT('Ctrl Pts',(0.40674169518067,1.60056250715929,19.3485645196005));
#260742=CARTESIAN_POINT('Ctrl Pts',(0.470470193764487,1.58701752756673,
19.345996177634));
#260743=CARTESIAN_POINT('Ctrl Pts',(0.533333555532824,1.56979974871069,
19.3433481324206));
#260744=CARTESIAN_POINT('Ctrl Pts',(0.594966184623827,1.54907512073393,
19.3405969475373));
#260745=CARTESIAN_POINT('Ctrl Pts',(0.657354927780642,1.52809624134921,
19.3378120108958));
#260746=CARTESIAN_POINT('Ctrl Pts',(0.718482121739586,1.50352435200272,
19.334921431136));
#260747=CARTESIAN_POINT('Ctrl Pts',(0.777981910400626,1.47552326328266,
19.3319398232081));
#260748=CARTESIAN_POINT('Ctrl Pts',(0.826996029950355,1.45245681647784,
19.3294836651156));
#260749=CARTESIAN_POINT('Ctrl Pts',(0.874906109707342,1.42706346889986,
19.326966518312));
#260750=CARTESIAN_POINT('Ctrl Pts',(0.921515992464549,1.39942577748952,
19.3244152569714));
#260751=CARTESIAN_POINT('Ctrl Pts',(0.93827791171197,1.38948666749393,19.3234977683609));
#260752=CARTESIAN_POINT('Ctrl Pts',(0.954871747356156,1.3792571955302,19.3225760189452));
#260753=CARTESIAN_POINT('Ctrl Pts',(0.971288581433974,1.36874078310259,
19.3216517525399));
#260754=CARTESIAN_POINT('Ctrl Pts',(0.981502107975134,1.36219812957159,
19.3210767318376));
#260755=CARTESIAN_POINT('Ctrl Pts',(0.991648267010085,1.35554352163652,
19.3205006731938));
#260756=CARTESIAN_POINT('Ctrl Pts',(1.00170977076115,1.34878827155813,19.3199249224124));
#260757=CARTESIAN_POINT('Ctrl Pts',(1.05661188860429,1.31192722722129,19.3167832511439));
#260758=CARTESIAN_POINT('Ctrl Pts',(1.10909531883384,1.27200922248131,19.3136431788134));
#260759=CARTESIAN_POINT('Ctrl Pts',(1.158902268571,1.22924104627546,19.3105953658323));
#260760=CARTESIAN_POINT('Ctrl Pts',(1.20768794730778,1.18734981391638,19.3076100470016));
#260761=CARTESIAN_POINT('Ctrl Pts',(1.25390751013265,1.1427249055078,19.3047139013212));
#260762=CARTESIAN_POINT('Ctrl Pts',(1.29733348672402,1.09549346531942,19.3020070352522));
#260763=CARTESIAN_POINT('Ctrl Pts',(1.341120979724,1.0478688286627,19.2992776348253));
#260764=CARTESIAN_POINT('Ctrl Pts',(1.38207405852357,0.997587493706231,
19.2967407157757));
#260765=CARTESIAN_POINT('Ctrl Pts',(1.42008879260803,0.944878769103382,
19.294289571119));
#260766=CARTESIAN_POINT('Ctrl Pts',(1.42805622448871,0.933831653217788,
19.2937758406261));
#260767=CARTESIAN_POINT('Ctrl Pts',(1.43589434238337,0.922677932764241,
19.2932659152927));
#260768=CARTESIAN_POINT('Ctrl Pts',(1.44360182306019,0.911419779173646,
19.2927588812907));
#260769=CARTESIAN_POINT('Ctrl Pts',(1.44978667999563,0.902385689795456,
19.2923520125751));
#260770=CARTESIAN_POINT('Ctrl Pts',(1.45588680057798,0.893285102373578,
19.2919470432148));
#260771=CARTESIAN_POINT('Ctrl Pts',(1.46189466840029,0.884130048077785,
19.2915439825939));
#260772=CARTESIAN_POINT('Ctrl Pts',(1.49777716073971,0.829450721675864,
19.2891366693722));
#260773=CARTESIAN_POINT('Ctrl Pts',(1.53044031248222,0.772728762214373,
19.2867908163825));
#260774=CARTESIAN_POINT('Ctrl Pts',(1.55980601960137,0.714292045780207,
19.2844219792007));
#260775=CARTESIAN_POINT('Ctrl Pts',(1.58977562232586,0.654653598493742,
19.282004427702));
#260776=CARTESIAN_POINT('Ctrl Pts',(1.61630980664176,0.593228839250153,
19.2795625518933));
#260777=CARTESIAN_POINT('Ctrl Pts',(1.63929945845588,0.530374359964422,
19.2770375290792));
#260778=CARTESIAN_POINT('Ctrl Pts',(1.65454361180149,0.488696333327143,
19.2753632177286));
#260779=CARTESIAN_POINT('Ctrl Pts',(1.6682288198921,0.446389900533039,19.2736530086561));
#260780=CARTESIAN_POINT('Ctrl Pts',(1.68031976473865,0.403561252742655,
19.2718980942992));
#260781=CARTESIAN_POINT('Ctrl Pts',(1.68822718816244,0.375551510158863,
19.270750388221));
#260782=CARTESIAN_POINT('Ctrl Pts',(1.69545268369885,0.347318448255623,
19.2695836996519));
#260783=CARTESIAN_POINT('Ctrl Pts',(1.70198595783479,0.318892072697381,
19.268397171781));
#260784=CARTESIAN_POINT('Ctrl Pts',(1.70459399601933,0.307544458719828,
19.2679235180004));
#260785=CARTESIAN_POINT('Ctrl Pts',(1.70709220223344,0.296163727665992,
19.2674466196719));
#260786=CARTESIAN_POINT('Ctrl Pts',(1.70947835319687,0.284759283781793,
19.2669667949665));
#260787=CARTESIAN_POINT('Ctrl Pts',(1.72348149822569,0.217832218340065,
19.2641509400432));
#260788=CARTESIAN_POINT('Ctrl Pts',(1.73358381185407,0.15029952798712,19.2612401281409));
#260789=CARTESIAN_POINT('Ctrl Pts',(1.73978101893805,0.0825694731200911,
19.2582607222238));
#260790=CARTESIAN_POINT('Ctrl Pts',(1.74595863583035,0.0150535219194175,
19.255290734603));
#260791=CARTESIAN_POINT('Ctrl Pts',(1.74825682320413,-0.052658285708984,
19.2522529617856));
#260792=CARTESIAN_POINT('Ctrl Pts',(1.74666231828795,-0.120199700306727,
19.2492066877895));
#260793=CARTESIAN_POINT('Ctrl Pts',(1.74508290680785,-0.18710177412028,
19.2461892495414));
#260794=CARTESIAN_POINT('Ctrl Pts',(1.73968555964442,-0.253836874474994,
19.2431639318862));
#260795=CARTESIAN_POINT('Ctrl Pts',(1.7304302287371,-0.320086946822075,
19.2402146636442));
#260796=CARTESIAN_POINT('Ctrl Pts',(1.72812829181856,-0.33656431418136,
19.2394811372563));
#260797=CARTESIAN_POINT('Ctrl Pts',(1.72558751100087,-0.353011850793722,
19.238752424137));
#260798=CARTESIAN_POINT('Ctrl Pts',(1.72280683630334,-0.369424990628833,
19.2380300175898));
#260799=CARTESIAN_POINT('Ctrl Pts',(1.72042618759322,-0.383476947232057,
19.2374115359614));
#260800=CARTESIAN_POINT('Ctrl Pts',(1.71786899991573,-0.397506569820592,
19.2367975566759));
#260801=CARTESIAN_POINT('Ctrl Pts',(1.71513970148883,-0.411486473048876,
19.2361901142341));
#260802=CARTESIAN_POINT('Ctrl Pts',(1.70823937626494,-0.446831042892538,
19.2346543531164));
#260803=CARTESIAN_POINT('Ctrl Pts',(1.70023434220433,-0.48188991188231,
19.2331589061797));
#260804=CARTESIAN_POINT('Ctrl Pts',(1.69112876633472,-0.516623403070588,
19.2317194100129));
#260805=CARTESIAN_POINT('Ctrl Pts',(1.67534951013464,-0.576813847259032,
19.2292248748907));
#260806=CARTESIAN_POINT('Ctrl Pts',(1.65626626225344,-0.6360319925359,19.2268976068215));
#260807=CARTESIAN_POINT('Ctrl Pts',(1.63403606258769,-0.694112962325006,
19.2246502715508));
#260808=CARTESIAN_POINT('Ctrl Pts',(1.63285826468605,-0.697190201637802,
19.22453120349));
#260809=CARTESIAN_POINT('Ctrl Pts',(1.6316716230637,-0.700264255588732,
19.2244123598069));
#260810=CARTESIAN_POINT('Ctrl Pts',(1.63047615768359,-0.703335101765461,
19.2242937275129));
#260811=CARTESIAN_POINT('Ctrl Pts',(1.60639738687566,-0.765187333127124,
19.2219042649107));
#260812=CARTESIAN_POINT('Ctrl Pts',(1.57874194851366,-0.825734976747993,
19.2196000450605));
#260813=CARTESIAN_POINT('Ctrl Pts',(1.5476754838404,-0.884731553557858,
19.2172915759605));
#260814=CARTESIAN_POINT('Ctrl Pts',(1.53362609556929,-0.91141195710507,
19.2162476020472));
#260815=CARTESIAN_POINT('Ctrl Pts',(1.51887890613618,-0.937774530179484,
19.2152030301504));
#260816=CARTESIAN_POINT('Ctrl Pts',(1.50344875767458,-0.963793647972006,
19.2141510806274));
#260817=CARTESIAN_POINT('Ctrl Pts',(1.49369512739682,-0.980240725959191,
19.2134861274194));
#260818=CARTESIAN_POINT('Ctrl Pts',(1.48366860524787,-0.996550535912571,
19.2128182462234));
#260819=CARTESIAN_POINT('Ctrl Pts',(1.47337295255235,-1.01271628114316,
19.2121459446014));
#260820=CARTESIAN_POINT('Ctrl Pts',(1.46691247836072,-1.0228602111046,19.2117240784598));
#260821=CARTESIAN_POINT('Ctrl Pts',(1.46034546319633,-1.03294810149321,
19.2113004423879));
#260822=CARTESIAN_POINT('Ctrl Pts',(1.45368231464851,-1.04296449077561,
19.2108752975433));
#260823=CARTESIAN_POINT('Ctrl Pts',(1.4155369652389,-1.10030655155332,19.2084414183452));
#260824=CARTESIAN_POINT('Ctrl Pts',(1.37417401990408,-1.15541367197863,
19.2059507779562));
#260825=CARTESIAN_POINT('Ctrl Pts',(1.3298832499431,-1.20801974313988,19.2033639327079));
#260826=CARTESIAN_POINT('Ctrl Pts',(1.28497334126005,-1.26136119225234,
19.2007409260638));
#260827=CARTESIAN_POINT('Ctrl Pts',(1.23705341007497,-1.31213075452912,
19.1980189316072));
#260828=CARTESIAN_POINT('Ctrl Pts',(1.18641672157972,-1.36005143141289,
19.1951940455184));
#260829=CARTESIAN_POINT('Ctrl Pts',(1.1376127125647,-1.40623772866376,19.1924713997404));
#260830=CARTESIAN_POINT('Ctrl Pts',(1.08628548983792,-1.44977771216266,
19.1896534817836));
#260831=CARTESIAN_POINT('Ctrl Pts',(1.03268431088215,-1.49042618895111,
19.1867688755557));
#260832=CARTESIAN_POINT('Ctrl Pts',(1.01557153862312,-1.5034036670497,19.1858479329497));
#260833=CARTESIAN_POINT('Ctrl Pts',(0.998226853649716,-1.51608643285646,
19.1849204260313));
#260834=CARTESIAN_POINT('Ctrl Pts',(0.980657938559474,-1.52846650461766,
19.1839879272984));
#260835=CARTESIAN_POINT('Ctrl Pts',(0.971285926992347,-1.53507056497949,
19.183490492547));
#260836=CARTESIAN_POINT('Ctrl Pts',(0.961858628457918,-1.54158248085602,
19.1829920951222));
#260837=CARTESIAN_POINT('Ctrl Pts',(0.952377750096971,-1.54800136299127,
19.1824930265051));
#260838=CARTESIAN_POINT('Ctrl Pts',(0.894011222757722,-1.58751751807428,
19.1794206421777));
#260839=CARTESIAN_POINT('Ctrl Pts',(0.833616384678822,-1.62350908373234,
19.1763206322423));
#260840=CARTESIAN_POINT('Ctrl Pts',(0.771507211253566,-1.65580953440538,
19.1732738050698));
#260841=CARTESIAN_POINT('Ctrl Pts',(0.710499521310594,-1.68753714839546,
19.1702810122633));
#260842=CARTESIAN_POINT('Ctrl Pts',(0.647837989219365,-1.71570510025019,
19.1673401380913));
#260843=CARTESIAN_POINT('Ctrl Pts',(0.583758119910228,-1.74014799595924,
19.1645467615866));
#260844=CARTESIAN_POINT('Ctrl Pts',(0.556870881118297,-1.75040397776415,
19.1633746902025));
#260845=CARTESIAN_POINT('Ctrl Pts',(0.52973315938917,-1.7600039036222,19.1622287671939));
#260846=CARTESIAN_POINT('Ctrl Pts',(0.502358946186095,-1.7689339647992,
19.1611166750896));
#260847=CARTESIAN_POINT('Ctrl Pts',(0.465569379798908,-1.78093551808863,
19.1596220792086));
#260848=CARTESIAN_POINT('Ctrl Pts',(0.428352078372298,-1.79172753015431,
19.1581885667143));
#260849=CARTESIAN_POINT('Ctrl Pts',(0.390751179581378,-1.80130877931094,
19.1567963208677));
#260850=CARTESIAN_POINT('Ctrl Pts',(0.372997738975067,-1.80583261100927,
19.1561389654655));
#260851=CARTESIAN_POINT('Ctrl Pts',(0.355158831924743,-1.81008642879012,
19.155490820199));
#260852=CARTESIAN_POINT('Ctrl Pts',(0.337239394906132,-1.8140696190854,
19.1548498726756));
#260853=CARTESIAN_POINT('Ctrl Pts',(0.325750913958142,-1.81662331570947,
19.1544389494192));
#260854=CARTESIAN_POINT('Ctrl Pts',(0.314237804738062,-1.81906386364226,
19.1540312889368));
#260855=CARTESIAN_POINT('Ctrl Pts',(0.302705048111772,-1.82139090102721,
19.1536264840241));
#260856=CARTESIAN_POINT('Ctrl Pts',(0.234929258408644,-1.83506645159538,
19.1512475235102));
#260857=CARTESIAN_POINT('Ctrl Pts',(0.166434815429164,-1.84483320125462,
19.1489639169012));
#260858=CARTESIAN_POINT('Ctrl Pts',(0.0975457067868387,-1.85075006770947,
19.1466810911127));
#260859=CARTESIAN_POINT('Ctrl Pts',(0.0272216740891075,-1.85679017939388,
19.1443507152586));
#260860=CARTESIAN_POINT('Ctrl Pts',(-0.0435137040245961,-1.85881719306894,
19.1420207113177));
#260861=CARTESIAN_POINT('Ctrl Pts',(-0.114293132667689,-1.85686692883475,
19.1396189337732));
#260862=CARTESIAN_POINT('Ctrl Pts',(-0.166082490785135,-1.85543991911195,
19.1378615514411));
#260863=CARTESIAN_POINT('Ctrl Pts',(-0.217894900467354,-1.85188299001889,
19.1360663381086));
#260864=CARTESIAN_POINT('Ctrl Pts',(-0.269579462386977,-1.84620588131199,
19.1342161854245));
#260865=CARTESIAN_POINT('Ctrl Pts',(-0.295213725564894,-1.8433901759393,
19.1332985554967));
#260866=CARTESIAN_POINT('Ctrl Pts',(-0.320816455402674,-1.84005288874687,
19.1323675628624));
#260867=CARTESIAN_POINT('Ctrl Pts',(-0.346368798976254,-1.83619504657529,
19.1314220396323));
#260868=CARTESIAN_POINT('Ctrl Pts',(-0.358227790062144,-1.83440459961328,
19.1309832168087));
#260869=CARTESIAN_POINT('Ctrl Pts',(-0.370075924525137,-1.83250202697373,
19.1305412729349));
#260870=CARTESIAN_POINT('Ctrl Pts',(-0.381911299618988,-1.83048742568155,
19.1300961371357));
#260871=CARTESIAN_POINT('Ctrl Pts',(-0.393814699867741,-1.82846124524093,
19.1296484428682));
#260872=CARTESIAN_POINT('Ctrl Pts',(-0.405696656235154,-1.82632317212201,
19.1291978400046));
#260873=CARTESIAN_POINT('Ctrl Pts',(-0.417551343430059,-1.8240746132133,
19.1287444538574));
#260874=CARTESIAN_POINT('Ctrl Pts',(-0.488299309374712,-1.81065536675976,
19.1260386762039));
#260875=CARTESIAN_POINT('Ctrl Pts',(-0.558119265200875,-1.7932942644785,
19.1232290772346));
#260876=CARTESIAN_POINT('Ctrl Pts',(-0.626627057207316,-1.77214222704198,
19.1203325981202));
#260877=CARTESIAN_POINT('Ctrl Pts',(-0.695199571035156,-1.75097020650063,
19.1174333825958));
#260878=CARTESIAN_POINT('Ctrl Pts',(-0.762457421690977,-1.72600098288857,
19.1144474078632));
#260879=CARTESIAN_POINT('Ctrl Pts',(-0.828042384602747,-1.69736752390752,
19.1114262784009));
#260880=CARTESIAN_POINT('Ctrl Pts',(-0.89245263817879,-1.66924692626062,
19.1084592611746));
#260881=CARTESIAN_POINT('Ctrl Pts',(-0.955249947312068,-1.63759322616612,
19.1054587713829));
#260882=CARTESIAN_POINT('Ctrl Pts',(-1.01611693502786,-1.60250014671125,
19.1025015557688));
#260883=CARTESIAN_POINT('Ctrl Pts',(-1.03057405121755,-1.59416484466702,
19.1017991584375));
#260884=CARTESIAN_POINT('Ctrl Pts',(-1.04492234147161,-1.58563532190556,
19.101099311358));
#260885=CARTESIAN_POINT('Ctrl Pts',(-1.0591576702315,-1.57691245590169,
19.1004032364767));
#260886=CARTESIAN_POINT('Ctrl Pts',(-1.06905904189517,-1.5708452733495,
19.0999190821434));
#260887=CARTESIAN_POINT('Ctrl Pts',(-1.07890500175412,-1.56468492224003,
19.0994367911956));
#260888=CARTESIAN_POINT('Ctrl Pts',(-1.08868331635203,-1.55843892477285,
19.0989573267413));
#260889=CARTESIAN_POINT('Ctrl Pts',(-1.1485032800246,-1.5202283172244,19.0960241478228));
#260890=CARTESIAN_POINT('Ctrl Pts',(-1.20589981934606,-1.47875182222852,
19.0931906358257));
#260891=CARTESIAN_POINT('Ctrl Pts',(-1.26063694790006,-1.43414075412667,
19.0905589254817));
#260892=CARTESIAN_POINT('Ctrl Pts',(-1.31217626795552,-1.39213591796416,
19.0880809628026));
#260893=CARTESIAN_POINT('Ctrl Pts',(-1.36136390512813,-1.34734673374201,
19.0857816278819));
#260894=CARTESIAN_POINT('Ctrl Pts',(-1.40810241422692,-1.29998288058792,
19.0835689684277));
#260895=CARTESIAN_POINT('Ctrl Pts',(-1.41071415027776,-1.29733620046965,
19.0834453255778));
#260896=CARTESIAN_POINT('Ctrl Pts',(-1.41331824040473,-1.29468146749932,
19.083321953376));
#260897=CARTESIAN_POINT('Ctrl Pts',(-1.41591466796309,-1.29201871356806,
19.0831988357779));
#260898=CARTESIAN_POINT('Ctrl Pts',(-1.46597636629649,-1.24067817698608,
19.0808250063846));
#260899=CARTESIAN_POINT('Ctrl Pts',(-1.51318808537753,-1.18635991928918,
19.0785452366125));
#260900=CARTESIAN_POINT('Ctrl Pts',(-1.55736793020904,-1.12932494144644,
19.0762615319601));
#260901=CARTESIAN_POINT('Ctrl Pts',(-1.57332878905255,-1.10871990686648,
19.0754364976546));
#260902=CARTESIAN_POINT('Ctrl Pts',(-1.58889343781319,-1.08776040053795,
19.0746111510968));
#260903=CARTESIAN_POINT('Ctrl Pts',(-1.60405173792419,-1.06645922023027,
19.073781620285));
#260904=CARTESIAN_POINT('Ctrl Pts',(-1.61079267917436,-1.05698652184314,
19.07341272546));
#260905=CARTESIAN_POINT('Ctrl Pts',(-1.61744777951959,-1.04745393357941,
19.0730433076787));
#260906=CARTESIAN_POINT('Ctrl Pts',(-1.62401578653282,-1.03786400668304,
19.0726731021241));
#260907=CARTESIAN_POINT('Ctrl Pts',(-1.66505382599379,-0.977944491127087,
19.0703599940341));
#260908=CARTESIAN_POINT('Ctrl Pts',(-1.70270243524567,-0.915773144665256,
19.0680128538593));
#260909=CARTESIAN_POINT('Ctrl Pts',(-1.73682775615862,-0.851717698488315,
19.0655766511745));
#260910=CARTESIAN_POINT('Ctrl Pts',(-1.77141300513714,-0.786798937427839,
19.0631076142787));
#260911=CARTESIAN_POINT('Ctrl Pts',(-1.80237881470471,-0.719945139265139,
19.0605469389338));
#260912=CARTESIAN_POINT('Ctrl Pts',(-1.82957727414585,-0.651537475102388,
19.0578738239924));
#260913=CARTESIAN_POINT('Ctrl Pts',(-1.85665818679246,-0.583425456421352,
19.0552122617677));
#260914=CARTESIAN_POINT('Ctrl Pts',(-1.88000423467638,-0.513773421692869,
19.0524392860477));
#260915=CARTESIAN_POINT('Ctrl Pts',(-1.89946522179181,-0.442951007160264,
19.0495708873325));
#260916=CARTESIAN_POINT('Ctrl Pts',(-1.90524807804013,-0.421906039606916,
19.0487185391276));
#260917=CARTESIAN_POINT('Ctrl Pts',(-1.91068785454722,-0.400757658309688,
19.0478580070861));
#260918=CARTESIAN_POINT('Ctrl Pts',(-1.91578049784076,-0.379515351958551,
19.0469903179249));
#260919=CARTESIAN_POINT('',(-1.5555,1.90493809607371E-16,19.4445));
#260920=CARTESIAN_POINT('Origin',(0.,0.,19.4445));
#260921=CARTESIAN_POINT('',(-1.,-1.22464679914735E-16,20.));
#260922=CARTESIAN_POINT('',(-1.5,1.83697019872103E-16,19.5));
#260923=CARTESIAN_POINT('Origin',(0.,0.,20.));
#260924=CARTESIAN_POINT('',(-1.08942750315406,-1.11028283125135,19.4445));
#260925=CARTESIAN_POINT('Origin',(0.,0.,19.4445));
#260926=CARTESIAN_POINT('Ctrl Pts',(-1.76525906551972,0.00187739100781683,
19.2347399361577));
#260927=CARTESIAN_POINT('Ctrl Pts',(-1.76288673923925,-0.0135139808696315,
19.2371286301425));
#260928=CARTESIAN_POINT('Ctrl Pts',(-1.76030651728755,-0.0288864918497785,
19.2395239781913));
#260929=CARTESIAN_POINT('Ctrl Pts',(-1.7575179265608,-0.0442367894856103,
19.2419254407942));
#260930=CARTESIAN_POINT('Ctrl Pts',(-1.74580272373018,-0.108725223944406,
19.2520142721216));
#260931=CARTESIAN_POINT('Ctrl Pts',(-1.73048046950318,-0.172445835478701,
19.2621498573833));
#260932=CARTESIAN_POINT('Ctrl Pts',(-1.71163450897447,-0.235094626728941,
19.2722956920152));
#260933=CARTESIAN_POINT('Ctrl Pts',(-1.69287082259393,-0.297469917675188,
19.2823972338715));
#260934=CARTESIAN_POINT('Ctrl Pts',(-1.6706129121074,-0.358782641587655,
19.2925086605069));
#260935=CARTESIAN_POINT('Ctrl Pts',(-1.644932474297,-0.418687137158304,
19.3026191459137));
#260936=CARTESIAN_POINT('Ctrl Pts',(-1.61976488651821,-0.477395312686684,
19.3125277203252));
#260937=CARTESIAN_POINT('Ctrl Pts',(-1.59130934495902,-0.534750477092066,
19.3224352424608));
#260938=CARTESIAN_POINT('Ctrl Pts',(-1.55963814107745,-0.590386771328957,
19.3323586504096));
#260939=CARTESIAN_POINT('Ctrl Pts',(-1.54639843002514,-0.613644758694142,
19.336506994577));
#260940=CARTESIAN_POINT('Ctrl Pts',(-1.53259688928402,-0.636601914221633,
19.3406584579712));
#260941=CARTESIAN_POINT('Ctrl Pts',(-1.51823942349062,-0.659229681251031,
19.3448158049077));
#260942=CARTESIAN_POINT('Ctrl Pts',(-1.51248796700394,-0.668294137286167,
19.346481196304));
#260943=CARTESIAN_POINT('Ctrl Pts',(-1.50665198420563,-0.677298321778638,
19.3481461842204));
#260944=CARTESIAN_POINT('Ctrl Pts',(-1.5007335643467,-0.686238803116579,
19.3498106393327));
#260945=CARTESIAN_POINT('Ctrl Pts',(-1.46657740072041,-0.737835775071166,
19.3594164805062));
#260946=CARTESIAN_POINT('Ctrl Pts',(-1.42966243454859,-0.787334493623003,
19.3690067664155));
#260947=CARTESIAN_POINT('Ctrl Pts',(-1.39012993525811,-0.834466342447257,
19.3786439892553));
#260948=CARTESIAN_POINT('Ctrl Pts',(-1.35128540926912,-0.880777968563028,
19.3881134981348));
#260949=CARTESIAN_POINT('Ctrl Pts',(-1.30991393831839,-0.924804577147456,
19.3976285642955));
#260950=CARTESIAN_POINT('Ctrl Pts',(-1.26613409219736,-0.966278551040951,
19.407269709704));
#260951=CARTESIAN_POINT('Ctrl Pts',(-1.22690813773515,-1.00343848547323,
19.415908002532));
#260952=CARTESIAN_POINT('Ctrl Pts',(-1.18574947917021,-1.0385488873518,
19.4246478209494));
#260953=CARTESIAN_POINT('Ctrl Pts',(-1.14272687263894,-1.07140620588509,
19.433559460605));
#260954=CARTESIAN_POINT('Ctrl Pts',(-1.139121171214,-1.07415996001129,19.434306340313));
#260955=CARTESIAN_POINT('Ctrl Pts',(-1.13550239128299,-1.07689786122677,
19.4350544268978));
#260956=CARTESIAN_POINT('Ctrl Pts',(-1.13187058166182,-1.07961977480601,
19.435803761741));
#260957=CARTESIAN_POINT('Ctrl Pts',(-1.11791505753042,-1.09007894932254,
19.4386831418786));
#260958=CARTESIAN_POINT('Ctrl Pts',(-1.10376673475157,-1.10030239106308,
19.4415810402526));
#260959=CARTESIAN_POINT('Ctrl Pts',(-1.08942750315449,-1.11028283125093,
19.4445));
#260960=CARTESIAN_POINT('Origin',(0.,0.,-1.29405622560371));
#260961=CARTESIAN_POINT('',(1.43457668357355,0.601306900797843,0.288226974368355));
#260962=CARTESIAN_POINT('',(1.43457668357355,0.601306900797845,0.150256559003723));
#260963=CARTESIAN_POINT('',(1.43457668357355,0.601306900797845,-1.29405622560371));
#260964=CARTESIAN_POINT('',(-0.903577205789261,-1.26614710171373,4.16052298801706E-5));
#260965=CARTESIAN_POINT('Ctrl Pts',(-0.903577205789261,-1.26614710171373,
4.16052298801706E-5));
#260966=CARTESIAN_POINT('Ctrl Pts',(-0.854906687410512,-1.3008804837524,
0.00434792480590926));
#260967=CARTESIAN_POINT('Ctrl Pts',(-0.804117853215522,-1.33288363666962,
0.00865424438193803));
#260968=CARTESIAN_POINT('Ctrl Pts',(-0.751556329563241,-1.36188961868921,
0.0129605639579671));
#260969=CARTESIAN_POINT('Ctrl Pts',(-0.701486215864377,-1.38952072061988,
0.0170627644995997));
#260970=CARTESIAN_POINT('Ctrl Pts',(-0.649808186603321,-1.4144320453083,
0.0211649650412323));
#260971=CARTESIAN_POINT('Ctrl Pts',(-0.596852682617935,-1.43643556251291,
0.0252671655828649));
#260972=CARTESIAN_POINT('Ctrl Pts',(-0.543944822024556,-1.45841928343353,
0.0293656754269535));
#260973=CARTESIAN_POINT('Ctrl Pts',(-0.489762251131014,-1.47750017440538,
0.0334641852710426));
#260974=CARTESIAN_POINT('Ctrl Pts',(-0.434658662711666,-1.49353677454883,
0.0375626951151311));
#260975=CARTESIAN_POINT('Ctrl Pts',(-0.379582507432974,-1.50956539092352,
0.0416591645295442));
#260976=CARTESIAN_POINT('Ctrl Pts',(-0.323586752688759,-1.5225525717234,
0.0457556339439569));
#260977=CARTESIAN_POINT('Ctrl Pts',(-0.267041427119008,-1.53240631889922,
0.0498521033583699));
#260978=CARTESIAN_POINT('Ctrl Pts',(-0.21050153208121,-1.54225911973529,
0.0539481793537368));
#260979=CARTESIAN_POINT('Ctrl Pts',(-0.153412694621264,-1.54897899533739,
0.0580442553491035));
#260980=CARTESIAN_POINT('Ctrl Pts',(-0.0961540102568588,-1.55252525142476,
0.0621403313444704));
#260981=CARTESIAN_POINT('Ctrl Pts',(-0.0388403927829789,-1.5560749097362,
0.0662403370527458));
#260982=CARTESIAN_POINT('Ctrl Pts',(0.0186428655038344,-1.55644484119256,
0.0703403427610216));
#260983=CARTESIAN_POINT('Ctrl Pts',(0.0759143162520156,-1.55364644195132,
0.074440348469297));
#260984=CARTESIAN_POINT('Ctrl Pts',(0.133217967513464,-1.55084646932769,
0.078542659380016));
#260985=CARTESIAN_POINT('Ctrl Pts',(0.190309046039257,-1.54487467884722,
0.0826449702907347));
#260986=CARTESIAN_POINT('Ctrl Pts',(0.246812163846152,-1.53579425893496,
0.0867472812014536));
#260987=CARTESIAN_POINT('Ctrl Pts',(0.303412116575455,-1.52669827701848,
0.0908566226438342));
#260988=CARTESIAN_POINT('Ctrl Pts',(0.359421580968227,-1.51448315467192,
0.0949659640862152));
#260989=CARTESIAN_POINT('Ctrl Pts',(0.414477772298942,-1.49926262751731,
0.0990753055285958));
#260990=CARTESIAN_POINT('Ctrl Pts',(0.43376155614573,-1.49393154033911,
0.100514628703922));
#260991=CARTESIAN_POINT('Ctrl Pts',(0.452928558882729,-1.48823218964303,
0.101953951879249));
#260992=CARTESIAN_POINT('Ctrl Pts',(0.471963787350009,-1.48217085163291,
0.103393275054576));
#260993=CARTESIAN_POINT('Ctrl Pts',(0.526915051038866,-1.46467286447328,
0.107548340883011));
#260994=CARTESIAN_POINT('Ctrl Pts',(0.581002785657055,-1.44407949213653,
0.111703406711447));
#260995=CARTESIAN_POINT('Ctrl Pts',(0.633855123512789,-1.42049566433572,
0.115858472539883));
#260996=CARTESIAN_POINT('Ctrl Pts',(0.686616524499013,-1.39695241448394,
0.1200063892299));
#260997=CARTESIAN_POINT('Ctrl Pts',(0.738146278099265,-1.37042913259137,
0.124154305919917));
#260998=CARTESIAN_POINT('Ctrl Pts',(0.78808935185062,-1.34107994672192,
0.128302222609935));
#260999=CARTESIAN_POINT('Ctrl Pts',(0.837984422238826,-1.31175897016202,
0.132446152481837));
#261000=CARTESIAN_POINT('Ctrl Pts',(0.886295389703398,-1.27961773351875,
0.136590082353739));
#261001=CARTESIAN_POINT('Ctrl Pts',(0.93269042664768,-1.24485694681749,
0.140734012225641));
#261002=CARTESIAN_POINT('Ctrl Pts',(0.9790585299433,-1.21011633974919,0.144875536427485));
#261003=CARTESIAN_POINT('Ctrl Pts',(1.02351249349905,-1.17275950805182,
0.149017060629328));
#261004=CARTESIAN_POINT('Ctrl Pts',(1.06575002859973,-1.13303006426999,
0.153158584831171));
#261005=CARTESIAN_POINT('Ctrl Pts',(1.10797911960402,-1.09330856316882,
0.157299281062597));
#261006=CARTESIAN_POINT('Ctrl Pts',(1.14799228441944,-1.05121574719031,
0.161439977294023));
#261007=CARTESIAN_POINT('Ctrl Pts',(1.18552251205272,-1.00703357611165,
0.165580673525449));
#261008=CARTESIAN_POINT('Ctrl Pts',(1.22308759591479,-0.962810370806427,
0.169725215431796));
#261009=CARTESIAN_POINT('Ctrl Pts',(1.25816479723646,-0.91649432854441,
0.173869757338144));
#261010=CARTESIAN_POINT('Ctrl Pts',(1.29052691186693,-0.86840113988134,
0.178014299244492));
#261011=CARTESIAN_POINT('Ctrl Pts',(1.32290291632652,-0.820287309607535,
0.182160619989446));
#261012=CARTESIAN_POINT('Ctrl Pts',(1.35256124440086,-0.770395258639722,
0.1863069407344));
#261013=CARTESIAN_POINT('Ctrl Pts',(1.37931939623386,-0.719067627677031,
0.190453261479354));
#261014=CARTESIAN_POINT('Ctrl Pts',(1.40612981146247,-0.667639744787388,
0.194607680720901));
#261015=CARTESIAN_POINT('Ctrl Pts',(1.4300285150549,-0.614771152497881,
0.198762099962448));
#261016=CARTESIAN_POINT('Ctrl Pts',(1.45088053259173,-0.560826114001785,
0.202916519203995));
#261017=CARTESIAN_POINT('Ctrl Pts',(1.47034269628481,-0.510476685329655,
0.206794033079372));
#261018=CARTESIAN_POINT('Ctrl Pts',(1.48715117737244,-0.459190042068452,
0.210671546954749));
#261019=CARTESIAN_POINT('Ctrl Pts',(1.50123608373896,-0.407271986367974,
0.214549060830126));
#261020=CARTESIAN_POINT('Ctrl Pts',(1.51627927690493,-0.35182161130828,
0.218690386921559));
#261021=CARTESIAN_POINT('Ctrl Pts',(1.52827855468159,-0.295417015861604,
0.222831713012991));
#261022=CARTESIAN_POINT('Ctrl Pts',(1.53711874677415,-0.238424428940231,
0.226973039104424));
#261023=CARTESIAN_POINT('Ctrl Pts',(1.54594565440517,-0.181517486744757,
0.231108141882315));
#261024=CARTESIAN_POINT('Ctrl Pts',(1.55162280443562,-0.124024815736767,
0.235243244660206));
#261025=CARTESIAN_POINT('Ctrl Pts',(1.55408530296203,-0.0663258706494377,
0.239378347438097));
#261026=CARTESIAN_POINT('Ctrl Pts',(1.5565451271801,-0.00868958743533708,
0.243508959435686));
#261027=CARTESIAN_POINT('Ctrl Pts',(1.55579719833732,0.0491520062809331,
0.247639571433274));
#261028=CARTESIAN_POINT('Ctrl Pts',(1.55182832188269,0.106813432688756,
0.251770183430863));
#261029=CARTESIAN_POINT('Ctrl Pts',(1.54786212709918,0.164435898704758,
0.25589800447665));
#261030=CARTESIAN_POINT('Ctrl Pts',(1.54067933707812,0.221877918651016,
0.260025825522438));
#261031=CARTESIAN_POINT('Ctrl Pts',(1.53031882756835,0.278755333563033,
0.264153646568225));
#261032=CARTESIAN_POINT('Ctrl Pts',(1.51995666694747,0.335641812790993,
0.268282125447604));
#261033=CARTESIAN_POINT('Ctrl Pts',(1.50641585292148,0.391962989945588,
0.272410604326983));
#261034=CARTESIAN_POINT('Ctrl Pts',(1.48978676610489,0.4473428679869,0.276539083206362));
#261035=CARTESIAN_POINT('Ctrl Pts',(1.47409422634919,0.499603761649568,
0.280435046927026));
#261036=CARTESIAN_POINT('Ctrl Pts',(1.45565201597827,0.551026120008104,
0.284331010647691));
#261037=CARTESIAN_POINT('Ctrl Pts',(1.43457668357355,0.601306900797843,
0.288226974368356));
#261038=CARTESIAN_POINT('',(0.903606778650206,-1.26612599672284,0.));
#261039=CARTESIAN_POINT('Origin',(0.,0.,0.));
#261040=CARTESIAN_POINT('Ctrl Pts',(0.903606778650177,-1.26612599672286,
0.));
#261041=CARTESIAN_POINT('Ctrl Pts',(0.951853445040324,-1.23169339292967,
0.00424530167179309));
#261042=CARTESIAN_POINT('Ctrl Pts',(0.998167624735184,-1.19447231163877,
0.00849060334358664));
#261043=CARTESIAN_POINT('Ctrl Pts',(1.04222559460503,-1.15470604915286,
0.0127359050153797));
#261044=CARTESIAN_POINT('Ctrl Pts',(1.08626235513991,-1.11495892999069,
0.0169791630154963));
#261045=CARTESIAN_POINT('Ctrl Pts',(1.12804469970472,-1.07266938416111,
0.0212224210156127));
#261046=CARTESIAN_POINT('Ctrl Pts',(1.16728248039808,-1.02812054787155,
0.0254656790157293));
#261047=CARTESIAN_POINT('Ctrl Pts',(1.20651063791617,-0.98358263730848,
0.0297078963449737));
#261048=CARTESIAN_POINT('Ctrl Pts',(1.24319514989636,-0.936786900956853,
0.033950113674218));
#261049=CARTESIAN_POINT('Ctrl Pts',(1.27708449593244,-0.888051485134154,
0.0381923310034624));
#261050=CARTESIAN_POINT('Ctrl Pts',(1.31097578868278,-0.839313269790677,
0.0424347920194664));
#261051=CARTESIAN_POINT('Ctrl Pts',(1.34207131961844,-0.788635552747116,
0.0466772530354706));
#261052=CARTESIAN_POINT('Ctrl Pts',(1.37016249066737,-0.736366076872226,
0.0509197140514746));
#261053=CARTESIAN_POINT('Ctrl Pts',(1.3982637792545,-0.684077775209748,
0.055163703065772));
#261054=CARTESIAN_POINT('Ctrl Pts',(1.42335832940938,-0.630197004108925,
0.0594076920800693));
#261055=CARTESIAN_POINT('Ctrl Pts',(1.44528398878409,-0.57509515887751,
0.0636516810943668));
#261056=CARTESIAN_POINT('Ctrl Pts',(1.46724280081557,-0.519909996992712,
0.0679020872251905));
#261057=CARTESIAN_POINT('Ctrl Pts',(1.48602297562656,-0.463500527170074,
0.0721524933560141));
#261058=CARTESIAN_POINT('Ctrl Pts',(1.50151122687381,-0.406256428345346,
0.0764028994868378));
#261059=CARTESIAN_POINT('Ctrl Pts',(1.51701148192575,-0.348967963828759,
0.0806565997949225));
#261060=CARTESIAN_POINT('Ctrl Pts',(1.52921462989051,-0.290844057345651,
0.0849103001030079));
#261061=CARTESIAN_POINT('Ctrl Pts',(1.5380585220928,-0.232284809270268,
0.0891640004110927));
#261062=CARTESIAN_POINT('Ctrl Pts',(1.54692121356449,-0.173601083074211,
0.0934267427174556));
#261063=CARTESIAN_POINT('Ctrl Pts',(1.55241033518493,-0.114480651008706,
0.0976894850238181));
#261064=CARTESIAN_POINT('Ctrl Pts',(1.55451568512429,-0.0553284258095596,
0.101952227330181));
#261065=CARTESIAN_POINT('Ctrl Pts',(1.55602358171541,-0.0129623387910441,
0.105005294410597));
#261066=CARTESIAN_POINT('Ctrl Pts',(1.55579679794536,0.0294199928847578,
0.108058361491013));
#261067=CARTESIAN_POINT('Ctrl Pts',(1.55384796201767,0.0716712001681464,
0.11111142857143));
#261068=CARTESIAN_POINT('Ctrl Pts',(1.55122812972079,0.128469761735095,
0.115215685696485));
#261069=CARTESIAN_POINT('Ctrl Pts',(1.54548304431742,0.185269471839644,
0.11931994282154));
#261070=CARTESIAN_POINT('Ctrl Pts',(1.53660820824037,0.241692913359763,
0.123424199946596));
#261071=CARTESIAN_POINT('Ctrl Pts',(1.52774704327412,0.298029438218638,
0.127522134729082));
#261072=CARTESIAN_POINT('Ctrl Pts',(1.51576574869432,0.353990320940755,
0.131620069511569));
#261073=CARTESIAN_POINT('Ctrl Pts',(1.50071177189604,0.409199740582322,
0.135718004294056));
#261074=CARTESIAN_POINT('Ctrl Pts',(1.48567802726089,0.464334960163706,
0.139810431556096));
#261075=CARTESIAN_POINT('Ctrl Pts',(1.46757992691381,0.518720207923678,
0.143902858818138));
#261076=CARTESIAN_POINT('Ctrl Pts',(1.44651611159788,0.57198897619425,0.147995286080179));
#261077=CARTESIAN_POINT('Ctrl Pts',(1.44263650403733,0.581800205215399,
0.14874904372136));
#261078=CARTESIAN_POINT('Ctrl Pts',(1.43865642718691,0.591573593139283,
0.149502801362542));
#261079=CARTESIAN_POINT('Ctrl Pts',(1.43457668357355,0.601306900797845,
0.150256559003723));
#261080=CARTESIAN_POINT('Origin',(0.,0.,-1.29405622560371));
#261081=CARTESIAN_POINT('',(1.43457668375786,0.60130690035812,0.986840263175809));
#261082=CARTESIAN_POINT('',(1.43457651222227,0.601307309601495,0.849135319448151));
#261083=CARTESIAN_POINT('',(1.43457668357355,0.601306900797845,-1.29405622560371));
#261084=CARTESIAN_POINT('',(-1.55549983609988,0.000714068102024366,0.594056225567426));
#261085=CARTESIAN_POINT('Ctrl Pts',(1.43457668375786,0.601306900358119,
0.986840263175809));
#261086=CARTESIAN_POINT('Ctrl Pts',(1.44583683266777,0.574442836313328,
0.984800154295232));
#261087=CARTESIAN_POINT('Ctrl Pts',(1.45634171559164,0.547264094095289,
0.982798230949018));
#261088=CARTESIAN_POINT('Ctrl Pts',(1.5016386947571,0.419506152666243,0.973602132403835));
#261089=CARTESIAN_POINT('Ctrl Pts',(1.52681576497426,0.315818555124705,
0.966729676129621));
#261090=CARTESIAN_POINT('Ctrl Pts',(1.55200054342739,0.131306418546304,
0.954382233635514));
#261091=CARTESIAN_POINT('Ctrl Pts',(1.55669114739927,0.0515453269029813,
0.949009910860428));
#261092=CARTESIAN_POINT('Ctrl Pts',(1.55503050182964,-0.0399874426081019,
0.942614787105728));
#261093=CARTESIAN_POINT('Ctrl Pts',(1.55468331354602,-0.0517555638892538,
0.941788406907512));
#261094=CARTESIAN_POINT('Ctrl Pts',(1.55390373565351,-0.0708307180837244,
0.940441594681791));
#261095=CARTESIAN_POINT('Ctrl Pts',(1.55355328974435,-0.0781407890977374,
0.939923719208182));
#261096=CARTESIAN_POINT('Ctrl Pts',(1.55283814721328,-0.0911396245309655,
0.938999600702741));
#261097=CARTESIAN_POINT('Ctrl Pts',(1.55249373789135,-0.0968294109483699,
0.938593999056129));
#261098=CARTESIAN_POINT('Ctrl Pts',(1.55170255476728,-0.108807993407129,
0.937737712596411));
#261099=CARTESIAN_POINT('Ctrl Pts',(1.55124880613886,-0.115096208412715,
0.937286816518539));
#261100=CARTESIAN_POINT('Ctrl Pts',(1.54994702760356,-0.131727602263499,
0.93609050347328));
#261101=CARTESIAN_POINT('Ctrl Pts',(1.54903370532627,-0.142065195007226,
0.935343056035774));
#261102=CARTESIAN_POINT('Ctrl Pts',(1.54423920383262,-0.190768135507098,
0.931802825306857));
#261103=CARTESIAN_POINT('Ctrl Pts',(1.53903603749094,-0.228986438630815,
0.928969073221727));
#261104=CARTESIAN_POINT('Ctrl Pts',(1.50668529352395,-0.41468172861502,
0.91491317193785));
#261105=CARTESIAN_POINT('Ctrl Pts',(1.45972829211868,-0.557889095625831,
0.903075161689915));
#261106=CARTESIAN_POINT('Ctrl Pts',(1.37552200936693,-0.727371015370615,
0.888647490019427));
#261107=CARTESIAN_POINT('Ctrl Pts',(1.3566756322814,-0.761945713191154,
0.885686831980741));
#261108=CARTESIAN_POINT('Ctrl Pts',(1.33313924907402,-0.801476183990503,
0.882310973640917));
#261109=CARTESIAN_POINT('Ctrl Pts',(1.32970608363188,-0.807159257075366,
0.881825881744756));
#261110=CARTESIAN_POINT('Ctrl Pts',(1.32409519286424,-0.816314255253958,
0.881045032225767));
#261111=CARTESIAN_POINT('Ctrl Pts',(1.32193999950714,-0.819799781559014,
0.880747885295143));
#261112=CARTESIAN_POINT('Ctrl Pts',(1.31808609700508,-0.825977860214509,
0.880221500845305));
#261113=CARTESIAN_POINT('Ctrl Pts',(1.31639287452608,-0.828673750809956,
0.879991913156345));
#261114=CARTESIAN_POINT('Ctrl Pts',(1.31272131505667,-0.834479829133666,
0.879497697023913));
#261115=CARTESIAN_POINT('Ctrl Pts',(1.31074019856379,-0.837588185726855,
0.879233255729667));
#261116=CARTESIAN_POINT('Ctrl Pts',(1.30519091059809,-0.846227070277718,
0.878498621396459));
#261117=CARTESIAN_POINT('Ctrl Pts',(1.30159860292242,-0.851742125626637,
0.878029990405404));
#261118=CARTESIAN_POINT('Ctrl Pts',(1.2805189302889,-0.883659664339501,
0.875318910789927));
#261119=CARTESIAN_POINT('Ctrl Pts',(1.26226201999178,-0.90954828932622,
0.873124099818739));
#261120=CARTESIAN_POINT('Ctrl Pts',(1.15562739257571,-1.05135604147518,
0.861014440896718));
#261121=CARTESIAN_POINT('Ctrl Pts',(1.05208641855925,-1.15496612643482,
0.851764217583685));
#261122=CARTESIAN_POINT('Ctrl Pts',(0.896211870003822,-1.27232798631137,
0.838604529048586));
#261123=CARTESIAN_POINT('Ctrl Pts',(0.855413467858603,-1.30010814549373,
0.835225745583971));
#261124=CARTESIAN_POINT('Ctrl Pts',(0.803513894797133,-1.3319456825008,
0.830964050857422));
#261125=CARTESIAN_POINT('Ctrl Pts',(0.793593493674383,-1.33788012703242,
0.830151086826246));
#261126=CARTESIAN_POINT('Ctrl Pts',(0.77787772791332,-1.34704509766607,
0.828865282310385));
#261127=CARTESIAN_POINT('Ctrl Pts',(0.772126116221676,-1.35035014455731,
0.828395140960181));
#261128=CARTESIAN_POINT('Ctrl Pts',(0.761473707929256,-1.35638102632723,
0.827525108222961));
#261129=CARTESIAN_POINT('Ctrl Pts',(0.756578951128922,-1.35911735536161,
0.827125601815906));
#261130=CARTESIAN_POINT('Ctrl Pts',(0.74570004676794,-1.36512203917527,
0.826238212423495));
#261131=CARTESIAN_POINT('Ctrl Pts',(0.739709019438026,-1.36837761798925,
0.825749884067379));
#261132=CARTESIAN_POINT('Ctrl Pts',(0.722457791994227,-1.377605694766,0.824344634524997));
#261133=CARTESIAN_POINT('Ctrl Pts',(0.711145565991381,-1.38347919299422,
0.823424248217281));
#261134=CARTESIAN_POINT('Ctrl Pts',(0.622488371515749,-1.42813685766515,
0.816217503291865));
#261135=CARTESIAN_POINT('Ctrl Pts',(0.542115755639979,-1.46053831291564,
0.809709917775539));
#261136=CARTESIAN_POINT('Ctrl Pts',(0.377990293606597,-1.51128390508164,
0.796508520150517));
#261137=CARTESIAN_POINT('Ctrl Pts',(0.294568798929559,-1.5297334385913,
0.789841846258124));
#261138=CARTESIAN_POINT('Ctrl Pts',(0.195970410793646,-1.54317139823791,
0.782201433144978));
#261139=CARTESIAN_POINT('Ctrl Pts',(0.181857865565668,-1.54489808818141,
0.781113760269311));
#261140=CARTESIAN_POINT('Ctrl Pts',(0.130414398780697,-1.55047755945355,
0.777174362278981));
#261141=CARTESIAN_POINT('Ctrl Pts',(0.0929673423124462,-1.55317295339527,
0.774355140186107));
#261142=CARTESIAN_POINT('Ctrl Pts',(0.0489134361121352,-1.55474453976543,
0.771121280070015));
#261143=CARTESIAN_POINT('Ctrl Pts',(0.0423694202775905,-1.55493663678642,
0.770643051405062));
#261144=CARTESIAN_POINT('Ctrl Pts',(0.0317545303461609,-1.55518116985824,
0.76987101495676));
#261145=CARTESIAN_POINT('Ctrl Pts',(0.0276844110498078,-1.55525894811373,
0.769575867994204));
#261146=CARTESIAN_POINT('Ctrl Pts',(0.02043167322982,-1.55536906426782,
0.769051552171228));
#261147=CARTESIAN_POINT('Ctrl Pts',(0.0172492255206549,-1.55540761353498,
0.768822045318464));
#261148=CARTESIAN_POINT('Ctrl Pts',(0.0103578028953234,-1.55546993610137,
0.768326277651991));
#261149=CARTESIAN_POINT('Ctrl Pts',(0.0066488593930855,-1.55549021200496,
0.768060213422123));
#261150=CARTESIAN_POINT('Ctrl Pts',(-0.0037390581158609,-1.55550984474637,
0.767317056100492));
#261151=CARTESIAN_POINT('Ctrl Pts',(-0.0104181154392727,-1.55547945175207,
0.766841581495767));
#261152=CARTESIAN_POINT('Ctrl Pts',(-0.0503949996502374,-1.55504002823789,
0.764008609472395));
#261153=CARTESIAN_POINT('Ctrl Pts',(-0.0836759185716972,-1.55360480951411,
0.761703837418819));
#261154=CARTESIAN_POINT('Ctrl Pts',(-0.284293527021595,-1.53848664680285,
0.747996011796078));
#261155=CARTESIAN_POINT('Ctrl Pts',(-0.448557735259256,-1.49885642117692,
0.737430691408286));
#261156=CARTESIAN_POINT('Ctrl Pts',(-0.607948811440686,-1.43178338495197,
0.725569150060148));
#261157=CARTESIAN_POINT('Ctrl Pts',(-0.61256343664806,-1.42981518173776,
0.725224384787615));
#261158=CARTESIAN_POINT('Ctrl Pts',(-0.640236731658547,-1.4178535707448,
0.723148504670547));
#261159=CARTESIAN_POINT('Ctrl Pts',(-0.663058805574347,-1.40732537722207,
0.721401427403274));
#261160=CARTESIAN_POINT('Ctrl Pts',(-0.69388534553605,-1.39218830365224,
0.71898797335305));
#261161=CARTESIAN_POINT('Ctrl Pts',(-0.702119507105201,-1.38805379463114,
0.718337982667155));
#261162=CARTESIAN_POINT('Ctrl Pts',(-0.715162553455551,-1.38135891288846,
0.717299638859661));
#261163=CARTESIAN_POINT('Ctrl Pts',(-0.719995653991411,-1.37884595983052,
0.716912950453329));
#261164=CARTESIAN_POINT('Ctrl Pts',(-0.729785059115935,-1.37369049090167,
0.716125730075693));
#261165=CARTESIAN_POINT('Ctrl Pts',(-0.734740445846722,-1.37104641534058,
0.715725147568553));
#261166=CARTESIAN_POINT('Ctrl Pts',(-0.746102777245424,-1.36490445795701,
0.714801754036403));
#261167=CARTESIAN_POINT('Ctrl Pts',(-0.752499593381453,-1.36138822242585,
0.7142782969495));
#261168=CARTESIAN_POINT('Ctrl Pts',(-0.765896063194354,-1.3539011156939,
0.713174342222554));
#261169=CARTESIAN_POINT('Ctrl Pts',(-0.772890104387216,-1.34992069867341,
0.712593513653113));
#261170=CARTESIAN_POINT('Ctrl Pts',(-0.791411080072929,-1.33918900786861,
0.711043305278424));
#261171=CARTESIAN_POINT('Ctrl Pts',(-0.80288223880487,-1.33234334405815,
0.710070559185372));
#261172=CARTESIAN_POINT('Ctrl Pts',(-0.8377042366089,-1.31094955358406,
0.707078210080837));
#261173=CARTESIAN_POINT('Ctrl Pts',(-0.860757373378667,-1.29592966307172,
0.705041934049246));
#261174=CARTESIAN_POINT('Ctrl Pts',(-1.00693362455144,-1.19506954839168,
0.691764309725466));
#261175=CARTESIAN_POINT('Ctrl Pts',(-1.11745434185532,-1.09242339138263,
0.679900215287483));
#261176=CARTESIAN_POINT('Ctrl Pts',(-1.23408884375215,-0.947573631162822,
0.66575961475814));
#261177=CARTESIAN_POINT('Ctrl Pts',(-1.25564760575025,-0.918814812967962,
0.663063603983283));
#261178=CARTESIAN_POINT('Ctrl Pts',(-1.27989063175237,-0.884026046909663,
0.659953526457898));
#261179=CARTESIAN_POINT('Ctrl Pts',(-1.28355537936585,-0.878696576104198,
0.659481133277693));
#261180=CARTESIAN_POINT('Ctrl Pts',(-1.28945899758859,-0.869995471623355,
0.658716649011529));
#261181=CARTESIAN_POINT('Ctrl Pts',(-1.29171808997526,-0.866637758319201,
0.658423260080281));
#261182=CARTESIAN_POINT('Ctrl Pts',(-1.29572802539076,-0.860627234249489,
0.657901016846207));
#261183=CARTESIAN_POINT('Ctrl Pts',(-1.29748386336071,-0.857977841859926,
0.657671832800638));
#261184=CARTESIAN_POINT('Ctrl Pts',(-1.30127644662579,-0.852216925735819,
0.657175698681653));
#261185=CARTESIAN_POINT('Ctrl Pts',(-1.30331015654204,-0.849103477612566,
0.656908950816116));
#261186=CARTESIAN_POINT('Ctrl Pts',(-1.30900020576421,-0.840323856965594,
0.656160542682049));
#261187=CARTESIAN_POINT('Ctrl Pts',(-1.31263095339804,-0.834641065297778,
0.65568054488375));
#261188=CARTESIAN_POINT('Ctrl Pts',(-1.33468636739009,-0.799620356293605,
0.652748375330769));
#261189=CARTESIAN_POINT('Ctrl Pts',(-1.3521653760523,-0.769694534397481,
0.650353475751293));
#261190=CARTESIAN_POINT('Ctrl Pts',(-1.44293941695222,-0.601627629744189,
0.637358374259133));
#261191=CARTESIAN_POINT('Ctrl Pts',(-1.49608206256403,-0.453626562026999,
0.627473876281463));
#261192=CARTESIAN_POINT('Ctrl Pts',(-1.53302315291613,-0.265796578912042,
0.61444331740302));
#261193=CARTESIAN_POINT('Ctrl Pts',(-1.53862046399076,-0.231202424336528,
0.612029060712096));
#261194=CARTESIAN_POINT('Ctrl Pts',(-1.5444090236771,-0.185735557307904,
0.608822535556316));
#261195=CARTESIAN_POINT('Ctrl Pts',(-1.54566155104945,-0.175006539541205,
0.608063484638057));
#261196=CARTESIAN_POINT('Ctrl Pts',(-1.54754357025943,-0.157284558829741,
0.606805336392547));
#261197=CARTESIAN_POINT('Ctrl Pts',(-1.54823765337242,-0.150298702760661,
0.606308269918999));
#261198=CARTESIAN_POINT('Ctrl Pts',(-1.54937570252006,-0.137998617920497,
0.605431010400524));
#261199=CARTESIAN_POINT('Ctrl Pts',(-1.54983967763059,-0.132686315988006,
0.605051451799069));
#261200=CARTESIAN_POINT('Ctrl Pts',(-1.55071152669844,-0.122074806719921,
0.604291869365344));
#261201=CARTESIAN_POINT('Ctrl Pts',(-1.55111957480982,-0.116775685896486,
0.603911856346569));
#261202=CARTESIAN_POINT('Ctrl Pts',(-1.55194821440675,-0.105242706461097,
0.603083235705015));
#261203=CARTESIAN_POINT('Ctrl Pts',(-1.55235841796768,-0.0990082194109238,
0.602634308592144));
#261204=CARTESIAN_POINT('Ctrl Pts',(-1.55350212664309,-0.0798657920501435,
0.601252778639819));
#261205=CARTESIAN_POINT('Ctrl Pts',(-1.55411225540398,-0.0669513333700773,
0.600316343869313));
#261206=CARTESIAN_POINT('Ctrl Pts',(-1.55519646398222,-0.0357569299454874,
0.598043315606796));
#261207=CARTESIAN_POINT('Ctrl Pts',(-1.5555093069421,-0.0174738240725086,
0.596701878951661));
#261208=CARTESIAN_POINT('Ctrl Pts',(-1.55549978924273,0.000809731943940699,
0.595350860080746));
#261209=CARTESIAN_POINT('Ctrl Pts',(1.43457668357355,0.601306900797843,
0.288226974368356));
#261210=CARTESIAN_POINT('Ctrl Pts',(1.4122238834107,0.65463541887017,0.292359089431473));
#261211=CARTESIAN_POINT('Ctrl Pts',(1.38690886232638,0.706679132697199,
0.29649120449459));
#261212=CARTESIAN_POINT('Ctrl Pts',(1.35881626030268,0.757098818343448,
0.300623319557707));
#261213=CARTESIAN_POINT('Ctrl Pts',(1.33039637739596,0.808105897041636,
0.304803574065702));
#261214=CARTESIAN_POINT('Ctrl Pts',(1.29913405570535,0.857450390029285,
0.308983828573697));
#261215=CARTESIAN_POINT('Ctrl Pts',(1.26526508811455,0.904811862653489,
0.313164083081692));
#261216=CARTESIAN_POINT('Ctrl Pts',(1.23139612052375,0.952173335277694,
0.317344337589686));
#261217=CARTESIAN_POINT('Ctrl Pts',(1.1949209015692,0.997551404037723,0.321524592097681));
#261218=CARTESIAN_POINT('Ctrl Pts',(1.15611469137679,1.04066280340116,0.325704846605676));
#261219=CARTESIAN_POINT('Ctrl Pts',(1.11759806302803,1.08345249450068,0.329853906987747));
#261220=CARTESIAN_POINT('Ctrl Pts',(1.07662202823306,1.12419052654482,0.334002967369818));
#261221=CARTESIAN_POINT('Ctrl Pts',(1.03343365835562,1.16258123319522,0.338152027751889));
#261222=CARTESIAN_POINT('Ctrl Pts',(0.990322062582344,1.20090369434065,
0.3422937125281));
#261223=CARTESIAN_POINT('Ctrl Pts',(0.94500632367177,1.23688676954466,0.346435397304311));
#261224=CARTESIAN_POINT('Ctrl Pts',(0.897771534387028,1.2702702555143,0.350577082080523));
#261225=CARTESIAN_POINT('Ctrl Pts',(0.850583732070946,1.30362053314676,
0.354714646901596));
#261226=CARTESIAN_POINT('Ctrl Pts',(0.801481084624065,1.33437604625786,
0.35885221172267));
#261227=CARTESIAN_POINT('Ctrl Pts',(0.750781715163885,1.36231680095915,
0.362989776543744));
#261228=CARTESIAN_POINT('Ctrl Pts',(0.70011331515327,1.39024048819387,0.367124813954588));
#261229=CARTESIAN_POINT('Ctrl Pts',(0.647850581517572,1.41535257465031,
0.371259851365431));
#261230=CARTESIAN_POINT('Ctrl Pts',(0.594338702158597,1.43747756751764,
0.375394888776275));
#261231=CARTESIAN_POINT('Ctrl Pts',(0.540838967678637,1.45959753896983,
0.379528987712714));
#261232=CARTESIAN_POINT('Ctrl Pts',(0.486091131091245,1.47873156394323,
0.383663086649154));
#261233=CARTESIAN_POINT('Ctrl Pts',(0.430460919615824,1.49475203518293,
0.387797185585594));
#261234=CARTESIAN_POINT('Ctrl Pts',(0.374780584803872,1.51078694101581,
0.39193500938352));
#261235=CARTESIAN_POINT('Ctrl Pts',(0.318216787375974,1.52370254132316,
0.396072833181446));
#261236=CARTESIAN_POINT('Ctrl Pts',(0.261149698318672,1.53342136579222,
0.400210656979373));
#261237=CARTESIAN_POINT('Ctrl Pts',(0.204059136497248,1.54314418779607,
0.40435018274184));
#261238=CARTESIAN_POINT('Ctrl Pts',(0.146465388528611,1.54966755249864,
0.408489708504307));
#261239=CARTESIAN_POINT('Ctrl Pts',(0.0887548629313491,1.55296581556261,
0.412629234266774));
#261240=CARTESIAN_POINT('Ctrl Pts',(0.0309320153197847,1.55627049803703,
0.416776816789547));
#261241=CARTESIAN_POINT('Ctrl Pts',(-0.0270075416867453,1.55633753304818,
0.420924399312321));
#261242=CARTESIAN_POINT('Ctrl Pts',(-0.0846771964969704,1.55319349161443,
0.425071981835094));
#261243=CARTESIAN_POINT('Ctrl Pts',(-0.139315241988193,1.55021472783564,
0.429001532017137));
#261244=CARTESIAN_POINT('Ctrl Pts',(-0.193710669010352,1.54435410883403,
0.43293108219918));
#261245=CARTESIAN_POINT('Ctrl Pts',(-0.247542712744338,1.53567667670222,
0.436860632381223));
#261246=CARTESIAN_POINT('Ctrl Pts',(-0.304376617262698,1.5265153609684,
0.441009307860645));
#261247=CARTESIAN_POINT('Ctrl Pts',(-0.360820124387077,1.51417557510158,
0.445157983340067));
#261248=CARTESIAN_POINT('Ctrl Pts',(-0.41649089269227,1.49870463611227,
0.449306658819489));
#261249=CARTESIAN_POINT('Ctrl Pts',(-0.472063006489406,1.48326111326829,
0.453447982405791));
#261250=CARTESIAN_POINT('Ctrl Pts',(-0.52686460200474,1.46469758906535,
0.457589305992092));
#261251=CARTESIAN_POINT('Ctrl Pts',(-0.58052252409489,1.44311255590772,
0.461730629578393));
#261252=CARTESIAN_POINT('Ctrl Pts',(-0.634127255235985,1.42154891993347,
0.465867847882132));
#261253=CARTESIAN_POINT('Ctrl Pts',(-0.686590078628672,1.39696990278649,
0.470005066185871));
#261254=CARTESIAN_POINT('Ctrl Pts',(-0.737553723513263,1.36952355033848,
0.47414228448961));
#261255=CARTESIAN_POINT('Ctrl Pts',(-0.78848642321298,1.34209386334783,
0.478276990669548));
#261256=CARTESIAN_POINT('Ctrl Pts',(-0.837921291451408,1.31180053869827,
0.482411696849487));
#261257=CARTESIAN_POINT('Ctrl Pts',(-0.885523783309722,1.27883848831384,
0.486546403029425));
#261258=CARTESIAN_POINT('Ctrl Pts',(-0.93311565385724,1.24588379259023,
0.49068018665263));
#261259=CARTESIAN_POINT('Ctrl Pts',(-0.978875531894772,1.21026184954031,
0.494813970275835));
#261260=CARTESIAN_POINT('Ctrl Pts',(-1.02249798073055,1.17221078710356,
0.49894775389904));
#261261=CARTESIAN_POINT('Ctrl Pts',(-1.06616003071023,1.13412518131496,
0.503085290235915));
#261262=CARTESIAN_POINT('Ctrl Pts',(-1.10768037977828,1.09360639149896,
0.50722282657279));
#261263=CARTESIAN_POINT('Ctrl Pts',(-1.14678789423033,1.05093186061075,
0.511360362909665));
#261264=CARTESIAN_POINT('Ctrl Pts',(-1.18591163465964,1.00823962376557,
0.515499615938882));
#261265=CARTESIAN_POINT('Ctrl Pts',(-1.22262021326341,0.963390265701144,
0.519638868968098));
#261266=CARTESIAN_POINT('Ctrl Pts',(-1.25668267034715,0.916694559844863,
0.523778121997314));
#261267=CARTESIAN_POINT('Ctrl Pts',(-1.29081166554661,0.869907637894784,
0.527925460705623));
#261268=CARTESIAN_POINT('Ctrl Pts',(-1.32228392475959,0.821267598677886,
0.532072799413932));
#261269=CARTESIAN_POINT('Ctrl Pts',(-1.35091225879012,0.771113687500481,
0.536220138122241));
#261270=CARTESIAN_POINT('Ctrl Pts',(-1.37805479274566,0.723562745986234,
0.540152231467085));
#261271=CARTESIAN_POINT('Ctrl Pts',(-1.40264115933879,0.674651551227338,
0.544084324811929));
#261272=CARTESIAN_POINT('Ctrl Pts',(-1.42455194944463,0.624685515546427,
0.548016418156773));
#261273=CARTESIAN_POINT('Ctrl Pts',(-1.44997193394591,0.566717005672345,
0.552578268797517));
#261274=CARTESIAN_POINT('Ctrl Pts',(-1.47188282144215,0.507119559173282,
0.557140119438261));
#261275=CARTESIAN_POINT('Ctrl Pts',(-1.49009537948839,0.446313802192301,
0.561701970079005));
#261276=CARTESIAN_POINT('Ctrl Pts',(-1.50824984121549,0.385702009763373,
0.566249268852294));
#261277=CARTESIAN_POINT('Ctrl Pts',(-1.52272935208436,0.323889902948767,
0.570796567625584));
#261278=CARTESIAN_POINT('Ctrl Pts',(-1.53339289085846,0.261316842673301,
0.575343866398873));
#261279=CARTESIAN_POINT('Ctrl Pts',(-1.54400289564074,0.199057916923692,
0.579868336441431));
#261280=CARTESIAN_POINT('Ctrl Pts',(-1.5508350072412,0.136045979691595,
0.584392806483988));
#261281=CARTESIAN_POINT('Ctrl Pts',(-1.55379868266219,0.0727317245584089,
0.588917276526546));
#261282=CARTESIAN_POINT('Ctrl Pts',(-1.55492074239655,0.048760686504574,
0.590630259540173));
#261283=CARTESIAN_POINT('Ctrl Pts',(-1.5554888037788,0.0247464728286803,
0.5923432425538));
#261284=CARTESIAN_POINT('Ctrl Pts',(-1.55549983609988,0.000714068102024366,
0.594056225567427));
#261285=CARTESIAN_POINT('',(-1.55549967037724,0.00101264816652329,0.455943774396293));
#261286=CARTESIAN_POINT('Ctrl Pts',(1.43457668357355,0.601306900797845,
0.150256559003723));
#261287=CARTESIAN_POINT('Ctrl Pts',(1.41244477849698,0.654108415205522,
0.154345564134033));
#261288=CARTESIAN_POINT('Ctrl Pts',(1.38737593218696,0.70572879733375,0.158434569264343));
#261289=CARTESIAN_POINT('Ctrl Pts',(1.3595270376115,0.755821727660225,0.162523574394653));
#261290=CARTESIAN_POINT('Ctrl Pts',(1.33168522965499,0.805901910999285,
0.166611539008934));
#261291=CARTESIAN_POINT('Ctrl Pts',(1.30106503569729,0.854454947945978,
0.170699503623215));
#261292=CARTESIAN_POINT('Ctrl Pts',(1.26786928821999,0.901159096934901,
0.174787468237496));
#261293=CARTESIAN_POINT('Ctrl Pts',(1.23464388225231,0.947904973393733,
0.178879085212951));
#261294=CARTESIAN_POINT('Ctrl Pts',(1.1988386337529,0.992798225217377,0.182970702188406));
#261295=CARTESIAN_POINT('Ctrl Pts',(1.1606988486626,1.03554740727468,0.187062319163861));
#261296=CARTESIAN_POINT('Ctrl Pts',(1.12254294605259,1.07831465474014,0.191155665218731));
#261297=CARTESIAN_POINT('Ctrl Pts',(1.08205091879801,1.11893564946202,0.195249011273601));
#261298=CARTESIAN_POINT('Ctrl Pts',(1.03950505573736,1.15715577563977,0.199342357328471));
#261299=CARTESIAN_POINT('Ctrl Pts',(0.996876335681916,1.19545033454887,
0.203443675071499));
#261300=CARTESIAN_POINT('Ctrl Pts',(0.952186207559337,1.231334351474,0.207544992814528));
#261301=CARTESIAN_POINT('Ctrl Pts',(0.905749257284517,1.2645942167069,0.211646310557557));
#261302=CARTESIAN_POINT('Ctrl Pts',(0.865831796715821,1.29318458173082,
0.215171826085992));
#261303=CARTESIAN_POINT('Ctrl Pts',(0.824624245025244,1.31983651539173,
0.218697341614427));
#261304=CARTESIAN_POINT('Ctrl Pts',(0.782340582356172,1.34444169200401,
0.222222857142862));
#261305=CARTESIAN_POINT('Ctrl Pts',(0.732513694933871,1.3734363269925,0.226377309577972));
#261306=CARTESIAN_POINT('Ctrl Pts',(0.680970078865944,1.39971700644518,
0.230531762013082));
#261307=CARTESIAN_POINT('Ctrl Pts',(0.62803644998017,1.42307781498283,0.234686214448193));
#261308=CARTESIAN_POINT('Ctrl Pts',(0.57519685881554,1.44639712254567,0.23883328640991));
#261309=CARTESIAN_POINT('Ctrl Pts',(0.520972627697919,1.46680664842633,
0.242980358371627));
#261310=CARTESIAN_POINT('Ctrl Pts',(0.465715749510109,1.48414591285973,
0.247127430333344));
#261311=CARTESIAN_POINT('Ctrl Pts',(0.410513858184165,1.50146792275814,
0.251270375488036));
#261312=CARTESIAN_POINT('Ctrl Pts',(0.354281848696871,1.51572557079087,
0.255413320642728));
#261313=CARTESIAN_POINT('Ctrl Pts',(0.297390804141844,1.5268067852914,0.25955626579742));
#261314=CARTESIAN_POINT('Ctrl Pts',(0.240534695323457,1.53788119502338,
0.263696666846234));
#261315=CARTESIAN_POINT('Ctrl Pts',(0.183020862092417,1.5457829393312,0.267837067895047));
#261316=CARTESIAN_POINT('Ctrl Pts',(0.125232503307728,1.55045060228157,
0.271977468943861));
#261317=CARTESIAN_POINT('Ctrl Pts',(0.067457613491804,1.55511717732068,
0.276116904972495));
#261318=CARTESIAN_POINT('Ctrl Pts',(0.00940884214340416,1.55655112581271,
0.28025634100113));
#261319=CARTESIAN_POINT('Ctrl Pts',(-0.0485257237120171,1.5547429061225,
0.284395777029764));
#261320=CARTESIAN_POINT('Ctrl Pts',(-0.106511142221802,1.55293309924906,
0.28853884649047));
#261321=CARTESIAN_POINT('Ctrl Pts',(-0.164381634955927,1.54787545179417,
0.292681915951174));
#261322=CARTESIAN_POINT('Ctrl Pts',(-0.221750711946079,1.53961257196459,
0.29682498541188));
#261323=CARTESIAN_POINT('Ctrl Pts',(-0.279142820729782,1.53134637486109,
0.30096971817842));
#261324=CARTESIAN_POINT('Ctrl Pts',(-0.336032602252372,1.51987248074845,
0.305114450944961));
#261325=CARTESIAN_POINT('Ctrl Pts',(-0.392043455057559,1.50528475025376,
0.309259183711501));
#261326=CARTESIAN_POINT('Ctrl Pts',(-0.448161169267607,1.49066918827113,
0.3134118240878));
#261327=CARTESIAN_POINT('Ctrl Pts',(-0.503396107270761,1.47292807543389,
0.317564464464097));
#261328=CARTESIAN_POINT('Ctrl Pts',(-0.557387425489713,1.45220505022739,
0.321717104840396));
#261329=CARTESIAN_POINT('Ctrl Pts',(-0.607735063982491,1.43288054740007,
0.325589498465025));
#261330=CARTESIAN_POINT('Ctrl Pts',(-0.65700115741559,1.41096367186595,
0.329461892089654));
#261331=CARTESIAN_POINT('Ctrl Pts',(-0.704912530853615,1.3866068562666,
0.333334285714283));
#261332=CARTESIAN_POINT('Ctrl Pts',(-0.756323677456407,1.36047085289833,
0.33748954535419));
#261333=CARTESIAN_POINT('Ctrl Pts',(-0.806382918185656,1.33141907534589,
0.341644804994096));
#261334=CARTESIAN_POINT('Ctrl Pts',(-0.854740172399903,1.29961513060051,
0.345800064634003));
#261335=CARTESIAN_POINT('Ctrl Pts',(-0.903014298954577,1.26786585784872,
0.349948181250295));
#261336=CARTESIAN_POINT('Ctrl Pts',(-0.949591816794133,1.23337409208899,
0.354096297866587));
#261337=CARTESIAN_POINT('Ctrl Pts',(-0.994147203454296,1.19634927502966,
0.35824441448288));
#261338=CARTESIAN_POINT('Ctrl Pts',(-1.03865980786,1.15936000934277,0.362388548061566));
#261339=CARTESIAN_POINT('Ctrl Pts',(-1.08115373165124,1.11984284205106,
0.366532681640253));
#261340=CARTESIAN_POINT('Ctrl Pts',(-1.12133387389361,1.0780494391533,0.370676815218939));
#261341=CARTESIAN_POINT('Ctrl Pts',(-1.16149072443867,1.03628026313071,
0.374818546518798));
#261342=CARTESIAN_POINT('Ctrl Pts',(-1.19933609381815,0.992237840738684,
0.378960277818658));
#261343=CARTESIAN_POINT('Ctrl Pts',(-1.2346109588276,0.946211408905432,
0.383102009118517));
#261344=CARTESIAN_POINT('Ctrl Pts',(-1.26987879766862,0.900194144774516,
0.38724291545415));
#261345=CARTESIAN_POINT('Ctrl Pts',(-1.30257683354686,0.852194067482814,
0.391383821789783));
#261346=CARTESIAN_POINT('Ctrl Pts',(-1.33248704857027,0.802532563446794,
0.395524728125416));
#261347=CARTESIAN_POINT('Ctrl Pts',(-1.36242502786447,0.752824960930891,
0.399669478273095));
#261348=CARTESIAN_POINT('Ctrl Pts',(-1.38956974624266,0.701453294866358,
0.403814228420773));
#261349=CARTESIAN_POINT('Ctrl Pts',(-1.4137479156562,0.648765813662959,
0.407958978568452));
#261350=CARTESIAN_POINT('Ctrl Pts',(-1.4379364745439,0.596055692398786,
0.412105509734944));
#261351=CARTESIAN_POINT('Ctrl Pts',(-1.45915575217786,0.542029112222462,
0.416252040901436));
#261352=CARTESIAN_POINT('Ctrl Pts',(-1.47728092802937,0.487053703076643,
0.420398572067927));
#261353=CARTESIAN_POINT('Ctrl Pts',(-1.49544144876342,0.431971089488012,
0.424553189150835));
#261354=CARTESIAN_POINT('Ctrl Pts',(-1.51049567417953,0.375936451861113,
0.428707806233743));
#261355=CARTESIAN_POINT('Ctrl Pts',(-1.52236917594838,0.319331085430567,
0.432862423316651));
#261356=CARTESIAN_POINT('Ctrl Pts',(-1.53340382511625,0.266724839039212,
0.43672352030634));
#261357=CARTESIAN_POINT('Ctrl Pts',(-1.54169180343469,0.213626099992122,
0.440584617296028));
#261358=CARTESIAN_POINT('Ctrl Pts',(-1.54721364558081,0.160343958191551,
0.444445714285717));
#261359=CARTESIAN_POINT('Ctrl Pts',(-1.55269485753403,0.107453871006541,
0.448278400989242));
#261360=CARTESIAN_POINT('Ctrl Pts',(-1.55546499597033,0.0542750055122627,
0.452111087692767));
#261361=CARTESIAN_POINT('Ctrl Pts',(-1.55549967037724,0.00101264816652329,
0.455943774396293));
#261362=CARTESIAN_POINT('Ctrl Pts',(-1.55549962174471,0.001084782031638,
0.45701111646594));
#261363=CARTESIAN_POINT('Ctrl Pts',(-1.55556478756272,-0.092358326631673,
0.463326330326788));
#261364=CARTESIAN_POINT('Ctrl Pts',(-1.54720985703089,-0.185626612070271,
0.469388769574297));
#261365=CARTESIAN_POINT('Ctrl Pts',(-1.51615471673349,-0.356853835541594,
0.480887140309857));
#261366=CARTESIAN_POINT('Ctrl Pts',(-1.495645018522,-0.434871419763208,
0.486275595113444));
#261367=CARTESIAN_POINT('Ctrl Pts',(-1.4632104215784,-0.528135211178076,
0.493126909322226));
#261368=CARTESIAN_POINT('Ctrl Pts',(-1.45693067234935,-0.545219686314061,
0.494399037463768));
#261369=CARTESIAN_POINT('Ctrl Pts',(-1.44750248897834,-0.569542790921271,
0.496236682839665));
#261370=CARTESIAN_POINT('Ctrl Pts',(-1.44459632749319,-0.57687424343297,
0.496794078538821));
#261371=CARTESIAN_POINT('Ctrl Pts',(-1.43945269032168,-0.589567600206732,
0.497765371087175));
#261372=CARTESIAN_POINT('Ctrl Pts',(-1.43724067089907,-0.59493970712838,
0.498178399808053));
#261373=CARTESIAN_POINT('Ctrl Pts',(-1.43292091393862,-0.605265966163441,
0.498976163203582));
#261374=CARTESIAN_POINT('Ctrl Pts',(-1.43081744478663,-0.61022182338937,
0.499360747493974));
#261375=CARTESIAN_POINT('Ctrl Pts',(-1.42577821069415,-0.621925148668543,
0.50027307258386));
#261376=CARTESIAN_POINT('Ctrl Pts',(-1.42282023327047,-0.628662848399482,
0.500801568303666));
#261377=CARTESIAN_POINT('Ctrl Pts',(-1.41222960331019,-0.652328607565677,
0.502669591634947));
#261378=CARTESIAN_POINT('Ctrl Pts',(-1.40434202246575,-0.66914011446761,
0.504017847988341));
#261379=CARTESIAN_POINT('Ctrl Pts',(-1.34593810188269,-0.788038167100328,
0.513710469081188));
#261380=CARTESIAN_POINT('Ctrl Pts',(-1.28465389742191,-0.884425076127365,
0.522442806288046));
#261381=CARTESIAN_POINT('Ctrl Pts',(-1.17148338845351,-1.02552364289129,
0.536476917782565));
#261382=CARTESIAN_POINT('Ctrl Pts',(-1.12621258351813,-1.07504335234977,
0.541688821325403));
#261383=CARTESIAN_POINT('Ctrl Pts',(-1.06111819536346,-1.13760684771389,
0.548547534586683));
#261384=CARTESIAN_POINT('Ctrl Pts',(-1.04398946837079,-1.15334612585476,
0.550298708421727));
#261385=CARTESIAN_POINT('Ctrl Pts',(-1.01902861948883,-1.17527024941115,
0.552768101193112));
#261386=CARTESIAN_POINT('Ctrl Pts',(-1.01148081493563,-1.18177242329834,
0.553504419840321));
#261387=CARTESIAN_POINT('Ctrl Pts',(-0.999688535024922,-1.19173531451974,
0.554638156960422));
#261388=CARTESIAN_POINT('Ctrl Pts',(-0.995487539136939,-1.19524674804193,
0.555038831952612));
#261389=CARTESIAN_POINT('Ctrl Pts',(-0.987610576480531,-1.2017604267163,
0.555783986126916));
#261390=CARTESIAN_POINT('Ctrl Pts',(-0.983939256244129,-1.20476815845657,
0.556128837487998));
#261391=CARTESIAN_POINT('Ctrl Pts',(-0.977722779393625,-1.20981364090498,
0.556708554006494));
#261392=CARTESIAN_POINT('Ctrl Pts',(-0.975184902858981,-1.2118602580989,
0.556944050584216));
#261393=CARTESIAN_POINT('Ctrl Pts',(-0.970292107171644,-1.21578062688915,
0.557395792764991));
#261394=CARTESIAN_POINT('Ctrl Pts',(-0.96793818281847,-1.21765552625629,
0.55761212507198));
#261395=CARTESIAN_POINT('Ctrl Pts',(-0.961754672744856,-1.22255142679077,
0.558177834815716));
#261396=CARTESIAN_POINT('Ctrl Pts',(-0.957916250883631,-1.2255612998578,
0.5585264273765));
#261397=CARTESIAN_POINT('Ctrl Pts',(-0.944540132935304,-1.23594885892021,
0.559732555535832));
#261398=CARTESIAN_POINT('Ctrl Pts',(-0.934930539456697,-1.24323390985299,
0.560583894509932));
#261399=CARTESIAN_POINT('Ctrl Pts',(-0.845670155910563,-1.30928201112414,
0.568363473303099));
#261400=CARTESIAN_POINT('Ctrl Pts',(-0.760652362002066,-1.36043801285723,
0.574852016429284));
#261401=CARTESIAN_POINT('Ctrl Pts',(-0.5663806517194,-1.45338589709508,
0.58902664040184));
#261402=CARTESIAN_POINT('Ctrl Pts',(-0.456139335157796,-1.49165982425734,
0.596697567974007));
#261403=CARTESIAN_POINT('Ctrl Pts',(-0.329632462533139,-1.52023069026283,
0.60575448640276));
#261404=CARTESIAN_POINT('Ctrl Pts',(-0.316557342524543,-1.52300700633236,
0.606692991139996));
#261405=CARTESIAN_POINT('Ctrl Pts',(-0.29657088110863,-1.52698236214167,
0.608132008131028));
#261406=CARTESIAN_POINT('Ctrl Pts',(-0.289684276929093,-1.5283037782484,
0.608628637152534));
#261407=CARTESIAN_POINT('Ctrl Pts',(-0.277131991510636,-1.53062444960719,
0.609535405835375));
#261408=CARTESIAN_POINT('Ctrl Pts',(-0.271469220883094,-1.53163892838432,
0.609945055743816));
#261409=CARTESIAN_POINT('Ctrl Pts',(-0.259214779273337,-1.53376420336377,
0.61083286000168));
#261410=CARTESIAN_POINT('Ctrl Pts',(-0.252621338661832,-1.53486396465486,
0.611311354156501));
#261411=CARTESIAN_POINT('Ctrl Pts',(-0.234653516730676,-1.53774201824591,
0.612617632606351));
#261412=CARTESIAN_POINT('Ctrl Pts',(-0.223266352886277,-1.53943655603616,
0.613448031172105));
#261413=CARTESIAN_POINT('Ctrl Pts',(-0.165196978701336,-1.547420099724,
0.617696485776978));
#261414=CARTESIAN_POINT('Ctrl Pts',(-0.118269986974262,-1.55171207053808,
0.621176149199674));
#261415=CARTESIAN_POINT('Ctrl Pts',(0.0776121458416323,-1.56069074976918,
0.635906204788179));
#261416=CARTESIAN_POINT('Ctrl Pts',(0.226628083829469,-1.54609452974489,
0.647699001427363));
#261417=CARTESIAN_POINT('Ctrl Pts',(0.400224041998137,-1.50342586392974,
0.661210471652759));
#261418=CARTESIAN_POINT('Ctrl Pts',(0.42896008176016,-1.4954805807889,0.663435421038839));
#261419=CARTESIAN_POINT('Ctrl Pts',(0.463704861335473,-1.48478983238796,
0.6660974766062));
#261420=CARTESIAN_POINT('Ctrl Pts',(0.469945298320114,-1.48282651224931,
0.66657447812802));
#261421=CARTESIAN_POINT('Ctrl Pts',(0.479711343937671,-1.47968614527584,
0.667319002318261));
#261422=CARTESIAN_POINT('Ctrl Pts',(0.483245339847857,-1.47853576362622,
0.667588014762107));
#261423=CARTESIAN_POINT('Ctrl Pts',(0.489851787363023,-1.47635902448932,
0.668090103164967));
#261424=CARTESIAN_POINT('Ctrl Pts',(0.492925129760577,-1.47533574469503,
0.668323344702695));
#261425=CARTESIAN_POINT('Ctrl Pts',(0.499925620123423,-1.47298059041426,
0.668853888605112));
#261426=CARTESIAN_POINT('Ctrl Pts',(0.503850651445381,-1.47164260861902,
0.669150829604249));
#261427=CARTESIAN_POINT('Ctrl Pts',(0.51424635642346,-1.46805240901666,
0.669936024435849));
#261428=CARTESIAN_POINT('Ctrl Pts',(0.520707676404355,-1.46577307622874,
0.67042274041432));
#261429=CARTESIAN_POINT('Ctrl Pts',(0.567575198396854,-1.44889079255949,
0.673945068790048));
#261430=CARTESIAN_POINT('Ctrl Pts',(0.607380539713545,-1.43266040582839,
0.676892920079519));
#261431=CARTESIAN_POINT('Ctrl Pts',(0.747361424869308,-1.36869874581491,
0.687276342988381));
#261432=CARTESIAN_POINT('Ctrl Pts',(0.843039364190159,-1.31193479532248,
0.694426294518487));
#261433=CARTESIAN_POINT('Ctrl Pts',(0.982647523431453,-1.20747919055378,
0.70604754353356));
#261434=CARTESIAN_POINT('Ctrl Pts',(1.03104924552293,-1.16642105784593,
0.710338162096891));
#261435=CARTESIAN_POINT('Ctrl Pts',(1.08846185699101,-1.11134687965338,
0.715873791633387));
#261436=CARTESIAN_POINT('Ctrl Pts',(1.09994191376926,-1.09998584230692,
0.717004875541091));
#261437=CARTESIAN_POINT('Ctrl Pts',(1.11652765822755,-1.08305276127474,
0.718676369477237));
#261438=CARTESIAN_POINT('Ctrl Pts',(1.12177323737976,-1.07761871530082,
0.719210667734281));
#261439=CARTESIAN_POINT('Ctrl Pts',(1.13097290706534,-1.06794855221589,
0.720157921503731));
#261440=CARTESIAN_POINT('Ctrl Pts',(1.13494332232841,-1.06372810442214,
0.720570164248097));
#261441=CARTESIAN_POINT('Ctrl Pts',(1.14266501472118,-1.0554277007378,0.721378698299613));
#261442=CARTESIAN_POINT('Ctrl Pts',(1.14641825408431,-1.05134968140428,
0.721774897393359));
#261443=CARTESIAN_POINT('Ctrl Pts',(1.15651984933984,-1.04025555278575,
0.722850019852584));
#261444=CARTESIAN_POINT('Ctrl Pts',(1.16282602213382,-1.03320153499968,
0.723530700116591));
#261445=CARTESIAN_POINT('Ctrl Pts',(1.18645679048247,-1.00627802557985,
0.726118137399223));
#261446=CARTESIAN_POINT('Ctrl Pts',(1.20333874726648,-0.986027830375289,
0.728042874818006));
#261447=CARTESIAN_POINT('Ctrl Pts',(1.3259517603024,-0.831110696873445,
0.742620883490304));
#261448=CARTESIAN_POINT('Ctrl Pts',(1.40930272161761,-0.68024490813505,
0.756195352769671));
#261449=CARTESIAN_POINT('Ctrl Pts',(1.4775797733656,-0.48730148935837,0.7717212422228));
#261450=CARTESIAN_POINT('Ctrl Pts',(1.48774236961112,-0.455332621677893,
0.774231956399745));
#261451=CARTESIAN_POINT('Ctrl Pts',(1.49869891412714,-0.416566101032296,
0.777183870802785));
#261452=CARTESIAN_POINT('Ctrl Pts',(1.50049132328187,-0.410062854876716,
0.777675970128448));
#261453=CARTESIAN_POINT('Ctrl Pts',(1.50321422759375,-0.399926614190292,
0.778437952446022));
#261454=CARTESIAN_POINT('Ctrl Pts',(1.50417395767503,-0.396301673775831,
0.778709457725458));
#261455=CARTESIAN_POINT('Ctrl Pts',(1.50593359648075,-0.389556960175037,
0.779212736876146));
#261456=CARTESIAN_POINT('Ctrl Pts',(1.50673691828212,-0.386438199026311,
0.779444697140971));
#261457=CARTESIAN_POINT('Ctrl Pts',(1.5085472860492,-0.379318280836124,
0.779972542843319));
#261458=CARTESIAN_POINT('Ctrl Pts',(1.50954810254671,-0.375315599970667,
0.780268068227494));
#261459=CARTESIAN_POINT('Ctrl Pts',(1.51212031595461,-0.364851501223028,
0.78103758624613));
#261460=CARTESIAN_POINT('Ctrl Pts',(1.51366624885886,-0.358383815372678,
0.781510166402932));
#261461=CARTESIAN_POINT('Ctrl Pts',(1.52391556767919,-0.314254258189725,
0.784715160089142));
#261462=CARTESIAN_POINT('Ctrl Pts',(1.53125484938355,-0.276285368156949,
0.787376444756763));
#261463=CARTESIAN_POINT('Ctrl Pts',(1.56009630481926,-0.0900684029963861,
0.800138251818949));
#261464=CARTESIAN_POINT('Ctrl Pts',(1.5615253191562,0.0604792571434754,
0.809644097899242));
#261465=CARTESIAN_POINT('Ctrl Pts',(1.53794014872663,0.234491756868512,
0.821587607966767));
#261466=CARTESIAN_POINT('Ctrl Pts',(1.53383820216485,0.259974099753254,
0.823358629138951));
#261467=CARTESIAN_POINT('Ctrl Pts',(1.52567544239771,0.303717167850341,
0.826445174071594));
#261468=CARTESIAN_POINT('Ctrl Pts',(1.52191559076324,0.322028812019329,
0.827751418801301));
#261469=CARTESIAN_POINT('Ctrl Pts',(1.51607662230241,0.348074615712525,
0.829631715009493));
#261470=CARTESIAN_POINT('Ctrl Pts',(1.5142662595924,0.355867887778959,0.830197200003529));
#261471=CARTESIAN_POINT('Ctrl Pts',(1.51102638306974,0.36934243790031,0.831180071202483));
#261472=CARTESIAN_POINT('Ctrl Pts',(1.50962473352477,0.375030304084151,
0.83159655633343));
#261473=CARTESIAN_POINT('Ctrl Pts',(1.50686844770303,0.385949389414232,
0.832399225539762));
#261474=CARTESIAN_POINT('Ctrl Pts',(1.50551861245698,0.39118174300281,0.832785249448855));
#261475=CARTESIAN_POINT('Ctrl Pts',(1.50226905505131,0.403511988455546,
0.833698269500556));
#261476=CARTESIAN_POINT('Ctrl Pts',(1.50034626408984,0.410603608100247,
0.834226004733339));
#261477=CARTESIAN_POINT('Ctrl Pts',(1.49344662401361,0.435355107610311,
0.836077292494928));
#261478=CARTESIAN_POINT('Ctrl Pts',(1.48820780252188,0.452939699594645,
0.837409280222865));
#261479=CARTESIAN_POINT('Ctrl Pts',(1.46857535280717,0.514815922319064,
0.842157835421304));
#261480=CARTESIAN_POINT('Ctrl Pts',(1.45252572406699,0.558484750630163,
0.84562283105088));
#261481=CARTESIAN_POINT('Ctrl Pts',(1.43457651222198,0.60130730960218,0.849135319448207));
#261482=CARTESIAN_POINT('Origin',(0.,0.,-1.29405622560371));
#261483=CARTESIAN_POINT('',(1.4345768916211,0.601306404445136,1.68861155768855));
#261484=CARTESIAN_POINT('',(1.4345766830264,0.601306902103224,1.55150291788058));
#261485=CARTESIAN_POINT('',(1.43457668357355,0.601306900797845,-1.29405622560371));
#261486=CARTESIAN_POINT('Ctrl Pts',(1.43457689162107,0.601306404445218,
1.68861155768856));
#261487=CARTESIAN_POINT('Ctrl Pts',(1.46947702985195,0.518042811291588,
1.68163625042359));
#261488=CARTESIAN_POINT('Ctrl Pts',(1.49709936625474,0.43181080253797,1.67456902722138));
#261489=CARTESIAN_POINT('Ctrl Pts',(1.52411100373657,0.312534953445863,
1.66530616586023));
#261490=CARTESIAN_POINT('Ctrl Pts',(1.53018504882352,0.281294393143988,
1.6629273033566));
#261491=CARTESIAN_POINT('Ctrl Pts',(1.53635576224867,0.243381714307792,
1.66011367482268));
#261492=CARTESIAN_POINT('Ctrl Pts',(1.53737320840994,0.236869815059113,
1.65963300038737));
#261493=CARTESIAN_POINT('Ctrl Pts',(1.53889542922779,0.226704014713604,
1.65888686010136));
#261494=CARTESIAN_POINT('Ctrl Pts',(1.53942863370877,0.22305455582014,1.65861985209019));
#261495=CARTESIAN_POINT('Ctrl Pts',(1.54039792179454,0.21625130867358,1.65812372998711));
#261496=CARTESIAN_POINT('Ctrl Pts',(1.54083729919612,0.213098108130243,
1.65789444121242));
#261497=CARTESIAN_POINT('Ctrl Pts',(1.54181982153206,0.205885075323176,
1.65737141436685));
#261498=CARTESIAN_POINT('Ctrl Pts',(1.54235661422442,0.201824433371913,
1.65707803584684));
#261499=CARTESIAN_POINT('Ctrl Pts',(1.54372048119464,0.191183950640804,
1.65631194094036));
#261500=CARTESIAN_POINT('Ctrl Pts',(1.54452154029196,0.184600765889703,
1.65584063722624));
#261501=CARTESIAN_POINT('Ctrl Pts',(1.54976293713854,0.139101556098071,
1.65260043595468));
#261502=CARTESIAN_POINT('Ctrl Pts',(1.55277456447938,0.100031003265328,
1.64990466842952));
#261503=CARTESIAN_POINT('Ctrl Pts',(1.56016830440318,-0.0887222602398739,
1.63711712084431));
#261504=CARTESIAN_POINT('Ctrl Pts',(1.54439998293609,-0.238393758104582,
1.62761359938984));
#261505=CARTESIAN_POINT('Ctrl Pts',(1.4978912336626,-0.421206422828224,
1.61478063638543));
#261506=CARTESIAN_POINT('Ctrl Pts',(1.48689220023166,-0.458523882902704,
1.61209884915661));
#261507=CARTESIAN_POINT('Ctrl Pts',(1.47119250802525,-0.505253580466083,
1.60864153569624));
#261508=CARTESIAN_POINT('Ctrl Pts',(1.46777896106303,-0.515085903845827,
1.60790845192241));
#261509=CARTESIAN_POINT('Ctrl Pts',(1.4621372395123,-0.530824624202725,
1.60672555992134));
#261510=CARTESIAN_POINT('Ctrl Pts',(1.45997128996035,-0.536753126851962,
1.60627781758587));
#261511=CARTESIAN_POINT('Ctrl Pts',(1.45578092220531,-0.548009709820546,
1.60542346358882));
#261512=CARTESIAN_POINT('Ctrl Pts',(1.45376317860275,-0.553340179694012,
1.60501708030802));
#261513=CARTESIAN_POINT('Ctrl Pts',(1.44909161791738,-0.565479563135545,
1.6040873953556));
#261514=CARTESIAN_POINT('Ctrl Pts',(1.44641903938144,-0.5722810608259,1.60356347223093));
#261515=CARTESIAN_POINT('Ctrl Pts',(1.43932985624929,-0.589955541496785,
1.6021939266074));
#261516=CARTESIAN_POINT('Ctrl Pts',(1.43483802551425,-0.600797638584102,
1.60134579023391));
#261517=CARTESIAN_POINT('Ctrl Pts',(1.39944658893884,-0.683562043775598,
1.59480835568747));
#261518=CARTESIAN_POINT('Ctrl Pts',(1.36328550187317,-0.753098071601887,
1.5889393615278));
#261519=CARTESIAN_POINT('Ctrl Pts',(1.26525957859566,-0.911216729579384,
1.57469059987665));
#261520=CARTESIAN_POINT('Ctrl Pts',(1.19910246823174,-0.996669405168262,
1.56622513101214));
#261521=CARTESIAN_POINT('Ctrl Pts',(1.09860471082236,-1.10184787091824,
1.55515355218109));
#261522=CARTESIAN_POINT('Ctrl Pts',(1.07157998861481,-1.12814801935732,
1.5523232740925));
#261523=CARTESIAN_POINT('Ctrl Pts',(1.03850671127694,-1.15807239764615,
1.54905389778769));
#261524=CARTESIAN_POINT('Ctrl Pts',(1.03335890032715,-1.16266816221884,
1.54855035221874));
#261525=CARTESIAN_POINT('Ctrl Pts',(1.02536270944577,-1.1697117873204,1.54777659413747));
#261526=CARTESIAN_POINT('Ctrl Pts',(1.02253585091559,-1.17218376789684,
1.54750465378764));
#261527=CARTESIAN_POINT('Ctrl Pts',(1.01730113813029,-1.17672797861439,
1.54700407515689));
#261528=CARTESIAN_POINT('Ctrl Pts',(1.01489590356021,-1.17880305675275,
1.54677523240642));
#261529=CARTESIAN_POINT('Ctrl Pts',(1.00944435880158,-1.18347723716559,
1.54625915666706));
#261530=CARTESIAN_POINT('Ctrl Pts',(1.00639436303822,-1.18607195035641,
1.54597224579061));
#261531=CARTESIAN_POINT('Ctrl Pts',(0.997143947400219,-1.19388015411474,
1.54510742757344));
#261532=CARTESIAN_POINT('Ctrl Pts',(0.990912657518758,-1.19905712412734,
1.5445321010844));
#261533=CARTESIAN_POINT('Ctrl Pts',(0.92541120981102,-1.25261649877008,
1.53855602084028));
#261534=CARTESIAN_POINT('Ctrl Pts',(0.862679011506789,-1.29661968602737,
1.53343762221019));
#261535=CARTESIAN_POINT('Ctrl Pts',(0.738559735937297,-1.37066889415537,
1.52387977958753));
#261536=CARTESIAN_POINT('Ctrl Pts',(0.67794524001386,-1.40163973610215,
1.51943809280941));
#261537=CARTESIAN_POINT('Ctrl Pts',(0.567678406388989,-1.44914898940796,
1.51146861785002));
#261538=CARTESIAN_POINT('Ctrl Pts',(0.518857327712806,-1.46733701175572,
1.50797639726936));
#261539=CARTESIAN_POINT('Ctrl Pts',(0.43938951931784,-1.492479811296,1.5022683428947));
#261540=CARTESIAN_POINT('Ctrl Pts',(0.409283745432885,-1.50101489646662,
1.50010099034716));
#261541=CARTESIAN_POINT('Ctrl Pts',(0.369570520878116,-1.51099015944331,
1.49722571107295));
#261542=CARTESIAN_POINT('Ctrl Pts',(0.360176691740485,-1.51325687675424,
1.49654442952803));
#261543=CARTESIAN_POINT('Ctrl Pts',(0.344772843703926,-1.51682224888713,
1.49542510164577));
#261544=CARTESIAN_POINT('Ctrl Pts',(0.338775061828581,-1.51817308103593,
1.49498873392159));
#261545=CARTESIAN_POINT('Ctrl Pts',(0.327153392927051,-1.52071823852205,
1.49414208908193));
#261546=CARTESIAN_POINT('Ctrl Pts',(0.321530573539484,-1.52191701223284,
1.49373196180002));
#261547=CARTESIAN_POINT('Ctrl Pts',(0.308527789413606,-1.52461390547677,
1.4927823166758));
#261548=CARTESIAN_POINT('Ctrl Pts',(0.301143386536314,-1.52608964830419,
1.49224209532387));
#261549=CARTESIAN_POINT('Ctrl Pts',(0.277256729467131,-1.53068318037579,
1.4904915009633));
#261550=CARTESIAN_POINT('Ctrl Pts',(0.260715127902871,-1.53358725662914,
1.48927440076023));
#261551=CARTESIAN_POINT('Ctrl Pts',(0.106842591276076,-1.55804005939559,
1.47790392897099));
#261552=CARTESIAN_POINT('Ctrl Pts',(-0.032722773851731,-1.56135060755476,
1.46714572098148));
#261553=CARTESIAN_POINT('Ctrl Pts',(-0.240844015057567,-1.5383550710855,
1.45092701946117));
#261554=CARTESIAN_POINT('Ctrl Pts',(-0.310260935249755,-1.52587110136056,
1.44550465560754));
#261555=CARTESIAN_POINT('Ctrl Pts',(-0.390844694214705,-1.50564938384172,
1.43935027825852));
#261556=CARTESIAN_POINT('Ctrl Pts',(-0.40305275318308,-1.50242741842925,
1.43842191607972));
#261557=CARTESIAN_POINT('Ctrl Pts',(-0.419834660048688,-1.49777903234407,
1.43715250077954));
#261558=CARTESIAN_POINT('Ctrl Pts',(-0.424442734661721,-1.49647971524599,
1.43680464517902));
#261559=CARTESIAN_POINT('Ctrl Pts',(-0.432210598619843,-1.49425068039647,
1.43621954316593));
#261560=CARTESIAN_POINT('Ctrl Pts',(-0.435373537421865,-1.4933321737233,
1.43598165949231));
#261561=CARTESIAN_POINT('Ctrl Pts',(-0.441396814462889,-1.49156227093823,
1.43552936711224));
#261562=CARTESIAN_POINT('Ctrl Pts',(-0.444257644164275,-1.49071268255076,
1.43531485230392));
#261563=CARTESIAN_POINT('Ctrl Pts',(-0.45179755210692,-1.4884499025236,
1.43475025069703));
#261564=CARTESIAN_POINT('Ctrl Pts',(-0.456472496883849,-1.48702286523591,
1.43440096272407));
#261565=CARTESIAN_POINT('Ctrl Pts',(-0.472917467684116,-1.48191814020581,
1.43317477187758));
#261566=CARTESIAN_POINT('Ctrl Pts',(-0.48465081702012,-1.47812242940753,
1.43230440566613));
#261567=CARTESIAN_POINT('Ctrl Pts',(-0.573096397349444,-1.44834404074764,
1.42576895241146));
#261568=CARTESIAN_POINT('Ctrl Pts',(-0.647730605375835,-1.41654114789611,
1.42039554307145));
#261569=CARTESIAN_POINT('Ctrl Pts',(-0.789923212516117,-1.34234906570331,
1.40982159961455));
#261570=CARTESIAN_POINT('Ctrl Pts',(-0.857373351170098,-1.3003037932978,
1.40463336501362));
#261571=CARTESIAN_POINT('Ctrl Pts',(-0.967449016110154,-1.21938532508896,
1.39546327076228));
#261572=CARTESIAN_POINT('Ctrl Pts',(-1.01166641417249,-1.18295730768821,
1.39155692237752));
#261573=CARTESIAN_POINT('Ctrl Pts',(-1.06235332445162,-1.1362753902485,
1.38673354107849));
#261574=CARTESIAN_POINT('Ctrl Pts',(-1.0708451767133,-1.12827609336263,
1.38591303010189));
#261575=CARTESIAN_POINT('Ctrl Pts',(-1.08399003772638,-1.11561160094031,
1.3846227937056));
#261576=CARTESIAN_POINT('Ctrl Pts',(-1.08870487708301,-1.11101095144756,
1.38415586041571));
#261577=CARTESIAN_POINT('Ctrl Pts',(-1.09701426352902,-1.10279912742805,
1.38332545373235));
#261578=CARTESIAN_POINT('Ctrl Pts',(-1.10062058289263,-1.0991999550681,
1.38296251096572));
#261579=CARTESIAN_POINT('Ctrl Pts',(-1.10889608061512,-1.09085930117704,
1.38212372074988));
#261580=CARTESIAN_POINT('Ctrl Pts',(-1.11355261563634,-1.08610547472691,
1.3816473280956));
#261581=CARTESIAN_POINT('Ctrl Pts',(-1.12627847264442,-1.07294586165086,
1.3803330570039));
#261582=CARTESIAN_POINT('Ctrl Pts',(-1.13428392403261,-1.06447920877463,
1.37949244521473));
#261583=CARTESIAN_POINT('Ctrl Pts',(-1.17659177373673,-1.01871477913086,
1.37497402674284));
#261584=CARTESIAN_POINT('Ctrl Pts',(-1.20914748061511,-0.979851669508349,
1.37122404324996));
#261585=CARTESIAN_POINT('Ctrl Pts',(-1.32874744011104,-0.822025411168555,
1.35630750471059));
#261586=CARTESIAN_POINT('Ctrl Pts',(-1.40059358326385,-0.692548704305531,
1.34463305868347));
#261587=CARTESIAN_POINT('Ctrl Pts',(-1.46344952503628,-0.527947840398722,
1.33132394168275));
#261588=CARTESIAN_POINT('Ctrl Pts',(-1.47299520060752,-0.500698369684845,
1.32917043733586));
#261589=CARTESIAN_POINT('Ctrl Pts',(-1.48372638718087,-0.467094522767675,
1.32658763593252));
#261590=CARTESIAN_POINT('Ctrl Pts',(-1.48563744191302,-0.460980129983615,
1.32612059549288));
#261591=CARTESIAN_POINT('Ctrl Pts',(-1.48857736898995,-0.451365674866176,
1.32539095751953));
#261592=CARTESIAN_POINT('Ctrl Pts',(-1.48963176629998,-0.44787359543901,
1.32512692426015));
#261593=CARTESIAN_POINT('Ctrl Pts',(-1.49158520023677,-0.441320763556021,
1.32463334585756));
#261594=CARTESIAN_POINT('Ctrl Pts',(-1.49248709623981,-0.438260988160894,
1.32440364433014));
#261595=CARTESIAN_POINT('Ctrl Pts',(-1.49452372650491,-0.431272308302537,
1.32388072335258));
#261596=CARTESIAN_POINT('Ctrl Pts',(-1.49565238449056,-0.427341688574858,
1.3235878583072));
#261597=CARTESIAN_POINT('Ctrl Pts',(-1.49860481923419,-0.416904669953052,
1.32281338064514));
#261598=CARTESIAN_POINT('Ctrl Pts',(-1.50040175098156,-0.410390665213693,
1.32233326918413));
#261599=CARTESIAN_POINT('Ctrl Pts',(-1.51309915801623,-0.36316327768386,
1.31887454049316));
#261600=CARTESIAN_POINT('Ctrl Pts',(-1.52238455704785,-0.322028997005506,
1.31598072507761));
#261601=CARTESIAN_POINT('Ctrl Pts',(-1.54687992645591,-0.188449381937575,
1.3068121129331));
#261602=CARTESIAN_POINT('Ctrl Pts',(-1.55541936552532,-0.094992260473266,
1.3007353902558));
#261603=CARTESIAN_POINT('Ctrl Pts',(-1.55557348769334,0.085302141614542,
1.28881070820183));
#261604=CARTESIAN_POINT('Ctrl Pts',(-1.54841048352085,0.171775820456287,
1.28300010839956));
#261605=CARTESIAN_POINT('Ctrl Pts',(-1.53212304440099,0.268925011977032,
1.27612020331118));
#261606=CARTESIAN_POINT('Ctrl Pts',(-1.53002224142329,0.280630739985389,
1.27528554538495));
#261607=CARTESIAN_POINT('Ctrl Pts',(-1.52640536660373,0.299534636872861,
1.27392785856942));
#261608=CARTESIAN_POINT('Ctrl Pts',(-1.52497206801355,0.306748317530233,
1.27340745450651));
#261609=CARTESIAN_POINT('Ctrl Pts',(-1.52233616893067,0.319539339119536,
1.27248045259176));
#261610=CARTESIAN_POINT('Ctrl Pts',(-1.52115392963752,0.325120779465095,
1.27207451030199));
#261611=CARTESIAN_POINT('Ctrl Pts',(-1.51860446781096,0.33683860255135,
1.27121917272598));
#261612=CARTESIAN_POINT('Ctrl Pts',(-1.51723069829119,0.342973438976443,
1.27076957468061));
#261613=CARTESIAN_POINT('Ctrl Pts',(-1.51350931723417,0.359131983730321,
1.26958056130195));
#261614=CARTESIAN_POINT('Ctrl Pts',(-1.51109935284875,0.36914085582507,
1.26883916035103));
#261615=CARTESIAN_POINT('Ctrl Pts',(-1.49942019375988,0.415613846987299,
1.26537320132012));
#261616=CARTESIAN_POINT('Ctrl Pts',(-1.4889300865898,0.451754947024388,
1.26260974702371));
#261617=CARTESIAN_POINT('Ctrl Pts',(-1.42994710317126,0.630483563644251,
1.24858609467863));
#261618=CARTESIAN_POINT('Ctrl Pts',(-1.36223632885688,0.765869029319142,
1.2366981416937));
#261619=CARTESIAN_POINT('Ctrl Pts',(-1.25342286279638,0.92200490502971,
1.22218514922512));
#261620=CARTESIAN_POINT('Ctrl Pts',(-1.2294382870733,0.953752631892701,
1.21919274905108));
#261621=CARTESIAN_POINT('Ctrl Pts',(-1.20004644150441,0.989703549733059,
1.21578522031566));
#261622=CARTESIAN_POINT('Ctrl Pts',(-1.19579916855584,0.994831106691519,
1.21529875563426));
#261623=CARTESIAN_POINT('Ctrl Pts',(-1.18888095655569,1.00307485364047,
1.21451611628556));
#261624=CARTESIAN_POINT('Ctrl Pts',(-1.18623043963367,1.00620794868729,
1.21421854255951));
#261625=CARTESIAN_POINT('Ctrl Pts',(-1.18150126728005,1.01175350031487,
1.21369167087887));
#261626=CARTESIAN_POINT('Ctrl Pts',(-1.17942757545345,1.01417009665563,
1.21346202045505));
#261627=CARTESIAN_POINT('Ctrl Pts',(-1.17493963846848,1.01936777371926,
1.21296797429861));
#261628=CARTESIAN_POINT('Ctrl Pts',(-1.17252293641021,1.02214665116949,
1.21270376409842));
#261629=CARTESIAN_POINT('Ctrl Pts',(-1.16577010957281,1.02985601532426,
1.21197047833673));
#261630=CARTESIAN_POINT('Ctrl Pts',(-1.16141253366209,1.03476774757171,
1.21150295529719));
#261631=CARTESIAN_POINT('Ctrl Pts',(-1.13603727428098,1.06300775983557,
1.20881193715266));
#261632=CARTESIAN_POINT('Ctrl Pts',(-1.11434635301835,1.08572498707744,
1.20663525466513));
#261633=CARTESIAN_POINT('Ctrl Pts',(-0.98805269827552,1.21021832758287,
1.19452812336636));
#261634=CARTESIAN_POINT('Ctrl Pts',(-0.870219668701142,1.29753718960344,
1.18526742193276));
#261635=CARTESIAN_POINT('Ctrl Pts',(-0.69850814393012,1.39072194000651,
1.1720915300266));
#261636=CARTESIAN_POINT('Ctrl Pts',(-0.653991108301251,1.41220251344607,
1.16870808846952));
#261637=CARTESIAN_POINT('Ctrl Pts',(-0.597888450156065,1.43605131667649,
1.16444121945438));
#261638=CARTESIAN_POINT('Ctrl Pts',(-0.587195965302839,1.44045647921834,
1.16362794962157));
#261639=CARTESIAN_POINT('Ctrl Pts',(-0.570293514032257,1.44720059922895,
1.16234177608077));
#261640=CARTESIAN_POINT('Ctrl Pts',(-0.56411584152675,1.44961980581849,
1.16187157423817));
#261641=CARTESIAN_POINT('Ctrl Pts',(-0.552688576281814,1.4540106711347,
1.16100149744248));
#261642=CARTESIAN_POINT('Ctrl Pts',(-0.54744341125555,1.45599361402702,
1.16060200790133));
#261643=CARTESIAN_POINT('Ctrl Pts',(-0.535798177752869,1.46032429099681,
1.15971473977937));
#261644=CARTESIAN_POINT('Ctrl Pts',(-0.529393198540841,1.46265838826402,
1.15922651632774));
#261645=CARTESIAN_POINT('Ctrl Pts',(-0.510974953709208,1.46923352475853,
1.15782182289244));
#261646=CARTESIAN_POINT('Ctrl Pts',(-0.498924905618295,1.47336908959832,
1.15690189176821));
#261647=CARTESIAN_POINT('Ctrl Pts',(-0.404891761676893,1.50435536065194,
1.14971427206073));
#261648=CARTESIAN_POINT('Ctrl Pts',(-0.320869261092523,1.52448691265095,
1.14322671525037));
#261649=CARTESIAN_POINT('Ctrl Pts',(-0.156310616436556,1.54970506991017,
1.13043476339516));
#261650=CARTESIAN_POINT('Ctrl Pts',(-0.0761772999499947,1.55570410311018,
1.12417006138014));
#261651=CARTESIAN_POINT('Ctrl Pts',(0.0600159012072503,1.55534866897435,
1.11368697014316));
#261652=CARTESIAN_POINT('Ctrl Pts',(0.115931073947269,1.55218328581326,
1.10943274265708));
#261653=CARTESIAN_POINT('Ctrl Pts',(0.179369142170793,1.54514358233649,
1.10474350499066));
#261654=CARTESIAN_POINT('Ctrl Pts',(0.187171545926944,1.54421785980289,
1.10416917537605));
#261655=CARTESIAN_POINT('Ctrl Pts',(0.198942925122992,1.54273070375616,
1.10330666627319));
#261656=CARTESIAN_POINT('Ctrl Pts',(0.202917137718063,1.54221300343609,
1.10301615429863));
#261657=CARTESIAN_POINT('Ctrl Pts',(0.21003819328198,1.54125737663815,1.10249689241487));
#261658=CARTESIAN_POINT('Ctrl Pts',(0.213185721119119,1.54082516614265,
1.102267830215));
#261659=CARTESIAN_POINT('Ctrl Pts',(0.220048544778588,1.53986134865761,
1.10176937874498));
#261660=CARTESIAN_POINT('Ctrl Pts',(0.223763242681018,1.53932593922779,
1.10150020595733));
#261661=CARTESIAN_POINT('Ctrl Pts',(0.234291303737873,1.53776958551781,
1.10073901430338));
#261662=CARTESIAN_POINT('Ctrl Pts',(0.241099988262787,1.53671679678208,
1.1002487450018));
#261663=CARTESIAN_POINT('Ctrl Pts',(0.28486852338225,1.52965105171671,1.09710873078209));
#261664=CARTESIAN_POINT('Ctrl Pts',(0.321611753136779,1.52234978643954,
1.09452597050568));
#261665=CARTESIAN_POINT('Ctrl Pts',(0.446436204462301,1.49282365835129,
1.08582332454664));
#261666=CARTESIAN_POINT('Ctrl Pts',(0.532819344676398,1.46421784164596,
1.07991637005052));
#261667=CARTESIAN_POINT('Ctrl Pts',(0.703502164570861,1.39057602712734,
1.06765060524126));
#261668=CARTESIAN_POINT('Ctrl Pts',(0.787136958830996,1.34500123516558,
1.06130476085849));
#261669=CARTESIAN_POINT('Ctrl Pts',(0.876016849973839,1.28542512671853,
1.05383229113049));
#261670=CARTESIAN_POINT('Ctrl Pts',(0.885873630831345,1.27865209264722,
1.0529930084074));
#261671=CARTESIAN_POINT('Ctrl Pts',(0.901616177077629,1.26756528408968,
1.05163482202807));
#261672=CARTESIAN_POINT('Ctrl Pts',(0.90755153417416,1.26332248050222,1.05111861572351));
#261673=CARTESIAN_POINT('Ctrl Pts',(0.918081768272671,1.2556825902466,1.05019525393344));
#261674=CARTESIAN_POINT('Ctrl Pts',(0.92268822089766,1.25230161946119,1.04978872487825));
#261675=CARTESIAN_POINT('Ctrl Pts',(0.932298319974304,1.24516634357961,
1.04893507346716));
#261676=CARTESIAN_POINT('Ctrl Pts',(0.937298146254264,1.24140709017123,
1.04848776320533));
#261677=CARTESIAN_POINT('Ctrl Pts',(0.950351644777962,1.23146865340416,
1.04731145205751));
#261678=CARTESIAN_POINT('Ctrl Pts',(0.958367625511021,1.2252407022056,1.04658054199366));
#261679=CARTESIAN_POINT('Ctrl Pts',(0.994582899057056,1.19653070897553,
1.04323856656561));
#261680=CARTESIAN_POINT('Ctrl Pts',(1.02205382972573,1.17315235604944,1.04059192817647));
#261681=CARTESIAN_POINT('Ctrl Pts',(1.14870224678509,1.05754521446165,1.02783211658105));
#261682=CARTESIAN_POINT('Ctrl Pts',(1.23635695789021,0.953586940733363,
1.01722326506742));
#261683=CARTESIAN_POINT('Ctrl Pts',(1.33955176781088,0.792650913198052,
1.00250881300004));
#261684=CARTESIAN_POINT('Ctrl Pts',(1.36712815246778,0.744081036960375,
0.998266531269419));
#261685=CARTESIAN_POINT('Ctrl Pts',(1.39554107001377,0.687100459326392,
0.993588779202292));
#261686=CARTESIAN_POINT('Ctrl Pts',(1.39899222286615,0.680046091520333,
0.993014731862127));
#261687=CARTESIAN_POINT('Ctrl Pts',(1.40412343565381,0.669353182435813,
0.992152560980039));
#261688=CARTESIAN_POINT('Ctrl Pts',(1.4058430349553,0.665733931413195,0.991862107628564));
#261689=CARTESIAN_POINT('Ctrl Pts',(1.40890082906937,0.65923349061345,0.991342931714634));
#261690=CARTESIAN_POINT('Ctrl Pts',(1.41024419491643,0.65635482220917,0.991113896958817));
#261691=CARTESIAN_POINT('Ctrl Pts',(1.41315528437642,0.650066515635028,
0.99061549895062));
#261692=CARTESIAN_POINT('Ctrl Pts',(1.41471948915563,0.646655318017194,
0.990346352190897));
#261693=CARTESIAN_POINT('Ctrl Pts',(1.41912069779765,0.63696481244076,0.989585115389858));
#261694=CARTESIAN_POINT('Ctrl Pts',(1.42192839346087,0.630672161887732,
0.989094776230573));
#261695=CARTESIAN_POINT('Ctrl Pts',(1.42805041300984,0.616702667701304,
0.988014564795362));
#261696=CARTESIAN_POINT('Ctrl Pts',(1.43134466050347,0.609017746848256,
0.987425839742894));
#261697=CARTESIAN_POINT('Ctrl Pts',(1.43457668375786,0.601306900358119,
0.986840263175809));
#261698=CARTESIAN_POINT('Ctrl Pts',(1.43457651222198,0.60130730960218,0.849135319448207));
#261699=CARTESIAN_POINT('Ctrl Pts',(1.38252124128554,0.725498830028205,
0.859322036099769));
#261700=CARTESIAN_POINT('Ctrl Pts',(1.31448918024001,0.842567569839434,
0.869970240706755));
#261701=CARTESIAN_POINT('Ctrl Pts',(1.21137563149819,0.976371402887454,
0.882789016303748));
#261702=CARTESIAN_POINT('Ctrl Pts',(1.189783341211,1.00257073499454,0.885330749105257));
#261703=CARTESIAN_POINT('Ctrl Pts',(1.16287889282022,1.03312084419423,0.888313744286222));
#261704=CARTESIAN_POINT('Ctrl Pts',(1.15837550673526,1.03816770705299,0.888807180358547));
#261705=CARTESIAN_POINT('Ctrl Pts',(1.15132316219203,1.04596811695431,0.889570627367972));
#261706=CARTESIAN_POINT('Ctrl Pts',(1.14879699377079,1.04874200516475,0.889842273298709));
#261707=CARTESIAN_POINT('Ctrl Pts',(1.14408330598466,1.05388045562734,0.890345729967646));
#261708=CARTESIAN_POINT('Ctrl Pts',(1.14189849863544,1.05624734078522,0.890577727452879));
#261709=CARTESIAN_POINT('Ctrl Pts',(1.13690032532251,1.06162841884838,0.891105409001971));
#261710=CARTESIAN_POINT('Ctrl Pts',(1.13408231802333,1.06463822326139,0.891400734663236));
#261711=CARTESIAN_POINT('Ctrl Pts',(1.12669988399016,1.0724605421027,0.892168848503456));
#261712=CARTESIAN_POINT('Ctrl Pts',(1.12211652159247,1.07725519681762,0.892640236320011));
#261713=CARTESIAN_POINT('Ctrl Pts',(1.09092229591283,1.10947235526492,0.89581283530405));
#261714=CARTESIAN_POINT('Ctrl Pts',(1.06333674677543,1.13593834694746,0.898444651305174));
#261715=CARTESIAN_POINT('Ctrl Pts',(0.923085691486571,1.26090521743907,
0.911172564597422));
#261716=CARTESIAN_POINT('Ctrl Pts',(0.79759056472164,1.34380982122556,0.920669819155478));
#261717=CARTESIAN_POINT('Ctrl Pts',(0.626333663297266,1.42437898806925,
0.933537487226954));
#261718=CARTESIAN_POINT('Ctrl Pts',(0.589862043573178,1.43986515860209,
0.93626745608184));
#261719=CARTESIAN_POINT('Ctrl Pts',(0.542973172057567,1.45769401865363,
0.939784966099226));
#261720=CARTESIAN_POINT('Ctrl Pts',(0.533066943695342,1.46134572958528,
0.940528505651257));
#261721=CARTESIAN_POINT('Ctrl Pts',(0.517099285981078,1.4670478899907,0.94172800107995));
#261722=CARTESIAN_POINT('Ctrl Pts',(0.511060914949056,1.46916231985436,
0.942181832208195));
#261723=CARTESIAN_POINT('Ctrl Pts',(0.499547569433473,1.47311432911384,
0.94304766663842));
#261724=CARTESIAN_POINT('Ctrl Pts',(0.494075056038687,1.47495879200626,
0.943459434697607));
#261725=CARTESIAN_POINT('Ctrl Pts',(0.481565043745473,1.47909774831759,
0.944401294543088));
#261726=CARTESIAN_POINT('Ctrl Pts',(0.474521230095981,1.48137255243881,
0.944932022237243));
#261727=CARTESIAN_POINT('Ctrl Pts',(0.456126223567672,1.48716857297521,
0.946319232153606));
#261728=CARTESIAN_POINT('Ctrl Pts',(0.444750627721582,1.4906100633129,0.947178287525633));
#261729=CARTESIAN_POINT('Ctrl Pts',(0.331054454726678,1.523589562191,0.955777998203588));
#261730=CARTESIAN_POINT('Ctrl Pts',(0.226017324457541,1.5426695990472,0.963862607440416));
#261731=CARTESIAN_POINT('Ctrl Pts',(0.0375777904095188,1.55723530395187,
0.978479558492936));
#261732=CARTESIAN_POINT('Ctrl Pts',(-0.04509950512612,1.55703592468897,
0.984921688476582));
#261733=CARTESIAN_POINT('Ctrl Pts',(-0.161636295081288,1.54746110488474,
0.993797166607807));
#261734=CARTESIAN_POINT('Ctrl Pts',(-0.195800477696142,1.54351054130787,
0.996372583099473));
#261735=CARTESIAN_POINT('Ctrl Pts',(-0.23653025993098,1.53742637980791,
0.999390396331067));
#261736=CARTESIAN_POINT('Ctrl Pts',(-0.243245311703895,1.53637826074077,
0.99988621036928));
#261737=CARTESIAN_POINT('Ctrl Pts',(-0.253667506920813,1.53468146722319,
1.0006528385931));
#261738=CARTESIAN_POINT('Ctrl Pts',(-0.257379419060607,1.53406331204561,
1.00092530246312));
#261739=CARTESIAN_POINT('Ctrl Pts',(-0.264266450442967,1.53289069452681,
1.00142971633006));
#261740=CARTESIAN_POINT('Ctrl Pts',(-0.267442064678358,1.53233983848057,
1.00166185695803));
#261741=CARTESIAN_POINT('Ctrl Pts',(-0.2746710671701,1.53106270652627,1.00218931038214));
#261742=CARTESIAN_POINT('Ctrl Pts',(-0.278723295630357,1.53033020357775,
1.00248426798976));
#261743=CARTESIAN_POINT('Ctrl Pts',(-0.289277435482008,1.52837906747988,
1.0032507629536));
#261744=CARTESIAN_POINT('Ctrl Pts',(-0.29577465647734,1.52713501868479,
1.00372090975551));
#261745=CARTESIAN_POINT('Ctrl Pts',(-0.339382301186448,1.51849654135683,
1.0068661021311));
#261746=CARTESIAN_POINT('Ctrl Pts',(-0.376223917661278,1.5097907943711,
1.00947311473199));
#261747=CARTESIAN_POINT('Ctrl Pts',(-0.421681062435962,1.49728147402012,
1.01266876901983));
#261748=CARTESIAN_POINT('Ctrl Pts',(-0.430625114309803,1.49473367118787,
1.0132965053976));
#261749=CARTESIAN_POINT('Ctrl Pts',(-0.520999676594754,1.46811104695537,
1.01963385005443));
#261750=CARTESIAN_POINT('Ctrl Pts',(-0.6003558147064,1.43748570540251,1.0251597029698));
#261751=CARTESIAN_POINT('Ctrl Pts',(-0.758675402697065,1.36097655669677,
1.03677743699352));
#261752=CARTESIAN_POINT('Ctrl Pts',(-0.836893915015948,1.31432506738727,
1.04286326187219));
#261753=CARTESIAN_POINT('Ctrl Pts',(-0.921088524245512,1.25353261447549,
1.05011908101066));
#261754=CARTESIAN_POINT('Ctrl Pts',(-0.931496399183518,1.24581801460567,
1.05102903771146));
#261755=CARTESIAN_POINT('Ctrl Pts',(-0.947309802829804,1.23378774658048,
1.05243241903047));
#261756=CARTESIAN_POINT('Ctrl Pts',(-0.952785115111711,1.22956438943957,
1.05292223614388));
#261757=CARTESIAN_POINT('Ctrl Pts',(-0.962706253104655,1.22180570561005,
1.05381702475892));
#261758=CARTESIAN_POINT('Ctrl Pts',(-0.967161245844507,1.2182822476736,
1.0542215212823));
#261759=CARTESIAN_POINT('Ctrl Pts',(-0.97683796289859,1.21054239413973,
1.05510610983604));
#261760=CARTESIAN_POINT('Ctrl Pts',(-0.98205187507166,1.20631646172496,
1.0555865786323));
#261761=CARTESIAN_POINT('Ctrl Pts',(-0.996263111772014,1.19464490539579,
1.05690686548452));
#261762=CARTESIAN_POINT('Ctrl Pts',(-1.00520402692733,1.18713162214269,
1.05774940952945));
#261763=CARTESIAN_POINT('Ctrl Pts',(-1.05177222238781,1.14709587205882,
1.06220183249665));
#261764=CARTESIAN_POINT('Ctrl Pts',(-1.08790417430716,1.11288689203241,
1.06588098051816));
#261765=CARTESIAN_POINT('Ctrl Pts',(-1.22430212971465,0.970749038285334,
1.08071090171115));
#261766=CARTESIAN_POINT('Ctrl Pts',(-1.31064717441965,0.85056667771223,
1.09237420420515));
#261767=CARTESIAN_POINT('Ctrl Pts',(-1.39251463357061,0.693801356321801,
1.10574303195069));
#261768=CARTESIAN_POINT('Ctrl Pts',(-1.40547258343405,0.667161485649584,
1.10795391944232));
#261769=CARTESIAN_POINT('Ctrl Pts',(-1.42034187203205,0.634233071156714,
1.11059983230143));
#261770=CARTESIAN_POINT('Ctrl Pts',(-1.42298360279155,0.628283608094607,
1.11107449419389));
#261771=CARTESIAN_POINT('Ctrl Pts',(-1.42706768767903,0.618927899193213,
1.11181540451949));
#261772=CARTESIAN_POINT('Ctrl Pts',(-1.42853533249328,0.615532886376711,
1.11208313600966));
#261773=CARTESIAN_POINT('Ctrl Pts',(-1.4312620000841,0.609163172322001,
1.11258329415791));
#261774=CARTESIAN_POINT('Ctrl Pts',(-1.43252385342851,0.606189816019058,
1.11281588291632));
#261775=CARTESIAN_POINT('Ctrl Pts',(-1.43538126528477,0.599398030131703,
1.11334518069764));
#261776=CARTESIAN_POINT('Ctrl Pts',(-1.4369708542588,0.595577148935932,
1.11364152785334));
#261777=CARTESIAN_POINT('Ctrl Pts',(-1.44114511426338,0.585429514616591,
1.11442493148459));
#261778=CARTESIAN_POINT('Ctrl Pts',(-1.44370340878653,0.579091900247909,
1.11491045541016));
#261779=CARTESIAN_POINT('Ctrl Pts',(-1.46194340211918,0.533034076933747,
1.11841333137365));
#261780=CARTESIAN_POINT('Ctrl Pts',(-1.47602703377542,0.492695490252898,
1.12134380955399));
#261781=CARTESIAN_POINT('Ctrl Pts',(-1.51662619730622,0.358950586458834,
1.13077519117541));
#261782=CARTESIAN_POINT('Ctrl Pts',(-1.53606582667053,0.263637374739793,
1.13706437900492));
#261783=CARTESIAN_POINT('Ctrl Pts',(-1.55246975725895,0.111846837466457,
1.14717764206141));
#261784=CARTESIAN_POINT('Ctrl Pts',(-1.55547510902623,0.0562885750329613,
1.15089681480198));
#261785=CARTESIAN_POINT('Ctrl Pts',(-1.55550236599615,-0.00497133169592584,
1.15508610382524));
#261786=CARTESIAN_POINT('Ctrl Pts',(-1.5554739555871,-0.01063467066421,
1.15547420582998));
#261787=CARTESIAN_POINT('Ctrl Pts',(-1.55537238880768,-0.0203280044423647,
1.15613995724327));
#261788=CARTESIAN_POINT('Ctrl Pts',(-1.55531449397086,-0.0243581608166827,
1.15641719143077));
#261789=CARTESIAN_POINT('Ctrl Pts',(-1.55479239393149,-0.0529614741374404,
1.15838804467652));
#261790=CARTESIAN_POINT('Ctrl Pts',(-1.5537615336251,-0.0775195895801902,
1.16009719197776));
#261791=CARTESIAN_POINT('Ctrl Pts',(-1.55154601512956,-0.111219642694066,
1.16247078817666));
#261792=CARTESIAN_POINT('Ctrl Pts',(-1.55086126777126,-0.120391725709347,
1.16311967475016));
#261793=CARTESIAN_POINT('Ctrl Pts',(-1.54963805580057,-0.135026941878215,
1.1641598740465));
#261794=CARTESIAN_POINT('Ctrl Pts',(-1.54915193533731,-0.140494337443032,
1.1645495449719));
#261795=CARTESIAN_POINT('Ctrl Pts',(-1.54809140733786,-0.151746627362062,
1.16535378797963));
#261796=CARTESIAN_POINT('Ctrl Pts',(-1.54751348834385,-0.157531095649165,
1.1657684640257));
#261797=CARTESIAN_POINT('Ctrl Pts',(-1.54609446047687,-0.170972221383311,
1.16673498023718));
#261798=CARTESIAN_POINT('Ctrl Pts',(-1.54522888264341,-0.178626082901079,
1.16728757946257));
#261799=CARTESIAN_POINT('Ctrl Pts',(-1.54227350249389,-0.203127814151401,
1.1690639200104));
#261800=CARTESIAN_POINT('Ctrl Pts',(-1.53996477971028,-0.219947494202914,
1.17029448681145));
#261801=CARTESIAN_POINT('Ctrl Pts',(-1.52674913907203,-0.305774691445692,
1.17663348793641));
#261802=CARTESIAN_POINT('Ctrl Pts',(-1.51147889498719,-0.374018726176664,
1.18187726894355));
#261803=CARTESIAN_POINT('Ctrl Pts',(-1.46263193063276,-0.539244088618074,
1.19505902221553));
#261804=CARTESIAN_POINT('Ctrl Pts',(-1.42395333003346,-0.634375148820113,
1.20309185189433));
#261805=CARTESIAN_POINT('Ctrl Pts',(-1.36916336120564,-0.738376720585995,
1.21208109386595));
#261806=CARTESIAN_POINT('Ctrl Pts',(-1.36192718835405,-0.751640108515646,
1.21323114937633));
#261807=CARTESIAN_POINT('Ctrl Pts',(-1.33971479523699,-0.79097954526294,
1.21664920723525));
#261808=CARTESIAN_POINT('Ctrl Pts',(-1.32417344773885,-0.816730903254209,
1.21889602967302));
#261809=CARTESIAN_POINT('Ctrl Pts',(-1.30422376742877,-0.84771845841536,
1.22159716373092));
#261810=CARTESIAN_POINT('Ctrl Pts',(-1.30051624307651,-0.853395410272971,
1.22209190194828));
#261811=CARTESIAN_POINT('Ctrl Pts',(-1.29467367034061,-0.862215036046148,
1.22286012446978));
#261812=CARTESIAN_POINT('Ctrl Pts',(-1.29256408861742,-0.865374345998211,
1.22313523233649));
#261813=CARTESIAN_POINT('Ctrl Pts',(-1.28864621004977,-0.871195471691298,
1.22364193293743));
#261814=CARTESIAN_POINT('Ctrl Pts',(-1.28684123972178,-0.873859387261356,
1.22387373303335));
#261815=CARTESIAN_POINT('Ctrl Pts',(-1.282737601231,-0.879875569033461,
1.22439706421126));
#261816=CARTESIAN_POINT('Ctrl Pts',(-1.28043405500053,-0.883224434899434,
1.22468826153219));
#261817=CARTESIAN_POINT('Ctrl Pts',(-1.27341448094159,-0.893344219461222,
1.2255680071401));
#261818=CARTESIAN_POINT('Ctrl Pts',(-1.26865757858146,-0.900086824119339,
1.22615387685606));
#261819=CARTESIAN_POINT('Ctrl Pts',(-1.25753405228508,-0.91559031891837,
1.22750113780947));
#261820=CARTESIAN_POINT('Ctrl Pts',(-1.25112906567896,-0.924323321020851,
1.2282601533158));
#261821=CARTESIAN_POINT('Ctrl Pts',(-1.22894868431004,-0.953912563954547,
1.23083497205084));
#261822=CARTESIAN_POINT('Ctrl Pts',(-1.2127380344378,-0.97443865103255,
1.23262650848742));
#261823=CARTESIAN_POINT('Ctrl Pts',(-1.12141374953853,-1.0842628208825,
1.24230248775796));
#261824=CARTESIAN_POINT('Ctrl Pts',(-1.03694961046443,-1.16530431190777,
1.2498048468105));
#261825=CARTESIAN_POINT('Ctrl Pts',(-0.89007153830761,-1.27749524643152,
1.26212606699102));
#261826=CARTESIAN_POINT('Ctrl Pts',(-0.833280868150213,-1.31524238070048,
1.26674248916005));
#261827=CARTESIAN_POINT('Ctrl Pts',(-0.764198252988644,-1.35488537484497,
1.27230860882707));
#261828=CARTESIAN_POINT('Ctrl Pts',(-0.754128585887999,-1.36051586253214,
1.27311864235395));
#261829=CARTESIAN_POINT('Ctrl Pts',(-0.737590325471856,-1.36952327115748,
1.27444743516849));
#261830=CARTESIAN_POINT('Ctrl Pts',(-0.731158826443947,-1.37296767832018,
1.27496379519455));
#261831=CARTESIAN_POINT('Ctrl Pts',(-0.719605741538495,-1.37905076687507,
1.27589077815736));
#261832=CARTESIAN_POINT('Ctrl Pts',(-0.714493242178622,-1.3817064978211,
1.27630079115074));
#261833=CARTESIAN_POINT('Ctrl Pts',(-0.703622064163257,-1.38727715301918,
1.27717228645444));
#261834=CARTESIAN_POINT('Ctrl Pts',(-0.697859775376042,-1.39018475033367,
1.2776340158875));
#261835=CARTESIAN_POINT('Ctrl Pts',(-0.682388600382008,-1.3978709326538,
1.27887326095563));
#261836=CARTESIAN_POINT('Ctrl Pts',(-0.672647821402575,-1.40258413068884,
1.27965302791472));
#261837=CARTESIAN_POINT('Ctrl Pts',(-0.624113562018207,-1.4254461791857,
1.28353670135107));
#261838=CARTESIAN_POINT('Ctrl Pts',(-0.584634855556928,-1.44208736654561,
1.28669153479107));
#261839=CARTESIAN_POINT('Ctrl Pts',(-0.392282042439899,-1.51397139325813,
1.30205889371115));
#261840=CARTESIAN_POINT('Ctrl Pts',(-0.232101698918667,-1.54664414741534,
1.31498316018246));
#261841=CARTESIAN_POINT('Ctrl Pts',(-0.0656800867438431,-1.55411816806265,
1.32750373701108));
#261842=CARTESIAN_POINT('Ctrl Pts',(-0.061572006395244,-1.55428634520056,
1.32781215649388));
#261843=CARTESIAN_POINT('Ctrl Pts',(-0.0374539076559448,-1.55517792429528,
1.32961887860166));
#261844=CARTESIAN_POINT('Ctrl Pts',(-0.0174308413185623,-1.55553124004874,
1.33110279299082));
#261845=CARTESIAN_POINT('Ctrl Pts',(0.00855751168281875,-1.55548788948749,
1.33300343140338));
#261846=CARTESIAN_POINT('Ctrl Pts',(0.0145203586239918,-1.5554436562103,
1.33343778559679));
#261847=CARTESIAN_POINT('Ctrl Pts',(0.0240608367071122,-1.55531801563273,
1.33412981839654));
#261848=CARTESIAN_POINT('Ctrl Pts',(0.0276386165324073,-1.55525855123701,
1.33438867895905));
#261849=CARTESIAN_POINT('Ctrl Pts',(0.0344768081015319,-1.55512129285711,
1.33488213799023));
#261850=CARTESIAN_POINT('Ctrl Pts',(0.0377371430473449,-1.5550455922745,
1.33511684100221));
#261851=CARTESIAN_POINT('Ctrl Pts',(0.0454336231117314,-1.5548426706669,
1.33566958485374));
#261852=CARTESIAN_POINT('Ctrl Pts',(0.049869498113839,-1.55470671803476,
1.33598713792246));
#261853=CARTESIAN_POINT('Ctrl Pts',(0.0645463066209577,-1.55419401641856,
1.33703461476313));
#261854=CARTESIAN_POINT('Ctrl Pts',(0.0747843859017205,-1.55373504074466,
1.33776014691153));
#261855=CARTESIAN_POINT('Ctrl Pts',(0.0992979569339379,-1.55239321921494,
1.33948659489171));
#261856=CARTESIAN_POINT('Ctrl Pts',(0.113567523707308,-1.55141459437482,
1.34048284793426));
#261857=CARTESIAN_POINT('Ctrl Pts',(0.167120684669559,-1.54699896582576,
1.34419581403078));
#261858=CARTESIAN_POINT('Ctrl Pts',(0.206285017593711,-1.54226525313204,
1.34685881021484));
#261859=CARTESIAN_POINT('Ctrl Pts',(0.382747902410267,-1.5140929555056,
1.3587881029105));
#261860=CARTESIAN_POINT('Ctrl Pts',(0.516688037151767,-1.47377321780688,
1.36771260038848));
#261861=CARTESIAN_POINT('Ctrl Pts',(0.648963766604163,-1.41366991402574,
1.37766025153078));
#261862=CARTESIAN_POINT('Ctrl Pts',(0.654437904623114,-1.41114408322439,
1.3780739488346));
#261863=CARTESIAN_POINT('Ctrl Pts',(0.660733584551883,-1.40819467169567,
1.37855214045405));
#261864=CARTESIAN_POINT('Ctrl Pts',(0.661569655888474,-1.40780207896875,
1.37861569382389));
#261865=CARTESIAN_POINT('Ctrl Pts',(0.685429427676946,-1.3965723341067,
1.38043078712612));
#261866=CARTESIAN_POINT('Ctrl Pts',(0.708182882465273,-1.38517315222568,
1.38219930606845));
#261867=CARTESIAN_POINT('Ctrl Pts',(0.738879068239845,-1.36884073468109,
1.38464248585462));
#261868=CARTESIAN_POINT('Ctrl Pts',(0.747072966504511,-1.36438601955547,
1.3853003535355));
#261869=CARTESIAN_POINT('Ctrl Pts',(0.760046894423242,-1.35718067175175,
1.3863513505034));
#261870=CARTESIAN_POINT('Ctrl Pts',(0.764853308343698,-1.3544777860084,
1.38674277496615));
#261871=CARTESIAN_POINT('Ctrl Pts',(0.774687543373235,-1.34887847038192,
1.38754796251197));
#261872=CARTESIAN_POINT('Ctrl Pts',(0.779713726449343,-1.34597935378947,
1.38796181734543));
#261873=CARTESIAN_POINT('Ctrl Pts',(0.791307006733607,-1.33920558918164,
1.3889218864577));
#261874=CARTESIAN_POINT('Ctrl Pts',(0.797862020718454,-1.33531066836961,
1.38946882777489));
#261875=CARTESIAN_POINT('Ctrl Pts',(0.81855282885753,-1.32280966102261,
1.39120849553862));
#261876=CARTESIAN_POINT('Ctrl Pts',(0.832579620378503,-1.31402635793779,
1.39240765564676));
#261877=CARTESIAN_POINT('Ctrl Pts',(0.902242356786235,-1.26884170102616,
1.39846573704371));
#261878=CARTESIAN_POINT('Ctrl Pts',(0.955636517604137,-1.22912858624269,
1.4034467655288));
#261879=CARTESIAN_POINT('Ctrl Pts',(1.07772192882836,-1.12555027518561,
1.41567175539374));
#261880=CARTESIAN_POINT('Ctrl Pts',(1.14350548523559,-1.05865076097756,
1.42299202352713));
#261881=CARTESIAN_POINT('Ctrl Pts',(1.23840459474117,-0.942908036495083,
1.43451282115944));
#261882=CARTESIAN_POINT('Ctrl Pts',(1.27157681244589,-0.89767226346097,
1.43877428982523));
#261883=CARTESIAN_POINT('Ctrl Pts',(1.30657310116219,-0.844102963157296,
1.4434758864979));
#261884=CARTESIAN_POINT('Ctrl Pts',(1.31085768188657,-0.837433714417966,
1.44405537460208));
#261885=CARTESIAN_POINT('Ctrl Pts',(1.3172551840952,-0.827306139236497,
1.44492622033476));
#261886=CARTESIAN_POINT('Ctrl Pts',(1.3194057954242,-0.823871965814587,
1.44521994484258));
#261887=CARTESIAN_POINT('Ctrl Pts',(1.3232398344969,-0.817696117369825,
1.44574529724105));
#261888=CARTESIAN_POINT('Ctrl Pts',(1.32492819013956,-0.814957601094243,
1.44597724209685));
#261889=CARTESIAN_POINT('Ctrl Pts',(1.32859703020646,-0.808965197342127,
1.44648258006633));
#261890=CARTESIAN_POINT('Ctrl Pts',(1.33057406037041,-0.805709271322412,
1.44675574787305));
#261891=CARTESIAN_POINT('Ctrl Pts',(1.33615953519471,-0.796434051337235,
1.44753004415994));
#261892=CARTESIAN_POINT('Ctrl Pts',(1.33973929443662,-0.790397450350637,
1.44802935450888));
#261893=CARTESIAN_POINT('Ctrl Pts',(1.36290014509709,-0.750731493259817,
1.45128154703851));
#261894=CARTESIAN_POINT('Ctrl Pts',(1.38125625693912,-0.716398193365103,
1.45396217975873));
#261895=CARTESIAN_POINT('Ctrl Pts',(1.44911985158528,-0.577136554520089,
1.46445757801275));
#261896=CARTESIAN_POINT('Ctrl Pts',(1.48811314193984,-0.467502050116821,
1.47191792241935));
#261897=CARTESIAN_POINT('Ctrl Pts',(1.53023523057209,-0.287563374418997,
1.48423302958865));
#261898=CARTESIAN_POINT('Ctrl Pts',(1.54145243529622,-0.21962462648746,
1.48889255798115));
#261899=CARTESIAN_POINT('Ctrl Pts',(1.54926363249993,-0.13963137424281,
1.49450878233733));
#261900=CARTESIAN_POINT('Ctrl Pts',(1.55026150334837,-0.128078031365681,
1.49532292982615));
#261901=CARTESIAN_POINT('Ctrl Pts',(1.55167789447218,-0.109222011713531,
1.49665709768085));
#261902=CARTESIAN_POINT('Ctrl Pts',(1.5521742583683,-0.10192548454021,1.49717468526005));
#261903=CARTESIAN_POINT('Ctrl Pts',(1.55296969674995,-0.0888739452898519,
1.49810299123497));
#261904=CARTESIAN_POINT('Ctrl Pts',(1.55328828124881,-0.0831202194113083,
1.49851309238664));
#261905=CARTESIAN_POINT('Ctrl Pts',(1.55389532834674,-0.0709300297506218,
1.49938384468053));
#261906=CARTESIAN_POINT('Ctrl Pts',(1.55417578578885,-0.064493295309973,
1.49984473803982));
#261907=CARTESIAN_POINT('Ctrl Pts',(1.55481823282952,-0.047291873891471,
1.50107949860333));
#261908=CARTESIAN_POINT('Ctrl Pts',(1.55510841098274,-0.036525028762168,
1.50185558925807));
#261909=CARTESIAN_POINT('Ctrl Pts',(1.55598557209485,0.0164421218369805,
1.50569010319984));
#261910=CARTESIAN_POINT('Ctrl Pts',(1.55496665518451,0.0586473530331255,
1.508797915883));
#261911=CARTESIAN_POINT('Ctrl Pts',(1.54219579600323,0.255394608700159,
1.52354541272151));
#261912=CARTESIAN_POINT('Ctrl Pts',(1.50911166648446,0.407629890403857,
1.53582378684819));
#261913=CARTESIAN_POINT('Ctrl Pts',(1.44786201765657,0.568843929349383,
1.54887888437283));
#261914=CARTESIAN_POINT('Ctrl Pts',(1.44135635704005,0.585132196267513,
1.55019705218249));
#261915=CARTESIAN_POINT('Ctrl Pts',(1.4345766830264,0.601306902103224,1.55150291788058));
#261916=CARTESIAN_POINT('Origin',(0.,0.,-1.29405622560371));
#261917=CARTESIAN_POINT('',(1.43457668658422,0.601306893615097,2.38964409368597));
#261918=CARTESIAN_POINT('',(1.43457657517513,0.6013071594109,2.25008958711186));
#261919=CARTESIAN_POINT('',(1.43457668357355,0.601306900797845,-1.29405622560371));
#261920=CARTESIAN_POINT('',(-1.5555004206877,-1.78579724124609E-5,1.99259704609395));
#261921=CARTESIAN_POINT('Ctrl Pts',(1.43457668658422,0.601306893615097,
2.38964409368597));
#261922=CARTESIAN_POINT('Ctrl Pts',(1.43678610929841,0.596035731168367,
2.38924668108184));
#261923=CARTESIAN_POINT('Ctrl Pts',(1.43896666337616,0.59075195326909,2.38884831054688));
#261924=CARTESIAN_POINT('Ctrl Pts',(1.44553656171715,0.574579937460446,
2.38762886929659));
#261925=CARTESIAN_POINT('Ctrl Pts',(1.44983152026026,0.563654686304953,
2.38680484467955));
#261926=CARTESIAN_POINT('Ctrl Pts',(1.45659918601195,0.545850235705615,
2.38546108115142));
#261927=CARTESIAN_POINT('Ctrl Pts',(1.4591478381475,0.539000233439249,2.38494387871763));
#261928=CARTESIAN_POINT('Ctrl Pts',(1.46359794946082,0.526776783272011,
2.38402046400456));
#261929=CARTESIAN_POINT('Ctrl Pts',(1.46551834029303,0.521410327613212,
2.38361488891971));
#261930=CARTESIAN_POINT('Ctrl Pts',(1.46950291902844,0.51007965365925,2.38275814456882));
#261931=CARTESIAN_POINT('Ctrl Pts',(1.47156038367609,0.504113198732518,
2.38230676137573));
#261932=CARTESIAN_POINT('Ctrl Pts',(1.47691373036322,0.488276927815953,
2.38110795487899));
#261933=CARTESIAN_POINT('Ctrl Pts',(1.48014693243878,0.478386427255533,
2.38035848671231));
#261934=CARTESIAN_POINT('Ctrl Pts',(1.49498575289909,0.43140285306159,2.37679401952542));
#261935=CARTESIAN_POINT('Ctrl Pts',(1.50529671741136,0.393918922890391,
2.37393737433536));
#261936=CARTESIAN_POINT('Ctrl Pts',(1.54847768374483,0.210302185578863,
2.35986792856474));
#261937=CARTESIAN_POINT('Ctrl Pts',(1.5615235007313,0.0603330201707153,
2.34804286310328));
#261938=CARTESIAN_POINT('Ctrl Pts',(1.55069848759065,-0.128256212374082,
2.33364373382289));
#261939=CARTESIAN_POINT('Ctrl Pts',(1.54697570840915,-0.167278970863317,
2.33069680404698));
#261940=CARTESIAN_POINT('Ctrl Pts',(1.54090371940103,-0.212696879512762,
2.32733457800986));
#261941=CARTESIAN_POINT('Ctrl Pts',(1.53998282667357,-0.219264982976112,
2.32685002305705));
#261942=CARTESIAN_POINT('Ctrl Pts',(1.53842526391811,-0.229879827650328,
2.32606984496707));
#261943=CARTESIAN_POINT('Ctrl Pts',(1.53781458206121,-0.233930203403862,
2.32577283670139));
#261944=CARTESIAN_POINT('Ctrl Pts',(1.53670082221325,-0.241124384585699,
2.32524657931238));
#261945=CARTESIAN_POINT('Ctrl Pts',(1.53620408593838,-0.244269099314983,
2.32501698094244));
#261946=CARTESIAN_POINT('Ctrl Pts',(1.53511107999725,-0.251053427668052,
2.32452260811069));
#261947=CARTESIAN_POINT('Ctrl Pts',(1.53451152127388,-0.254692448490967,
2.3242580215438));
#261948=CARTESIAN_POINT('Ctrl Pts',(1.53280456371452,-0.264827961491769,
2.32352263929779));
#261949=CARTESIAN_POINT('Ctrl Pts',(1.53166879664065,-0.271319703048497,
2.32305341053326));
#261950=CARTESIAN_POINT('Ctrl Pts',(1.52481143993769,-0.30909857269985,
2.32033205082952));
#261951=CARTESIAN_POINT('Ctrl Pts',(1.51817208260253,-0.340214272863052,
2.31812797496159));
#261952=CARTESIAN_POINT('Ctrl Pts',(1.47581071834769,-0.51264514435571,
2.30601115615178));
#261953=CARTESIAN_POINT('Ctrl Pts',(1.42131820898492,-0.64860250446206,
2.29676096859634));
#261954=CARTESIAN_POINT('Ctrl Pts',(1.32419373939082,-0.817623560151233,
2.28361163953145));
#261955=CARTESIAN_POINT('Ctrl Pts',(1.29769404248287,-0.859061520411838,
2.28024426477329));
#261956=CARTESIAN_POINT('Ctrl Pts',(1.26260409914782,-0.908594783141957,
2.27599536734309));
#261957=CARTESIAN_POINT('Ctrl Pts',(1.25582449039136,-0.917942496977848,
2.27518327465635));
#261958=CARTESIAN_POINT('Ctrl Pts',(1.24498915198541,-0.932537520370693,
2.27389855692975));
#261959=CARTESIAN_POINT('Ctrl Pts',(1.24100276469926,-0.937835993657894,
2.27342862352172));
#261960=CARTESIAN_POINT('Ctrl Pts',(1.23358271634179,-0.947568138914866,
2.27255880197799));
#261961=CARTESIAN_POINT('Ctrl Pts',(1.23015870603126,-0.952009061095374,
2.27215929765912));
#261962=CARTESIAN_POINT('Ctrl Pts',(1.22251650452936,-0.961810884728172,
2.27127169829564));
#261963=CARTESIAN_POINT('Ctrl Pts',(1.21828693224431,-0.967162721473227,
2.2707831566448));
#261964=CARTESIAN_POINT('Ctrl Pts',(1.2060445395556,-0.98244574969127,2.26937664268453));
#261965=CARTESIAN_POINT('Ctrl Pts',(1.19794470160068,-0.99230618073998,
2.26845519522419));
#261966=CARTESIAN_POINT('Ctrl Pts',(1.13358226689048,-1.06872191575334,
2.26120185383137));
#261967=CARTESIAN_POINT('Ctrl Pts',(1.0719482159986,-1.13052961366926,2.25464533705512));
#261968=CARTESIAN_POINT('Ctrl Pts',(0.935154014689978,-1.24641949876183,
2.24086439806583));
#261969=CARTESIAN_POINT('Ctrl Pts',(0.859678980927541,-1.29962543300971,
2.23364978730705));
#261970=CARTESIAN_POINT('Ctrl Pts',(0.765218397286501,-1.35436720140672,
2.22530153127022));
#261971=CARTESIAN_POINT('Ctrl Pts',(0.750358554990978,-1.36265615309226,
2.22400726819537));
#261972=CARTESIAN_POINT('Ctrl Pts',(0.71045926054688,-1.3840616792585,2.22058743254789));
#261973=CARTESIAN_POINT('Ctrl Pts',(0.685191622707292,-1.39674328315993,
2.21847850344823));
#261974=CARTESIAN_POINT('Ctrl Pts',(0.653617823016518,-1.41152664984378,
2.21592428952644));
#261975=CARTESIAN_POINT('Ctrl Pts',(0.647627382874243,-1.41428516180637,
2.21544321704364));
#261976=CARTESIAN_POINT('Ctrl Pts',(0.638222636378641,-1.41854362651684,
2.21469367173399));
#261977=CARTESIAN_POINT('Ctrl Pts',(0.634820266992627,-1.42006949947069,
2.21442367204616));
#261978=CARTESIAN_POINT('Ctrl Pts',(0.628798046681575,-1.42274433742558,
2.21394786686686));
#261979=CARTESIAN_POINT('Ctrl Pts',(0.626180524578857,-1.4238983054019,
2.21374176152263));
#261980=CARTESIAN_POINT('Ctrl Pts',(0.620005327180566,-1.42660039860182,
2.21325716122959));
#261981=CARTESIAN_POINT('Ctrl Pts',(0.616445034239869,-1.42814243815917,
2.2129790388802));
#261982=CARTESIAN_POINT('Ctrl Pts',(0.605994470590375,-1.43262244077089,
2.21216627941702));
#261983=CARTESIAN_POINT('Ctrl Pts',(0.599088572995391,-1.43552403110779,
2.21163378624781));
#261984=CARTESIAN_POINT('Ctrl Pts',(0.541806936928805,-1.45910618477904,
2.20725263587288));
#261985=CARTESIAN_POINT('Ctrl Pts',(0.490391329979952,-1.47718093741309,
2.20354693949995));
#261986=CARTESIAN_POINT('Ctrl Pts',(0.308130978808746,-1.53068309418289,
2.19083910864413));
#261987=CARTESIAN_POINT('Ctrl Pts',(0.17371079658686,-1.55169632297072,
2.18216175852264));
#261988=CARTESIAN_POINT('Ctrl Pts',(0.00120546028995934,-1.55594120670977,
2.17041158087723));
#261989=CARTESIAN_POINT('Ctrl Pts',(-0.0358720376666462,-1.55552798529379,
2.16785440830424));
#261990=CARTESIAN_POINT('Ctrl Pts',(-0.0835559209501208,-1.55329086795311,
2.16450791626522));
#261991=CARTESIAN_POINT('Ctrl Pts',(-0.0942091586292589,-1.55268114458328,
2.16375657035142));
#261992=CARTESIAN_POINT('Ctrl Pts',(-0.111210263763817,-1.55153250058144,
2.16255124547342));
#261993=CARTESIAN_POINT('Ctrl Pts',(-0.117562694432409,-1.55106409726087,
2.16209947646046));
#261994=CARTESIAN_POINT('Ctrl Pts',(-0.12901495873897,-1.55014889513055,
2.16128241086261));
#261995=CARTESIAN_POINT('Ctrl Pts',(-0.134115832388011,-1.54971590912812,
2.16091755257312));
#261996=CARTESIAN_POINT('Ctrl Pts',(-0.146114833788221,-1.54863769343651,
2.16005703117796));
#261997=CARTESIAN_POINT('Ctrl Pts',(-0.153010922460385,-1.54797154525459,
2.15956071864182));
#261998=CARTESIAN_POINT('Ctrl Pts',(-0.173104313523285,-1.5458949845325,
2.15810934853828));
#261999=CARTESIAN_POINT('Ctrl Pts',(-0.18628800127005,-1.54436173445071,
2.15715046185232));
#262000=CARTESIAN_POINT('Ctrl Pts',(-0.314728477263464,-1.52775570111333,
2.14774150665099));
#262001=CARTESIAN_POINT('Ctrl Pts',(-0.427947542120583,-1.49998035679443,
2.13887672629642));
#262002=CARTESIAN_POINT('Ctrl Pts',(-0.630096265997753,-1.42562263696625,
2.12218677420738));
#262003=CARTESIAN_POINT('Ctrl Pts',(-0.719718212567711,-1.38254501764455,
2.11444849765602));
#262004=CARTESIAN_POINT('Ctrl Pts',(-0.814878654287223,-1.32502692653596,
2.10621687176514));
#262005=CARTESIAN_POINT('Ctrl Pts',(-0.825053000972391,-1.31871571852921,
2.10533678675925));
#262006=CARTESIAN_POINT('Ctrl Pts',(-0.839158840664227,-1.30973860991628,
2.10411772407558));
#262007=CARTESIAN_POINT('Ctrl Pts',(-0.843152190556915,-1.30717143914941,
2.10377273335587));
#262008=CARTESIAN_POINT('Ctrl Pts',(-0.849865099423164,-1.30281240720588,
2.10319308925342));
#262009=CARTESIAN_POINT('Ctrl Pts',(-0.852590862541924,-1.30103023686938,
2.10295780792959));
#262010=CARTESIAN_POINT('Ctrl Pts',(-0.857793811955234,-1.29760504843669,
2.10250888922487));
#262011=CARTESIAN_POINT('Ctrl Pts',(-0.860271918645518,-1.29596346860348,
2.10229515591094));
#262012=CARTESIAN_POINT('Ctrl Pts',(-0.866360056846332,-1.29190532686278,
2.10177022300406));
#262013=CARTESIAN_POINT('Ctrl Pts',(-0.869964729811259,-1.28948070624696,
2.10145955972542));
#262014=CARTESIAN_POINT('Ctrl Pts',(-0.882805769328071,-1.28076504829234,
2.10035319022252));
#262015=CARTESIAN_POINT('Ctrl Pts',(-0.891984735415166,-1.27438941699862,
2.0995629277965));
#262016=CARTESIAN_POINT('Ctrl Pts',(-0.945887088008152,-1.23608155805066,
2.09492050776294));
#262017=CARTESIAN_POINT('Ctrl Pts',(-0.988966929288186,-1.20189262821392,
2.09120263997248));
#262018=CARTESIAN_POINT('Ctrl Pts',(-1.1069636989661,-1.0975979403738,2.08070607756059));
#262019=CARTESIAN_POINT('Ctrl Pts',(-1.17687619950312,-1.02227833783407,
2.07407380692125));
#262020=CARTESIAN_POINT('Ctrl Pts',(-1.27561529786001,-0.892232060693595,
2.06314391828747));
#262021=CARTESIAN_POINT('Ctrl Pts',(-1.30948804563383,-0.84173158121097,
2.05900941019903));
#262022=CARTESIAN_POINT('Ctrl Pts',(-1.34599267974516,-0.779749310318439,
2.0539798148085));
#262023=CARTESIAN_POINT('Ctrl Pts',(-1.35156298258034,-0.770053747148933,
2.0531944003065));
#262024=CARTESIAN_POINT('Ctrl Pts',(-1.36051819034682,-0.75406994874633,
2.05190130437675));
#262025=CARTESIAN_POINT('Ctrl Pts',(-1.36396524770807,-0.747816845115493,
2.05139585044705));
#262026=CARTESIAN_POINT('Ctrl Pts',(-1.37007758263689,-0.736545957316435,
2.05048543989793));
#262027=CARTESIAN_POINT('Ctrl Pts',(-1.37275866916872,-0.73153685097631,
2.05008105343884));
#262028=CARTESIAN_POINT('Ctrl Pts',(-1.37840614616144,-0.720845223401461,
2.04921833292539));
#262029=CARTESIAN_POINT('Ctrl Pts',(-1.38136496417427,-0.715158844841251,
2.04875974091322));
#262030=CARTESIAN_POINT('Ctrl Pts',(-1.38923911182671,-0.699794796298017,
2.04752123586148));
#262031=CARTESIAN_POINT('Ctrl Pts',(-1.39408835039792,-0.690083855001626,
2.04673903020258));
#262032=CARTESIAN_POINT('Ctrl Pts',(-1.41826233301869,-0.640378913816671,
2.04273761372666));
#262033=CARTESIAN_POINT('Ctrl Pts',(-1.43596738234061,-0.599624998511741,
2.03946331280328));
#262034=CARTESIAN_POINT('Ctrl Pts',(-1.48248932051099,-0.478613517406358,
2.02974938906059));
#262035=CARTESIAN_POINT('Ctrl Pts',(-1.50648069938332,-0.396683811319334,
2.02317447377145));
#262036=CARTESIAN_POINT('Ctrl Pts',(-1.54209589229059,-0.223431707399583,
2.00945799042065));
#262037=CARTESIAN_POINT('Ctrl Pts',(-1.55258247384778,-0.132185124857028,
2.00233764832531));
#262038=CARTESIAN_POINT('Ctrl Pts',(-1.55521973276162,-0.0310229204717739,
1.9948613494224));
#262039=CARTESIAN_POINT('Ctrl Pts',(-1.555380450164,-0.0215059495709297,
1.99416218843355));
#262040=CARTESIAN_POINT('Ctrl Pts',(-1.55547726732396,-0.00894362252634021,
1.99324532762615));
#262041=CARTESIAN_POINT('Ctrl Pts',(-1.555491792201,-0.00589935211516795,
1.9930236087652));
#262042=CARTESIAN_POINT('Ctrl Pts',(-1.55549911544723,-0.00190944265546296,
1.99273364645012));
#262043=CARTESIAN_POINT('Ctrl Pts',(-1.55549998878868,-0.000963856086597575,
1.99266497327083));
#262044=CARTESIAN_POINT('Ctrl Pts',(-1.55549999989275,-1.82662448845978E-5,
1.99259634653107));
#262045=CARTESIAN_POINT('Ctrl Pts',(-1.55549999989689,-1.79106135396723E-5,
1.99259632072092));
#262046=CARTESIAN_POINT('Ctrl Pts',(-1.55550001419639,0.00122397189078814,
1.99250619038201));
#262047=CARTESIAN_POINT('Ctrl Pts',(-1.55549854125183,0.0024658604726738,
1.99241614011376));
#262048=CARTESIAN_POINT('Ctrl Pts',(-1.55548839673815,0.00672173958508773,
1.99210782204593));
#262049=CARTESIAN_POINT('Ctrl Pts',(-1.55547245236403,0.00973573472252594,
1.99188995188346));
#262050=CARTESIAN_POINT('Ctrl Pts',(-1.5554216770202,0.0159302645811493,
1.99144318405574));
#262051=CARTESIAN_POINT('Ctrl Pts',(-1.55538585119196,0.0191107512606468,
1.99121434951327));
#262052=CARTESIAN_POINT('Ctrl Pts',(-1.55527764779643,0.0266605291434597,
1.99067241280553));
#262053=CARTESIAN_POINT('Ctrl Pts',(-1.55519661253696,0.0310297140168148,
1.99035979047689));
#262054=CARTESIAN_POINT('Ctrl Pts',(-1.55487169938468,0.0453034971727461,
1.9893415923815));
#262055=CARTESIAN_POINT('Ctrl Pts',(-1.55455160002381,0.0552063828148327,
1.98864008556239));
#262056=CARTESIAN_POINT('Ctrl Pts',(-1.55371304455279,0.0752234716368273,
1.98723077622798));
#262057=CARTESIAN_POINT('Ctrl Pts',(-1.5531903950852,0.0853370074145378,
1.98652321169287));
#262058=CARTESIAN_POINT('Ctrl Pts',(-1.55101132197374,0.120783184334668,
1.98405676230046));
#262059=CARTESIAN_POINT('Ctrl Pts',(-1.54883349697656,0.146080987139074,
1.98232054345841));
#262060=CARTESIAN_POINT('Ctrl Pts',(-1.52946455362371,0.320875943342886,
1.97042121525242));
#262061=CARTESIAN_POINT('Ctrl Pts',(-1.49127930262326,0.467242146655841,
1.96087082834798));
#262062=CARTESIAN_POINT('Ctrl Pts',(-1.41795514707373,0.640631973628924,
1.94805158680147));
#262063=CARTESIAN_POINT('Ctrl Pts',(-1.40198728668171,0.674861004225701,
1.9454461799346));
#262064=CARTESIAN_POINT('Ctrl Pts',(-1.38009638921,0.717649252686303,1.9420748319237));
#262065=CARTESIAN_POINT('Ctrl Pts',(-1.37531073844183,0.72677840984685,
1.94134874078717));
#262066=CARTESIAN_POINT('Ctrl Pts',(-1.36745937970235,0.74140046830073,
1.94017443625196));
#262067=CARTESIAN_POINT('Ctrl Pts',(-1.36445040457722,0.746923624521823,
1.93972823462468));
#262068=CARTESIAN_POINT('Ctrl Pts',(-1.35864854721157,0.757421229779946,
1.93887503909602));
#262069=CARTESIAN_POINT('Ctrl Pts',(-1.35586162734086,0.7623988720296,1.93846826339771));
#262070=CARTESIAN_POINT('Ctrl Pts',(-1.3494217067841,0.773754046179482,
1.9375351592846));
#262071=CARTESIAN_POINT('Ctrl Pts',(-1.3457507850193,0.780121200777997,
1.93700819278008));
#262072=CARTESIAN_POINT('Ctrl Pts',(-1.33603076072164,0.796707650176765,
1.93562545575384));
#262073=CARTESIAN_POINT('Ctrl Pts',(-1.32990961254919,0.806883933006071,
1.93476709137393));
#262074=CARTESIAN_POINT('Ctrl Pts',(-1.26940322177066,0.904915448829829,
1.9263986265754));
#262075=CARTESIAN_POINT('Ctrl Pts',(-1.20651956868282,0.987197473210816,
1.91856558891341));
#262076=CARTESIAN_POINT('Ctrl Pts',(-1.08510869471353,1.11698719679562,
1.90482909823418));
#262077=CARTESIAN_POINT('Ctrl Pts',(-1.0304200461595,1.16762843184032,1.8990223214414));
#262078=CARTESIAN_POINT('Ctrl Pts',(-0.948527679079825,1.23320890041879,
1.89099589884613));
#262079=CARTESIAN_POINT('Ctrl Pts',(-0.924184084959288,1.25155622552125,
1.88868566335576));
#262080=CARTESIAN_POINT('Ctrl Pts',(-0.884704823860423,1.27953049176129,
1.88507468077004));
#262081=CARTESIAN_POINT('Ctrl Pts',(-0.869915568752658,1.28963090942132,
1.88375087845846));
#262082=CARTESIAN_POINT('Ctrl Pts',(-0.851551850914984,1.30171282680102,
1.88214527982586));
#262083=CARTESIAN_POINT('Ctrl Pts',(-0.848140521747118,1.3039380716193,
1.88184860630438));
#262084=CARTESIAN_POINT('Ctrl Pts',(-0.84157321761236,1.30818531455725,
1.8812805707));
#262085=CARTESIAN_POINT('Ctrl Pts',(-0.838418602781028,1.31020935164603,
1.88100907925787));
#262086=CARTESIAN_POINT('Ctrl Pts',(-0.832630539148359,1.31389357482074,
1.88051348643079));
#262087=CARTESIAN_POINT('Ctrl Pts',(-0.829999428162655,1.31555725469188,
1.88028916042363));
#262088=CARTESIAN_POINT('Ctrl Pts',(-0.824071527267918,1.31928066702593,
1.87978589619794));
#262089=CARTESIAN_POINT('Ctrl Pts',(-0.82077200685949,1.32133594293423,
1.87950725195935));
#262090=CARTESIAN_POINT('Ctrl Pts',(-0.811380379494651,1.3271372480057,
1.87871820931261));
#262091=CARTESIAN_POINT('Ctrl Pts',(-0.805269988564278,1.33085372825764,
1.87820969243765));
#262092=CARTESIAN_POINT('Ctrl Pts',(-0.766455829364956,1.35409618904179,
1.87500861558817));
#262093=CARTESIAN_POINT('Ctrl Pts',(-0.733066475141972,1.37245953278343,
1.87238479674321));
#262094=CARTESIAN_POINT('Ctrl Pts',(-0.56645380388515,1.45627463095802,
1.8597461301558));
#262095=CARTESIAN_POINT('Ctrl Pts',(-0.425009595465675,1.50365518876915,
1.85032423358379));
#262096=CARTESIAN_POINT('Ctrl Pts',(-0.238621175762419,1.53763571528676,
1.83745759292732));
#262097=CARTESIAN_POINT('Ctrl Pts',(-0.197985151011992,1.54339399908261,
1.83463214355934));
#262098=CARTESIAN_POINT('Ctrl Pts',(-0.146637237718799,1.54860901894201,
1.83101347968691));
#262099=CARTESIAN_POINT('Ctrl Pts',(-0.136092201497207,1.54957132003462,
1.8302678219552));
#262100=CARTESIAN_POINT('Ctrl Pts',(-0.119207433701079,1.55093848412426,
1.82906948443873));
#262101=CARTESIAN_POINT('Ctrl Pts',(-0.112873483647187,1.55141231408734,
1.82861896930488));
#262102=CARTESIAN_POINT('Ctrl Pts',(-0.100858842132922,1.55223713915853,
1.82776245321388));
#262103=CARTESIAN_POINT('Ctrl Pts',(-0.0951787643389158,1.55259577593654,
1.82735669865388));
#262104=CARTESIAN_POINT('Ctrl Pts',(-0.0822723549671218,1.55333958850972,
1.82643279439289));
#262105=CARTESIAN_POINT('Ctrl Pts',(-0.0750450926790592,1.55370552177986,
1.82591405151677));
#262106=CARTESIAN_POINT('Ctrl Pts',(-0.056327483516959,1.5545223362645,
1.82456687443632));
#262107=CARTESIAN_POINT('Ctrl Pts',(-0.0448344048639791,1.55489624807369,
1.8237360593247));
#262108=CARTESIAN_POINT('Ctrl Pts',(0.0363500978597772,1.55663664853768,
1.81784067734403));
#262109=CARTESIAN_POINT('Ctrl Pts',(0.106049312290989,1.55344450346363,
1.81263499302348));
#262110=CARTESIAN_POINT('Ctrl Pts',(0.315395539172179,1.52970185517637,
1.79656972815335));
#262111=CARTESIAN_POINT('Ctrl Pts',(0.452678852057619,1.49483838672386,
1.78539095311863));
#262112=CARTESIAN_POINT('Ctrl Pts',(0.59369970741916,1.43778467629534,1.77405784404128));
#262113=CARTESIAN_POINT('Ctrl Pts',(0.603972194002272,1.43349981667712,
1.77323366411187));
#262114=CARTESIAN_POINT('Ctrl Pts',(0.621925383880897,1.42578392677025,
1.77179671640506));
#262115=CARTESIAN_POINT('Ctrl Pts',(0.629625777317752,1.42240021722516,
1.77118152167332));
#262116=CARTESIAN_POINT('Ctrl Pts',(0.64100733787043,1.41728838715945,1.77027431798438));
#262117=CARTESIAN_POINT('Ctrl Pts',(0.644709614890929,1.41560810009983,
1.76997954572683));
#262118=CARTESIAN_POINT('Ctrl Pts',(0.65129681426246,1.41258728182764,1.76945572138618));
#262119=CARTESIAN_POINT('Ctrl Pts',(0.654184246032052,1.41125240193651,
1.76922633270959));
#262120=CARTESIAN_POINT('Ctrl Pts',(0.660429662715938,1.40834181527724,
1.7687306669433));
#262121=CARTESIAN_POINT('Ctrl Pts',(0.66378610875806,1.40676295467731,1.76846458718092));
#262122=CARTESIAN_POINT('Ctrl Pts',(0.67301685914613,1.40238044915316,1.76773357575377));
#262123=CARTESIAN_POINT('Ctrl Pts',(0.678879353614273,1.39955187259324,
1.76727014596271));
#262124=CARTESIAN_POINT('Ctrl Pts',(0.709072087295222,1.38474991746273,
1.76488686325054));
#262125=CARTESIAN_POINT('Ctrl Pts',(0.733105794834983,1.37217771734653,
1.76300136101093));
#262126=CARTESIAN_POINT('Ctrl Pts',(0.77266394948833,1.35014827679315,1.75989673219746));
#262127=CARTESIAN_POINT('Ctrl Pts',(0.7883722841313,1.34103659188896,1.75866357564278));
#262128=CARTESIAN_POINT('Ctrl Pts',(0.882929419251218,1.28395245030337,
1.75121624498494));
#262129=CARTESIAN_POINT('Ctrl Pts',(0.957543059242679,1.22931347021834,
1.74522565333123));
#262130=CARTESIAN_POINT('Ctrl Pts',(1.09234809824048,1.11083473925866,1.73335461401746));
#262131=CARTESIAN_POINT('Ctrl Pts',(1.15285859151246,1.04789875654755,1.72750663759628));
#262132=CARTESIAN_POINT('Ctrl Pts',(1.21581750678459,0.970325143893713,
1.72052444175251));
#262133=CARTESIAN_POINT('Ctrl Pts',(1.22373672547135,0.960318439021049,
1.71962795593485));
#262134=CARTESIAN_POINT('Ctrl Pts',(1.23569882941055,0.944814895266383,
1.71824473691866));
#262135=CARTESIAN_POINT('Ctrl Pts',(1.23983029878132,0.939386827064705,
1.71776150360598));
#262136=CARTESIAN_POINT('Ctrl Pts',(1.24729275858127,0.929447400600994,
1.71687846043688));
#262137=CARTESIAN_POINT('Ctrl Pts',(1.25063532968746,0.924944845231504,
1.71647911170693));
#262138=CARTESIAN_POINT('Ctrl Pts',(1.25787689958614,0.915079187808012,
1.71560548311861));
#262139=CARTESIAN_POINT('Ctrl Pts',(1.26176608340618,0.909709053884518,
1.71513083375291));
#262140=CARTESIAN_POINT('Ctrl Pts',(1.27233378375205,0.894919172739021,
1.71382591642106));
#262141=CARTESIAN_POINT('Ctrl Pts',(1.2789418120262,0.88544983544469,1.71299297838618));
#262142=CARTESIAN_POINT('Ctrl Pts',(1.31312552045382,0.835283346940942,
1.7085925973663));
#262143=CARTESIAN_POINT('Ctrl Pts',(1.33886288296008,0.793373868182999,
1.70495740101626));
#262144=CARTESIAN_POINT('Ctrl Pts',(1.38923264894595,0.701903118062805,
1.69710031627947));
#262145=CARTESIAN_POINT('Ctrl Pts',(1.41326210986097,0.652158504367882,
1.69287163113236));
#262146=CARTESIAN_POINT('Ctrl Pts',(1.43457689162107,0.601306404445218,
1.68861155768856));
#262147=CARTESIAN_POINT('',(-1.55549938654046,-0.00138147466141999,1.85539356957841));
#262148=CARTESIAN_POINT('Ctrl Pts',(1.4345766830264,0.601306902103224,1.55150291788058));
#262149=CARTESIAN_POINT('Ctrl Pts',(1.42949793920172,0.613423589013786,
1.55248115921441));
#262150=CARTESIAN_POINT('Ctrl Pts',(1.42426542712662,0.625476549069427,
1.55345249348743));
#262151=CARTESIAN_POINT('Ctrl Pts',(1.41633033900459,0.643138661774095,
1.55487178320529));
#262152=CARTESIAN_POINT('Ctrl Pts',(1.4137462589228,0.6487992650372,1.55532603237192));
#262153=CARTESIAN_POINT('Ctrl Pts',(1.40944611972224,0.658071326022222,
1.556068884512));
#262154=CARTESIAN_POINT('Ctrl Pts',(1.40775001343898,0.661691873281577,
1.55635864851411));
#262155=CARTESIAN_POINT('Ctrl Pts',(1.40466500343922,0.668211652089188,
1.55687984476214));
#262156=CARTESIAN_POINT('Ctrl Pts',(1.40328106519625,0.671113132438782,
1.55711157102549));
#262157=CARTESIAN_POINT('Ctrl Pts',(1.40021806432876,0.677483931037409,
1.5576198891324));
#262158=CARTESIAN_POINT('Ctrl Pts',(1.39853510143924,0.680951301782332,
1.55789623606678));
#262159=CARTESIAN_POINT('Ctrl Pts',(1.39365850047321,0.6909041128148,1.55868867763136));
#262160=CARTESIAN_POINT('Ctrl Pts',(1.39043245945046,0.697373709107659,
1.55920281757204));
#262161=CARTESIAN_POINT('Ctrl Pts',(1.3672564223466,0.743051394906098,1.56282763042489));
#262162=CARTESIAN_POINT('Ctrl Pts',(1.34569387037553,0.781424593151184,
1.56584566725153));
#262163=CARTESIAN_POINT('Ctrl Pts',(1.28259567922718,0.883336705198955,
1.57392930813408));
#262164=CARTESIAN_POINT('Ctrl Pts',(1.2379930195827,0.944833370609119,1.57888734305577));
#262165=CARTESIAN_POINT('Ctrl Pts',(1.12281510440974,1.08140208053106,1.59065878281291));
#262166=CARTESIAN_POINT('Ctrl Pts',(1.04893893423033,1.15319844964057,1.59749006433035));
#262167=CARTESIAN_POINT('Ctrl Pts',(0.959168498732369,1.22463022042804,
1.60550191833294));
#262168=CARTESIAN_POINT('Ctrl Pts',(0.949721307648552,1.23197110742839,
1.60634152159061));
#262169=CARTESIAN_POINT('Ctrl Pts',(0.934276113839804,1.24368947520281,
1.6077090730623));
#262170=CARTESIAN_POINT('Ctrl Pts',(0.928329666999248,1.24813436518062,
1.60823437875882));
#262171=CARTESIAN_POINT('Ctrl Pts',(0.917701113890401,1.25596109490459,
1.60917129753163));
#262172=CARTESIAN_POINT('Ctrl Pts',(0.913031528153976,1.25935977119364,
1.6095822488111));
#262173=CARTESIAN_POINT('Ctrl Pts',(0.903162867687791,1.26645876618844,
1.6104493938483));
#262174=CARTESIAN_POINT('Ctrl Pts',(0.897959745182865,1.27015324501291,
1.61090580166129));
#262175=CARTESIAN_POINT('Ctrl Pts',(0.884142810635234,1.27983663183219,
1.61211583395515));
#262176=CARTESIAN_POINT('Ctrl Pts',(0.875491020225945,1.28577049945362,
1.61287152777009));
#262177=CARTESIAN_POINT('Ctrl Pts',(0.834492921488233,1.31328357399765,
1.61644384867149));
#262178=CARTESIAN_POINT('Ctrl Pts',(0.801407613239618,1.3337306780114,1.61930205921672));
#262179=CARTESIAN_POINT('Ctrl Pts',(0.637036195741412,1.42698888555464,
1.63339930743493));
#262180=CARTESIAN_POINT('Ctrl Pts',(0.49644928956724,1.48176788807067,1.64525271623756));
#262181=CARTESIAN_POINT('Ctrl Pts',(0.312686866350959,1.52423522319639,
1.6596225523211));
#262182=CARTESIAN_POINT('Ctrl Pts',(0.274816419531242,1.53151645114127,
1.66252053084479));
#262183=CARTESIAN_POINT('Ctrl Pts',(0.230139881534336,1.53839529596743,
1.66583737893387));
#262184=CARTESIAN_POINT('Ctrl Pts',(0.223562299561263,1.5393649190997,1.66632312995626));
#262185=CARTESIAN_POINT('Ctrl Pts',(0.212891388633283,1.54086811343609,
1.66710678251544));
#262186=CARTESIAN_POINT('Ctrl Pts',(0.20880189007726,1.54142760391925,1.66740606536487));
#262187=CARTESIAN_POINT('Ctrl Pts',(0.201515529782023,1.54239493215045,
1.66793739230427));
#262188=CARTESIAN_POINT('Ctrl Pts',(0.19831958767141,1.54280911888772,1.66816978525784));
#262189=CARTESIAN_POINT('Ctrl Pts',(0.191399234354368,1.54368412111581,
1.66867156779913));
#262190=CARTESIAN_POINT('Ctrl Pts',(0.187674439745266,1.5441413918967,1.66894075718334));
#262191=CARTESIAN_POINT('Ctrl Pts',(0.17723912503843,1.54538415598162,1.66969251809616));
#262192=CARTESIAN_POINT('Ctrl Pts',(0.170524979162174,1.5461394286817,1.67017343489546));
#262193=CARTESIAN_POINT('Ctrl Pts',(0.130503759600618,1.55037753216908,
1.67302471411423));
#262194=CARTESIAN_POINT('Ctrl Pts',(0.0970931573111436,1.55282808649424,
1.67534185874847));
#262195=CARTESIAN_POINT('Ctrl Pts',(-0.107253913315879,1.56119373741955,
1.68927255530099));
#262196=CARTESIAN_POINT('Ctrl Pts',(-0.278122108333887,1.53996374451727,
1.70002491625374));
#262197=CARTESIAN_POINT('Ctrl Pts',(-0.443325082000494,1.49098782518629,
1.71187508691197));
#262198=CARTESIAN_POINT('Ctrl Pts',(-0.444527182648,1.49062986923554,1.71196138738509));
#262199=CARTESIAN_POINT('Ctrl Pts',(-0.469993564734121,1.48301306315438,
1.71379120525399));
#262200=CARTESIAN_POINT('Ctrl Pts',(-0.494076136857859,1.47516451321403,
1.71555153770954));
#262201=CARTESIAN_POINT('Ctrl Pts',(-0.52673290763341,1.46363224530571,
1.71798512910616));
#262202=CARTESIAN_POINT('Ctrl Pts',(-0.535482390997831,1.46045387044117,
1.71864176765678));
#262203=CARTESIAN_POINT('Ctrl Pts',(-0.549365279600562,1.45526918801366,
1.71969129137074));
#262204=CARTESIAN_POINT('Ctrl Pts',(-0.554517563422742,1.45331376187195,
1.72008248044149));
#262205=CARTESIAN_POINT('Ctrl Pts',(-0.565074550062345,1.44924279836446,
1.72088754764572));
#262206=CARTESIAN_POINT('Ctrl Pts',(-0.570478014085313,1.44712431031574,
1.72130151920057));
#262207=CARTESIAN_POINT('Ctrl Pts',(-0.582821028996978,1.44220522056503,
1.72225159077979));
#262208=CARTESIAN_POINT('Ctrl Pts',(-0.589752431596045,1.43938470044253,
1.72278835320441));
#262209=CARTESIAN_POINT('Ctrl Pts',(-0.611390071788284,1.43039740297878,
1.72447429107726));
#262210=CARTESIAN_POINT('Ctrl Pts',(-0.626021575923056,1.42405459924818,
1.72562938090733));
#262211=CARTESIAN_POINT('Ctrl Pts',(-0.659917215290968,1.40873740908626,
1.72834156570365));
#262212=CARTESIAN_POINT('Ctrl Pts',(-0.679099671132186,1.39959114535965,
1.72990429881964));
#262213=CARTESIAN_POINT('Ctrl Pts',(-0.746010359930316,1.36598849205803,
1.73545590740555));
#262214=CARTESIAN_POINT('Ctrl Pts',(-0.79265113832465,1.3394622377052,1.7395110802964));
#262215=CARTESIAN_POINT('Ctrl Pts',(-0.904029186446442,1.26826088489775,
1.74964176990572));
#262216=CARTESIAN_POINT('Ctrl Pts',(-0.96692966888749,1.22098343534443,
1.75576913779383));
#262217=CARTESIAN_POINT('Ctrl Pts',(-1.07353906818084,1.12742932829995,
1.76671717593721));
#262218=CARTESIAN_POINT('Ctrl Pts',(-1.11850902213156,1.0828308649186,1.77154788201603));
#262219=CARTESIAN_POINT('Ctrl Pts',(-1.16597338339633,1.02963607527253,
1.77678706172197));
#262220=CARTESIAN_POINT('Ctrl Pts',(-1.17125884182497,1.0236196124858,1.77737257427929));
#262221=CARTESIAN_POINT('Ctrl Pts',(-1.17915976994911,1.01448462097367,
1.77825066547507));
#262222=CARTESIAN_POINT('Ctrl Pts',(-1.18180974435766,1.01139633103077,
1.77854566842986));
#262223=CARTESIAN_POINT('Ctrl Pts',(-1.18653373032254,1.00584706292034,
1.77907238458635));
#262224=CARTESIAN_POINT('Ctrl Pts',(-1.18861224342836,1.00339002517113,
1.77930442209405));
#262225=CARTESIAN_POINT('Ctrl Pts',(-1.19312553998957,0.998021093069249,
1.77980889308389));
#262226=CARTESIAN_POINT('Ctrl Pts',(-1.1955572930282,0.99510673613754,1.78008110723755));
#262227=CARTESIAN_POINT('Ctrl Pts',(-1.20241453719153,0.986827188448362,
1.78084997135814));
#262228=CARTESIAN_POINT('Ctrl Pts',(-1.20681482330775,0.981441086455878,
1.78134484328317));
#262229=CARTESIAN_POINT('Ctrl Pts',(-1.2344088629729,0.947198826155264,
1.78445902357458));
#262230=CARTESIAN_POINT('Ctrl Pts',(-1.25660464510444,0.917549007079306,
1.78701308876241));
#262231=CARTESIAN_POINT('Ctrl Pts',(-1.31058486458874,0.839802122581353,
1.79343686479274));
#262232=CARTESIAN_POINT('Ctrl Pts',(-1.34079371490773,0.790679097576037,
1.79724414685384));
#262233=CARTESIAN_POINT('Ctrl Pts',(-1.39692084927034,0.68690250745392,
1.80501613569411));
#262234=CARTESIAN_POINT('Ctrl Pts',(-1.42251840494302,0.63218985647847,
1.80897367910986));
#262235=CARTESIAN_POINT('Ctrl Pts',(-1.47032488640934,0.512296374354675,
1.81757527571476));
#262236=CARTESIAN_POINT('Ctrl Pts',(-1.49151670245953,0.446854349824916,
1.82223016809479));
#262237=CARTESIAN_POINT('Ctrl Pts',(-1.51114722757016,0.368983563398039,
1.82784170148304));
#262238=CARTESIAN_POINT('Ctrl Pts',(-1.51385682428068,0.357704230111939,
1.82865611756081));
#262239=CARTESIAN_POINT('Ctrl Pts',(-1.51806885680709,0.339264940776269,
1.82999064228205));
#262240=CARTESIAN_POINT('Ctrl Pts',(-1.51964741766889,0.332122683238821,
1.83050831603216));
#262241=CARTESIAN_POINT('Ctrl Pts',(-1.52237946125015,0.319334050182801,
1.83143672332191));
#262242=CARTESIAN_POINT('Ctrl Pts',(-1.52355205904101,0.313691857399968,
1.83184683915886));
#262243=CARTESIAN_POINT('Ctrl Pts',(-1.52576013074415,0.302762772016354,
1.83264229694041));
#262244=CARTESIAN_POINT('Ctrl Pts',(-1.52679954597543,0.297476751611537,
1.83302750693188));
#262245=CARTESIAN_POINT('Ctrl Pts',(-1.52899934045419,0.285974225842405,
1.83386681425304));
#262246=CARTESIAN_POINT('Ctrl Pts',(-1.53014930694245,0.279755852892933,
1.83432123552279));
#262247=CARTESIAN_POINT('Ctrl Pts',(-1.53286352839187,0.264561280920582,
1.83543335865316));
#262248=CARTESIAN_POINT('Ctrl Pts',(-1.53438687724789,0.255578114084439,
1.83609234040411));
#262249=CARTESIAN_POINT('Ctrl Pts',(-1.53996566034564,0.220830808418806,
1.83864734805022));
#262250=CARTESIAN_POINT('Ctrl Pts',(-1.54345157031347,0.194980973357823,
1.84056099832855));
#262251=CARTESIAN_POINT('Ctrl Pts',(-1.55247491780949,0.112448658570735,
1.84671483795149));
#262252=CARTESIAN_POINT('Ctrl Pts',(-1.55554994910745,0.0555504721415419,
1.85102502171189));
#262253=CARTESIAN_POINT('Ctrl Pts',(-1.55549938654046,-0.00138147466141999,
1.85539356957841));
#262254=CARTESIAN_POINT('Ctrl Pts',(-1.55549938776457,-0.0013800956646107,
1.85539346376413));
#262255=CARTESIAN_POINT('Ctrl Pts',(-1.55538499258098,-0.130314373632887,
1.86528695038457));
#262256=CARTESIAN_POINT('Ctrl Pts',(-1.53924107972692,-0.258738026691858,
1.87546978858605));
#262257=CARTESIAN_POINT('Ctrl Pts',(-1.50487644833776,-0.393744166409597,
1.88583137537503));
#262258=CARTESIAN_POINT('Ctrl Pts',(-1.5022203898513,-0.403759220324333,
1.88659759205956));
#262259=CARTESIAN_POINT('Ctrl Pts',(-1.49796387007771,-0.419185301674853,
1.88777327251184));
#262260=CARTESIAN_POINT('Ctrl Pts',(-1.49643376510856,-0.424615193295317,
1.88818623609406));
#262261=CARTESIAN_POINT('Ctrl Pts',(-1.49351459876753,-0.434762666153521,
1.88895620939144));
#262262=CARTESIAN_POINT('Ctrl Pts',(-1.49213264558227,-0.439482198017928,
1.88931359583662));
#262263=CARTESIAN_POINT('Ctrl Pts',(-1.48977183557845,-0.447405125687906,
1.88991225021017));
#262264=CARTESIAN_POINT('Ctrl Pts',(-1.48880498216734,-0.450612022002268,
1.89015420063082));
#262265=CARTESIAN_POINT('Ctrl Pts',(-1.48694934173345,-0.456695708852062,
1.89061247602489));
#262266=CARTESIAN_POINT('Ctrl Pts',(-1.48606255163317,-0.459573071906472,
1.89082891833997));
#262267=CARTESIAN_POINT('Ctrl Pts',(-1.48371393148164,-0.46711574703639,
1.89139554012947));
#262268=CARTESIAN_POINT('Ctrl Pts',(-1.48223843588305,-0.471776824914916,
1.89174492909669));
#262269=CARTESIAN_POINT('Ctrl Pts',(-1.47702516980499,-0.487979585419309,
1.89295707142932));
#262270=CARTESIAN_POINT('Ctrl Pts',(-1.47317424690282,-0.499484824934753,
1.89381354141442));
#262271=CARTESIAN_POINT('Ctrl Pts',(-1.43724840276836,-0.602787383732344,
1.9014752561513));
#262272=CARTESIAN_POINT('Ctrl Pts',(-1.39676087985296,-0.691448179988233,
1.90785665448435));
#262273=CARTESIAN_POINT('Ctrl Pts',(-1.32169692530766,-0.821907808632035,
1.91776334461363));
#262274=CARTESIAN_POINT('Ctrl Pts',(-1.29279161788773,-0.866662986828566,
1.92126556897074));
#262275=CARTESIAN_POINT('Ctrl Pts',(-1.23593806779234,-0.94549963738856,
1.92775448249206));
#262276=CARTESIAN_POINT('Ctrl Pts',(-1.20872877063328,-0.980044252883185,
1.93072127399104));
#262277=CARTESIAN_POINT('Ctrl Pts',(-1.16203011148658,-1.03442503248422,
1.93564591353479));
#262278=CARTESIAN_POINT('Ctrl Pts',(-1.1434070225353,-1.05497362250637,
1.93757086389945));
#262279=CARTESIAN_POINT('Ctrl Pts',(-1.11799061111316,-1.08155404918583,
1.94015469906845));
#262280=CARTESIAN_POINT('Ctrl Pts',(-1.1116786785005,-1.08804075173548,
1.94079297721551));
#262281=CARTESIAN_POINT('Ctrl Pts',(-1.10151978967503,-1.09830024568838,
1.94181512995576));
#262282=CARTESIAN_POINT('Ctrl Pts',(-1.0977091453651,-1.10210884561348,
1.9421974121334));
#262283=CARTESIAN_POINT('Ctrl Pts',(-1.0897821085005,-1.10994973287904,
1.94299037406554));
#262284=CARTESIAN_POINT('Ctrl Pts',(-1.08566294827885,-1.11397909074632,
1.94340117328898));
#262285=CARTESIAN_POINT('Ctrl Pts',(-1.07626796928543,-1.12306764595055,
1.94433536886532));
#262286=CARTESIAN_POINT('Ctrl Pts',(-1.07097872002294,-1.12811269692917,
1.94485936502879));
#262287=CARTESIAN_POINT('Ctrl Pts',(-1.05721632549102,-1.14105567807739,
1.94621792822754));
#262288=CARTESIAN_POINT('Ctrl Pts',(-1.04869030294633,-1.14889645067528,
1.94705489950776));
#262289=CARTESIAN_POINT('Ctrl Pts',(-0.98862738161977,-1.20290638284154,
1.95291996585733));
#262290=CARTESIAN_POINT('Ctrl Pts',(-0.934155516572659,-1.24568001294183,
1.95808678075277));
#262291=CARTESIAN_POINT('Ctrl Pts',(-0.781485943385103,-1.34990435444065,
1.97217863977512));
#262292=CARTESIAN_POINT('Ctrl Pts',(-0.678977632791914,-1.40426095260128,
1.98127493536658));
#262293=CARTESIAN_POINT('Ctrl Pts',(-0.535260017485219,-1.46102239890852,
1.9930455335592));
#262294=CARTESIAN_POINT('Ctrl Pts',(-0.498598212611087,-1.47393696946553,
1.99596535599343));
#262295=CARTESIAN_POINT('Ctrl Pts',(-0.454776574836293,-1.48755097448557,
1.99932984970858));
#262296=CARTESIAN_POINT('Ctrl Pts',(-0.448051324438485,-1.48959043042102,
1.99984275035747));
#262297=CARTESIAN_POINT('Ctrl Pts',(-0.437657738833779,-1.49266556157411,
2.00062987404458));
#262298=CARTESIAN_POINT('Ctrl Pts',(-0.433999148669779,-1.4937334149272,
2.00090589052176));
#262299=CARTESIAN_POINT('Ctrl Pts',(-0.42724509040867,-1.49567785047648,
2.00141345010194));
#262300=CARTESIAN_POINT('Ctrl Pts',(-0.424150845743791,-1.49655827154781,
2.0016452060117));
#262301=CARTESIAN_POINT('Ctrl Pts',(-0.417155450802506,-1.49852526789335,
2.00216742583565));
#262302=CARTESIAN_POINT('Ctrl Pts',(-0.413252780308723,-1.49960621138355,
2.00245756229349));
#262303=CARTESIAN_POINT('Ctrl Pts',(-0.40170970674649,-1.5027548739734,
2.0033122751829));
#262304=CARTESIAN_POINT('Ctrl Pts',(-0.394057538850978,-1.50477957283972,
2.00387444798146));
#262305=CARTESIAN_POINT('Ctrl Pts',(-0.332756678753086,-1.52049957092653,
2.00834506589394));
#262306=CARTESIAN_POINT('Ctrl Pts',(-0.278419906757475,-1.53138170264221,
2.01210734784367));
#262307=CARTESIAN_POINT('Ctrl Pts',(-0.0891465103870856,-1.55887639352212,
2.02488919281763));
#262308=CARTESIAN_POINT('Ctrl Pts',(0.047293221060649,-1.56070725254469,
2.03359773365823));
#262309=CARTESIAN_POINT('Ctrl Pts',(0.205730075032876,-1.5420165184012,
2.04447952219237));
#262310=CARTESIAN_POINT('Ctrl Pts',(0.229154778366163,-1.53870978370918,
2.04610662302219));
#262311=CARTESIAN_POINT('Ctrl Pts',(0.269737219950002,-1.53203376487535,
2.04896359376813));
#262312=CARTESIAN_POINT('Ctrl Pts',(0.286930768307157,-1.5289069022523,
2.05018598565427));
#262313=CARTESIAN_POINT('Ctrl Pts',(0.311710154985867,-1.52396776922958,
2.05196674293335));
#262314=CARTESIAN_POINT('Ctrl Pts',(0.319341223582539,-1.52238699459602,
2.05251777034855));
#262315=CARTESIAN_POINT('Ctrl Pts',(0.332657803918739,-1.51952393910869,
2.05348408439427));
#262316=CARTESIAN_POINT('Ctrl Pts',(0.338348637947812,-1.51826691116625,
2.05389855878551));
#262317=CARTESIAN_POINT('Ctrl Pts',(0.349360875367013,-1.51576946925564,
2.05470361324727));
#262318=CARTESIAN_POINT('Ctrl Pts',(0.354683079283868,-1.51453293692481,
2.05509406349522));
#262319=CARTESIAN_POINT('Ctrl Pts',(0.367361603793998,-1.51151678261298,
2.05602751618959));
#262320=CARTESIAN_POINT('Ctrl Pts',(0.374711606521245,-1.5097114758275,
2.05657133595602));
#262321=CARTESIAN_POINT('Ctrl Pts',(0.401108853599507,-1.50302314578475,
2.05853429542472));
#262322=CARTESIAN_POINT('Ctrl Pts',(0.420075544011653,-1.49783288812394,
2.05996324906894));
#262323=CARTESIAN_POINT('Ctrl Pts',(0.6113186963147,-1.4415809674105,2.07456739024955));
#262324=CARTESIAN_POINT('Ctrl Pts',(0.773595403711356,-1.36139020385998,
2.08881230446037));
#262325=CARTESIAN_POINT('Ctrl Pts',(0.945861485354785,-1.23534332848347,
2.10500840146732));
#262326=CARTESIAN_POINT('Ctrl Pts',(0.97253404260021,-1.21445669426599,
2.10754445494982));
#262327=CARTESIAN_POINT('Ctrl Pts',(1.00369283351676,-1.18837145249997,
2.11052214192413));
#262328=CARTESIAN_POINT('Ctrl Pts',(1.00885167484771,-1.18399506579218,
2.11101565497474));
#262329=CARTESIAN_POINT('Ctrl Pts',(1.01682911972012,-1.17713758241263,
2.11177938428429));
#262330=CARTESIAN_POINT('Ctrl Pts',(1.01966748396584,-1.17467977321128,
2.11205123336971));
#262331=CARTESIAN_POINT('Ctrl Pts',(1.02492535535232,-1.17009343643565,
2.11255498474));
#262332=CARTESIAN_POINT('Ctrl Pts',(1.02734712686369,-1.16796768589668,
2.11278707447444));
#262333=CARTESIAN_POINT('Ctrl Pts',(1.03285384397178,-1.16310369309019,
2.11331497276618));
#262334=CARTESIAN_POINT('Ctrl Pts',(1.03593451372078,-1.16036069746794,
2.11361042268479));
#262335=CARTESIAN_POINT('Ctrl Pts',(1.04394540730739,-1.15317055090816,
2.11437914111468));
#262336=CARTESIAN_POINT('Ctrl Pts',(1.04885820209299,-1.14870396925677,
2.11485100519347));
#262337=CARTESIAN_POINT('Ctrl Pts',(1.08196312978606,-1.11821639460408,
2.11803489272853));
#262338=CARTESIAN_POINT('Ctrl Pts',(1.10921570273056,-1.0911889172588,2.12067694432897));
#262339=CARTESIAN_POINT('Ctrl Pts',(1.23785287999457,-0.953808185164887,
2.13342705634154));
#262340=CARTESIAN_POINT('Ctrl Pts',(1.32392613459265,-0.83021427623846,
2.14293675167309));
#262341=CARTESIAN_POINT('Ctrl Pts',(1.40857223896123,-0.661094844466187,
2.1557981836645));
#262342=CARTESIAN_POINT('Ctrl Pts',(1.42480998331716,-0.625330483879022,
2.15850489772792));
#262343=CARTESIAN_POINT('Ctrl Pts',(1.44366156506559,-0.57925150487408,
2.16199604935914));
#262344=CARTESIAN_POINT('Ctrl Pts',(1.44754772196033,-0.569470458694504,
2.16273728224994));
#262345=CARTESIAN_POINT('Ctrl Pts',(1.45363283673408,-0.553690023419767,
2.16393381203582));
#262346=CARTESIAN_POINT('Ctrl Pts',(1.45589465606157,-0.547715084972244,
2.16438700080556));
#262347=CARTESIAN_POINT('Ctrl Pts',(1.46013036130729,-0.536314193282347,
2.16525210349797));
#262348=CARTESIAN_POINT('Ctrl Pts',(1.4621109745447,-0.530890838489971,
2.16566378517008));
#262349=CARTESIAN_POINT('Ctrl Pts',(1.46656449221328,-0.518482159325499,
2.16660613951145));
#262350=CARTESIAN_POINT('Ctrl Pts',(1.46901775021251,-0.511489985632441,
2.16713745238744));
#262351=CARTESIAN_POINT('Ctrl Pts',(1.47528591587566,-0.493207599844335,
2.16852760986062));
#262352=CARTESIAN_POINT('Ctrl Pts',(1.47902113470459,-0.481890795235131,
2.16938904835694));
#262353=CARTESIAN_POINT('Ctrl Pts',(1.51470066127733,-0.369466273351515,
2.17795781999972));
#262354=CARTESIAN_POINT('Ctrl Pts',(1.53635080533132,-0.265406936443129,
2.18600603168384));
#262355=CARTESIAN_POINT('Ctrl Pts',(1.55578618964926,-0.077432978740626,
2.20062071586958));
#262356=CARTESIAN_POINT('Ctrl Pts',(1.55770196251515,0.00566340668308941,
2.20709852841827));
#262357=CARTESIAN_POINT('Ctrl Pts',(1.55101756352495,0.12293564772127,2.21601557926069));
#262358=CARTESIAN_POINT('Ctrl Pts',(1.54791200045187,0.157281765443562,
2.21859831285309));
#262359=CARTESIAN_POINT('Ctrl Pts',(1.54283022917094,0.198245672491054,
2.22162324447463));
#262360=CARTESIAN_POINT('Ctrl Pts',(1.54194908384755,0.20498656074154,2.22211920424176));
#262361=CARTESIAN_POINT('Ctrl Pts',(1.54051173636375,0.215448348308985,
2.2228858893746));
#262362=CARTESIAN_POINT('Ctrl Pts',(1.5399861958074,0.219173260687879,2.22315826748154));
#262363=CARTESIAN_POINT('Ctrl Pts',(1.53898549879714,0.226084637262817,
2.22366249174206));
#262364=CARTESIAN_POINT('Ctrl Pts',(1.53851396021596,0.229271505604267,
2.22389452858872));
#262365=CARTESIAN_POINT('Ctrl Pts',(1.53741759886222,0.236525490328586,
2.22442165847497));
#262366=CARTESIAN_POINT('Ctrl Pts',(1.53678653743202,0.240591604769501,
2.22471639704041));
#262367=CARTESIAN_POINT('Ctrl Pts',(1.53510031819862,0.251179024854326,
2.22548203696888));
#262368=CARTESIAN_POINT('Ctrl Pts',(1.53401972506342,0.257696287670466,
2.22595155222362));
#262369=CARTESIAN_POINT('Ctrl Pts',(1.52649951879612,0.301327693421585,
2.22908406235724));
#262370=CARTESIAN_POINT('Ctrl Pts',(1.51875445814113,0.338207976083737,
2.23167962899964));
#262371=CARTESIAN_POINT('Ctrl Pts',(1.49045761928223,0.45219417480216,2.23964144827837));
#262372=CARTESIAN_POINT('Ctrl Pts',(1.46533588500121,0.527922725757585,
2.24484847407491));
#262373=CARTESIAN_POINT('Ctrl Pts',(1.43457657517513,0.601307159410884,
2.25008958711186));
#262374=CARTESIAN_POINT('Origin',(0.,0.,-1.29405622560371));
#262375=CARTESIAN_POINT('',(1.43457670182626,0.601306857251191,3.08743730443809));
#262376=CARTESIAN_POINT('',(1.43457668232327,0.601306903780717,2.94872114469929));
#262377=CARTESIAN_POINT('',(1.43457668357355,0.601306900797845,-1.29405622560371));
#262378=CARTESIAN_POINT('Ctrl Pts',(1.43457670182626,0.601306857251181,
3.08743730443809));
#262379=CARTESIAN_POINT('Ctrl Pts',(1.46774209616445,0.522182028637142,
3.08172695245763));
#262380=CARTESIAN_POINT('Ctrl Pts',(1.49431527012455,0.440423298556932,
3.07614889058204));
#262381=CARTESIAN_POINT('Ctrl Pts',(1.52964391206799,0.290538795584047,
3.06591309957777));
#262382=CARTESIAN_POINT('Ctrl Pts',(1.5408998950646,0.223268878613844,3.06131690589896));
#262383=CARTESIAN_POINT('Ctrl Pts',(1.54937676033112,0.138888701868872,
3.05542021869638));
#262384=CARTESIAN_POINT('Ctrl Pts',(1.55077681655962,0.122268739439419,
3.05425275856998));
#262385=CARTESIAN_POINT('Ctrl Pts',(1.55242485109702,0.098055925063515,
3.05254175184623));
#262386=CARTESIAN_POINT('Ctrl Pts',(1.55288491538876,0.090478277050115,
3.05200482820358));
#262387=CARTESIAN_POINT('Ctrl Pts',(1.55359529967532,0.077167501855097,
3.05105899907139));
#262388=CARTESIAN_POINT('Ctrl Pts',(1.55386939980407,0.0714357421323946,
3.05065084429601));
#262389=CARTESIAN_POINT('Ctrl Pts',(1.55434089145987,0.0602832155659266,
3.04985492729094));
#262390=CARTESIAN_POINT('Ctrl Pts',(1.55454165569358,0.0548626674629069,
3.04946727657302));
#262391=CARTESIAN_POINT('Ctrl Pts',(1.55500338651687,0.0403432225422172,
3.04842669971374));
#262392=CARTESIAN_POINT('Ctrl Pts',(1.55521283904623,0.0312430217269055,
3.04777217504043));
#262393=CARTESIAN_POINT('Ctrl Pts',(1.55568968887484,-0.00225329086883831,
3.04535404575373));
#262394=CARTESIAN_POINT('Ctrl Pts',(1.55546296879262,-0.0266516949009347,
3.04357519287758));
#262395=CARTESIAN_POINT('Ctrl Pts',(1.54896109538769,-0.224722200085808,
3.02898273588573));
#262396=CARTESIAN_POINT('Ctrl Pts',(1.5141880028679,-0.396216312241429,
3.01520270121296));
#262397=CARTESIAN_POINT('Ctrl Pts',(1.43978562106666,-0.589682159621664,
2.99947919619744));
#262398=CARTESIAN_POINT('Ctrl Pts',(1.42672036046807,-0.620626397851031,
2.99696533613715));
#262399=CARTESIAN_POINT('Ctrl Pts',(1.40986150927731,-0.657202818956143,
2.99401454272213));
#262400=CARTESIAN_POINT('Ctrl Pts',(1.40702140041963,-0.663261489688012,
2.99352645908383));
#262401=CARTESIAN_POINT('Ctrl Pts',(1.40254588781376,-0.67265076112479,
2.9927713624617));
#262402=CARTESIAN_POINT('Ctrl Pts',(1.40093756073984,-0.675994057337581,
2.9925027481483));
#262403=CARTESIAN_POINT('Ctrl Pts',(1.397928035989,-0.682193209345491,2.99200520516163));
#262404=CARTESIAN_POINT('Ctrl Pts',(1.39653005189859,-0.685050496793545,
2.99177609203497));
#262405=CARTESIAN_POINT('Ctrl Pts',(1.39332576720341,-0.691549041637331,
2.99125546689188));
#262406=CARTESIAN_POINT('Ctrl Pts',(1.39151395467407,-0.695187518231353,
2.99096430163952));
#262407=CARTESIAN_POINT('Ctrl Pts',(1.38675548170837,-0.704650330570732,
2.99020779649077));
#262408=CARTESIAN_POINT('Ctrl Pts',(1.38378634610123,-0.710463374658684,
2.98974381240098));
#262409=CARTESIAN_POINT('Ctrl Pts',(1.36367801113416,-0.749227634954817,
2.98665353206283));
#262410=CARTESIAN_POINT('Ctrl Pts',(1.34539822847524,-0.781577848333375,
2.98409293756511));
#262411=CARTESIAN_POINT('Ctrl Pts',(1.32116138060967,-0.82109539922213,
2.98094856265592));
#262412=CARTESIAN_POINT('Ctrl Pts',(1.31627725142367,-0.828902437897368,
2.98032654045963));
#262413=CARTESIAN_POINT('Ctrl Pts',(1.2525261400118,-0.928820905353651,
2.97234883778091));
#262414=CARTESIAN_POINT('Ctrl Pts',(1.18417591170568,-1.01452448147179,
2.96530066416187));
#262415=CARTESIAN_POINT('Ctrl Pts',(1.0633040219609,-1.13706104320945,2.95382583976959));
#262416=CARTESIAN_POINT('Ctrl Pts',(1.01654568798507,-1.17904903767613,
2.94957586124099));
#262417=CARTESIAN_POINT('Ctrl Pts',(0.954864096200996,-1.22803515713081,
2.9440943431103));
#262418=CARTESIAN_POINT('Ctrl Pts',(0.942193879515839,-1.23778287660688,
2.94297470923135));
#262419=CARTESIAN_POINT('Ctrl Pts',(0.923391289703923,-1.251792506168,2.94132108960339));
#262420=CARTESIAN_POINT('Ctrl Pts',(0.917374572372189,-1.25620851886206,
2.94079310659225));
#262421=CARTESIAN_POINT('Ctrl Pts',(0.90669108507752,-1.26393205593711,
2.93985751731442));
#262422=CARTESIAN_POINT('Ctrl Pts',(0.902037377766745,-1.26725748500327,
2.93945061008496));
#262423=CARTESIAN_POINT('Ctrl Pts',(0.892901035371278,-1.27371027503062,
2.93865292886185));
#262424=CARTESIAN_POINT('Ctrl Pts',(0.888420044164304,-1.27683982840649,
2.93826224643868));
#262425=CARTESIAN_POINT('Ctrl Pts',(0.876256230401911,-1.28524008434027,
2.93720313320042));
#262426=CARTESIAN_POINT('Ctrl Pts',(0.868542501960563,-1.2904654086738,
2.9365329990759));
#262427=CARTESIAN_POINT('Ctrl Pts',(0.839246145170708,-1.30992927153032,
2.93399313329773));
#262428=CARTESIAN_POINT('Ctrl Pts',(0.817357712092558,-1.32369747684409,
2.93210609734005));
#262429=CARTESIAN_POINT('Ctrl Pts',(0.79009169463593,-1.33991411309846,
2.92976665035238));
#262430=CARTESIAN_POINT('Ctrl Pts',(0.785028994360522,-1.3428865152119,
2.92933273525665));
#262431=CARTESIAN_POINT('Ctrl Pts',(0.636043349168608,-1.4292282440149,
2.91657696721538));
#262432=CARTESIAN_POINT('Ctrl Pts',(0.479696703621871,-1.48899749632878,
2.90339088856393));
#262433=CARTESIAN_POINT('Ctrl Pts',(0.284395554843879,-1.52964158812443,
2.88826310779952));
#262434=CARTESIAN_POINT('Ctrl Pts',(0.25165473062136,-1.53536788196153,
2.8857761781118));
#262435=CARTESIAN_POINT('Ctrl Pts',(0.212147366300636,-1.54097964149389,
2.88285268485845));
#262436=CARTESIAN_POINT('Ctrl Pts',(0.205535918879187,-1.54187540057457,
2.88236603748075));
#262437=CARTESIAN_POINT('Ctrl Pts',(0.195243435083639,-1.54320250894074,
2.88161267637891));
#262438=CARTESIAN_POINT('Ctrl Pts',(0.191566382148108,-1.5436632743428,
2.881344372868));
#262439=CARTESIAN_POINT('Ctrl Pts',(0.18472948109058,-1.54449518957619,
2.88084710723366));
#262440=CARTESIAN_POINT('Ctrl Pts',(0.181570168731373,-1.54486978284983,
2.88061796254175));
#262441=CARTESIAN_POINT('Ctrl Pts',(0.174366006877567,-1.5457015606306,
2.8800968837267));
#262442=CARTESIAN_POINT('Ctrl Pts',(0.170320500182812,-1.54615256269456,
2.87980529879377));
#262443=CARTESIAN_POINT('Ctrl Pts',(0.159763775885368,-1.54728751315787,
2.87904697823008));
#262444=CARTESIAN_POINT('Ctrl Pts',(0.153249838935343,-1.54794625337149,
2.87858160908596));
#262445=CARTESIAN_POINT('Ctrl Pts',(0.10934872973357,-1.55210603541351,
2.87546117164698));
#262446=CARTESIAN_POINT('Ctrl Pts',(0.071845772791788,-1.5542937466236,
2.8728732748488));
#262447=CARTESIAN_POINT('Ctrl Pts',(0.0251877133311025,-1.55532274585193,
2.86970903563867));
#262448=CARTESIAN_POINT('Ctrl Pts',(0.0160769427927272,-1.5554436030528,
2.86909379072456));
#262449=CARTESIAN_POINT('Ctrl Pts',(-0.0830404683954157,-1.55588745232811,
2.86242403333929));
#262450=CARTESIAN_POINT('Ctrl Pts',(-0.172915846772297,-1.54847775808896,
2.856578566149));
#262451=CARTESIAN_POINT('Ctrl Pts',(-0.347314940947573,-1.51871813082405,
2.84487518722786));
#262452=CARTESIAN_POINT('Ctrl Pts',(-0.431591415105831,-1.49694951544136,
2.83904396725075));
#262453=CARTESIAN_POINT('Ctrl Pts',(-0.525641819905539,-1.4640504143463,
2.83208050575296));
#262454=CARTESIAN_POINT('Ctrl Pts',(-0.537628837112943,-1.45969111630673,
2.83118444417943));
#262455=CARTESIAN_POINT('Ctrl Pts',(-0.555940981005288,-1.4527754097963,
2.82980174376558));
#262456=CARTESIAN_POINT('Ctrl Pts',(-0.562305369598177,-1.45032390668688,
2.82931860066859));
#262457=CARTESIAN_POINT('Ctrl Pts',(-0.573872816114587,-1.44578064948175,
2.82843565107156));
#262458=CARTESIAN_POINT('Ctrl Pts',(-0.579081105289074,-1.44370245115743,
2.82803630518541));
#262459=CARTESIAN_POINT('Ctrl Pts',(-0.590424061378311,-1.43910515847063,
2.82716259799904));
#262460=CARTESIAN_POINT('Ctrl Pts',(-0.596554058799803,-1.43657491339688,
2.82668786672457));
#262461=CARTESIAN_POINT('Ctrl Pts',(-0.613317280508964,-1.42952985670212,
2.82538250756394));
#262462=CARTESIAN_POINT('Ctrl Pts',(-0.623916494545244,-1.42493575020628,
2.82454920662095));
#262463=CARTESIAN_POINT('Ctrl Pts',(-0.679411582045571,-1.40014417303658,
2.82014334839106));
#262464=CARTESIAN_POINT('Ctrl Pts',(-0.72337615810115,-1.37794402819099,
2.81650283576617));
#262465=CARTESIAN_POINT('Ctrl Pts',(-0.893125605647638,-1.2818637863929,
2.80182550577675));
#262466=CARTESIAN_POINT('Ctrl Pts',(-1.00928541666132,-1.19255241530577,
2.79028406414977));
#262467=CARTESIAN_POINT('Ctrl Pts',(-1.13347603197739,-1.06574694037192,
2.7768422008073));
#262468=CARTESIAN_POINT('Ctrl Pts',(-1.15495411164472,-1.0424326464691,
2.77447296926127));
#262469=CARTESIAN_POINT('Ctrl Pts',(-1.18001709079506,-1.01350049549463,
2.77166915728551));
#262470=CARTESIAN_POINT('Ctrl Pts',(-1.18429598751108,-1.00849720230472,
2.77118903238763));
#262471=CARTESIAN_POINT('Ctrl Pts',(-1.19092129557197,-1.00064994286264,
2.77044355691128));
#262472=CARTESIAN_POINT('Ctrl Pts',(-1.19328951176967,-0.997824625005049,
2.77017666852129));
#262473=CARTESIAN_POINT('Ctrl Pts',(-1.19768432471044,-0.992543523345301,
2.76968065075127));
#262474=CARTESIAN_POINT('Ctrl Pts',(-1.19971340665289,-0.990089960356257,
2.76945134742045));
#262475=CARTESIAN_POINT('Ctrl Pts',(-1.20433711945371,-0.984463888972264,
2.76892813547101));
#262476=CARTESIAN_POINT('Ctrl Pts',(-1.20692675473208,-0.981287346161066,
2.76863458738079));
#262477=CARTESIAN_POINT('Ctrl Pts',(-1.21367878275593,-0.972937893945883,
2.76786775731323));
#262478=CARTESIAN_POINT('Ctrl Pts',(-1.21782072160465,-0.967748431868068,
2.7673958924056));
#262479=CARTESIAN_POINT('Ctrl Pts',(-1.24610217968112,-0.931845285032626,
2.76416253977896));
#262480=CARTESIAN_POINT('Ctrl Pts',(-1.26911296168295,-0.900255079734131,
2.76147376513764));
#262481=CARTESIAN_POINT('Ctrl Pts',(-1.37438254850477,-0.743664530601003,
2.74869960249207));
#262482=CARTESIAN_POINT('Ctrl Pts',(-1.43950589647837,-0.608106265900794,
2.7392028206991));
#262483=CARTESIAN_POINT('Ctrl Pts',(-1.49595404852199,-0.428050970372786,
2.72636753936062));
#262484=CARTESIAN_POINT('Ctrl Pts',(-1.50623046029735,-0.390353060063493,
2.72367439103407));
#262485=CARTESIAN_POINT('Ctrl Pts',(-1.51743733177194,-0.342159066350754,
2.72020430087715));
#262486=CARTESIAN_POINT('Ctrl Pts',(-1.51969585961313,-0.331983986682047,
2.71947019446641));
#262487=CARTESIAN_POINT('Ctrl Pts',(-1.52315831369877,-0.315608747190726,
2.71828604571868));
#262488=CARTESIAN_POINT('Ctrl Pts',(-1.52442705738191,-0.309422485409392,
2.71783807722669));
#262489=CARTESIAN_POINT('Ctrl Pts',(-1.5267690223959,-0.297639177172171,
2.71698354918531));
#262490=CARTESIAN_POINT('Ctrl Pts',(-1.52784922562394,-0.292043609255253,
2.71657721949318));
#262491=CARTESIAN_POINT('Ctrl Pts',(-1.53024325749635,-0.279265356581206,
2.71564801860801));
#262492=CARTESIAN_POINT('Ctrl Pts',(-1.53153729927371,-0.272079150366061,
2.71512452833244));
#262493=CARTESIAN_POINT('Ctrl Pts',(-1.53477574995357,-0.253339510907867,
2.71375685811168));
#262494=CARTESIAN_POINT('Ctrl Pts',(-1.53664027710408,-0.241772941500433,
2.71291017558365));
#262495=CARTESIAN_POINT('Ctrl Pts',(-1.54984432395086,-0.153528220502592,
2.70643007995584));
#262496=CARTESIAN_POINT('Ctrl Pts',(-1.55556693000821,-0.0761328717606003,
2.7006206256036));
#262497=CARTESIAN_POINT('Ctrl Pts',(-1.5554244222916,0.0874127041405672,
2.68809930640455));
#262498=CARTESIAN_POINT('Ctrl Pts',(-1.54820777027417,0.173313721931464,
2.68137810810466));
#262499=CARTESIAN_POINT('Ctrl Pts',(-1.53126018567324,0.27400806299856,
2.67351039372902));
#262500=CARTESIAN_POINT('Ctrl Pts',(-1.52834947844039,0.289803503858001,
2.67227693440786));
#262501=CARTESIAN_POINT('Ctrl Pts',(-1.51673895875536,0.34775873708832,
2.66775939431766));
#262502=CARTESIAN_POINT('Ctrl Pts',(-1.50653393184117,0.389601770587477,
2.66451336604147));
#262503=CARTESIAN_POINT('Ctrl Pts',(-1.4927231447756,0.437497415182287,
2.66085441510424));
#262504=CARTESIAN_POINT('Ctrl Pts',(-1.49079869057939,0.444010860111326,
2.66035806671069));
#262505=CARTESIAN_POINT('Ctrl Pts',(-1.48764426143674,0.454435482371629,
2.6595658926794));
#262506=CARTESIAN_POINT('Ctrl Pts',(-1.48644140658161,0.458354668425679,
2.65926857659677));
#262507=CARTESIAN_POINT('Ctrl Pts',(-1.48427470715647,0.465316050527937,
2.65874143026232));
#262508=CARTESIAN_POINT('Ctrl Pts',(-1.48331698031487,0.468360085662373,
2.65851125116392));
#262509=CARTESIAN_POINT('Ctrl Pts',(-1.48124634835806,0.474871313764481,
2.65801961268047));
#262510=CARTESIAN_POINT('Ctrl Pts',(-1.48013063539409,0.47833755034198,
2.65775831998459));
#262511=CARTESIAN_POINT('Ctrl Pts',(-1.47702761955545,0.487863017417177,
2.65704136931015));
#262512=CARTESIAN_POINT('Ctrl Pts',(-1.47501518342424,0.493914086777181,
2.6565871531279));
#262513=CARTESIAN_POINT('Ctrl Pts',(-1.46382750705937,0.52687532536351,
2.6541187831204));
#262514=CARTESIAN_POINT('Ctrl Pts',(-1.45395228286217,0.553544585872945,
2.65214284052181));
#262515=CARTESIAN_POINT('Ctrl Pts',(-1.38832521458323,0.716879516271307,
2.64008496955723));
#262516=CARTESIAN_POINT('Ctrl Pts',(-1.31408591333191,0.84531122344867,
2.63072916912009));
#262517=CARTESIAN_POINT('Ctrl Pts',(-1.19140830038867,1.00135625400519,
2.61735628775353));
#262518=CARTESIAN_POINT('Ctrl Pts',(-1.15802832559165,1.03977765962633,
2.61387541394079));
#262519=CARTESIAN_POINT('Ctrl Pts',(-1.11475543628918,1.08491320696422,
2.60949954607314));
#262520=CARTESIAN_POINT('Ctrl Pts',(-1.10658752416475,1.09324305972751,
2.60867920520538));
#262521=CARTESIAN_POINT('Ctrl Pts',(-1.0936124475559,1.10618099299924,2.60738428416947));
#262522=CARTESIAN_POINT('Ctrl Pts',(-1.08886794833194,1.11085154873121,
2.60691246753445));
#262523=CARTESIAN_POINT('Ctrl Pts',(-1.0804399564771,1.11904231773449,2.6060772149358));
#262524=CARTESIAN_POINT('Ctrl Pts',(-1.07676885125618,1.12257518601835,
2.60571433758587));
#262525=CARTESIAN_POINT('Ctrl Pts',(-1.06831381323696,1.13063221259578,
2.6048806936157));
#262526=CARTESIAN_POINT('Ctrl Pts',(-1.06351840707287,1.13514413140526,
2.60440940964866));
#262527=CARTESIAN_POINT('Ctrl Pts',(-1.05015816767556,1.14755558941676,
2.60310048957236));
#262528=CARTESIAN_POINT('Ctrl Pts',(-1.0415331586253,1.15538940348336,2.60226009217872));
#262529=CARTESIAN_POINT('Ctrl Pts',(-0.990213015635063,1.20096018260002,
2.59728537030449));
#262530=CARTESIAN_POINT('Ctrl Pts',(-0.945563734261361,1.23642018763241,
2.59305848426494));
#262531=CARTESIAN_POINT('Ctrl Pts',(-0.768596323846064,1.36176567643758,
2.57666024283518));
#262532=CARTESIAN_POINT('Ctrl Pts',(-0.624669107862679,1.43350152776506,
2.56391299303347));
#262533=CARTESIAN_POINT('Ctrl Pts',(-0.459877410272278,1.48602300904074,
2.55108669900979));
#262534=CARTESIAN_POINT('Ctrl Pts',(-0.447354641892783,1.48984075343229,
2.55012318946272));
#262535=CARTESIAN_POINT('Ctrl Pts',(-0.429974232812458,1.4949005017355,
2.54880270726187));
#262536=CARTESIAN_POINT('Ctrl Pts',(-0.425157012455512,1.49627767062338,
2.54843848806312));
#262537=CARTESIAN_POINT('Ctrl Pts',(-0.417437529773943,1.49844426113464,
2.54785775648594));
#262538=CARTESIAN_POINT('Ctrl Pts',(-0.414539541907525,1.49924856631844,
2.5476403996089));
#262539=CARTESIAN_POINT('Ctrl Pts',(-0.408484178970388,1.50091026691433,
2.54718762740592));
#262540=CARTESIAN_POINT('Ctrl Pts',(-0.405326411272183,1.50176611175629,
2.54695230844253));
#262541=CARTESIAN_POINT('Ctrl Pts',(-0.397648783096102,1.50382098724377,
2.54638204289761));
#262542=CARTESIAN_POINT('Ctrl Pts',(-0.393126118415454,1.50500962552287,
2.54604769207873));
#262543=CARTESIAN_POINT('Ctrl Pts',(-0.377080507556957,1.50914943779184,
2.54486682445075));
#262544=CARTESIAN_POINT('Ctrl Pts',(-0.365528759811657,1.51198891641533,
2.54402643591899));
#262545=CARTESIAN_POINT('Ctrl Pts',(-0.293270803642644,1.52887372718614,
2.53882375712783));
#262546=CARTESIAN_POINT('Ctrl Pts',(-0.231791194904814,1.53939517082956,
2.53463332818678));
#262547=CARTESIAN_POINT('Ctrl Pts',(-0.105269907564111,1.55329261530381,
2.52618638666746));
#262548=CARTESIAN_POINT('Ctrl Pts',(-0.0403193927686453,1.55633361141347,
2.52194200073317));
#262549=CARTESIAN_POINT('Ctrl Pts',(0.113215025401039,1.55390204546577,
2.51179222792609));
#262550=CARTESIAN_POINT('Ctrl Pts',(0.201503106760171,1.54493435817493,
2.50585647253301));
#262551=CARTESIAN_POINT('Ctrl Pts',(0.300241775964519,1.52629516488186,
2.49883861227433));
#262552=CARTESIAN_POINT('Ctrl Pts',(0.311917226452365,1.52395199543456,
2.49800288003116));
#262553=CARTESIAN_POINT('Ctrl Pts',(0.330762786646527,1.51994420623441,
2.49664378160146));
#262554=CARTESIAN_POINT('Ctrl Pts',(0.337950160475337,1.51836230747804,
2.49612304914987));
#262555=CARTESIAN_POINT('Ctrl Pts',(0.350689693844656,1.51546347594091,
2.49519567094962));
#262556=CARTESIAN_POINT('Ctrl Pts',(0.356246382530431,1.51416687377099,
2.49478968259899));
#262557=CARTESIAN_POINT('Ctrl Pts',(0.367907947435551,1.51137800960125,
2.49393446109253));
#262558=CARTESIAN_POINT('Ctrl Pts',(0.3740111515848,1.50987926737252,2.49348502626209));
#262559=CARTESIAN_POINT('Ctrl Pts',(0.390077659837113,1.50583048134034,
2.49229693506263));
#262560=CARTESIAN_POINT('Ctrl Pts',(0.400024897876221,1.50321857721106,
2.4915562987319));
#262561=CARTESIAN_POINT('Ctrl Pts',(0.446125973649888,1.49062356597216,
2.48809961677071));
#262562=CARTESIAN_POINT('Ctrl Pts',(0.481934162274265,1.47943435637402,
2.48534492991948));
#262563=CARTESIAN_POINT('Ctrl Pts',(0.643988906997105,1.42228841929179,
2.47254262700393));
#262564=CARTESIAN_POINT('Ctrl Pts',(0.764343325177799,1.36139405210565,
2.46201572695771));
#262565=CARTESIAN_POINT('Ctrl Pts',(0.920977311222372,1.25476187833795,
2.44743564227172));
#262566=CARTESIAN_POINT('Ctrl Pts',(0.964922439106366,1.22129144378709,
2.44324134478558));
#262567=CARTESIAN_POINT('Ctrl Pts',(1.01297668773709,1.18047447181703,2.43860940188017));
#262568=CARTESIAN_POINT('Ctrl Pts',(1.01891537024943,1.17535238276979,2.43803615902145));
#262569=CARTESIAN_POINT('Ctrl Pts',(1.0278277857804,1.16754714209027,2.43717496063763));
#262570=CARTESIAN_POINT('Ctrl Pts',(1.03083019268011,1.16489716329847,2.43688468280418));
#262571=CARTESIAN_POINT('Ctrl Pts',(1.03619592245224,1.16012428281628,2.43636568290767));
#262572=CARTESIAN_POINT('Ctrl Pts',(1.03856299538568,1.15800571955851,2.43613664977717));
#262573=CARTESIAN_POINT('Ctrl Pts',(1.04371395960431,1.15336703642048,2.43563808555478));
#262574=CARTESIAN_POINT('Ctrl Pts',(1.04649521718309,1.15084408648365,2.43536877190514));
#262575=CARTESIAN_POINT('Ctrl Pts',(1.05436096960117,1.14365676804982,2.43460669806228));
#262576=CARTESIAN_POINT('Ctrl Pts',(1.05942369023692,1.13896852748979,2.4341156942714));
#262577=CARTESIAN_POINT('Ctrl Pts',(1.09192886131023,1.10846343600315,2.4309586078739));
#262578=CARTESIAN_POINT('Ctrl Pts',(1.11845959081112,1.08168782791421,2.42836036331622));
#262579=CARTESIAN_POINT('Ctrl Pts',(1.21694413442665,0.9747915270411,2.41850125243184));
#262580=CARTESIAN_POINT('Ctrl Pts',(1.28148137261592,0.888245829324381,
2.41155201942595));
#262581=CARTESIAN_POINT('Ctrl Pts',(1.37374439069927,0.733272660487642,
2.39958638004565));
#262582=CARTESIAN_POINT('Ctrl Pts',(1.40649269259679,0.668308691645928,
2.39469560923041));
#262583=CARTESIAN_POINT('Ctrl Pts',(1.43457668658422,0.601306893615097,
2.38964409368597));
#262584=CARTESIAN_POINT('Ctrl Pts',(1.43457657517513,0.601307159410884,
2.25008958711186));
#262585=CARTESIAN_POINT('Ctrl Pts',(1.40787999711051,0.66499887657981,2.25463844676208));
#262586=CARTESIAN_POINT('Ctrl Pts',(1.3769368821431,0.726924889666375,2.25921276655968));
#262587=CARTESIAN_POINT('Ctrl Pts',(1.32835359323674,0.809800221634025,
2.26573866177729));
#262588=CARTESIAN_POINT('Ctrl Pts',(1.3141934242662,0.832583434589511,2.26757744870429));
#262589=CARTESIAN_POINT('Ctrl Pts',(1.28886519172717,0.871078496194537,
2.27077179473554));
#262590=CARTESIAN_POINT('Ctrl Pts',(1.27798087916106,0.886970148501126,
2.27211717264022));
#262591=CARTESIAN_POINT('Ctrl Pts',(1.26210337007526,0.909252972981009,
2.2740442368232));
#262592=CARTESIAN_POINT('Ctrl Pts',(1.25735063731273,0.915813985489399,
2.27461676737545));
#262593=CARTESIAN_POINT('Ctrl Pts',(1.24906008264253,0.927072672666492,
2.27560828412533));
#262594=CARTESIAN_POINT('Ctrl Pts',(1.24554643765249,0.931788012572387,
2.27602632922705));
#262595=CARTESIAN_POINT('Ctrl Pts',(1.2387618040858,0.940786098525371,2.276829481103));
#262596=CARTESIAN_POINT('Ctrl Pts',(1.23549512466424,0.945072000444913,
2.27721441512732));
#262597=CARTESIAN_POINT('Ctrl Pts',(1.22776703827887,0.955102746664643,
2.27812099159363));
#262598=CARTESIAN_POINT('Ctrl Pts',(1.22328750921978,0.960833400452387,
2.27864334477606));
#262599=CARTESIAN_POINT('Ctrl Pts',(1.20765321046644,0.980547777970117,
2.28045586327725));
#262600=CARTESIAN_POINT('Ctrl Pts',(1.19629791741044,0.99436988331831,2.28175399212581));
#262601=CARTESIAN_POINT('Ctrl Pts',(1.1033233685304,1.1036441198971,2.29224334566138));
#262602=CARTESIAN_POINT('Ctrl Pts',(1.01067128419277,1.18906819411496,2.30191358507367));
#262603=CARTESIAN_POINT('Ctrl Pts',(0.865672066590175,1.29345064413419,
2.31576709535217));
#262604=CARTESIAN_POINT('Ctrl Pts',(0.820991429587782,1.32226183013476,
2.31988077752487));
#262605=CARTESIAN_POINT('Ctrl Pts',(0.742978329420344,1.36708474471614,
2.32672393845409));
#262606=CARTESIAN_POINT('Ctrl Pts',(0.710389348395907,1.38429946877727,
2.32948868689261));
#262607=CARTESIAN_POINT('Ctrl Pts',(0.67098696973409,1.40335477384006,2.33269700132653));
#262608=CARTESIAN_POINT('Ctrl Pts',(0.664737137268901,1.4063259501083,2.33320196049432));
#262609=CARTESIAN_POINT('Ctrl Pts',(0.655035605193385,1.41085894242009,
2.33397950893901));
#262610=CARTESIAN_POINT('Ctrl Pts',(0.651597784565557,1.41244997343553,
2.33425382509069));
#262611=CARTESIAN_POINT('Ctrl Pts',(0.645227946972664,1.41536974253692,
2.33475980830705));
#262612=CARTESIAN_POINT('Ctrl Pts',(0.642297638311491,1.41670192907245,
2.33499167788606));
#262613=CARTESIAN_POINT('Ctrl Pts',(0.635644518256468,1.41970170656476,
2.33551611289776));
#262614=CARTESIAN_POINT('Ctrl Pts',(0.631919273235037,1.42136375441045,
2.33580833858881));
#262615=CARTESIAN_POINT('Ctrl Pts',(0.622251917433307,1.42563140320678,
2.33656313397546));
#262616=CARTESIAN_POINT('Ctrl Pts',(0.616299885785098,1.42821455014051,
2.33702438121305));
#262617=CARTESIAN_POINT('Ctrl Pts',(0.577848895946942,1.44461691803642,
2.33998293013297));
#262618=CARTESIAN_POINT('Ctrl Pts',(0.544900379448127,1.45736455604692,
2.34242105548473));
#262619=CARTESIAN_POINT('Ctrl Pts',(0.501891423484348,1.47234157218497,
2.34551560285442));
#262620=CARTESIAN_POINT('Ctrl Pts',(0.492206433915786,1.47560751585966,
2.34620679838473));
#262621=CARTESIAN_POINT('Ctrl Pts',(0.392691362852711,1.50807689887382,
2.3532579082713));
#262622=CARTESIAN_POINT('Ctrl Pts',(0.300406549579926,1.52913713562619,
2.35938349736952));
#262623=CARTESIAN_POINT('Ctrl Pts',(0.131635370515287,1.55177324016713,
2.3706616584296));
#262624=CARTESIAN_POINT('Ctrl Pts',(0.0558672381891772,1.55634334883733,
2.37575044688581));
#262625=CARTESIAN_POINT('Ctrl Pts',(-0.0376270146164141,1.55514560233141,
2.382243851419));
#262626=CARTESIAN_POINT('Ctrl Pts',(-0.0553224707870181,1.55461667823798,
2.38348194285182));
#262627=CARTESIAN_POINT('Ctrl Pts',(-0.0808294004021085,1.5534182383694,
2.38528144391646));
#262628=CARTESIAN_POINT('Ctrl Pts',(-0.0886513463083985,1.55299148420934,
2.38583529464545));
#262629=CARTESIAN_POINT('Ctrl Pts',(-0.102292937229947,1.55214382294013,
2.38680489062743));
#262630=CARTESIAN_POINT('Ctrl Pts',(-0.108114110830074,1.55174921602793,
2.3872198069088));
#262631=CARTESIAN_POINT('Ctrl Pts',(-0.119371162576086,1.55092247074394,
2.38802449941711));
#262632=CARTESIAN_POINT('Ctrl Pts',(-0.124807267737676,1.55049447894449,
2.38841413991957));
#262633=CARTESIAN_POINT('Ctrl Pts',(-0.13921462186189,1.54928391020798,
2.38944965329036));
#262634=CARTESIAN_POINT('Ctrl Pts',(-0.148181400589745,1.54845200492632,
2.39009706079054));
#262635=CARTESIAN_POINT('Ctrl Pts',(-0.180373823824945,1.54518312734855,
2.39243224235653));
#262636=CARTESIAN_POINT('Ctrl Pts',(-0.203550054538218,1.54230116346145,
2.39413382220271));
#262637=CARTESIAN_POINT('Ctrl Pts',(-0.399585175939417,1.51342879244656,
2.40870889729388));
#262638=CARTESIAN_POINT('Ctrl Pts',(-0.566976169987425,1.45898741140259,
2.42256666584745));
#262639=CARTESIAN_POINT('Ctrl Pts',(-0.751575039869815,1.36229550207755,
2.43837576876498));
#262640=CARTESIAN_POINT('Ctrl Pts',(-0.780890978319354,1.34570568342085,
2.44089704195184));
#262641=CARTESIAN_POINT('Ctrl Pts',(-0.815414932305842,1.32466009120535,
2.44385975133892));
#262642=CARTESIAN_POINT('Ctrl Pts',(-0.821159231444159,1.32110688066728,
2.44435247750877));
#262643=CARTESIAN_POINT('Ctrl Pts',(-0.830058506708602,1.31552164737929,
2.44511525613897));
#262644=CARTESIAN_POINT('Ctrl Pts',(-0.833229488323259,1.31351549282064,
2.44538693504053));
#262645=CARTESIAN_POINT('Ctrl Pts',(-0.839110402794,1.30976500478088,2.44589053516614));
#262646=CARTESIAN_POINT('Ctrl Pts',(-0.841822150807203,1.30802373930058,
2.44612264279364));
#262647=CARTESIAN_POINT('Ctrl Pts',(-0.847995212652573,1.30403274893734,
2.44665079212162));
#262648=CARTESIAN_POINT('Ctrl Pts',(-0.851452993612248,1.30177766600631,
2.44694647382793));
#262649=CARTESIAN_POINT('Ctrl Pts',(-0.860457754109468,1.29585374614435,
2.44771619587982));
#262650=CARTESIAN_POINT('Ctrl Pts',(-0.865990332165826,1.29216300317849,
2.44818882579668));
#262651=CARTESIAN_POINT('Ctrl Pts',(-0.903461756381395,1.26681731596414,
2.45138915219043));
#262652=CARTESIAN_POINT('Ctrl Pts',(-0.934612153072268,1.24401366517864,
2.45404605446767));
#262653=CARTESIAN_POINT('Ctrl Pts',(-1.08263455729948,1.12695127719115,
2.46682818372891));
#262654=CARTESIAN_POINT('Ctrl Pts',(-1.18628659767463,1.01727438248153,
2.47635589619498));
#262655=CARTESIAN_POINT('Ctrl Pts',(-1.29493883918945,0.862681913000764,
2.48921095800829));
#262656=CARTESIAN_POINT('Ctrl Pts',(-1.31605869328874,0.830105877099318,
2.49188708597596));
#262657=CARTESIAN_POINT('Ctrl Pts',(-1.34130764699851,0.787771526290683,
2.4953438173391));
#262658=CARTESIAN_POINT('Ctrl Pts',(-1.34658700302873,0.778712793810908,
2.49608227432604));
#262659=CARTESIAN_POINT('Ctrl Pts',(-1.35493081692038,0.764057219761254,
2.49727539489196));
#262660=CARTESIAN_POINT('Ctrl Pts',(-1.35805318489658,0.758493571824898,
2.49772797212015));
#262661=CARTESIAN_POINT('Ctrl Pts',(-1.36393683834896,0.747856878170622,
2.49859261336942));
#262662=CARTESIAN_POINT('Ctrl Pts',(-1.3667042744486,0.7427873408882,2.49900444922148));
#262663=CARTESIAN_POINT('Ctrl Pts',(-1.37296548099196,0.731164271938896,
2.49994815346791));
#262664=CARTESIAN_POINT('Ctrl Pts',(-1.37644065568313,0.724600940101763,
2.50048066871829));
#262665=CARTESIAN_POINT('Ctrl Pts',(-1.38539505704458,0.707392482455828,
2.5018760389895));
#262666=CARTESIAN_POINT('Ctrl Pts',(-1.39079852268976,0.69670872156705,
2.50274151984586));
#262667=CARTESIAN_POINT('Ctrl Pts',(-1.44160069586674,0.59331582697167,
2.51111115917462));
#262668=CARTESIAN_POINT('Ctrl Pts',(-1.47777843919311,0.496385912627004,
2.51893711419881));
#262669=CARTESIAN_POINT('Ctrl Pts',(-1.52279333931768,0.325672301892699,
2.53258185991097));
#262670=CARTESIAN_POINT('Ctrl Pts',(-1.53645671527855,0.253501648326342,
2.53830305351554));
#262671=CARTESIAN_POINT('Ctrl Pts',(-1.5503087862466,0.135024752427407,
2.54743274328808));
#262672=CARTESIAN_POINT('Ctrl Pts',(-1.55361973207785,0.089194837883794,
2.55090014149526));
#262673=CARTESIAN_POINT('Ctrl Pts',(-1.55510086053665,0.0359839820638677,
2.55480543319032));
#262674=CARTESIAN_POINT('Ctrl Pts',(-1.55525260587007,0.0286857272568646,
2.55533843638348));
#262675=CARTESIAN_POINT('Ctrl Pts',(-1.55540616765941,0.0175177963063136,
2.55614974754471));
#262676=CARTESIAN_POINT('Ctrl Pts',(-1.55544492957266,0.0136488655404375,
2.55643002229322));
#262677=CARTESIAN_POINT('Ctrl Pts',(-1.55548946381145,0.00656571190506091,
2.55694164937043));
#262678=CARTESIAN_POINT('Ctrl Pts',(-1.55549970995759,0.00335162418207283,
2.5571732400069));
#262679=CARTESIAN_POINT('Ctrl Pts',(-1.55550034567455,-0.00384388205011361,
2.55769045072654));
#262680=CARTESIAN_POINT('Ctrl Pts',(-1.55548541215615,-0.00782523789051597,
2.55797577183294));
#262681=CARTESIAN_POINT('Ctrl Pts',(-1.55539568864849,-0.0196458685768857,
2.55882046094463));
#262682=CARTESIAN_POINT('Ctrl Pts',(-1.55527692028593,-0.0274848409070515,
2.55937745432954));
#262683=CARTESIAN_POINT('Ctrl Pts',(-1.553548405089,-0.10358334601925,2.56475674076048));
#262684=CARTESIAN_POINT('Ctrl Pts',(-1.54750491514884,-0.171678409652982,
2.56935404680753));
#262685=CARTESIAN_POINT('Ctrl Pts',(-1.52736745018196,-0.301092762550527,
2.57804658936515));
#262686=CARTESIAN_POINT('Ctrl Pts',(-1.51399714917435,-0.362382484248962,
2.58214444458106));
#262687=CARTESIAN_POINT('Ctrl Pts',(-1.47235783137446,-0.509845793888468,
2.59226745183739));
#262688=CARTESIAN_POINT('Ctrl Pts',(-1.44019143391049,-0.594663994081574,
2.5983274905965));
#262689=CARTESIAN_POINT('Ctrl Pts',(-1.39561276286524,-0.687014985489912,
2.60548853499373));
#262690=CARTESIAN_POINT('Ctrl Pts',(-1.39026531057886,-0.697772832792645,
2.60633156853736));
#262691=CARTESIAN_POINT('Ctrl Pts',(-1.38140579429891,-0.715089937570975,
2.60770360957363));
#262692=CARTESIAN_POINT('Ctrl Pts',(-1.37797026375547,-0.721687976952016,
2.60822994562417));
#262693=CARTESIAN_POINT('Ctrl Pts',(-1.37178276421229,-0.733365989556275,
2.60916801759704));
#262694=CARTESIAN_POINT('Ctrl Pts',(-1.36904955107434,-0.738455788713131,
2.60957908572664));
#262695=CARTESIAN_POINT('Ctrl Pts',(-1.36324155012157,-0.749128391751868,
2.61044577506964));
#262696=CARTESIAN_POINT('Ctrl Pts',(-1.3601606839041,-0.754707746771307,
2.61090160670166));
#262697=CARTESIAN_POINT('Ctrl Pts',(-1.35193540969707,-0.769389508477288,
2.6121084842876));
#262698=CARTESIAN_POINT('Ctrl Pts',(-1.34673344259631,-0.778459114164683,
2.61286158031631));
#262699=CARTESIAN_POINT('Ctrl Pts',(-1.32195828403722,-0.82066284903708,
2.61640216284323));
#262700=CARTESIAN_POINT('Ctrl Pts',(-1.30125287953495,-0.853112933451776,
2.61923033809146));
#262701=CARTESIAN_POINT('Ctrl Pts',(-1.19384205686457,-1.00842959781245,
2.63331204196824));
#262702=CARTESIAN_POINT('Ctrl Pts',(-1.09083915533347,-1.11903727593352,
2.64518484806637));
#262703=CARTESIAN_POINT('Ctrl Pts',(-0.943393153877153,-1.23737255934958,
2.65959141878237));
#262704=CARTESIAN_POINT('Ctrl Pts',(-0.912276745096169,-1.26048929177823,
2.66250478509144));
#262705=CARTESIAN_POINT('Ctrl Pts',(-0.874836809362642,-1.28619016569747,
2.66583707748606));
#262706=CARTESIAN_POINT('Ctrl Pts',(-0.869322997972508,-1.28992329802167,
2.66632357139289));
#262707=CARTESIAN_POINT('Ctrl Pts',(-0.860350154723142,-1.29591470486006,
2.66710818095526));
#262708=CARTESIAN_POINT('Ctrl Pts',(-0.856905878619585,-1.2981947570607,
2.66740768335076));
#262709=CARTESIAN_POINT('Ctrl Pts',(-0.850758055354086,-1.30222938384827,
2.66793924668592));
#262710=CARTESIAN_POINT('Ctrl Pts',(-0.848058103445263,-1.30398929857616,
2.6681716577564));
#262711=CARTESIAN_POINT('Ctrl Pts',(-0.842204289031549,-1.30777912969043,
2.66867330538221));
#262712=CARTESIAN_POINT('Ctrl Pts',(-0.839048552356202,-1.30980603301041,
2.66894234268938));
#262713=CARTESIAN_POINT('Ctrl Pts',(-0.830195976003729,-1.31544684601059,
2.66969324906925));
#262714=CARTESIAN_POINT('Ctrl Pts',(-0.824482818683226,-1.31903519640998,
2.67017346945639));
#262715=CARTESIAN_POINT('Ctrl Pts',(-0.790235631203481,-1.34023589912645,
2.67302717577542));
#262716=CARTESIAN_POINT('Ctrl Pts',(-0.761158915107036,-1.35696062934189,
2.67534728406832));
#262717=CARTESIAN_POINT('Ctrl Pts',(-0.580179981659949,-1.4534084906595,
2.68931552706292));
#262718=CARTESIAN_POINT('Ctrl Pts',(-0.416494468965732,-1.50849210368012,
2.70009826825702));
#262719=CARTESIAN_POINT('Ctrl Pts',(-0.221557597978971,-1.53985779190144,
2.71368259492742));
#262720=CARTESIAN_POINT('Ctrl Pts',(-0.195913525058172,-1.5433300181157,
2.7154803715659));
#262721=CARTESIAN_POINT('Ctrl Pts',(-0.160863244168044,-1.54718823118976,
2.71795779258158));
#262722=CARTESIAN_POINT('Ctrl Pts',(-0.151521547159138,-1.5481310086368,
2.71862001843417));
#262723=CARTESIAN_POINT('Ctrl Pts',(-0.13666878387214,-1.54949425129131,
2.71967624306559));
#262724=CARTESIAN_POINT('Ctrl Pts',(-0.131162912912977,-1.54997002555289,
2.72006850591722));
#262725=CARTESIAN_POINT('Ctrl Pts',(-0.11987650525895,-1.55088474110086,
2.72087414087667));
#262726=CARTESIAN_POINT('Ctrl Pts',(-0.11409582319336,-1.55132072704217,
2.7212875988703));
#262727=CARTESIAN_POINT('Ctrl Pts',(-0.100743303483416,-1.55225275484565,
2.72224460354692));
#262728=CARTESIAN_POINT('Ctrl Pts',(-0.093170058503897,-1.5527257209637,
2.72278886228998));
#262729=CARTESIAN_POINT('Ctrl Pts',(-0.06926787321072,-1.55404297123155,
2.72451142882781));
#262730=CARTESIAN_POINT('Ctrl Pts',(-0.0529293998675839,-1.55468518852481,
2.7256959923748));
#262731=CARTESIAN_POINT('Ctrl Pts',(0.0283501065787997,-1.55659736144991,
2.73162629913285));
#262732=CARTESIAN_POINT('Ctrl Pts',(0.0933072134609718,-1.5540562042871,
2.73648838369896));
#262733=CARTESIAN_POINT('Ctrl Pts',(0.223011635854469,-1.54082079516736,
2.74643428385114));
#262734=CARTESIAN_POINT('Ctrl Pts',(0.287627980718051,-1.53007584740424,
2.75150974494844));
#262735=CARTESIAN_POINT('Ctrl Pts',(0.375845769790922,-1.50961962402928,
2.75853082719658));
#262736=CARTESIAN_POINT('Ctrl Pts',(0.400179418852243,-1.50335222855512,
2.76047689001292));
#262737=CARTESIAN_POINT('Ctrl Pts',(0.482864518482418,-1.47990582537885,
2.76710497754921));
#262738=CARTESIAN_POINT('Ctrl Pts',(0.540362574835862,-1.45989369333721,
2.77174228132225));
#262739=CARTESIAN_POINT('Ctrl Pts',(0.603913458445661,-1.43350354150583,
2.77679890775196));
#262740=CARTESIAN_POINT('Ctrl Pts',(0.611256296257649,-1.4303879251203,
2.77738206110409));
#262741=CARTESIAN_POINT('Ctrl Pts',(0.622302541884912,-1.42560032987945,
2.77825731767137));
#262742=CARTESIAN_POINT('Ctrl Pts',(0.626023748415112,-1.42397016177547,
2.77855182259394));
#262743=CARTESIAN_POINT('Ctrl Pts',(0.632680925735021,-1.42102267775762,
2.77907800881327));
#262744=CARTESIAN_POINT('Ctrl Pts',(0.635619221716408,-1.41971081919212,
2.77931001154286));
#262745=CARTESIAN_POINT('Ctrl Pts',(0.642019359098197,-1.41682950250657,
2.77981482380017));
#262746=CARTESIAN_POINT('Ctrl Pts',(0.645479521440103,-1.41525647317628,
2.78008741166917));
#262747=CARTESIAN_POINT('Ctrl Pts',(0.655276966453399,-1.41075903661987,
2.78085839519975));
#262748=CARTESIAN_POINT('Ctrl Pts',(0.66160048975873,-1.40780458835677,
2.78135499726987));
#262749=CARTESIAN_POINT('Ctrl Pts',(0.702294004470904,-1.38845719583962,
2.78454559791216));
#262750=CARTESIAN_POINT('Ctrl Pts',(0.736075590181329,-1.37084775988776,
2.78717046325614));
#262751=CARTESIAN_POINT('Ctrl Pts',(0.864663726083719,-1.29769215027956,
2.7972012688602));
#262752=CARTESIAN_POINT('Ctrl Pts',(0.954130363923101,-1.23340472004064,
2.80428568144567));
#262753=CARTESIAN_POINT('Ctrl Pts',(1.0924122186762,-1.10991863187252,2.81660083761174));
#262754=CARTESIAN_POINT('Ctrl Pts',(1.14499703284813,-1.05558663847816,
2.82169748327598));
#262755=CARTESIAN_POINT('Ctrl Pts',(1.20096509202446,-0.988636094904325,
2.82779357805644));
#262756=CARTESIAN_POINT('Ctrl Pts',(1.20840311233166,-0.979530696410439,
2.82861886537459));
#262757=CARTESIAN_POINT('Ctrl Pts',(1.22032954586665,-0.964588123836426,
2.82996765162779));
#262758=CARTESIAN_POINT('Ctrl Pts',(1.22488108698391,-0.958801735787404,
2.83048862698344));
#262759=CARTESIAN_POINT('Ctrl Pts',(1.23292513864038,-0.948424547906283,
2.83142070051063));
#262760=CARTESIAN_POINT('Ctrl Pts',(1.23643353756728,-0.943846187735028,
2.83183116191293));
#262761=CARTESIAN_POINT('Ctrl Pts',(1.24378996623189,-0.934134853196116,
2.83270026469177));
#262762=CARTESIAN_POINT('Ctrl Pts',(1.24763185863574,-0.928997388099676,
2.83315913567376));
#262763=CARTESIAN_POINT('Ctrl Pts',(1.25776375913431,-0.915272572501554,
2.83438273642862));
#262764=CARTESIAN_POINT('Ctrl Pts',(1.26399748739438,-0.906644305757947,
2.83514961951849));
#262765=CARTESIAN_POINT('Ctrl Pts',(1.29361765540512,-0.86474698709582,
2.83886292879876));
#262766=CARTESIAN_POINT('Ctrl Pts',(1.3157798722374,-0.830636352481715,
2.84185504503788));
#262767=CARTESIAN_POINT('Ctrl Pts',(1.41280088785832,-0.66766500870913,
2.85602404337296));
#262768=CARTESIAN_POINT('Ctrl Pts',(1.47022494052532,-0.529346745876509,
2.86779386198882));
#262769=CARTESIAN_POINT('Ctrl Pts',(1.51640914243423,-0.348567405116211,
2.8820002333459));
#262770=CARTESIAN_POINT('Ctrl Pts',(1.52439753028294,-0.311783045213684,
2.88482721174136));
#262771=CARTESIAN_POINT('Ctrl Pts',(1.53221319825499,-0.268228907256127,
2.88807387336371));
#262772=CARTESIAN_POINT('Ctrl Pts',(1.53334035109987,-0.261708623170449,
2.88855728202526));
#262773=CARTESIAN_POINT('Ctrl Pts',(1.53510144267666,-0.251119031949921,
2.88933790610767));
#262774=CARTESIAN_POINT('Ctrl Pts',(1.53576087317674,-0.247054141826135,
2.88963648593991));
#262775=CARTESIAN_POINT('Ctrl Pts',(1.53690744903566,-0.239804343712694,
2.89016704834123));
#262776=CARTESIAN_POINT('Ctrl Pts',(1.53740084834131,-0.236620502888031,
2.89039937575605));
#262777=CARTESIAN_POINT('Ctrl Pts',(1.53844854508629,-0.229718212893933,
2.89090157008159));
#262778=CARTESIAN_POINT('Ctrl Pts',(1.53899925519365,-0.225999284372101,
2.89117123375325));
#262779=CARTESIAN_POINT('Ctrl Pts',(1.54050637653601,-0.215560713225502,
2.89192566935078));
#262780=CARTESIAN_POINT('Ctrl Pts',(1.54143231378084,-0.208836643731767,
2.89240876752484));
#262781=CARTESIAN_POINT('Ctrl Pts',(1.5467676100949,-0.168121967208169,
2.89531776400866));
#262782=CARTESIAN_POINT('Ctrl Pts',(1.5500969398411,-0.133996135898236,
2.89768784641757));
#262783=CARTESIAN_POINT('Ctrl Pts',(1.55755985801762,-0.0178999546183899,
2.90560569119024));
#262784=CARTESIAN_POINT('Ctrl Pts',(1.55633654998758,0.0642802138626112,
2.91097104270541));
#262785=CARTESIAN_POINT('Ctrl Pts',(1.53857498879349,0.25269671574714,2.92343378259378));
#262786=CARTESIAN_POINT('Ctrl Pts',(1.51751547903197,0.35806481569268,2.93053979639105));
#262787=CARTESIAN_POINT('Ctrl Pts',(1.482271045949,0.471799359505524,2.93885597595728));
#262788=CARTESIAN_POINT('Ctrl Pts',(1.47861538631174,0.483134158211466,
2.9396918199761));
#262789=CARTESIAN_POINT('Ctrl Pts',(1.47247539816963,0.501449227225489,
2.94105444354732));
#262790=CARTESIAN_POINT('Ctrl Pts',(1.47007067159434,0.508455841538123,
2.94157861202159));
#262791=CARTESIAN_POINT('Ctrl Pts',(1.46570288103446,0.5208921647549,2.94251425181334));
#262792=CARTESIAN_POINT('Ctrl Pts',(1.46375944703422,0.52632866381182,2.94292506789212));
#262793=CARTESIAN_POINT('Ctrl Pts',(1.45960137890462,0.537759143482083,
2.94379270033739));
#262794=CARTESIAN_POINT('Ctrl Pts',(1.45737999025646,0.543750534206534,
2.94424973476265));
#262795=CARTESIAN_POINT('Ctrl Pts',(1.45140027483632,0.559578751723736,
2.94546322940269));
#262796=CARTESIAN_POINT('Ctrl Pts',(1.44757892383351,0.569391241871289,
2.94622178030161));
#262797=CARTESIAN_POINT('Ctrl Pts',(1.44068771213679,0.586568683636156,
2.94756096891561));
#262798=CARTESIAN_POINT('Ctrl Pts',(1.43766040000972,0.593949879505714,
2.94814012489374));
#262799=CARTESIAN_POINT('Ctrl Pts',(1.43457668232327,0.601306903780717,
2.94872114469929));
#262800=CARTESIAN_POINT('Origin',(0.,0.,-1.29405622560371));
#262801=CARTESIAN_POINT('',(1.43457681153698,0.601306595507149,3.78763867041446));
#262802=CARTESIAN_POINT('',(1.43457668196675,0.601306904631308,3.65081500619461));
#262803=CARTESIAN_POINT('',(1.43457668357355,0.601306900797845,-1.29405622560371));
#262804=CARTESIAN_POINT('',(-1.55549981857965,-0.000751264718236687,3.39526827503829));
#262805=CARTESIAN_POINT('Ctrl Pts',(1.43457681153698,0.601306595507149,
3.78763867041446));
#262806=CARTESIAN_POINT('Ctrl Pts',(1.45228495682761,0.559059105126902,
3.78410173349879));
#262807=CARTESIAN_POINT('Ctrl Pts',(1.46812981601876,0.516022379834169,
3.78058974358071));
#262808=CARTESIAN_POINT('Ctrl Pts',(1.48860755329112,0.451766629824114,
3.77553199083611));
#262809=CARTESIAN_POINT('Ctrl Pts',(1.4947295481773,0.43107915613783,3.7739312732006));
#262810=CARTESIAN_POINT('Ctrl Pts',(1.5020235734551,0.404403778784375,3.77190807115718));
#262811=CARTESIAN_POINT('Ctrl Pts',(1.50359314973623,0.398528386534485,
3.77146496846811));
#262812=CARTESIAN_POINT('Ctrl Pts',(1.50603094392167,0.38918354821158,3.77076436611229));
#262813=CARTESIAN_POINT('Ctrl Pts',(1.50692170200068,0.385720135578987,
3.77050560992117));
#262814=CARTESIAN_POINT('Ctrl Pts',(1.50858835203985,0.379146029881205,
3.77001620077042));
#262815=CARTESIAN_POINT('Ctrl Pts',(1.50936656214683,0.376036047720497,
3.76978542472547));
#262816=CARTESIAN_POINT('Ctrl Pts',(1.51116273365963,0.36876254236952,3.76924740410533));
#262817=CARTESIAN_POINT('Ctrl Pts',(1.51217310828068,0.364597191476883,
3.76894059650567));
#262818=CARTESIAN_POINT('Ctrl Pts',(1.51538571844277,0.351109842973347,
3.76795120853024));
#262819=CARTESIAN_POINT('Ctrl Pts',(1.5175191280994,0.341771422989115,3.7672724200373));
#262820=CARTESIAN_POINT('Ctrl Pts',(1.53684926574886,0.253407332177902,
3.76090308475515));
#262821=CARTESIAN_POINT('Ctrl Pts',(1.54794717545517,0.173160517748061,
3.7555198102427));
#262822=CARTESIAN_POINT('Ctrl Pts',(1.56056567214749,-0.0388810575686845,
3.74150111489887));
#262823=CARTESIAN_POINT('Ctrl Pts',(1.55169748158616,-0.170609119704074,
3.73295215226419));
#262824=CARTESIAN_POINT('Ctrl Pts',(1.52296156721753,-0.316986740024555,
3.722592210792));
#262825=CARTESIAN_POINT('Ctrl Pts',(1.51926228542067,-0.334267246674258,
3.72135625840327));
#262826=CARTESIAN_POINT('Ctrl Pts',(1.51368930793458,-0.358292948888097,
3.7196181087253));
#262827=CARTESIAN_POINT('Ctrl Pts',(1.51206317070268,-0.365094676910799,
3.71912381141409));
#262828=CARTESIAN_POINT('Ctrl Pts',(1.5090039472547,-0.377519547388339,
3.71821667831772));
#262829=CARTESIAN_POINT('Ctrl Pts',(1.50758514848097,-0.383146107776329,
3.71780430742775));
#262830=CARTESIAN_POINT('Ctrl Pts',(1.50464970696429,-0.394518469808338,
3.7169675612951));
#262831=CARTESIAN_POINT('Ctrl Pts',(1.50313155450186,-0.4002637777037,3.71654314349472));
#262832=CARTESIAN_POINT('Ctrl Pts',(1.49930956471333,-0.414399302433667,
3.71549466496931));
#262833=CARTESIAN_POINT('Ctrl Pts',(1.4969682048874,-0.42277906824087,3.71486939913729));
#262834=CARTESIAN_POINT('Ctrl Pts',(1.48802499017834,-0.453781028454427,
3.71254204715143));
#262835=CARTESIAN_POINT('Ctrl Pts',(1.48097992077509,-0.476270883424295,
3.7108256743585));
#262836=CARTESIAN_POINT('Ctrl Pts',(1.42411971780435,-0.644303145615583,
3.69778134956352));
#262837=CARTESIAN_POINT('Ctrl Pts',(1.35347502552335,-0.781874651013664,
3.68571967058551));
#262838=CARTESIAN_POINT('Ctrl Pts',(1.25215522599585,-0.923086737694484,
3.672359514497));
#262839=CARTESIAN_POINT('Ctrl Pts',(1.24015883741703,-0.939142134830813,
3.67082634275174));
#262840=CARTESIAN_POINT('Ctrl Pts',(1.20673646821736,-0.982115403112518,
3.66669195004829));
#262841=CARTESIAN_POINT('Ctrl Pts',(1.18472075176358,-1.00856371279372,
3.66411343206859));
#262842=CARTESIAN_POINT('Ctrl Pts',(1.15759680630836,-1.03903353441394,
3.66112193902722));
#262843=CARTESIAN_POINT('Ctrl Pts',(1.15332019217965,-1.04377851562435,
3.66065546216106));
#262844=CARTESIAN_POINT('Ctrl Pts',(1.14630307427229,-1.05146835008178,
3.65989865350859));
#262845=CARTESIAN_POINT('Ctrl Pts',(1.14358022018729,-1.05442909211347,
3.65960706512636));
#262846=CARTESIAN_POINT('Ctrl Pts',(1.13868569475551,-1.05970997780205,
3.65908666829663));
#262847=CARTESIAN_POINT('Ctrl Pts',(1.13651837895164,-1.06203405003917,
3.65885754132213));
#262848=CARTESIAN_POINT('Ctrl Pts',(1.13178399489142,-1.06707976985674,
3.65835986677598));
#262849=CARTESIAN_POINT('Ctrl Pts',(1.12921422906795,-1.06979879977451,
3.65809153060942));
#262850=CARTESIAN_POINT('Ctrl Pts',(1.12192167289263,-1.07745938789422,
3.65733500208633));
#262851=CARTESIAN_POINT('Ctrl Pts',(1.11717600594268,-1.08237920758373,
3.65684852594792));
#262852=CARTESIAN_POINT('Ctrl Pts',(1.08699520392428,-1.11325758465683,
3.65379006558649));
#262853=CARTESIAN_POINT('Ctrl Pts',(1.06068682475235,-1.1383518851365,3.65128112577189));
#262854=CARTESIAN_POINT('Ctrl Pts',(0.964226133867791,-1.22411000159353,
3.64251465889047));
#262855=CARTESIAN_POINT('Ctrl Pts',(0.889556521303112,-1.27940194143842,
3.63648742405289));
#262856=CARTESIAN_POINT('Ctrl Pts',(0.729795156973847,-1.37691581603811,
3.62413543362215));
#262857=CARTESIAN_POINT('Ctrl Pts',(0.644889292852592,-1.41866554003948,
3.61782900111829));
#262858=CARTESIAN_POINT('Ctrl Pts',(0.545593974309176,-1.45672567951637,
3.61040227455098));
#262859=CARTESIAN_POINT('Ctrl Pts',(0.534409140939756,-1.4608659576953,
3.60956527654516));
#262860=CARTESIAN_POINT('Ctrl Pts',(0.516316624485444,-1.46732766550339,
3.60821009075901));
#262861=CARTESIAN_POINT('Ctrl Pts',(0.509438151575961,-1.46972994156417,
3.60769458138776));
#262862=CARTESIAN_POINT('Ctrl Pts',(0.497137138509152,-1.47392928816994,
3.60677203736411));
#262863=CARTESIAN_POINT('Ctrl Pts',(0.491721058912517,-1.47574499139884,
3.6063656254041));
#262864=CARTESIAN_POINT('Ctrl Pts',(0.480349156264552,-1.47948779073394,
3.60551177679746));
#262865=CARTESIAN_POINT('Ctrl Pts',(0.47439146861482,-1.48140884540511,
3.6050641500061));
#262866=CARTESIAN_POINT('Ctrl Pts',(0.458722597262361,-1.48635705623752,
3.60388600257941));
#262867=CARTESIAN_POINT('Ctrl Pts',(0.448993173344979,-1.48932496152393,
3.60315356147507));
#262868=CARTESIAN_POINT('Ctrl Pts',(0.404420976842879,-1.50244500610665,
3.59979351815833));
#262869=CARTESIAN_POINT('Ctrl Pts',(0.369261360520735,-1.51147046407328,
3.59712986563063));
#262870=CARTESIAN_POINT('Ctrl Pts',(0.201730177319029,-1.5482814758348,
3.58436385052272));
#262871=CARTESIAN_POINT('Ctrl Pts',(0.066432027133175,-1.55995042232364,
3.57376843586547));
#262872=CARTESIAN_POINT('Ctrl Pts',(-0.124291199208441,-1.55152691528764,
3.55907537328113));
#262873=CARTESIAN_POINT('Ctrl Pts',(-0.179783991445488,-1.54607999382093,
3.55484037053534));
#262874=CARTESIAN_POINT('Ctrl Pts',(-0.242631479585287,-1.53648034316866,
3.55016963475518));
#262875=CARTESIAN_POINT('Ctrl Pts',(-0.250383073118482,-1.53523620444844,
3.5495957727605));
#262876=CARTESIAN_POINT('Ctrl Pts',(-0.262075895247744,-1.53326857584135,
3.54873382976801));
#262877=CARTESIAN_POINT('Ctrl Pts',(-0.26602413752954,-1.5325884835016,
3.54844342062868));
#262878=CARTESIAN_POINT('Ctrl Pts',(-0.273098342554592,-1.53134177676573,
3.54792428115634));
#262879=CARTESIAN_POINT('Ctrl Pts',(-0.276225222729987,-1.5307808363484,
3.54769523900785));
#262880=CARTESIAN_POINT('Ctrl Pts',(-0.283043043753944,-1.52953619603863,
3.54719676566028));
#262881=CARTESIAN_POINT('Ctrl Pts',(-0.286733230157128,-1.528848715583,
3.54692755129187));
#262882=CARTESIAN_POINT('Ctrl Pts',(-0.297192987953784,-1.5268608629737,
3.54616604130273));
#262883=CARTESIAN_POINT('Ctrl Pts',(-0.303956569229325,-1.52552881837807,
3.54567549797882));
#262884=CARTESIAN_POINT('Ctrl Pts',(-0.347493136481235,-1.51665352095195,
3.5425286608509));
#262885=CARTESIAN_POINT('Ctrl Pts',(-0.383995410676809,-1.50782541677269,
3.539939698296));
#262886=CARTESIAN_POINT('Ctrl Pts',(-0.522902388275454,-1.4688577774429,
3.53015243409652));
#262887=CARTESIAN_POINT('Ctrl Pts',(-0.622426285678056,-1.42953110078364,
3.52326086316968));
#262888=CARTESIAN_POINT('Ctrl Pts',(-0.787591802583994,-1.34371936694108,
3.51091781051548));
#262889=CARTESIAN_POINT('Ctrl Pts',(-0.855123298424616,-1.30178490941716,
3.5055716927596));
#262890=CARTESIAN_POINT('Ctrl Pts',(-0.928667192730548,-1.24791688309828,
3.49920368167366));
#262891=CARTESIAN_POINT('Ctrl Pts',(-0.938100521604567,-1.24084112597254,
3.49837598998781));
#262892=CARTESIAN_POINT('Ctrl Pts',(-0.953261431373565,-1.22919752048136,
3.49702742177383));
#262893=CARTESIAN_POINT('Ctrl Pts',(-0.959038918513254,-1.22469516630268,
3.49650911200703));
#262894=CARTESIAN_POINT('Ctrl Pts',(-0.969093940758407,-1.2167445784329,
3.49559919038582));
#262895=CARTESIAN_POINT('Ctrl Pts',(-0.973385442714616,-1.21331414466905,
3.49520829137425));
#262896=CARTESIAN_POINT('Ctrl Pts',(-0.982343395788234,-1.20607544575574,
3.49438693171287));
#262897=CARTESIAN_POINT('Ctrl Pts',(-0.987006071298748,-1.20226267572384,
3.49395629401762));
#262898=CARTESIAN_POINT('Ctrl Pts',(-0.999035001351912,-1.19230922374725,
3.49283712703259));
#262899=CARTESIAN_POINT('Ctrl Pts',(-1.00636672256549,-1.18612740926773,
3.49214693384171));
#262900=CARTESIAN_POINT('Ctrl Pts',(-1.02225315382704,-1.17247927927087,
3.49063345945227));
#262901=CARTESIAN_POINT('Ctrl Pts',(-1.03078415404837,-1.16498634579644,
3.48980910496562));
#262902=CARTESIAN_POINT('Ctrl Pts',(-1.05551298293407,-1.1427822894922,
3.4873848137032));
#262903=CARTESIAN_POINT('Ctrl Pts',(-1.07148275069573,-1.12782252353667,
3.48577467467052));
#262904=CARTESIAN_POINT('Ctrl Pts',(-1.12740088558028,-1.07318107590871,
3.47997283705036));
#262905=CARTESIAN_POINT('Ctrl Pts',(-1.16550020470256,-1.03167746573578,
3.47570772852948));
#262906=CARTESIAN_POINT('Ctrl Pts',(-1.2609046484283,-0.915703676367821,
3.46417932460461));
#262907=CARTESIAN_POINT('Ctrl Pts',(-1.31385835809563,-0.837955433560799,
3.4568287418661));
#262908=CARTESIAN_POINT('Ctrl Pts',(-1.3641631101764,-0.747483901960602,
3.44890655835622));
#262909=CARTESIAN_POINT('Ctrl Pts',(-1.36876930105928,-0.73901541395515,
3.44817089410334));
#262910=CARTESIAN_POINT('Ctrl Pts',(-1.39028693681688,-0.69856378795933,
3.44468628528528));
#262911=CARTESIAN_POINT('Ctrl Pts',(-1.40615955824313,-0.666036747091945,
3.44197096923252));
#262912=CARTESIAN_POINT('Ctrl Pts',(-1.42352145684948,-0.627063711645005,
3.43884151283026));
#262913=CARTESIAN_POINT('Ctrl Pts',(-1.42612130725718,-0.621128213395096,
3.43836822817792));
#262914=CARTESIAN_POINT('Ctrl Pts',(-1.43028585119029,-0.611456489184943,
3.43760261065442));
#262915=CARTESIAN_POINT('Ctrl Pts',(-1.4318731406569,-0.607730173971907,
3.43730897340904));
#262916=CARTESIAN_POINT('Ctrl Pts',(-1.43468059831586,-0.601067335704458,
3.43678637632814));
#262917=CARTESIAN_POINT('Ctrl Pts',(-1.43590633025794,-0.598133239860774,
3.43655708633019));
#262918=CARTESIAN_POINT('Ctrl Pts',(-1.43854663313726,-0.591758122095598,
3.43606072880717));
#262919=CARTESIAN_POINT('Ctrl Pts',(-1.43995785769421,-0.588315782235392,
3.43579386353481));
#262920=CARTESIAN_POINT('Ctrl Pts',(-1.44389054899149,-0.578624009771287,
3.43504565321599));
#262921=CARTESIAN_POINT('Ctrl Pts',(-1.44638381597577,-0.572363104544709,
3.43456596491598));
#262922=CARTESIAN_POINT('Ctrl Pts',(-1.46137739088142,-0.533988661253052,
3.43164697466891));
#262923=CARTESIAN_POINT('Ctrl Pts',(-1.47284955156609,-0.501480235914487,
3.42926425445776));
#262924=CARTESIAN_POINT('Ctrl Pts',(-1.53105158791671,-0.317262296235985,
3.41611746690408));
#262925=CARTESIAN_POINT('Ctrl Pts',(-1.55542315334262,-0.159487272665282,
3.4060917948684));
#262926=CARTESIAN_POINT('Ctrl Pts',(-1.55549981857965,-0.000751264718236687,
3.39526827503829));
#262927=CARTESIAN_POINT('Ctrl Pts',(-1.55549981945131,-0.000749457767515238,
3.39526815183013));
#262928=CARTESIAN_POINT('Ctrl Pts',(-1.55551551317976,0.031822880291549,
3.39304718442064));
#262929=CARTESIAN_POINT('Ctrl Pts',(-1.55450810755596,0.0643860290742983,
3.39080044892672));
#262930=CARTESIAN_POINT('Ctrl Pts',(-1.55193830940151,0.105561257287131,
3.38791462042648));
#262931=CARTESIAN_POINT('Ctrl Pts',(-1.55132467008113,0.114225469361474,
3.38730486765438));
#262932=CARTESIAN_POINT('Ctrl Pts',(-1.55015512784323,0.128983600474185,
3.38626174224459));
#262933=CARTESIAN_POINT('Ctrl Pts',(-1.54963576541783,0.135080280521943,
3.38582950756042));
#262934=CARTESIAN_POINT('Ctrl Pts',(-1.54859869653279,0.146459904282944,
3.38502019759924));
#262935=CARTESIAN_POINT('Ctrl Pts',(-1.5480898904487,0.151743587292015,
3.38464340535572));
#262936=CARTESIAN_POINT('Ctrl Pts',(-1.54697665844573,0.162715038651089,
3.38385883031495));
#262937=CARTESIAN_POINT('Ctrl Pts',(-1.54636788564916,0.168402274939897,
3.3834509167941));
#262938=CARTESIAN_POINT('Ctrl Pts',(-1.54490645612242,0.18137846361503,
3.38251736478529));
#262939=CARTESIAN_POINT('Ctrl Pts',(-1.54403356124884,0.188664950502778,
3.38199109819578));
#262940=CARTESIAN_POINT('Ctrl Pts',(-1.54112563059196,0.211565546626314,
3.38033047644349));
#262941=CARTESIAN_POINT('Ctrl Pts',(-1.53890510533234,0.227154644840348,
3.37919032517134));
#262942=CARTESIAN_POINT('Ctrl Pts',(-1.53053872248536,0.280117783514749,
3.37528220642439));
#262943=CARTESIAN_POINT('Ctrl Pts',(-1.52326517167634,0.317297210056309,
3.37247956685669));
#262944=CARTESIAN_POINT('Ctrl Pts',(-1.48094035748025,0.498302709708821,
3.35853604265877));
#262945=CARTESIAN_POINT('Ctrl Pts',(-1.4268472150639,0.636855835611352,
3.34682716900537));
#262946=CARTESIAN_POINT('Ctrl Pts',(-1.33727291321783,0.79525914961694,
3.33301825889263));
#262947=CARTESIAN_POINT('Ctrl Pts',(-1.31957184442428,0.824297610163576,
3.33047230154255));
#262948=CARTESIAN_POINT('Ctrl Pts',(-1.29725097816734,0.858350293523376,
3.32748900978086));
#262949=CARTESIAN_POINT('Ctrl Pts',(-1.2935339564547,0.863941684748613,
3.32699924052793));
#262950=CARTESIAN_POINT('Ctrl Pts',(-1.28770415471284,0.872589285154732,
3.32624210750205));
#262951=CARTESIAN_POINT('Ctrl Pts',(-1.28561649363749,0.87566219668557,
3.32597312880769));
#262952=CARTESIAN_POINT('Ctrl Pts',(-1.28172113572727,0.881351970200548,
3.32547525920051));
#262953=CARTESIAN_POINT('Ctrl Pts',(-1.27991643736251,0.883970745473139,
3.32524618162784));
#262954=CARTESIAN_POINT('Ctrl Pts',(-1.27579093688326,0.88991808606258,
3.32472608179312));
#262955=CARTESIAN_POINT('Ctrl Pts',(-1.27346513623701,0.893243114909643,
3.324435403479));
#262956=CARTESIAN_POINT('Ctrl Pts',(-1.26737734971728,0.901874276014599,
3.32368100305429));
#262957=CARTESIAN_POINT('Ctrl Pts',(-1.2635949954457,0.907166053004247,
3.3232186244172));
#262958=CARTESIAN_POINT('Ctrl Pts',(-1.2382670172783,0.942135885849864,
3.32016289002876));
#262959=CARTESIAN_POINT('Ctrl Pts',(-1.21570866804082,0.971070650456909,
3.31763357307961));
#262960=CARTESIAN_POINT('Ctrl Pts',(-1.16144304584891,1.03581606862865,
3.31190087639963));
#262961=CARTESIAN_POINT('Ctrl Pts',(-1.12906569480635,1.07101639464612,
3.30872835986349));
#262962=CARTESIAN_POINT('Ctrl Pts',(-1.02654759999703,1.17264775015576,
3.29920115594701));
#262963=CARTESIAN_POINT('Ctrl Pts',(-0.951802795982941,1.23408789430428,
3.29290931757748));
#262964=CARTESIAN_POINT('Ctrl Pts',(-0.846841718172696,1.3051249021125,
3.28433399908301));
#262965=CARTESIAN_POINT('Ctrl Pts',(-0.82135053929949,1.32131563591338,
3.28227091451346));
#262966=CARTESIAN_POINT('Ctrl Pts',(-0.783146223420403,1.34404826863669,
3.27919519350072));
#262967=CARTESIAN_POINT('Ctrl Pts',(-0.770787399388576,1.35117375560407,
3.27820267659231));
#262968=CARTESIAN_POINT('Ctrl Pts',(-0.748224082938496,1.3637723464734,
3.27639383215283));
#262969=CARTESIAN_POINT('Ctrl Pts',(-0.738053054623798,1.36930346053753,
3.27557959528765));
#262970=CARTESIAN_POINT('Ctrl Pts',(-0.722072087278263,1.37776430188822,
3.27430154645416));
#262971=CARTESIAN_POINT('Ctrl Pts',(-0.716303746362942,1.38077207076284,
3.2738404960097));
#262972=CARTESIAN_POINT('Ctrl Pts',(-0.710458372943106,1.38377351999047,
3.27337350397857));
#262973=CARTESIAN_POINT('Ctrl Pts',(-0.710399957552157,1.38380351012044,
3.27336883714324));
#262974=CARTESIAN_POINT('Ctrl Pts',(-0.710281781006218,1.38386417183291,
3.27335939600262));
#262975=CARTESIAN_POINT('Ctrl Pts',(-0.7102220197613,1.38389484324436,3.27335462169115));
#262976=CARTESIAN_POINT('Ctrl Pts',(-0.710119845631572,1.38394727396405,
3.27334645906318));
#262977=CARTESIAN_POINT('Ctrl Pts',(-0.710077433730436,1.3839690351952,
3.27334307081405));
#262978=CARTESIAN_POINT('Ctrl Pts',(-0.709988068657457,1.38401488256044,
3.27333593154164));
#262979=CARTESIAN_POINT('Ctrl Pts',(-0.709941115259242,1.3840389682553,
3.27333218050285));
#262980=CARTESIAN_POINT('Ctrl Pts',(-0.709842180129513,1.38408971267103,
3.27332427674834));
#262981=CARTESIAN_POINT('Ctrl Pts',(-0.709790198117694,1.38411637085501,
3.27332012401335));
#262982=CARTESIAN_POINT('Ctrl Pts',(-0.709680666593918,1.38417253463769,
3.2733113738032));
#262983=CARTESIAN_POINT('Ctrl Pts',(-0.709623116746646,1.38420203957417,
3.27330677630508));
#262984=CARTESIAN_POINT('Ctrl Pts',(-0.70950185288945,1.38426420017001,
3.27329708891478));
#262985=CARTESIAN_POINT('Ctrl Pts',(-0.709438138467444,1.38429685501836,
3.27329199899436));
#262986=CARTESIAN_POINT('Ctrl Pts',(-0.709303885421847,1.38436565054444,
3.27328127404572));
#262987=CARTESIAN_POINT('Ctrl Pts',(-0.709233346282192,1.38440179023404,
3.273275638982));
#262988=CARTESIAN_POINT('Ctrl Pts',(-0.709084713923514,1.38447792549329,
3.27326376545767));
#262989=CARTESIAN_POINT('Ctrl Pts',(-0.709006620095092,1.38451791984052,
3.27325752695537));
#262990=CARTESIAN_POINT('Ctrl Pts',(-0.708842071856696,1.38460217268322,
3.27324438214823));
#262991=CARTESIAN_POINT('Ctrl Pts',(-0.708755616693444,1.38464642968473,
3.27323747579176));
#262992=CARTESIAN_POINT('Ctrl Pts',(-0.708573453953337,1.38473965853182,
3.27322292405972));
#262993=CARTESIAN_POINT('Ctrl Pts',(-0.708477745443298,1.38478862855231,
3.27321527861989));
#262994=CARTESIAN_POINT('Ctrl Pts',(-0.708276101185557,1.38489177506655,
3.27319917088203));
#262995=CARTESIAN_POINT('Ctrl Pts',(-0.708170160205065,1.38494595141957,
3.27319070817865));
#262996=CARTESIAN_POINT('Ctrl Pts',(-0.707946962568743,1.38506005845577,
3.27317287900641));
#262997=CARTESIAN_POINT('Ctrl Pts',(-0.707829705892194,1.38511998570453,
3.27316351255163));
#262998=CARTESIAN_POINT('Ctrl Pts',(-0.707588120153607,1.38524341604903,
3.27314421487366));
#262999=CARTESIAN_POINT('Ctrl Pts',(-0.70746379316258,1.38530691576024,
3.27313428382644));
#263000=CARTESIAN_POINT('Ctrl Pts',(-0.702461597832995,1.38786092596588,
3.27273472001348));
#263001=CARTESIAN_POINT('Ctrl Pts',(-0.697570675714839,1.39032564430966,
3.27234418922685));
#263002=CARTESIAN_POINT('Ctrl Pts',(-0.686137757793286,1.39601160488472,
3.27143157018871));
#263003=CARTESIAN_POINT('Ctrl Pts',(-0.679585971804953,1.39921275266236,
3.27090879192916));
#263004=CARTESIAN_POINT('Ctrl Pts',(-0.662478951758425,1.40742260407319,
3.26954420132373));
#263005=CARTESIAN_POINT('Ctrl Pts',(-0.651889540458947,1.41235858094296,
3.26869990486133));
#263006=CARTESIAN_POINT('Ctrl Pts',(-0.571842095188852,1.44857859561112,
3.26231937269221));
#263007=CARTESIAN_POINT('Ctrl Pts',(-0.500237121934826,1.47483648988481,
3.25661335849307));
#263008=CARTESIAN_POINT('Ctrl Pts',(-0.321533724486945,1.52585311757628,
3.2423942515112));
#263009=CARTESIAN_POINT('Ctrl Pts',(-0.21317716024154,1.54472190463823,
3.23377630413257));
#263010=CARTESIAN_POINT('Ctrl Pts',(-0.0658559685848307,1.55456902334545,
3.22253667813031));
#263011=CARTESIAN_POINT('Ctrl Pts',(-0.0278879192548577,1.55571357150846,
3.21968519758869));
#263012=CARTESIAN_POINT('Ctrl Pts',(0.017000911691727,1.55542245532995,
3.21639460841116));
#263013=CARTESIAN_POINT('Ctrl Pts',(0.0239139970512186,1.55533153092179,
3.21589011161483));
#263014=CARTESIAN_POINT('Ctrl Pts',(0.0345836246196253,1.55512004200872,
3.21511520627182));
#263015=CARTESIAN_POINT('Ctrl Pts',(0.0383406033473937,1.55503195179263,
3.21484306197811));
#263016=CARTESIAN_POINT('Ctrl Pts',(0.0452726000767095,1.55484427893354,
3.21434229237984));
#263017=CARTESIAN_POINT('Ctrl Pts',(0.0484476123790022,1.55474858716306,
3.21411346139317));
#263018=CARTESIAN_POINT('Ctrl Pts',(0.0556210320237971,1.55451039154857,
3.21359764379745));
#263019=CARTESIAN_POINT('Ctrl Pts',(0.0596191909802766,1.55436218741715,
3.21331097787211));
#263020=CARTESIAN_POINT('Ctrl Pts',(0.0716935259977487,1.55386795810465,
3.21244763651832));
#263021=CARTESIAN_POINT('Ctrl Pts',(0.0797677893749526,1.55347439636167,
3.21187352897399));
#263022=CARTESIAN_POINT('Ctrl Pts',(0.15507294591503,1.54921512917367,3.20654602932862));
#263023=CARTESIAN_POINT('Ctrl Pts',(0.221999508046671,1.54104965111159,
3.20201055650979));
#263024=CARTESIAN_POINT('Ctrl Pts',(0.382992674229787,1.51069618754045,
3.19113545704856));
#263025=CARTESIAN_POINT('Ctrl Pts',(0.475920657562925,1.48404378345445,
3.18487707321645));
#263026=CARTESIAN_POINT('Ctrl Pts',(0.602760507023185,1.43451593337269,
3.17575331840211));
#263027=CARTESIAN_POINT('Ctrl Pts',(0.639170658572096,1.41866721852994,
3.17306421684574));
#263028=CARTESIAN_POINT('Ctrl Pts',(0.69050082763851,1.39394671175148,3.16914203717298));
#263029=CARTESIAN_POINT('Ctrl Pts',(0.70594234865254,1.38619053128106,3.16794459084792));
#263030=CARTESIAN_POINT('Ctrl Pts',(0.73331232641578,1.37186683086779,3.16578821511187));
#263031=CARTESIAN_POINT('Ctrl Pts',(0.745289958969322,1.3653968017026,3.16483267165329));
#263032=CARTESIAN_POINT('Ctrl Pts',(0.76329403627544,1.35536395145273,3.1633774712189));
#263033=CARTESIAN_POINT('Ctrl Pts',(0.76938411724057,1.35191616010507,3.16288191445814));
#263034=CARTESIAN_POINT('Ctrl Pts',(0.780365669575825,1.34560091355362,
3.16198219316066));
#263035=CARTESIAN_POINT('Ctrl Pts',(0.785265151926864,1.34274756987973,
3.16157854236464));
#263036=CARTESIAN_POINT('Ctrl Pts',(0.795754259779842,1.33656191611745,
3.1607095048516));
#263037=CARTESIAN_POINT('Ctrl Pts',(0.801338774282202,1.33322119846095,
3.16024381839727));
#263038=CARTESIAN_POINT('Ctrl Pts',(0.816314566616588,1.32413443064572,
3.15898678914332));
#263039=CARTESIAN_POINT('Ctrl Pts',(0.825665917885608,1.31832364863173,
3.15819309019915));
#263040=CARTESIAN_POINT('Ctrl Pts',(0.870280228598846,1.28994013809138,
3.15436328859284));
#263041=CARTESIAN_POINT('Ctrl Pts',(0.904680668575205,1.26605114664814,
3.15127878231632));
#263042=CARTESIAN_POINT('Ctrl Pts',(1.06041827369226,1.14831054178011,3.13667091107057));
#263043=CARTESIAN_POINT('Ctrl Pts',(1.16838432729194,1.03825254450101,3.12452442670456));
#263044=CARTESIAN_POINT('Ctrl Pts',(1.27758068440472,0.887931263723227,
3.11044394375497));
#263045=CARTESIAN_POINT('Ctrl Pts',(1.29583675966283,0.861070158552939,
3.10801519796255));
#263046=CARTESIAN_POINT('Ctrl Pts',(1.31679272047913,0.82805864518375,3.10515079325348));
#263047=CARTESIAN_POINT('Ctrl Pts',(1.32030954079294,0.822439608299907,
3.10466731934354));
#263048=CARTESIAN_POINT('Ctrl Pts',(1.32573140848259,0.813652349549277,
3.10391779410263));
#263049=CARTESIAN_POINT('Ctrl Pts',(1.32766120782145,0.810499618374063,
3.10365017836393));
#263050=CARTESIAN_POINT('Ctrl Pts',(1.33123163248425,0.80461961185084,3.10315352232265));
#263051=CARTESIAN_POINT('Ctrl Pts',(1.33287511131194,0.801894205656458,
3.10292430363258));
#263052=CARTESIAN_POINT('Ctrl Pts',(1.33660840669026,0.795660037311968,
3.10240220212653));
#263053=CARTESIAN_POINT('Ctrl Pts',(1.33869277680272,0.792148078439551,
3.10210967395048));
#263054=CARTESIAN_POINT('Ctrl Pts',(1.34410510315408,0.782946465496307,
3.1013472684211));
#263055=CARTESIAN_POINT('Ctrl Pts',(1.34741081520692,0.777243716799086,
3.10087878172937));
#263056=CARTESIAN_POINT('Ctrl Pts',(1.3697572451804,0.738122395296404,3.09769105710446));
#263057=CARTESIAN_POINT('Ctrl Pts',(1.38759098388224,0.704025182244774,
3.09504232460242));
#263058=CARTESIAN_POINT('Ctrl Pts',(1.40850880864417,0.660140968020444,
3.09174909346945));
#263059=CARTESIAN_POINT('Ctrl Pts',(1.41278418143391,0.650940877528165,
3.09106494698954));
#263060=CARTESIAN_POINT('Ctrl Pts',(1.42303060888839,0.628315217936988,
3.08939615253733));
#263061=CARTESIAN_POINT('Ctrl Pts',(1.428900212522,0.614849625316866,3.08841467113574));
#263062=CARTESIAN_POINT('Ctrl Pts',(1.43457670182626,0.601306857251181,
3.08743730443809));
#263063=CARTESIAN_POINT('',(-1.55549947507011,0.00127791103983615,3.25533765336848));
#263064=CARTESIAN_POINT('Ctrl Pts',(1.43457668232327,0.601306903780717,
2.94872114469929));
#263065=CARTESIAN_POINT('Ctrl Pts',(1.42245865255591,0.630217669365907,
2.95100436774854));
#263066=CARTESIAN_POINT('Ctrl Pts',(1.40946959757188,0.658755155633724,
2.95331658692606));
#263067=CARTESIAN_POINT('Ctrl Pts',(1.32947041243761,0.821300206040414,
2.96683563098988));
#263068=CARTESIAN_POINT('Ctrl Pts',(1.24424164167907,0.94544917436953,2.97866702762622));
#263069=CARTESIAN_POINT('Ctrl Pts',(1.11660624355328,1.08362363781819,2.9929963563998));
#263070=CARTESIAN_POINT('Ctrl Pts',(1.08956087377236,1.11081384470458,2.99587787148548));
#263071=CARTESIAN_POINT('Ctrl Pts',(1.05668376036441,1.14150941440539,2.99917821109605));
#263072=CARTESIAN_POINT('Ctrl Pts',(1.05180273231258,1.14600843325333,2.99966318772031));
#263073=CARTESIAN_POINT('Ctrl Pts',(1.04384250819401,1.1532519578066,3.00044583753614));
#263074=CARTESIAN_POINT('Ctrl Pts',(1.04078100297414,1.15601564219912,3.0007448864676));
#263075=CARTESIAN_POINT('Ctrl Pts',(1.0353080083478,1.16091686239938,3.00127595736976));
#263076=CARTESIAN_POINT('Ctrl Pts',(1.0329008396858,1.16305910840185,3.00150832687416));
#263077=CARTESIAN_POINT('Ctrl Pts',(1.02767425360739,1.16768145381597,3.00201024118986));
#263078=CARTESIAN_POINT('Ctrl Pts',(1.02485251105918,1.17015882703852,3.00227958479922));
#263079=CARTESIAN_POINT('Ctrl Pts',(1.01692091170457,1.17707174503205,3.00303221637908));
#263080=CARTESIAN_POINT('Ctrl Pts',(1.01179096021632,1.18148427450294,3.00351384343232));
#263081=CARTESIAN_POINT('Ctrl Pts',(0.980793807567881,1.20779652631221,
3.00639438651572));
#263082=CARTESIAN_POINT('Ctrl Pts',(0.954242911156409,1.22888154295084,
3.00873874862865));
#263083=CARTESIAN_POINT('Ctrl Pts',(0.782171907016893,1.35658597745834,
3.02332864685264));
#263084=CARTESIAN_POINT('Ctrl Pts',(0.6197277517959,1.43807792081024,3.03463511473062));
#263085=CARTESIAN_POINT('Ctrl Pts',(0.428601843589367,1.49540842706723,
3.04846325505601));
#263086=CARTESIAN_POINT('Ctrl Pts',(0.410187001979165,1.50056405116865,
3.04979845186935));
#263087=CARTESIAN_POINT('Ctrl Pts',(0.384441582809637,1.5072627174754,3.05167129474415));
#263088=CARTESIAN_POINT('Ctrl Pts',(0.377187299924965,1.50909441962825,
3.05219967290755));
#263089=CARTESIAN_POINT('Ctrl Pts',(0.364634735537623,1.51216777190815,
3.0531152458029));
#263090=CARTESIAN_POINT('Ctrl Pts',(0.359342581925982,1.51343409774031,
3.05350164352768));
#263091=CARTESIAN_POINT('Ctrl Pts',(0.348355610294849,1.5160022242349,3.05430470821913));
#263092=CARTESIAN_POINT('Ctrl Pts',(0.342659894783035,1.51729976270497,
3.05472150468727));
#263093=CARTESIAN_POINT('Ctrl Pts',(0.329267193135695,1.52027149264878,
3.05570274809804));
#263094=CARTESIAN_POINT('Ctrl Pts',(0.321564593725083,1.52191934860861,
3.05626802540339));
#263095=CARTESIAN_POINT('Ctrl Pts',(0.296270532187378,1.52713004429368,
3.05812756139498));
#263096=CARTESIAN_POINT('Ctrl Pts',(0.278630476160886,1.53044680014764,
3.05942957310171));
#263097=CARTESIAN_POINT('Ctrl Pts',(0.236802024620758,1.53756445286809,
3.06253042528793));
#263098=CARTESIAN_POINT('Ctrl Pts',(0.212574118963641,1.54110082946908,
3.0643371345177));
#263099=CARTESIAN_POINT('Ctrl Pts',(0.0543418606711603,1.56039473933996,
3.07620905396344));
#263100=CARTESIAN_POINT('Ctrl Pts',(-0.0811324640171465,1.55922754567866,
3.08678189113481));
#263101=CARTESIAN_POINT('Ctrl Pts',(-0.269041554539805,1.53303778457616,
3.10137761908434));
#263102=CARTESIAN_POINT('Ctrl Pts',(-0.322930037961329,1.52259840227671,
3.10554464299519));
#263103=CARTESIAN_POINT('Ctrl Pts',(-0.383823573167472,1.5074223322848,
3.11015547717816));
#263104=CARTESIAN_POINT('Ctrl Pts',(-0.391472398761162,1.50545408141071,
3.1107328234122));
#263105=CARTESIAN_POINT('Ctrl Pts',(-0.403016460707738,1.50238954694443,
3.11160109628738));
#263106=CARTESIAN_POINT('Ctrl Pts',(-0.406922802407952,1.50133622225514,
3.11189436942759));
#263107=CARTESIAN_POINT('Ctrl Pts',(-0.413927678720256,1.49941804541915,
3.11241924823709));
#263108=CARTESIAN_POINT('Ctrl Pts',(-0.417027664726775,1.49855881620741,
3.11265116823625));
#263109=CARTESIAN_POINT('Ctrl Pts',(-0.423797474038313,1.49665978060452,
3.11315684161599));
#263110=CARTESIAN_POINT('Ctrl Pts',(-0.427466140915138,1.49561609281795,
3.11343036749624));
#263111=CARTESIAN_POINT('Ctrl Pts',(-0.437896536184823,1.49260726756071,
3.11420668572888));
#263112=CARTESIAN_POINT('Ctrl Pts',(-0.444648928289597,1.49060966290774,
3.11470764503976));
#263113=CARTESIAN_POINT('Ctrl Pts',(-0.488890511746678,1.47719399759256,
3.11798076965843));
#263114=CARTESIAN_POINT('Ctrl Pts',(-0.525954224242145,1.46440733520357,
3.12067966989121));
#263115=CARTESIAN_POINT('Ctrl Pts',(-0.672773715273248,1.40746074047854,
3.13134555018392));
#263116=CARTESIAN_POINT('Ctrl Pts',(-0.777815979175703,1.35224870075751,
3.13894557828339));
#263117=CARTESIAN_POINT('Ctrl Pts',(-0.930490623375034,1.24827056208346,
3.15127083069428));
#263118=CARTESIAN_POINT('Ctrl Pts',(-0.982932447592461,1.20740804818085,
3.1557760286771));
#263119=CARTESIAN_POINT('Ctrl Pts',(-1.0411808964787,1.15570510607355,3.16121937653398));
#263120=CARTESIAN_POINT('Ctrl Pts',(-1.04967885035192,1.147992269194,3.16202520269222));
#263121=CARTESIAN_POINT('Ctrl Pts',(-1.06342463163254,1.13523621293507,
3.16334845187816));
#263122=CARTESIAN_POINT('Ctrl Pts',(-1.06872388923758,1.13024884501007,
3.16386350909661));
#263123=CARTESIAN_POINT('Ctrl Pts',(-1.07815373615492,1.12124838262156,
3.16478902937418));
#263124=CARTESIAN_POINT('Ctrl Pts',(-1.08229743121077,1.11724915890713,
3.16519888983791));
#263125=CARTESIAN_POINT('Ctrl Pts',(-1.09027623244304,1.10946250000858,
3.16599430707404));
#263126=CARTESIAN_POINT('Ctrl Pts',(-1.09411405392934,1.10567795383662,
3.16637973413627));
#263127=CARTESIAN_POINT('Ctrl Pts',(-1.10438290736315,1.0954458329791,3.16741873040797));
#263128=CARTESIAN_POINT('Ctrl Pts',(-1.11077702985881,1.08896169007784,
3.16807391007661));
#263129=CARTESIAN_POINT('Ctrl Pts',(-1.13673711391532,1.06216958053223,
3.17076831420438));
#263130=CARTESIAN_POINT('Ctrl Pts',(-1.15580486766016,1.04138868791256,
3.17282870520902));
#263131=CARTESIAN_POINT('Ctrl Pts',(-1.20380218345447,0.986136319789469,
3.17823646081524));
#263132=CARTESIAN_POINT('Ctrl Pts',(-1.23181784886212,0.950909373012751,
3.18161740428921));
#263133=CARTESIAN_POINT('Ctrl Pts',(-1.28895833107738,0.872291271880543,
3.18901705356084));
#263134=CARTESIAN_POINT('Ctrl Pts',(-1.31750405972983,0.828545764783225,
3.19304683850954));
#263135=CARTESIAN_POINT('Ctrl Pts',(-1.39245855187102,0.699981865965765,
3.20458025825976));
#263136=CARTESIAN_POINT('Ctrl Pts',(-1.43324406485111,0.612152428725425,
3.21210845457625));
#263137=CARTESIAN_POINT('Ctrl Pts',(-1.46969263819697,0.5096388186464,3.22016516025574));
#263138=CARTESIAN_POINT('Ctrl Pts',(-1.47363274563239,0.49813123949159,
3.22105942646282));
#263139=CARTESIAN_POINT('Ctrl Pts',(-1.47896855035198,0.481929693052078,
3.22230319042214));
#263140=CARTESIAN_POINT('Ctrl Pts',(-1.48047755438171,0.47727394093664,
3.22265884746795));
#263141=CARTESIAN_POINT('Ctrl Pts',(-1.48287967441495,0.469741622874787,
3.22323132831454));
#263142=CARTESIAN_POINT('Ctrl Pts',(-1.48378643707873,0.466869500630587,
3.22344893560381));
#263143=CARTESIAN_POINT('Ctrl Pts',(-1.48568365230811,0.460798813716566,
3.22390741490636));
#263144=CARTESIAN_POINT('Ctrl Pts',(-1.48667212963436,0.457599651293138,
3.22414816644432));
#263145=CARTESIAN_POINT('Ctrl Pts',(-1.48908526833037,0.449699281870232,
3.22474064249161));
#263146=CARTESIAN_POINT('Ctrl Pts',(-1.4904980211127,0.444994417144961,
3.22509167906687));
#263147=CARTESIAN_POINT('Ctrl Pts',(-1.4934830516549,0.434879708684663,
3.22584265824799));
#263148=CARTESIAN_POINT('Ctrl Pts',(-1.49504828275043,0.429467835059389,
3.22624221020648));
#263149=CARTESIAN_POINT('Ctrl Pts',(-1.49940305727876,0.414098597418418,
3.22737082452772));
#263150=CARTESIAN_POINT('Ctrl Pts',(-1.50212282341242,0.404121533713502,
3.22809626407978));
#263151=CARTESIAN_POINT('Ctrl Pts',(-1.53832983940184,0.265883022023333,
3.23805792544598));
#263152=CARTESIAN_POINT('Ctrl Pts',(-1.55539054677746,0.13386765848789,
3.24654259388127));
#263153=CARTESIAN_POINT('Ctrl Pts',(-1.55549947507011,0.00127791103983615,
3.25533765336848));
#263154=CARTESIAN_POINT('Ctrl Pts',(-1.5554994762935,0.00127642103556679,
3.25533775220476));
#263155=CARTESIAN_POINT('Ctrl Pts',(-1.55556457573093,-0.0780564464206632,
3.26060013061482));
#263156=CARTESIAN_POINT('Ctrl Pts',(-1.5495606928194,-0.157269483732473,
3.26594478189099));
#263157=CARTESIAN_POINT('Ctrl Pts',(-1.53615483445118,-0.244729426438979,
3.2721277023867));
#263158=CARTESIAN_POINT('Ctrl Pts',(-1.53468696410739,-0.253771715318804,
3.2727702323005));
#263159=CARTESIAN_POINT('Ctrl Pts',(-1.53206754625742,-0.269053021556787,
3.27386194570828));
#263160=CARTESIAN_POINT('Ctrl Pts',(-1.53095752842476,-0.275298998777278,
3.27430982484675));
#263161=CARTESIAN_POINT('Ctrl Pts',(-1.52883382825815,-0.286838674369593,
3.27514045922882));
#263162=CARTESIAN_POINT('Ctrl Pts',(-1.52783077498162,-0.292134252067406,
3.27552287379926));
#263163=CARTESIAN_POINT('Ctrl Pts',(-1.5256990345478,-0.303077339597831,
3.27631572950416));
#263164=CARTESIAN_POINT('Ctrl Pts',(-1.52456646572806,-0.308723999289791,
3.27672628834616));
#263165=CARTESIAN_POINT('Ctrl Pts',(-1.52193129050685,-0.321494006526159,
3.2776581117536));
#263166=CARTESIAN_POINT('Ctrl Pts',(-1.52040998986305,-0.328613311729287,
3.2781799643184));
#263167=CARTESIAN_POINT('Ctrl Pts',(-1.51635981562754,-0.346936715384596,
3.27952931444606));
#263168=CARTESIAN_POINT('Ctrl Pts',(-1.51375675800904,-0.358123776593075,
3.28035916222648));
#263169=CARTESIAN_POINT('Ctrl Pts',(-1.49519692997988,-0.434067247794134,
3.28603482323786));
#263170=CARTESIAN_POINT('Ctrl Pts',(-1.47521598446976,-0.497758631914721,
3.29100915833726));
#263171=CARTESIAN_POINT('Ctrl Pts',(-1.42828360251659,-0.619389533929868,
3.3009335133554));
#263172=CARTESIAN_POINT('Ctrl Pts',(-1.40172659660111,-0.677347023317625,
3.30586499761823));
#263173=CARTESIAN_POINT('Ctrl Pts',(-1.34198748279839,-0.789061695121617,
3.31568894214456));
#263174=CARTESIAN_POINT('Ctrl Pts',(-1.30893197931883,-0.842761422371147,
3.3205721331193));
#263175=CARTESIAN_POINT('Ctrl Pts',(-1.25481325262656,-0.919778667336661,
3.3276976380773));
#263176=CARTESIAN_POINT('Ctrl Pts',(-1.23615560748826,-0.94470564615604,
3.33002403423597));
#263177=CARTESIAN_POINT('Ctrl Pts',(-1.21263038331133,-0.974244199820357,
3.33279022888197));
#263178=CARTESIAN_POINT('Ctrl Pts',(-1.20846673216654,-0.979404088667083,
3.33327379190739));
#263179=CARTESIAN_POINT('Ctrl Pts',(-1.20191228281821,-0.987421385032341,
3.33402549165318));
#263180=CARTESIAN_POINT('Ctrl Pts',(-1.19954406228006,-0.99029701132986,
3.33429518125567));
#263181=CARTESIAN_POINT('Ctrl Pts',(-1.19510555140728,-0.995647216658856,
3.33479703837405));
#263182=CARTESIAN_POINT('Ctrl Pts',(-1.19303791325238,-0.998123838458429,
3.3350293800104));
#263183=CARTESIAN_POINT('Ctrl Pts',(-1.18828160088191,-1.00378506499656,
3.33556057724508));
#263184=CARTESIAN_POINT('Ctrl Pts',(-1.18558782337883,-1.00696530915993,
3.33585905649905));
#263185=CARTESIAN_POINT('Ctrl Pts',(-1.17847662411039,-1.01529261837258,
3.33664092555214));
#263186=CARTESIAN_POINT('Ctrl Pts',(-1.1740381993345,-1.02042175860083,
3.33712283138497));
#263187=CARTESIAN_POINT('Ctrl Pts',(-1.14227753536441,-1.05664351425257,
3.3405297083049));
#263188=CARTESIAN_POINT('Ctrl Pts',(-1.11375443117199,-1.08666705944277,
3.3433731285709));
#263189=CARTESIAN_POINT('Ctrl Pts',(-1.05464705106878,-1.14410772890806,
3.34894111057736));
#263190=CARTESIAN_POINT('Ctrl Pts',(-1.02410877252334,-1.17152228698045,
3.35166435486929));
#263191=CARTESIAN_POINT('Ctrl Pts',(-0.921728772019352,-1.25636356849182,
3.36044439132946));
#263192=CARTESIAN_POINT('Ctrl Pts',(-0.845878469305043,-1.30863366995126,
3.36643636751983));
#263193=CARTESIAN_POINT('Ctrl Pts',(-0.73656342221112,-1.37046975170061,
3.37490143682063));
#263194=CARTESIAN_POINT('Ctrl Pts',(-0.70674059524315,-1.38608459200649,
3.37719346706223));
#263195=CARTESIAN_POINT('Ctrl Pts',(-0.662526312616567,-1.40743658802385,
3.38058367841519));
#263196=CARTESIAN_POINT('Ctrl Pts',(-0.648517389898912,-1.41394626156147,
3.38165667290346));
#263197=CARTESIAN_POINT('Ctrl Pts',(-0.623139855817195,-1.42528223361025,
3.38359994329796));
#263198=CARTESIAN_POINT('Ctrl Pts',(-0.611806183874596,-1.43018387043294,
3.38446763794292));
#263199=CARTESIAN_POINT('Ctrl Pts',(-0.594182710133811,-1.43755793206207,
3.38581719334363));
#263200=CARTESIAN_POINT('Ctrl Pts',(-0.587932945936292,-1.4401252548069,
3.38629584293086));
#263201=CARTESIAN_POINT('Ctrl Pts',(-0.581612273954868,-1.4426737040073,
3.38678003856248));
#263202=CARTESIAN_POINT('Ctrl Pts',(-0.581557804409939,-1.44269566214742,
3.38678421121533));
#263203=CARTESIAN_POINT('Ctrl Pts',(-0.581447687413543,-1.44274004602388,
3.38679264677229));
#263204=CARTESIAN_POINT('Ctrl Pts',(-0.581392039911287,-1.44276247162426,
3.38679690968066));
#263205=CARTESIAN_POINT('Ctrl Pts',(-0.581279534917941,-1.44280780287709,
3.38680552820755));
#263206=CARTESIAN_POINT('Ctrl Pts',(-0.581222677358193,-1.44283070839306,
3.38680988383171));
#263207=CARTESIAN_POINT('Ctrl Pts',(-0.58110771909995,-1.4428770123353,
3.38681869033094));
#263208=CARTESIAN_POINT('Ctrl Pts',(-0.581049618345017,-1.442900410612,
3.38682314121074));
#263209=CARTESIAN_POINT('Ctrl Pts',(-0.580932139514336,-1.44294771332037,
3.38683214084115));
#263210=CARTESIAN_POINT('Ctrl Pts',(-0.580872761377508,-1.44297161759573,
3.38683668959687));
#263211=CARTESIAN_POINT('Ctrl Pts',(-0.580752692522672,-1.44301994594932,
3.3868458876817));
#263212=CARTESIAN_POINT('Ctrl Pts',(-0.580692001736192,-1.44304436986515,
3.38685053701653));
#263213=CARTESIAN_POINT('Ctrl Pts',(-0.580569271179736,-1.4430937515746,
3.38685993904974));
#263214=CARTESIAN_POINT('Ctrl Pts',(-0.580507231346287,-1.44311870919425,
3.38686469175348));
#263215=CARTESIAN_POINT('Ctrl Pts',(-0.580381765175071,-1.4431691728019,
3.38687430340046));
#263216=CARTESIAN_POINT('Ctrl Pts',(-0.580318338759307,-1.44319467861169,
3.3868791623502));
#263217=CARTESIAN_POINT('Ctrl Pts',(-0.58020870096192,-1.44323875911389,
3.38688756146686));
#263218=CARTESIAN_POINT('Ctrl Pts',(-0.580162490370144,-1.44325733576796,
3.38689110156763));
#263219=CARTESIAN_POINT('Ctrl Pts',(-0.580065254054557,-1.44329641933415,
3.38689855066025));
#263220=CARTESIAN_POINT('Ctrl Pts',(-0.580014228133236,-1.44331692576065,
3.38690245966864));
#263221=CARTESIAN_POINT('Ctrl Pts',(-0.579906847384672,-1.44336007359386,
3.38691068594024));
#263222=CARTESIAN_POINT('Ctrl Pts',(-0.579850492318087,-1.44338271440633,
3.38691500322352));
#263223=CARTESIAN_POINT('Ctrl Pts',(-0.579731882508308,-1.44343035817603,
3.38692408977627));
#263224=CARTESIAN_POINT('Ctrl Pts',(-0.579669627474473,-1.44345536040586,
3.38692885907012));
#263225=CARTESIAN_POINT('Ctrl Pts',(-0.579538583315963,-1.4435079791753,
3.38693889825251));
#263226=CARTESIAN_POINT('Ctrl Pts',(-0.579469793839462,-1.44353559482344,
3.38694416817059));
#263227=CARTESIAN_POINT('Ctrl Pts',(-0.579324975309748,-1.44359372043994,
3.38695526265647));
#263228=CARTESIAN_POINT('Ctrl Pts',(-0.579248945826049,-1.44362422931685,
3.38696108726044));
#263229=CARTESIAN_POINT('Ctrl Pts',(-0.579088862447392,-1.4436884523993,
3.3869733512542));
#263230=CARTESIAN_POINT('Ctrl Pts',(-0.579004808014012,-1.44372216527224,
3.38697979068918));
#263231=CARTESIAN_POINT('Ctrl Pts',(-0.578827801267903,-1.44379314186904,
3.38699335127407));
#263232=CARTESIAN_POINT('Ctrl Pts',(-0.578734848304132,-1.44383040395578,
3.38700047247871));
#263233=CARTESIAN_POINT('Ctrl Pts',(-0.573298418678159,-1.44600909804026,
3.38741696348327));
#263234=CARTESIAN_POINT('Ctrl Pts',(-0.56794316612072,-1.44812083297473,
3.38782732404715));
#263235=CARTESIAN_POINT('Ctrl Pts',(-0.55581269380091,-1.45282660058535,
3.38875712065688));
#263236=CARTESIAN_POINT('Ctrl Pts',(-0.549030841810344,-1.45540304156594,
3.38927713457183));
#263237=CARTESIAN_POINT('Ctrl Pts',(-0.5315439608046,-1.46190672978584,
3.39061859530969));
#263238=CARTESIAN_POINT('Ctrl Pts',(-0.520813491094521,-1.46576381572419,
3.39144234652724));
#263239=CARTESIAN_POINT('Ctrl Pts',(-0.449184255053168,-1.49062522843342,
3.39694614317823));
#263240=CARTESIAN_POINT('Ctrl Pts',(-0.387082251491503,-1.50794404522555,
3.40174577732764));
#263241=CARTESIAN_POINT('Ctrl Pts',(-0.200863419202999,-1.54761393051519,
3.41622013688214));
#263242=CARTESIAN_POINT('Ctrl Pts',(-0.0749139098115009,-1.55879411021227,
3.42615277500801));
#263243=CARTESIAN_POINT('Ctrl Pts',(0.0850777475656494,-1.55354584464973,
3.43830130569816));
#263244=CARTESIAN_POINT('Ctrl Pts',(0.119114695138189,-1.55130752900714,
3.440855275023));
#263245=CARTESIAN_POINT('Ctrl Pts',(0.159809111012734,-1.54728387217716,
3.44385192284407));
#263246=CARTESIAN_POINT('Ctrl Pts',(0.166560342685347,-1.54657168920358,
3.44434717820296));
#263247=CARTESIAN_POINT('Ctrl Pts',(0.177043121451004,-1.54539642754252,
3.44511301251469));
#263248=CARTESIAN_POINT('Ctrl Pts',(0.180777905784097,-1.54496399139518,
3.44538523846394));
#263249=CARTESIAN_POINT('Ctrl Pts',(0.187710226967688,-1.54413584276426,
3.44588932641909));
#263250=CARTESIAN_POINT('Ctrl Pts',(0.190908075665918,-1.54374374078353,
3.44612137818574));
#263251=CARTESIAN_POINT('Ctrl Pts',(0.198190192746293,-1.54282787507327,
3.44664872775242));
#263252=CARTESIAN_POINT('Ctrl Pts',(0.202273612220895,-1.54229782839002,
3.44694366988646));
#263253=CARTESIAN_POINT('Ctrl Pts',(0.212912062093942,-1.54087393056,3.44771019041575));
#263254=CARTESIAN_POINT('Ctrl Pts',(0.219463670693843,-1.53995445303672,
3.44818037747277));
#263255=CARTESIAN_POINT('Ctrl Pts',(0.263209983521974,-1.53353007339282,
3.4513086209682));
#263256=CARTESIAN_POINT('Ctrl Pts',(0.300204156182742,-1.52671936599132,
3.45389952253976));
#263257=CARTESIAN_POINT('Ctrl Pts',(0.482334447487755,-1.48631099021652,
3.46654717759309));
#263258=CARTESIAN_POINT('Ctrl Pts',(0.622366138452038,-1.43332961786917,
3.47600213656755));
#263259=CARTESIAN_POINT('Ctrl Pts',(0.788364511324682,-1.34153617000343,
3.48888698906256));
#263260=CARTESIAN_POINT('Ctrl Pts',(0.823203841668285,-1.32044418391014,
3.49169105915656));
#263261=CARTESIAN_POINT('Ctrl Pts',(0.866059315765286,-1.29214353062344,
3.49529163781995));
#263262=CARTESIAN_POINT('Ctrl Pts',(0.874884495245487,-1.28618457156308,
3.49604147917818));
#263263=CARTESIAN_POINT('Ctrl Pts',(0.888927836291067,-1.27649078234281,
3.49724858264547));
#263264=CARTESIAN_POINT('Ctrl Pts',(0.894185392106557,-1.27281337903213,
3.49770366852515));
#263265=CARTESIAN_POINT('Ctrl Pts',(0.904125883549563,-1.26576850377727,
3.49857023271642));
#263266=CARTESIAN_POINT('Ctrl Pts',(0.908813145639846,-1.26240729684418,
3.49898146623335));
#263267=CARTESIAN_POINT('Ctrl Pts',(0.919439060930761,-1.25469766834677,
3.49991977866266));
#263268=CARTESIAN_POINT('Ctrl Pts',(0.925365722378492,-1.25033303648256,
3.50044747781748));
#263269=CARTESIAN_POINT('Ctrl Pts',(0.940674112759945,-1.23889086275214,
3.50182200395248));
#263270=CARTESIAN_POINT('Ctrl Pts',(0.950006852292963,-1.23174888785683,
3.5026713301628));
#263271=CARTESIAN_POINT('Ctrl Pts',(1.01856377937654,-1.17804236267732,
3.50899647575765));
#263272=CARTESIAN_POINT('Ctrl Pts',(1.07440649729285,-1.12734346779031,
3.51463791465493));
#263273=CARTESIAN_POINT('Ctrl Pts',(1.2052041757994,-0.990017760278477,
3.52914230118053));
#263274=CARTESIAN_POINT('Ctrl Pts',(1.2746855521503,-0.898792283161244,
3.53813530052346));
#263275=CARTESIAN_POINT('Ctrl Pts',(1.35113078869099,-0.771487668291091,
3.54940517824461));
#263276=CARTESIAN_POINT('Ctrl Pts',(1.36775198189399,-0.741621598017589,
3.55196439986789));
#263277=CARTESIAN_POINT('Ctrl Pts',(1.3864780124704,-0.705198524059447,
3.55496554660474));
#263278=CARTESIAN_POINT('Ctrl Pts',(1.38953931266988,-0.699147152229028,
3.55546028155649));
#263279=CARTESIAN_POINT('Ctrl Pts',(1.39423550872059,-0.689711330810145,
3.55622548721787));
#263280=CARTESIAN_POINT('Ctrl Pts',(1.3958978291903,-0.686340749846035,
3.55649760068546));
#263281=CARTESIAN_POINT('Ctrl Pts',(1.39896260984374,-0.680069296178067,
3.55700158805259));
#263282=CARTESIAN_POINT('Ctrl Pts',(1.40036826116462,-0.677170115119824,
3.55723365102325));
#263283=CARTESIAN_POINT('Ctrl Pts',(1.40355072950968,-0.670553929169158,
3.55776116375599));
#263284=CARTESIAN_POINT('Ctrl Pts',(1.40532179379059,-0.666834221665083,
3.55805625696772));
#263285=CARTESIAN_POINT('Ctrl Pts',(1.40990133448869,-0.657116684596081,
3.55882343116313));
#263286=CARTESIAN_POINT('Ctrl Pts',(1.41268636073715,-0.65110779482949,
3.55929411692055));
#263287=CARTESIAN_POINT('Ctrl Pts',(1.43119848023104,-0.610488619647277,
3.56245224463541));
#263288=CARTESIAN_POINT('Ctrl Pts',(1.44569218371073,-0.575326123662344,
3.56507099572242));
#263289=CARTESIAN_POINT('Ctrl Pts',(1.51071781923886,-0.399541183608317,
3.57777263425468));
#263290=CARTESIAN_POINT('Ctrl Pts',(1.54209641145772,-0.252678798261506,
3.58725566517923));
#263291=CARTESIAN_POINT('Ctrl Pts',(1.55470808556724,-0.0637159556006852,
3.60012770876487));
#263292=CARTESIAN_POINT('Ctrl Pts',(1.55583157354864,-0.0237613914067299,
3.60288097891822));
#263293=CARTESIAN_POINT('Ctrl Pts',(1.55530558667639,0.0267734064996201,
3.60642448385329));
#263294=CARTESIAN_POINT('Ctrl Pts',(1.55508739942901,0.0373557699431689,
3.60716987608417));
#263295=CARTESIAN_POINT('Ctrl Pts',(1.55456395130295,0.0543337469354434,
3.60837151464195));
#263296=CARTESIAN_POINT('Ctrl Pts',(1.55432716797192,0.0607312722262737,
3.60882562004844));
#263297=CARTESIAN_POINT('Ctrl Pts',(1.55380186411863,0.0728925203749078,
3.60969142353515));
#263298=CARTESIAN_POINT('Ctrl Pts',(1.55352074673013,0.0786564701469008,
3.61010288328317));
#263299=CARTESIAN_POINT('Ctrl Pts',(1.55280673027343,0.0917935641681788,
3.61104325842404));
#263300=CARTESIAN_POINT('Ctrl Pts',(1.55235338061458,0.0991654083658013,
3.61157280425712));
#263301=CARTESIAN_POINT('Ctrl Pts',(1.55103690918677,0.118342104049182,
3.61295531133463));
#263302=CARTESIAN_POINT('Ctrl Pts',(1.55009152933668,0.130140629844021,
3.61381081993734));
#263303=CARTESIAN_POINT('Ctrl Pts',(1.54185007546671,0.220089088830683,
3.62037188301625));
#263304=CARTESIAN_POINT('Ctrl Pts',(1.52878420515685,0.297583496632999,
3.62625784230878));
#263305=CARTESIAN_POINT('Ctrl Pts',(1.50511088588568,0.393222412612422,
3.633804783071));
#263306=CARTESIAN_POINT('Ctrl Pts',(1.49991488516801,0.412599013088281,
3.63534823479072));
#263307=CARTESIAN_POINT('Ctrl Pts',(1.47933721737735,0.483801462586178,
3.64106872112974));
#263308=CARTESIAN_POINT('Ctrl Pts',(1.46163180323961,0.53491570248639,3.6452733433651));
#263309=CARTESIAN_POINT('Ctrl Pts',(1.43909084970007,0.59045096367321,3.64990718000055));
#263310=CARTESIAN_POINT('Ctrl Pts',(1.43684906500452,0.595885533791599,
3.65036133090783));
#263311=CARTESIAN_POINT('Ctrl Pts',(1.43457668196674,0.601306904631308,
3.65081500619461));
#263312=CARTESIAN_POINT('Origin',(0.,0.,-1.29405622560371));
#263313=CARTESIAN_POINT('',(1.43457668488586,0.601306897666988,4.48971815675999));
#263314=CARTESIAN_POINT('',(1.43457657355106,0.601307163285539,4.35096339883543));
#263315=CARTESIAN_POINT('',(1.43457668357355,0.601306900797845,-1.29405622560371));
#263316=CARTESIAN_POINT('Ctrl Pts',(1.43457668488586,0.601306897666987,
4.48971815675999));
#263317=CARTESIAN_POINT('Ctrl Pts',(1.4496294055982,0.565394650091241,4.48688128567671));
#263318=CARTESIAN_POINT('Ctrl Pts',(1.46332789596575,0.528930871216676,
4.48399969080137));
#263319=CARTESIAN_POINT('Ctrl Pts',(1.52292031548538,0.350193919453911,
4.46986194584548));
#263320=CARTESIAN_POINT('Ctrl Pts',(1.54950444596061,0.202352133044675,
4.45802888519858));
#263321=CARTESIAN_POINT('Ctrl Pts',(1.55569384384153,0.0208255808088899,
4.44426720952001));
#263322=CARTESIAN_POINT('Ctrl Pts',(1.55579170206273,-0.0113843345359859,
4.44185894189328));
#263323=CARTESIAN_POINT('Ctrl Pts',(1.5547042178844,-0.0501874368977438,
4.43901536873532));
#263324=CARTESIAN_POINT('Ctrl Pts',(1.55447679251389,-0.0567969160773385,
4.43853303521036));
#263325=CARTESIAN_POINT('Ctrl Pts',(1.55405668083049,-0.0670948677577418,
4.437784888774));
#263326=CARTESIAN_POINT('Ctrl Pts',(1.55389300360795,-0.0707843388302729,
4.43751752053279));
#263327=CARTESIAN_POINT('Ctrl Pts',(1.55356378936395,-0.07765265115957,
4.43702108242808));
#263328=CARTESIAN_POINT('Ctrl Pts',(1.55340163663461,-0.0808315376028501,
4.43679183568499));
#263329=CARTESIAN_POINT('Ctrl Pts',(1.55300889694254,-0.0880927561640625,
4.43626935971131));
#263330=CARTESIAN_POINT('Ctrl Pts',(1.55277197142233,-0.0921746899584727,
4.43597648710965));
#263331=CARTESIAN_POINT('Ctrl Pts',(1.55211006461084,-0.102850658388751,
4.43521258828929));
#263332=CARTESIAN_POINT('Ctrl Pts',(1.55165915192597,-0.109443094599776,
4.43474296161927));
#263333=CARTESIAN_POINT('Ctrl Pts',(1.54827591980018,-0.154671374342359,
4.43153408075855));
#263334=CARTESIAN_POINT('Ctrl Pts',(1.5439425954447,-0.193192771068081,
4.42886638416777));
#263335=CARTESIAN_POINT('Ctrl Pts',(1.53652738683792,-0.242458863410164,
4.42549235834147));
#263336=CARTESIAN_POINT('Ctrl Pts',(1.53476356330938,-0.253384146084462,
4.42474654763777));
#263337=CARTESIAN_POINT('Ctrl Pts',(1.51650866915956,-0.35926266401958,
4.41753434534373));
#263338=CARTESIAN_POINT('Ctrl Pts',(1.49134280153566,-0.452511390464715,
4.41129165747051));
#263339=CARTESIAN_POINT('Ctrl Pts',(1.43963174351419,-0.591374246483627,
4.40145451822027));
#263340=CARTESIAN_POINT('Ctrl Pts',(1.41914447914593,-0.638976743083573,
4.39797998350777));
#263341=CARTESIAN_POINT('Ctrl Pts',(1.38258539116952,-0.713449127435685,
4.39229793029168));
#263342=CARTESIAN_POINT('Ctrl Pts',(1.36801099680807,-0.741011270646466,
4.39013831339894));
#263343=CARTESIAN_POINT('Ctrl Pts',(1.34785359972908,-0.776507607160127,
4.3872718485655));
#263344=CARTESIAN_POINT('Ctrl Pts',(1.34301001484466,-0.784855071217839,
4.38659143755161));
#263345=CARTESIAN_POINT('Ctrl Pts',(1.33495563597446,-0.798443150711165,
4.38547317573753));
#263346=CARTESIAN_POINT('Ctrl Pts',(1.33179085095163,-0.803710857389672,
4.3850369973022));
#263347=CARTESIAN_POINT('Ctrl Pts',(1.32560444073762,-0.813871109499376,
4.38419046054938));
#263348=CARTESIAN_POINT('Ctrl Pts',(1.32258673155626,-0.818765932399785,
4.38378025067284));
#263349=CARTESIAN_POINT('Ctrl Pts',(1.31555102040395,-0.830037692975204,
4.38283003593794));
#263350=CARTESIAN_POINT('Ctrl Pts',(1.31151370000568,-0.836402337416092,
4.38228932491039));
#263351=CARTESIAN_POINT('Ctrl Pts',(1.29831131991099,-0.8568846308752,4.38053551968538));
#263352=CARTESIAN_POINT('Ctrl Pts',(1.28896361348408,-0.870882492515712,
4.37931566375303));
#263353=CARTESIAN_POINT('Ctrl Pts',(1.20048636909602,-0.998828386910547,
4.36796256639652));
#263354=CARTESIAN_POINT('Ctrl Pts',(1.1066874867825,-1.10183978589384,4.35722733646156));
#263355=CARTESIAN_POINT('Ctrl Pts',(0.946422225887876,-1.23646907425629,
4.34101417006435));
#263356=CARTESIAN_POINT('Ctrl Pts',(0.889291785282419,-1.27817574512089,
4.33557555991543));
#263357=CARTESIAN_POINT('Ctrl Pts',(0.818822832638556,-1.32259942951951,
4.32940468565497));
#263358=CARTESIAN_POINT('Ctrl Pts',(0.808045810486581,-1.32921107350094,
4.32847502440679));
#263359=CARTESIAN_POINT('Ctrl Pts',(0.793075598681423,-1.3381458407426,
4.32720413967129));
#263360=CARTESIAN_POINT('Ctrl Pts',(0.788950886555265,-1.34058185000729,
4.3268560934979));
#263361=CARTESIAN_POINT('Ctrl Pts',(0.781970868843404,-1.34466079777616,
4.32627076394256));
#263362=CARTESIAN_POINT('Ctrl Pts',(0.779121505342163,-1.34631377525703,
4.32603284219349));
#263363=CARTESIAN_POINT('Ctrl Pts',(0.773681239626328,-1.34944673554357,
4.32558055065654));
#263364=CARTESIAN_POINT('Ctrl Pts',(0.771091308150122,-1.35092832804917,
4.32536607441216));
#263365=CARTESIAN_POINT('Ctrl Pts',(0.764249913284072,-1.35481592231552,
4.32480170832947));
#263366=CARTESIAN_POINT('Ctrl Pts',(0.759991304406713,-1.35720939146146,
4.32445261608534));
#263367=CARTESIAN_POINT('Ctrl Pts',(0.744957158128021,-1.36556609195917,
4.32322772896582));
#263368=CARTESIAN_POINT('Ctrl Pts',(0.734121777711956,-1.37142158346597,
4.32235845288608));
#263369=CARTESIAN_POINT('Ctrl Pts',(0.65240973054253,-1.41433315597924,
4.31589492371475));
#263370=CARTESIAN_POINT('Ctrl Pts',(0.578828674008771,-1.44600753949109,
4.31058501428635));
#263371=CARTESIAN_POINT('Ctrl Pts',(0.427674721716568,-1.49767586447515,
4.30005117247523));
#263372=CARTESIAN_POINT('Ctrl Pts',(0.350353179279664,-1.51762665615863,
4.29484049618524));
#263373=CARTESIAN_POINT('Ctrl Pts',(0.214871896188,-1.54167391977124,4.28560815878372));
#263374=CARTESIAN_POINT('Ctrl Pts',(0.15738570946834,-1.54859835510715,
4.281661533238));
#263375=CARTESIAN_POINT('Ctrl Pts',(0.0879781719606484,-1.5530540684106,
4.27679344498549));
#263376=CARTESIAN_POINT('Ctrl Pts',(0.0762961996199487,-1.55367177191675,
4.27597070638206));
#263377=CARTESIAN_POINT('Ctrl Pts',(0.0580198643052897,-1.55443154639989,
4.27467774170055));
#263378=CARTESIAN_POINT('Ctrl Pts',(0.0514294988808367,-1.5546635460165,
4.27421032753634));
#263379=CARTESIAN_POINT('Ctrl Pts',(0.039744854766824,-1.55500050086644,
4.27337943361898));
#263380=CARTESIAN_POINT('Ctrl Pts',(0.034651126462614,-1.55512234550101,
4.27301648719875));
#263381=CARTESIAN_POINT('Ctrl Pts',(0.0229108768374192,-1.55534546899381,
4.27217821786568));
#263382=CARTESIAN_POINT('Ctrl Pts',(0.0162641628112747,-1.55542917250117,
4.27170235267692));
#263383=CARTESIAN_POINT('Ctrl Pts',(-0.00200294249263999,-1.55554211493817,
4.27039090302117));
#263384=CARTESIAN_POINT('Ctrl Pts',(-0.013623233797216,-1.55548374372541,
4.26955260430709));
#263385=CARTESIAN_POINT('Ctrl Pts',(-0.0754543521291461,-1.55448026236994,
4.26506957355809));
#263386=CARTESIAN_POINT('Ctrl Pts',(-0.12559244726126,-1.55123426058943,
4.26135400405865));
#263387=CARTESIAN_POINT('Ctrl Pts',(-0.321357330760294,-1.52900750748695,
4.24651777380385));
#263388=CARTESIAN_POINT('Ctrl Pts',(-0.464127891150248,-1.49188144309349,
4.23489079933847));
#263389=CARTESIAN_POINT('Ctrl Pts',(-0.617902306033279,-1.42764555644481,
4.22229129623412));
#263390=CARTESIAN_POINT('Ctrl Pts',(-0.636090150108855,-1.41963534111109,
4.22080146125937));
#263391=CARTESIAN_POINT('Ctrl Pts',(-0.666027906535529,-1.40575934101143,
4.21835529105081));
#263392=CARTESIAN_POINT('Ctrl Pts',(-0.677865564961396,-1.40008956986362,
4.21738968682946));
#263393=CARTESIAN_POINT('Ctrl Pts',(-0.693987705959558,-1.39211527657428,
4.2160782237036));
#263394=CARTESIAN_POINT('Ctrl Pts',(-0.698334807808633,-1.38993970272594,
4.21572497244544));
#263395=CARTESIAN_POINT('Ctrl Pts',(-0.705623365473424,-1.38624920630204,
4.21513339842743));
#263396=CARTESIAN_POINT('Ctrl Pts',(-0.708570283326058,-1.38474522933057,
4.21489440707879));
#263397=CARTESIAN_POINT('Ctrl Pts',(-0.71415413900671,-1.38187298289882,
4.21444196425293));
#263398=CARTESIAN_POINT('Ctrl Pts',(-0.716791982960632,-1.3805065478642,
4.21422839713211));
#263399=CARTESIAN_POINT('Ctrl Pts',(-0.723694699294365,-1.37690573871875,
4.21366993542193));
#263400=CARTESIAN_POINT('Ctrl Pts',(-0.72795318665476,-1.37465908166417,
4.21332580682127));
#263401=CARTESIAN_POINT('Ctrl Pts',(-0.742699123595152,-1.3667918044138,
4.21213534435835));
#263402=CARTESIAN_POINT('Ctrl Pts',(-0.753132810915957,-1.36107046720772,
4.21129505779315));
#263403=CARTESIAN_POINT('Ctrl Pts',(-0.851752753088455,-1.30551062607219,
4.20336206317367));
#263404=CARTESIAN_POINT('Ctrl Pts',(-0.934952469340575,-1.24728153121076,
4.19673216721475));
#263405=CARTESIAN_POINT('Ctrl Pts',(-1.09850602031394,-1.10718842834496,
4.18255932922575));
#263406=CARTESIAN_POINT('Ctrl Pts',(-1.17667246754693,-1.02372761708732,
4.17503308528831));
#263407=CARTESIAN_POINT('Ctrl Pts',(-1.25305610327961,-0.921743281344272,
4.16613635260185));
#263408=CARTESIAN_POINT('Ctrl Pts',(-1.26095993217026,-0.910900820246568,
4.16519437960877));
#263409=CARTESIAN_POINT('Ctrl Pts',(-1.27274803285324,-0.894282455660537,
4.16375569395895));
#263410=CARTESIAN_POINT('Ctrl Pts',(-1.27673557929078,-0.888580285264104,
4.16326293965605));
#263411=CARTESIAN_POINT('Ctrl Pts',(-1.28359206471301,-0.878634111464093,
4.16240488055949));
#263412=CARTESIAN_POINT('Ctrl Pts',(-1.28647856994604,-0.874402297767903,
4.162040248974));
#263413=CARTESIAN_POINT('Ctrl Pts',(-1.29289620856387,-0.864893036107552,
4.16122184143734));
#263414=CARTESIAN_POINT('Ctrl Pts',(-1.29641601765793,-0.859608094992573,
4.16076764782077));
#263415=CARTESIAN_POINT('Ctrl Pts',(-1.30571418159077,-0.845460034128013,
4.15955337822951));
#263416=CARTESIAN_POINT('Ctrl Pts',(-1.31143454184425,-0.836559397465484,
4.15879116226563));
#263417=CARTESIAN_POINT('Ctrl Pts',(-1.3363162870448,-0.796962022263645,
4.15540698539514));
#263418=CARTESIAN_POINT('Ctrl Pts',(-1.3544924211383,-0.765662825511044,
4.15274948624549));
#263419=CARTESIAN_POINT('Ctrl Pts',(-1.44689764714555,-0.592937212205354,
4.13816300746388));
#263420=CARTESIAN_POINT('Ctrl Pts',(-1.50008148799625,-0.441390248115223,
4.12550887901513));
#263421=CARTESIAN_POINT('Ctrl Pts',(-1.53528366002654,-0.252119500937636,
4.11091413652309));
#263422=CARTESIAN_POINT('Ctrl Pts',(-1.54026781020884,-0.219626129507415,
4.10845510820709));
#263423=CARTESIAN_POINT('Ctrl Pts',(-1.54501867130841,-0.180393440283004,
4.10555993194058));
#263424=CARTESIAN_POINT('Ctrl Pts',(-1.54577591035135,-0.173785290652867,
4.10507479419847));
#263425=CARTESIAN_POINT('Ctrl Pts',(-1.54688854268592,-0.163492465079236,
4.1043232576365));
#263426=CARTESIAN_POINT('Ctrl Pts',(-1.54727319813199,-0.159811140882374,
4.1040552811243));
#263427=CARTESIAN_POINT('Ctrl Pts',(-1.5479640997769,-0.152962482369794,
4.10355830603934));
#263428=CARTESIAN_POINT('Ctrl Pts',(-1.54827376481576,-0.149795609806687,
4.10332912688423));
#263429=CARTESIAN_POINT('Ctrl Pts',(-1.54895801519293,-0.142569062247267,
4.10280756508848));
#263430=CARTESIAN_POINT('Ctrl Pts',(-1.54932635978687,-0.138508852546755,
4.10251553421505));
#263431=CARTESIAN_POINT('Ctrl Pts',(-1.55024643188225,-0.127903824039332,
4.10175528321589));
#263432=CARTESIAN_POINT('Ctrl Pts',(-1.55077268557221,-0.121356785923434,
4.10128844097641));
#263433=CARTESIAN_POINT('Ctrl Pts',(-1.55406118177974,-0.0769228370596933,
4.09813578325049));
#263434=CARTESIAN_POINT('Ctrl Pts',(-1.55547649964676,-0.0389452410474964,
4.09551872723645));
#263435=CARTESIAN_POINT('Ctrl Pts',(-1.55556939098356,0.113117882334024,
4.08521302295828));
#263436=CARTESIAN_POINT('Ctrl Pts',(-1.54309197620292,0.226854212899771,
4.07787141785222));
#263437=CARTESIAN_POINT('Ctrl Pts',(-1.50276449358015,0.407891633369894,
4.06552717888365));
#263438=CARTESIAN_POINT('Ctrl Pts',(-1.4824659799087,0.476412806834417,
4.06069798505634));
#263439=CARTESIAN_POINT('Ctrl Pts',(-1.45350419185649,0.554111115996123,
4.05490346341675));
#263440=CARTESIAN_POINT('Ctrl Pts',(-1.44935119513,0.564884647659886,4.05409279664466));
#263441=CARTESIAN_POINT('Ctrl Pts',(-1.44239560745538,0.582346748246318,
4.0527665462406));
#263442=CARTESIAN_POINT('Ctrl Pts',(-1.43966544716021,0.589063851069534,
4.0522533901517));
#263443=CARTESIAN_POINT('Ctrl Pts',(-1.43470802870151,0.601020409480702,
4.05133448841096));
#263444=CARTESIAN_POINT('Ctrl Pts',(-1.43249876461341,0.606267224939563,
4.05092935683803));
#263445=CARTESIAN_POINT('Ctrl Pts',(-1.42776700186372,0.617334494761621,
4.05007071967775));
#263446=CARTESIAN_POINT('Ctrl Pts',(-1.42523760735243,0.623151867861369,
4.04961698559424));
#263447=CARTESIAN_POINT('Ctrl Pts',(-1.41840622783767,0.638604229514652,
4.04840524524267));
#263448=CARTESIAN_POINT('Ctrl Pts',(-1.41404173374574,0.648211041364376,
4.04764511466429));
#263449=CARTESIAN_POINT('Ctrl Pts',(-1.39241945760784,0.694546707755396,
4.04394513519803));
#263450=CARTESIAN_POINT('Ctrl Pts',(-1.37382809364769,0.730631835584284,
4.04095968849643));
#263451=CARTESIAN_POINT('Ctrl Pts',(-1.28062769438369,0.895368323678686,
4.02682178739395));
#263452=CARTESIAN_POINT('Ctrl Pts',(-1.18922762977399,1.01361519780563,
4.01507769280092));
#263453=CARTESIAN_POINT('Ctrl Pts',(-1.0549445414778,1.14374026281844,4.00083332591914));
#263454=CARTESIAN_POINT('Ctrl Pts',(-1.02643547462342,1.16939325983568,
3.99795185372611));
#263455=CARTESIAN_POINT('Ctrl Pts',(-0.991950346270438,1.19818951803847,
3.99465566098604));
#263456=CARTESIAN_POINT('Ctrl Pts',(-0.986869064260426,1.20237808725454,
3.99417459983979));
#263457=CARTESIAN_POINT('Ctrl Pts',(-0.978595065489628,1.20911066891497,
3.99339893251544));
#263458=CARTESIAN_POINT('Ctrl Pts',(-0.975418735680899,1.2116745449994,
3.99310296646358));
#263459=CARTESIAN_POINT('Ctrl Pts',(-0.969748102419786,1.21621502852914,
3.99257784581393));
#263460=CARTESIAN_POINT('Ctrl Pts',(-0.96725779501266,1.21819650978198,
3.99234834786266));
#263461=CARTESIAN_POINT('Ctrl Pts',(-0.961860747412773,1.22246383420884,
3.99185338451835));
#263462=CARTESIAN_POINT('Ctrl Pts',(-0.958951935834489,1.22474695708687,
3.99158811137077));
#263463=CARTESIAN_POINT('Ctrl Pts',(-0.950801235675756,1.23109759209628,
3.99084887112872));
#263464=CARTESIAN_POINT('Ctrl Pts',(-0.945541339666491,1.23514203645756,
3.99037649772629));
#263465=CARTESIAN_POINT('Ctrl Pts',(-0.914305448458741,1.25884348934004,
3.98759774920589));
#263466=CARTESIAN_POINT('Ctrl Pts',(-0.887740714003841,1.27771601005347,
3.98534182920958));
#263467=CARTESIAN_POINT('Ctrl Pts',(-0.731486775138291,1.38149609712096,
3.97255183732372));
#263468=CARTESIAN_POINT('Ctrl Pts',(-0.590276034206814,1.44747635458024,
3.96275163431774));
#263469=CARTESIAN_POINT('Ctrl Pts',(-0.402911855832,1.50295465313333,3.94948220288578));
#263470=CARTESIAN_POINT('Ctrl Pts',(-0.363766666040113,1.51290580938595,
3.94670242458542));
#263471=CARTESIAN_POINT('Ctrl Pts',(-0.31353502297122,1.52361306475423,
3.94310367541299));
#263472=CARTESIAN_POINT('Ctrl Pts',(-0.302764931428852,1.52578975190809,
3.9423302841545));
#263473=CARTESIAN_POINT('Ctrl Pts',(-0.285647918992407,1.52906081731417,
3.94109788132783));
#263474=CARTESIAN_POINT('Ctrl Pts',(-0.279315556943456,1.53023022256615,
3.94064125896278));
#263475=CARTESIAN_POINT('Ctrl Pts',(-0.267945873538773,1.53225695205301,
3.93982006144905));
#263476=CARTESIAN_POINT('Ctrl Pts',(-0.262911213324307,1.53312884358279,
3.93945595443612));
#263477=CARTESIAN_POINT('Ctrl Pts',(-0.25113618520361,1.53510831066129,
3.93860324010663));
#263478=CARTESIAN_POINT('Ctrl Pts',(-0.244392682199628,1.53619631659251,
3.93811402067429));
#263479=CARTESIAN_POINT('Ctrl Pts',(-0.224987760607153,1.53919612873552,
3.93670361899967));
#263480=CARTESIAN_POINT('Ctrl Pts',(-0.212309881224785,1.54099601272446,
3.93577893158095));
#263481=CARTESIAN_POINT('Ctrl Pts',(-0.111220825004964,1.55407654789613,
3.92837830418685));
#263482=CARTESIAN_POINT('Ctrl Pts',(-0.0220277197653859,1.55789387736974,
3.92166687004201));
#263483=CARTESIAN_POINT('Ctrl Pts',(0.162991155967391,1.54991873904261,
3.90742065816221));
#263484=CARTESIAN_POINT('Ctrl Pts',(0.258403588082749,1.53689353713582,
3.89989188140377));
#263485=CARTESIAN_POINT('Ctrl Pts',(0.389244266044576,1.50649621335559,
3.88966003358217));
#263486=CARTESIAN_POINT('Ctrl Pts',(0.426156866801691,1.49647347636279,
3.88678645844192));
#263487=CARTESIAN_POINT('Ctrl Pts',(0.468948085682516,1.48314235218931,
3.88349818738217));
#263488=CARTESIAN_POINT('Ctrl Pts',(0.475217769165342,1.48114537432502,
3.88301750079174));
#263489=CARTESIAN_POINT('Ctrl Pts',(0.485354724867895,1.47784562472242,
3.88224231720864));
#263490=CARTESIAN_POINT('Ctrl Pts',(0.48922978656204,1.4765673423296,3.88194646303792));
#263491=CARTESIAN_POINT('Ctrl Pts',(0.496117987115583,1.47426501002547,
3.88142146415251));
#263492=CARTESIAN_POINT('Ctrl Pts',(0.499133050812023,1.47324694983624,
3.88119197671732));
#263493=CARTESIAN_POINT('Ctrl Pts',(0.505645836467736,1.47102556716418,
3.88069694878178));
#263494=CARTESIAN_POINT('Ctrl Pts',(0.509142393101847,1.46981902134488,
3.88043160099852));
#263495=CARTESIAN_POINT('Ctrl Pts',(0.518903426597858,1.46641180078459,
3.87969194100505));
#263496=CARTESIAN_POINT('Ctrl Pts',(0.525158266509693,1.46418343623874,
3.87921922541267));
#263497=CARTESIAN_POINT('Ctrl Pts',(0.562094027811293,1.45075747195474,
3.87643413088317));
#263498=CARTESIAN_POINT('Ctrl Pts',(0.592433138159572,1.43863487796326,
3.87417247627393));
#263499=CARTESIAN_POINT('Ctrl Pts',(0.765650759609296,1.36301181653492,
3.86128632071859));
#263500=CARTESIAN_POINT('Ctrl Pts',(0.898688880043385,1.279214587416,3.851406447969));
#263501=CARTESIAN_POINT('Ctrl Pts',(1.04663740270753,1.15137478840919,3.83811531485476));
#263502=CARTESIAN_POINT('Ctrl Pts',(1.07528827803231,1.1246636994786,3.83541743835888));
#263503=CARTESIAN_POINT('Ctrl Pts',(1.11056752652789,1.08919156946057,3.83191134638785));
#263504=CARTESIAN_POINT('Ctrl Pts',(1.11815476297379,1.08140113803515,3.83114582533601));
#263505=CARTESIAN_POINT('Ctrl Pts',(1.1300865642747,1.06888996352268,3.82992308858041));
#263506=CARTESIAN_POINT('Ctrl Pts',(1.13448478598546,1.06422068435184,3.82946819741248));
#263507=CARTESIAN_POINT('Ctrl Pts',(1.14233646183328,1.05578113165068,3.82864849753494));
#263508=CARTESIAN_POINT('Ctrl Pts',(1.14580046636822,1.05202076030249,3.82828414638647));
#263509=CARTESIAN_POINT('Ctrl Pts',(1.15387161754523,1.0431719216984,3.82742876172132));
#263510=CARTESIAN_POINT('Ctrl Pts',(1.15846371303028,1.03806993540541,3.82693710325898));
#263511=CARTESIAN_POINT('Ctrl Pts',(1.17163119133005,1.0232441979354,3.82551267313542));
#263512=CARTESIAN_POINT('Ctrl Pts',(1.18011878204187,1.01344362371414,3.82457628692552));
#263513=CARTESIAN_POINT('Ctrl Pts',(1.25152779253115,0.928874491273502,
3.81653835031673));
#263514=CARTESIAN_POINT('Ctrl Pts',(1.30738406671698,0.84845124364151,3.80915069464098));
#263515=CARTESIAN_POINT('Ctrl Pts',(1.38487019825216,0.710873001728965,
3.79696702009401));
#263516=CARTESIAN_POINT('Ctrl Pts',(1.41132923121526,0.656769881463216,
3.79228202654749));
#263517=CARTESIAN_POINT('Ctrl Pts',(1.43457681153698,0.601306595507149,
3.78763867041446));
#263518=CARTESIAN_POINT('Ctrl Pts',(1.43457668196674,0.601306904631308,
3.65081500619461));
#263519=CARTESIAN_POINT('Ctrl Pts',(1.41248223415038,0.654019054440599,
3.65522610449217));
#263520=CARTESIAN_POINT('Ctrl Pts',(1.38749513607011,0.705483256301638,
3.6595938904266));
#263521=CARTESIAN_POINT('Ctrl Pts',(1.3538881908303,0.765970957718364,3.66471482813885));
#263522=CARTESIAN_POINT('Ctrl Pts',(1.34792834150311,0.776410942282884,
3.66559814297501));
#263523=CARTESIAN_POINT('Ctrl Pts',(1.33945480041942,0.790862485526851,
3.66681903248342));
#263524=CARTESIAN_POINT('Ctrl Pts',(1.3370431276979,0.794932896313606,3.66716270131296));
#263525=CARTESIAN_POINT('Ctrl Pts',(1.33291145681734,0.80183431587057,3.66774496213212));
#263526=CARTESIAN_POINT('Ctrl Pts',(1.33120093211004,0.804670927149445,
3.66798415655261));
#263527=CARTESIAN_POINT('Ctrl Pts',(1.32789880561523,0.810107588488455,
3.668442326523));
#263528=CARTESIAN_POINT('Ctrl Pts',(1.32630861255695,0.812708439463858,
3.66866139408254));
#263529=CARTESIAN_POINT('Ctrl Pts',(1.32204398440995,0.819637627171099,
3.66924476884178));
#263530=CARTESIAN_POINT('Ctrl Pts',(1.31935591039348,0.823957596145479,
3.66960819389876));
#263531=CARTESIAN_POINT('Ctrl Pts',(1.30953576221684,0.839568149258955,
3.67092075227493));
#263532=CARTESIAN_POINT('Ctrl Pts',(1.30227929595905,0.850780381050817,
3.67186214561297));
#263533=CARTESIAN_POINT('Ctrl Pts',(1.19831733338818,1.00696837842723,3.68497784886838));
#263534=CARTESIAN_POINT('Ctrl Pts',(1.07805144237437,1.13480284649737,3.69585901537796));
#263535=CARTESIAN_POINT('Ctrl Pts',(0.904337337247798,1.26635407895836,
3.71062707569195));
#263536=CARTESIAN_POINT('Ctrl Pts',(0.868515681298962,1.29118495651451,
3.71362287655073));
#263537=CARTESIAN_POINT('Ctrl Pts',(0.822508707573054,1.32029467236599,
3.71743842292436));
#263538=CARTESIAN_POINT('Ctrl Pts',(0.813255097019537,1.32601460490569,
3.71820425857743));
#263539=CARTESIAN_POINT('Ctrl Pts',(0.798406411914479,1.33497912710978,
3.7194310089638));
#263540=CARTESIAN_POINT('Ctrl Pts',(0.792849656737897,1.33828677342476,
3.71988961857966));
#263541=CARTESIAN_POINT('Ctrl Pts',(0.782306001615559,1.34447414645509,
3.72075900646976));
#263542=CARTESIAN_POINT('Ctrl Pts',(0.777323405731917,1.34736102508348,
3.72116951706343));
#263543=CARTESIAN_POINT('Ctrl Pts',(0.766010916427692,1.35383176090927,
3.7221008531065));
#263544=CARTESIAN_POINT('Ctrl Pts',(0.759671722474857,1.35739899501897,
3.72262226412219));
#263545=CARTESIAN_POINT('Ctrl Pts',(0.743276266197914,1.36647433479872,
3.72396971842492));
#263546=CARTESIAN_POINT('Ctrl Pts',(0.733183860748704,1.37191586068914,
3.72479810088033));
#263547=CARTESIAN_POINT('Ctrl Pts',(0.664473441948673,1.40798777019503,
3.73043184144804));
#263548=CARTESIAN_POINT('Ctrl Pts',(0.604022176256144,1.43495972218187,
3.73536351028652));
#263549=CARTESIAN_POINT('Ctrl Pts',(0.430912554946466,1.49931727905603,
3.74941793161595));
#263550=CARTESIAN_POINT('Ctrl Pts',(0.315431020303203,1.52778858303827,
3.75874492849165));
#263551=CARTESIAN_POINT('Ctrl Pts',(0.158920749501713,1.54785795632627,
3.77076796451315));
#263552=CARTESIAN_POINT('Ctrl Pts',(0.11981987160918,1.5513748431871,3.77371769432799));
#263553=CARTESIAN_POINT('Ctrl Pts',(0.0736006353177334,1.55377368263397,
3.77711110179891));
#263554=CARTESIAN_POINT('Ctrl Pts',(0.0665747110034731,1.55409057755694,
3.77762439984716));
#263555=CARTESIAN_POINT('Ctrl Pts',(0.0557371723841911,1.55450575792803,
3.77841200200046));
#263556=CARTESIAN_POINT('Ctrl Pts',(0.0519270631922611,1.55463769566144,
3.77868810291033));
#263557=CARTESIAN_POINT('Ctrl Pts',(0.04490098527156,1.55485513815668,3.77919574121096));
#263558=CARTESIAN_POINT('Ctrl Pts',(0.0416852548692331,1.55494467395382,
3.77942749191928));
#263559=CARTESIAN_POINT('Ctrl Pts',(0.0344223289403372,1.55512434879558,
3.77994960392184));
#263560=CARTESIAN_POINT('Ctrl Pts',(0.0303750504421464,1.55520866582593,
3.78023963835893));
#263561=CARTESIAN_POINT('Ctrl Pts',(0.0181593010589105,1.55541545163537,
3.78111240783904));
#263562=CARTESIAN_POINT('Ctrl Pts',(0.00998997673869821,1.55548937491343,
3.78169252610975));
#263563=CARTESIAN_POINT('Ctrl Pts',(-0.0685451418059095,1.55558127518474,
3.78723862509665));
#263564=CARTESIAN_POINT('Ctrl Pts',(-0.138846094609719,1.55088886811156,
3.79196697433598));
#263565=CARTESIAN_POINT('Ctrl Pts',(-0.266743725079774,1.53358110516601,
3.8005228848376));
#263566=CARTESIAN_POINT('Ctrl Pts',(-0.324399319969653,1.52242848288096,
3.80436256999112));
#263567=CARTESIAN_POINT('Ctrl Pts',(-0.470997861812928,1.48536314494387,
3.81434851175503));
#263568=CARTESIAN_POINT('Ctrl Pts',(-0.558491506946601,1.45472540837135,
3.82053688684906));
#263569=CARTESIAN_POINT('Ctrl Pts',(-0.654563695136473,1.41113262753592,
3.82790772914782));
#263570=CARTESIAN_POINT('Ctrl Pts',(-0.666322562000888,1.40561842221868,
3.82881992215711));
#263571=CARTESIAN_POINT('Ctrl Pts',(-0.684240171225715,1.39694078136309,
3.83022602558785));
#263572=CARTESIAN_POINT('Ctrl Pts',(-0.690449346872053,1.39388229601962,
3.83071630599239));
#263573=CARTESIAN_POINT('Ctrl Pts',(-0.701265216818251,1.38846466680611,
3.83157571112684));
#263574=CARTESIAN_POINT('Ctrl Pts',(-0.705880971661034,1.38612376357573,
3.83194419468438));
#263575=CARTESIAN_POINT('Ctrl Pts',(-0.716285244587605,1.38078173934341,
3.83277874513233));
#263576=CARTESIAN_POINT('Ctrl Pts',(-0.722066715881598,1.3777671859728,
3.83324527855689));
#263577=CARTESIAN_POINT('Ctrl Pts',(-0.737658513367,1.36951227464327,3.83451112815336));
#263578=CARTESIAN_POINT('Ctrl Pts',(-0.747431700709627,1.3642029884067,
3.83531286761553));
#263579=CARTESIAN_POINT('Ctrl Pts',(-0.792894886804613,1.33886991800512,
3.83908216576555));
#263580=CARTESIAN_POINT('Ctrl Pts',(-0.827839502350788,1.31754929315272,
3.84209567848846));
#263581=CARTESIAN_POINT('Ctrl Pts',(-0.964941933419628,1.2262907817828,
3.85440952449655));
#263582=CARTESIAN_POINT('Ctrl Pts',(-1.05941783009147,1.14565578102305,
3.8640860672503));
#263583=CARTESIAN_POINT('Ctrl Pts',(-1.18102815281365,1.01382692200413,
3.87791569442675));
#263584=CARTESIAN_POINT('Ctrl Pts',(-1.21651868233831,0.970956351383092,
3.8821584403891));
#263585=CARTESIAN_POINT('Ctrl Pts',(-1.25636712957263,0.91719654836222,
3.88710489124932));
#263586=CARTESIAN_POINT('Ctrl Pts',(-1.2629954953069,0.908047504990818,
3.88793434034297));
#263587=CARTESIAN_POINT('Ctrl Pts',(-1.27219080253282,0.895059838170542,
3.88909362383332));
#263588=CARTESIAN_POINT('Ctrl Pts',(-1.27484102535098,0.891281051920285,
3.88942878277673));
#263589=CARTESIAN_POINT('Ctrl Pts',(-1.27935206517222,0.88478775615689,
3.890000979148));
#263590=CARTESIAN_POINT('Ctrl Pts',(-1.28122114532435,0.882079054132552,
3.89023856997621));
#263591=CARTESIAN_POINT('Ctrl Pts',(-1.2848209877176,0.876826519626964,
3.89069713366457));
#263592=CARTESIAN_POINT('Ctrl Pts',(-1.28655280544414,0.874283475340645,
3.8909181815385));
#263593=CARTESIAN_POINT('Ctrl Pts',(-1.29071748419781,0.868128785562189,
3.8914508728641));
#263594=CARTESIAN_POINT('Ctrl Pts',(-1.29314276559258,0.864512001856784,
3.8917620119057));
#263595=CARTESIAN_POINT('Ctrl Pts',(-1.30208644392789,0.851052587662169,
3.892913056396));
#263596=CARTESIAN_POINT('Ctrl Pts',(-1.30850813862925,0.841145699512007,
3.89374681983822));
#263597=CARTESIAN_POINT('Ctrl Pts',(-1.3703013348674,0.743395432380443,
3.90185263972659));
#263598=CARTESIAN_POINT('Ctrl Pts',(-1.41686716636135,0.650274509475742,
3.90863816772539));
#263599=CARTESIAN_POINT('Ctrl Pts',(-1.49233389381873,0.451946009021947,
3.92260693563284));
#263600=CARTESIAN_POINT('Ctrl Pts',(-1.52017276594882,0.346966380250798,
3.9297670519908));
#263601=CARTESIAN_POINT('Ctrl Pts',(-1.5392498347612,0.224780066138408,
3.9383799795859));
#263602=CARTESIAN_POINT('Ctrl Pts',(-1.541394111577,0.209571694903565,3.93945627755315));
#263603=CARTESIAN_POINT('Ctrl Pts',(-1.54423725939253,0.186992761666482,
3.94106161821623));
#263604=CARTESIAN_POINT('Ctrl Pts',(-1.54510932229686,0.179644607351197,
3.94158522416555));
#263605=CARTESIAN_POINT('Ctrl Pts',(-1.546568281975,0.166553657327033,3.94252023423077));
#263606=CARTESIAN_POINT('Ctrl Pts',(-1.54717570725876,0.160813248227054,
3.94293098636375));
#263607=CARTESIAN_POINT('Ctrl Pts',(-1.54838861694445,0.14870718984261,
3.943798870711));
#263608=CARTESIAN_POINT('Ctrl Pts',(-1.54898682778632,0.142340937487493,
3.94425622299247));
#263609=CARTESIAN_POINT('Ctrl Pts',(-1.55046797591417,0.125461585725873,
3.94547146644935));
#263610=CARTESIAN_POINT('Ctrl Pts',(-1.55128322375806,0.114943043846042,
3.94623145909429));
#263611=CARTESIAN_POINT('Ctrl Pts',(-1.55435043694713,0.0693539477777701,
3.94953768983712));
#263612=CARTESIAN_POINT('Ctrl Pts',(-1.55552037157283,0.034223609396336,
3.95211724177831));
#263613=CARTESIAN_POINT('Ctrl Pts',(-1.55541993858913,-0.136754236632592,
3.96483779332785));
#263614=CARTESIAN_POINT('Ctrl Pts',(-1.53754511327777,-0.271984690434862,
3.97547988788291));
#263615=CARTESIAN_POINT('Ctrl Pts',(-1.48800799561479,-0.456590779125059,
3.99018758041753));
#263616=CARTESIAN_POINT('Ctrl Pts',(-1.47082090478669,-0.509244862790918,
3.99439363263666));
#263617=CARTESIAN_POINT('Ctrl Pts',(-1.44800754874389,-0.568257879032682,
3.99904231310736));
#263618=CARTESIAN_POINT('Ctrl Pts',(-1.44509764761657,-0.575617645868236,
3.99962085330804));
#263619=CARTESIAN_POINT('Ctrl Pts',(-1.44061408907592,-0.58670920621473,
4.00049056258533));
#263620=CARTESIAN_POINT('Ctrl Pts',(-1.43908187994513,-0.590457441415419,
4.00078408946524));
#263621=CARTESIAN_POINT('Ctrl Pts',(-1.43630611885773,-0.597172782637498,
4.00130923697414));
#263622=CARTESIAN_POINT('Ctrl Pts',(-1.43506798932785,-0.600142038222562,
4.00154117339725));
#263623=CARTESIAN_POINT('Ctrl Pts',(-1.43234284054855,-0.606620774364344,
4.00204666659691));
#263624=CARTESIAN_POINT('Ctrl Pts',(-1.4308521337207,-0.610128633183781,
4.0023199970875));
#263625=CARTESIAN_POINT('Ctrl Pts',(-1.42657585102065,-0.620089502334404,
4.00309520297843));
#263626=CARTESIAN_POINT('Ctrl Pts',(-1.42375936345784,-0.626529272712305,
4.00359525359604));
#263627=CARTESIAN_POINT('Ctrl Pts',(-1.40497093270187,-0.668707125197741,
4.00686440131286));
#263628=CARTESIAN_POINT('Ctrl Pts',(-1.38769680705483,-0.703854218763706,
4.00956038134491));
#263629=CARTESIAN_POINT('Ctrl Pts',(-1.31320564274172,-0.841988685470106,
4.02019051734059));
#263630=CARTESIAN_POINT('Ctrl Pts',(-1.24570103455101,-0.938981872534296,
4.02776046557674));
#263631=CARTESIAN_POINT('Ctrl Pts',(-1.12367153420295,-1.07769391969544,
4.04008430254892));
#263632=CARTESIAN_POINT('Ctrl Pts',(-1.07626024052109,-1.12504397923258,
4.04462363752967));
#263633=CARTESIAN_POINT('Ctrl Pts',(-1.01731124870653,-1.17677109299921,
4.05010465158792));
#263634=CARTESIAN_POINT('Ctrl Pts',(-1.00858757953179,-1.18425650263217,
4.05091177634744));
#263635=CARTESIAN_POINT('Ctrl Pts',(-0.994202718114478,-1.19632530875286,
4.05223673067819));
#263636=CARTESIAN_POINT('Ctrl Pts',(-0.98859076599963,-1.2009669367611,
4.05275218405477));
#263637=CARTESIAN_POINT('Ctrl Pts',(-0.978482743262037,-1.20920839485114,
4.05367814057749));
#263638=CARTESIAN_POINT('Ctrl Pts',(-0.973998852478831,-1.21282301049138,
4.05408803884237));
#263639=CARTESIAN_POINT('Ctrl Pts',(-0.964442216133727,-1.22043976126517,
4.05495992825379));
#263640=CARTESIAN_POINT('Ctrl Pts',(-0.959364414684744,-1.22443534604672,
4.05542216985932));
#263641=CARTESIAN_POINT('Ctrl Pts',(-0.945690112324847,-1.23505800606424,
4.05666433401356));
#263642=CARTESIAN_POINT('Ctrl Pts',(-0.937049031460018,-1.24162682334011,
4.05744652687098));
#263643=CARTESIAN_POINT('Ctrl Pts',(-0.893630544478683,-1.27392149298274,
4.06136390295115));
#263644=CARTESIAN_POINT('Ctrl Pts',(-0.85786263575134,-1.29827675702903,
4.06455109272063));
#263645=CARTESIAN_POINT('Ctrl Pts',(-0.677790454380509,-1.41019991428294,
4.08042346862211));
#263646=CARTESIAN_POINT('Ctrl Pts',(-0.520943356939866,-1.47535267949552,
4.09388503637533));
#263647=CARTESIAN_POINT('Ctrl Pts',(-0.33926571652047,-1.51815693950149,
4.10782140738633));
#263648=CARTESIAN_POINT('Ctrl Pts',(-0.32174316597514,-1.52196686194536,
4.10914762114653));
#263649=CARTESIAN_POINT('Ctrl Pts',(-0.298549639874176,-1.52659132148868,
4.1108761528686));
#263650=CARTESIAN_POINT('Ctrl Pts',(-0.29293536543642,-1.5276785737662,
4.11129249747033));
#263651=CARTESIAN_POINT('Ctrl Pts',(-0.283852127923382,-1.5293857052043,
4.11196261942163));
#263652=CARTESIAN_POINT('Ctrl Pts',(-0.280386901669633,-1.53002478798759,
4.11221745340248));
#263653=CARTESIAN_POINT('Ctrl Pts',(-0.273689173249273,-1.5312365143614,
4.11270839398404));
#263654=CARTESIAN_POINT('Ctrl Pts',(-0.270457011655737,-1.53181070356316,
4.11294458134071));
#263655=CARTESIAN_POINT('Ctrl Pts',(-0.262721997262527,-1.53315957340096,
4.11350811502675));
#263656=CARTESIAN_POINT('Ctrl Pts',(-0.258217454185146,-1.53392466344834,
4.11383492228367));
#263657=CARTESIAN_POINT('Ctrl Pts',(-0.242841356666374,-1.53646661884572,
4.11494599965505));
#263658=CARTESIAN_POINT('Ctrl Pts',(-0.23195399546229,-1.53814789848327,
4.11572511347373));
#263659=CARTESIAN_POINT('Ctrl Pts',(-0.168706260736674,-1.54722807288897,
4.1202120300487));
#263660=CARTESIAN_POINT('Ctrl Pts',(-0.116007606723696,-1.55206961291846,
4.12379566224567));
#263661=CARTESIAN_POINT('Ctrl Pts',(0.0777742173168805,-1.5599443465302,
4.13674072016949));
#263662=CARTESIAN_POINT('Ctrl Pts',(0.218823709911104,-1.54647724371604,
4.14577731547206));
#263663=CARTESIAN_POINT('Ctrl Pts',(0.361642554461439,-1.5128869756134,
4.1558377876486));
#263664=CARTESIAN_POINT('Ctrl Pts',(0.367149554280194,-1.51155996958776,
4.15622704356669));
#263665=CARTESIAN_POINT('Ctrl Pts',(0.396818803031542,-1.50423895367792,
4.15833164093067));
#263666=CARTESIAN_POINT('Ctrl Pts',(0.420840569521701,-1.49769592609991,
4.16006246247689));
#263667=CARTESIAN_POINT('Ctrl Pts',(0.453552730883087,-1.48793670384046,
4.16246145737352));
#263668=CARTESIAN_POINT('Ctrl Pts',(0.462387673820956,-1.4852149160423,
4.16311362580804));
#263669=CARTESIAN_POINT('Ctrl Pts',(0.476437860270363,-1.48074894878524,
4.164157793315));
#263670=CARTESIAN_POINT('Ctrl Pts',(0.481669127153877,-1.4790555549275,
4.16454812791854));
#263671=CARTESIAN_POINT('Ctrl Pts',(0.492409067032947,-1.47551594844627,
4.16535277266688));
#263672=CARTESIAN_POINT('Ctrl Pts',(0.497916587541557,-1.47366654083732,
4.16576718236396));
#263673=CARTESIAN_POINT('Ctrl Pts',(0.510675431126764,-1.46930247348155,
4.16673142601889));
#263674=CARTESIAN_POINT('Ctrl Pts',(0.517918706230046,-1.46676493152849,
4.1672820073791));
#263675=CARTESIAN_POINT('Ctrl Pts',(0.540976526368626,-1.45849497966674,
4.16904504567866));
#263676=CARTESIAN_POINT('Ctrl Pts',(0.55671650194667,-1.45255977604736,
4.17026418346186));
#263677=CARTESIAN_POINT('Ctrl Pts',(0.636160456066184,-1.421122282574,4.17649976708454));
#263678=CARTESIAN_POINT('Ctrl Pts',(0.698214194750551,-1.39168354780934,
4.18164658268046));
#263679=CARTESIAN_POINT('Ctrl Pts',(0.836049938356933,-1.31474973943011,
4.19371478994464));
#263680=CARTESIAN_POINT('Ctrl Pts',(0.91009460993814,-1.26462355798037,
4.20068731267486));
#263681=CARTESIAN_POINT('Ctrl Pts',(0.988398205587733,-1.20115885285792,
4.20845147774913));
#263682=CARTESIAN_POINT('Ctrl Pts',(0.997288339773477,-1.19378791188782,
4.20933894142703));
#263683=CARTESIAN_POINT('Ctrl Pts',(1.01323283366311,-1.18026566950767,
4.21094050999283));
#263684=CARTESIAN_POINT('Ctrl Pts',(1.02031531446666,-1.17414841088826,
4.21165554394833));
#263685=CARTESIAN_POINT('Ctrl Pts',(1.05592503856544,-1.14282615689047,
4.21526756329304));
#263686=CARTESIAN_POINT('Ctrl Pts',(1.08357830840925,-1.11664137220616,
4.21812849655396));
#263687=CARTESIAN_POINT('Ctrl Pts',(1.1148856267033,-1.0847369182519,4.22140821448593));
#263688=CARTESIAN_POINT('Ctrl Pts',(1.11949569800391,-1.07997848532729,
4.221892242288));
#263689=CARTESIAN_POINT('Ctrl Pts',(1.12692348029859,-1.07221299088711,
4.22267366633463));
#263690=CARTESIAN_POINT('Ctrl Pts',(1.12975982814149,-1.0692239990075,4.22297243145923));
#263691=CARTESIAN_POINT('Ctrl Pts',(1.13479286430116,-1.0638777122507,4.22350319460486));
#263692=CARTESIAN_POINT('Ctrl Pts',(1.13699413265376,-1.06152483461684,
4.22373553853354));
#263693=CARTESIAN_POINT('Ctrl Pts',(1.14174676413533,-1.05641312765597,
4.22423762175113));
#263694=CARTESIAN_POINT('Ctrl Pts',(1.14429544374883,-1.05365189124394,
4.2245071586076));
#263695=CARTESIAN_POINT('Ctrl Pts',(1.15141395257934,-1.04588341344925,
4.22526087925594));
#263696=CARTESIAN_POINT('Ctrl Pts',(1.15596116663405,-1.04085541284043,
4.22574339438784));
#263697=CARTESIAN_POINT('Ctrl Pts',(1.18319760407226,-1.01034055750956,
4.22864106613245));
#263698=CARTESIAN_POINT('Ctrl Pts',(1.20507811896355,-0.984140125181842,
4.23100091095797));
#263699=CARTESIAN_POINT('Ctrl Pts',(1.30251310311015,-0.85934033870235,
4.24177863056146));
#263700=CARTESIAN_POINT('Ctrl Pts',(1.36695060340608,-0.752633848788471,
4.24973944472308));
#263701=CARTESIAN_POINT('Ctrl Pts',(1.44516833388122,-0.579165914038873,
4.26243869235881));
#263702=CARTESIAN_POINT('Ctrl Pts',(1.46845638987722,-0.517280117187117,
4.26692044781474));
#263703=CARTESIAN_POINT('Ctrl Pts',(1.49108537513476,-0.443143382239921,
4.27233793344677));
#263704=CARTESIAN_POINT('Ctrl Pts',(1.49431050029174,-0.432143228029316,
4.2731428590699));
#263705=CARTESIAN_POINT('Ctrl Pts',(1.49938268743468,-0.414107118481615,
4.27446492570531));
#263706=CARTESIAN_POINT('Ctrl Pts',(1.50130253499648,-0.40709193571732,
4.27497970809834));
#263707=CARTESIAN_POINT('Ctrl Pts',(1.50465411644762,-0.394498922106461,
4.27590492595451));
#263708=CARTESIAN_POINT('Ctrl Pts',(1.50610421713621,-0.388926079324327,
4.27631476040796));
#263709=CARTESIAN_POINT('Ctrl Pts',(1.50911713722793,-0.377077632642883,
4.27718701079093));
#263710=CARTESIAN_POINT('Ctrl Pts',(1.51067182493599,-0.370800094291751,
4.27764967979514));
#263711=CARTESIAN_POINT('Ctrl Pts',(1.51473712958283,-0.353935126891896,
4.27889419984797));
#263712=CARTESIAN_POINT('Ctrl Pts',(1.5171758355512,-0.343330917087015,
4.27967833623452));
#263713=CARTESIAN_POINT('Ctrl Pts',(1.52882873833049,-0.290110292316033,
4.28362261958471));
#263714=CARTESIAN_POINT('Ctrl Pts',(1.53635860865336,-0.247149391869968,
4.28683563920812));
#263715=CARTESIAN_POINT('Ctrl Pts',(1.56500597751739,-0.0305271532176449,
4.30319814874146));
#263716=CARTESIAN_POINT('Ctrl Pts',(1.5585246537258,0.145462889455811,4.31719136789475));
#263717=CARTESIAN_POINT('Ctrl Pts',(1.52030008014965,0.32929352736384,4.33111142013338));
#263718=CARTESIAN_POINT('Ctrl Pts',(1.5175176579023,0.341887039580946,4.33206042734252));
#263719=CARTESIAN_POINT('Ctrl Pts',(1.51343593795752,0.359328634364998,
4.33336704067547));
#263720=CARTESIAN_POINT('Ctrl Pts',(1.5122694307825,0.364206776949679,4.33373163565615));
#263721=CARTESIAN_POINT('Ctrl Pts',(1.5103593067695,0.372027180441728,4.33431468798085));
#263722=CARTESIAN_POINT('Ctrl Pts',(1.50963065292883,0.374972999965682,
4.33453398355718));
#263723=CARTESIAN_POINT('Ctrl Pts',(1.50808561069267,0.381141830230326,
4.33499248910738));
#263724=CARTESIAN_POINT('Ctrl Pts',(1.50726750335325,0.384364381294637,
4.33523159311462));
#263725=CARTESIAN_POINT('Ctrl Pts',(1.50524435844471,0.392227817504962,
4.33581407538145));
#263726=CARTESIAN_POINT('Ctrl Pts',(1.50402816905935,0.396865856138813,
4.33615681765806));
#263727=CARTESIAN_POINT('Ctrl Pts',(1.49958146602152,0.413509671475075,
4.33738406569791));
#263728=CARTESIAN_POINT('Ctrl Pts',(1.49622837548985,0.425482662310641,
4.33826185065595));
#263729=CARTESIAN_POINT('Ctrl Pts',(1.4875503041076,0.455097660655022,4.34042344894152));
#263730=CARTESIAN_POINT('Ctrl Pts',(1.48205459103537,0.472688107251331,
4.34169886508878));
#263731=CARTESIAN_POINT('Ctrl Pts',(1.46376367029956,0.527774103569199,
4.34567828967784));
#263732=CARTESIAN_POINT('Ctrl Pts',(1.44986059937387,0.564843095112567,
4.34833476639215));
#263733=CARTESIAN_POINT('Ctrl Pts',(1.43457657355089,0.601307163285946,
4.35096339883546));
#263734=CARTESIAN_POINT('Origin',(0.,0.,-1.29405622560371));
#263735=CARTESIAN_POINT('',(1.43457674133487,0.601306762992916,5.18837549714138));
#263736=CARTESIAN_POINT('',(1.43231908414271,0.600352779935808,5.05019128547067));
#263737=CARTESIAN_POINT('',(1.43457668357355,0.601306900797845,-1.29405622560371));
#263738=CARTESIAN_POINT('',(-1.55549950191149,0.00135080560319381,4.79375124639878));
#263739=CARTESIAN_POINT('Ctrl Pts',(1.43457674133486,0.601306762992946,
5.18837549714138));
#263740=CARTESIAN_POINT('Ctrl Pts',(1.44511665628854,0.576161000831655,
5.18657941512783));
#263741=CARTESIAN_POINT('Ctrl Pts',(1.45499927553352,0.550728945127526,
5.18477898999173));
#263742=CARTESIAN_POINT('Ctrl Pts',(1.49012990958986,0.452757154467981,
5.17786919516953));
#263743=CARTESIAN_POINT('Ctrl Pts',(1.5106566959811,0.378668668901701,5.17269057112632));
#263744=CARTESIAN_POINT('Ctrl Pts',(1.52791039167112,0.291902219434232,
5.16651001909783));
#263745=CARTESIAN_POINT('Ctrl Pts',(1.53006217189651,0.280404721248481,
5.16568890524646));
#263746=CARTESIAN_POINT('Ctrl Pts',(1.53334524896578,0.261697977929183,
5.16434895645143));
#263747=CARTESIAN_POINT('Ctrl Pts',(1.53455587125645,0.25450296441266,5.16383263406341));
#263748=CARTESIAN_POINT('Ctrl Pts',(1.53662174083545,0.241674048030772,
5.16291020372617));
#263749=CARTESIAN_POINT('Ctrl Pts',(1.5374967388295,0.236043420595086,5.16250472794051));
#263750=CARTESIAN_POINT('Ctrl Pts',(1.53927664022648,0.224159750156223,
5.16164758571647));
#263751=CARTESIAN_POINT('Ctrl Pts',(1.54017442039981,0.217905762445593,
5.16119570223162));
#263752=CARTESIAN_POINT('Ctrl Pts',(1.54245410721025,0.201306981085136,
5.15999414384703));
#263753=CARTESIAN_POINT('Ctrl Pts',(1.54377002253141,0.190953609932005,
5.15924240728233));
#263754=CARTESIAN_POINT('Ctrl Pts',(1.54953539191411,0.141629240685879,
5.15564961722445));
#263755=CARTESIAN_POINT('Ctrl Pts',(1.55261353490029,0.102515718359522,
5.15276610768367));
#263756=CARTESIAN_POINT('Ctrl Pts',(1.56029845675663,-0.0860812013401728,
5.13868291784823));
#263757=CARTESIAN_POINT('Ctrl Pts',(1.54480671724319,-0.235582682449016,
5.12687535157839));
#263758=CARTESIAN_POINT('Ctrl Pts',(1.49869668795058,-0.41834109111477,
5.11250962193625));
#263759=CARTESIAN_POINT('Ctrl Pts',(1.48773700552715,-0.455785329332024,
5.10957691072483));
#263760=CARTESIAN_POINT('Ctrl Pts',(1.47327985518892,-0.499069806126764,
5.10622842352198));
#263761=CARTESIAN_POINT('Ctrl Pts',(1.47113933508363,-0.505344698249422,
5.10574404660611));
#263762=CARTESIAN_POINT('Ctrl Pts',(1.46761174412288,-0.515473365386924,
5.10496409831294));
#263763=CARTESIAN_POINT('Ctrl Pts',(1.46624948829557,-0.519335595762319,
5.10466714309885));
#263764=CARTESIAN_POINT('Ctrl Pts',(1.46380116425743,-0.526190589930062,
5.10414094368091));
#263765=CARTESIAN_POINT('Ctrl Pts',(1.46272114810832,-0.529185439132385,
5.10391135053028));
#263766=CARTESIAN_POINT('Ctrl Pts',(1.46036997794362,-0.535642961879161,
5.10341694812502));
#263767=CARTESIAN_POINT('Ctrl Pts',(1.45909570169352,-0.539104432513673,
5.10315232698491));
#263768=CARTESIAN_POINT('Ctrl Pts',(1.45550967446661,-0.54873973513554,
5.10241675061996));
#263769=CARTESIAN_POINT('Ctrl Pts',(1.45317093385964,-0.554903550633025,
5.10194736365208));
#263770=CARTESIAN_POINT('Ctrl Pts',(1.43930726854894,-0.590752798997594,
5.09922315618627));
#263771=CARTESIAN_POINT('Ctrl Pts',(1.42691113019264,-0.620096185616808,
5.09701650839229));
#263772=CARTESIAN_POINT('Ctrl Pts',(1.35281569164905,-0.781477274138088,
5.08489882734599));
#263773=CARTESIAN_POINT('Ctrl Pts',(1.27369802629424,-0.904720226578485,
5.0756496725934));
#263774=CARTESIAN_POINT('Ctrl Pts',(1.14650171308311,-1.05239207209561,
5.06250280738294));
#263775=CARTESIAN_POINT('Ctrl Pts',(1.1126866684412,-1.08808216994098,5.05913685044029));
#263776=CARTESIAN_POINT('Ctrl Pts',(1.06891311172136,-1.13010544455532,
5.05488953970839));
#263777=CARTESIAN_POINT('Ctrl Pts',(1.06049559540173,-1.13800818786546,
5.05407755197911));
#263778=CARTESIAN_POINT('Ctrl Pts',(1.04710705239501,-1.15030040933622,
5.05279296410192));
#263779=CARTESIAN_POINT('Ctrl Pts',(1.04219447285095,-1.15475317240732,
5.05232305467617));
#263780=CARTESIAN_POINT('Ctrl Pts',(1.03307474280039,-1.16291369924173,
5.05145325598756));
#263781=CARTESIAN_POINT('Ctrl Pts',(1.02887570206087,-1.16663039746671,
5.05105375039945));
#263782=CARTESIAN_POINT('Ctrl Pts',(1.01952412232708,-1.17481800766422,
5.05016612159405));
#263783=CARTESIAN_POINT('Ctrl Pts',(1.01436210958863,-1.17927787015013,
5.0496775516157));
#263784=CARTESIAN_POINT('Ctrl Pts',(0.999459053284507,-1.19198352777962,
5.04827087530776));
#263785=CARTESIAN_POINT('Ctrl Pts',(0.98964584809316,-1.20014341100722,
5.04734929257613));
#263786=CARTESIAN_POINT('Ctrl Pts',(0.911981033914877,-1.26312305061513,
5.04008998686995));
#263787=CARTESIAN_POINT('Ctrl Pts',(0.839740027161673,-1.31225790795481,
5.03352720670584));
#263788=CARTESIAN_POINT('Ctrl Pts',(0.691906041537649,-1.39558319102782,
5.0204826246957));
#263789=CARTESIAN_POINT('Ctrl Pts',(0.616930312737117,-1.43030867292629,
5.01403793598719));
#263790=CARTESIAN_POINT('Ctrl Pts',(0.521606335950648,-1.46556246225637,
5.00622639805155));
#263791=CARTESIAN_POINT('Ctrl Pts',(0.503535264990488,-1.47186914709442,
5.00476218649622));
#263792=CARTESIAN_POINT('Ctrl Pts',(0.452160624595348,-1.4887415827988,
5.00065379415605));
#263793=CARTESIAN_POINT('Ctrl Pts',(0.418608262441636,-1.49852204731149,
4.99803409329177));
#263794=CARTESIAN_POINT('Ctrl Pts',(0.378535284889602,-1.5087519520649,
4.9950009921966));
#263795=CARTESIAN_POINT('Ctrl Pts',(0.372308771431782,-1.51030049900207,
4.99453241871477));
#263796=CARTESIAN_POINT('Ctrl Pts',(0.362154982095782,-1.5127591571304,
4.99377289608467));
#263797=CARTESIAN_POINT('Ctrl Pts',(0.358233519220936,-1.5136925861087,
4.99348067570635));
#263798=CARTESIAN_POINT('Ctrl Pts',(0.351213561048297,-1.5153347441316,
4.99295960226092));
#263799=CARTESIAN_POINT('Ctrl Pts',(0.348116492459623,-1.51604922761923,
4.99273042707443));
#263800=CARTESIAN_POINT('Ctrl Pts',(0.341375553850311,-1.51758259370568,
4.99223316818022));
#263801=CARTESIAN_POINT('Ctrl Pts',(0.337730922926314,-1.51839784706743,
4.99196529301813));
#263802=CARTESIAN_POINT('Ctrl Pts',(0.32743705508155,-1.5206615449312,4.9912113749073));
#263803=CARTESIAN_POINT('Ctrl Pts',(0.320781088372202,-1.5220795173554,
4.99072702940935));
#263804=CARTESIAN_POINT('Ctrl Pts',(0.279115178601945,-1.53067047261114,
4.98771338608054));
#263805=CARTESIAN_POINT('Ctrl Pts',(0.243872642686833,-1.53667954383986,
4.98524501563371));
#263806=CARTESIAN_POINT('Ctrl Pts',(0.119716552090874,-1.55346901745102,
4.9767304014672));
#263807=CARTESIAN_POINT('Ctrl Pts',(0.0301045339338664,-1.55778509748695,
4.97090001568472));
#263808=CARTESIAN_POINT('Ctrl Pts',(-0.079524991373503,-1.55359652177789,
4.96366612663505));
#263809=CARTESIAN_POINT('Ctrl Pts',(-0.0996457580148266,-1.55243585318808,
4.9623347078501));
#263810=CARTESIAN_POINT('Ctrl Pts',(-0.197933206649732,-1.54484744562266,
4.95579463698577));
#263811=CARTESIAN_POINT('Ctrl Pts',(-0.275548843800916,-1.53290616649866,
4.95051007562073));
#263812=CARTESIAN_POINT('Ctrl Pts',(-0.363361780290477,-1.51250993099005,
4.94421220008269));
#263813=CARTESIAN_POINT('Ctrl Pts',(-0.374766523701754,-1.50972451598622,
4.9433881196476));
#263814=CARTESIAN_POINT('Ctrl Pts',(-0.393218630615451,-1.50499594038704,
4.94204428298487));
#263815=CARTESIAN_POINT('Ctrl Pts',(-0.400285896940939,-1.50313168733213,
4.94152706369445));
#263816=CARTESIAN_POINT('Ctrl Pts',(-0.412840520722027,-1.49972512209381,
4.94060363012479));
#263817=CARTESIAN_POINT('Ctrl Pts',(-0.418333073292665,-1.49820231464093,
4.94019805313648));
#263818=CARTESIAN_POINT('Ctrl Pts',(-0.429889428686015,-1.49492981760381,
4.93934131637627));
#263819=CARTESIAN_POINT('Ctrl Pts',(-0.435951185867858,-1.49317334620884,
4.93888994273688));
#263820=CARTESIAN_POINT('Ctrl Pts',(-0.451141461550569,-1.48867138692364,
4.93775376196994));
#263821=CARTESIAN_POINT('Ctrl Pts',(-0.460255632774021,-1.48587881792385,
4.93706743178289));
#263822=CARTESIAN_POINT('Ctrl Pts',(-0.501373085326017,-1.47286589230966,
4.93394969732927));
#263823=CARTESIAN_POINT('Ctrl Pts',(-0.533063498035386,-1.46169486921233,
4.93148745237136));
#263824=CARTESIAN_POINT('Ctrl Pts',(-0.618453142547712,-1.42844843843008,
4.92468325954966));
#263825=CARTESIAN_POINT('Ctrl Pts',(-0.671313888997831,-1.40438083582509,
4.92028129313621));
#263826=CARTESIAN_POINT('Ctrl Pts',(-0.812122273003252,-1.33050177653107,
4.90806142300212));
#263827=CARTESIAN_POINT('Ctrl Pts',(-0.896759722897099,-1.27498994923714,
4.90014119504225));
#263828=CARTESIAN_POINT('Ctrl Pts',(-1.00359603224231,-1.18898430943612,
4.88971043858193));
#263829=CARTESIAN_POINT('Ctrl Pts',(-1.03097578303879,-1.16532319025755,
4.88699559969048));
#263830=CARTESIAN_POINT('Ctrl Pts',(-1.06225966717474,-1.1363215354992,
4.88386662329599));
#263831=CARTESIAN_POINT('Ctrl Pts',(-1.0669838748675,-1.13188676431571,
4.88339336162019));
#263832=CARTESIAN_POINT('Ctrl Pts',(-1.07461586352522,-1.12463211735273,
4.88262777380986));
#263833=CARTESIAN_POINT('Ctrl Pts',(-1.07754052069459,-1.12183023706423,
4.8823341434636));
#263834=CARTESIAN_POINT('Ctrl Pts',(-1.08274178058477,-1.11680821888323,
4.8818115538238));
#263835=CARTESIAN_POINT('Ctrl Pts',(-1.08502254388912,-1.11459250002306,
4.88158226440692));
#263836=CARTESIAN_POINT('Ctrl Pts',(-1.08944696822507,-1.11026780362926,
4.88113721537358));
#263837=CARTESIAN_POINT('Ctrl Pts',(-1.09159129617159,-1.10815961616078,
4.88092139794605));
#263838=CARTESIAN_POINT('Ctrl Pts',(-1.09777911380515,-1.10204069911733,
4.88029821893327));
#263839=CARTESIAN_POINT('Ctrl Pts',(-1.10180676680968,-1.09801390543519,
4.87989209220409));
#263840=CARTESIAN_POINT('Ctrl Pts',(-1.12013114783766,-1.07949107710251,
4.87804153174208));
#263841=CARTESIAN_POINT('Ctrl Pts',(-1.13416536724222,-1.06473649301567,
4.87661628095115));
#263842=CARTESIAN_POINT('Ctrl Pts',(-1.17284360760615,-1.02244002497955,
4.87265053641538));
#263843=CARTESIAN_POINT('Ctrl Pts',(-1.19680284400498,-0.994288242983664,
4.87014872059939));
#263844=CARTESIAN_POINT('Ctrl Pts',(-1.25768183783196,-0.917363091393411,
4.8635849916298));
#263845=CARTESIAN_POINT('Ctrl Pts',(-1.29276707498899,-0.867221158893708,
4.85957802836032));
#263846=CARTESIAN_POINT('Ctrl Pts',(-1.38099410670971,-0.723830107117304,
4.84849212400466));
#263847=CARTESIAN_POINT('Ctrl Pts',(-1.42757813784364,-0.62696921113851,
4.84138372230398));
#263848=CARTESIAN_POINT('Ctrl Pts',(-1.46781896986126,-0.515001680400421,
4.83307252974104));
#263849=CARTESIAN_POINT('Ctrl Pts',(-1.47168024637885,-0.503861586239718,
4.83224496394543));
#263850=CARTESIAN_POINT('Ctrl Pts',(-1.47773421905505,-0.485731891844201,
4.83089656065398));
#263851=CARTESIAN_POINT('Ctrl Pts',(-1.48000488606757,-0.478768656893854,
4.83037828887711));
#263852=CARTESIAN_POINT('Ctrl Pts',(-1.48395557725663,-0.466356733587377,
4.82945367603051));
#263853=CARTESIAN_POINT('Ctrl Pts',(-1.48565499038759,-0.460914315448052,
4.82904797827144));
#263854=CARTESIAN_POINT('Ctrl Pts',(-1.48917000411102,-0.44943595450738,
4.82819170750025));
#263855=CARTESIAN_POINT('Ctrl Pts',(-1.49097891076522,-0.443398087322087,
4.82774092431618));
#263856=CARTESIAN_POINT('Ctrl Pts',(-1.49457898433125,-0.431110400010262,
4.82682271794426));
#263857=CARTESIAN_POINT('Ctrl Pts',(-1.49636776269077,-0.424860016707826,
4.82635522700537));
#263858=CARTESIAN_POINT('Ctrl Pts',(-1.50070702967631,-0.409330271867054,
4.82519255412897));
#263859=CARTESIAN_POINT('Ctrl Pts',(-1.50321065606974,-0.400038218326202,
4.82449587349808));
#263860=CARTESIAN_POINT('Ctrl Pts',(-1.5099754364029,-0.373970587772576,
4.82253835731351));
#263861=CARTESIAN_POINT('Ctrl Pts',(-1.51404293375601,-0.357146705601624,
4.82127143326522));
#263862=CARTESIAN_POINT('Ctrl Pts',(-1.54297058110204,-0.228106164304975,
4.81152441339957));
#263863=CARTESIAN_POINT('Ctrl Pts',(-1.55559911830794,-0.113535921865477,
4.80266052462882));
#263864=CARTESIAN_POINT('Ctrl Pts',(-1.5554994142228,0.00134994538273571,
4.79375115972409));
#263865=CARTESIAN_POINT('Ctrl Pts',(-1.55549941348635,0.00135079370216905,
4.79375109393717));
#263866=CARTESIAN_POINT('Ctrl Pts',(-1.55543982818356,0.069965937072524,
4.78843000999));
#263867=CARTESIAN_POINT('Ctrl Pts',(-1.55084024178991,0.138509195077084,
4.78311715906412));
#263868=CARTESIAN_POINT('Ctrl Pts',(-1.53903776772294,0.226613171187347,
4.77643903602023));
#263869=CARTESIAN_POINT('Ctrl Pts',(-1.53595525860854,0.246642097481528,
4.77493141603258));
#263870=CARTESIAN_POINT('Ctrl Pts',(-1.5315242001828,0.272112308381628,
4.77303229281784));
#263871=CARTESIAN_POINT('Ctrl Pts',(-1.53053662561479,0.27761326380552,
4.77262321010403));
#263872=CARTESIAN_POINT('Ctrl Pts',(-1.52884369292503,0.286759474109722,
4.77194497886987));
#263873=CARTESIAN_POINT('Ctrl Pts',(-1.528154904379,0.290407683044102,4.77167496151767));
#263874=CARTESIAN_POINT('Ctrl Pts',(-1.5268831462123,0.297013798197322,
4.77118699127725));
#263875=CARTESIAN_POINT('Ctrl Pts',(-1.52630462953548,0.299972526718701,
4.77096879467688));
#263876=CARTESIAN_POINT('Ctrl Pts',(-1.52509885048197,0.306045483211395,
4.7705216873708));
#263877=CARTESIAN_POINT('Ctrl Pts',(-1.524470656883,0.309159438179908,4.77029284219876));
#263878=CARTESIAN_POINT('Ctrl Pts',(-1.52302894460566,0.316194753018226,
4.76977673267639));
#263879=CARTESIAN_POINT('Ctrl Pts',(-1.52220982034231,0.320114904008777,
4.76948979061479));
#263880=CARTESIAN_POINT('Ctrl Pts',(-1.51968757989683,0.331957179008913,
4.76862478833012));
#263881=CARTESIAN_POINT('Ctrl Pts',(-1.51793765671912,0.339869367601111,
4.76804931055348));
#263882=CARTESIAN_POINT('Ctrl Pts',(-1.49879387502669,0.423328469941545,
4.76200154058142));
#263883=CARTESIAN_POINT('Ctrl Pts',(-1.47583442862184,0.49750037380237,
4.75681921959069));
#263884=CARTESIAN_POINT('Ctrl Pts',(-1.4254014638762,0.625644100516097,
4.74771549031625));
#263885=CARTESIAN_POINT('Ctrl Pts',(-1.40013891305393,0.680302088247146,
4.74377981351629));
#263886=CARTESIAN_POINT('Ctrl Pts',(-1.33827749464894,0.796015985039271,
4.73509304183178));
#263887=CARTESIAN_POINT('Ctrl Pts',(-1.30053147529157,0.856296762508328,
4.73033181777074));
#263888=CARTESIAN_POINT('Ctrl Pts',(-1.24612144789291,0.931250502293052,
4.72392908008005));
#263889=CARTESIAN_POINT('Ctrl Pts',(-1.23307965899597,0.948451704524512,
4.72242432616688));
#263890=CARTESIAN_POINT('Ctrl Pts',(-1.21564741200728,0.970476140085881,
4.72044790699084));
#263891=CARTESIAN_POINT('Ctrl Pts',(-1.21157819230199,0.975551562160408,
4.71998892662598));
#263892=CARTESIAN_POINT('Ctrl Pts',(-1.20350208479432,0.9854961922074,4.71908253682474));
#263893=CARTESIAN_POINT('Ctrl Pts',(-1.19949718490783,0.990366858406006,
4.71863521246902));
#263894=CARTESIAN_POINT('Ctrl Pts',(-1.19181533593243,0.999594395807111,
4.71778117481726));
#263895=CARTESIAN_POINT('Ctrl Pts',(-1.18814382423592,1.00395567752366,
4.71737468714752));
#263896=CARTESIAN_POINT('Ctrl Pts',(-1.17970419424875,1.01386973112551,
4.71644408580829));
#263897=CARTESIAN_POINT('Ctrl Pts',(-1.17492072492786,1.01940919377976,
4.71591934622949));
#263898=CARTESIAN_POINT('Ctrl Pts',(-1.1623411767919,1.03377069205574,4.71454626729671));
#263899=CARTESIAN_POINT('Ctrl Pts',(-1.15448384974252,1.04253819187838,
4.7136953927718));
#263900=CARTESIAN_POINT('Ctrl Pts',(-1.09262295439683,1.11000794484178,
4.70704699132472));
#263901=CARTESIAN_POINT('Ctrl Pts',(-1.03428526917837,1.1645568158285,4.70106257585066));
#263902=CARTESIAN_POINT('Ctrl Pts',(-0.899099408804229,1.27276381111295,
4.68779097043489));
#263903=CARTESIAN_POINT('Ctrl Pts',(-0.82105951223368,1.32444996704154,
4.68047954029265));
#263904=CARTESIAN_POINT('Ctrl Pts',(-0.70923240487482,1.38481150561327,
4.67073174931814));
#263905=CARTESIAN_POINT('Ctrl Pts',(-0.679095037032262,1.39983705104924,
4.66817261701057));
#263906=CARTESIAN_POINT('Ctrl Pts',(-0.631100562305024,1.42185034743603,
4.66422565181814));
#263907=CARTESIAN_POINT('Ctrl Pts',(-0.613562611104443,1.42950597844899,
4.66280947280792));
#263908=CARTESIAN_POINT('Ctrl Pts',(-0.590840131533242,1.43892947658228,
4.66101188555856));
#263909=CARTESIAN_POINT('Ctrl Pts',(-0.58578234729258,1.44099588604967,
4.66061410569835));
#263910=CARTESIAN_POINT('Ctrl Pts',(-0.577928137760229,1.44415661664662,
4.66000013438606));
#263911=CARTESIAN_POINT('Ctrl Pts',(-0.575139324048191,1.44526953339813,
4.65978285730039));
#263912=CARTESIAN_POINT('Ctrl Pts',(-0.569388302008386,1.44754528013879,
4.65933631567059));
#263913=CARTESIAN_POINT('Ctrl Pts',(-0.566425786505574,1.44870708054433,
4.65910712326779));
#263914=CARTESIAN_POINT('Ctrl Pts',(-0.559657483629574,1.45133744897327,
4.6585853789857));
#263915=CARTESIAN_POINT('Ctrl Pts',(-0.555849473156135,1.45280014248085,
4.65829317984575));
#263916=CARTESIAN_POINT('Ctrl Pts',(-0.5458878753069,1.45658158698531,4.65753220005038));
#263917=CARTESIAN_POINT('Ctrl Pts',(-0.539725175582285,1.45887635899957,
4.65706480159645));
#263918=CARTESIAN_POINT('Ctrl Pts',(-0.497711319978021,1.47421816701328,
4.65390004667076));
#263919=CARTESIAN_POINT('Ctrl Pts',(-0.461401588683426,1.48598281862127,
4.65127205055478));
#263920=CARTESIAN_POINT('Ctrl Pts',(-0.41599855517151,1.49886861389726,
4.64807395067595));
#263921=CARTESIAN_POINT('Ctrl Pts',(-0.407283296304176,1.50126021784478,
4.64746401951149));
#263922=CARTESIAN_POINT('Ctrl Pts',(-0.275813348439974,1.53610849487521,
4.63831584352315));
#263923=CARTESIAN_POINT('Ctrl Pts',(-0.149556377549204,1.55349224672585,
4.63017890659324));
#263924=CARTESIAN_POINT('Ctrl Pts',(0.0116176225624342,1.55583269551161,
4.61932043467574));
#263925=CARTESIAN_POINT('Ctrl Pts',(0.0458256458859801,1.55520098190422,
4.61699199032896));
#263926=CARTESIAN_POINT('Ctrl Pts',(0.102804957954734,1.55226724579149,
4.61305335520266));
#263927=CARTESIAN_POINT('Ctrl Pts',(0.125596922893809,1.55058949456994,
4.61146181967363));
#263928=CARTESIAN_POINT('Ctrl Pts',(0.157052910614164,1.54757591020215,
4.60923923700843));
#263929=CARTESIAN_POINT('Ctrl Pts',(0.165755788399802,1.54666797586798,
4.60862155866719));
#263930=CARTESIAN_POINT('Ctrl Pts',(0.180365545238223,1.54501907913603,
4.60757979348178));
#263931=CARTESIAN_POINT('Ctrl Pts',(0.186276747632084,1.54431753739259,
4.60715695116993));
#263932=CARTESIAN_POINT('Ctrl Pts',(0.197933874911923,1.54286616664685,
4.60632037906376));
#263933=CARTESIAN_POINT('Ctrl Pts',(0.203679928295563,1.542118125228,4.60590671204742));
#263934=CARTESIAN_POINT('Ctrl Pts',(0.216320005406149,1.54040071793235,
4.604993800779));
#263935=CARTESIAN_POINT('Ctrl Pts',(0.223211937784856,1.53941714439342,
4.60449411602925));
#263936=CARTESIAN_POINT('Ctrl Pts',(0.247377095126415,1.53580275653071,
4.6027351548794));
#263937=CARTESIAN_POINT('Ctrl Pts',(0.26461179835137,1.53292729248878,4.60146820779354));
#263938=CARTESIAN_POINT('Ctrl Pts',(0.41299061380514,1.50559479240169,4.59044843309601));
#263939=CARTESIAN_POINT('Ctrl Pts',(0.540506912813754,1.46465474421342,
4.58014558056329));
#263940=CARTESIAN_POINT('Ctrl Pts',(0.728697270556073,1.37627768166781,
4.56403096489449));
#263941=CARTESIAN_POINT('Ctrl Pts',(0.793830706540837,1.33976688924317,
4.55827814329));
#263942=CARTESIAN_POINT('Ctrl Pts',(0.866930080054803,1.29158071974666,
4.55178915562403));
#263943=CARTESIAN_POINT('Ctrl Pts',(0.877671321333322,1.28430588283984,
4.55083492530268));
#263944=CARTESIAN_POINT('Ctrl Pts',(0.892292918818326,1.27413382788035,
4.5495362836906));
#263945=CARTESIAN_POINT('Ctrl Pts',(0.896252234757086,1.27135187800589,
4.5491846626269));
#263946=CARTESIAN_POINT('Ctrl Pts',(0.902893000656428,1.2666394100847,4.54859504681989));
#263947=CARTESIAN_POINT('Ctrl Pts',(0.905581370000086,1.26471876274122,
4.54835639297709));
#263948=CARTESIAN_POINT('Ctrl Pts',(0.910678535725685,1.26105261712095,
4.54790400937536));
#263949=CARTESIAN_POINT('Ctrl Pts',(0.913088468273824,1.25930875804642,
4.54769016681631));
#263950=CARTESIAN_POINT('Ctrl Pts',(0.919403244627676,1.25471164502745,
4.54712990411588));
#263951=CARTESIAN_POINT('Ctrl Pts',(0.923299852821414,1.25184704411527,
4.54678425957444));
#263952=CARTESIAN_POINT('Ctrl Pts',(0.936839917069813,1.24179542038698,
4.54558320678598));
#263953=CARTESIAN_POINT('Ctrl Pts',(0.946413652218577,1.23451452753686,
4.54473398944022));
#263954=CARTESIAN_POINT('Ctrl Pts',(1.03376837031311,1.16646708721101,4.5369753672142));
#263955=CARTESIAN_POINT('Ctrl Pts',(1.10569721084739,1.09852736346917,4.53050425029717));
#263956=CARTESIAN_POINT('Ctrl Pts',(1.24760810260063,0.936319330900016,
4.51632054322286));
#263957=CARTESIAN_POINT('Ctrl Pts',(1.3143521250063,0.840055254219469,4.50862303891695));
#263958=CARTESIAN_POINT('Ctrl Pts',(1.37595330447654,0.725608150931165,
4.49954531719119));
#263959=CARTESIAN_POINT('Ctrl Pts',(1.38206446684497,0.713899485485251,
4.49861789230063));
#263960=CARTESIAN_POINT('Ctrl Pts',(1.39114678072451,0.695944464919384,
4.49719692833209));
#263961=CARTESIAN_POINT('Ctrl Pts',(1.39422670555933,0.689753546190524,
4.49670719812811));
#263962=CARTESIAN_POINT('Ctrl Pts',(1.39975453296839,0.678453821338464,
4.49581363122083));
#263963=CARTESIAN_POINT('Ctrl Pts',(1.40221601379396,0.673351757521678,
4.49541027494994));
#263964=CARTESIAN_POINT('Ctrl Pts',(1.40747289066054,0.662301671924632,
4.49453685345166));
#263965=CARTESIAN_POINT('Ctrl Pts',(1.41025855922475,0.656349172514253,
4.49406646140498));
#263966=CARTESIAN_POINT('Ctrl Pts',(1.41772736123915,0.640122541054997,
4.49278434072176));
#263967=CARTESIAN_POINT('Ctrl Pts',(1.42233640257936,0.629814959941075,
4.49197009360227));
#263968=CARTESIAN_POINT('Ctrl Pts',(1.42945258601954,0.613423861039553,
4.49067531280411));
#263969=CARTESIAN_POINT('Ctrl Pts',(1.43203395656596,0.607373248773018,
4.49019736530848));
#263970=CARTESIAN_POINT('Ctrl Pts',(1.43457668488586,0.601306897666987,
4.48971815675999));
#263971=CARTESIAN_POINT('',(-1.55745558960329,-0.000855737989990104,4.65594377439629));
#263972=CARTESIAN_POINT('Ctrl Pts',(1.43457657355089,0.601307163285945,
4.35096339883546));
#263973=CARTESIAN_POINT('Ctrl Pts',(1.3925736165063,0.70151627748767,4.35818730285665));
#263974=CARTESIAN_POINT('Ctrl Pts',(1.34014205752647,0.797155671392286,
4.3652215223073));
#263975=CARTESIAN_POINT('Ctrl Pts',(1.24926110570256,0.928160613025819,
4.37596550768122));
#263976=CARTESIAN_POINT('Ctrl Pts',(1.21844401629644,0.968260671976808,
4.37942473078782));
#263977=CARTESIAN_POINT('Ctrl Pts',(1.17813738289257,1.01573138667639,4.38378252913333));
#263978=CARTESIAN_POINT('Ctrl Pts',(1.17044168169656,1.02458977121553,4.38460761692097));
#263979=CARTESIAN_POINT('Ctrl Pts',(1.15817971255643,1.03838587060438,4.38591200630471));
#263980=CARTESIAN_POINT('Ctrl Pts',(1.15368027067242,1.04338262077613,4.38638852569846));
#263981=CARTESIAN_POINT('Ctrl Pts',(1.14532097352347,1.05254566287716,4.38727004947023));
#263982=CARTESIAN_POINT('Ctrl Pts',(1.14147040807607,1.05672030866841,4.38767465694277));
#263983=CARTESIAN_POINT('Ctrl Pts',(1.13289095749044,1.06592023322632,4.38857303209543));
#263984=CARTESIAN_POINT('Ctrl Pts',(1.12815134461678,1.07093529494876,4.38906725390287));
#263985=CARTESIAN_POINT('Ctrl Pts',(1.11446520717654,1.08522514368831,4.39048859677501));
#263986=CARTESIAN_POINT('Ctrl Pts',(1.10543677678242,1.09442031435196,4.39141925307576));
#263987=CARTESIAN_POINT('Ctrl Pts',(1.03403721774355,1.16535358639662,4.39872727890072));
#263988=CARTESIAN_POINT('Ctrl Pts',(0.966668379230519,1.22181381575873,
4.40533220998903));
#263989=CARTESIAN_POINT('Ctrl Pts',(0.816790833778861,1.3272359643014,4.41942070862936));
#263990=CARTESIAN_POINT('Ctrl Pts',(0.73377697850713,1.37487225366508,4.42690201459907));
#263991=CARTESIAN_POINT('Ctrl Pts',(0.610826736534131,1.43109959018635,
4.43721133966659));
#263992=CARTESIAN_POINT('Ctrl Pts',(0.574112032521799,1.446219684007,4.44019747186926));
#263993=CARTESIAN_POINT('Ctrl Pts',(0.530558407192917,1.46223563137892,
4.44360301920776));
#263994=CARTESIAN_POINT('Ctrl Pts',(0.524246272883247,1.464510537625,4.44409327460879));
#263995=CARTESIAN_POINT('Ctrl Pts',(0.514010261963211,1.46812495650136,
4.44488274036146));
#263996=CARTESIAN_POINT('Ctrl Pts',(0.510095493087323,1.46948971630194,
4.44518336488401));
#263997=CARTESIAN_POINT('Ctrl Pts',(0.503126525789564,1.47188802039723,
4.44571615038264));
#263998=CARTESIAN_POINT('Ctrl Pts',(0.500074529233449,1.47292773464216,
4.44594866791129));
#263999=CARTESIAN_POINT('Ctrl Pts',(0.493475316980536,1.47515299169103,
4.44644967198994));
#264000=CARTESIAN_POINT('Ctrl Pts',(0.489927055354002,1.47633523245712,
4.44671796406293));
#264001=CARTESIAN_POINT('Ctrl Pts',(0.480012605910325,1.47959893482561,
4.44746467807316));
#264002=CARTESIAN_POINT('Ctrl Pts',(0.473637084705325,1.48165212721813,
4.4479414808778));
#264003=CARTESIAN_POINT('Ctrl Pts',(0.436081603369163,1.49347942444672,
4.45073143993949));
#264004=CARTESIAN_POINT('Ctrl Pts',(0.404610380642764,1.50231115028648,
4.45299395824059));
#264005=CARTESIAN_POINT('Ctrl Pts',(0.221670035916833,1.54748233417003,
4.46584043499046));
#264006=CARTESIAN_POINT('Ctrl Pts',(0.0657021567112895,1.56190000766365,
4.47568738531465));
#264007=CARTESIAN_POINT('Ctrl Pts',(-0.129110054987841,1.55063202977053,
4.48894925454823));
#264008=CARTESIAN_POINT('Ctrl Pts',(-0.168296258386443,1.54686942687954,
4.49166008962598));
#264009=CARTESIAN_POINT('Ctrl Pts',(-0.218173429158706,1.5401626809573,
4.49518658248991));
#264010=CARTESIAN_POINT('Ctrl Pts',(-0.229035775078956,1.53858484712221,
4.49595920066771));
#264011=CARTESIAN_POINT('Ctrl Pts',(-0.246290837520988,1.53589165303461,
4.49719428222171));
#264012=CARTESIAN_POINT('Ctrl Pts',(-0.25269499175137,1.53485099776413,
4.49765438489526));
#264013=CARTESIAN_POINT('Ctrl Pts',(-0.264199550809712,1.53290758855465,
4.4984840796035));
#264014=CARTESIAN_POINT('Ctrl Pts',(-0.269302342276915,1.53201936180647,
4.49885320641426));
#264015=CARTESIAN_POINT('Ctrl Pts',(-0.281256462273991,1.52987697731346,
4.4997206244924));
#264016=CARTESIAN_POINT('Ctrl Pts',(-0.288103943261745,1.5286022629328,
4.50021956109151));
#264017=CARTESIAN_POINT('Ctrl Pts',(-0.307898801275203,1.52477955896852,
4.50166802673732));
#264018=CARTESIAN_POINT('Ctrl Pts',(-0.320822325406211,1.52211280490506,
4.50262130475922));
#264019=CARTESIAN_POINT('Ctrl Pts',(-0.438144241765479,1.49634306930411,
4.51134710542526));
#264020=CARTESIAN_POINT('Ctrl Pts',(-0.539912647461299,1.46270239625917,
4.51946572721778));
#264021=CARTESIAN_POINT('Ctrl Pts',(-0.664985955054351,1.40651623139191,
4.53007154407853));
#264022=CARTESIAN_POINT('Ctrl Pts',(-0.692196018374761,1.39332654980192,
4.53241749329191));
#264023=CARTESIAN_POINT('Ctrl Pts',(-0.793746432921847,1.34039216664292,
4.54129509196237));
#264024=CARTESIAN_POINT('Ctrl Pts',(-0.865208618602949,1.29541590314831,
4.54780421116186));
#264025=CARTESIAN_POINT('Ctrl Pts',(-0.93905595959341,1.24008774000993,
4.55458479661798));
#264026=CARTESIAN_POINT('Ctrl Pts',(-0.94539408590019,1.23526261488423,
4.55516715780997));
#264027=CARTESIAN_POINT('Ctrl Pts',(-0.954906675474257,1.22790470998422,
4.55604146210108));
#264028=CARTESIAN_POINT('Ctrl Pts',(-0.958108617332074,1.22540793782187,
4.55633579934273));
#264029=CARTESIAN_POINT('Ctrl Pts',(-0.963688500381046,1.22102168214147,
4.55684875533966));
#264030=CARTESIAN_POINT('Ctrl Pts',(-0.966070711390577,1.21913775071165,
4.55706775694634));
#264031=CARTESIAN_POINT('Ctrl Pts',(-0.971307282633841,1.21497150923385,
4.55754917265716));
#264032=CARTESIAN_POINT('Ctrl Pts',(-0.974159120302818,1.21268611545753,
4.557811362684));
#264033=CARTESIAN_POINT('Ctrl Pts',(-0.981861403890726,1.20646898756828,
4.55851960214041));
#264034=CARTESIAN_POINT('Ctrl Pts',(-0.986696344337618,1.20251800901501,
4.55896430603432));
#264035=CARTESIAN_POINT('Ctrl Pts',(-0.997539627959024,1.19354774915675,
4.55996226191552));
#264036=CARTESIAN_POINT('Ctrl Pts',(-1.0035341827339,1.18851196432758,4.56051440354957));
#264037=CARTESIAN_POINT('Ctrl Pts',(-1.02202353918242,1.17274016877445,
4.56221970549458));
#264038=CARTESIAN_POINT('Ctrl Pts',(-1.03438643712738,1.16185040692115,
4.56336325704867));
#264039=CARTESIAN_POINT('Ctrl Pts',(-1.0828982469832,1.11773089354859,4.56787499274436));
#264040=CARTESIAN_POINT('Ctrl Pts',(-1.11764068087646,1.08299173656077,
4.57116196803684));
#264041=CARTESIAN_POINT('Ctrl Pts',(-1.16510332410368,1.03081215639836,
4.57583795785081));
#264042=CARTESIAN_POINT('Ctrl Pts',(-1.17919363371615,1.01466342053513,
4.57725191187616));
#264043=CARTESIAN_POINT('Ctrl Pts',(-1.27072220942585,0.905281006040948,
4.58664838314353));
#264044=CARTESIAN_POINT('Ctrl Pts',(-1.33735941336891,0.80357571374348,
4.59457211990098));
#264045=CARTESIAN_POINT('Ctrl Pts',(-1.39364965226534,0.690900651535222,
4.60331021588151));
#264046=CARTESIAN_POINT('Ctrl Pts',(-1.39576455578136,0.686618065247832,
4.60364221142822));
#264047=CARTESIAN_POINT('Ctrl Pts',(-1.40460218122327,0.668512697610301,
4.60504536521014));
#264048=CARTESIAN_POINT('Ctrl Pts',(-1.41113934638228,0.654600817253124,
4.60612252326215));
#264049=CARTESIAN_POINT('Ctrl Pts',(-1.42051747353244,0.633849468875813,
4.60772890202038));
#264050=CARTESIAN_POINT('Ctrl Pts',(-1.4235176325813,0.627082600714812,
4.60825267559974));
#264051=CARTESIAN_POINT('Ctrl Pts',(-1.42877137131088,0.615000767014447,
4.60918787325602));
#264052=CARTESIAN_POINT('Ctrl Pts',(-1.43104389260085,0.609694145217382,
4.60959864437981));
#264053=CARTESIAN_POINT('Ctrl Pts',(-1.4357707443131,0.598484327717549,
4.61046645334659));
#264054=CARTESIAN_POINT('Ctrl Pts',(-1.43821831982671,0.592578419292713,
4.61092371065716));
#264055=CARTESIAN_POINT('Ctrl Pts',(-1.44460612035277,0.576892179088964,
4.61213843158502));
#264056=CARTESIAN_POINT('Ctrl Pts',(-1.44848336388064,0.56708673379532,
4.61289799344693));
#264057=CARTESIAN_POINT('Ctrl Pts',(-1.46640752382706,0.520373617331626,
4.61651835272937));
#264058=CARTESIAN_POINT('Ctrl Pts',(-1.47914407698259,0.482982407722027,
4.6194221097683));
#264059=CARTESIAN_POINT('Ctrl Pts',(-1.53366633122595,0.300432004587034,
4.63364103423943));
#264060=CARTESIAN_POINT('Ctrl Pts',(-1.55557443644557,0.150202672118163,
4.64557540615709));
#264061=CARTESIAN_POINT('Ctrl Pts',(-1.55549980996415,-0.000768896282191608,
4.65706502508871));
#264062=CARTESIAN_POINT('Ctrl Pts',(-1.55745558960329,-0.000855737989990104,
4.65594377439629));
#264063=CARTESIAN_POINT('Ctrl Pts',(-1.55778526239128,-0.0506452214687281,
4.6595225162642));
#264064=CARTESIAN_POINT('Ctrl Pts',(-1.53303562869902,-0.615384490639257,
4.70013840098925));
#264065=CARTESIAN_POINT('Ctrl Pts',(-0.844180592856045,-1.63308701924324,
4.77779142857144));
#264066=CARTESIAN_POINT('Ctrl Pts',(0.913832949672081,-1.59515623870176,
4.88890285714287));
#264067=CARTESIAN_POINT('Ctrl Pts',(1.66723696927671,-0.371518783166273,
4.97970280944262));
#264068=CARTESIAN_POINT('Ctrl Pts',(1.52348731929008,0.384421868064892,
5.03346561888522));
#264069=CARTESIAN_POINT('Ctrl Pts',(1.43231908414271,0.600352779935808,
5.05019128547067));
#264070=CARTESIAN_POINT('Origin',(0.,0.,-1.29405622560371));
#264071=CARTESIAN_POINT('',(1.4345766835797,0.601306900783165,5.88690895590303));
#264072=CARTESIAN_POINT('',(1.43457651448711,0.601307304198121,5.74991065382822));
#264073=CARTESIAN_POINT('',(1.43457668357355,0.601306900797845,-1.29405622560371));
#264074=CARTESIAN_POINT('Ctrl Pts',(1.4345766835797,0.601306900783166,5.88690895590303));
#264075=CARTESIAN_POINT('Ctrl Pts',(1.43760164985763,0.594090043492366,
5.88632812774606));
#264076=CARTESIAN_POINT('Ctrl Pts',(1.440572208625,0.586850238760621,5.8857498616395));
#264077=CARTESIAN_POINT('Ctrl Pts',(1.4466166851779,0.571796220422545,5.8845569986114));
#264078=CARTESIAN_POINT('Ctrl Pts',(1.44968222818281,0.563978897874419,
5.8839428497635));
#264079=CARTESIAN_POINT('Ctrl Pts',(1.45413701090922,0.552342566307581,
5.88303688502469));
#264080=CARTESIAN_POINT('Ctrl Pts',(1.45557476325637,0.548542493012787,
5.88274231652757));
#264081=CARTESIAN_POINT('Ctrl Pts',(1.45811155518032,0.541757381345078,
5.88221871311359));
#264082=CARTESIAN_POINT('Ctrl Pts',(1.45921634087792,0.538774571396475,
5.88198934275535));
#264083=CARTESIAN_POINT('Ctrl Pts',(1.46159030083687,0.532304250568302,
5.88149355544579));
#264084=CARTESIAN_POINT('Ctrl Pts',(1.46285614499002,0.528815584602741,
5.88122733669668));
#264085=CARTESIAN_POINT('Ctrl Pts',(1.46631063343231,0.519187688202058,
5.88049557425245));
#264086=CARTESIAN_POINT('Ctrl Pts',(1.46847323072993,0.513039086155522,
5.88003153747311));
#264087=CARTESIAN_POINT('Ctrl Pts',(1.47946873082851,0.4811379472619,5.87764001132807));
#264088=CARTESIAN_POINT('Ctrl Pts',(1.48766374394749,0.455168400565725,
5.87574715491127));
#264089=CARTESIAN_POINT('Ctrl Pts',(1.50015101596917,0.411646602599681,
5.87264297777104));
#264090=CARTESIAN_POINT('Ctrl Pts',(1.50482651389881,0.394212137364547,
5.87141730358523));
#264091=CARTESIAN_POINT('Ctrl Pts',(1.53154543901685,0.287166257390051,
5.86397828661293));
#264092=CARTESIAN_POINT('Ctrl Pts',(1.5458827972227,0.195817085607539,5.85798850949133));
#264093=CARTESIAN_POINT('Ctrl Pts',(1.5573077374083,0.0248757706043105,
5.84665639342991));
#264094=CARTESIAN_POINT('Ctrl Pts',(1.55656029097849,-0.0542562838534247,
5.84136217036904));
#264095=CARTESIAN_POINT('Ctrl Pts',(1.54826686664179,-0.15090961124136,
5.83462749312036));
#264096=CARTESIAN_POINT('Ctrl Pts',(1.54641772477851,-0.168808100256128,
5.83336937149769));
#264097=CARTESIAN_POINT('Ctrl Pts',(1.54331944000417,-0.194439195446802,
5.83155011038271));
#264098=CARTESIAN_POINT('Ctrl Pts',(1.54232167966579,-0.202201204307544,
5.83099685184627));
#264099=CARTESIAN_POINT('Ctrl Pts',(1.5404857944463,-0.215678298501292,
5.83003204468773));
#264100=CARTESIAN_POINT('Ctrl Pts',(1.53967432188042,-0.221396911071885,
5.82962134240612));
#264101=CARTESIAN_POINT('Ctrl Pts',(1.53804843607064,-0.232413399560746,
5.82882755777302));
#264102=CARTESIAN_POINT('Ctrl Pts',(1.5372384501844,-0.237711854863806,
5.82844462077677));
#264103=CARTESIAN_POINT('Ctrl Pts',(1.53525481621018,-0.250253347521404,
5.82753539951784));
#264104=CARTESIAN_POINT('Ctrl Pts',(1.5340572803879,-0.257492418735662,
5.82700836638343));
#264105=CARTESIAN_POINT('Ctrl Pts',(1.52964741552402,-0.283026611572056,
5.82514134001439));
#264106=CARTESIAN_POINT('Ctrl Pts',(1.52615876312676,-0.301271725949632,
5.8237926568179));
#264107=CARTESIAN_POINT('Ctrl Pts',(1.49442911492725,-0.452480240343094,
5.81248832210308));
#264108=CARTESIAN_POINT('Ctrl Pts',(1.44920184131936,-0.581252611122845,
5.80196317095399));
#264109=CARTESIAN_POINT('Ctrl Pts',(1.35606506510378,-0.765257459134564,
5.78598902043888));
#264110=CARTESIAN_POINT('Ctrl Pts',(1.32006059964869,-0.825817019634387,
5.78057275089209));
#264111=CARTESIAN_POINT('Ctrl Pts',(1.27290556863947,-0.894120176361791,
5.77442456487));
#264112=CARTESIAN_POINT('Ctrl Pts',(1.26561013835471,-0.904417205465,5.77349669180073));
#264113=CARTESIAN_POINT('Ctrl Pts',(1.25537537470487,-0.918496505518134,
5.77222783054844));
#264114=CARTESIAN_POINT('Ctrl Pts',(1.25254294299408,-0.922355321804584,
5.77188004746141));
#264115=CARTESIAN_POINT('Ctrl Pts',(1.24773172160197,-0.928846944856834,
5.77129503289012));
#264116=CARTESIAN_POINT('Ctrl Pts',(1.24576231985563,-0.931486628583284,
5.77105716456047));
#264117=CARTESIAN_POINT('Ctrl Pts',(1.24199229107978,-0.936506436518979,
5.77060487766612));
#264118=CARTESIAN_POINT('Ctrl Pts',(1.24019318287166,-0.938887653722996,
5.77039035311786));
#264119=CARTESIAN_POINT('Ctrl Pts',(1.23542896114701,-0.945155770959277,
5.7698256763789));
#264120=CARTESIAN_POINT('Ctrl Pts',(1.23245232504911,-0.949033939137008,
5.76947632345311));
#264121=CARTESIAN_POINT('Ctrl Pts',(1.22190000733758,-0.962648852823616,
5.76824967752111));
#264122=CARTESIAN_POINT('Ctrl Pts',(1.21422656757306,-0.972309780703132,
5.76737892765205));
#264123=CARTESIAN_POINT('Ctrl Pts',(1.15549749332188,-1.04447044640089,
5.76086349709704));
#264124=CARTESIAN_POINT('Ctrl Pts',(1.09975471704661,-1.10301238381767,
5.75550833181416));
#264125=CARTESIAN_POINT('Ctrl Pts',(0.989570970483146,-1.20202913052037,
5.74574124376241));
#264126=CARTESIAN_POINT('Ctrl Pts',(0.936555041376363,-1.24378015919661,
5.74132978626769));
#264127=CARTESIAN_POINT('Ctrl Pts',(0.829494637148359,-1.31735507832076,
5.73266781579023));
#264128=CARTESIAN_POINT('Ctrl Pts',(0.775910055300904,-1.34961026548057,
5.72843729011691));
#264129=CARTESIAN_POINT('Ctrl Pts',(0.70640360875591,-1.38593955883786,
5.72297909695103));
#264130=CARTESIAN_POINT('Ctrl Pts',(0.692159447126213,-1.39310795922849,
5.72186221047449));
#264131=CARTESIAN_POINT('Ctrl Pts',(0.671097198446779,-1.40330481053261,
5.72021189349902));
#264132=CARTESIAN_POINT('Ctrl Pts',(0.664363180544266,-1.40650538636429,
5.71968443101563));
#264133=CARTESIAN_POINT('Ctrl Pts',(0.652423961343773,-1.41207504356847,
5.71874943416538));
#264134=CARTESIAN_POINT('Ctrl Pts',(0.64722817615901,-1.4144640823972,5.71834259583911));
#264135=CARTESIAN_POINT('Ctrl Pts',(0.637038654316781,-1.41908135941536,
5.717544796921));
#264136=CARTESIAN_POINT('Ctrl Pts',(0.632046103469724,-1.42131202535296,
5.71715392670268));
#264137=CARTESIAN_POINT('Ctrl Pts',(0.618503453806651,-1.42727740104034,
5.71609367064213));
#264138=CARTESIAN_POINT('Ctrl Pts',(0.609931465069502,-1.43096153084624,
5.71542257495602));
#264139=CARTESIAN_POINT('Ctrl Pts',(0.577396273525147,-1.44459928553603,
5.71287505596254));
#264140=CARTESIAN_POINT('Ctrl Pts',(0.553219699467053,-1.45402935531549,
5.71098119445812));
#264141=CARTESIAN_POINT('Ctrl Pts',(0.52322110508008,-1.46487384033214,
5.70862865841382));
#264142=CARTESIAN_POINT('Ctrl Pts',(0.517610810543786,-1.46686561754613,
5.70818858513641));
#264143=CARTESIAN_POINT('Ctrl Pts',(0.355113580444933,-1.52350737871315,
5.69543903540739));
#264144=CARTESIAN_POINT('Ctrl Pts',(0.190496349643747,-1.55269753174366,
5.682268353988));
#264145=CARTESIAN_POINT('Ctrl Pts',(-0.00876213502222772,-1.55582993524719,
5.66715605219676));
#264146=CARTESIAN_POINT('Ctrl Pts',(-0.0419856252360379,-1.55528813601466,
5.66466988085725));
#264147=CARTESIAN_POINT('Ctrl Pts',(-0.0818324990848134,-1.55336029151481,
5.66174715680883));
#264148=CARTESIAN_POINT('Ctrl Pts',(-0.0884937939355788,-1.5529950437509,
5.66126055016976));
#264149=CARTESIAN_POINT('Ctrl Pts',(-0.0988513779800285,-1.55236026318874,
5.66050723829953));
#264150=CARTESIAN_POINT('Ctrl Pts',(-0.10254929403598,-1.552120364124,5.66023894360849));
#264151=CARTESIAN_POINT('Ctrl Pts',(-0.109420432661839,-1.55164994145406,
5.65974168582727));
#264152=CARTESIAN_POINT('Ctrl Pts',(-0.112593777416775,-1.5514228996353,
5.65951254022215));
#264153=CARTESIAN_POINT('Ctrl Pts',(-0.119825869056215,-1.55088316174212,
5.65899144845466));
#264154=CARTESIAN_POINT('Ctrl Pts',(-0.123884097077734,-1.55056426883275,
5.65869985155167));
#264155=CARTESIAN_POINT('Ctrl Pts',(-0.134466409555283,-1.54969090612779,
5.65794147919158));
#264156=CARTESIAN_POINT('Ctrl Pts',(-0.140988417253301,-1.54911116129101,
5.65747607052642));
#264157=CARTESIAN_POINT('Ctrl Pts',(-0.184899658410045,-1.54492824617979,
5.65435476902267));
#264158=CARTESIAN_POINT('Ctrl Pts',(-0.222155199826792,-1.54001260163709,
5.65176609003573));
#264159=CARTESIAN_POINT('Ctrl Pts',(-0.391195909823523,-1.51144519651127,
5.64014255456864));
#264160=CARTESIAN_POINT('Ctrl Pts',(-0.519765890991624,-1.47219211228039,
5.63159716724919));
#264161=CARTESIAN_POINT('Ctrl Pts',(-0.674428952727528,-1.40214638010192,
5.62017948898414));
#264162=CARTESIAN_POINT('Ctrl Pts',(-0.7066046586172,-1.38621010063511,
5.6177396996839));
#264163=CARTESIAN_POINT('Ctrl Pts',(-0.759285193505354,-1.3578071077113,
5.61361176207627));
#264164=CARTESIAN_POINT('Ctrl Pts',(-0.780105265922131,-1.34595312433692,
5.61194415670442));
#264165=CARTESIAN_POINT('Ctrl Pts',(-0.808149145782261,-1.32911695124852,
5.60964355769668));
#264166=CARTESIAN_POINT('Ctrl Pts',(-0.815617590338711,-1.32454703677803,
5.60902549188111));
#264167=CARTESIAN_POINT('Ctrl Pts',(-0.82809905274682,-1.31676408567938,
5.60798325730435));
#264168=CARTESIAN_POINT('Ctrl Pts',(-0.833132990323881,-1.31358483438699,
5.60756033558916));
#264169=CARTESIAN_POINT('Ctrl Pts',(-0.843029163522539,-1.30725500421949,
5.6067237496953));
#264170=CARTESIAN_POINT('Ctrl Pts',(-0.847892297447702,-1.30410600292387,
5.60631014902021));
#264171=CARTESIAN_POINT('Ctrl Pts',(-0.858557168427101,-1.29711535964268,
5.60539755846031));
#264172=CARTESIAN_POINT('Ctrl Pts',(-0.864350920414028,-1.2932618262127,
5.60489812922958));
#264173=CARTESIAN_POINT('Ctrl Pts',(-0.88458334349444,-1.27960817232303,
5.60314101875784));
#264174=CARTESIAN_POINT('Ctrl Pts',(-0.898882291490211,-1.26960440539808,
5.60187568824488));
#264175=CARTESIAN_POINT('Ctrl Pts',(-1.02117629704056,-1.18094401615705,
5.59084334430135));
#264176=CARTESIAN_POINT('Ctrl Pts',(-1.11876750765334,-1.08893218909319,
5.58052442856601));
#264177=CARTESIAN_POINT('Ctrl Pts',(-1.25053687268821,-0.92804920404406,
5.56440632368165));
#264178=CARTESIAN_POINT('Ctrl Pts',(-1.29350224133291,-0.86716335104238,
5.5586654505749));
#264179=CARTESIAN_POINT('Ctrl Pts',(-1.338640577178,-0.792331752790214,
5.55218852672417));
#264180=CARTESIAN_POINT('Ctrl Pts',(-1.34519567651387,-0.78115096032571,
5.55123521126765));
#264181=CARTESIAN_POINT('Ctrl Pts',(-1.35400462724587,-0.765686042958562,
5.54993760172661));
#264182=CARTESIAN_POINT('Ctrl Pts',(-1.35637912969309,-0.761471801979394,
5.5495861124621));
#264183=CARTESIAN_POINT('Ctrl Pts',(-1.36034220414077,-0.754360822834889,
5.54899665487783));
#264184=CARTESIAN_POINT('Ctrl Pts',(-1.36194125923689,-0.751470006381479,
5.5487580282248));
#264185=CARTESIAN_POINT('Ctrl Pts',(-1.36496280836634,-0.745966240713117,
5.54830564895086));
#264186=CARTESIAN_POINT('Ctrl Pts',(-1.36638702998467,-0.743354279737981,
5.54809178376104));
#264187=CARTESIAN_POINT('Ctrl Pts',(-1.3701076083442,-0.736484077874733,
5.54753137357699));
#264188=CARTESIAN_POINT('Ctrl Pts',(-1.3723916330671,-0.732219135625162,
5.54718560497088));
#264189=CARTESIAN_POINT('Ctrl Pts',(-1.38028903064516,-0.717305611915265,
5.54598368591826));
#264190=CARTESIAN_POINT('Ctrl Pts',(-1.38579885374374,-0.70660222864203,
5.54513373818601));
#264191=CARTESIAN_POINT('Ctrl Pts',(-1.43514813428337,-0.607938203977148,
5.53740421887553));
#264192=CARTESIAN_POINT('Ctrl Pts',(-1.47069023433529,-0.516057534786653,
5.53095906933564));
#264193=CARTESIAN_POINT('Ctrl Pts',(-1.52907535595516,-0.308614489205268,
5.51677667812562));
#264194=CARTESIAN_POINT('Ctrl Pts',(-1.54797135539625,-0.192596692072913,
5.50905452405191));
#264195=CARTESIAN_POINT('Ctrl Pts',(-1.5543052043772,-0.0623707568372182,
5.49994839313294));
#264196=CARTESIAN_POINT('Ctrl Pts',(-1.55477884503724,-0.049168117372399,
5.4990207193885));
#264197=CARTESIAN_POINT('Ctrl Pts',(-1.55524412947786,-0.0290477502464651,
5.49759945213287));
#264198=CARTESIAN_POINT('Ctrl Pts',(-1.55535789835207,-0.0221332172942355,
5.49710967003003));
#264199=CARTESIAN_POINT('Ctrl Pts',(-1.55547562514631,-0.0101006118354341,
5.49625490273249));
#264200=CARTESIAN_POINT('Ctrl Pts',(-1.55550043820327,-0.00498280903079771,
5.49589057438442));
#264201=CARTESIAN_POINT('Ctrl Pts',(-1.55549944070673,0.00651333868513192,
5.49507039971071));
#264202=CARTESIAN_POINT('Ctrl Pts',(-1.55545965525977,0.0128915569025155,
5.49461412335422));
#264203=CARTESIAN_POINT('Ctrl Pts',(-1.55524796979287,0.029978431198106,
5.49338838448767));
#264204=CARTESIAN_POINT('Ctrl Pts',(-1.5550047003345,0.0406856873065747,
5.49261671029927));
#264205=CARTESIAN_POINT('Ctrl Pts',(-1.5532456061059,0.0939025174494717,
5.48876282624848));
#264206=CARTESIAN_POINT('Ctrl Pts',(-1.55009723945784,0.13633596400759,
5.48563029389698));
#264207=CARTESIAN_POINT('Ctrl Pts',(-1.52691884218012,0.336889722907466,
5.47052607851178));
#264208=CARTESIAN_POINT('Ctrl Pts',(-1.48441224788886,0.491407369625553,
5.45787219155486));
#264209=CARTESIAN_POINT('Ctrl Pts',(-1.40823479323957,0.661189805556878,
5.44383764123695));
#264210=CARTESIAN_POINT('Ctrl Pts',(-1.39664399424696,0.685334206331063,
5.44184206252578));
#264211=CARTESIAN_POINT('Ctrl Pts',(-1.38147966816369,0.714937890392895,
5.43940584921647));
#264212=CARTESIAN_POINT('Ctrl Pts',(-1.37848855595424,0.720688258359481,
5.43893313586419));
#264213=CARTESIAN_POINT('Ctrl Pts',(-1.37373225928131,0.729694210803432,
5.43819379019823));
#264214=CARTESIAN_POINT('Ctrl Pts',(-1.3719912905888,0.732962387027253,
5.43792569601348));
#264215=CARTESIAN_POINT('Ctrl Pts',(-1.36873267570472,0.739027223064927,
5.43742861652167));
#264216=CARTESIAN_POINT('Ctrl Pts',(-1.36721813286294,0.741825418456715,
5.43719944991717));
#264217=CARTESIAN_POINT('Ctrl Pts',(-1.36374449084891,0.748196374914809,
5.43667806259875));
#264218=CARTESIAN_POINT('Ctrl Pts',(-1.36177993410677,0.751766096497224,
5.43638619272176));
#264219=CARTESIAN_POINT('Ctrl Pts',(-1.35569526299095,0.762720202165408,
5.4354912558632));
#264220=CARTESIAN_POINT('Ctrl Pts',(-1.35152885188499,0.770078907600953,
5.43489104086439));
#264221=CARTESIAN_POINT('Ctrl Pts',(-1.34170198202646,0.787109660189673,
5.43350333120464));
#264222=CARTESIAN_POINT('Ctrl Pts',(-1.33599652822017,0.79675537022244,
5.43271844246537));
#264223=CARTESIAN_POINT('Ctrl Pts',(-1.31588020877409,0.829940509631854,
5.43001877061165));
#264224=CARTESIAN_POINT('Ctrl Pts',(-1.30094669851466,0.853158756935452,
5.42813106263847));
#264225=CARTESIAN_POINT('Ctrl Pts',(-1.20865960042166,0.988581441625445,
5.41705054041824));
#264226=CARTESIAN_POINT('Ctrl Pts',(-1.11744993954983,1.09062446694038,
5.40835566747347));
#264227=CARTESIAN_POINT('Ctrl Pts',(-0.977262860678338,1.21115569376459,
5.39587975576391));
#264228=CARTESIAN_POINT('Ctrl Pts',(-0.938961870076119,1.24108445488677,
5.39255089490556));
#264229=CARTESIAN_POINT('Ctrl Pts',(-0.889937014517213,1.27582317964514,
5.38834499465083));
#264230=CARTESIAN_POINT('Ctrl Pts',(-0.880474350500349,1.282371857557,5.38753565908545));
#264231=CARTESIAN_POINT('Ctrl Pts',(-0.865453774515862,1.29252228595158,
5.38625435279685));
#264232=CARTESIAN_POINT('Ctrl Pts',(-0.859943891123002,1.29619466021367,
5.38578504985767));
#264233=CARTESIAN_POINT('Ctrl Pts',(-0.849724527981963,1.30291209473848,
5.38491582838685));
#264234=CARTESIAN_POINT('Ctrl Pts',(-0.845021684222362,1.30596709443694,
5.38451628993596));
#264235=CARTESIAN_POINT('Ctrl Pts',(-0.834553409773153,1.31268714034153,
5.38362791242899));
#264236=CARTESIAN_POINT('Ctrl Pts',(-0.828780175938554,1.31633975074721,
5.38313862267693));
#264237=CARTESIAN_POINT('Ctrl Pts',(-0.812113376640613,1.32673139574289,
5.38172781738645));
#264238=CARTESIAN_POINT('Ctrl Pts',(-0.801160612843261,1.33337391122609,
5.38080279354729));
#264239=CARTESIAN_POINT('Ctrl Pts',(-0.71317080460275,1.38526150080613,
5.37338631186429));
#264240=CARTESIAN_POINT('Ctrl Pts',(-0.632462609298558,1.42391980058423,
5.3666581715158));
#264241=CARTESIAN_POINT('Ctrl Pts',(-0.459368629489077,1.48919986369108,
5.35242585160925));
#264242=CARTESIAN_POINT('Ctrl Pts',(-0.36691683939528,1.51463122860939,
5.34492977670614));
#264243=CARTESIAN_POINT('Ctrl Pts',(-0.234905577203705,1.53813994148863,
5.33471467655072));
#264244=CARTESIAN_POINT('Ctrl Pts',(-0.196856071665377,1.54347121938797,
5.33182783774703));
#264245=CARTESIAN_POINT('Ctrl Pts',(-0.152090523920295,1.5480607640834,
5.32852625739485));
#264246=CARTESIAN_POINT('Ctrl Pts',(-0.145532139610621,1.54869107868809,
5.32804493713997));
#264247=CARTESIAN_POINT('Ctrl Pts',(-0.134903172230235,1.54964449297277,
5.32726893519353));
#264248=CARTESIAN_POINT('Ctrl Pts',(-0.130835066101718,1.54999326030462,
5.32697289176202));
#264249=CARTESIAN_POINT('Ctrl Pts',(-0.123593649868051,1.55058536948606,
5.3264476868671));
#264250=CARTESIAN_POINT('Ctrl Pts',(-0.120420926686394,1.55083499427229,
5.32621818161246));
#264251=CARTESIAN_POINT('Ctrl Pts',(-0.113560861469582,1.55135355374082,
5.32572326280352));
#264252=CARTESIAN_POINT('Ctrl Pts',(-0.109873324350047,1.55161908061548,
5.32545804116904));
#264253=CARTESIAN_POINT('Ctrl Pts',(-0.0995688161021603,1.5523241534375,
5.3247190905951));
#264254=CARTESIAN_POINT('Ctrl Pts',(-0.0929498230270874,1.55273454302193,
5.32424695333003));
#264255=CARTESIAN_POINT('Ctrl Pts',(-0.053861911191322,1.55490722049207,
5.32147257228365));
#264256=CARTESIAN_POINT('Ctrl Pts',(-0.02134391341106,1.55569354281076,
5.31922059879102));
#264257=CARTESIAN_POINT('Ctrl Pts',(0.165266267824599,1.5543525388127,5.30649548754598));
#264258=CARTESIAN_POINT('Ctrl Pts',(0.318342429843081,1.53035681546692,
5.29674899074108));
#264259=CARTESIAN_POINT('Ctrl Pts',(0.504687949867082,1.47192569638736,
5.2834961145528));
#264260=CARTESIAN_POINT('Ctrl Pts',(0.543463772375996,1.45805411647056,
5.2806632859163));
#264261=CARTESIAN_POINT('Ctrl Pts',(0.591797969527179,1.43856711438559,
5.27701219482872));
#264262=CARTESIAN_POINT('Ctrl Pts',(0.601911013982638,1.4343651207774,5.27624150181153));
#264263=CARTESIAN_POINT('Ctrl Pts',(0.61794896698783,1.42750183782438,5.27500804314016));
#264264=CARTESIAN_POINT('Ctrl Pts',(0.623903170190132,1.42490956018206,
5.27454762081009));
#264265=CARTESIAN_POINT('Ctrl Pts',(0.635026300503056,1.4199838059676,5.27368272997243));
#264266=CARTESIAN_POINT('Ctrl Pts',(0.640199055061689,1.41765919031144,
5.27327856989081));
#264267=CARTESIAN_POINT('Ctrl Pts',(0.651743242714566,1.41239521027049,
5.27237216394042));
#264268=CARTESIAN_POINT('Ctrl Pts',(0.658107696066416,1.40944093235926,
5.27186941199308));
#264269=CARTESIAN_POINT('Ctrl Pts',(0.676841997207182,1.40059021144632,
5.27038037702634));
#264270=CARTESIAN_POINT('Ctrl Pts',(0.689153872910023,1.39457339236177,
5.26938995481999));
#264271=CARTESIAN_POINT('Ctrl Pts',(0.798461747688608,1.33935363625879,
5.26048765781328));
#264272=CARTESIAN_POINT('Ctrl Pts',(0.890107321274177,1.2802768811826,5.25221726769949));
#264273=CARTESIAN_POINT('Ctrl Pts',(1.05773847899523,1.1454648875892,5.23556725138612));
#264274=CARTESIAN_POINT('Ctrl Pts',(1.1335961695884,1.07045045700489,5.22724289133022));
#264275=CARTESIAN_POINT('Ctrl Pts',(1.20862984886372,0.979250053559702,
5.21850438455071));
#264276=CARTESIAN_POINT('Ctrl Pts',(1.21595192674479,0.970143140305076,
5.21764575323557));
#264277=CARTESIAN_POINT('Ctrl Pts',(1.22612325787585,0.957196345648021,
5.21644558075253));
#264278=CARTESIAN_POINT('Ctrl Pts',(1.22905826174672,0.953424815332332,
5.21609837002398));
#264279=CARTESIAN_POINT('Ctrl Pts',(1.2339655426084,0.947058557291241,5.21551641121575));
#264280=CARTESIAN_POINT('Ctrl Pts',(1.23594711074264,0.944471074958277,
5.21528101827747));
#264281=CARTESIAN_POINT('Ctrl Pts',(1.23996884025106,0.939185268137,5.21480249108676));
#264282=CARTESIAN_POINT('Ctrl Pts',(1.24200835466986,0.936486486932858,
5.21455940195158));
#264283=CARTESIAN_POINT('Ctrl Pts',(1.24716584365623,0.929615370937746,
5.21394355765565));
#264284=CARTESIAN_POINT('Ctrl Pts',(1.25027172890505,0.925433944402657,
5.21357163640402));
#264285=CARTESIAN_POINT('Ctrl Pts',(1.26266356395552,0.908574667351218,
5.21208312612106));
#264286=CARTESIAN_POINT('Ctrl Pts',(1.27177857845415,0.895771455267055,
5.21097768334453));
#264287=CARTESIAN_POINT('Ctrl Pts',(1.29510390025228,0.861934082654363,
5.20811430674465));
#264288=CARTESIAN_POINT('Ctrl Pts',(1.30899663067788,0.840685708132529,
5.20637362846489));
#264289=CARTESIAN_POINT('Ctrl Pts',(1.36545653188261,0.749536845693514,
5.19910236539426));
#264290=CARTESIAN_POINT('Ctrl Pts',(1.40297178841824,0.676708759370786,
5.19376122252171));
#264291=CARTESIAN_POINT('Ctrl Pts',(1.43457674133486,0.601306762992946,
5.18837549714138));
#264292=CARTESIAN_POINT('',(-1.55596208451267,0.00138090387652695,5.3559437743963));
#264293=CARTESIAN_POINT('Ctrl Pts',(1.43231908414271,0.600352779935808,
5.05019128547067));
#264294=CARTESIAN_POINT('Ctrl Pts',(1.32160532361985,0.862577042890051,
5.07050276174236));
#264295=CARTESIAN_POINT('Ctrl Pts',(0.815607745123861,1.52283096854995,
5.12785138087118));
#264296=CARTESIAN_POINT('Ctrl Pts',(-0.66589513819016,1.71353370282299,
5.22223714285715));
#264297=CARTESIAN_POINT('Ctrl Pts',(-1.4993495737318,0.726990709360215,
5.30384316289402));
#264298=CARTESIAN_POINT('Ctrl Pts',(-1.55692912760588,0.106428400307349,
5.34841204007373));
#264299=CARTESIAN_POINT('Ctrl Pts',(-1.55596208451267,0.00138090387652695,
5.3559437743963));
#264300=CARTESIAN_POINT('Ctrl Pts',(-1.5554993720197,0.00139772898855563,
5.35620969761336));
#264301=CARTESIAN_POINT('Ctrl Pts',(-1.55560008096552,-0.110678863304792,
5.36359495551528));
#264302=CARTESIAN_POINT('Ctrl Pts',(-1.54358838605568,-0.222430311866365,
5.37091855286445));
#264303=CARTESIAN_POINT('Ctrl Pts',(-1.51593216532635,-0.349052143694656,
5.37983742834118));
#264304=CARTESIAN_POINT('Ctrl Pts',(-1.51190115728801,-0.366118257267673,
5.38105217793184));
#264305=CARTESIAN_POINT('Ctrl Pts',(-1.50518211486557,-0.392558335020044,
5.38295601981498));
#264306=CARTESIAN_POINT('Ctrl Pts',(-1.50269290442263,-0.401981682143839,
5.38363891226452));
#264307=CARTESIAN_POINT('Ctrl Pts',(-1.49837405339774,-0.417730531464308,
5.38478784617263));
#264308=CARTESIAN_POINT('Ctrl Pts',(-1.49659248347777,-0.424069023660975,
5.38525234836641));
#264309=CARTESIAN_POINT('Ctrl Pts',(-1.4930045361474,-0.436530012191539,
5.38616974755778));
#264310=CARTESIAN_POINT('Ctrl Pts',(-1.49120060468622,-0.442653081857937,
5.38662255778795));
#264311=CARTESIAN_POINT('Ctrl Pts',(-1.4876929703892,-0.454294206575662,
5.38748737435947));
#264312=CARTESIAN_POINT('Ctrl Pts',(-1.48599612138359,-0.459814229721807,
5.38789915097486));
#264313=CARTESIAN_POINT('Ctrl Pts',(-1.48204883040551,-0.47240509624171,
5.38884233841758));
#264314=CARTESIAN_POINT('Ctrl Pts',(-1.47977846693024,-0.479469494273115,
5.38937439355564));
#264315=CARTESIAN_POINT('Ctrl Pts',(-1.47371965499815,-0.497868919860951,
5.39076776819668));
#264316=CARTESIAN_POINT('Ctrl Pts',(-1.46985102681954,-0.509176813133323,
5.39163170128635));
#264317=CARTESIAN_POINT('Ctrl Pts',(-1.43071575014064,-0.619404096999735,
5.40012957990073));
#264318=CARTESIAN_POINT('Ctrl Pts',(-1.3856547099048,-0.714535842966949,
5.40809739847534));
#264319=CARTESIAN_POINT('Ctrl Pts',(-1.29946391861826,-0.857193203136812,
5.4209844183645));
#264320=CARTESIAN_POINT('Ctrl Pts',(-1.26444586653384,-0.908054745038845,
5.42578839805882));
#264321=CARTESIAN_POINT('Ctrl Pts',(-1.20330473306388,-0.986438128405728,
5.43343549883851));
#264322=CARTESIAN_POINT('Ctrl Pts',(-1.1790344887421,-1.01532288560463,
5.43631180977595));
#264323=CARTESIAN_POINT('Ctrl Pts',(-1.13985601310225,-1.05864857444442,
5.44068672169018));
#264324=CARTESIAN_POINT('Ctrl Pts',(-1.12566964056317,-1.07372087017383,
5.44222077248859));
#264325=CARTESIAN_POINT('Ctrl Pts',(-1.10716166983749,-1.09261445886645,
5.44415454710481));
#264326=CARTESIAN_POINT('Ctrl Pts',(-1.10311471663873,-1.09670016121536,
5.44457338548001));
#264327=CARTESIAN_POINT('Ctrl Pts',(-1.09688818726383,-1.10291697094071,
5.44521157948093));
#264328=CARTESIAN_POINT('Ctrl Pts',(-1.09472491065436,-1.10506421106432,
5.44543217107678));
#264329=CARTESIAN_POINT('Ctrl Pts',(-1.09026344195423,-1.10946664861493,
5.44588475691598));
#264330=CARTESIAN_POINT('Ctrl Pts',(-1.08796458636857,-1.11172104253873,
5.4461166809356));
#264331=CARTESIAN_POINT('Ctrl Pts',(-1.08272857119958,-1.11682399298928,
5.44664204814988));
#264332=CARTESIAN_POINT('Ctrl Pts',(-1.07978716487821,-1.11966810698839,
5.44693514648195));
#264333=CARTESIAN_POINT('Ctrl Pts',(-1.07212295850001,-1.1270205145044,
5.44769370277198));
#264334=CARTESIAN_POINT('Ctrl Pts',(-1.06738287120381,-1.1315107991009,
5.44815781635469));
#264335=CARTESIAN_POINT('Ctrl Pts',(-1.0362445132388,-1.16063836124619,
5.45117513167626));
#264336=CARTESIAN_POINT('Ctrl Pts',(-1.00902089527395,-1.18438230583711,
5.45366643288268));
#264337=CARTESIAN_POINT('Ctrl Pts',(-0.903616925325389,-1.27003839080889,
5.4628879131404));
#264338=CARTESIAN_POINT('Ctrl Pts',(-0.820369091235699,-1.32533724535424,
5.46934827738685));
#264339=CARTESIAN_POINT('Ctrl Pts',(-0.680639846534117,-1.39991112836339,
5.4798238499985));
#264340=CARTESIAN_POINT('Ctrl Pts',(-0.627368189042677,-1.42458063477618,
5.48373908755192));
#264341=CARTESIAN_POINT('Ctrl Pts',(-0.541301285447167,-1.45867182259952,
5.49006298510955));
#264342=CARTESIAN_POINT('Ctrl Pts',(-0.509370679774071,-1.47012645220616,
5.49240826590177));
#264343=CARTESIAN_POINT('Ctrl Pts',(-0.467890339048307,-1.48349329864626,
5.49546655712975));
#264344=CARTESIAN_POINT('Ctrl Pts',(-0.458660256851397,-1.48637293361412,
5.49614778182696));
#264345=CARTESIAN_POINT('Ctrl Pts',(-0.44329539777211,-1.49100977702656,
5.49728323622555));
#264346=CARTESIAN_POINT('Ctrl Pts',(-0.437175483210059,-1.49281564821363,
5.49773587425982));
#264347=CARTESIAN_POINT('Ctrl Pts',(-0.425495351505285,-1.49618425093073,
5.49860056120874));
#264348=CARTESIAN_POINT('Ctrl Pts',(-0.419937189310278,-1.49775377224279,
5.49901238154789));
#264349=CARTESIAN_POINT('Ctrl Pts',(-0.407213825088192,-1.50127022239679,
5.49995595064675));
#264350=CARTESIAN_POINT('Ctrl Pts',(-0.400043213580722,-1.50319686126834,
5.50048834559686));
#264351=CARTESIAN_POINT('Ctrl Pts',(-0.381280279539176,-1.50809442823809,
5.50188319398329));
#264352=CARTESIAN_POINT('Ctrl Pts',(-0.369667179995152,-1.5109829969951,
5.50274827004915));
#264353=CARTESIAN_POINT('Ctrl Pts',(-0.257367010087211,-1.53754371967827,
5.51113228396625));
#264354=CARTESIAN_POINT('Ctrl Pts',(-0.15460955814862,-1.5512466469733,
5.51897438915023));
#264355=CARTESIAN_POINT('Ctrl Pts',(0.0337023303501034,-1.55745725200963,
5.53353688051234));
#264356=CARTESIAN_POINT('Ctrl Pts',(0.118766336248085,-1.55328824256979,
5.54017788768958));
#264357=CARTESIAN_POINT('Ctrl Pts',(0.237667903967209,-1.53763204424795,
5.54928528431979));
#264358=CARTESIAN_POINT('Ctrl Pts',(0.272110665054296,-1.53191207206746,
5.55190087127096));
#264359=CARTESIAN_POINT('Ctrl Pts',(0.313022189079387,-1.52369415666191,
5.55495900003768));
#264360=CARTESIAN_POINT('Ctrl Pts',(0.319700713136032,-1.52230687856444,
5.5554566467108));
#264361=CARTESIAN_POINT('Ctrl Pts',(0.330052900554546,-1.52008536627153,
5.55622536916249));
#264362=CARTESIAN_POINT('Ctrl Pts',(0.333732912440647,-1.51928166640972,
5.55649811147286));
#264363=CARTESIAN_POINT('Ctrl Pts',(0.34055438795616,-1.51776590225812,
5.55700266307007));
#264364=CARTESIAN_POINT('Ctrl Pts',(0.343696534133728,-1.51705745375395,
5.55723466527917));
#264365=CARTESIAN_POINT('Ctrl Pts',(0.350841000766122,-1.51542327972931,
5.55776127428947));
#264366=CARTESIAN_POINT('Ctrl Pts',(0.354841866555703,-1.51449145766812,
5.55805552944753));
#264367=CARTESIAN_POINT('Ctrl Pts',(0.365244785517725,-1.51202507799577,
5.55881907974442));
#264368=CARTESIAN_POINT('Ctrl Pts',(0.371640959276129,-1.51046568689452,
5.55928700114717));
#264369=CARTESIAN_POINT('Ctrl Pts',(0.414111780358202,-1.49982516061323,
5.56238493240159));
#264370=CARTESIAN_POINT('Ctrl Pts',(0.449864175281268,-1.48949214936153,
5.5649491993143));
#264371=CARTESIAN_POINT('Ctrl Pts',(0.626308820930151,-1.43156237469475,
5.57754451570754));
#264372=CARTESIAN_POINT('Ctrl Pts',(0.760046158775416,-1.36527287940747,
5.58697157107993));
#264373=CARTESIAN_POINT('Ctrl Pts',(0.904919711866183,-1.26548438444147,
5.59891337837999));
#264374=CARTESIAN_POINT('Ctrl Pts',(0.92706035373409,-1.24935558150297,
5.60078995742166));
#264375=CARTESIAN_POINT('Ctrl Pts',(0.964273401359281,-1.22071297504079,
5.60404411337837));
#264376=CARTESIAN_POINT('Ctrl Pts',(0.979556766843766,-1.20848328107542,
5.60541097795788));
#264377=CARTESIAN_POINT('Ctrl Pts',(1.00087363731089,-1.19075551272447,
5.60736348297189));
#264378=CARTESIAN_POINT('Ctrl Pts',(1.0071013489349,-1.1854929765185,5.60793962953443));
#264379=CARTESIAN_POINT('Ctrl Pts',(1.01775605099478,-1.17634500107702,
5.60893542568157));
#264380=CARTESIAN_POINT('Ctrl Pts',(1.02220292202003,-1.17248288915765,
5.60935411215551));
#264381=CARTESIAN_POINT('Ctrl Pts',(1.03066809774478,-1.16504611343838,
5.61015711698945));
#264382=CARTESIAN_POINT('Ctrl Pts',(1.03469001598894,-1.16147567500198,
5.61054125578786));
#264383=CARTESIAN_POINT('Ctrl Pts',(1.04407511456429,-1.15305666689221,
5.61144386434116));
#264384=CARTESIAN_POINT('Ctrl Pts',(1.04942312719099,-1.14819145562112,
5.61196302930434));
#264385=CARTESIAN_POINT('Ctrl Pts',(1.06769778090363,-1.13133224605936,
5.61375391933813));
#264386=CARTESIAN_POINT('Ctrl Pts',(1.08045383737794,-1.1191562268552,5.61503335872999));
#264387=CARTESIAN_POINT('Ctrl Pts',(1.1844558585827,-1.01644785851733,5.62571641954513));
#264388=CARTESIAN_POINT('Ctrl Pts',(1.26434595302489,-0.915159639529413,
5.63562496555821));
#264389=CARTESIAN_POINT('Ctrl Pts',(1.37123089292751,-0.73850445279877,
5.65163257242835));
#264390=CARTESIAN_POINT('Ctrl Pts',(1.40653370284033,-0.668826317083173,
5.65766084437124));
#264391=CARTESIAN_POINT('Ctrl Pts',(1.44156922136692,-0.584495995090591,
5.66443251661433));
#264392=CARTESIAN_POINT('Ctrl Pts',(1.4465177870522,-0.572139591269316,
5.66541195377123));
#264393=CARTESIAN_POINT('Ctrl Pts',(1.45307946601034,-0.55512572373256,
5.66674172138828));
#264394=CARTESIAN_POINT('Ctrl Pts',(1.45482977518503,-0.550522325348872,
5.66709963914956));
#264395=CARTESIAN_POINT('Ctrl Pts',(1.45773423973904,-0.542772848290416,
5.66769893223863));
#264396=CARTESIAN_POINT('Ctrl Pts',(1.45890013233382,-0.539631247376007,
5.66794099318638));
#264397=CARTESIAN_POINT('Ctrl Pts',(1.46109388075835,-0.533660921638923,
5.66839928900607));
#264398=CARTESIAN_POINT('Ctrl Pts',(1.46212369030483,-0.530832951450371,
5.6686156421557));
#264399=CARTESIAN_POINT('Ctrl Pts',(1.46480244351849,-0.523409863400469,
5.66918168088108));
#264400=CARTESIAN_POINT('Ctrl Pts',(1.46643799155516,-0.51880989031911,
5.6695305790947));
#264401=CARTESIAN_POINT('Ctrl Pts',(1.47204851976286,-0.502791782365244,
5.67073929244131));
#264402=CARTESIAN_POINT('Ctrl Pts',(1.47591215050701,-0.49133468100059,
5.6715928711729));
#264403=CARTESIAN_POINT('Ctrl Pts',(1.50981852203538,-0.386779001030871,
5.67929331027264));
#264404=CARTESIAN_POINT('Ctrl Pts',(1.53115450803153,-0.291070212453557,
5.68571083158051));
#264405=CARTESIAN_POINT('Ctrl Pts',(1.55755952524534,-0.080982927464409,
5.69964733234562));
#264406=CARTESIAN_POINT('Ctrl Pts',(1.55930812127068,0.0332129866934599,
5.70714925867247));
#264407=CARTESIAN_POINT('Ctrl Pts',(1.54712797524903,0.161902788200686,
5.71615158635484));
#264408=CARTESIAN_POINT('Ctrl Pts',(1.54544903856824,0.177213780866496,
5.71723092341854));
#264409=CARTESIAN_POINT('Ctrl Pts',(1.54262628416476,0.199848140760663,
5.71883993188617));
#264410=CARTESIAN_POINT('Ctrl Pts',(1.54165700654947,0.207192670463991,
5.71936412982183));
#264411=CARTESIAN_POINT('Ctrl Pts',(1.53983905227946,0.220248215519711,
5.72029980260937));
#264412=CARTESIAN_POINT('Ctrl Pts',(1.53901096706326,0.22596199897237,5.72071062205208));
#264413=CARTESIAN_POINT('Ctrl Pts',(1.53719943496688,0.237989444999662,
5.72157824138033));
#264414=CARTESIAN_POINT('Ctrl Pts',(1.53620885773022,0.244301907434522,
5.72203525921971));
#264415=CARTESIAN_POINT('Ctrl Pts',(1.53348304950316,0.260999717136409,
5.72324866261563));
#264416=CARTESIAN_POINT('Ctrl Pts',(1.5316812403549,0.271373696731041,5.72400713829426));
#264417=CARTESIAN_POINT('Ctrl Pts',(1.52344421706974,0.31610042155577,5.72729782624887));
#264418=CARTESIAN_POINT('Ctrl Pts',(1.51595801684094,0.350246609163335,
5.729862966271));
#264419=CARTESIAN_POINT('Ctrl Pts',(1.4884278583792,0.458280961304234,5.73815604510771));
#264420=CARTESIAN_POINT('Ctrl Pts',(1.46409864409644,0.530874509686054,
5.74400369568442));
#264421=CARTESIAN_POINT('Ctrl Pts',(1.43457651448711,0.601307304198132,
5.74991065382822));
#264422=CARTESIAN_POINT('Origin',(0.,0.,-1.29405622560371));
#264423=CARTESIAN_POINT('',(1.43315705713265,0.600696421508096,6.58835745434585));
#264424=CARTESIAN_POINT('',(1.43457668334549,0.60130690134194,6.45155991302018));
#264425=CARTESIAN_POINT('',(1.43457668357355,0.601306900797845,-1.29405622560371));
#264426=CARTESIAN_POINT('',(-1.55592048424612,-0.00138931664391115,6.1940562256037));
#264427=CARTESIAN_POINT('Ctrl Pts',(-1.55592048424612,-0.00138931664391115,
6.1940562256037));
#264428=CARTESIAN_POINT('Ctrl Pts',(-1.55690316545381,-0.107885618591398,
6.20169131463905));
#264429=CARTESIAN_POINT('Ctrl Pts',(-1.49836903718625,-0.730118810983662,
6.24637833226625));
#264430=CARTESIAN_POINT('Ctrl Pts',(-0.660529380526586,-1.71587418409115,
6.32811727848531));
#264431=CARTESIAN_POINT('Ctrl Pts',(1.08360676610026,-1.48536852485539,
6.43927306426084));
#264432=CARTESIAN_POINT('Ctrl Pts',(1.67047740112632,-0.244146230934245,
6.5260197895477));
#264433=CARTESIAN_POINT('Ctrl Pts',(1.50279954967853,0.438061975745323,
6.57571458624271));
#264434=CARTESIAN_POINT('Ctrl Pts',(1.43315705713258,0.600696421508238,
6.58835745434586));
#264435=CARTESIAN_POINT('Ctrl Pts',(-1.55549936581116,-0.0014046213329422,
6.19381419951655));
#264436=CARTESIAN_POINT('Ctrl Pts',(-1.55559995768813,0.109992377391697,
6.18647623964182));
#264437=CARTESIAN_POINT('Ctrl Pts',(-1.5437345883581,0.221069845459952,
6.1791922833572));
#264438=CARTESIAN_POINT('Ctrl Pts',(-1.51645035231152,0.346779410486837,
6.17033606758573));
#264439=CARTESIAN_POINT('Ctrl Pts',(-1.51251281990397,0.36356919682226,
6.16914097311621));
#264440=CARTESIAN_POINT('Ctrl Pts',(-1.50595038895181,0.389596986829181,
6.16726719245273));
#264441=CARTESIAN_POINT('Ctrl Pts',(-1.50351762436012,0.398882353793074,
6.1665945059703));
#264442=CARTESIAN_POINT('Ctrl Pts',(-1.49929592233644,0.414408159240896,
6.16546232485091));
#264443=CARTESIAN_POINT('Ctrl Pts',(-1.49755355186387,0.420661077583915,
6.1650043224194));
#264444=CARTESIAN_POINT('Ctrl Pts',(-1.49404420316901,0.432957051387873,
6.16409959416163));
#264445=CARTESIAN_POINT('Ctrl Pts',(-1.49227957028254,0.439000650760043,
6.16365295158166));
#264446=CARTESIAN_POINT('Ctrl Pts',(-1.48884660487773,0.45049812884336,
6.16279942718374));
#264447=CARTESIAN_POINT('Ctrl Pts',(-1.48718486789767,0.455953883688627,
6.16239276649154));
#264448=CARTESIAN_POINT('Ctrl Pts',(-1.48331670470011,0.46840755989857,
6.16146065461254));
#264449=CARTESIAN_POINT('Ctrl Pts',(-1.48109070555724,0.475399208145836,
6.16093457016266));
#264450=CARTESIAN_POINT('Ctrl Pts',(-1.47514528317225,0.493626078830945,
6.1595556612995));
#264451=CARTESIAN_POINT('Ctrl Pts',(-1.47134701874494,0.504834872206382,
6.15870026636689));
#264452=CARTESIAN_POINT('Ctrl Pts',(-1.43223606788575,0.616060375724229,
6.15013613425963));
#264453=CARTESIAN_POINT('Ctrl Pts',(-1.38691635996763,0.712239245048984,
6.14208580235825));
#264454=CARTESIAN_POINT('Ctrl Pts',(-1.29902174483058,0.858048841244031,
6.12891833708842));
#264455=CARTESIAN_POINT('Ctrl Pts',(-1.26248897714576,0.910948445461001,
6.12391547192843));
#264456=CARTESIAN_POINT('Ctrl Pts',(-1.20080679163367,0.989397948564389,
6.11624966212053));
#264457=CARTESIAN_POINT('Ctrl Pts',(-1.17786910808064,1.01659726025983,
6.11354162528091));
#264458=CARTESIAN_POINT('Ctrl Pts',(-1.14072582611868,1.05769456292195,
6.10939709115395));
#264459=CARTESIAN_POINT('Ctrl Pts',(-1.12715345633909,1.07214662429912,
6.10792885481236));
#264460=CARTESIAN_POINT('Ctrl Pts',(-1.10934199121306,1.09040031210602,
6.10606465355531));
#264461=CARTESIAN_POINT('Ctrl Pts',(-1.10535398718619,1.09444280792487,
6.10565117240773));
#264462=CARTESIAN_POINT('Ctrl Pts',(-1.09922437005198,1.10058849816159,
6.105021724754));
#264463=CARTESIAN_POINT('Ctrl Pts',(-1.09709871711301,1.10270742417311,
6.10480454717122));
#264464=CARTESIAN_POINT('Ctrl Pts',(-1.09270613010868,1.10706083609024,
6.10435805271474));
#264465=CARTESIAN_POINT('Ctrl Pts',(-1.09043850050444,1.10929448683168,
6.10412880875691));
#264466=CARTESIAN_POINT('Ctrl Pts',(-1.08524260572583,1.1143811962086,6.10360636966391));
#264467=CARTESIAN_POINT('Ctrl Pts',(-1.08230993985161,1.11722968044911,
6.10331353096193));
#264468=CARTESIAN_POINT('Ctrl Pts',(-1.07460924746732,1.12465054782277,
6.10254977915666));
#264469=CARTESIAN_POINT('Ctrl Pts',(-1.06982319776137,1.1292042415359,6.10208026472591));
#264470=CARTESIAN_POINT('Ctrl Pts',(-1.03678564814397,1.16023926800848,
6.09887323626815));
#264471=CARTESIAN_POINT('Ctrl Pts',(-1.00757999456037,1.18569086175973,
6.09620718836363));
#264472=CARTESIAN_POINT('Ctrl Pts',(-0.968707744519267,1.21709157635007,
6.09282295284952));
#264473=CARTESIAN_POINT('Ctrl Pts',(-0.959887216061676,1.22406010563807,
6.0920654352186));
#264474=CARTESIAN_POINT('Ctrl Pts',(-0.857030882951737,1.30352467453182,
6.08334134968763));
#264475=CARTESIAN_POINT('Ctrl Pts',(-0.755066623329114,1.36512092762015,
6.07570822534614));
#264476=CARTESIAN_POINT('Ctrl Pts',(-0.597442886922968,1.43722723014515,
6.06406984218799));
#264477=CARTESIAN_POINT('Ctrl Pts',(-0.546646606590043,1.45730454093235,
6.06034658884857));
#264478=CARTESIAN_POINT('Ctrl Pts',(-0.482900812913554,1.47869786334938,
6.05564817972521));
#264479=CARTESIAN_POINT('Ctrl Pts',(-0.470848745896762,1.48257951152687,
6.05475886305659));
#264480=CARTESIAN_POINT('Ctrl Pts',(-0.452145866058088,1.48835215892423,
6.05337658536766));
#264481=CARTESIAN_POINT('Ctrl Pts',(-0.445527371360085,1.49034673540911,
6.05288700943861));
#264482=CARTESIAN_POINT('Ctrl Pts',(-0.433986256752834,1.49374106475996,
6.05203246962971));
#264483=CARTESIAN_POINT('Ctrl Pts',(-0.429069574434188,1.4951607735452,
6.05166816146186));
#264484=CARTESIAN_POINT('Ctrl Pts',(-0.418007402686111,1.49829595569729,
6.05084785963008));
#264485=CARTESIAN_POINT('Ctrl Pts',(-0.411858215829622,1.49999792245561,
6.05039143505964));
#264486=CARTESIAN_POINT('Ctrl Pts',(-0.395350600192748,1.50445772777548,
6.04916487957339));
#264487=CARTESIAN_POINT('Ctrl Pts',(-0.384974009857124,1.50714636076748,
6.0483925318378));
#264488=CARTESIAN_POINT('Ctrl Pts',(-0.33811869748617,1.51877139069401,
6.04489832091019));
#264489=CARTESIAN_POINT('Ctrl Pts',(-0.301354286149111,1.52649138082734,
6.04213801313193));
#264490=CARTESIAN_POINT('Ctrl Pts',(-0.108483908898618,1.55975255500343,
6.02754708258555));
#264491=CARTESIAN_POINT('Ctrl Pts',(0.0505287076312072,1.56269865734192,
6.01501648797829));
#264492=CARTESIAN_POINT('Ctrl Pts',(0.239710993218713,1.53726795454164,
6.00054666131007));
#264493=CARTESIAN_POINT('Ctrl Pts',(0.272045959317536,1.53187647077777,
5.99809467836447));
#264494=CARTESIAN_POINT('Ctrl Pts',(0.310706905389217,1.52416719476881,
5.99520665769792));
#264495=CARTESIAN_POINT('Ctrl Pts',(0.317216300699603,1.52282574233159,
5.99472190467843));
#264496=CARTESIAN_POINT('Ctrl Pts',(0.327336207596194,1.52067253162558,
5.99397083314885));
#264497=CARTESIAN_POINT('Ctrl Pts',(0.33095265342718,1.5198895628334,5.99370294002241));
#264498=CARTESIAN_POINT('Ctrl Pts',(0.337673996924638,1.51840924914802,
5.99320603882047));
#264499=CARTESIAN_POINT('Ctrl Pts',(0.340779520636499,1.51771528777115,
5.99297685066957));
#264500=CARTESIAN_POINT('Ctrl Pts',(0.347860498016751,1.51611014028559,
5.99245516477276));
#264501=CARTESIAN_POINT('Ctrl Pts',(0.351834509882506,1.51519284655054,
5.99216301945526));
#264502=CARTESIAN_POINT('Ctrl Pts',(0.362203979803586,1.51275633716185,
5.99140227279873));
#264503=CARTESIAN_POINT('Ctrl Pts',(0.368593585181396,1.51121217293298,
5.99093505228011));
#264504=CARTESIAN_POINT('Ctrl Pts',(0.411948749266478,1.50044327043869,
5.98777415159275));
#264505=CARTESIAN_POINT('Ctrl Pts',(0.448578125712332,1.48990269616049,
5.98514964017806));
#264506=CARTESIAN_POINT('Ctrl Pts',(0.625805278134611,1.43177286890446,
5.97251027938462));
#264507=CARTESIAN_POINT('Ctrl Pts',(0.759482126864277,1.36557645836434,
5.96308836602181));
#264508=CARTESIAN_POINT('Ctrl Pts',(0.915561793950484,1.25817735681684,
5.95022170537104));
#264509=CARTESIAN_POINT('Ctrl Pts',(0.948425911564556,1.23359290205442,
5.94739625490069));
#264510=CARTESIAN_POINT('Ctrl Pts',(0.988499181471111,1.20106691792519,
5.94377758968457));
#264511=CARTESIAN_POINT('Ctrl Pts',(0.99665214115052,1.19431020794068,5.94303193172343));
#264512=CARTESIAN_POINT('Ctrl Pts',(1.00958418624195,1.18336822870272,5.94183359383481));
#264513=CARTESIAN_POINT('Ctrl Pts',(1.01440782510956,1.17923592041396,5.94138307855857));
#264514=CARTESIAN_POINT('Ctrl Pts',(1.02350543414919,1.17134506807683,5.94052656219198));
#264515=CARTESIAN_POINT('Ctrl Pts',(1.02778436002013,1.16759237320069,5.94012080749884));
#264516=CARTESIAN_POINT('Ctrl Pts',(1.03745688906656,1.15901502189924,5.9391969029256));
#264517=CARTESIAN_POINT('Ctrl Pts',(1.04283757767704,1.15417607017538,5.93867815987015));
#264518=CARTESIAN_POINT('Ctrl Pts',(1.056680474666,1.14155107371608,5.93733098230401));
#264519=CARTESIAN_POINT('Ctrl Pts',(1.06509032282664,1.13370854740197,5.9365001668849));
#264520=CARTESIAN_POINT('Ctrl Pts',(1.12386011639745,1.07767222660874,5.93060478248615));
#264521=CARTESIAN_POINT('Ctrl Pts',(1.17100979067523,1.02624186046265,5.92539909596041));
#264522=CARTESIAN_POINT('Ctrl Pts',(1.30267052076028,0.861698690562025,
5.90933031214765));
#264523=CARTESIAN_POINT('Ctrl Pts',(1.37539926577459,0.740101219154342,
5.89814771015041));
#264524=CARTESIAN_POINT('Ctrl Pts',(1.43203068847703,0.607354196561737,
5.88739643025262));
#264525=CARTESIAN_POINT('Ctrl Pts',(1.43330846763704,0.604332565412531,
5.88715246788332));
#264526=CARTESIAN_POINT('Ctrl Pts',(1.4345766835797,0.601306900783166,5.88690895590303));
#264527=CARTESIAN_POINT('Ctrl Pts',(1.43457651448711,0.601307304198132,
5.74991065382822));
#264528=CARTESIAN_POINT('Ctrl Pts',(1.41180695153713,0.655630077304515,
5.7544665194476));
#264529=CARTESIAN_POINT('Ctrl Pts',(1.38594843674904,0.708667726693511,
5.75905554294631));
#264530=CARTESIAN_POINT('Ctrl Pts',(1.33828009928411,0.793770154190295,
5.76656295528035));
#264531=CARTESIAN_POINT('Ctrl Pts',(1.31820785094815,0.826675988765404,
5.7695033392196));
#264532=CARTESIAN_POINT('Ctrl Pts',(1.28915655018164,0.870548113609486,
5.77344569337955));
#264533=CARTESIAN_POINT('Ctrl Pts',(1.28122078522012,0.882185900063432,
5.77449363627982));
#264534=CARTESIAN_POINT('Ctrl Pts',(1.26730896618942,0.902003769100277,
5.77627985810507));
#264535=CARTESIAN_POINT('Ctrl Pts',(1.26140920459256,0.910236039896046,
5.77702236001538));
#264536=CARTESIAN_POINT('Ctrl Pts',(1.25282153391853,0.921975032771996,
5.77808122089535));
#264537=CARTESIAN_POINT('Ctrl Pts',(1.25019860012604,0.925528615681598,
5.77840176484539));
#264538=CARTESIAN_POINT('Ctrl Pts',(1.24561469228472,0.931683906540591,
5.778956939514));
#264539=CARTESIAN_POINT('Ctrl Pts',(1.24366063115574,0.934290692831366,
5.77919204018651));
#264540=CARTESIAN_POINT('Ctrl Pts',(1.23953760697897,0.93975509601168,5.77968480380213));
#264541=CARTESIAN_POINT('Ctrl Pts',(1.23736694113728,0.942611358558621,
5.7799423448059));
#264542=CARTESIAN_POINT('Ctrl Pts',(1.23153622841073,0.950228831547422,
5.78062919244219));
#264543=CARTESIAN_POINT('Ctrl Pts',(1.22785840833142,0.954976463811629,
5.7810572760752));
#264544=CARTESIAN_POINT('Ctrl Pts',(1.21155863938543,0.975767705815738,
5.78293258594268));
#264545=CARTESIAN_POINT('Ctrl Pts',(1.19864835055544,0.991584182083082,
5.78436079627033));
#264546=CARTESIAN_POINT('Ctrl Pts',(1.08772916974027,1.12213852820329,5.79620824773255));
#264547=CARTESIAN_POINT('Ctrl Pts',(0.973805412762164,1.22231978636575,
5.80575577791448));
#264548=CARTESIAN_POINT('Ctrl Pts',(0.816008943042499,1.32479985295201,
5.81839198853135));
#264549=CARTESIAN_POINT('Ctrl Pts',(0.784082562296911,1.34394176064681,
5.82091823074569));
#264550=CARTESIAN_POINT('Ctrl Pts',(0.729908212316746,1.37383497412449,
5.8251826310554));
#264551=CARTESIAN_POINT('Ctrl Pts',(0.708034904521157,1.38523463398125,
5.82689855265673));
#264552=CARTESIAN_POINT('Ctrl Pts',(0.677893886280831,1.4000427547761,5.82925996470202));
#264553=CARTESIAN_POINT('Ctrl Pts',(0.669853373008423,1.40390750727926,
5.82988959876278));
#264554=CARTESIAN_POINT('Ctrl Pts',(0.656313131284455,1.41027295878831,
5.83094962045063));
#264555=CARTESIAN_POINT('Ctrl Pts',(0.650831199682456,1.41281120190569,
5.83137870557954));
#264556=CARTESIAN_POINT('Ctrl Pts',(0.640002896059365,1.41774852543471,
5.83222618540237));
#264557=CARTESIAN_POINT('Ctrl Pts',(0.634657473828427,1.42014945605064,
5.83264450813044));
#264558=CARTESIAN_POINT('Ctrl Pts',(0.622882337572623,1.42535857592253,
5.83356599127214));
#264559=CARTESIAN_POINT('Ctrl Pts',(0.616446963624959,1.42815356823556,
5.83406959144869));
#264560=CARTESIAN_POINT('Ctrl Pts',(0.593908526390495,1.43776167638116,
5.83583345824784));
#264561=CARTESIAN_POINT('Ctrl Pts',(0.577710222744153,1.44434650551658,
5.83710137774138));
#264562=CARTESIAN_POINT('Ctrl Pts',(0.43681501265674,1.49887303322602,5.84813642402534));
#264563=CARTESIAN_POINT('Ctrl Pts',(0.306557510246776,1.53082804601885,
5.85845467701028));
#264564=CARTESIAN_POINT('Ctrl Pts',(0.100195224064705,1.55403864404595,
5.87454796021508));
#264565=CARTESIAN_POINT('Ctrl Pts',(0.026025065254874,1.55704861479061,
5.8802657231426));
#264566=CARTESIAN_POINT('Ctrl Pts',(-0.0610735337307294,1.55435490044076,
5.88672445621464));
#264567=CARTESIAN_POINT('Ctrl Pts',(-0.0740578598872797,1.5537903964849,
5.88768047043065));
#264568=CARTESIAN_POINT('Ctrl Pts',(-0.0919055364529692,1.55279020712327,
5.88898382568743));
#264569=CARTESIAN_POINT('Ctrl Pts',(-0.0967757044030916,1.55249428976086,
5.88933837610575));
#264570=CARTESIAN_POINT('Ctrl Pts',(-0.104978896586389,1.55195710225332,
5.88993362701216));
#264571=CARTESIAN_POINT('Ctrl Pts',(-0.108312648043226,1.55172800032342,
5.89017499331925));
#264572=CARTESIAN_POINT('Ctrl Pts',(-0.114655805699035,1.55127154422388,
5.89063317994442));
#264573=CARTESIAN_POINT('Ctrl Pts',(-0.117665317002589,1.55104617316807,
5.8908501125612));
#264574=CARTESIAN_POINT('Ctrl Pts',(-0.125586291950338,1.55042981399786,
5.89141992489533));
#264575=CARTESIAN_POINT('Ctrl Pts',(-0.130496641383189,1.55002424278468,
5.89177199683449));
#264576=CARTESIAN_POINT('Ctrl Pts',(-0.147716255580492,1.54851957701059,
5.89300281948117));
#264577=CARTESIAN_POINT('Ctrl Pts',(-0.160014695861664,1.5472970933286,
5.89387502824556));
#264578=CARTESIAN_POINT('Ctrl Pts',(-0.259622846841005,1.53619550216969,
5.90089320826332));
#264579=CARTESIAN_POINT('Ctrl Pts',(-0.34598004547932,1.51907968591768,
5.90669544162653));
#264580=CARTESIAN_POINT('Ctrl Pts',(-0.513515191808521,1.4708351981456,
5.91817767831307));
#264581=CARTESIAN_POINT('Ctrl Pts',(-0.594445555122932,1.44003025540019,
5.92384110794829));
#264582=CARTESIAN_POINT('Ctrl Pts',(-0.712488709514929,1.38344388420044,
5.93270686741078));
#264583=CARTESIAN_POINT('Ctrl Pts',(-0.751736218238954,1.36251575173322,
5.93576237472295));
#264584=CARTESIAN_POINT('Ctrl Pts',(-0.79946059501787,1.33437732309553,
5.93964473527473));
#264585=CARTESIAN_POINT('Ctrl Pts',(-0.808831239408744,1.32871821643117,
5.94041530704239));
#264586=CARTESIAN_POINT('Ctrl Pts',(-0.823653889917207,1.31955164057771,
5.94164787498295));
#264587=CARTESIAN_POINT('Ctrl Pts',(-0.829145175752436,1.31610810260629,
5.94210752728332));
#264588=CARTESIAN_POINT('Ctrl Pts',(-0.839472076276543,1.3095419107176,
5.94297777585417));
#264589=CARTESIAN_POINT('Ctrl Pts',(-0.844312206399271,1.30642653037365,
5.94338809776495));
#264590=CARTESIAN_POINT('Ctrl Pts',(-0.855209122891349,1.29932681226943,
5.94431749154319));
#264591=CARTESIAN_POINT('Ctrl Pts',(-0.861255532406906,1.29532687518016,
5.94483713926254));
#264592=CARTESIAN_POINT('Ctrl Pts',(-0.876725669093412,1.28493657140105,
5.94617703026707));
#264593=CARTESIAN_POINT('Ctrl Pts',(-0.886107443914718,1.27848483620163,
5.9469995688791));
#264594=CARTESIAN_POINT('Ctrl Pts',(-0.947728311148291,1.23510481133937,
5.95246967027297));
#264595=CARTESIAN_POINT('Ctrl Pts',(-0.997710069147358,1.19509219453146,
5.95723511038795));
#264596=CARTESIAN_POINT('Ctrl Pts',(-1.11598861430016,1.08780259006151,
5.96937179304928));
#264597=CARTESIAN_POINT('Ctrl Pts',(-1.18080297379458,1.01707756660921,
5.97684597219249));
#264598=CARTESIAN_POINT('Ctrl Pts',(-1.27351028392199,0.895021840161294,
5.98867373891221));
#264599=CARTESIAN_POINT('Ctrl Pts',(-1.30575501748159,0.847288556945824,
5.99307022136888));
#264600=CARTESIAN_POINT('Ctrl Pts',(-1.34117731913795,0.788007435196004,
5.99817649747513));
#264601=CARTESIAN_POINT('Ctrl Pts',(-1.3469627845853,0.778076858113244,
5.99902046879497));
#264602=CARTESIAN_POINT('Ctrl Pts',(-1.35493256617952,0.764041613367275,
6.00019640535912));
#264603=CARTESIAN_POINT('Ctrl Pts',(-1.35720917065368,0.759990206811264,
6.00053389786424));
#264604=CARTESIAN_POINT('Ctrl Pts',(-1.3610697066289,0.753047390055815,
6.00110884453054));
#264605=CARTESIAN_POINT('Ctrl Pts',(-1.36266265370051,0.750161056731348,
6.00134686549667));
#264606=CARTESIAN_POINT('Ctrl Pts',(-1.36572057929681,0.744578380764795,
6.00180528211072));
#264607=CARTESIAN_POINT('Ctrl Pts',(-1.36718676185103,0.741882756560779,
6.00202575753861));
#264608=CARTESIAN_POINT('Ctrl Pts',(-1.37069988566621,0.73537797940553,
6.00255572686452));
#264609=CARTESIAN_POINT('Ctrl Pts',(-1.37273895409416,0.731564566030282,
6.00286472744016));
#264610=CARTESIAN_POINT('Ctrl Pts',(-1.38019015543334,0.717488670432404,
6.00399926211218));
#264611=CARTESIAN_POINT('Ctrl Pts',(-1.38550350642506,0.707173891056844,
6.00481887936912));
#264612=CARTESIAN_POINT('Ctrl Pts',(-1.43919734741206,0.600009622085865,
6.0132234902045));
#264613=CARTESIAN_POINT('Ctrl Pts',(-1.47746462869008,0.498404016884063,
6.02027769473693));
#264614=CARTESIAN_POINT('Ctrl Pts',(-1.5313287821953,0.292479790475092,
6.03429394692431));
#264615=CARTESIAN_POINT('Ctrl Pts',(-1.54751808866646,0.188932480653449,
6.04122168592858));
#264616=CARTESIAN_POINT('Ctrl Pts',(-1.55402229161874,0.0694525188932073,
6.04955785862182));
#264617=CARTESIAN_POINT('Ctrl Pts',(-1.55462402921913,0.0543418335736241,
6.0506178362248));
#264618=CARTESIAN_POINT('Ctrl Pts',(-1.55519079218697,0.0318736557810259,
6.05220346647178));
#264619=CARTESIAN_POINT('Ctrl Pts',(-1.55532409756881,0.0245209748386396,
6.05272387752729));
#264620=CARTESIAN_POINT('Ctrl Pts',(-1.55546890945959,0.0114009480816709,
6.05365532295415));
#264621=CARTESIAN_POINT('Ctrl Pts',(-1.55550048769016,0.00563392131872312,
6.05406572381775));
#264622=CARTESIAN_POINT('Ctrl Pts',(-1.55549944508379,-0.00655278324734221,
6.0549350968532));
#264623=CARTESIAN_POINT('Ctrl Pts',(-1.55545915372167,-0.0129723339010835,
6.05539430070872));
#264624=CARTESIAN_POINT('Ctrl Pts',(-1.55524616967184,-0.0300557611713273,
6.0566197336781));
#264625=CARTESIAN_POINT('Ctrl Pts',(-1.55500354024369,-0.0407182559079988,
6.05738812754367));
#264626=CARTESIAN_POINT('Ctrl Pts',(-1.55329993415077,-0.0922686507356349,
6.06112097744222));
#264627=CARTESIAN_POINT('Ctrl Pts',(-1.5503359179664,-0.133087012044085,
6.06413170916431));
#264628=CARTESIAN_POINT('Ctrl Pts',(-1.52914025500215,-0.321667487676258,
6.0783112911403));
#264629=CARTESIAN_POINT('Ctrl Pts',(-1.49136253134308,-0.46643782989504,
6.09007018255088));
#264630=CARTESIAN_POINT('Ctrl Pts',(-1.41905879998039,-0.638169093086119,
6.1042558048259));
#264631=CARTESIAN_POINT('Ctrl Pts',(-1.40325369535684,-0.672210759999545,
6.10707424891338));
#264632=CARTESIAN_POINT('Ctrl Pts',(-1.38323788402782,-0.711531270015986,
6.1103113770089));
#264633=CARTESIAN_POINT('Ctrl Pts',(-1.3802069597247,-0.717392880136795,
6.11079344491076));
#264634=CARTESIAN_POINT('Ctrl Pts',(-1.37522663822729,-0.726876094037405,
6.11157233636648));
#264635=CARTESIAN_POINT('Ctrl Pts',(-1.37330006023757,-0.730509485345017,
6.1118705146768));
#264636=CARTESIAN_POINT('Ctrl Pts',(-1.36983869633044,-0.736975286810254,
6.1124006425734));
#264637=CARTESIAN_POINT('Ctrl Pts',(-1.3683095041684,-0.739810603353431,
6.11263293470359));
#264638=CARTESIAN_POINT('Ctrl Pts',(-1.3649747403771,-0.745947967920077,
6.11313537206751));
#264639=CARTESIAN_POINT('Ctrl Pts',(-1.36316599255241,-0.749248216729731,
6.11340531230543));
#264640=CARTESIAN_POINT('Ctrl Pts',(-1.35805285445855,-0.758497862705271,
6.11416130786497));
#264641=CARTESIAN_POINT('Ctrl Pts',(-1.35472131826895,-0.764432284504369,
6.11464567830022));
#264642=CARTESIAN_POINT('Ctrl Pts',(-1.334210215944,-0.800413180279256,
6.11757960881499));
#264643=CARTESIAN_POINT('Ctrl Pts',(-1.31606909580525,-0.82990406590892,
6.11997223452674));
#264644=CARTESIAN_POINT('Ctrl Pts',(-1.2507873815931,-0.928496024990666,
6.12801729146392));
#264645=CARTESIAN_POINT('Ctrl Pts',(-1.19906559260512,-0.994393284479451,
6.13348066747959));
#264646=CARTESIAN_POINT('Ctrl Pts',(-1.07091092811761,-1.13304431993926,
6.14591691450504));
#264647=CARTESIAN_POINT('Ctrl Pts',(-0.991893969471411,-1.20282216477062,
6.15289694048487));
#264648=CARTESIAN_POINT('Ctrl Pts',(-0.896738851148734,-1.27105566128855,
6.16107437810008));
#264649=CARTESIAN_POINT('Ctrl Pts',(-0.886947588750496,-1.27790728227964,
6.16191304189168));
#264650=CARTESIAN_POINT('Ctrl Pts',(-0.870950596091194,-1.28882906773578,
6.16327935965435));
#264651=CARTESIAN_POINT('Ctrl Pts',(-0.86479284395614,-1.29296892471322,
6.16380437894695));
#264652=CARTESIAN_POINT('Ctrl Pts',(-0.853790332077212,-1.3002521558323,
6.16474097235305));
#264653=CARTESIAN_POINT('Ctrl Pts',(-0.8489572067864,-1.30341292739308,
6.16515188630179));
#264654=CARTESIAN_POINT('Ctrl Pts',(-0.838744861992011,-1.31001070789687,
6.16601914337189));
#264655=CARTESIAN_POINT('Ctrl Pts',(-0.833361874563006,-1.31344165538679,
6.16647570153448));
#264656=CARTESIAN_POINT('Ctrl Pts',(-0.819068431820425,-1.32242860615638,
6.16768657598666));
#264657=CARTESIAN_POINT('Ctrl Pts',(-0.810122707848137,-1.32792759688571,
6.16844296684248));
#264658=CARTESIAN_POINT('Ctrl Pts',(-0.767698548077798,-1.35341775800188,
6.17202393764307));
#264659=CARTESIAN_POINT('Ctrl Pts',(-0.733534626916184,-1.37223435959762,
6.17489034764616));
#264660=CARTESIAN_POINT('Ctrl Pts',(-0.564657761904698,-1.45713813560855,
6.18899145817112));
#264661=CARTESIAN_POINT('Ctrl Pts',(-0.42157343428595,-1.50477619778259,
6.2008391547421));
#264662=CARTESIAN_POINT('Ctrl Pts',(-0.236034660355262,-1.53796949024919,
6.21519928309077));
#264663=CARTESIAN_POINT('Ctrl Pts',(-0.197893471849304,-1.54334095333417,
6.21809367851642));
#264664=CARTESIAN_POINT('Ctrl Pts',(-0.152977552361988,-1.54797360731217,
6.22140692768028));
#264665=CARTESIAN_POINT('Ctrl Pts',(-0.14636207657615,-1.5486131108868,
6.221892504896));
#264666=CARTESIAN_POINT('Ctrl Pts',(-0.135632464236921,-1.54958094815667,
6.22267593050289));
#264667=CARTESIAN_POINT('Ctrl Pts',(-0.131520855827859,-1.54993533600361,
6.22297515898371));
#264668=CARTESIAN_POINT('Ctrl Pts',(-0.124196093301675,-1.55053731502337,
6.22350642476018));
#264669=CARTESIAN_POINT('Ctrl Pts',(-0.120983540116742,-1.55079128789203,
6.22373881061804));
#264670=CARTESIAN_POINT('Ctrl Pts',(-0.114027742097437,-1.55131944169977,
6.2242406188666));
#264671=CARTESIAN_POINT('Ctrl Pts',(-0.110284291180253,-1.55159005929032,
6.22450984083079));
#264672=CARTESIAN_POINT('Ctrl Pts',(-0.0997973042108043,-1.55231002837404,
6.22526178711578));
#264673=CARTESIAN_POINT('Ctrl Pts',(-0.0930516552347153,-1.55272899116993,
6.22574285538301));
#264674=CARTESIAN_POINT('Ctrl Pts',(-0.0526068693072738,-1.55497643860261,
6.22861269498564));
#264675=CARTESIAN_POINT('Ctrl Pts',(-0.0188551430630736,-1.55575194808541,
6.23094738317539));
#264676=CARTESIAN_POINT('Ctrl Pts',(0.191501298438252,-1.55373711752684,
6.24527279663668));
#264677=CARTESIAN_POINT('Ctrl Pts',(0.366529471419132,-1.52198541230324,
6.25635598380528));
#264678=CARTESIAN_POINT('Ctrl Pts',(0.553100067501514,-1.45400867752475,
6.27007414253767));
#264679=CARTESIAN_POINT('Ctrl Pts',(0.573537611795688,-1.44606896228839,
6.27160172034684));
#264680=CARTESIAN_POINT('Ctrl Pts',(0.601917957479531,-1.43434729809278,
6.27376142898982));
#264681=CARTESIAN_POINT('Ctrl Pts',(0.610007533615243,-1.4309256452903,
6.27438147415663));
#264682=CARTESIAN_POINT('Ctrl Pts',(0.623033575706379,-1.42528547965077,
6.27538728972449));
#264683=CARTESIAN_POINT('Ctrl Pts',(0.627988287562152,-1.42310935781394,
6.27577161646394));
#264684=CARTESIAN_POINT('Ctrl Pts',(0.638286731446648,-1.41852200105435,
6.2765741441187));
#264685=CARTESIAN_POINT('Ctrl Pts',(0.643628379213044,-1.41610632607762,
6.27699249168142));
#264686=CARTESIAN_POINT('Ctrl Pts',(0.656226386956023,-1.41032307423207,
6.27798416631339));
#264687=CARTESIAN_POINT('Ctrl Pts',(0.66347061416635,-1.40692963020744,
6.27855837480454));
#264688=CARTESIAN_POINT('Ctrl Pts',(0.687522377090093,-1.39543589454731,
6.28047830867178));
#264689=CARTESIAN_POINT('Ctrl Pts',(0.704209720761646,-1.38708938707098,
6.28183250063242));
#264690=CARTESIAN_POINT('Ctrl Pts',(0.743550666022141,-1.36651933913611,
6.28507959997411));
#264691=CARTESIAN_POINT('Ctrl Pts',(0.766058271678354,-1.35403001421563,
6.28698140805058));
#264692=CARTESIAN_POINT('Ctrl Pts',(0.917605537363094,-1.26494924863414,
6.30009522657793));
#264693=CARTESIAN_POINT('Ctrl Pts',(1.03527503212876,-1.17059290372971,
6.3119445922639));
#264694=CARTESIAN_POINT('Ctrl Pts',(1.16385246951167,-1.0327203076879,6.32630784546666));
#264695=CARTESIAN_POINT('Ctrl Pts',(1.18906945241916,-1.00358270876691,
6.32920353471376));
#264696=CARTESIAN_POINT('Ctrl Pts',(1.21734097895795,-0.968351884577592,
6.33251808115515));
#264697=CARTESIAN_POINT('Ctrl Pts',(1.22146788821302,-0.963141024819116,
6.3330037193182));
#264698=CARTESIAN_POINT('Ctrl Pts',(1.2281028550902,-0.954652114442307,
6.3337872236471));
#264699=CARTESIAN_POINT('Ctrl Pts',(1.23063143399829,-0.951390328419722,
6.33408647034435));
#264700=CARTESIAN_POINT('Ctrl Pts',(1.23511128678741,-0.945563717713477,
6.33461775589966));
#264701=CARTESIAN_POINT('Ctrl Pts',(1.23706759690874,-0.943002861286291,
6.33485014342425));
#264702=CARTESIAN_POINT('Ctrl Pts',(1.24128499793184,-0.93744647247841,
6.33535194094589));
#264703=CARTESIAN_POINT('Ctrl Pts',(1.24354320844632,-0.934448834546821,
6.33562115059495));
#264704=CARTESIAN_POINT('Ctrl Pts',(1.24983707636303,-0.926030883822506,
6.33637302751293));
#264705=CARTESIAN_POINT('Ctrl Pts',(1.25384836018243,-0.920592314411871,
6.33685403922019));
#264706=CARTESIAN_POINT('Ctrl Pts',(1.27767042080742,-0.887849380866199,
6.33972279858213));
#264707=CARTESIAN_POINT('Ctrl Pts',(1.29662596430493,-0.859930095167336,
6.34205651048334));
#264708=CARTESIAN_POINT('Ctrl Pts',(1.40886595318109,-0.682452361077834,
6.35635658870539));
#264709=CARTESIAN_POINT('Ctrl Pts',(1.47707432958275,-0.518562963539632,
6.36741842354178));
#264710=CARTESIAN_POINT('Ctrl Pts',(1.5213142930603,-0.325077958816658,
6.38112630161971));
#264711=CARTESIAN_POINT('Ctrl Pts',(1.52579753660768,-0.303339164458439,
6.38267241735419));
#264712=CARTESIAN_POINT('Ctrl Pts',(1.53141188168072,-0.272829350451758,
6.38485418796489));
#264713=CARTESIAN_POINT('Ctrl Pts',(1.53293579996874,-0.264132605411793,
6.38547742388281));
#264714=CARTESIAN_POINT('Ctrl Pts',(1.53527557458462,-0.250077061660111,
6.3864870355796));
#264715=CARTESIAN_POINT('Ctrl Pts',(1.53613761871812,-0.244726054374228,
6.38687194625963));
#264716=CARTESIAN_POINT('Ctrl Pts',(1.53787287635663,-0.233584165689512,
6.38767460144337));
#264717=CARTESIAN_POINT('Ctrl Pts',(1.53874138608654,-0.227792649823775,
6.38809248764551));
#264718=CARTESIAN_POINT('Ctrl Pts',(1.54071371698038,-0.214114252100162,
6.38908109957948));
#264719=CARTESIAN_POINT('Ctrl Pts',(1.5417897057404,-0.206223591147435,
6.3896526917213));
#264720=CARTESIAN_POINT('Ctrl Pts',(1.5451571337787,-0.180027796294164,
6.39155478977296));
#264721=CARTESIAN_POINT('Ctrl Pts',(1.54718344155232,-0.161690813930811,
6.39289354811955));
#264722=CARTESIAN_POINT('Ctrl Pts',(1.55122017601129,-0.118066018562273,
6.39609723055154));
#264723=CARTESIAN_POINT('Ctrl Pts',(1.5529390133741,-0.0927572297755599,
6.39797074142814));
#264724=CARTESIAN_POINT('Ctrl Pts',(1.56055818214423,0.0828679691374859,
6.41107826785458));
#264725=CARTESIAN_POINT('Ctrl Pts',(1.54523986935127,0.233298120599414,
6.42295609127557));
#264726=CARTESIAN_POINT('Ctrl Pts',(1.49913029790243,0.416765548773638,
6.43737179825731));
#264727=CARTESIAN_POINT('Ctrl Pts',(1.48826951949714,0.454026026771004,
6.44028882961641));
#264728=CARTESIAN_POINT('Ctrl Pts',(1.47392367033915,0.497165599076847,
6.44362480996212));
#264729=CARTESIAN_POINT('Ctrl Pts',(1.47178113440391,0.503472854818314,
6.44411149011784));
#264730=CARTESIAN_POINT('Ctrl Pts',(1.46824420866228,0.513669408261775,
6.44489634019957));
#264731=CARTESIAN_POINT('Ctrl Pts',(1.46687475475194,0.517567166843468,
6.44519589821853));
#264732=CARTESIAN_POINT('Ctrl Pts',(1.46440932251141,0.524495923211836,
6.44572752200996));
#264733=CARTESIAN_POINT('Ctrl Pts',(1.46331943955215,0.527529009501955,
6.44595993823178));
#264734=CARTESIAN_POINT('Ctrl Pts',(1.46094103086649,0.534083904337845,
6.44646155339418));
#264735=CARTESIAN_POINT('Ctrl Pts',(1.45964919597237,0.537604443846408,
6.44673055332526));
#264736=CARTESIAN_POINT('Ctrl Pts',(1.45599858235928,0.547443018496049,
6.44748124927357));
#264737=CARTESIAN_POINT('Ctrl Pts',(1.45361139066549,0.55375053920999,6.44796129809443));
#264738=CARTESIAN_POINT('Ctrl Pts',(1.44584453024801,0.573876043197192,
6.44948969276664));
#264739=CARTESIAN_POINT('Ctrl Pts',(1.44030845088325,0.587632253594381,
6.45052937770318));
#264740=CARTESIAN_POINT('Ctrl Pts',(1.43457668334549,0.60130690134194,6.45155991302018));
#264741=CARTESIAN_POINT('Origin',(0.,0.,-1.29405622560371));
#264742=CARTESIAN_POINT('',(1.4345768221925,0.601306570085576,7.28923406038337));
#264743=CARTESIAN_POINT('',(1.43457650415244,0.601307328854198,7.14927790964297));
#264744=CARTESIAN_POINT('',(1.43457668357355,0.601306900797845,-1.29405622560371));
#264745=CARTESIAN_POINT('',(-1.55751602490984,0.000817960485851865,6.89405622560371));
#264746=CARTESIAN_POINT('Ctrl Pts',(1.43457682219249,0.601306570085596,
7.28923406038337));
#264747=CARTESIAN_POINT('Ctrl Pts',(1.44980351843734,0.564979234582981,
7.28657956429081));
#264748=CARTESIAN_POINT('Ctrl Pts',(1.46365495195722,0.52806263480983,7.28389089081866));
#264749=CARTESIAN_POINT('Ctrl Pts',(1.48191627802783,0.473122508224971,
7.27987552565566));
#264750=CARTESIAN_POINT('Ctrl Pts',(1.48742440572936,0.455509988635428,
7.27858631906853));
#264751=CARTESIAN_POINT('Ctrl Pts',(1.49467709042677,0.430783218925999,
7.27677168274819));
#264752=CARTESIAN_POINT('Ctrl Pts',(1.49668686348088,0.423747820942215,
7.27625485183045));
#264753=CARTESIAN_POINT('Ctrl Pts',(1.50008137180983,0.411539550455861,
7.27535698876009));
#264754=CARTESIAN_POINT('Ctrl Pts',(1.50148918227773,0.406373175586266,
7.27497670898746));
#264755=CARTESIAN_POINT('Ctrl Pts',(1.50436096109021,0.395615662351214,
7.27418417387299));
#264756=CARTESIAN_POINT('Ctrl Pts',(1.50582049732888,0.390023437391185,
7.2737717821648));
#264757=CARTESIAN_POINT('Ctrl Pts',(1.50918820865661,0.376819297021503,
7.27279705461033));
#264758=CARTESIAN_POINT('Ctrl Pts',(1.51106999725939,0.369200881570351,
7.27223387958147));
#264759=CARTESIAN_POINT('Ctrl Pts',(1.51710528139918,0.34394773934382,7.27036429166985));
#264760=CARTESIAN_POINT('Ctrl Pts',(1.52100818995956,0.326255293828729,
7.26904992232478));
#264761=CARTESIAN_POINT('Ctrl Pts',(1.54049053092949,0.229973750910464,
7.26186964160514));
#264762=CARTESIAN_POINT('Ctrl Pts',(1.55028696858727,0.150351130317674,
7.25582347061479));
#264763=CARTESIAN_POINT('Ctrl Pts',(1.55827222221061,-0.0260542502123737,
7.24224319494439));
#264764=CARTESIAN_POINT('Ctrl Pts',(1.55365686578769,-0.122643212766432,
7.23468248039912));
#264765=CARTESIAN_POINT('Ctrl Pts',(1.53471228532792,-0.256371141204358,
7.22439181526886));
#264766=CARTESIAN_POINT('Ctrl Pts',(1.5278829947406,-0.294350353101164,
7.2214920862619));
#264767=CARTESIAN_POINT('Ctrl Pts',(1.51823964181167,-0.338485099496349,
7.21817753884491));
#264768=CARTESIAN_POINT('Ctrl Pts',(1.51679037739624,-0.344921335538409,
7.21769556919996));
#264769=CARTESIAN_POINT('Ctrl Pts',(1.51437734263109,-0.355328307549209,
7.21691872867417));
#264770=CARTESIAN_POINT('Ctrl Pts',(1.51343882013,-0.359304718558758,7.21662249137146));
#264771=CARTESIAN_POINT('Ctrl Pts',(1.51174131779941,-0.366372171276095,
7.2160970752956));
#264772=CARTESIAN_POINT('Ctrl Pts',(1.51098850913695,-0.369464620467438,
7.21586755163463));
#264773=CARTESIAN_POINT('Ctrl Pts',(1.50934116187564,-0.376142475060763,
7.21537274391553));
#264774=CARTESIAN_POINT('Ctrl Pts',(1.50844333872061,-0.379727006041249,
7.21510765096319));
#264775=CARTESIAN_POINT('Ctrl Pts',(1.5059006669027,-0.389727208140776,
7.21436942384523));
#264776=CARTESIAN_POINT('Ctrl Pts',(1.50422757777804,-0.396135726473404,
7.21389787631992));
#264777=CARTESIAN_POINT('Ctrl Pts',(1.49413664832617,-0.433801555090046,
7.21113436112351));
#264778=CARTESIAN_POINT('Ctrl Pts',(1.48478492887269,-0.464803415669506,
7.20889220545473));
#264779=CARTESIAN_POINT('Ctrl Pts',(1.4260832831902,-0.639485621365874,
7.19632423251459));
#264780=CARTESIAN_POINT('Ctrl Pts',(1.35686271881169,-0.775620951241863,
7.18670765682073));
#264781=CARTESIAN_POINT('Ctrl Pts',(1.24400408316791,-0.934827104907211,
7.17348550232125));
#264782=CARTESIAN_POINT('Ctrl Pts',(1.21755533854447,-0.969023372149023,
7.17051536321887));
#264783=CARTESIAN_POINT('Ctrl Pts',(1.18256389585577,-1.01056729328593,
7.16671092483038));
#264784=CARTESIAN_POINT('Ctrl Pts',(1.17531782166127,-1.01898558811702,
7.16592938978439));
#264785=CARTESIAN_POINT('Ctrl Pts',(1.16366968831985,-1.0322285341878,7.16468250086537));
#264786=CARTESIAN_POINT('Ctrl Pts',(1.15932622761147,-1.03710442382538,
7.16421957951519));
#264787=CARTESIAN_POINT('Ctrl Pts',(1.1511556392524,-1.04616111033051,7.16335244141609));
#264788=CARTESIAN_POINT('Ctrl Pts',(1.14733609830745,-1.05034863284039,
7.16294854828634));
#264789=CARTESIAN_POINT('Ctrl Pts',(1.13876972896462,-1.05963782169625,
7.16204590495589));
#264790=CARTESIAN_POINT('Ctrl Pts',(1.13401135776446,-1.06472862566507,
7.16154666784467));
#264791=CARTESIAN_POINT('Ctrl Pts',(1.11995694726716,-1.07956382596798,
7.16007824939796));
#264792=CARTESIAN_POINT('Ctrl Pts',(1.11056858721707,-1.08921944985359,
7.15910510005958));
#264793=CARTESIAN_POINT('Ctrl Pts',(1.08901498001704,-1.11081826568846,
7.15688769233486));
#264794=CARTESIAN_POINT('Ctrl Pts',(1.07677656674325,-1.12268563225708,
7.15564028887177));
#264795=CARTESIAN_POINT('Ctrl Pts',(1.03595626132954,-1.16098683240311,
7.15151629245127));
#264796=CARTESIAN_POINT('Ctrl Pts',(1.00657885799072,-1.1865472344246,7.14860518128167));
#264797=CARTESIAN_POINT('Ctrl Pts',(0.913670224496102,-1.26144911397863,
7.13956943016963));
#264798=CARTESIAN_POINT('Ctrl Pts',(0.847249784712435,-1.30698614250228,
7.13333326578048));
#264799=CARTESIAN_POINT('Ctrl Pts',(0.704178867092309,-1.38956895390409,
7.12052553051608));
#264800=CARTESIAN_POINT('Ctrl Pts',(0.627390403625713,-1.4258873899547,
7.11397574231193));
#264801=CARTESIAN_POINT('Ctrl Pts',(0.540634244719874,-1.45854621330736,
7.10716491698234));
#264802=CARTESIAN_POINT('Ctrl Pts',(0.533232397201672,-1.46126851074942,
7.1065884075079));
#264803=CARTESIAN_POINT('Ctrl Pts',(0.522032304066222,-1.4652913141117,
7.1057232813387));
#264804=CARTESIAN_POINT('Ctrl Pts',(0.518249353345248,-1.46663355015495,
7.10543231148562));
#264805=CARTESIAN_POINT('Ctrl Pts',(0.511462736045827,-1.46901198587162,
7.10491257500398));
#264806=CARTESIAN_POINT('Ctrl Pts',(0.50846106464916,-1.47005363554193,
7.10468349336731));
#264807=CARTESIAN_POINT('Ctrl Pts',(0.501911855616568,-1.47230390344355,
7.10418540366442));
#264808=CARTESIAN_POINT('Ctrl Pts',(0.498363140151507,-1.47350889927565,
7.10391660983425));
#264809=CARTESIAN_POINT('Ctrl Pts',(0.488301147792028,-1.47688502414884,
7.10315748672371));
#264810=CARTESIAN_POINT('Ctrl Pts',(0.481777693494745,-1.47902591058986,
7.10266889240957));
#264811=CARTESIAN_POINT('Ctrl Pts',(0.440048746574028,-1.49241525217801,
7.09956488126824));
#264812=CARTESIAN_POINT('Ctrl Pts',(0.404462467550888,-1.50245028302582,
7.09701469974492));
#264813=CARTESIAN_POINT('Ctrl Pts',(0.316362647524366,-1.523935797338,7.09085932684453));
#264814=CARTESIAN_POINT('Ctrl Pts',(0.263548412745544,-1.53395197480168,
7.087303362482));
#264815=CARTESIAN_POINT('Ctrl Pts',(0.0863369584395551,-1.55813474255322,
7.07551464856515));
#264816=CARTESIAN_POINT('Ctrl Pts',(-0.0392162564204408,-1.56003060934021,
7.06735179576436));
#264817=CARTESIAN_POINT('Ctrl Pts',(-0.173350459862813,-1.54584129878287,
7.05799061092119));
#264818=CARTESIAN_POINT('Ctrl Pts',(-0.183056160874355,-1.5447220259772,
7.05730989789165));
#264819=CARTESIAN_POINT('Ctrl Pts',(-0.203488662192368,-1.5421704577941,
7.0558693254736));
#264820=CARTESIAN_POINT('Ctrl Pts',(-0.214212303050778,-1.54071750665779,
7.055108876351));
#264821=CARTESIAN_POINT('Ctrl Pts',(-0.231875947900591,-1.53813628064714,
7.05384861515069));
#264822=CARTESIAN_POINT('Ctrl Pts',(-0.238825142958862,-1.53707261416418,
7.05335084032911));
#264823=CARTESIAN_POINT('Ctrl Pts',(-0.251367648035335,-1.53506570814196,
7.05244874767385));
#264824=CARTESIAN_POINT('Ctrl Pts',(-0.256963496349401,-1.53413890595804,
7.05204495623546));
#264825=CARTESIAN_POINT('Ctrl Pts',(-0.268945449604897,-1.53208702189175,
7.05117745086141));
#264826=CARTESIAN_POINT('Ctrl Pts',(-0.275329818535755,-1.53095257476621,
7.05071344698351));
#264827=CARTESIAN_POINT('Ctrl Pts',(-0.292714567407997,-1.52775119425046,
7.04944502247785));
#264828=CARTESIAN_POINT('Ctrl Pts',(-0.303699840449521,-1.52560542875238,
7.04863811472978));
#264829=CARTESIAN_POINT('Ctrl Pts',(-0.3628927446723,-1.51337856776211,
7.04426007127144));
#264830=CARTESIAN_POINT('Ctrl Pts',(-0.410618861651596,-1.50113190230789,
7.04062059963461));
#264831=CARTESIAN_POINT('Ctrl Pts',(-0.564861692088216,-1.45364658881012,
7.02848372873606));
#264832=CARTESIAN_POINT('Ctrl Pts',(-0.668151969939364,-1.4091572707714,
7.01972644472135));
#264833=CARTESIAN_POINT('Ctrl Pts',(-0.821178600096131,-1.322611668823,
7.00615400190544));
#264834=CARTESIAN_POINT('Ctrl Pts',(-0.874641579021902,-1.28788204446359,
7.00129040258078));
#264835=CARTESIAN_POINT('Ctrl Pts',(-0.932214900820325,-1.24523843313029,
6.9960257821059));
#264836=CARTESIAN_POINT('Ctrl Pts',(-0.938563377745482,-1.24046046683518,
6.99544490834053));
#264837=CARTESIAN_POINT('Ctrl Pts',(-0.948073631203309,-1.23318808472561,
6.99457453775762));
#264838=CARTESIAN_POINT('Ctrl Pts',(-0.951262659299366,-1.2307297902086,
6.99428264628133));
#264839=CARTESIAN_POINT('Ctrl Pts',(-0.95681758258171,-1.22641323116009,
6.99377419655252));
#264840=CARTESIAN_POINT('Ctrl Pts',(-0.959187660756776,-1.22456046479528,
6.99355726002511));
#264841=CARTESIAN_POINT('Ctrl Pts',(-0.96437944529423,-1.2204775582992,
6.99308205609744));
#264842=CARTESIAN_POINT('Ctrl Pts',(-0.967198794575505,-1.21824450637017,
6.99282399965478));
#264843=CARTESIAN_POINT('Ctrl Pts',(-0.974789562867427,-1.2121893137751,
6.99212912982872));
#264844=CARTESIAN_POINT('Ctrl Pts',(-0.979546302858022,-1.20834873615893,
6.99169360192371));
#264845=CARTESIAN_POINT('Ctrl Pts',(-0.990201661037585,-1.19964136128516,
6.9907174700733));
#264846=CARTESIAN_POINT('Ctrl Pts',(-0.996087330823707,-1.1947588713179,
6.99017791987711));
#264847=CARTESIAN_POINT('Ctrl Pts',(-1.01418301167748,-1.17952082557038,
6.98851704219005));
#264848=CARTESIAN_POINT('Ctrl Pts',(-1.02626975563306,-1.16901967276755,
6.98740481155359));
#264849=CARTESIAN_POINT('Ctrl Pts',(-1.07330159088528,-1.12686590671051,
6.98305529545409));
#264850=CARTESIAN_POINT('Ctrl Pts',(-1.10696471594757,-1.09381577668366,
6.97989357237831));
#264851=CARTESIAN_POINT('Ctrl Pts',(-1.1840559434951,-1.01091753964176,
6.97238029030133));
#264852=CARTESIAN_POINT('Ctrl Pts',(-1.22590920149169,-0.959734154720861,
6.9680656534008));
#264853=CARTESIAN_POINT('Ctrl Pts',(-1.3154604921601,-0.834765592845174,
6.95790059055422));
#264854=CARTESIAN_POINT('Ctrl Pts',(-1.36041206472146,-0.759305903550564,
6.95202242856061));
#264855=CARTESIAN_POINT('Ctrl Pts',(-1.403971165674,-0.669766280299547,
6.94506804150315));
#264856=CARTESIAN_POINT('Ctrl Pts',(-1.40905461392838,-0.659004541281474,
6.94423274570462));
#264857=CARTESIAN_POINT('Ctrl Pts',(-1.41707987438916,-0.641497476987945,
6.94287421868809));
#264858=CARTESIAN_POINT('Ctrl Pts',(-1.42009826241936,-0.634787606287648,
6.94235361754942));
#264859=CARTESIAN_POINT('Ctrl Pts',(-1.42537267035586,-0.622836701043467,
6.94142638720285));
#264860=CARTESIAN_POINT('Ctrl Pts',(-1.42764768549906,-0.617604153212343,
6.94102041464069));
#264861=CARTESIAN_POINT('Ctrl Pts',(-1.43236828068934,-0.606581294118535,
6.94016513852163));
#264862=CARTESIAN_POINT('Ctrl Pts',(-1.43480764956757,-0.600788452368654,
6.93971563284157));
#264863=CARTESIAN_POINT('Ctrl Pts',(-1.44114729873036,-0.585474656329408,
6.93852715202588));
#264864=CARTESIAN_POINT('Ctrl Pts',(-1.44498828118243,-0.575929655106208,
6.9377861945832));
#264865=CARTESIAN_POINT('Ctrl Pts',(-1.46240779871984,-0.531369994085493,
6.93432566127589));
#264866=CARTESIAN_POINT('Ctrl Pts',(-1.4748090098645,-0.49591186200197,
6.93156733891674));
#264867=CARTESIAN_POINT('Ctrl Pts',(-1.53046738830976,-0.316138069170886,
6.91754578495121));
#264868=CARTESIAN_POINT('Ctrl Pts',(-1.55387437704227,-0.166532381881811,
6.90565390303645));
#264869=CARTESIAN_POINT('Ctrl Pts',(-1.55547524062006,-0.0103886318065344,
6.89374573174244));
#264870=CARTESIAN_POINT('Ctrl Pts',(-1.55550243327175,-0.00483002150656961,
6.89332261268853));
#264871=CARTESIAN_POINT('Ctrl Pts',(-1.55549982932971,0.000728666766646221,
6.89290035850054));
#264872=CARTESIAN_POINT('Ctrl Pts',(1.43315705713258,0.600696421508238,
6.58835745434586));
#264873=CARTESIAN_POINT('Ctrl Pts',(1.29870118847464,0.914687993023714,
6.61276651483456));
#264874=CARTESIAN_POINT('Ctrl Pts',(0.70689197534916,1.60275587211439,6.6742275039151));
#264875=CARTESIAN_POINT('Ctrl Pts',(-0.852081690047566,1.62925752158921,
6.7727404215875));
#264876=CARTESIAN_POINT('Ctrl Pts',(-1.53450515466516,0.61017599513106,
6.85023095151808));
#264877=CARTESIAN_POINT('Ctrl Pts',(-1.55781672113823,0.0479304507923726,
6.89066955285682));
#264878=CARTESIAN_POINT('Ctrl Pts',(-1.55751602490984,0.000817960485851865,
6.89405622560371));
#264879=CARTESIAN_POINT('',(-1.55549951640608,-0.00134079452263982,6.75626891037593));
#264880=CARTESIAN_POINT('Ctrl Pts',(1.43457668334549,0.60130690134194,6.45155991302018));
#264881=CARTESIAN_POINT('Ctrl Pts',(1.42736364796658,0.618515505380319,
6.45285677086583));
#264882=CARTESIAN_POINT('Ctrl Pts',(1.41984071126925,0.635594942557183,
6.45413914262176));
#264883=CARTESIAN_POINT('Ctrl Pts',(1.34044988766294,0.807387152896391,
6.46703010256774));
#264884=CARTESIAN_POINT('Ctrl Pts',(1.24390481061379,0.949416472487348,
6.47775656379845));
#264885=CARTESIAN_POINT('Ctrl Pts',(1.12478115298201,1.07445425078909,6.48962931242059));
#264886=CARTESIAN_POINT('Ctrl Pts',(1.12334294696658,1.07595780706174,6.48977246789771));
#264887=CARTESIAN_POINT('Ctrl Pts',(1.10455265666818,1.09552316378153,6.49164040861345));
#264888=CARTESIAN_POINT('Ctrl Pts',(1.08677070458871,1.11316525595325,6.49338159815424));
#264889=CARTESIAN_POINT('Ctrl Pts',(1.06183692715151,1.13673588571189,6.49579275338506));
#264890=CARTESIAN_POINT('Ctrl Pts',(1.05504579303966,1.14304177599866,6.49644649928914));
#264891=CARTESIAN_POINT('Ctrl Pts',(1.04413300796446,1.1529947066736,6.49749255663191));
#264892=CARTESIAN_POINT('Ctrl Pts',(1.040047568465,1.15668128101585,6.49788319246831));
#264893=CARTESIAN_POINT('Ctrl Pts',(1.03161038509193,1.16421389465039,6.49868798350287));
#264894=CARTESIAN_POINT('Ctrl Pts',(1.02725649685429,1.16805739033491,6.49910223607983));
#264895=CARTESIAN_POINT('Ctrl Pts',(1.01710971179226,1.17691408920699,6.50006530675118));
#264896=CARTESIAN_POINT('Ctrl Pts',(1.01130114299623,1.18190902081393,6.50061486652449));
#264897=CARTESIAN_POINT('Ctrl Pts',(0.992679622734716,1.19768435022372,
6.50237132424888));
#264898=CARTESIAN_POINT('Ctrl Pts',(0.979729781961769,1.20830052130919,
6.50358483294207));
#264899=CARTESIAN_POINT('Ctrl Pts',(0.913324580904114,1.26096956222477,
6.50977010574473));
#264900=CARTESIAN_POINT('Ctrl Pts',(0.857331032259533,1.29968730097642,
6.51486986700256));
#264901=CARTESIAN_POINT('Ctrl Pts',(0.713250637645021,1.3859437523413,6.52770373386735));
#264902=CARTESIAN_POINT('Ctrl Pts',(0.622769007797595,1.42888895221082,
6.53553148005357));
#264903=CARTESIAN_POINT('Ctrl Pts',(0.51911339925616,1.46635860418252,6.54398248008834));
#264904=CARTESIAN_POINT('Ctrl Pts',(0.509395006342337,1.4697629103079,6.54476981505109));
#264905=CARTESIAN_POINT('Ctrl Pts',(0.463009340447153,1.48549623018356,
6.54850207613884));
#264906=CARTESIAN_POINT('Ctrl Pts',(0.425920608118182,1.49655235562314,
6.55141066086021));
#264907=CARTESIAN_POINT('Ctrl Pts',(0.382010178631786,1.50787690680752,
6.5547381475351));
#264908=CARTESIAN_POINT('Ctrl Pts',(0.375555019197983,1.5094975900748,6.55522440426853));
#264909=CARTESIAN_POINT('Ctrl Pts',(0.365077905219191,1.5120566874842,6.55600870752146));
#264910=CARTESIAN_POINT('Ctrl Pts',(0.361062357294251,1.51302058091003,
6.5563081390591));
#264911=CARTESIAN_POINT('Ctrl Pts',(0.35390621333556,1.51470823214912,6.55683962538624));
#264912=CARTESIAN_POINT('Ctrl Pts',(0.3507671671067,1.51543823086579,6.55707202990087));
#264913=CARTESIAN_POINT('Ctrl Pts',(0.343969443372104,1.51699681727166,
6.55757371893119));
#264914=CARTESIAN_POINT('Ctrl Pts',(0.340310034417461,1.5178219272582,6.55784280389447));
#264915=CARTESIAN_POINT('Ctrl Pts',(0.330058127270287,1.52009454899066,
6.55859397860941));
#264916=CARTESIAN_POINT('Ctrl Pts',(0.323459032658118,1.52151242645805,
6.55907441777574));
#264917=CARTESIAN_POINT('Ctrl Pts',(0.283967576647959,1.5297289881583,6.56193227462683));
#264918=CARTESIAN_POINT('Ctrl Pts',(0.250868261128905,1.53550444636292,
6.56425613363933));
#264919=CARTESIAN_POINT('Ctrl Pts',(0.046521088956556,1.56437525767921,
6.57831224024227));
#264920=CARTESIAN_POINT('Ctrl Pts',(-0.127397564425102,1.55987665963063,
6.5891687766805));
#264921=CARTESIAN_POINT('Ctrl Pts',(-0.321462024222304,1.52212410634915,
6.60278457595101));
#264922=CARTESIAN_POINT('Ctrl Pts',(-0.345772531017217,1.51678636097919,
6.60451489800401));
#264923=CARTESIAN_POINT('Ctrl Pts',(-0.378921775291969,1.50866960674231,
6.60691330690904));
#264924=CARTESIAN_POINT('Ctrl Pts',(-0.387880194449341,1.50639126466654,
6.60756539915968));
#264925=CARTESIAN_POINT('Ctrl Pts',(-0.402134019548054,1.5026305973321,
6.60860947540982));
#264926=CARTESIAN_POINT('Ctrl Pts',(-0.407442896471344,1.50119977565252,
6.60899979547739));
#264927=CARTESIAN_POINT('Ctrl Pts',(-0.418345622164745,1.49819923408625,
6.60980443324914));
#264928=CARTESIAN_POINT('Ctrl Pts',(-0.423938478027348,1.49662626255378,
6.61021885061083));
#264929=CARTESIAN_POINT('Ctrl Pts',(-0.4368995041676,1.49290253809984,6.6111831512814));
#264930=CARTESIAN_POINT('Ctrl Pts',(-0.444260773028511,1.49072852211365,
6.61173378227081));
#264931=CARTESIAN_POINT('Ctrl Pts',(-0.467124464799687,1.48379176121603,
6.61345340950718));
#264932=CARTESIAN_POINT('Ctrl Pts',(-0.482568248420444,1.47884113578744,
6.61462849091278));
#264933=CARTESIAN_POINT('Ctrl Pts',(-0.518624909398208,1.4666579594764,
6.61740484021058));
#264934=CARTESIAN_POINT('Ctrl Pts',(-0.539167956053008,1.45923102824412,
6.6190122249473));
#264935=CARTESIAN_POINT('Ctrl Pts',(-0.61172113015982,1.43125967582583,
6.62478252197996));
#264936=CARTESIAN_POINT('Ctrl Pts',(-0.662767142101544,1.40834849525905,
6.62901760050886));
#264937=CARTESIAN_POINT('Ctrl Pts',(-0.805636238460955,1.33473450397939,
6.64135282472932));
#264938=CARTESIAN_POINT('Ctrl Pts',(-0.893714272359956,1.27743504748951,
6.64957962180708));
#264939=CARTESIAN_POINT('Ctrl Pts',(-1.00275147222613,1.18966639630935,
6.66021633085421));
#264940=CARTESIAN_POINT('Ctrl Pts',(-1.02938985958108,1.16669346722089,
6.66285361299601));
#264941=CARTESIAN_POINT('Ctrl Pts',(-1.05999000382307,1.138439034368,6.66590847478991));
#264942=CARTESIAN_POINT('Ctrl Pts',(-1.06472364982352,1.13401313775313,
6.66638178559031));
#264943=CARTESIAN_POINT('Ctrl Pts',(-1.07238998807715,1.12675489037632,
6.66714935083362));
#264944=CARTESIAN_POINT('Ctrl Pts',(-1.07533938486133,1.12394042453737,
6.66744489768758));
#264945=CARTESIAN_POINT('Ctrl Pts',(-1.08059762100106,1.11888310018409,
6.66797219560122));
#264946=CARTESIAN_POINT('Ctrl Pts',(-1.08291058636913,1.11664464937999,
6.668204274092));
#264947=CARTESIAN_POINT('Ctrl Pts',(-1.08740207938593,1.11227077324681,
6.66865519817617));
#264948=CARTESIAN_POINT('Ctrl Pts',(-1.08958126134632,1.1101361315753,6.66887410067713));
#264949=CARTESIAN_POINT('Ctrl Pts',(-1.09585025457557,1.10395902869163,
6.66950423968003));
#264950=CARTESIAN_POINT('Ctrl Pts',(-1.09992400754824,1.09990022178073,
6.66991422425773));
#264951=CARTESIAN_POINT('Ctrl Pts',(-1.11869757792601,1.08098691574727,
6.67180650976796));
#264952=CARTESIAN_POINT('Ctrl Pts',(-1.13312048253265,1.06585884091123,
6.67326859409705));
#264953=CARTESIAN_POINT('Ctrl Pts',(-1.17305867459872,1.02224061320622,
6.67735749206441));
#264954=CARTESIAN_POINT('Ctrl Pts',(-1.19783561822219,0.993092552341752,
6.67994298350009));
#264955=CARTESIAN_POINT('Ctrl Pts',(-1.25855679429963,0.916075632111055,
6.68649708116946));
#264956=CARTESIAN_POINT('Ctrl Pts',(-1.29285867530171,0.866992930502283,
6.69041836967635));
#264957=CARTESIAN_POINT('Ctrl Pts',(-1.37997084549852,0.72563207510828,
6.70135419759506));
#264958=CARTESIAN_POINT('Ctrl Pts',(-1.42627666917936,0.629755019693429,
6.70839998321902));
#264959=CARTESIAN_POINT('Ctrl Pts',(-1.46650654768444,0.518729596602149,
6.71664778198961));
#264960=CARTESIAN_POINT('Ctrl Pts',(-1.4704317857451,0.507496008336282,
6.71748292678769));
#264961=CARTESIAN_POINT('Ctrl Pts',(-1.4765898541024,0.489200862225769,
6.71884463418445));
#264962=CARTESIAN_POINT('Ctrl Pts',(-1.47890186885667,0.482166298815238,
6.71936859154224));
#264963=CARTESIAN_POINT('Ctrl Pts',(-1.48292687951533,0.469618407404525,
6.72030399492354));
#264964=CARTESIAN_POINT('Ctrl Pts',(-1.48465958643075,0.464111505284981,
6.72071478693031));
#264965=CARTESIAN_POINT('Ctrl Pts',(-1.48824595880427,0.452487644748402,
6.72158251356072));
#264966=CARTESIAN_POINT('Ctrl Pts',(-1.49009265289354,0.446368666114793,
6.72203966699562));
#264967=CARTESIAN_POINT('Ctrl Pts',(-1.49376838642326,0.433912164038169,
6.72297112580997));
#264968=CARTESIAN_POINT('Ctrl Pts',(-1.49559492870028,0.427574046377751,
6.72344550199953));
#264969=CARTESIAN_POINT('Ctrl Pts',(-1.50002826236283,0.411814306676032,
6.7246261969643));
#264970=CARTESIAN_POINT('Ctrl Pts',(-1.50258662212174,0.40237948007269,
6.72533406332898));
#264971=CARTESIAN_POINT('Ctrl Pts',(-1.5095040387726,0.375882834090415,
6.7273251544176));
#264972=CARTESIAN_POINT('Ctrl Pts',(-1.51366241564198,0.358770668745993,
6.72861467932014));
#264973=CARTESIAN_POINT('Ctrl Pts',(-1.54286918620225,0.229019096079115,
6.73842229826593));
#264974=CARTESIAN_POINT('Ctrl Pts',(-1.55559877422798,0.113999451242998,
6.74732589837675));
#264975=CARTESIAN_POINT('Ctrl Pts',(-1.55549942292528,-0.00133988026452862,
6.75626900298645));
#264976=CARTESIAN_POINT('Ctrl Pts',(-1.55549942214842,-0.00134078183929962,
6.75626907289215));
#264977=CARTESIAN_POINT('Ctrl Pts',(-1.55542406061211,-0.0887709831925335,
6.76304817777256));
#264978=CARTESIAN_POINT('Ctrl Pts',(-1.54797750370825,-0.176053511463977,
6.76981111638233));
#264979=CARTESIAN_POINT('Ctrl Pts',(-1.53227353243141,-0.267862619476418,
6.77665509403429));
#264980=CARTESIAN_POINT('Ctrl Pts',(-1.53128442875315,-0.273460348044416,
6.77707126039852));
#264981=CARTESIAN_POINT('Ctrl Pts',(-1.52958837228819,-0.282761156806125,
6.77776073212102));
#264982=CARTESIAN_POINT('Ctrl Pts',(-1.52889861437371,-0.286467255018727,
6.77803493630822));
#264983=CARTESIAN_POINT('Ctrl Pts',(-1.52762537391392,-0.293172822163733,
6.77853005890441));
#264984=CARTESIAN_POINT('Ctrl Pts',(-1.52704651614358,-0.296173132900708,
6.77875122983635));
#264985=CARTESIAN_POINT('Ctrl Pts',(-1.52584008499915,-0.302328685466161,
6.77920421689561));
#264986=CARTESIAN_POINT('Ctrl Pts',(-1.52521157115125,-0.305483653691516,
6.77943596681603));
#264987=CARTESIAN_POINT('Ctrl Pts',(-1.52377009509107,-0.312604114455763,
6.77995806155847));
#264988=CARTESIAN_POINT('Ctrl Pts',(-1.52295144016092,-0.316568392267801,
6.78024807961978));
#264989=CARTESIAN_POINT('Ctrl Pts',(-1.52043416371531,-0.328522331506228,
6.78112075071142));
#264990=CARTESIAN_POINT('Ctrl Pts',(-1.51868804075455,-0.33650202237091,
6.78170078783826));
#264991=CARTESIAN_POINT('Ctrl Pts',(-1.50010832170874,-0.418318627315836,
6.7876257421574));
#264992=CARTESIAN_POINT('Ctrl Pts',(-1.4779638882258,-0.490858206746161,
6.79269476745083));
#264993=CARTESIAN_POINT('Ctrl Pts',(-1.42975813781908,-0.615395146280879,
6.80152888825742));
#264994=CARTESIAN_POINT('Ctrl Pts',(-1.40591156335138,-0.668081036752133,
6.80531088671053));
#264995=CARTESIAN_POINT('Ctrl Pts',(-1.34488506924146,-0.785090540428699,
6.81403720897344));
#264996=CARTESIAN_POINT('Ctrl Pts',(-1.30592450511069,-0.848317269759493,
6.81899829000765));
#264997=CARTESIAN_POINT('Ctrl Pts',(-1.24967850604569,-0.926484625750097,
6.8256513668287));
#264998=CARTESIAN_POINT('Ctrl Pts',(-1.23636979593911,-0.944171474002994,
6.82719367026841));
#264999=CARTESIAN_POINT('Ctrl Pts',(-1.21860185400942,-0.966764439633387,
6.82921570760253));
#265000=CARTESIAN_POINT('Ctrl Pts',(-1.21448184658903,-0.971935081283433,
6.82968209512258));
#265001=CARTESIAN_POINT('Ctrl Pts',(-1.2063075296743,-0.982060783460762,
6.83060269910703));
#265002=CARTESIAN_POINT('Ctrl Pts',(-1.20225534038524,-0.987017392374869,
6.83105682521746));
#265003=CARTESIAN_POINT('Ctrl Pts',(-1.19449268146211,-0.996393890818971,
6.8319226446484));
#265004=CARTESIAN_POINT('Ctrl Pts',(-1.19078797909769,-1.00081843454054,
6.8323340994998));
#265005=CARTESIAN_POINT('Ctrl Pts',(-1.18228615972498,-1.01085816439156,
6.83327443050409));
#265006=CARTESIAN_POINT('Ctrl Pts',(-1.17747353227078,-1.0164599693611,
6.83380393687924));
#265007=CARTESIAN_POINT('Ctrl Pts',(-1.16484554529409,-1.03094866997374,
6.83518627327986));
#265008=CARTESIAN_POINT('Ctrl Pts',(-1.1569684640822,-1.0397808727059,6.83604164962985));
#265009=CARTESIAN_POINT('Ctrl Pts',(-1.09613056009097,-1.10644826859371,
6.84259752373628));
#265010=CARTESIAN_POINT('Ctrl Pts',(-1.03897406707593,-1.16028405762339,
6.84847809352742));
#265011=CARTESIAN_POINT('Ctrl Pts',(-0.906068315858519,-1.26774612903609,
6.86156960601368));
#265012=CARTESIAN_POINT('Ctrl Pts',(-0.829082082361456,-1.3193793267871,
6.86880720546502));
#265013=CARTESIAN_POINT('Ctrl Pts',(-0.717326181869039,-1.38066816991362,
6.8785934699848));
#265014=CARTESIAN_POINT('Ctrl Pts',(-0.686125915325519,-1.39643583182716,
6.88125293451276));
#265015=CARTESIAN_POINT('Ctrl Pts',(-0.636560140915106,-1.41942205170845,
6.88533985310382));
#265016=CARTESIAN_POINT('Ctrl Pts',(-0.618544707175861,-1.42736481544873,
6.88679769713944));
#265017=CARTESIAN_POINT('Ctrl Pts',(-0.595253848761335,-1.43710960264431,
6.88864304755565));
#265018=CARTESIAN_POINT('Ctrl Pts',(-0.590113880236908,-1.43922783649988,
6.88904786030592));
#265019=CARTESIAN_POINT('Ctrl Pts',(-0.582142460661991,-1.44246305618098,
6.88967179880626));
#265020=CARTESIAN_POINT('Ctrl Pts',(-0.579318973528266,-1.44359933509804,
6.88989205012515));
#265021=CARTESIAN_POINT('Ctrl Pts',(-0.573499579563226,-1.44592145830078,
6.8903444370472));
#265022=CARTESIAN_POINT('Ctrl Pts',(-0.570503361138275,-1.44710626652208,
6.89057649990763));
#265023=CARTESIAN_POINT('Ctrl Pts',(-0.563667641530295,-1.44978481574006,
6.89110401104251));
#265024=CARTESIAN_POINT('Ctrl Pts',(-0.559825875760635,-1.45127261806413,
6.89139910277527));
#265025=CARTESIAN_POINT('Ctrl Pts',(-0.549793038126816,-1.45511227211957,
6.89216627057087));
#265026=CARTESIAN_POINT('Ctrl Pts',(-0.543592691746166,-1.45743991260658,
6.89263695144555));
#265027=CARTESIAN_POINT('Ctrl Pts',(-0.501703795651539,-1.47286069798531,
6.89579497216544));
#265028=CARTESIAN_POINT('Ctrl Pts',(-0.46555689445601,-1.48468269548983,
6.8984136264371));
#265029=CARTESIAN_POINT('Ctrl Pts',(-0.420054569411901,-1.49773869614989,
6.90162168801619));
#265030=CARTESIAN_POINT('Ctrl Pts',(-0.411076558086052,-1.50022768692937,
6.90225044801685));
#265031=CARTESIAN_POINT('Ctrl Pts',(-0.259385083996849,-1.54081741856284,
6.91281121068327));
#265032=CARTESIAN_POINT('Ctrl Pts',(-0.111985542306284,-1.55848057479781,
6.92221832751334));
#265033=CARTESIAN_POINT('Ctrl Pts',(0.0690446190827033,-1.55432480770115,
6.93459354645539));
#265034=CARTESIAN_POINT('Ctrl Pts',(0.102354712595635,-1.55248703731043,
6.93690059672432));
#265035=CARTESIAN_POINT('Ctrl Pts',(0.145152533173765,-1.54874251088973,
6.93991546402861));
#265036=CARTESIAN_POINT('Ctrl Pts',(0.154718873959221,-1.54781610199424,
6.94059261513072));
#265037=CARTESIAN_POINT('Ctrl Pts',(0.170629645649542,-1.54612632096563,
6.94172456580286));
#265038=CARTESIAN_POINT('Ctrl Pts',(0.176979158084729,-1.54541238889452,
6.9421778105535));
#265039=CARTESIAN_POINT('Ctrl Pts',(0.189057317595645,-1.54397892295273,
6.94304295589299));
#265040=CARTESIAN_POINT('Ctrl Pts',(0.194786723712315,-1.54326657271953,
6.94345462385947));
#265041=CARTESIAN_POINT('Ctrl Pts',(0.207858741765374,-1.54156734549442,
6.94439685641547));
#265042=CARTESIAN_POINT('Ctrl Pts',(0.215198485994634,-1.5405598804762,
6.94492806061016));
#265043=CARTESIAN_POINT('Ctrl Pts',(0.234320339342767,-1.53779586741691,
6.94631774691426));
#265044=CARTESIAN_POINT('Ctrl Pts',(0.246089762117461,-1.53595636838536,
6.94717882004342));
#265045=CARTESIAN_POINT('Ctrl Pts',(0.362470814006211,-1.51639466813727,
6.95575211592624));
#265046=CARTESIAN_POINT('Ctrl Pts',(0.465008717111574,-1.48815186590056,
6.96380569461293));
#265047=CARTESIAN_POINT('Ctrl Pts',(0.641150984790634,-1.41964222218781,
6.97842215571859));
#265048=CARTESIAN_POINT('Ctrl Pts',(0.715920133943383,-1.38344422793985,
6.98489615127094));
#265049=CARTESIAN_POINT('Ctrl Pts',(0.817169494143555,-1.32400980897541,
6.99380873929622));
#265050=CARTESIAN_POINT('Ctrl Pts',(0.846305289703434,-1.30557871142229,
6.99639069397384));
#265051=CARTESIAN_POINT('Ctrl Pts',(0.880427828268098,-1.28237018621743,
6.99941483807776));
#265052=CARTESIAN_POINT('Ctrl Pts',(0.886023439824617,-1.2785104316846,
6.99991075757306));
#265053=CARTESIAN_POINT('Ctrl Pts',(0.894676066689899,-1.27245791107993,
7.00067739409668));
#265054=CARTESIAN_POINT('Ctrl Pts',(0.897750640820932,-1.27029059175353,
7.00094976353715));
#265055=CARTESIAN_POINT('Ctrl Pts',(0.903443768448993,-1.26624641600661,
7.00145398002501));
#265056=CARTESIAN_POINT('Ctrl Pts',(0.906064331919369,-1.26437259364856,
7.00168601771242));
#265057=CARTESIAN_POINT('Ctrl Pts',(0.912018893128433,-1.26008679097672,
7.00221316009567));
#265058=CARTESIAN_POINT('Ctrl Pts',(0.915349151790441,-1.25766971561904,
7.00250791024947));
#265059=CARTESIAN_POINT('Ctrl Pts',(0.924001119187815,-1.25133761568002,
7.00327360038148));
#265060=CARTESIAN_POINT('Ctrl Pts',(0.929307620550339,-1.24740179860647,
7.00374315395292));
#265061=CARTESIAN_POINT('Ctrl Pts',(0.964709381324021,-1.22079311296761,
7.00687650154718));
#265062=CARTESIAN_POINT('Ctrl Pts',(0.994000345917764,-1.19706470475705,
7.00947282622629));
#265063=CARTESIAN_POINT('Ctrl Pts',(1.1347085111601,-1.0743475660386,7.02212957897043));
#265064=CARTESIAN_POINT('Ctrl Pts',(1.23236022889502,-0.960770979524193,
7.03158855237073));
#265065=CARTESIAN_POINT('Ctrl Pts',(1.32675847905031,-0.812410522510614,
7.04353423970992));
#265066=CARTESIAN_POINT('Ctrl Pts',(1.34056179585364,-0.789425648698518,
7.04537209575693));
#265067=CARTESIAN_POINT('Ctrl Pts',(1.36324602177683,-0.749340520580184,
7.04856496693988));
#265068=CARTESIAN_POINT('Ctrl Pts',(1.37241603328718,-0.732410476557945,
7.0499098137681));
#265069=CARTESIAN_POINT('Ctrl Pts',(1.38499413251151,-0.708122247654651,
7.05183624861529));
#265070=CARTESIAN_POINT('Ctrl Pts',(1.38866284015097,-0.700900404222524,
7.05240868918543));
#265071=CARTESIAN_POINT('Ctrl Pts',(1.39489713048349,-0.688387117170729,
7.05340009949497));
#265072=CARTESIAN_POINT('Ctrl Pts',(1.39748944876384,-0.683109117621849,
7.05381812868427));
#265073=CARTESIAN_POINT('Ctrl Pts',(1.40240011178259,-0.672965987145075,
7.054621284566));
#265074=CARTESIAN_POINT('Ctrl Pts',(1.40472322609171,-0.668103248094057,
7.0550062386791));
#265075=CARTESIAN_POINT('Ctrl Pts',(1.41012281025365,-0.656648180570069,
7.05591291528658));
#265076=CARTESIAN_POINT('Ctrl Pts',(1.41317837217083,-0.650046196926284,
7.05643534891474));
#265077=CARTESIAN_POINT('Ctrl Pts',(1.42358928812409,-0.627131557897748,
7.05824841579472));
#265078=CARTESIAN_POINT('Ctrl Pts',(1.43070913907085,-0.610714140918362,
7.05954701895264));
#265079=CARTESIAN_POINT('Ctrl Pts',(1.48548617045424,-0.478187581895869,
7.07003102146907));
#265080=CARTESIAN_POINT('Ctrl Pts',(1.51920425457528,-0.356844221990392,
7.0796947388204));
#265081=CARTESIAN_POINT('Ctrl Pts',(1.54593906630705,-0.180223371577389,
7.0935459493728));
#265082=CARTESIAN_POINT('Ctrl Pts',(1.55119672392109,-0.127268864418318,
7.09766363105027));
#265083=CARTESIAN_POINT('Ctrl Pts',(1.55548881281783,-0.0373288627441701,
7.10451216913307));
#265084=CARTESIAN_POINT('Ctrl Pts',(1.55593676981206,-0.00045633274773518,
7.10727837327658));
#265085=CARTESIAN_POINT('Ctrl Pts',(1.55491207236157,0.0433196824626526,
7.11048814905978));
#265086=CARTESIAN_POINT('Ctrl Pts',(1.55470393780829,0.0502376176737323,
7.1109931767934));
#265087=CARTESIAN_POINT('Ctrl Pts',(1.55431043866859,0.0609398164856241,
7.11177080789822));
#265088=CARTESIAN_POINT('Ctrl Pts',(1.55415741421752,0.0647250620030301,
7.11204513871522));
#265089=CARTESIAN_POINT('Ctrl Pts',(1.5538487872311,0.07172557385834,7.11255113535687));
#265090=CARTESIAN_POINT('Ctrl Pts',(1.5536970342818,0.0749408938002778,
7.11278300378511));
#265091=CARTESIAN_POINT('Ctrl Pts',(1.55333035531211,0.0822295222501443,
7.11330741894152));
#265092=CARTESIAN_POINT('Ctrl Pts',(1.55310938838683,0.0863024669016945,
7.11359962603701));
#265093=CARTESIAN_POINT('Ctrl Pts',(1.55249548642105,0.0968509159461085,
7.11435434134753));
#265094=CARTESIAN_POINT('Ctrl Pts',(1.55207805314158,0.103325002420016,
7.11481552756932));
#265095=CARTESIAN_POINT('Ctrl Pts',(1.54912856434855,0.145006556759354,
7.11777284290209));
#265096=CARTESIAN_POINT('Ctrl Pts',(1.54543897428523,0.180125158876393,
7.12020985217078));
#265097=CARTESIAN_POINT('Ctrl Pts',(1.53803873330106,0.233128265713526,
7.12384636490497));
#265098=CARTESIAN_POINT('Ctrl Pts',(1.53520372741407,0.251120474114648,
7.12507346123859));
#265099=CARTESIAN_POINT('Ctrl Pts',(1.52292842849498,0.321017374935997,
7.12982605222567));
#265100=CARTESIAN_POINT('Ctrl Pts',(1.51116591693839,0.372479776320444,
7.13329485088506));
#265101=CARTESIAN_POINT('Ctrl Pts',(1.4796724576334,0.483856277205171,7.14091293977094));
#265102=CARTESIAN_POINT('Ctrl Pts',(1.45888357768414,0.543316423205788,
7.14505442302371));
#265103=CARTESIAN_POINT('Ctrl Pts',(1.43457650415244,0.601307328854198,
7.14927790964297));
#265104=CARTESIAN_POINT('Origin',(0.,0.,-1.29405622560371));
#265105=CARTESIAN_POINT('',(1.43457668592364,0.601306895191089,7.98692484967426));
#265106=CARTESIAN_POINT('',(1.43457666579773,0.601306943206762,7.84913521677167));
#265107=CARTESIAN_POINT('',(1.43457668357355,0.601306900797845,-1.29405622560371));
#265108=CARTESIAN_POINT('Ctrl Pts',(1.43457668592364,0.601306895191089,
7.98692484967426));
#265109=CARTESIAN_POINT('Ctrl Pts',(1.4484903359964,0.568112201815517,7.98444320077674));
#265110=CARTESIAN_POINT('Ctrl Pts',(1.46125114251322,0.534436261602293,
7.98201129489878));
#265111=CARTESIAN_POINT('Ctrl Pts',(1.51632301583225,0.372322798635339,
7.97057171645316));
#265112=CARTESIAN_POINT('Ctrl Pts',(1.54293548610503,0.239187956891495,
7.96190572417245));
#265113=CARTESIAN_POINT('Ctrl Pts',(1.55443513335324,0.0680494455109081,
7.95021155000991));
#265114=CARTESIAN_POINT('Ctrl Pts',(1.55560003676253,0.0317408277435369,
7.94770345237973));
#265115=CARTESIAN_POINT('Ctrl Pts',(1.55546336579658,-0.0147475571720663,
7.94444182936921));
#265116=CARTESIAN_POINT('Ctrl Pts',(1.55533362640663,-0.0249213681375513,
7.94372497744379));
#265117=CARTESIAN_POINT('Ctrl Pts',(1.55496285388788,-0.0413517238984559,
7.94256201781539));
#265118=CARTESIAN_POINT('Ctrl Pts',(1.55478383588616,-0.0476094909004445,
7.94211785127168));
#265119=CARTESIAN_POINT('Ctrl Pts',(1.55436924002932,-0.0595747001656667,
7.94126613811837));
#265120=CARTESIAN_POINT('Ctrl Pts',(1.55413998810361,-0.0652822719111739,
7.94085879608236));
#265121=CARTESIAN_POINT('Ctrl Pts',(1.55354685010361,-0.078265591668855,
7.93992970910407));
#265122=CARTESIAN_POINT('Ctrl Pts',(1.55316328151474,-0.0855402590273948,
7.93940735707378));
#265123=CARTESIAN_POINT('Ctrl Pts',(1.55201724681829,-0.104713251272965,
7.93802583144157));
#265124=CARTESIAN_POINT('Ctrl Pts',(1.55116906911848,-0.11660576185849,
7.93716400149181));
#265125=CARTESIAN_POINT('Ctrl Pts',(1.54263816321354,-0.219530350653884,
7.92966112478029));
#265126=CARTESIAN_POINT('Ctrl Pts',(1.52708790129757,-0.309714086254081,
7.92277153388331));
#265127=CARTESIAN_POINT('Ctrl Pts',(1.48792472941349,-0.457680949966964,
7.91098407923764));
#265128=CARTESIAN_POINT('Ctrl Pts',(1.46858901422948,-0.516369892297193,
7.90617844004671));
#265129=CARTESIAN_POINT('Ctrl Pts',(1.42269008746057,-0.632032078818221,
7.89655816682876));
#265130=CARTESIAN_POINT('Ctrl Pts',(1.39605716109568,-0.688867094774696,
7.89175328311457));
#265131=CARTESIAN_POINT('Ctrl Pts',(1.36035606595042,-0.754422945728574,
7.88622983645625));
#265132=CARTESIAN_POINT('Ctrl Pts',(1.35452908330613,-0.76483566405017,
7.88535317364935));
#265133=CARTESIAN_POINT('Ctrl Pts',(1.34624942920058,-0.779239786077756,
7.88414245658443));
#265134=CARTESIAN_POINT('Ctrl Pts',(1.3438978763913,-0.783288369120164,
7.88380238047899));
#265135=CARTESIAN_POINT('Ctrl Pts',(1.33987152789863,-0.790148878032278,
7.88322656256454));
#265136=CARTESIAN_POINT('Ctrl Pts',(1.33820608510347,-0.792966225833744,
7.88299022825843));
#265137=CARTESIAN_POINT('Ctrl Pts',(1.33499378199385,-0.798361377661278,
7.88253793627869));
#265138=CARTESIAN_POINT('Ctrl Pts',(1.33344833169778,-0.800939969296144,
7.88232188687473));
#265139=CARTESIAN_POINT('Ctrl Pts',(1.32973590387375,-0.807093645464354,
7.88180654684937));
#265140=CARTESIAN_POINT('Ctrl Pts',(1.32756195490934,-0.810664532074981,
7.88150770589522));
#265141=CARTESIAN_POINT('Ctrl Pts',(1.31971501779874,-0.823437539563362,
7.88043932172574));
#265142=CARTESIAN_POINT('Ctrl Pts',(1.31396035915565,-0.832589515672145,
7.87967487155107));
#265143=CARTESIAN_POINT('Ctrl Pts',(1.24525467391682,-0.939369426124861,
7.87075886489449));
#265144=CARTESIAN_POINT('Ctrl Pts',(1.17164260428635,-1.02972668702184,
7.86322724283071));
#265145=CARTESIAN_POINT('Ctrl Pts',(1.01627665008431,-1.18195865824474,
7.84889218010191));
#265146=CARTESIAN_POINT('Ctrl Pts',(0.93716956593279,-1.24561354629004,
7.84215103890584));
#265147=CARTESIAN_POINT('Ctrl Pts',(0.841555827145406,-1.30825589206276,
7.83416536255652));
#265148=CARTESIAN_POINT('Ctrl Pts',(0.830578836038413,-1.31525224513411,
7.83325114060816));
#265149=CARTESIAN_POINT('Ctrl Pts',(0.813672050998817,-1.32573199055336,
7.83184627477718));
#265150=CARTESIAN_POINT('Ctrl Pts',(0.807804618642334,-1.3293153172613,
7.83135930643416));
#265151=CARTESIAN_POINT('Ctrl Pts',(0.79753186809214,-1.33549590794552,
7.83050763376491));
#265152=CARTESIAN_POINT('Ctrl Pts',(0.793137102364446,-1.33811058454446,
7.83014357080237));
#265153=CARTESIAN_POINT('Ctrl Pts',(0.783207544126694,-1.343952096949,7.82932160713624));
#265154=CARTESIAN_POINT('Ctrl Pts',(0.77766557730404,-1.34716648699303,
7.82886326424046));
#265155=CARTESIAN_POINT('Ctrl Pts',(0.762694701399174,-1.35572656615261,
7.82762613312845));
#265156=CARTESIAN_POINT('Ctrl Pts',(0.753229667836946,-1.36100800370388,
7.82684506106099));
#265157=CARTESIAN_POINT('Ctrl Pts',(0.709646099979314,-1.38473351386116,
7.82325268350788));
#265158=CARTESIAN_POINT('Ctrl Pts',(0.674903213385856,-1.401994882431,7.82040023457189));
#265159=CARTESIAN_POINT('Ctrl Pts',(0.496623167178186,-1.48240722903888,
7.80580461695882));
#265160=CARTESIAN_POINT('Ctrl Pts',(0.344802928880277,-1.52488064767716,
7.79338364404336));
#265161=CARTESIAN_POINT('Ctrl Pts',(0.156776018803869,-1.54792438909802,
7.77902478567505));
#265162=CARTESIAN_POINT('Ctrl Pts',(0.12421220902423,-1.55087728726743,
7.77657922809565));
#265163=CARTESIAN_POINT('Ctrl Pts',(0.0849470063881252,-1.55319295690233,
7.7736977351942));
#265164=CARTESIAN_POINT('Ctrl Pts',(0.0783147489128923,-1.55354148951048,
7.77321333429218));
#265165=CARTESIAN_POINT('Ctrl Pts',(0.0679851028948251,-1.55401800483553,
7.77246268840421));
#265166=CARTESIAN_POINT('Ctrl Pts',(0.064289252963008,-1.55417528815055,
7.77219487161495));
#265167=CARTESIAN_POINT('Ctrl Pts',(0.0574129588258846,-1.55444335023006,
7.77169803797595));
#265168=CARTESIAN_POINT('Ctrl Pts',(0.0542327646099745,-1.55455755264304,
7.7714688415151));
#265169=CARTESIAN_POINT('Ctrl Pts',(0.0469744318787375,-1.55479590250337,
7.77094704166991));
#265170=CARTESIAN_POINT('Ctrl Pts',(0.0428961428320419,-1.55491376534127,
7.77065479132075));
#265171=CARTESIAN_POINT('Ctrl Pts',(0.0322411489464894,-1.55517974266837,
7.76989358968594));
#265172=CARTESIAN_POINT('Ctrl Pts',(0.0256637941083301,-1.55530218845769,
7.76942602191656));
#265173=CARTESIAN_POINT('Ctrl Pts',(-0.0191120575347989,-1.5558516215098,
7.76625761562317));
#265174=CARTESIAN_POINT('Ctrl Pts',(-0.0573181555389714,-1.55491310732951,
7.76362631915188));
#265175=CARTESIAN_POINT('Ctrl Pts',(-0.243697359489083,-1.543454180537,
7.75097367563435));
#265176=CARTESIAN_POINT('Ctrl Pts',(-0.389874003196824,-1.51315690462803,
7.74154475309823));
#265177=CARTESIAN_POINT('Ctrl Pts',(-0.554886744404079,-1.45341230531076,
7.72962467096044));
#265178=CARTESIAN_POINT('Ctrl Pts',(-0.579984266073731,-1.4435805283024,
7.72777716468133));
#265179=CARTESIAN_POINT('Ctrl Pts',(-0.622581294392751,-1.4256032907814,
7.72457213111181));
#265180=CARTESIAN_POINT('Ctrl Pts',(-0.640208273143459,-1.41777484826615,
7.72322496936125));
#265181=CARTESIAN_POINT('Ctrl Pts',(-0.664975222466122,-1.40621937454652,
7.72130003448778));
#265182=CARTESIAN_POINT('Ctrl Pts',(-0.672239329712773,-1.40276129653536,
7.72073148345927));
#265183=CARTESIAN_POINT('Ctrl Pts',(-0.684706589668946,-1.39670717923464,
7.71974865975055));
#265184=CARTESIAN_POINT('Ctrl Pts',(-0.689922667784157,-1.39413800223002,
7.71933532465271));
#265185=CARTESIAN_POINT('Ctrl Pts',(-0.699875088446938,-1.38916640987235,
7.71854250394612));
#265186=CARTESIAN_POINT('Ctrl Pts',(-0.704613781951205,-1.3867688598829,
7.71816319296184));
#265187=CARTESIAN_POINT('Ctrl Pts',(-0.715695166034011,-1.3810907539711,
7.71727184466424));
#265188=CARTESIAN_POINT('Ctrl Pts',(-0.722027681939302,-1.37779071877645,
7.71675912804184));
#265189=CARTESIAN_POINT('Ctrl Pts',(-0.743728774016894,-1.36629103287496,
7.71499035452341));
#265190=CARTESIAN_POINT('Ctrl Pts',(-0.758981695200941,-1.357877172766,
7.71372676072522));
#265191=CARTESIAN_POINT('Ctrl Pts',(-0.903270818546592,-1.27509334835873,
7.7015721810353));
#265192=CARTESIAN_POINT('Ctrl Pts',(-1.0211140946012,-1.18282131655117,
7.68997794583094));
#265193=CARTESIAN_POINT('Ctrl Pts',(-1.16573200959568,-1.03164476795007,
7.67381614680732));
#265194=CARTESIAN_POINT('Ctrl Pts',(-1.20487961982564,-0.985641336427132,
7.66919820917181));
#265195=CARTESIAN_POINT('Ctrl Pts',(-1.24831497998684,-0.928130945372148,
7.66386735198637));
#265196=CARTESIAN_POINT('Ctrl Pts',(-1.25526612206363,-0.918707965513631,
7.66300727902685));
#265197=CARTESIAN_POINT('Ctrl Pts',(-1.26482664167549,-0.90543658544346,
7.66181548120623));
#265198=CARTESIAN_POINT('Ctrl Pts',(-1.26752594902065,-0.901653932402147,
7.66147797555259));
#265199=CARTESIAN_POINT('Ctrl Pts',(-1.27209353211102,-0.895192137311736,
7.66090521043141));
#265200=CARTESIAN_POINT('Ctrl Pts',(-1.27397038085016,-0.892519123977094,
7.66066937316643));
#265201=CARTESIAN_POINT('Ctrl Pts',(-1.27756312786667,-0.887367899797427,
7.66021701520931));
#265202=CARTESIAN_POINT('Ctrl Pts',(-1.27928025122308,-0.884890600317002,
7.66000040771928));
#265203=CARTESIAN_POINT('Ctrl Pts',(-1.28337878888532,-0.878940762208461,
7.65948237489491));
#265204=CARTESIAN_POINT('Ctrl Pts',(-1.28575334300132,-0.875463489417652,
7.65918140991428));
#265205=CARTESIAN_POINT('Ctrl Pts',(-1.29428883190386,-0.862854571490478,
7.6580963667929));
#265206=CARTESIAN_POINT('Ctrl Pts',(-1.30036703847048,-0.853666899575775,
7.65731759472373));
#265207=CARTESIAN_POINT('Ctrl Pts',(-1.36838130548613,-0.748445831285959,
7.64852315279615));
#265208=CARTESIAN_POINT('Ctrl Pts',(-1.41966190567854,-0.645916061713906,
7.64110544999641));
#265209=CARTESIAN_POINT('Ctrl Pts',(-1.49487787601367,-0.442159977318249,
7.6267953288364));
#265210=CARTESIAN_POINT('Ctrl Pts',(-1.52083831292748,-0.342361535955896,
7.61995605885141));
#265211=CARTESIAN_POINT('Ctrl Pts',(-1.53877546691929,-0.22786020952655,
7.61185946083534));
#265212=CARTESIAN_POINT('Ctrl Pts',(-1.54063110139788,-0.214955818453811,
7.61094384646689));
#265213=CARTESIAN_POINT('Ctrl Pts',(-1.54321775922033,-0.195208920423094,
7.60953728221444));
#265214=CARTESIAN_POINT('Ctrl Pts',(-1.5440659790193,-0.188382124067505,
7.60905002182774));
#265215=CARTESIAN_POINT('Ctrl Pts',(-1.54546577691489,-0.176470783312541,
7.60819802898854));
#265216=CARTESIAN_POINT('Ctrl Pts',(-1.54603761988124,-0.171388686163955,
7.60783393950662));
#265217=CARTESIAN_POINT('Ctrl Pts',(-1.5472690277887,-0.159936903911657,
7.60701216700153));
#265218=CARTESIAN_POINT('Ctrl Pts',(-1.54791433749113,-0.153565813610403,
7.60655404306999));
#265219=CARTESIAN_POINT('Ctrl Pts',(-1.54954462222545,-0.136414433117057,
7.60531811971433));
#265220=CARTESIAN_POINT('Ctrl Pts',(-1.55045641628011,-0.125627719988751,
7.60453804413628));
#265221=CARTESIAN_POINT('Ctrl Pts',(-1.55410823177456,-0.0762959265605068,
7.60095704199649));
#265222=CARTESIAN_POINT('Ctrl Pts',(-1.55552369452298,-0.0376697688026779,
7.59811528973775));
#265223=CARTESIAN_POINT('Ctrl Pts',(-1.55540688544925,0.150416635516563,
7.58408028982375));
#265224=CARTESIAN_POINT('Ctrl Pts',(-1.53377345062266,0.299066134190454,
7.57227920445095));
#265225=CARTESIAN_POINT('Ctrl Pts',(-1.48021912918154,0.479632940477266,
7.55792515932282));
#265226=CARTESIAN_POINT('Ctrl Pts',(-1.46774814891127,0.51653889492002,
7.55499703045648));
#265227=CARTESIAN_POINT('Ctrl Pts',(-1.45154947782828,0.55913167113645,
7.55165343608403));
#265228=CARTESIAN_POINT('Ctrl Pts',(-1.44915565021815,0.565307012043805,
7.55116956610826));
#265229=CARTESIAN_POINT('Ctrl Pts',(-1.44521858207372,0.575274069562436,
7.55039027216243));
#265230=CARTESIAN_POINT('Ctrl Pts',(-1.44369972204418,0.579075227144306,
7.55009346803085));
#265231=CARTESIAN_POINT('Ctrl Pts',(-1.44097297017293,0.585821887140048,
7.549567433638));
#265232=CARTESIAN_POINT('Ctrl Pts',(-1.4397710258027,0.588769715745958,
7.5493378552839));
#265233=CARTESIAN_POINT('Ctrl Pts',(-1.43715635942363,0.595126426887807,
7.54884336836737));
#265234=CARTESIAN_POINT('Ctrl Pts',(-1.4357405569223,0.598533975132536,
7.54857864854596));
#265235=CARTESIAN_POINT('Ctrl Pts',(-1.43175906701959,0.608021190500929,
7.54784251799717));
#265236=CARTESIAN_POINT('Ctrl Pts',(-1.42916675767156,0.614089714134972,
7.54737267936209));
#265237=CARTESIAN_POINT('Ctrl Pts',(-1.4137968856831,0.649445622806684,
7.54464031872284));
#265238=CARTESIAN_POINT('Ctrl Pts',(-1.40015682304061,0.678352780941315,
7.54242630705351));
#265239=CARTESIAN_POINT('Ctrl Pts',(-1.31926184017515,0.836937168853864,
7.53027955017825));
#265240=CARTESIAN_POINT('Ctrl Pts',(-1.23489001193914,0.957063538313597,
7.52101017719817));
#265241=CARTESIAN_POINT('Ctrl Pts',(-1.10166319482847,1.09922410818106,
7.50786412318238));
#265242=CARTESIAN_POINT('Ctrl Pts',(-1.06668764609383,1.13319552506213,
7.50452525525777));
#265243=CARTESIAN_POINT('Ctrl Pts',(-1.02154822820113,1.17309510832862,
7.50030817755837));
#265244=CARTESIAN_POINT('Ctrl Pts',(-1.01283400866784,1.18062702577618,
7.49949811776615));
#265245=CARTESIAN_POINT('Ctrl Pts',(-0.998977887428836,1.19233691020467,
7.4982159153385));
#265246=CARTESIAN_POINT('Ctrl Pts',(-0.993891436302199,1.1965801007002,
7.49774644674226));
#265247=CARTESIAN_POINT('Ctrl Pts',(-0.984448981794201,1.20435538824518,
7.4968770678271));
#265248=CARTESIAN_POINT('Ctrl Pts',(-0.980100661277052,1.20789668068229,
7.49647753857119));
#265249=CARTESIAN_POINT('Ctrl Pts',(-0.97041495948219,1.21569802645794,
7.49558936661091));
#265250=CARTESIAN_POINT('Ctrl Pts',(-0.965068509004436,1.21994657886965,
7.4951002742896));
#265251=CARTESIAN_POINT('Ctrl Pts',(-0.94962358502861,1.23205480764965,
7.49369060207251));
#265252=CARTESIAN_POINT('Ctrl Pts',(-0.939456083731016,1.23982508880584,
7.49276652264346));
#265253=CARTESIAN_POINT('Ctrl Pts',(-0.858021967181582,1.30048239965521,
7.48539426721553));
#265254=CARTESIAN_POINT('Ctrl Pts',(-0.782457311706423,1.34729779674673,
7.47871271480738));
#265255=CARTESIAN_POINT('Ctrl Pts',(-0.617249944267438,1.43104726627118,
7.46446618506832));
#265256=CARTESIAN_POINT('Ctrl Pts',(-0.527299781985503,1.4665771805919,
7.45690437412503));
#265257=CARTESIAN_POINT('Ctrl Pts',(-0.397943811212079,1.50422120406867,
7.44664242473013));
#265258=CARTESIAN_POINT('Ctrl Pts',(-0.360865070993057,1.51354474945307,
7.44377009301013));
#265259=CARTESIAN_POINT('Ctrl Pts',(-0.317041739816991,1.52286180224509,
7.44048306877063));
#265260=CARTESIAN_POINT('Ctrl Pts',(-0.310597780899483,1.52418914709239,
7.44000244062227));
#265261=CARTESIAN_POINT('Ctrl Pts',(-0.300144060798938,1.52627338320887,
7.4392273325203));
#265262=CARTESIAN_POINT('Ctrl Pts',(-0.296139492547621,1.52705543432753,
7.43893149580905));
#265263=CARTESIAN_POINT('Ctrl Pts',(-0.289006193982606,1.52841937851943,
7.43840651592074));
#265264=CARTESIAN_POINT('Ctrl Pts',(-0.285878716748918,1.52900743516621,
7.43817703012195));
#265265=CARTESIAN_POINT('Ctrl Pts',(-0.279112012511478,1.53025828436994,
7.43768199208547));
#265266=CARTESIAN_POINT('Ctrl Pts',(-0.275472223684608,1.53091769444417,
7.43741663263853));
#265267=CARTESIAN_POINT('Ctrl Pts',(-0.265291788270658,1.53272457173178,
7.43667690704203));
#265268=CARTESIAN_POINT('Ctrl Pts',(-0.258745990050451,1.53384316752804,
7.43620413796779));
#265269=CARTESIAN_POINT('Ctrl Pts',(-0.219951830195686,1.54021719316147,
7.43341804977357));
#265270=CARTESIAN_POINT('Ctrl Pts',(-0.187548638084819,1.54449788451224,
7.43115549720283));
#265271=CARTESIAN_POINT('Ctrl Pts',(0.000741595742554217,1.56335808149029,
7.41825407281852));
#265272=CARTESIAN_POINT('Ctrl Pts',(0.157984611973251,1.55535825196448,
7.408361542596));
#265273=CARTESIAN_POINT('Ctrl Pts',(0.349576205186626,1.51621079659059,
7.39506688557467));
#265274=CARTESIAN_POINT('Ctrl Pts',(0.387445070355439,1.50697862893708,
7.39238197219455));
#265275=CARTESIAN_POINT('Ctrl Pts',(0.435368255556078,1.49336954259144,
7.38889056135292));
#265276=CARTESIAN_POINT('Ctrl Pts',(0.445780026480189,1.49029469101661,
7.38812631095396));
#265277=CARTESIAN_POINT('Ctrl Pts',(0.462287246255746,1.48523124370274,
7.38690513489867));
#265278=CARTESIAN_POINT('Ctrl Pts',(0.468404199163538,1.48331346966603,
7.3864505234079));
#265279=CARTESIAN_POINT('Ctrl Pts',(0.479378581668486,1.47979815207504,
7.38563106308403));
#265280=CARTESIAN_POINT('Ctrl Pts',(0.484240347923218,1.47821435514059,
7.38526667009684));
#265281=CARTESIAN_POINT('Ctrl Pts',(0.495615530637807,1.4744465707116,7.38441084253332));
#265282=CARTESIAN_POINT('Ctrl Pts',(0.502122417439701,1.4722433627612,7.38391878089058));
#265283=CARTESIAN_POINT('Ctrl Pts',(0.520891652498736,1.46574926636116,
7.38249202597401));
#265284=CARTESIAN_POINT('Ctrl Pts',(0.533114847244496,1.46134785936857,
7.38155369987066));
#265285=CARTESIAN_POINT('Ctrl Pts',(0.638448881193241,1.42192110264971,
7.37338576809402));
#265286=CARTESIAN_POINT('Ctrl Pts',(0.728037177866663,1.37819849138836,
7.36585900048933));
#265287=CARTESIAN_POINT('Ctrl Pts',(0.906587736774849,1.26876831388936,
7.34969140542793));
#265288=CARTESIAN_POINT('Ctrl Pts',(0.993997183648702,1.20151844453834,
7.34106041651668));
#265289=CARTESIAN_POINT('Ctrl Pts',(1.08523484875561,1.11449751864845,7.33165915261177));
#265290=CARTESIAN_POINT('Ctrl Pts',(1.09671131097907,1.10320612333384,7.33046909443327));
#265291=CARTESIAN_POINT('Ctrl Pts',(1.11219993606577,1.08748663153601,7.32885505999204));
#265292=CARTESIAN_POINT('Ctrl Pts',(1.11636447197925,1.0832110784049,7.32842027621277));
#265293=CARTESIAN_POINT('Ctrl Pts',(1.12296740869996,1.07635359371893,7.32772977833455));
#265294=CARTESIAN_POINT('Ctrl Pts',(1.12542169884342,1.07378715776256,7.32747286772583));
#265295=CARTESIAN_POINT('Ctrl Pts',(1.1300800178901,1.068882466794,7.32698479525348));
#265296=CARTESIAN_POINT('Ctrl Pts',(1.13228556417248,1.06654581525542,7.32675352223954));
#265297=CARTESIAN_POINT('Ctrl Pts',(1.13745098943792,1.06103925700916,7.32621139669419));
#265298=CARTESIAN_POINT('Ctrl Pts',(1.14040487350684,1.05786378328897,7.32590100187879));
#265299=CARTESIAN_POINT('Ctrl Pts',(1.15003152216796,1.04742779549515,7.32488802482539));
#265300=CARTESIAN_POINT('Ctrl Pts',(1.15664871235854,1.0401159830777,7.32418949077711));
#265301=CARTESIAN_POINT('Ctrl Pts',(1.22661614222199,0.961310351995921,
7.31677292968199));
#265302=CARTESIAN_POINT('Ctrl Pts',(1.28333255929694,0.884176656949972,
7.31048285538611));
#265303=CARTESIAN_POINT('Ctrl Pts',(1.3714501797936,0.737816074514749,7.29923695429479));
#265304=CARTESIAN_POINT('Ctrl Pts',(1.40551794632882,0.670634250618102,
7.29429994409142));
#265305=CARTESIAN_POINT('Ctrl Pts',(1.43457682219249,0.601306570085596,
7.28923406038337));
#265306=CARTESIAN_POINT('Ctrl Pts',(1.43457650415244,0.601307328854198,
7.14927790964297));
#265307=CARTESIAN_POINT('Ctrl Pts',(1.41398943702625,0.650423182547385,
7.15285502485694));
#265308=CARTESIAN_POINT('Ctrl Pts',(1.39087866118477,0.69848514105456,7.15649046759798));
#265309=CARTESIAN_POINT('Ctrl Pts',(1.35892565540541,0.75702021784198,7.16114736762822));
#265310=CARTESIAN_POINT('Ctrl Pts',(1.35237734923916,0.76865729223107,7.16208487945091));
#265311=CARTESIAN_POINT('Ctrl Pts',(1.34217024319219,0.786262206804669,
7.1635218694139));
#265312=CARTESIAN_POINT('Ctrl Pts',(1.33861951138496,0.792292256939287,
7.16401746119829));
#265313=CARTESIAN_POINT('Ctrl Pts',(1.33208386438546,0.8032221012684,7.16492206085695));
#265314=CARTESIAN_POINT('Ctrl Pts',(1.32911228162822,0.808129758721763,
7.16533057855338));
#265315=CARTESIAN_POINT('Ctrl Pts',(1.32263175798516,0.818700104313822,
7.16621560053504));
#265316=CARTESIAN_POINT('Ctrl Pts',(1.31911346601522,0.824356894348964,
7.166692441843));
#265317=CARTESIAN_POINT('Ctrl Pts',(1.30944361895239,0.839683876093768,
7.16799333233084));
#265318=CARTESIAN_POINT('Ctrl Pts',(1.30322145758343,0.849308790968366,
7.16881997710542));
#265319=CARTESIAN_POINT('Ctrl Pts',(1.27115064649358,0.897736061732842,
7.17302969502846));
#265320=CARTESIAN_POINT('Ctrl Pts',(1.24367576003486,0.935427047437751,
7.17647328433812));
#265321=CARTESIAN_POINT('Ctrl Pts',(1.1299708632001,1.07753154109983,7.19014209277467));
#265322=CARTESIAN_POINT('Ctrl Pts',(1.03195347200524,1.17173855075625,7.2008022149012));
#265323=CARTESIAN_POINT('Ctrl Pts',(0.887859264275082,1.27796447570786,
7.21448426746454));
#265324=CARTESIAN_POINT('Ctrl Pts',(0.851629092608341,1.30238858240716,
7.21777675723082));
#265325=CARTESIAN_POINT('Ctrl Pts',(0.808266580492868,1.32903629235091,
7.22151003593733));
#265326=CARTESIAN_POINT('Ctrl Pts',(0.80209165533007,1.33277204104875,7.22203692171207));
#265327=CARTESIAN_POINT('Ctrl Pts',(0.792581609299095,1.33843545862533,
7.22284087991231));
#265328=CARTESIAN_POINT('Ctrl Pts',(0.789265067188458,1.34039387453564,
7.22311986563767));
#265329=CARTESIAN_POINT('Ctrl Pts',(0.783166996480675,1.34396430028767,
7.22363024431901));
#265330=CARTESIAN_POINT('Ctrl Pts',(0.780387754915278,1.34558000031406,
7.22386186790278));
#265331=CARTESIAN_POINT('Ctrl Pts',(0.774138150741288,1.34918730445588,
7.2243805180618));
#265332=CARTESIAN_POINT('Ctrl Pts',(0.770665107094253,1.35117413852363,
7.22466723736186));
#265333=CARTESIAN_POINT('Ctrl Pts',(0.761762942798098,1.35622133480047,
7.22539842056664));
#265334=CARTESIAN_POINT('Ctrl Pts',(0.756322957720293,1.35926254898649,
7.22584169583896));
#265335=CARTESIAN_POINT('Ctrl Pts',(0.723864564103367,1.37715316083802,
7.22846647902005));
#265336=CARTESIAN_POINT('Ctrl Pts',(0.696425516106974,1.39123059601253,
7.23060305489848));
#265337=CARTESIAN_POINT('Ctrl Pts',(0.655607738352279,1.41066129077763,
7.23368941997518));
#265338=CARTESIAN_POINT('Ctrl Pts',(0.642546320808682,1.41665840404741,
7.23466360318313));
#265339=CARTESIAN_POINT('Ctrl Pts',(0.535898850775492,1.46384680800252,
7.24252425889092));
#265340=CARTESIAN_POINT('Ctrl Pts',(0.438538686898448,1.49590150191927,
7.24913551212262));
#265341=CARTESIAN_POINT('Ctrl Pts',(0.270498627689884,1.53339438374838,
7.26056963867525));
#265342=CARTESIAN_POINT('Ctrl Pts',(0.201324681096081,1.54399944986193,
7.26527976158312));
#265343=CARTESIAN_POINT('Ctrl Pts',(0.114754839431906,1.55135425860986,
7.27131859697339));
#265344=CARTESIAN_POINT('Ctrl Pts',(0.0978099212591027,1.55251469836456,
7.2725071375248));
#265345=CARTESIAN_POINT('Ctrl Pts',(0.0731557546212608,1.55379787836017,
7.27424741052073));
#265346=CARTESIAN_POINT('Ctrl Pts',(0.0654588031021716,1.55414116234069,
7.27479227033663));
#265347=CARTESIAN_POINT('Ctrl Pts',(0.0519495029807814,1.55464314382103,
7.27575144859764));
#265348=CARTESIAN_POINT('Ctrl Pts',(0.046138172307158,1.55482646069212,
7.27616499118432));
#265349=CARTESIAN_POINT('Ctrl Pts',(0.0348383495075163,1.55511950479854,
7.27697097312598));
#265350=CARTESIAN_POINT('Ctrl Pts',(0.0293500280368556,1.55523276689732,
7.27736329587723));
#265351=CARTESIAN_POINT('Ctrl Pts',(0.0146647588522598,1.55545806464564,
7.2784154044956));
#265352=CARTESIAN_POINT('Ctrl Pts',(0.00546734866940089,1.55551758182868,
7.27907681780282));
#265353=CARTESIAN_POINT('Ctrl Pts',(-0.028301481047181,1.55543660874141,
7.28151468293943));
#265354=CARTESIAN_POINT('Ctrl Pts',(-0.0528668654284095,1.55479547992107,
7.28330656675624));
#265355=CARTESIAN_POINT('Ctrl Pts',(-0.0823972219991191,1.55332415382531,
7.28548418914188));
#265356=CARTESIAN_POINT('Ctrl Pts',(-0.0873876539609487,1.55305139191809,
7.28585300083938));
#265357=CARTESIAN_POINT('Ctrl Pts',(-0.0978636054624743,1.55242815555241,
7.28662891961178));
#265358=CARTESIAN_POINT('Ctrl Pts',(-0.103348746186629,1.55207264608256,
7.2870361690614));
#265359=CARTESIAN_POINT('Ctrl Pts',(-0.261417359777088,1.54098607779415,
7.29880057662247));
#265360=CARTESIAN_POINT('Ctrl Pts',(-0.411578121216026,1.50783404403569,
7.31086310221171));
#265361=CARTESIAN_POINT('Ctrl Pts',(-0.594161124822741,1.43817948313455,
7.32578728750056));
#265362=CARTESIAN_POINT('Ctrl Pts',(-0.633249149293904,1.42140211836148,
7.328990172764));
#265363=CARTESIAN_POINT('Ctrl Pts',(-0.678073181700608,1.39994587100844,
7.33263496929858));
#265364=CARTESIAN_POINT('Ctrl Pts',(-0.684520533918495,1.39680468407892,
7.333158517463));
#265365=CARTESIAN_POINT('Ctrl Pts',(-0.6943882030226,1.39191236577429,7.33395846109885));
#265366=CARTESIAN_POINT('Ctrl Pts',(-0.697824026860519,1.39019302217144,
7.334236740962));
#265367=CARTESIAN_POINT('Ctrl Pts',(-0.704123452002819,1.38701144624944,
7.33474644209801));
#265368=CARTESIAN_POINT('Ctrl Pts',(-0.706988878182494,1.38555307160924,
7.33497808977931));
#265369=CARTESIAN_POINT('Ctrl Pts',(-0.71341996703927,1.38225478797445,
7.33549755542729));
#265370=CARTESIAN_POINT('Ctrl Pts',(-0.716983039370784,1.38040996464118,
7.3357850614605));
#265371=CARTESIAN_POINT('Ctrl Pts',(-0.726094470739885,1.37564761643639,
7.33651960615635));
#265372=CARTESIAN_POINT('Ctrl Pts',(-0.731632474806084,1.37271026454167,
7.33696543753028));
#265373=CARTESIAN_POINT('Ctrl Pts',(-0.764812012845302,1.35485403219029,
7.33963364953554));
#265374=CARTESIAN_POINT('Ctrl Pts',(-0.792016620364079,1.33913288715165,
7.34180936497323));
#265375=CARTESIAN_POINT('Ctrl Pts',(-0.901735160130949,1.27121370357814,
7.35061355678636));
#265376=CARTESIAN_POINT('Ctrl Pts',(-0.979727552594015,1.21212543894205,
7.35695310320468));
#265377=CARTESIAN_POINT('Ctrl Pts',(-1.12131590887796,1.08220389796188,
7.36963683760438));
#265378=CARTESIAN_POINT('Ctrl Pts',(-1.18498025485092,1.01209307693474,
7.37595089388379));
#265379=CARTESIAN_POINT('Ctrl Pts',(-1.24972659564271,0.926246903548408,
7.38346285296436));
#265380=CARTESIAN_POINT('Ctrl Pts',(-1.25743823670015,0.91575048618445,
7.38437762187835));
#265381=CARTESIAN_POINT('Ctrl Pts',(-1.26904923122958,0.89952338225409,
7.38578686996342));
#265382=CARTESIAN_POINT('Ctrl Pts',(-1.27304374357368,0.893861225606914,
7.38627769340818));
#265383=CARTESIAN_POINT('Ctrl Pts',(-1.27995575823998,0.883923243014669,
7.3871376894154));
#265384=CARTESIAN_POINT('Ctrl Pts',(-1.28289002168109,0.87965915767313,
7.38750621778068));
#265385=CARTESIAN_POINT('Ctrl Pts',(-1.28946897310009,0.869995663453272,
7.38834038882606));
#265386=CARTESIAN_POINT('Ctrl Pts',(-1.29310111469933,0.864587873957569,
7.38880649552927));
#265387=CARTESIAN_POINT('Ctrl Pts',(-1.30282756740133,0.849908047852611,
7.39006998705747));
#265388=CARTESIAN_POINT('Ctrl Pts',(-1.30885671215645,0.840593513760586,
7.39086977975392));
#265389=CARTESIAN_POINT('Ctrl Pts',(-1.33649926011445,0.796869566371059,
7.39461605198089));
#265390=CARTESIAN_POINT('Ctrl Pts',(-1.35685678220359,0.761689231409419,
7.39760780518503));
#265391=CARTESIAN_POINT('Ctrl Pts',(-1.38448052263844,0.709322980046774,
7.40203334317762));
#265392=CARTESIAN_POINT('Ctrl Pts',(-1.39285332149625,0.692737312959795,
7.40343101771053));
#265393=CARTESIAN_POINT('Ctrl Pts',(-1.45625877456422,0.561338527483712,
7.41447081481527));
#265394=CARTESIAN_POINT('Ctrl Pts',(-1.49729632470014,0.44032785169477,
7.42449674037175));
#265395=CARTESIAN_POINT('Ctrl Pts',(-1.53130192038005,0.276253267129787,
7.43727361028639));
#265396=CARTESIAN_POINT('Ctrl Pts',(-1.53794026375515,0.236520353452068,
7.44030240415309));
#265397=CARTESIAN_POINT('Ctrl Pts',(-1.54392402291332,0.189549359214922,
7.44377455408231));
#265398=CARTESIAN_POINT('Ctrl Pts',(-1.54477056875129,0.18252189773683,
7.44429119016678));
#265399=CARTESIAN_POINT('Ctrl Pts',(-1.54600032748235,0.171691132720457,
7.44508281345796));
#265400=CARTESIAN_POINT('Ctrl Pts',(-1.54641752623545,0.167891908783323,
7.44535962579538));
#265401=CARTESIAN_POINT('Ctrl Pts',(-1.54716001997004,0.160892720638553,
7.44586793269665));
#265402=CARTESIAN_POINT('Ctrl Pts',(-1.54748939183999,0.157693302018606,
7.44609964486358));
#265403=CARTESIAN_POINT('Ctrl Pts',(-1.54820971888121,0.150476598889468,
7.44662087074211));
#265404=CARTESIAN_POINT('Ctrl Pts',(-1.54859496304228,0.146458806106144,
7.44691006256263));
#265405=CARTESIAN_POINT('Ctrl Pts',(-1.54954575356094,0.136119392907673,
7.44765182348297));
#265406=CARTESIAN_POINT('Ctrl Pts',(-1.55008826370437,0.129795646622869,
7.44810314480199));
#265407=CARTESIAN_POINT('Ctrl Pts',(-1.55318941425712,0.0908495592073391,
7.45086922410159));
#265408=CARTESIAN_POINT('Ctrl Pts',(-1.55475707142191,0.0581536124806726,
7.4531332783272));
#265409=CARTESIAN_POINT('Ctrl Pts',(-1.55542535573004,0.0172809625157889,
7.4559183916929));
#265410=CARTESIAN_POINT('Ctrl Pts',(-1.55549454975572,0.00913120996006105,
7.45647148409281));
#265411=CARTESIAN_POINT('Ctrl Pts',(-1.55558306867206,-0.13120281373001,
7.46596250448332));
#265412=CARTESIAN_POINT('Ctrl Pts',(-1.53881797602093,-0.26286247137312,
7.47441018750964));
#265413=CARTESIAN_POINT('Ctrl Pts',(-1.4925081184459,-0.441266040778045,
7.4868162065679));
#265414=CARTESIAN_POINT('Ctrl Pts',(-1.47688878599857,-0.491014008997499,
7.49037918562025));
#265415=CARTESIAN_POINT('Ctrl Pts',(-1.45504567123091,-0.550036002399161,
7.49478217292608));
#265416=CARTESIAN_POINT('Ctrl Pts',(-1.45118142837119,-0.560151730168049,
7.49554312891732));
#265417=CARTESIAN_POINT('Ctrl Pts',(-1.44461681341238,-0.576812472106778,
7.49680736949767));
#265418=CARTESIAN_POINT('Ctrl Pts',(-1.44197676452556,-0.583380984559844,
7.4973086347027));
#265419=CARTESIAN_POINT('Ctrl Pts',(-1.43711434861855,-0.595244125472339,
7.49821921669866));
#265420=CARTESIAN_POINT('Ctrl Pts',(-1.43490731337792,-0.600544936129068,
7.49862801047416));
#265421=CARTESIAN_POINT('Ctrl Pts',(-1.43010113693995,-0.611910552986962,
7.49950871304516));
#265422=CARTESIAN_POINT('Ctrl Pts',(-1.42749266247622,-0.617971263759118,
7.49998093199145));
#265423=CARTESIAN_POINT('Ctrl Pts',(-1.42024089598966,-0.634529594556464,
7.50127828213408));
#265424=CARTESIAN_POINT('Ctrl Pts',(-1.41551992219933,-0.644992516036362,
7.50210604663793));
#265425=CARTESIAN_POINT('Ctrl Pts',(-1.3886593592306,-0.7028070478571,7.50672556396649));
#265426=CARTESIAN_POINT('Ctrl Pts',(-1.36426220500353,-0.749066096014676,
7.51059451184402));
#265427=CARTESIAN_POINT('Ctrl Pts',(-1.27167108507637,-0.9050456889936,
7.52426660179247));
#265428=CARTESIAN_POINT('Ctrl Pts',(-1.19218687269172,-1.00744147854868,
7.53442651934219));
#265429=CARTESIAN_POINT('Ctrl Pts',(-1.08977095396671,-1.11005928583765,
7.54551256557175));
#265430=CARTESIAN_POINT('Ctrl Pts',(-1.07838302587464,-1.1211255203613,
7.54672085795936));
#265431=CARTESIAN_POINT('Ctrl Pts',(-1.04550822943724,-1.15210718197175,
7.55013613159798));
#265432=CARTESIAN_POINT('Ctrl Pts',(-1.02362396859282,-1.1715940765663,
7.55232380795466));
#265433=CARTESIAN_POINT('Ctrl Pts',(-0.996054008029764,-1.19478110321958,
7.55496377647592));
#265434=CARTESIAN_POINT('Ctrl Pts',(-0.990879334823756,-1.19907615260726,
7.55545442047196));
#265435=CARTESIAN_POINT('Ctrl Pts',(-0.982747568153337,-1.20573703816376,
7.55621767786679));
#265436=CARTESIAN_POINT('Ctrl Pts',(-0.97980949717901,-1.20812579559375,
7.55649188164494));
#265437=CARTESIAN_POINT('Ctrl Pts',(-0.974357567619555,-1.21252544012498,
7.55699776171194));
#265438=CARTESIAN_POINT('Ctrl Pts',(-0.971846207608002,-1.21453923841869,
7.55722963983249));
#265439=CARTESIAN_POINT('Ctrl Pts',(-0.966136717817111,-1.21908849066606,
7.55775422589511));
#265440=CARTESIAN_POINT('Ctrl Pts',(-0.962934853161479,-1.22161916127019,
7.55804659326358));
#265441=CARTESIAN_POINT('Ctrl Pts',(-0.953163544083775,-1.22927986295967,
7.55893344045983));
#265442=CARTESIAN_POINT('Ctrl Pts',(-0.946562650311138,-1.23436983131031,
7.55952517771302));
#265443=CARTESIAN_POINT('Ctrl Pts',(-0.93118061511606,-1.24603500794568,
7.5608879987941));
#265444=CARTESIAN_POINT('Ctrl Pts',(-0.92237008940139,-1.25257096157342,
7.56165662960579));
#265445=CARTESIAN_POINT('Ctrl Pts',(-0.891928383832259,-1.27465827217729,
7.56427450201624));
#265446=CARTESIAN_POINT('Ctrl Pts',(-0.869966124707353,-1.2897476806665,
7.56609857267938));
#265447=CARTESIAN_POINT('Ctrl Pts',(-0.744964293400565,-1.37098473805262,
7.57619099081975));
#265448=CARTESIAN_POINT('Ctrl Pts',(-0.634780217955134,-1.42535231875577,
7.5840448544213));
#265449=CARTESIAN_POINT('Ctrl Pts',(-0.460876068021626,-1.48695062201216,
7.59638505187517));
#265450=CARTESIAN_POINT('Ctrl Pts',(-0.401218774456614,-1.50414456753985,
7.60060300657389));
#265451=CARTESIAN_POINT('Ctrl Pts',(-0.329660130594825,-1.52020803139373,
7.60572997214039));
#265452=CARTESIAN_POINT('Ctrl Pts',(-0.31859424337832,-1.52256558368447,
7.60652457906888));
#265453=CARTESIAN_POINT('Ctrl Pts',(-0.300418613494051,-1.52623102748755,
7.60783309026897));
#265454=CARTESIAN_POINT('Ctrl Pts',(-0.293323589054237,-1.52761047440765,
7.60834471761083));
#265455=CARTESIAN_POINT('Ctrl Pts',(-0.28056355729229,-1.52999916630627,
7.60926647645861));
#265456=CARTESIAN_POINT('Ctrl Pts',(-0.274902038801047,-1.53102652688094,
7.6096760251542));
#265457=CARTESIAN_POINT('Ctrl Pts',(-0.262837521846903,-1.53314672458383,
7.61055004194072));
#265458=CARTESIAN_POINT('Ctrl Pts',(-0.256433135898578,-1.53423091040514,
7.61101477565972));
#265459=CARTESIAN_POINT('Ctrl Pts',(-0.239155631092851,-1.53704458258821,
7.61227068502825));
#265460=CARTESIAN_POINT('Ctrl Pts',(-0.228270811383216,-1.53869876513861,
7.61306421925459));
#265461=CARTESIAN_POINT('Ctrl Pts',(-0.172508789370332,-1.54656831177633,
7.61714203885514));
#265462=CARTESIAN_POINT('Ctrl Pts',(-0.127397517273259,-1.55093582030455,
7.6204836108021));
#265463=CARTESIAN_POINT('Ctrl Pts',(0.00710775874016667,-1.55805053643489,
7.63058333437894));
#265464=CARTESIAN_POINT('Ctrl Pts',(0.0966102331198495,-1.5550674457057,
7.63749282959576));
#265465=CARTESIAN_POINT('Ctrl Pts',(0.219958641650496,-1.54026410120411,
7.64712659900582));
#265466=CARTESIAN_POINT('Ctrl Pts',(0.254419274053056,-1.53494828579841,
7.64982844410327));
#265467=CARTESIAN_POINT('Ctrl Pts',(0.343449220867888,-1.51813384095952,
7.65680151142424));
#265468=CARTESIAN_POINT('Ctrl Pts',(0.397637107601824,-1.50485016320981,
7.66103921955609));
#265469=CARTESIAN_POINT('Ctrl Pts',(0.458579561074521,-1.48638748216307,
7.66571797101357));
#265470=CARTESIAN_POINT('Ctrl Pts',(0.466140996847573,-1.48403353705964,
7.66629689758326));
#265471=CARTESIAN_POINT('Ctrl Pts',(0.477542316735609,-1.48038845951527,
7.66716707162346));
#265472=CARTESIAN_POINT('Ctrl Pts',(0.481395524026743,-1.47913995476937,
7.66746068056055));
#265473=CARTESIAN_POINT('Ctrl Pts',(0.488300437989079,-1.4768728049707,
7.66798591503389));
#265474=CARTESIAN_POINT('Ctrl Pts',(0.491353886214399,-1.47585973552692,
7.66821785683763));
#265475=CARTESIAN_POINT('Ctrl Pts',(0.49801717093406,-1.4736260269877,7.66872329208184));
#265476=CARTESIAN_POINT('Ctrl Pts',(0.501625667673291,-1.47240159614631,
7.66899655962782));
#265477=CARTESIAN_POINT('Ctrl Pts',(0.511873158073115,-1.46888238506152,
7.6697714073045));
#265478=CARTESIAN_POINT('Ctrl Pts',(0.518501272205361,-1.46655583827937,
7.67027116530838));
#265479=CARTESIAN_POINT('Ctrl Pts',(0.561873409342252,-1.45100090043244,
7.67353353147966));
#265480=CARTESIAN_POINT('Ctrl Pts',(0.598127702132498,-1.4364362977732,
7.6762233711843));
#265481=CARTESIAN_POINT('Ctrl Pts',(0.740704026296866,-1.37282250640302,
7.68679917912225));
#265482=CARTESIAN_POINT('Ctrl Pts',(0.841888953050843,-1.31320640691412,
7.69432490466026));
#265483=CARTESIAN_POINT('Ctrl Pts',(0.946141601383891,-1.23473720740609,
7.70302539410244));
#265484=CARTESIAN_POINT('Ctrl Pts',(0.956745708425602,-1.22653884528527,
7.70392201923503));
#265485=CARTESIAN_POINT('Ctrl Pts',(1.0070467310327,-1.18660033216036,7.70823597009322));
#265486=CARTESIAN_POINT('Ctrl Pts',(1.04527436196011,-1.15306726263229,
7.71170006718917));
#265487=CARTESIAN_POINT('Ctrl Pts',(1.09251232593085,-1.10734807081034,
7.71628113087147));
#265488=CARTESIAN_POINT('Ctrl Pts',(1.10308489011261,-1.09681658922292,
7.71732729402976));
#265489=CARTESIAN_POINT('Ctrl Pts',(1.11861159496126,-1.08089863363399,
7.71889622211266));
#265490=CARTESIAN_POINT('Ctrl Pts',(1.12368212060252,-1.07562644310819,
7.7194139079532));
#265491=CARTESIAN_POINT('Ctrl Pts',(1.1326805079814,-1.06613710508224,7.72034232949656));
#265492=CARTESIAN_POINT('Ctrl Pts',(1.13662250295984,-1.06193349326789,
7.72075244743263));
#265493=CARTESIAN_POINT('Ctrl Pts',(1.14492159629079,-1.05298446849821,
7.72162317146589));
#265494=CARTESIAN_POINT('Ctrl Pts',(1.14927274318288,-1.04823371059283,
7.72208401944987));
#265495=CARTESIAN_POINT('Ctrl Pts',(1.16081725136802,-1.03547066548159,
7.72331850520579));
#265496=CARTESIAN_POINT('Ctrl Pts',(1.16795702523926,-1.0274106124187,7.72409436458778));
#265497=CARTESIAN_POINT('Ctrl Pts',(1.20264076782716,-0.987427549722852,
7.72792566049681));
#265498=CARTESIAN_POINT('Ctrl Pts',(1.22896007070618,-0.954470793493423,
7.73103038492061));
#265499=CARTESIAN_POINT('Ctrl Pts',(1.34534226448227,-0.79593286110363,
7.74574064312489));
#265500=CARTESIAN_POINT('Ctrl Pts',(1.41769039691832,-0.658479161179764,
7.7579806652478));
#265501=CARTESIAN_POINT('Ctrl Pts',(1.47885315116279,-0.483261694965158,
7.77203516592401));
#265502=CARTESIAN_POINT('Ctrl Pts',(1.48822529707258,-0.453579451468234,
7.77436214251193));
#265503=CARTESIAN_POINT('Ctrl Pts',(1.49840357577635,-0.417619491806089,
7.77710175178937));
#265504=CARTESIAN_POINT('Ctrl Pts',(1.50006958328761,-0.411595146538542,
7.77755806504056));
#265505=CARTESIAN_POINT('Ctrl Pts',(1.50274391385478,-0.401692709279255,
7.77830359925158));
#265506=CARTESIAN_POINT('Ctrl Pts',(1.50377362481527,-0.39782054949852,
7.77859399515349));
#265507=CARTESIAN_POINT('Ctrl Pts',(1.5056026007616,-0.390834229148045,
7.77911585070944));
#265508=CARTESIAN_POINT('Ctrl Pts',(1.50640717759243,-0.387721552142953,
7.77934760804672));
#265509=CARTESIAN_POINT('Ctrl Pts',(1.50815325127212,-0.380879007136704,
7.77985543096226));
#265510=CARTESIAN_POINT('Ctrl Pts',(1.5090905638084,-0.377148138653765,
7.78013125484866));
#265511=CARTESIAN_POINT('Ctrl Pts',(1.51174107369642,-0.366429982573151,
7.78092070089002));
#265512=CARTESIAN_POINT('Ctrl Pts',(1.51341968106794,-0.35943411122582,
7.78143239121367));
#265513=CARTESIAN_POINT('Ctrl Pts',(1.52481154014552,-0.310461559730384,
7.78499091343881));
#265514=CARTESIAN_POINT('Ctrl Pts',(1.53282668064198,-0.268104121047499,
7.78794893120415));
#265515=CARTESIAN_POINT('Ctrl Pts',(1.56259413327522,-0.0649040653522604,
7.80180981163363));
#265516=CARTESIAN_POINT('Ctrl Pts',(1.56084819286634,0.098344275979195,
7.81208305174017));
#265517=CARTESIAN_POINT('Ctrl Pts',(1.5297333463465,0.283059065311713,7.82498177226162));
#265518=CARTESIAN_POINT('Ctrl Pts',(1.52498161346089,0.307632088629587,
7.82672155928336));
#265519=CARTESIAN_POINT('Ctrl Pts',(1.51766163396118,0.341129362340106,
7.82913106988495));
#265520=CARTESIAN_POINT('Ctrl Pts',(1.51560305295116,0.350162042918745,
7.82978460283131));
#265521=CARTESIAN_POINT('Ctrl Pts',(1.51219342557476,0.364529243151413,
7.8308304050178));
#265522=CARTESIAN_POINT('Ctrl Pts',(1.51089452116865,0.369876019702916,
7.83122100016026));
#265523=CARTESIAN_POINT('Ctrl Pts',(1.50816630265589,0.380852183806567,
7.83202577124372));
#265524=CARTESIAN_POINT('Ctrl Pts',(1.50673377486618,0.386480675290505,
7.83244004485625));
#265525=CARTESIAN_POINT('Ctrl Pts',(1.50333819150548,0.399516270086498,
7.83340327303896));
#265526=CARTESIAN_POINT('Ctrl Pts',(1.50135187074254,0.40691709773435,7.8339529700567));
#265527=CARTESIAN_POINT('Ctrl Pts',(1.49484833245561,0.430452603071676,
7.83571031090906));
#265528=CARTESIAN_POINT('Ctrl Pts',(1.49012520958054,0.446528609978834,
7.83692457487138));
#265529=CARTESIAN_POINT('Ctrl Pts',(1.47049041665882,0.509574951384381,
7.84174352386162));
#265530=CARTESIAN_POINT('Ctrl Pts',(1.45361447403242,0.555887219104188,
7.84541014903729));
#265531=CARTESIAN_POINT('Ctrl Pts',(1.43457666579773,0.601306943206762,
7.84913521677167));
#265532=CARTESIAN_POINT('Origin',(0.,0.,-1.29405622560371));
#265533=CARTESIAN_POINT('',(1.43456415251412,0.601298694836466,8.68837676241652));
#265534=CARTESIAN_POINT('',(1.43457668241997,0.601306903550017,8.55150209358323));
#265535=CARTESIAN_POINT('',(1.43457668357355,0.601306900797845,-1.29405622560371));
#265536=CARTESIAN_POINT('',(-1.55430433363989,-0.00129356757865576,8.29405691353744));
#265537=CARTESIAN_POINT('Ctrl Pts',(-1.55430433363989,-0.00129356757865576,
8.29405691353744));
#265538=CARTESIAN_POINT('Ctrl Pts',(-1.55556915289093,-0.163823035851805,
8.30567841650669));
#265539=CARTESIAN_POINT('Ctrl Pts',(-1.45729141273118,-0.84303952995183,
8.35435184806778));
#265540=CARTESIAN_POINT('Ctrl Pts',(-0.472877852103197,-1.77676948847047,
8.44007720822072));
#265541=CARTESIAN_POINT('Ctrl Pts',(1.23652006183316,-1.36071356826243,
8.55123299399628));
#265542=CARTESIAN_POINT('Ctrl Pts',(1.66634991413392,-0.123264202437792,
8.63399951206154));
#265543=CARTESIAN_POINT('Ctrl Pts',(1.482431870734,0.490255529475159,8.67971410153496));
#265544=CARTESIAN_POINT('Ctrl Pts',(1.43456415251406,0.601298694836608,
8.68837676241653));
#265545=CARTESIAN_POINT('Ctrl Pts',(-1.55549950636669,-0.00123923080959585,
8.29474377359494));
#265546=CARTESIAN_POINT('Ctrl Pts',(-1.55555800331462,0.0721869404360917,
8.28986293506811));
#265547=CARTESIAN_POINT('Ctrl Pts',(-1.55041757773132,0.145517316076241,
8.28490362734154));
#265548=CARTESIAN_POINT('Ctrl Pts',(-1.53880297273442,0.227494320910168,
8.27912116304748));
#265549=CARTESIAN_POINT('Ctrl Pts',(-1.53740301704474,0.236770376927224,
8.2784634717434));
#265550=CARTESIAN_POINT('Ctrl Pts',(-1.53490673599696,0.25235400078937,
8.27735257567762));
#265551=CARTESIAN_POINT('Ctrl Pts',(-1.53385520664464,0.258668577097848,
8.27690077535223));
#265552=CARTESIAN_POINT('Ctrl Pts',(-1.53185454943286,0.270241444900713,
8.27606961412405));
#265553=CARTESIAN_POINT('Ctrl Pts',(-1.53091724405785,0.27550170546079,
8.27569063094717));
#265554=CARTESIAN_POINT('Ctrl Pts',(-1.52892979495897,0.286332080958602,
8.27490782764597));
#265555=CARTESIAN_POINT('Ctrl Pts',(-1.52787627095401,0.291901486109944,
8.27450390570557));
#265556=CARTESIAN_POINT('Ctrl Pts',(-1.52545868616356,0.304310175100152,
8.27360083350147));
#265557=CARTESIAN_POINT('Ctrl Pts',(-1.52407902999164,0.311146257036973,
8.27310119413207));
#265558=CARTESIAN_POINT('Ctrl Pts',(-1.52047867761881,0.328387009307086,
8.27183559523233));
#265559=CARTESIAN_POINT('Ctrl Pts',(-1.51819714916477,0.338778456780612,
8.2710677113846));
#265560=CARTESIAN_POINT('Ctrl Pts',(-1.50435830457567,0.398859574621789,
8.26659771098052));
#265561=CARTESIAN_POINT('Ctrl Pts',(-1.49046996029146,0.447974403057745,
8.26282169437105));
#265562=CARTESIAN_POINT('Ctrl Pts',(-1.46171716586699,0.533378582557028,
8.25603193112348));
#265563=CARTESIAN_POINT('Ctrl Pts',(-1.44784595434876,0.569957461870795,
8.25304859337332));
#265564=CARTESIAN_POINT('Ctrl Pts',(-1.3917206393871,0.70264629207826,8.24196843163985));
#265565=CARTESIAN_POINT('Ctrl Pts',(-1.34114979006821,0.794931228218884,
8.23372851004576));
#265566=CARTESIAN_POINT('Ctrl Pts',(-1.26394783602608,0.907190332163691,
8.22341385383531));
#265567=CARTESIAN_POINT('Ctrl Pts',(-1.2454505818406,0.932422453899455,
8.22107613301032));
#265568=CARTESIAN_POINT('Ctrl Pts',(-1.22215290023892,0.962271206866444,
8.21830261698896));
#265569=CARTESIAN_POINT('Ctrl Pts',(-1.21806939548715,0.967435030923994,
8.21782250223291));
#265570=CARTESIAN_POINT('Ctrl Pts',(-1.21164816643309,0.97544992744695,
8.21707703902307));
#265571=CARTESIAN_POINT('Ctrl Pts',(-1.2093329463875,0.978318795550197,
8.216810152838));
#265572=CARTESIAN_POINT('Ctrl Pts',(-1.20499915399602,0.983650052755884,
8.21631413699351));
#265573=CARTESIAN_POINT('Ctrl Pts',(-1.20298324009485,0.986114451662576,
8.21608483339675));
#265574=CARTESIAN_POINT('Ctrl Pts',(-1.19835508364815,0.991736930764364,
8.21556161803745));
#265575=CARTESIAN_POINT('Ctrl Pts',(-1.19573791829188,0.994890887557919,
8.21526806682134));
#265576=CARTESIAN_POINT('Ctrl Pts',(-1.1888481588737,1.00312730512772,8.21450122317806));
#265577=CARTESIAN_POINT('Ctrl Pts',(-1.18455537518924,1.00819288949375,
8.21402934790199));
#265578=CARTESIAN_POINT('Ctrl Pts',(-1.15459670129965,1.04308930798161,
8.21077562438545));
#265579=CARTESIAN_POINT('Ctrl Pts',(-1.1278366120487,1.07196738629967,8.20806760178269));
#265580=CARTESIAN_POINT('Ctrl Pts',(-1.06915709114227,1.13065784706923,
8.20245030725981));
#265581=CARTESIAN_POINT('Ctrl Pts',(-1.03702062841388,1.1602037328346,8.19955350748688));
#265582=CARTESIAN_POINT('Ctrl Pts',(-0.938469635021524,1.24343933836468,
8.19103707450139));
#265583=CARTESIAN_POINT('Ctrl Pts',(-0.868836231641056,1.29305437859497,
8.18546985188624));
#265584=CARTESIAN_POINT('Ctrl Pts',(-0.763174934736102,1.35593435694536,
8.17721510886089));
#265585=CARTESIAN_POINT('Ctrl Pts',(-0.730179824001388,1.37398364306361,
8.17466352251371));
#265586=CARTESIAN_POINT('Ctrl Pts',(-0.681686880066569,1.39827040782312,
8.17092603907807));
#265587=CARTESIAN_POINT('Ctrl Pts',(-0.666690549737799,1.40548241228625,
8.16977197673378));
#265588=CARTESIAN_POINT('Ctrl Pts',(-0.639697457887556,1.41793466311354,
8.16769576166707));
#265589=CARTESIAN_POINT('Ctrl Pts',(-0.627744647926366,1.42326673012896,
8.16677676610204));
#265590=CARTESIAN_POINT('Ctrl Pts',(-0.609427304986174,1.43116234551455,
8.16536829773446));
#265591=CARTESIAN_POINT('Ctrl Pts',(-0.603110521025703,1.43383576325269,
8.16488256109587));
#265592=CARTESIAN_POINT('Ctrl Pts',(-0.59154038896699,1.43864254257833,
8.16399271655461));
#265593=CARTESIAN_POINT('Ctrl Pts',(-0.58629263596578,1.44078913812796,
8.16358906422052));
#265594=CARTESIAN_POINT('Ctrl Pts',(-0.574997115473913,1.44533764610249,
8.16272004480705));
#265595=CARTESIAN_POINT('Ctrl Pts',(-0.568945796546169,1.44773038659055,
8.16225437810499));
#265596=CARTESIAN_POINT('Ctrl Pts',(-0.552617302692956,1.45406862042579,
8.1609974539653));
#265597=CARTESIAN_POINT('Ctrl Pts',(-0.542313132386138,1.45794303420796,
8.1602038410533));
#265598=CARTESIAN_POINT('Ctrl Pts',(-0.492638271464822,1.47602153529082,
8.15637516730867));
#265599=CARTESIAN_POINT('Ctrl Pts',(-0.452749721826082,1.48874078033503,
8.153291737583));
#265600=CARTESIAN_POINT('Ctrl Pts',(-0.396595415101199,1.5041811741996,
8.14893429421699));
#265601=CARTESIAN_POINT('Ctrl Pts',(-0.380723384715419,1.50827669866467,
8.14770094190195));
#265602=CARTESIAN_POINT('Ctrl Pts',(-0.265723312576222,1.53601978136456,
8.13875370447867));
#265603=CARTESIAN_POINT('Ctrl Pts',(-0.164554415138191,1.55012375297761,
8.13080024651919));
#265604=CARTESIAN_POINT('Ctrl Pts',(-0.00266892152673535,1.55665938383207,
8.11828696858117));
#265605=CARTESIAN_POINT('Ctrl Pts',(0.0575071180737391,1.55559962465264,
8.11368801022367));
#265606=CARTESIAN_POINT('Ctrl Pts',(0.128473761944692,1.55022461798343,
8.10842694656259));
#265607=CARTESIAN_POINT('Ctrl Pts',(0.139461833169841,1.54927476236112,
8.10761705045185));
#265608=CARTESIAN_POINT('Ctrl Pts',(0.155134359159196,1.5477518639912,8.10646944470276));
#265609=CARTESIAN_POINT('Ctrl Pts',(0.159827419346596,1.54727428062307,
8.10612677052034));
#265610=CARTESIAN_POINT('Ctrl Pts',(0.1677794949402,1.54642848094481,8.1055478592966));
#265611=CARTESIAN_POINT('Ctrl Pts',(0.171039623380809,1.54607129641874,
8.10531101485583));
#265612=CARTESIAN_POINT('Ctrl Pts',(0.177278292394793,1.54536780351663,
8.10485875628473));
#265613=CARTESIAN_POINT('Ctrl Pts',(0.180256981511212,1.54502319145505,
8.10464324552976));
#265614=CARTESIAN_POINT('Ctrl Pts',(0.188163432242469,1.54408529787098,
8.10407228480597));
#265615=CARTESIAN_POINT('Ctrl Pts',(0.193089438524406,1.54347703412698,
8.10371766807415));
#265616=CARTESIAN_POINT('Ctrl Pts',(0.210704272527838,1.54121630308869,
8.10245330711154));
#265617=CARTESIAN_POINT('Ctrl Pts',(0.223375968460891,1.53943080005486,
8.10155064672995));
#265618=CARTESIAN_POINT('Ctrl Pts',(0.240675904031166,1.53677503314644,
8.10032593511558));
#265619=CARTESIAN_POINT('Ctrl Pts',(0.245323884734482,1.5360399038166,8.09999764791956));
#265620=CARTESIAN_POINT('Ctrl Pts',(0.275934691326711,1.53105597921151,
8.09784016383745));
#265621=CARTESIAN_POINT('Ctrl Pts',(0.301791122452567,1.52616993207907,
8.09603938571672));
#265622=CARTESIAN_POINT('Ctrl Pts',(0.474057723194178,1.48906721226896,
8.08411180186584));
#265623=CARTESIAN_POINT('Ctrl Pts',(0.615273187488639,1.43648768689398,
8.07459684579213));
#265624=CARTESIAN_POINT('Ctrl Pts',(0.780661816275275,1.34597113673286,
8.06176754120594));
#265625=CARTESIAN_POINT('Ctrl Pts',(0.813828608596464,1.32618013281126,
8.05910472413832));
#265626=CARTESIAN_POINT('Ctrl Pts',(0.854935022211891,1.29952844186988,
8.05566874818335));
#265627=CARTESIAN_POINT('Ctrl Pts',(0.863590412455415,1.29379273983518,
8.0549373796178));
#265628=CARTESIAN_POINT('Ctrl Pts',(0.877409291745758,1.28443487770958,
8.05375659357633));
#265629=CARTESIAN_POINT('Ctrl Pts',(0.882609412425551,1.28086714505725,
8.05330922865636));
#265630=CARTESIAN_POINT('Ctrl Pts',(0.892468757460877,1.27401423325673,
8.0524551602779));
#265631=CARTESIAN_POINT('Ctrl Pts',(0.897131909043185,1.27073486053164,
8.05204868271276));
#265632=CARTESIAN_POINT('Ctrl Pts',(0.907739537359039,1.26318752922213,
8.05111817032449));
#265633=CARTESIAN_POINT('Ctrl Pts',(0.91367209445602,1.25890313451357,8.05059351002539));
#265634=CARTESIAN_POINT('Ctrl Pts',(0.92906665220717,1.24761930298959,8.04922077452249));
#265635=CARTESIAN_POINT('Ctrl Pts',(0.938479674543701,1.24055417283532,
8.04837016622288));
#265636=CARTESIAN_POINT('Ctrl Pts',(1.01078806641354,1.18498772500172,8.04174676509041));
#265637=CARTESIAN_POINT('Ctrl Pts',(1.06995465723761,1.131848726626,8.03578874999882));
#265638=CARTESIAN_POINT('Ctrl Pts',(1.19852823919503,0.997248252399454,
8.02152436166095));
#265639=CARTESIAN_POINT('Ctrl Pts',(1.26411410745924,0.912682093294212,
8.01314245103618));
#265640=CARTESIAN_POINT('Ctrl Pts',(1.34036313858407,0.790200050946843,
8.00216318935175));
#265641=CARTESIAN_POINT('Ctrl Pts',(1.35904440555938,0.75762018550548,7.99934476888847));
#265642=CARTESIAN_POINT('Ctrl Pts',(1.37974025109851,0.718292842199205,
7.99608726125419));
#265643=CARTESIAN_POINT('Ctrl Pts',(1.38290994378434,0.712171229262564,
7.99558425044966));
#265644=CARTESIAN_POINT('Ctrl Pts',(1.38774265323152,0.702683903396858,
7.99481113663631));
#265645=CARTESIAN_POINT('Ctrl Pts',(1.38943430421857,0.699333007058198,
7.99453931024038));
#265646=CARTESIAN_POINT('Ctrl Pts',(1.39253523132513,0.693134887057267,
7.99403883668529));
#265647=CARTESIAN_POINT('Ctrl Pts',(1.39394790605636,0.690289488341606,
7.99380998574304));
#265648=CARTESIAN_POINT('Ctrl Pts',(1.3971224453454,0.683845869428415,7.99329375981481));
#265649=CARTESIAN_POINT('Ctrl Pts',(1.39887912982315,0.680245162820598,
7.99300670775675));
#265650=CARTESIAN_POINT('Ctrl Pts',(1.40403681074975,0.669568900780746,
7.99215964817462));
#265651=CARTESIAN_POINT('Ctrl Pts',(1.40739824525674,0.662474199451847,
7.99160201259709));
#265652=CARTESIAN_POINT('Ctrl Pts',(1.41900527544585,0.637489073498865,
7.98965553833988));
#265653=CARTESIAN_POINT('Ctrl Pts',(1.42696355777115,0.619470026600121,
7.98828273283126));
#265654=CARTESIAN_POINT('Ctrl Pts',(1.43457668592364,0.601306895191089,
7.98692484967426));
#265655=CARTESIAN_POINT('',(-1.55549984464226,0.000695210683922209,8.15469955740614));
#265656=CARTESIAN_POINT('Ctrl Pts',(1.43457666579773,0.601306943206762,
7.84913521677167));
#265657=CARTESIAN_POINT('Ctrl Pts',(1.42730805505206,0.618648135565035,
7.85055744285088));
#265658=CARTESIAN_POINT('Ctrl Pts',(1.41972430193386,0.635859233078565,
7.85198801424808));
#265659=CARTESIAN_POINT('Ctrl Pts',(1.37048245083437,0.742334480696986,
7.86095394217987));
#265660=CARTESIAN_POINT('Ctrl Pts',(1.3207408205474,0.827601753122177,7.86866671493112));
#265661=CARTESIAN_POINT('Ctrl Pts',(1.2564382022965,0.917104424693805,7.87712260980895));
#265662=CARTESIAN_POINT('Ctrl Pts',(1.24949566175549,0.926540924272781,
7.87801871951594));
#265663=CARTESIAN_POINT('Ctrl Pts',(1.219219555577,0.966733816464096,7.88185276884756));
#265664=CARTESIAN_POINT('Ctrl Pts',(1.19484968360784,0.996697268569604,
7.88475525689621));
#265665=CARTESIAN_POINT('Ctrl Pts',(1.16500159638469,1.03072584615701,7.88807662292849));
#265666=CARTESIAN_POINT('Ctrl Pts',(1.16058348785602,1.03569805515343,7.8885625842427));
#265667=CARTESIAN_POINT('Ctrl Pts',(1.15337162942885,1.04371029388466,7.88934650595298));
#265668=CARTESIAN_POINT('Ctrl Pts',(1.15059749402807,1.04676773972782,7.8896458492236));
#265669=CARTESIAN_POINT('Ctrl Pts',(1.14563616852879,1.05219219018185,7.89017723965831));
#265670=CARTESIAN_POINT('Ctrl Pts',(1.14345376789805,1.05456347230107,7.890409636042));
#265671=CARTESIAN_POINT('Ctrl Pts',(1.13871450846461,1.05968089353644,7.89091137680006));
#265672=CARTESIAN_POINT('Ctrl Pts',(1.1361550814151,1.06242456659007,7.8911805212424));
#265673=CARTESIAN_POINT('Ctrl Pts',(1.12896122891252,1.07008055832774,7.89193203090513));
#265674=CARTESIAN_POINT('Ctrl Pts',(1.1243046280568,1.07497207659651,7.89241274316735));
#265675=CARTESIAN_POINT('Ctrl Pts',(1.09625128525972,1.10405895436659,7.89527579304267));
#265676=CARTESIAN_POINT('Ctrl Pts',(1.07210398950781,1.12752229277917,7.89760434502244));
#265677=CARTESIAN_POINT('Ctrl Pts',(0.91825730188085,1.26759542740874,7.91177412484334));
#265678=CARTESIAN_POINT('Ctrl Pts',(0.770475841595645,1.36248779742735,
7.92272624386276));
#265679=CARTESIAN_POINT('Ctrl Pts',(0.605598892397629,1.43277818241746,
7.93508636522951));
#265680=CARTESIAN_POINT('Ctrl Pts',(0.601170094425466,1.43464206519247,
7.93541834226346));
#265681=CARTESIAN_POINT('Ctrl Pts',(0.578159704862451,1.44420084922901,
7.93714316009448));
#265682=CARTESIAN_POINT('Ctrl Pts',(0.559439533646009,1.45155505605429,
7.93854638720514));
#265683=CARTESIAN_POINT('Ctrl Pts',(0.532628873587588,1.46149193906925,
7.94055866077775));
#265684=CARTESIAN_POINT('Ctrl Pts',(0.524651142286897,1.46437473985649,
7.94115774668733));
#265685=CARTESIAN_POINT('Ctrl Pts',(0.511597302619728,1.46897145976029,
7.94213872303459));
#265686=CARTESIAN_POINT('Ctrl Pts',(0.506535134111979,1.47072468743797,
7.94251930801296));
#265687=CARTESIAN_POINT('Ctrl Pts',(0.495869849559574,1.47435689957113,
7.94332155963113));
#265688=CARTESIAN_POINT('Ctrl Pts',(0.490264892187487,1.47623016793789,
7.9437434072615));
#265689=CARTESIAN_POINT('Ctrl Pts',(0.476799849649903,1.48064526287979,
7.94475747505836));
#265690=CARTESIAN_POINT('Ctrl Pts',(0.468929997378719,1.48315647987392,
7.94535068714778));
#265691=CARTESIAN_POINT('Ctrl Pts',(0.441718424162171,1.49160128371891,
7.94740389332921));
#265692=CARTESIAN_POINT('Ctrl Pts',(0.422281935910763,1.49721990729342,
7.94887404595857));
#265693=CARTESIAN_POINT('Ctrl Pts',(0.375120281843121,1.50986185401646,
7.95245173759724));
#265694=CARTESIAN_POINT('Ctrl Pts',(0.347301152079581,1.51650247644447,
7.95457078053504));
#265695=CARTESIAN_POINT('Ctrl Pts',(0.152721044668739,1.55731550160999,
7.96945553271814));
#265696=CARTESIAN_POINT('Ctrl Pts',(-0.0184402589523456,1.56467212140176,
7.98304228174234));
#265697=CARTESIAN_POINT('Ctrl Pts',(-0.202249216803116,1.54236832477644,
7.99684462788507));
#265698=CARTESIAN_POINT('Ctrl Pts',(-0.217098798676894,1.54034832101533,
7.99795273923506));
#265699=CARTESIAN_POINT('Ctrl Pts',(-0.238234470083694,1.53716147417307,
7.99951788751245));
#265700=CARTESIAN_POINT('Ctrl Pts',(-0.244545590625157,1.53617008118294,
7.99998370275324));
#265701=CARTESIAN_POINT('Ctrl Pts',(-0.254511481761831,1.53454159793358,
8.0007166509895));
#265702=CARTESIAN_POINT('Ctrl Pts',(-0.258170294445346,1.53393028198326,
8.00098518130552));
#265703=CARTESIAN_POINT('Ctrl Pts',(-0.264690632544561,1.53281687064055,
8.00146268690545));
#265704=CARTESIAN_POINT('Ctrl Pts',(-0.267552916491008,1.53231985140351,
8.00167193948902));
#265705=CARTESIAN_POINT('Ctrl Pts',(-0.274371886361038,1.53111608706629,
8.00216960642937));
#265706=CARTESIAN_POINT('Ctrl Pts',(-0.278327240138321,1.5304020231553,
8.00245760334093));
#265707=CARTESIAN_POINT('Ctrl Pts',(-0.290172500371273,1.52821614486414,
8.00331817593359));
#265708=CARTESIAN_POINT('Ctrl Pts',(-0.298053992456243,1.52669855907883,
8.00388824145394));
#265709=CARTESIAN_POINT('Ctrl Pts',(-0.391399048218723,1.5079744873099,
8.01061360755716));
#265710=CARTESIAN_POINT('Ctrl Pts',(-0.475296904680038,1.48367051915359,
8.01640117515553));
#265711=CARTESIAN_POINT('Ctrl Pts',(-0.675038640745276,1.40710951123746,
8.03050681749235));
#265712=CARTESIAN_POINT('Ctrl Pts',(-0.787350601947044,1.34748242581591,
8.03876534231254));
#265713=CARTESIAN_POINT('Ctrl Pts',(-0.905761800256386,1.26471030273796,
8.04879311890734));
#265714=CARTESIAN_POINT('Ctrl Pts',(-0.920162887013234,1.25427142391436,
8.05003638002903));
#265715=CARTESIAN_POINT('Ctrl Pts',(-0.94018249975763,1.23922950647102,
8.05180018777003));
#265716=CARTESIAN_POINT('Ctrl Pts',(-0.9459530192095,1.2348302655848,8.05231284062802));
#265717=CARTESIAN_POINT('Ctrl Pts',(-0.955951634973251,1.2270964572363,
8.05320867774298));
#265718=CARTESIAN_POINT('Ctrl Pts',(-0.960193625093525,1.22377998217461,
8.05359114624131));
#265719=CARTESIAN_POINT('Ctrl Pts',(-0.968867534849446,1.21692567872993,
8.05437821398781));
#265720=CARTESIAN_POINT('Ctrl Pts',(-0.973297493021202,1.21338551011197,
8.05478290256705));
#265721=CARTESIAN_POINT('Ctrl Pts',(-0.983346662927458,1.2052643489925,
8.055707198145));
#265722=CARTESIAN_POINT('Ctrl Pts',(-0.988953368012524,1.20066816524898,
8.05622741087243));
#265723=CARTESIAN_POINT('Ctrl Pts',(-1.00101201611682,1.19064113529947,
8.05735621021343));
#265724=CARTESIAN_POINT('Ctrl Pts',(-1.00745230361953,1.18519670105929,
8.05796533989271));
#265725=CARTESIAN_POINT('Ctrl Pts',(-1.02464008268982,1.17042532736829,
8.05960809504129));
#265726=CARTESIAN_POINT('Ctrl Pts',(-1.03530415450326,1.16100302704433,
8.06064560209993));
#265727=CARTESIAN_POINT('Ctrl Pts',(-1.06800974981506,1.13129688163075,
8.06388562423304));
#265728=CARTESIAN_POINT('Ctrl Pts',(-1.08959456654628,1.11052281400064,
8.06610804271856));
#265729=CARTESIAN_POINT('Ctrl Pts',(-1.17685988271648,1.02154084800991,
8.07545410371289));
#265730=CARTESIAN_POINT('Ctrl Pts',(-1.23683677135708,0.948037675725988,
8.08278659224037));
#265731=CARTESIAN_POINT('Ctrl Pts',(-1.31342154224361,0.834443983160994,
8.09340763237767));
#265732=CARTESIAN_POINT('Ctrl Pts',(-1.33564789414527,0.798384548309486,
8.09668419310973));
#265733=CARTESIAN_POINT('Ctrl Pts',(-1.36516207445875,0.745811564344188,
8.10129358583867));
#265734=CARTESIAN_POINT('Ctrl Pts',(-1.37367692318553,0.730009683604519,
8.102658280228));
#265735=CARTESIAN_POINT('Ctrl Pts',(-1.39441034049294,0.68988459796727,
8.10606612882671));
#265736=CARTESIAN_POINT('Ctrl Pts',(-1.40626831732991,0.665380053068993,
8.10809531623437));
#265737=CARTESIAN_POINT('Ctrl Pts',(-1.42018317087241,0.634588971080162,
8.11057059727069));
#265738=CARTESIAN_POINT('Ctrl Pts',(-1.4228504663441,0.62858567879715,8.11104974353517));
#265739=CARTESIAN_POINT('Ctrl Pts',(-1.42698098787906,0.619128080526867,
8.11179897662974));
#265740=CARTESIAN_POINT('Ctrl Pts',(-1.42846984503033,0.615685165089961,
8.11207056314471));
#265741=CARTESIAN_POINT('Ctrl Pts',(-1.43121475475749,0.609274127607548,
8.11257408126341));
#265742=CARTESIAN_POINT('Ctrl Pts',(-1.43247402632282,0.606307513605492,
8.11280619870262));
#265743=CARTESIAN_POINT('Ctrl Pts',(-1.43532596925313,0.599530372652278,
8.11333448478689));
#265744=CARTESIAN_POINT('Ctrl Pts',(-1.43691269073794,0.595717404482938,
8.1136302926996));
#265745=CARTESIAN_POINT('Ctrl Pts',(-1.44175014153162,0.583960994625517,
8.11453812868929));
#265746=CARTESIAN_POINT('Ctrl Pts',(-1.44495040187356,0.575996752476573,
8.11514722111935));
#265747=CARTESIAN_POINT('Ctrl Pts',(-1.45224261295408,0.557405865129144,
8.11655624172759));
#265748=CARTESIAN_POINT('Ctrl Pts',(-1.45628418123386,0.546759825960961,
8.11735347964851));
#265749=CARTESIAN_POINT('Ctrl Pts',(-1.50866120053581,0.404089323234228,
8.12792178803465));
#265750=CARTESIAN_POINT('Ctrl Pts',(-1.5390041328113,0.266130468189784,
8.13687311818724));
#265751=CARTESIAN_POINT('Ctrl Pts',(-1.55377744778944,0.0842840725283926,
8.14902846580751));
#265752=CARTESIAN_POINT('Ctrl Pts',(-1.55548116180681,0.0424971396828533,
8.15184108608667));
#265753=CARTESIAN_POINT('Ctrl Pts',(-1.55549984464226,0.000695210683922209,
8.15469955740614));
#265754=CARTESIAN_POINT('Ctrl Pts',(-1.55549984541589,0.000693477583077501,
8.1546996759179));
#265755=CARTESIAN_POINT('Ctrl Pts',(-1.55551244193536,-0.0275610537365116,
8.15663175905029));
#265756=CARTESIAN_POINT('Ctrl Pts',(-1.55475520526371,-0.0558094470224839,
8.15858374748494));
#265757=CARTESIAN_POINT('Ctrl Pts',(-1.55275005271705,-0.0928773194767488,
8.16117949874512));
#265758=CARTESIAN_POINT('Ctrl Pts',(-1.55219521431651,-0.101729708683359,
8.16180197062797));
#265759=CARTESIAN_POINT('Ctrl Pts',(-1.55112211179105,-0.116787020498887,
8.16286536690637));
#265760=CARTESIAN_POINT('Ctrl Pts',(-1.55064223989501,-0.122994535146789,
8.16330509806123));
#265761=CARTESIAN_POINT('Ctrl Pts',(-1.54967842768822,-0.134558327597623,
8.16412683505985));
#265762=CARTESIAN_POINT('Ctrl Pts',(-1.54920394879388,-0.139915318991582,
8.16450854067227));
#265763=CARTESIAN_POINT('Ctrl Pts',(-1.54818471353681,-0.150781257181499,
8.16528492657029));
#265764=CARTESIAN_POINT('Ctrl Pts',(-1.54763831026069,-0.156289967383135,
8.16567965304291));
#265765=CARTESIAN_POINT('Ctrl Pts',(-1.54629651323254,-0.169120008274647,
8.16660166535254));
#265766=CARTESIAN_POINT('Ctrl Pts',(-1.54547851332105,-0.176438786676814,
8.16712965264073));
#265767=CARTESIAN_POINT('Ctrl Pts',(-1.5432187838445,-0.195434006353405,
8.16850542309485));
#265768=CARTESIAN_POINT('Ctrl Pts',(-1.54169652016432,-0.207100196109016,
8.16935571296635));
#265769=CARTESIAN_POINT('Ctrl Pts',(-1.53458140822736,-0.257192479572518,
8.17303044559702));
#265770=CARTESIAN_POINT('Ctrl Pts',(-1.52768355327927,-0.295415877311185,
8.17589525876432));
#265771=CARTESIAN_POINT('Ctrl Pts',(-1.4880610929816,-0.476015974110608,
8.18973221108268));
#265772=CARTESIAN_POINT('Ctrl Pts',(-1.43681605042174,-0.613566951592995,
8.20126562593808));
#265773=CARTESIAN_POINT('Ctrl Pts',(-1.34874398360052,-0.775861864746508,
8.21532888814008));
#265774=CARTESIAN_POINT('Ctrl Pts',(-1.32906243806224,-0.809114098102147,
8.21823095575528));
#265775=CARTESIAN_POINT('Ctrl Pts',(-1.30437138717968,-0.847493126873946,
8.22157678999231));
#265776=CARTESIAN_POINT('Ctrl Pts',(-1.3005416550474,-0.85335849691161,
8.22208801214488));
#265777=CARTESIAN_POINT('Ctrl Pts',(-1.29456988272814,-0.862370892743268,
8.22287311261104));
#265778=CARTESIAN_POINT('Ctrl Pts',(-1.29245576033801,-0.865536161191009,
8.22314877020993));
#265779=CARTESIAN_POINT('Ctrl Pts',(-1.288533175707,-0.871362643832293,
8.223655994387));
#265780=CARTESIAN_POINT('Ctrl Pts',(-1.28672808660578,-0.874025991316987,
8.22388777160646));
#265781=CARTESIAN_POINT('Ctrl Pts',(-1.28262892148569,-0.880033947065127,
8.22441044702358));
#265782=CARTESIAN_POINT('Ctrl Pts',(-1.2803300236797,-0.883375191915229,
8.22470101522176));
#265783=CARTESIAN_POINT('Ctrl Pts',(-1.27348971330408,-0.893234182090516,
8.22555818849869));
#265784=CARTESIAN_POINT('Ctrl Pts',(-1.26891131982115,-0.899726304753611,
8.22612236931559));
#265785=CARTESIAN_POINT('Ctrl Pts',(-1.23122461094052,-0.952305819261857,
8.2306920474689));
#265786=CARTESIAN_POINT('Ctrl Pts',(-1.1956622249532,-0.996591178561573,
8.23454392134266));
#265787=CARTESIAN_POINT('Ctrl Pts',(-1.08738312172775,-1.1172649361665,
8.24536949961092));
#265788=CARTESIAN_POINT('Ctrl Pts',(-1.00922571578585,-1.18833810846182,
8.2521792645424));
#265789=CARTESIAN_POINT('Ctrl Pts',(-0.891813400720532,-1.27510750763813,
8.26195329623408));
#265790=CARTESIAN_POINT('Ctrl Pts',(-0.858214452678401,-1.29795910761857,
8.26470255861118));
#265791=CARTESIAN_POINT('Ctrl Pts',(-0.808824990976642,-1.32879360651692,
8.26870880145344));
#265792=CARTESIAN_POINT('Ctrl Pts',(-0.793731531196933,-1.3378641670446,
8.26992853616171));
#265793=CARTESIAN_POINT('Ctrl Pts',(-0.770024961148751,-1.35156848268343,
8.27183939208041));
#265794=CARTESIAN_POINT('Ctrl Pts',(-0.761516328677205,-1.35638072743053,
8.27252425541972));
#265795=CARTESIAN_POINT('Ctrl Pts',(-0.745483964851621,-1.36524978059206,
8.27381326905052));
#265796=CARTESIAN_POINT('Ctrl Pts',(-0.737971020715449,-1.36932540786271,
8.27441673131353));
#265797=CARTESIAN_POINT('Ctrl Pts',(-0.725213945074318,-1.37611039546432,
8.27544063255058));
#265798=CARTESIAN_POINT('Ctrl Pts',(-0.719987222419312,-1.37885223444655,
8.27585991592883));
#265799=CARTESIAN_POINT('Ctrl Pts',(-0.709527589709048,-1.3842634711791,
8.27669860793923));
#265800=CARTESIAN_POINT('Ctrl Pts',(-0.704294910821525,-1.38693310402755,
8.27711799977296));
#265801=CARTESIAN_POINT('Ctrl Pts',(-0.692728956386209,-1.39275154554504,
8.27804465802654));
#265802=CARTESIAN_POINT('Ctrl Pts',(-0.686389104643297,-1.39588691110642,
8.27855238301017));
#265803=CARTESIAN_POINT('Ctrl Pts',(-0.663983446606174,-1.40677805405715,
8.28034612251041));
#265804=CARTESIAN_POINT('Ctrl Pts',(-0.647806371713254,-1.41430030980481,
8.28164013901022));
#265805=CARTESIAN_POINT('Ctrl Pts',(-0.512491814695007,-1.47441226928871,
8.29245971060249));
#265806=CARTESIAN_POINT('Ctrl Pts',(-0.387335072559399,-1.51211650823842,
8.3025050722933));
#265807=CARTESIAN_POINT('Ctrl Pts',(-0.183365180826234,-1.54655688073541,
8.31854055383755));
#265808=CARTESIAN_POINT('Ctrl Pts',(-0.106900169584929,-1.55371682464372,
8.32446377851203));
#265809=CARTESIAN_POINT('Ctrl Pts',(-0.0170093461110924,-1.55546304857193,
8.33112977073088));
#265810=CARTESIAN_POINT('Ctrl Pts',(-0.00380383773568808,-1.55555140555301,
8.33210139524807));
#265811=CARTESIAN_POINT('Ctrl Pts',(0.0143113180819958,-1.55544191170809,
8.33342236134905));
#265812=CARTESIAN_POINT('Ctrl Pts',(0.0192207864782227,-1.55538899239275,
8.33377916317426));
#265813=CARTESIAN_POINT('Ctrl Pts',(0.0274773969647955,-1.55526089462312,
8.33437711564759));
#265814=CARTESIAN_POINT('Ctrl Pts',(0.030824659769978,-1.55519815418104,
8.33461894534316));
#265815=CARTESIAN_POINT('Ctrl Pts',(0.0371833147952799,-1.55505843138009,
8.33507720001624));
#265816=CARTESIAN_POINT('Ctrl Pts',(0.0401947167397025,-1.55498350765366,
8.3352937413044));
#265817=CARTESIAN_POINT('Ctrl Pts',(0.048100675981779,-1.55476382519448,
8.33586101039787));
#265818=CARTESIAN_POINT('Ctrl Pts',(0.0529948541975249,-1.55460470034463,
8.33621094419673));
#265819=CARTESIAN_POINT('Ctrl Pts',(0.0700577243134016,-1.55396926154776,
8.3374268945739));
#265820=CARTESIAN_POINT('Ctrl Pts',(0.0822219186751048,-1.55337314608538,
8.33828657539033));
#265821=CARTESIAN_POINT('Ctrl Pts',(0.189904609910514,-1.54682755096889,
8.34584330448779));
#265822=CARTESIAN_POINT('Ctrl Pts',(0.284706751868626,-1.53221637266549,
8.35213025716064));
#265823=CARTESIAN_POINT('Ctrl Pts',(0.489974097122149,-1.48085445827633,
8.36605780251259));
#265824=CARTESIAN_POINT('Ctrl Pts',(0.598861091612789,-1.44026555854898,
8.37368077995249));
#265825=CARTESIAN_POINT('Ctrl Pts',(0.715983769892291,-1.38100876611635,
8.38282184065024));
#265826=CARTESIAN_POINT('Ctrl Pts',(0.729636696281835,-1.37384432615348,
8.38390226794513));
#265827=CARTESIAN_POINT('Ctrl Pts',(0.749691127121491,-1.36293741271369,
8.38551259198718));
#265828=CARTESIAN_POINT('Ctrl Pts',(0.756176307316571,-1.35935005273988,
8.38603700206355));
#265829=CARTESIAN_POINT('Ctrl Pts',(0.767667799366387,-1.35288570745279,
8.38697291250531));
#265830=CARTESIAN_POINT('Ctrl Pts',(0.77268423118742,-1.35002691263698,
8.38738375623345));
#265831=CARTESIAN_POINT('Ctrl Pts',(0.78321698762521,-1.3439465049668,8.38825128139421));
#265832=CARTESIAN_POINT('Ctrl Pts',(0.788729601884819,-1.34071871426513,
8.38870818002621));
#265833=CARTESIAN_POINT('Ctrl Pts',(0.803269051301569,-1.3320847535513,
8.38992092757991));
#265834=CARTESIAN_POINT('Ctrl Pts',(0.812261045021169,-1.32662087427383,
8.39067886258509));
#265835=CARTESIAN_POINT('Ctrl Pts',(0.850821362833999,-1.3026511416881,
8.39396403196277));
#265836=CARTESIAN_POINT('Ctrl Pts',(0.879815810956882,-1.28324618304458,
8.39652405763323));
#265837=CARTESIAN_POINT('Ctrl Pts',(1.0182149848856,-1.18372429314097,8.40920365416642));
#265838=CARTESIAN_POINT('Ctrl Pts',(1.11746302435258,-1.09051780445893,
8.41982343343961));
#265839=CARTESIAN_POINT('Ctrl Pts',(1.23605321658796,-0.945735629460135,
8.43422792636109));
#265840=CARTESIAN_POINT('Ctrl Pts',(1.26675074408639,-0.904205276125732,
8.43815510800583));
#265841=CARTESIAN_POINT('Ctrl Pts',(1.30135394670512,-0.852159935255421,
8.44277167605445));
#265842=CARTESIAN_POINT('Ctrl Pts',(1.30728342132691,-0.843035422761084,
8.44357019096705));
#265843=CARTESIAN_POINT('Ctrl Pts',(1.31555406803297,-0.830011092872329,
8.44469388930826));
#265844=CARTESIAN_POINT('Ctrl Pts',(1.3179744641749,-0.826162352933088,
8.44502397726409));
#265845=CARTESIAN_POINT('Ctrl Pts',(1.32211131616985,-0.81951977910019,
8.44559022517637));
#265846=CARTESIAN_POINT('Ctrl Pts',(1.32383586434436,-0.816731048646797,
8.44582690949355));
#265847=CARTESIAN_POINT('Ctrl Pts',(1.32739993131185,-0.810926722507489,
8.44631734578963));
#265848=CARTESIAN_POINT('Ctrl Pts',(1.3292380063044,-0.807910298360363,
8.44657100449176));
#265849=CARTESIAN_POINT('Ctrl Pts',(1.33404494526406,-0.799960924884837,
8.44723637418835));
#265850=CARTESIAN_POINT('Ctrl Pts',(1.33699676246489,-0.795017645888552,
8.44764699291721));
#265851=CARTESIAN_POINT('Ctrl Pts',(1.3491905121833,-0.774337312145648,
8.44935228504416));
#265852=CARTESIAN_POINT('Ctrl Pts',(1.35818305471665,-0.758453807609469,
8.45063191425919));
#265853=CARTESIAN_POINT('Ctrl Pts',(1.44007360680162,-0.607681298488383,
8.46253424349309));
#265854=CARTESIAN_POINT('Ctrl Pts',(1.49294033200526,-0.462852173570799,
8.47222293855819));
#265855=CARTESIAN_POINT('Ctrl Pts',(1.53127017564436,-0.276020082219223,
8.48503002308784));
#265856=CARTESIAN_POINT('Ctrl Pts',(1.53745600752223,-0.239173856146586,
8.48756523609307));
#265857=CARTESIAN_POINT('Ctrl Pts',(1.5455232677581,-0.177622247026707,
8.49184336619711));
#265858=CARTESIAN_POINT('Ctrl Pts',(1.54815166592574,-0.153029849557383,
8.49356385512024));
#265859=CARTESIAN_POINT('Ctrl Pts',(1.55092970867647,-0.119486563925837,
8.49593056843196));
#265860=CARTESIAN_POINT('Ctrl Pts',(1.5515901191088,-0.11058072412401,8.49656084221378));
#265861=CARTESIAN_POINT('Ctrl Pts',(1.55256877394082,-0.0956397921955695,
8.4976216397552));
#265862=CARTESIAN_POINT('Ctrl Pts',(1.55292860474211,-0.0896075575141326,
8.49805085678861));
#265863=CARTESIAN_POINT('Ctrl Pts',(1.55356803438445,-0.0777234470354274,
8.49889836466892));
#265864=CARTESIAN_POINT('Ctrl Pts',(1.55384974080651,-0.0718717813026383,
8.49931658235498));
#265865=CARTESIAN_POINT('Ctrl Pts',(1.55439592261739,-0.0590145182079294,
8.50023755327579));
#265866=CARTESIAN_POINT('Ctrl Pts',(1.554646105391,-0.0520084764169287,
8.50074074441379));
#265867=CARTESIAN_POINT('Ctrl Pts',(1.55535375237179,-0.027558308799545,
8.50250166755727));
#265868=CARTESIAN_POINT('Ctrl Pts',(1.55556501577039,-0.0101089593831158,
8.50376701847313));
#265869=CARTESIAN_POINT('Ctrl Pts',(1.55485085571641,0.141242898917533,
8.51482172073673));
#265870=CARTESIAN_POINT('Ctrl Pts',(1.53693109243143,0.274477213372955,
8.52516514656097));
#265871=CARTESIAN_POINT('Ctrl Pts',(1.484104561208,0.471030322134393,8.54093747456058));
#265872=CARTESIAN_POINT('Ctrl Pts',(1.46151586399023,0.537036359679634,
8.54631269398345));
#265873=CARTESIAN_POINT('Ctrl Pts',(1.43457668241997,0.601306903550017,
8.55150209358323));
#265874=CARTESIAN_POINT('Origin',(0.,0.,-1.29405622560371));
#265875=CARTESIAN_POINT('',(1.43457668359376,0.601306900749626,9.38971141570882));
#265876=CARTESIAN_POINT('',(1.43457655129078,0.601307216393289,9.25009119722734));
#265877=CARTESIAN_POINT('',(1.43457668357355,0.601306900797845,-1.29405622560371));
#265878=CARTESIAN_POINT('',(-1.55786019784847,-0.000159437891840058,8.99395693065775));
#265879=CARTESIAN_POINT('Ctrl Pts',(1.43457668359376,0.601306900749626,
9.38971141570882));
#265880=CARTESIAN_POINT('Ctrl Pts',(1.43708782974321,0.59531589730263,9.38925480768558));
#265881=CARTESIAN_POINT('Ctrl Pts',(1.43956140763381,0.589309257252912,
9.3887969624209));
#265882=CARTESIAN_POINT('Ctrl Pts',(1.44448384727649,0.577140049795941,
9.38786918830465));
#265883=CARTESIAN_POINT('Ctrl Pts',(1.44693105037016,0.570977018036914,
9.38739921991267));
#265884=CARTESIAN_POINT('Ctrl Pts',(1.45137486284903,0.559573679883019,
9.38652936498683));
#265885=CARTESIAN_POINT('Ctrl Pts',(1.45338269392861,0.554337838511073,
9.38612986247685));
#265886=CARTESIAN_POINT('Ctrl Pts',(1.45776990785797,0.542709563069248,
9.38524230590606));
#265887=CARTESIAN_POINT('Ctrl Pts',(1.46013563181875,0.536312136776179,
9.38475380546448));
#265888=CARTESIAN_POINT('Ctrl Pts',(1.46680529529987,0.517904662512241,
9.38334752778272));
#265889=CARTESIAN_POINT('Ctrl Pts',(1.47100356448313,0.50585720219307,9.38242627721276));
#265890=CARTESIAN_POINT('Ctrl Pts',(1.502679910392,0.411227603627131,9.3751815920839));
#265891=CARTESIAN_POINT('Ctrl Pts',(1.52332624045224,0.32653810716284,9.36863416421773));
#265892=CARTESIAN_POINT('Ctrl Pts',(1.55089160657538,0.150456047651188,
9.35493523266033));
#265893=CARTESIAN_POINT('Ctrl Pts',(1.55704487368799,0.0592675873812509,
9.34779588125369));
#265894=CARTESIAN_POINT('Ctrl Pts',(1.554950757354,-0.0427167520753653,
9.33999099470973));
#265895=CARTESIAN_POINT('Ctrl Pts',(1.55461718296239,-0.0534976892118548,
9.33916836363109));
#265896=CARTESIAN_POINT('Ctrl Pts',(1.55273367216501,-0.0990413922451764,
9.33570553358018));
#265897=CARTESIAN_POINT('Ctrl Pts',(1.55012949824933,-0.133753731040844,
9.33309649786047));
#265898=CARTESIAN_POINT('Ctrl Pts',(1.54566909894136,-0.174723661316817,
9.33007416584904));
#265899=CARTESIAN_POINT('Ctrl Pts',(1.54493610074346,-0.181090501291612,
9.32960613141598));
#265900=CARTESIAN_POINT('Ctrl Pts',(1.54367825470275,-0.191452152488843,
9.32884730646945));
#265901=CARTESIAN_POINT('Ctrl Pts',(1.54317720960378,-0.195449690426616,
9.32855524849525));
#265902=CARTESIAN_POINT('Ctrl Pts',(1.54225311823264,-0.202597311335451,
9.32803434909998));
#265903=CARTESIAN_POINT('Ctrl Pts',(1.54183594517856,-0.205748074262633,
9.32780518648238));
#265904=CARTESIAN_POINT('Ctrl Pts',(1.54090733402752,-0.212600089139369,
9.32730782159261));
#265905=CARTESIAN_POINT('Ctrl Pts',(1.54039221751622,-0.216300778946665,
9.3270398285977));
#265906=CARTESIAN_POINT('Ctrl Pts',(1.53890020230165,-0.226743979105504,
9.32628524355941));
#265907=CARTESIAN_POINT('Ctrl Pts',(1.53789231821848,-0.233482091007748,
9.32580035375259));
#265908=CARTESIAN_POINT('Ctrl Pts',(1.53129768603991,-0.275673285368937,
9.32277535445665));
#265909=CARTESIAN_POINT('Ctrl Pts',(1.52452904303368,-0.310934195779292,
9.32029670515759));
#265910=CARTESIAN_POINT('Ctrl Pts',(1.49645596996693,-0.434004670457138,
9.31171915445632));
#265911=CARTESIAN_POINT('Ctrl Pts',(1.46873082809848,-0.520166288232315,
9.30583967550527));
#265912=CARTESIAN_POINT('Ctrl Pts',(1.39593911572236,-0.693108312589602,
9.29346503308832));
#265913=CARTESIAN_POINT('Ctrl Pts',(1.34987471105787,-0.779024492887918,
9.28697864986752));
#265914=CARTESIAN_POINT('Ctrl Pts',(1.28949204232985,-0.870019024575766,
9.27935186945889));
#265915=CARTESIAN_POINT('Ctrl Pts',(1.28277559157784,-0.879891810432988,
9.27851388472833));
#265916=CARTESIAN_POINT('Ctrl Pts',(1.27177663628408,-0.895665999834283,
9.27715741122022));
#265917=CARTESIAN_POINT('Ctrl Pts',(1.26756504606718,-0.901616463126115,
9.27664160918329));
#265918=CARTESIAN_POINT('Ctrl Pts',(1.25997870785372,-0.912176815841824,
9.27571873238146));
#265919=CARTESIAN_POINT('Ctrl Pts',(1.25662007403171,-0.916798165110904,
9.27531228195168));
#265920=CARTESIAN_POINT('Ctrl Pts',(1.2495293832226,-0.926442512273304,
9.27445854994562));
#265921=CARTESIAN_POINT('Ctrl Pts',(1.24579232860497,-0.93146169001161,
9.27401107922755));
#265922=CARTESIAN_POINT('Ctrl Pts',(1.23590712222881,-0.944572447064959,
9.27283379027277));
#265923=CARTESIAN_POINT('Ctrl Pts',(1.22970987159247,-0.952626445741894,
9.27210205667022));
#265924=CARTESIAN_POINT('Ctrl Pts',(1.20108555357693,-0.989082078169204,
9.26875021014017));
#265925=CARTESIAN_POINT('Ctrl Pts',(1.17775222723403,-1.01675422411608,
9.2660942621835));
#265926=CARTESIAN_POINT('Ctrl Pts',(1.06269048508816,-1.14393216648936,
9.2533311911762));
#265927=CARTESIAN_POINT('Ctrl Pts',(0.959206442916029,-1.2319913831661,
9.24272983267382));
#265928=CARTESIAN_POINT('Ctrl Pts',(0.798833805246429,-1.33587377223353,
9.22802347072433));
#265929=CARTESIAN_POINT('Ctrl Pts',(0.750393671296776,-1.36367338065486,
9.22378151251973));
#265930=CARTESIAN_POINT('Ctrl Pts',(0.693574904321774,-1.39233447116312,
9.21910651229777));
#265931=CARTESIAN_POINT('Ctrl Pts',(0.686564799796904,-1.39580450279551,
9.21853478569913));
#265932=CARTESIAN_POINT('Ctrl Pts',(0.67593036465239,-1.40096909078124,
9.21767541117008));
#265933=CARTESIAN_POINT('Ctrl Pts',(0.672325322353087,-1.4027027172853,
9.21738545518905));
#265934=CARTESIAN_POINT('Ctrl Pts',(0.665845668532286,-1.4057879944465,
9.2168667970653));
#265935=CARTESIAN_POINT('Ctrl Pts',(0.66297358222074,-1.40714475784646,
9.21663778568924));
#265936=CARTESIAN_POINT('Ctrl Pts',(0.656693993042301,-1.41008771915786,
9.21613899712574));
#265937=CARTESIAN_POINT('Ctrl Pts',(0.653284895777016,-1.41167036590579,
9.21586943888595));
#265938=CARTESIAN_POINT('Ctrl Pts',(0.643586594910419,-1.41613007004704,
9.21510597516643));
#265939=CARTESIAN_POINT('Ctrl Pts',(0.637283786663551,-1.41897761097587,
9.21461383622869));
#265940=CARTESIAN_POINT('Ctrl Pts',(0.596207884186789,-1.43720636569848,
9.21143126205587));
#265941=CARTESIAN_POINT('Ctrl Pts',(0.560896216417073,-1.45135178853981,
9.2088099338956));
#265942=CARTESIAN_POINT('Ctrl Pts',(0.421501637436629,-1.50134244486121,
9.19876834908841));
#265943=CARTESIAN_POINT('Ctrl Pts',(0.314248318636299,-1.52739794544497,
9.19167233571938));
#265944=CARTESIAN_POINT('Ctrl Pts',(0.130036948838862,-1.55190538356977,
9.17932935659739));
#265945=CARTESIAN_POINT('Ctrl Pts',(0.0543187616693528,-1.55639548479748,
9.17421689624834));
#265946=CARTESIAN_POINT('Ctrl Pts',(-0.03308692001655,-1.55519184969553,
9.16810953719753));
#265947=CARTESIAN_POINT('Ctrl Pts',(-0.0447531224733314,-1.55489986128824,
9.16729031136669));
#265948=CARTESIAN_POINT('Ctrl Pts',(-0.0636978486098668,-1.55421232422148,
9.16595283738004));
#265949=CARTESIAN_POINT('Ctrl Pts',(-0.0709789740614843,-1.55389682625837,
9.1654370863183));
#265950=CARTESIAN_POINT('Ctrl Pts',(-0.083947558787496,-1.55324354698987,
9.16451529420166));
#265951=CARTESIAN_POINT('Ctrl Pts',(-0.089635926527065,-1.55292566080488,
9.16410988204529));
#265952=CARTESIAN_POINT('Ctrl Pts',(-0.101633093109031,-1.55218907996871,
9.16325247746616));
#265953=CARTESIAN_POINT('Ctrl Pts',(-0.107941326798252,-1.55176315634095,
9.16280026595736));
#265954=CARTESIAN_POINT('Ctrl Pts',(-0.124675497895407,-1.55053075424559,
9.1615969031419));
#265955=CARTESIAN_POINT('Ctrl Pts',(-0.135096039160965,-1.54965759118301,
9.16084367912342));
#265956=CARTESIAN_POINT('Ctrl Pts',(-0.184794427023072,-1.54498816071306,
9.15723217088881));
#265957=CARTESIAN_POINT('Ctrl Pts',(-0.2239238094753,-1.53980356022411,
9.1543308907466));
#265958=CARTESIAN_POINT('Ctrl Pts',(-0.410048982104664,-1.50789795051632,
9.14023845424061));
#265959=CARTESIAN_POINT('Ctrl Pts',(-0.552875578340974,-1.46157820652359,
9.12844228588015));
#265960=CARTESIAN_POINT('Ctrl Pts',(-0.721762028534701,-1.37846019630435,
9.11409711253588));
#265961=CARTESIAN_POINT('Ctrl Pts',(-0.756005457253897,-1.35998136604669,
9.11117246334961));
#265962=CARTESIAN_POINT('Ctrl Pts',(-0.795720985351208,-1.33658524018408,
9.10779036250197));
#265963=CARTESIAN_POINT('Ctrl Pts',(-0.801893410212408,-1.33289120142185,
9.10726503162118));
#265964=CARTESIAN_POINT('Ctrl Pts',(-0.811369857228142,-1.32713013278613,
9.10645922271762));
#265965=CARTESIAN_POINT('Ctrl Pts',(-0.814692000188145,-1.32509334776792,
9.10617687020374));
#265966=CARTESIAN_POINT('Ctrl Pts',(-0.820654653568288,-1.32140678180109,
9.10567039636167));
#265967=CARTESIAN_POINT('Ctrl Pts',(-0.823297871655288,-1.31976155363469,
9.10544598877598));
#265968=CARTESIAN_POINT('Ctrl Pts',(-0.829104539703971,-1.31612305349541,
9.10495324606138));
#265969=CARTESIAN_POINT('Ctrl Pts',(-0.832265743548619,-1.31412631151305,
9.10468514359611));
#265970=CARTESIAN_POINT('Ctrl Pts',(-0.838844900947324,-1.30993739144024,
9.10412741121316));
#265971=CARTESIAN_POINT('Ctrl Pts',(-0.842261538605066,-1.30774318537765,
9.10383791417431));
#265972=CARTESIAN_POINT('Ctrl Pts',(-0.8510686045647,-1.30203834826217,
9.1030919321819));
#265973=CARTESIAN_POINT('Ctrl Pts',(-0.856445986912409,-1.29850756839574,
9.1026367012634));
#265974=CARTESIAN_POINT('Ctrl Pts',(-0.872244722920112,-1.28799330753161,
9.10129947321614));
#265975=CARTESIAN_POINT('Ctrl Pts',(-0.882603961824333,-1.28091681528722,
9.10042296128793));
#265976=CARTESIAN_POINT('Ctrl Pts',(-0.919532160059527,-1.25503008217532,
9.09729507261248));
#265977=CARTESIAN_POINT('Ctrl Pts',(-0.945596347514915,-1.23551113238845,
9.09508102422457));
#265978=CARTESIAN_POINT('Ctrl Pts',(-1.02755900790384,-1.17001649347504,
9.08802938135205));
#265979=CARTESIAN_POINT('Ctrl Pts',(-1.0808695580341,-1.12095414855578,
9.08329936039649));
#265980=CARTESIAN_POINT('Ctrl Pts',(-1.20085631060762,-0.993979871023113,
9.07178861950553));
#265981=CARTESIAN_POINT('Ctrl Pts',(-1.26361801551808,-0.912861827809228,
9.06498491870761));
#265982=CARTESIAN_POINT('Ctrl Pts',(-1.32425082194038,-0.816137499257763,
9.0570112643999));
#265983=CARTESIAN_POINT('Ctrl Pts',(-1.33042931883999,-0.806026346372209,
9.05617960397344));
#265984=CARTESIAN_POINT('Ctrl Pts',(-1.34024787976547,-0.78953769599985,
9.05482583732866));
#265985=CARTESIAN_POINT('Ctrl Pts',(-1.34395944369447,-0.783203142861648,
9.0543063308309));
#265986=CARTESIAN_POINT('Ctrl Pts',(-1.35047453122471,-0.771901110008587,
9.05338033180251));
#265987=CARTESIAN_POINT('Ctrl Pts',(-1.35329585806625,-0.766944001914903,
9.05297448964885));
#265988=CARTESIAN_POINT('Ctrl Pts',(-1.35917282831588,-0.756484688098322,
9.05211875231449));
#265989=CARTESIAN_POINT('Ctrl Pts',(-1.3622224618819,-0.750979242558053,
9.05166865125024));
#265990=CARTESIAN_POINT('Ctrl Pts',(-1.37018709592266,-0.736392690734526,
9.05047689615475));
#265991=CARTESIAN_POINT('Ctrl Pts',(-1.37504515341261,-0.727281024994862,
9.04973324006295));
#265992=CARTESIAN_POINT('Ctrl Pts',(-1.39733941673783,-0.684444434102731,
9.04624014078062));
#265993=CARTESIAN_POINT('Ctrl Pts',(-1.41362643656675,-0.650139571347242,
9.04345105471816));
#265994=CARTESIAN_POINT('Ctrl Pts',(-1.48811712682496,-0.477175770179261,
9.02941492504455));
#265995=CARTESIAN_POINT('Ctrl Pts',(-1.52724876445989,-0.331188207408493,
9.01754441939057));
#265996=CARTESIAN_POINT('Ctrl Pts',(-1.54810063201712,-0.154104849470554,
9.0039485522831));
#265997=CARTESIAN_POINT('Ctrl Pts',(-1.55062342261023,-0.126218411708337,
9.00183410260287));
#265998=CARTESIAN_POINT('Ctrl Pts',(-1.55336170101859,-0.0829644403757517,
8.99860940119671));
#265999=CARTESIAN_POINT('Ctrl Pts',(-1.55410453770933,-0.0676373139414937,
8.99747738523281));
#266000=CARTESIAN_POINT('Ctrl Pts',(-1.55480004012722,-0.0469638390379281,
8.99596701961603));
#266001=CARTESIAN_POINT('Ctrl Pts',(-1.55495211093905,-0.0416257360374791,
8.99557851124372));
#266002=CARTESIAN_POINT('Ctrl Pts',(-1.55514835847844,-0.0332155277550246,
8.99496885980852));
#266003=CARTESIAN_POINT('Ctrl Pts',(-1.55521092786053,-0.0301439624707253,
8.99474671740288));
#266004=CARTESIAN_POINT('Ctrl Pts',(-1.55531754705947,-0.0240188204175105,
8.99430478429321));
#266005=CARTESIAN_POINT('Ctrl Pts',(-1.55536170413299,-0.0209653386465418,
8.99408499822506));
#266006=CARTESIAN_POINT('Ctrl Pts',(-1.55543652242247,-0.0144683391402729,
8.99361843759601));
#266007=CARTESIAN_POINT('Ctrl Pts',(-1.55546474138346,-0.0110248379756254,
8.99337180139868));
#266008=CARTESIAN_POINT('Ctrl Pts',(-1.55549342183002,-0.00514031481975871,
8.99295139280277));
#266009=CARTESIAN_POINT('Ctrl Pts',(-1.55549957307726,-0.00269935885603639,
8.99277731573819));
#266010=CARTESIAN_POINT('Ctrl Pts',(-1.55549997854072,-0.000258379212321887,
8.99260354023743));
#266011=CARTESIAN_POINT('Ctrl Pts',(1.43456415251406,0.601298694836608,
8.68837676241653));
#266012=CARTESIAN_POINT('Ctrl Pts',(1.27769209139973,0.965209298280632,
8.71676603012681));
#266013=CARTESIAN_POINT('Ctrl Pts',(0.593832905914069,1.67495416287262,
8.78220722642894));
#266014=CARTESIAN_POINT('Ctrl Pts',(-1.01228645751357,1.52943817244966,
8.8841003002866));
#266015=CARTESIAN_POINT('Ctrl Pts',(-1.55731054943609,0.506487777198142,
8.95760410643398));
#266016=CARTESIAN_POINT('Ctrl Pts',(-1.55803294000962,-0.000152196472590984,
8.9940559839895));
#266017=CARTESIAN_POINT('Ctrl Pts',(1.43457668241997,0.601306903550017,
8.55150209358323));
#266018=CARTESIAN_POINT('Ctrl Pts',(1.43294790499825,0.605192782950805,
8.55181585132967));
#266019=CARTESIAN_POINT('Ctrl Pts',(1.43130322378101,0.609072319093551,
8.55212891636632));
#266020=CARTESIAN_POINT('Ctrl Pts',(1.42452938068502,0.624871727868597,
8.55340300328474));
#266021=CARTESIAN_POINT('Ctrl Pts',(1.41926682430825,0.636734123311139,
8.55435758008135));
#266022=CARTESIAN_POINT('Ctrl Pts',(1.4118231888063,0.652961952056135,8.5556593120359));
#266023=CARTESIAN_POINT('Ctrl Pts',(1.40976930475961,0.657384618296571,
8.55601365367349));
#266024=CARTESIAN_POINT('Ctrl Pts',(1.40627318000372,0.664821145362487,
8.55660865427335));
#266025=CARTESIAN_POINT('Ctrl Pts',(1.4048419793831,0.667840119964732,8.55684997783004));
#266026=CARTESIAN_POINT('Ctrl Pts',(1.40209925353854,0.673577793675263,
8.5573081591844));
#266027=CARTESIAN_POINT('Ctrl Pts',(1.40078952982971,0.676297312171823,
8.5575251289057));
#266028=CARTESIAN_POINT('Ctrl Pts',(1.39731990249647,0.683448347075764,
8.55809518131543));
#266029=CARTESIAN_POINT('Ctrl Pts',(1.39514680971701,0.687873487020718,
8.55844745492299));
#266030=CARTESIAN_POINT('Ctrl Pts',(1.38744511501492,0.703370060084105,
8.55967966761848));
#266031=CARTESIAN_POINT('Ctrl Pts',(1.38180527781063,0.714386161877841,
8.56055304538535));
#266032=CARTESIAN_POINT('Ctrl Pts',(1.3377637669938,0.797937479593499,8.56716652542998));
#266033=CARTESIAN_POINT('Ctrl Pts',(1.29380119009789,0.867409091330136,
8.57260762206276));
#266034=CARTESIAN_POINT('Ctrl Pts',(1.2205720385713,0.965081595183283,8.58065486027094));
#266035=CARTESIAN_POINT('Ctrl Pts',(1.19536561268969,0.996132333608182,
8.58327948272111));
#266036=CARTESIAN_POINT('Ctrl Pts',(1.10759113573785,1.09612243001964,8.5920647709369));
#266037=CARTESIAN_POINT('Ctrl Pts',(1.04004740167493,1.16040509418459,8.59828717763937));
#266038=CARTESIAN_POINT('Ctrl Pts',(0.956991100698802,1.22634302913323,
8.60569621180159));
#266039=CARTESIAN_POINT('Ctrl Pts',(0.946710687737284,1.2342965800921,8.60660912083667));
#266040=CARTESIAN_POINT('Ctrl Pts',(0.930803212418372,1.24628791549676,
8.60801609844018));
#266041=CARTESIAN_POINT('Ctrl Pts',(0.92524666303307,1.25041864921468,8.60850652985363));
#266042=CARTESIAN_POINT('Ctrl Pts',(0.91508175162889,1.25787038362365,8.60940194129295));
#266043=CARTESIAN_POINT('Ctrl Pts',(0.910482397524518,1.26120351902126,
8.6098064427075));
#266044=CARTESIAN_POINT('Ctrl Pts',(0.900415563992273,1.2684151518989,8.61069044981573));
#266045=CARTESIAN_POINT('Ctrl Pts',(0.894941084224529,1.27228363135493,
8.61117032897003));
#266046=CARTESIAN_POINT('Ctrl Pts',(0.879889594374731,1.28277438548819,
8.61248748947261));
#266047=CARTESIAN_POINT('Ctrl Pts',(0.870263134664788,1.28932458484947,
8.61332747572133));
#266048=CARTESIAN_POINT('Ctrl Pts',(0.819552601233491,1.32300325537439,
8.61774073083784));
#266049=CARTESIAN_POINT('Ctrl Pts',(0.777275618046955,1.34827508421444,
8.62138181587654));
#266050=CARTESIAN_POINT('Ctrl Pts',(0.604355723756177,1.4408029212872,8.63614013232065));
#266051=CARTESIAN_POINT('Ctrl Pts',(0.465696561192639,1.49140060577076,
8.64776999108561));
#266052=CARTESIAN_POINT('Ctrl Pts',(0.302173282617808,1.5260022509477,8.66041392425533));
#266053=CARTESIAN_POINT('Ctrl Pts',(0.282250441036827,1.52981251854891,
8.66193530806882));
#266054=CARTESIAN_POINT('Ctrl Pts',(0.249089931401012,1.53548458794357,
8.66443020459504));
#266055=CARTESIAN_POINT('Ctrl Pts',(0.235893068706918,1.53756730132498,
8.66541335235504));
#266056=CARTESIAN_POINT('Ctrl Pts',(0.217789249468635,1.54018583851988,
8.66674729738313));
#266057=CARTESIAN_POINT('Ctrl Pts',(0.21290465038176,1.5408686465746,8.667105742651));
#266058=CARTESIAN_POINT('Ctrl Pts',(0.204694528961621,1.54197653622339,
8.66770566979936));
#266059=CARTESIAN_POINT('Ctrl Pts',(0.201370768142125,1.54241411524346,
8.66794784041032));
#266060=CARTESIAN_POINT('Ctrl Pts',(0.195061706470477,1.54322397298209,
8.66840615734571));
#266061=CARTESIAN_POINT('Ctrl Pts',(0.192076708130791,1.54359834112799,
8.66862242287279));
#266062=CARTESIAN_POINT('Ctrl Pts',(0.184251652195814,1.54455668247093,
8.66918788678919));
#266063=CARTESIAN_POINT('Ctrl Pts',(0.179409849818223,1.54512657222969,
8.66953630091653));
#266064=CARTESIAN_POINT('Ctrl Pts',(0.162592392152359,1.54702590296565,
8.67074163023774));
#266065=CARTESIAN_POINT('Ctrl Pts',(0.15060362899934,1.54823899994514,8.67159235524857));
#266066=CARTESIAN_POINT('Ctrl Pts',(0.133465560367894,1.54977217136858,
8.67279788754486));
#266067=CARTESIAN_POINT('Ctrl Pts',(0.12832728995872,1.55020609832039,8.67315796928092));
#266068=CARTESIAN_POINT('Ctrl Pts',(-0.0473456028925387,1.56416223982192,
8.68542544609605));
#266069=CARTESIAN_POINT('Ctrl Pts',(-0.21896689607696,1.54948982019231,
8.69612922595204));
#266070=CARTESIAN_POINT('Ctrl Pts',(-0.412518540428051,1.50007614896009,
8.70966938683897));
#266071=CARTESIAN_POINT('Ctrl Pts',(-0.440057686731791,1.49222956312449,
8.71162862253972));
#266072=CARTESIAN_POINT('Ctrl Pts',(-0.486677539757825,1.47754366397614,
8.71501316555678));
#266073=CARTESIAN_POINT('Ctrl Pts',(-0.505870275489752,1.47108310604703,
8.7164265467917));
#266074=CARTESIAN_POINT('Ctrl Pts',(-0.532709714808772,1.46146122095425,
8.71843401251776));
#266075=CARTESIAN_POINT('Ctrl Pts',(-0.540466264432843,1.45861055559183,
8.71901785001398));
#266076=CARTESIAN_POINT('Ctrl Pts',(-0.553730691119689,1.45361532165968,
8.72002278118651));
#266077=CARTESIAN_POINT('Ctrl Pts',(-0.559249796227693,1.45150089400996,
8.72044286456909));
#266078=CARTESIAN_POINT('Ctrl Pts',(-0.569747765982819,1.44741024827953,
8.72124569819816));
#266079=CARTESIAN_POINT('Ctrl Pts',(-0.57472874595762,1.44543966007406,
8.72162825472493));
#266080=CARTESIAN_POINT('Ctrl Pts',(-0.587568008358263,1.44028330093527,
8.72261864630698));
#266081=CARTESIAN_POINT('Ctrl Pts',(-0.595410506342982,1.43705896714615,
8.72322777187408));
#266082=CARTESIAN_POINT('Ctrl Pts',(-0.621745983254385,1.42597892004827,
8.72528761661021));
#266083=CARTESIAN_POINT('Ctrl Pts',(-0.640112304522696,1.41782936757454,
8.72674821329347));
#266084=CARTESIAN_POINT('Ctrl Pts',(-0.820588347441405,1.33352665846721,
8.74134837108429));
#266085=CARTESIAN_POINT('Ctrl Pts',(-0.96853620943392,1.23026973780936,
8.75554746866012));
#266086=CARTESIAN_POINT('Ctrl Pts',(-1.11963404372768,1.08034496154894,
8.77169781227758));
#266087=CARTESIAN_POINT('Ctrl Pts',(-1.14287605070558,1.05572742568699,
8.77423221042278));
#266088=CARTESIAN_POINT('Ctrl Pts',(-1.16977861139558,1.0253019055079,8.77720822069005));
#266089=CARTESIAN_POINT('Ctrl Pts',(-1.17422589995149,1.02020563490455,
8.77770164613725));
#266090=CARTESIAN_POINT('Ctrl Pts',(-1.18108987088981,1.01223567492973,
8.77846526972874));
#266091=CARTESIAN_POINT('Ctrl Pts',(-1.18352955728001,1.0093820548104,8.77873709998626));
#266092=CARTESIAN_POINT('Ctrl Pts',(-1.18804408426532,1.00406269131246,
8.77924083474713));
#266093=CARTESIAN_POINT('Ctrl Pts',(-1.19012157667092,1.00159935469506,
8.77947292658358));
#266094=CARTESIAN_POINT('Ctrl Pts',(-1.1948411351344,0.995967835180395,
8.78000085310709));
#266095=CARTESIAN_POINT('Ctrl Pts',(-1.19747826187294,0.992795588388715,
8.78029632900425));
#266096=CARTESIAN_POINT('Ctrl Pts',(-1.20432761903731,0.984489377877451,
8.78106515970762));
#266097=CARTESIAN_POINT('Ctrl Pts',(-1.20851970640838,0.979338793532901,
8.78153710941247));
#266098=CARTESIAN_POINT('Ctrl Pts',(-1.23672130387915,0.944232209751514,
8.78472285229903));
#266099=CARTESIAN_POINT('Ctrl Pts',(-1.25965013735718,0.9134200517235,8.78736658101541));
#266100=CARTESIAN_POINT('Ctrl Pts',(-1.36637287071368,0.758330177962056,
8.8001202779947));
#266101=CARTESIAN_POINT('Ctrl Pts',(-1.43304413195573,0.623241797617836,
8.80963197987196));
#266102=CARTESIAN_POINT('Ctrl Pts',(-1.49148170260505,0.44339652385938,
8.82249267980329));
#266103=CARTESIAN_POINT('Ctrl Pts',(-1.50218482803531,0.405658042549305,
8.8251959633974));
#266104=CARTESIAN_POINT('Ctrl Pts',(-1.51393597937493,0.357335664355005,
8.82868325567042));
#266105=CARTESIAN_POINT('Ctrl Pts',(-1.51631805605968,0.34708856200853,
8.82942417908086));
#266106=CARTESIAN_POINT('Ctrl Pts',(-1.51997912360252,0.330582088682228,
8.83062032884774));
#266107=CARTESIAN_POINT('Ctrl Pts',(-1.52132384427807,0.324337497316657,
8.83107344951197));
#266108=CARTESIAN_POINT('Ctrl Pts',(-1.52381076358988,0.312432945245481,
8.83193850072135));
#266109=CARTESIAN_POINT('Ctrl Pts',(-1.52495998770773,0.306774547097003,
8.83235019947034));
#266110=CARTESIAN_POINT('Ctrl Pts',(-1.52751244883558,0.293838229614379,
8.83329270352586));
#266111=CARTESIAN_POINT('Ctrl Pts',(-1.52889521403715,0.28655646477498,
8.83382414977589));
#266112=CARTESIAN_POINT('Ctrl Pts',(-1.53236650727532,0.267535611177085,
8.83521488493412));
#266113=CARTESIAN_POINT('Ctrl Pts',(-1.53437215786387,0.255782099308269,
8.83607677127004));
#266114=CARTESIAN_POINT('Ctrl Pts',(-1.54913520174073,0.162835522053381,
8.84291379045758));
#266115=CARTESIAN_POINT('Ctrl Pts',(-1.55557218656414,0.0807845889713736,
8.84908756436364));
#266116=CARTESIAN_POINT('Ctrl Pts',(-1.5554125167081,-0.0994275799248632,
8.86291519286666));
#266117=CARTESIAN_POINT('Ctrl Pts',(-1.54605549837665,-0.197245125438095,
8.87059845036504));
#266118=CARTESIAN_POINT('Ctrl Pts',(-1.51963977204217,-0.334714930633707,
8.88128956086565));
#266119=CARTESIAN_POINT('Ctrl Pts',(-1.51006240959696,-0.3755681086635,
8.88444990933905));
#266120=CARTESIAN_POINT('Ctrl Pts',(-1.49702438071354,-0.422545335812145,
8.8880285740104));
#266121=CARTESIAN_POINT('Ctrl Pts',(-1.4951614769981,-0.429090572582635,
8.88852590314068));
#266122=CARTESIAN_POINT('Ctrl Pts',(-1.49208659238871,-0.439630840598437,
8.88932449275765));
#266123=CARTESIAN_POINT('Ctrl Pts',(-1.49090140557738,-0.443633491905357,
8.88962721962317));
#266124=CARTESIAN_POINT('Ctrl Pts',(-1.48877148275661,-0.450721793436307,
8.89016230824777));
#266125=CARTESIAN_POINT('Ctrl Pts',(-1.4878332444938,-0.453809321490379,
8.89039503857323));
#266126=CARTESIAN_POINT('Ctrl Pts',(-1.48579246223208,-0.460450707248406,
8.8908948976787));
#266127=CARTESIAN_POINT('Ctrl Pts',(-1.48468677412678,-0.464003532476387,
8.89116184068603));
#266128=CARTESIAN_POINT('Ctrl Pts',(-1.48158149721771,-0.473856739139912,
8.89190098289509));
#266129=CARTESIAN_POINT('Ctrl Pts',(-1.47955444991638,-0.480148493722978,
8.89237161572774));
#266130=CARTESIAN_POINT('Ctrl Pts',(-1.46773046541493,-0.516062982034744,
8.89505140105996));
#266131=CARTESIAN_POINT('Ctrl Pts',(-1.45708328553198,-0.545401107985013,
8.89721447049713));
#266132=CARTESIAN_POINT('Ctrl Pts',(-1.41869925217996,-0.641999750913337,
8.9043122384248));
#266133=CARTESIAN_POINT('Ctrl Pts',(-1.38712772717246,-0.70763677550596,
8.90909774444182));
#266134=CARTESIAN_POINT('Ctrl Pts',(-1.29606025304211,-0.867256095542365,
8.92119401540413));
#266135=CARTESIAN_POINT('Ctrl Pts',(-1.23088839732899,-0.957504446385221,
8.92849406760265));
#266136=CARTESIAN_POINT('Ctrl Pts',(-1.14421176049384,-1.0539008406205,
8.93748288452177));
#266137=CARTESIAN_POINT('Ctrl Pts',(-1.13150404915165,-1.06753270193161,
8.93878462573347));
#266138=CARTESIAN_POINT('Ctrl Pts',(-1.11341233445029,-1.08625410923874,
8.94061782036083));
#266139=CARTESIAN_POINT('Ctrl Pts',(-1.10823187230834,-1.09153888164788,
8.94114051852411));
#266140=CARTESIAN_POINT('Ctrl Pts',(-1.0991918139056,-1.10063026964419,
8.94204894269147));
#266141=CARTESIAN_POINT('Ctrl Pts',(-1.09534962970172,-1.1044540830527,
8.94243390127562));
#266142=CARTESIAN_POINT('Ctrl Pts',(-1.08731545425743,-1.11236668567763,
8.94323656779136));
#266143=CARTESIAN_POINT('Ctrl Pts',(-1.08312021128489,-1.11645203508887,
8.94365441701959));
#266144=CARTESIAN_POINT('Ctrl Pts',(-1.07316743844822,-1.12603520082923,
8.94464278213152));
#266145=CARTESIAN_POINT('Ctrl Pts',(-1.06739062119892,-1.13151265209997,
8.94521416321622));
#266146=CARTESIAN_POINT('Ctrl Pts',(-1.04810047996199,-1.1495239616127,
8.94711482768254));
#266147=CARTESIAN_POINT('Ctrl Pts',(-1.03440691260082,-1.16186154052354,
8.94845234641342));
#266148=CARTESIAN_POINT('Ctrl Pts',(-1.00137744485528,-1.19057352380103,
8.95165254750529));
#266149=CARTESIAN_POINT('Ctrl Pts',(-0.981854856164721,-1.20672408124809,
8.95352379176451));
#266150=CARTESIAN_POINT('Ctrl Pts',(-0.843709525186548,-1.31543617809473,
8.96663084708343));
#266151=CARTESIAN_POINT('Ctrl Pts',(-0.712601543449115,-1.39082797112042,
8.97851098818748));
#266152=CARTESIAN_POINT('Ctrl Pts',(-0.536671406595769,-1.46050356352762,
8.99293089748741));
#266153=CARTESIAN_POINT('Ctrl Pts',(-0.500057279028089,-1.47344161718641,
8.99584960600123));
#266154=CARTESIAN_POINT('Ctrl Pts',(-0.456633636296178,-1.48698028122117,
8.99918727561483));
#266155=CARTESIAN_POINT('Ctrl Pts',(-0.450260599096057,-1.48892243977853,
8.9996740426337));
#266156=CARTESIAN_POINT('Ctrl Pts',(-0.439915312128538,-1.49200262678201,
9.00045900488997));
#266157=CARTESIAN_POINT('Ctrl Pts',(-0.435950750804253,-1.49316585284811,
9.00075858885146));
#266158=CARTESIAN_POINT('Ctrl Pts',(-0.428885350400509,-1.49520834458975,
9.00129024084628));
#266159=CARTESIAN_POINT('Ctrl Pts',(-0.425786374017088,-1.49609378112933,
9.00152265947749));
#266160=CARTESIAN_POINT('Ctrl Pts',(-0.419075911288086,-1.49798854844369,
9.00202425952587));
#266161=CARTESIAN_POINT('Ctrl Pts',(-0.41546352436777,-1.49899445343014,
9.00229324204476));
#266162=CARTESIAN_POINT('Ctrl Pts',(-0.405345345873723,-1.50177257451984,
9.00304383996673));
#266163=CARTESIAN_POINT('Ctrl Pts',(-0.39883151078298,-1.50351559533693,
9.00352380886692));
#266164=CARTESIAN_POINT('Ctrl Pts',(-0.359920645324104,-1.51365698279392,
9.00637275468749));
#266165=CARTESIAN_POINT('Ctrl Pts',(-0.327267814101156,-1.52105112787937,
9.00868856120706));
#266166=CARTESIAN_POINT('Ctrl Pts',(-0.12732290473174,-1.5595898679393,
9.02255901386915));
#266167=CARTESIAN_POINT('Ctrl Pts',(0.0439083767719911,-1.56416577747891,
9.03325970940069));
#266168=CARTESIAN_POINT('Ctrl Pts',(0.215299283205228,-1.54053058283668,
9.04514989790096));
#266169=CARTESIAN_POINT('Ctrl Pts',(0.2181015203611,-1.54013635261787,9.04534458652009));
#266170=CARTESIAN_POINT('Ctrl Pts',(0.245474402131607,-1.53620921956422,
9.04724918874785));
#266171=CARTESIAN_POINT('Ctrl Pts',(0.269956974732322,-1.53209645942151,
9.04897514164185));
#266172=CARTESIAN_POINT('Ctrl Pts',(0.303396730470763,-1.5256526278948,
9.05136842418234));
#266173=CARTESIAN_POINT('Ctrl Pts',(0.312448017306929,-1.52382471005529,
9.05201984930471));
#266174=CARTESIAN_POINT('Ctrl Pts',(0.326860148154003,-1.52078036055114,
9.05306312648649));
#266175=CARTESIAN_POINT('Ctrl Pts',(0.332231852587348,-1.51961589100823,
9.05345331931353));
#266176=CARTESIAN_POINT('Ctrl Pts',(0.343269472975116,-1.51716185160155,
9.05425789634303));
#266177=CARTESIAN_POINT('Ctrl Pts',(0.348934552610121,-1.51586895586077,
9.05467238112592));
#266178=CARTESIAN_POINT('Ctrl Pts',(0.362071532443969,-1.51279326491763,
9.05563718252595));
#266179=CARTESIAN_POINT('Ctrl Pts',(0.369537679069446,-1.51098681556572,
9.05618824926663));
#266180=CARTESIAN_POINT('Ctrl Pts',(0.393345254603278,-1.50503951676996,
9.05795441980577));
#266181=CARTESIAN_POINT('Ctrl Pts',(0.409632369885046,-1.5006884141512,
9.05917623794978));
#266182=CARTESIAN_POINT('Ctrl Pts',(0.492119489609785,-1.47720913826289,
9.06543586224443));
#266183=CARTESIAN_POINT('Ctrl Pts',(0.557057287389644,-1.45396460422588,
9.07060518040054));
#266184=CARTESIAN_POINT('Ctrl Pts',(0.677789300441647,-1.40147099197126,
9.08067182051833));
#266185=CARTESIAN_POINT('Ctrl Pts',(0.733775945339606,-1.37298630199348,
9.08554254086479));
#266186=CARTESIAN_POINT('Ctrl Pts',(0.829035159674219,-1.31702641011422,
9.09410680469196));
#266187=CARTESIAN_POINT('Ctrl Pts',(0.869052328162863,-1.29097109248076,
9.09779766728948));
#266188=CARTESIAN_POINT('Ctrl Pts',(0.938199312171517,-1.24127468990473,
9.10428000736169));
#266189=CARTESIAN_POINT('Ctrl Pts',(0.967793867134395,-1.21834166079712,
9.10709139056436));
#266190=CARTESIAN_POINT('Ctrl Pts',(1.00159821008633,-1.19013644556336,
9.11032143640038));
#266191=CARTESIAN_POINT('Ctrl Pts',(1.00663464826271,-1.18587959866864,
9.11080317628418));
#266192=CARTESIAN_POINT('Ctrl Pts',(1.01476690024465,-1.17891699866809,
9.11158164379128));
#266193=CARTESIAN_POINT('Ctrl Pts',(1.0178792558709,-1.17623083325594,9.1118797238133));
#266194=CARTESIAN_POINT('Ctrl Pts',(1.02341123827559,-1.171417971529,9.11240974545337));
#266195=CARTESIAN_POINT('Ctrl Pts',(1.02583493705782,-1.16929607425101,
9.1126420290517));
#266196=CARTESIAN_POINT('Ctrl Pts',(1.03107663833455,-1.16467823275677,
9.1131445263873));
#266197=CARTESIAN_POINT('Ctrl Pts',(1.03389217465392,-1.16217958680195,
9.11341453469688));
#266198=CARTESIAN_POINT('Ctrl Pts',(1.04177558718018,-1.15513213524064,
9.11417091436946));
#266199=CARTESIAN_POINT('Ctrl Pts',(1.04682278671226,-1.15056015995352,
9.11465559809923));
#266200=CARTESIAN_POINT('Ctrl Pts',(1.07739951787051,-1.12249463870121,
9.11759571596163));
#266201=CARTESIAN_POINT('Ctrl Pts',(1.10216958258371,-1.09818332411337,
9.11999393635995));
#266202=CARTESIAN_POINT('Ctrl Pts',(1.18407214874722,-1.01223192990374,
9.12807091655622));
#266203=CARTESIAN_POINT('Ctrl Pts',(1.23701709666197,-0.946800618795461,
9.13355893523025));
#266204=CARTESIAN_POINT('Ctrl Pts',(1.34346167849062,-0.790978414027506,
9.14598957386394));
#266205=CARTESIAN_POINT('Ctrl Pts',(1.39361947133258,-0.698824797248738,
9.15293884176142));
#266206=CARTESIAN_POINT('Ctrl Pts',(1.43877118918238,-0.591321061156696,
9.16108200174805));
#266207=CARTESIAN_POINT('Ctrl Pts',(1.4432726163604,-0.580247596361419,
9.16192087094849));
#266208=CARTESIAN_POINT('Ctrl Pts',(1.45036101584806,-0.562217256554662,
9.16328745778708));
#266209=CARTESIAN_POINT('Ctrl Pts',(1.45302666345906,-0.555291663628217,
9.16381253902381));
#266210=CARTESIAN_POINT('Ctrl Pts',(1.45767844013214,-0.542943059928113,
9.16474920191221));
#266211=CARTESIAN_POINT('Ctrl Pts',(1.45968413064646,-0.537527523243102,
9.16516012304043));
#266212=CARTESIAN_POINT('Ctrl Pts',(1.46384306085866,-0.526103112962152,
9.16602735304448));
#266213=CARTESIAN_POINT('Ctrl Pts',(1.46598955907289,-0.520091917587838,
9.16648387674281));
#266214=CARTESIAN_POINT('Ctrl Pts',(1.47156856927894,-0.504159117042972,
9.16769456159315));
#266215=CARTESIAN_POINT('Ctrl Pts',(1.47493768409899,-0.494215830760699,
9.16845079614699));
#266216=CARTESIAN_POINT('Ctrl Pts',(1.49033700413312,-0.447207340245067,
9.17202983869718));
#266217=CARTESIAN_POINT('Ctrl Pts',(1.50107123344732,-0.409735820065769,
9.17489442187347));
#266218=CARTESIAN_POINT('Ctrl Pts',(1.54626152262505,-0.226207679508899,
9.18899459191443));
#266219=CARTESIAN_POINT('Ctrl Pts',(1.5608619184384,-0.0760940320435691,
9.2008434729993));
#266220=CARTESIAN_POINT('Ctrl Pts',(1.55192565273712,0.11220605471138,9.21520581950105));
#266221=CARTESIAN_POINT('Ctrl Pts',(1.54867179088438,0.150597893631395,
9.21810113358521));
#266222=CARTESIAN_POINT('Ctrl Pts',(1.54318869143675,0.195430526934642,
9.22141530384782));
#266223=CARTESIAN_POINT('Ctrl Pts',(1.54233950766328,0.20202295796946,9.22190092432289));
#266224=CARTESIAN_POINT('Ctrl Pts',(1.54089460277449,0.212699564731272,
9.22268440580536));
#266225=CARTESIAN_POINT('Ctrl Pts',(1.54032485093962,0.216787076043851,
9.22298364721597));
#266226=CARTESIAN_POINT('Ctrl Pts',(1.53928124184963,0.224062253529249,
9.22351492703107));
#266227=CARTESIAN_POINT('Ctrl Pts',(1.53881374123598,0.227250754586009,
9.22374731407181));
#266228=CARTESIAN_POINT('Ctrl Pts',(1.53778033195706,0.234149494723338,
9.22424911470589));
#266229=CARTESIAN_POINT('Ctrl Pts',(1.5372109044494,0.237859141680731,9.22451832792846));
#266230=CARTESIAN_POINT('Ctrl Pts',(1.53557856595667,0.248242595406701,
9.22527022497462));
#266231=CARTESIAN_POINT('Ctrl Pts',(1.53448556483765,0.254911698724805,
9.22575125309384));
#266232=CARTESIAN_POINT('Ctrl Pts',(1.52767568739513,0.294831317394578,
9.22862032584849));
#266233=CARTESIAN_POINT('Ctrl Pts',(1.52092120064672,0.327898834581176,
9.23095432098361));
#266234=CARTESIAN_POINT('Ctrl Pts',(1.49346582700328,0.443063532072579,
9.23901662325647));
#266235=CARTESIAN_POINT('Ctrl Pts',(1.46718301667972,0.523515915387443,
9.24453541249253));
#266236=CARTESIAN_POINT('Ctrl Pts',(1.43457655129078,0.601307216393289,
9.25009119722734));
#266237=CARTESIAN_POINT('Origin',(0.,0.,-1.29405622560371));
#266238=CARTESIAN_POINT('',(1.43457678342463,0.601306662576624,10.0876445460468));
#266239=CARTESIAN_POINT('',(1.4345766815454,0.601306905636538,9.94872080685755));
#266240=CARTESIAN_POINT('',(1.43457668357355,0.601306900797845,-1.29405622560371));
#266241=CARTESIAN_POINT('Ctrl Pts',(1.43457678342482,0.601306662576175,
10.0876445460468));
#266242=CARTESIAN_POINT('Ctrl Pts',(1.47844253086014,0.496653268933943,
10.0801366808513));
#266243=CARTESIAN_POINT('Ctrl Pts',(1.51076896683316,0.387410400172105,
10.0727718155593));
#266244=CARTESIAN_POINT('Ctrl Pts',(1.53762167463432,0.238194528969206,
10.0624490528545));
#266245=CARTESIAN_POINT('Ctrl Pts',(1.54296881157422,0.200658646562479,
10.0598339115176));
#266246=CARTESIAN_POINT('Ctrl Pts',(1.54802077539321,0.152703766849103,
10.0564515996699));
#266247=CARTESIAN_POINT('Ctrl Pts',(1.54899983593301,0.142429844505044,
10.0557246046814));
#266248=CARTESIAN_POINT('Ctrl Pts',(1.55041114718988,0.125877401753474,
10.0545491900554));
#266249=CARTESIAN_POINT('Ctrl Pts',(1.55090766847366,0.11960454572007,10.0541027891499));
#266250=CARTESIAN_POINT('Ctrl Pts',(1.5517816891392,0.107640027855507,10.0532494452295));
#266251=CARTESIAN_POINT('Ctrl Pts',(1.55216596926851,0.101948950930017,
10.0528427217393));
#266252=CARTESIAN_POINT('Ctrl Pts',(1.55297339534685,0.0889259204743075,
10.0519100672809));
#266253=CARTESIAN_POINT('Ctrl Pts',(1.55337593174265,0.0815928749452438,
10.0513835004106));
#266254=CARTESIAN_POINT('Ctrl Pts',(1.55429255227922,0.0624139347931474,
10.050002498383));
#266255=CARTESIAN_POINT('Ctrl Pts',(1.55472313640854,0.0505647303947134,
10.0491454799586));
#266256=CARTESIAN_POINT('Ctrl Pts',(1.55762805556826,-0.0661224749199538,
10.040666643287));
#266257=CARTESIAN_POINT('Ctrl Pts',(1.54962956088441,-0.170929903483639,
10.0327114813115));
#266258=CARTESIAN_POINT('Ctrl Pts',(1.51630818856622,-0.35705656482159,
10.0180914144968));
#266259=CARTESIAN_POINT('Ctrl Pts',(1.49474476658779,-0.438655801965744,
10.0115109153316));
#266260=CARTESIAN_POINT('Ctrl Pts',(1.45512961956112,-0.550799475247924,
10.0024806842266));
#266261=CARTESIAN_POINT('Ctrl Pts',(1.44249072004974,-0.583097986228494,
9.99988295825648));
#266262=CARTESIAN_POINT('Ctrl Pts',(1.42611305243361,-0.62115004119941,
9.99684734036577));
#266263=CARTESIAN_POINT('Ctrl Pts',(1.42340413339682,-0.627332837894983,
9.99635491101084));
#266264=CARTESIAN_POINT('Ctrl Pts',(1.41913885838132,-0.636897958311962,
9.99559456524021));
#266265=CARTESIAN_POINT('Ctrl Pts',(1.41761050755092,-0.640292556837241,
9.99532501235459));
#266266=CARTESIAN_POINT('Ctrl Pts',(1.41475421204201,-0.646576274980252,
9.99482662492826));
#266267=CARTESIAN_POINT('Ctrl Pts',(1.41342960668861,-0.649466786786311,
9.9945976002582));
#266268=CARTESIAN_POINT('Ctrl Pts',(1.41039888165141,-0.656027150627278,
9.99407831408346));
#266269=CARTESIAN_POINT('Ctrl Pts',(1.40868729902373,-0.65969441584352,
9.99378839214965));
#266270=CARTESIAN_POINT('Ctrl Pts',(1.40420270791728,-0.669206134942573,
9.99303725764256));
#266271=CARTESIAN_POINT('Ctrl Pts',(1.40140748219221,-0.675040123760145,
9.99257736950926));
#266272=CARTESIAN_POINT('Ctrl Pts',(1.38283468593363,-0.71319127534365,
9.98957421366076));
#266273=CARTESIAN_POINT('Ctrl Pts',(1.36597528757749,-0.744973549731163,
9.98709249666989));
#266274=CARTESIAN_POINT('Ctrl Pts',(1.34313440185583,-0.78464411938279,
9.98398395977101));
#266275=CARTESIAN_POINT('Ctrl Pts',(1.33816096509159,-0.793096245307337,
9.98332101981667));
#266276=CARTESIAN_POINT('Ctrl Pts',(1.28624675827276,-0.879443289256175,
9.97653590590134));
#266277=CARTESIAN_POINT('Ctrl Pts',(1.23263816642673,-0.953129719043354,
9.97063088270741));
#266278=CARTESIAN_POINT('Ctrl Pts',(1.11574952135114,-1.08731432660721,
9.95885933593548));
#266279=CARTESIAN_POINT('Ctrl Pts',(1.05320970919655,-1.14799621593321,
9.95302188042457));
#266280=CARTESIAN_POINT('Ctrl Pts',(0.976065209279602,-1.2112141445352,
9.94605144783859));
#266281=CARTESIAN_POINT('Ctrl Pts',(0.966099084841004,-1.21917822236438,
9.94515522833313));
#266282=CARTESIAN_POINT('Ctrl Pts',(0.950656027440404,-1.23121074138343,
9.94377233504581));
#266283=CARTESIAN_POINT('Ctrl Pts',(0.94524823212154,-1.23536737418218,
9.94328915855291));
#266284=CARTESIAN_POINT('Ctrl Pts',(0.935344942960903,-1.24287631458332,
9.94240617457333));
#266285=CARTESIAN_POINT('Ctrl Pts',(0.930858300528754,-1.24624015282011,
9.94200682789183));
#266286=CARTESIAN_POINT('Ctrl Pts',(0.921026522439148,-1.25352876660994,
9.94113315067698));
#266287=CARTESIAN_POINT('Ctrl Pts',(0.915674302963068,-1.25744375306774,
9.94065845034418));
#266288=CARTESIAN_POINT('Ctrl Pts',(0.900931545649483,-1.26808359532461,
9.93935325727198));
#266289=CARTESIAN_POINT('Ctrl Pts',(0.891491049673795,-1.27473814944232,
9.93852009259508));
#266290=CARTESIAN_POINT('Ctrl Pts',(0.841448092651728,-1.30918536701686,
9.9341162857535));
#266291=CARTESIAN_POINT('Ctrl Pts',(0.799622372412186,-1.33514204815298,
9.93047776386972));
#266292=CARTESIAN_POINT('Ctrl Pts',(0.629242157930082,-1.42999852539775,
9.91580440818312));
#266293=CARTESIAN_POINT('Ctrl Pts',(0.492527918992509,-1.48264895356484,
9.90426496893743));
#266294=CARTESIAN_POINT('Ctrl Pts',(0.319577904150437,-1.52264816033673,
9.89082068520897));
#266295=CARTESIAN_POINT('Ctrl Pts',(0.288443018036543,-1.52885200404884,
9.88844783324883));
#266296=CARTESIAN_POINT('Ctrl Pts',(0.250641988381717,-1.53518800786845,
9.88564033074139));
#266297=CARTESIAN_POINT('Ctrl Pts',(0.244139559977051,-1.53623549798116,
9.8851599990577));
#266298=CARTESIAN_POINT('Ctrl Pts',(0.233986672846962,-1.53780495571834,
9.88441427347687));
#266299=CARTESIAN_POINT('Ctrl Pts',(0.230340782598476,-1.53835528066253,
9.88414734013157));
#266300=CARTESIAN_POINT('Ctrl Pts',(0.223543067305137,-1.53935664610953,
9.88365128310761));
#266301=CARTESIAN_POINT('Ctrl Pts',(0.220391844459914,-1.53981096958914,
9.88342198520346));
#266302=CARTESIAN_POINT('Ctrl Pts',(0.213181922643759,-1.54082786398965,
9.88289884277056));
#266303=CARTESIAN_POINT('Ctrl Pts',(0.209122382309097,-1.54138407570767,
9.88260535840243));
#266304=CARTESIAN_POINT('Ctrl Pts',(0.198482043803342,-1.54279913517462,
9.8818388049991));
#266305=CARTESIAN_POINT('Ctrl Pts',(0.191897771730655,-1.54363193235054,
9.88136715137549));
#266306=CARTESIAN_POINT('Ctrl Pts',(0.146307234202684,-1.54910213285693,
9.87811868363861));
#266307=CARTESIAN_POINT('Ctrl Pts',(0.10713878918169,-1.5523031775849,9.87541542431602));
#266308=CARTESIAN_POINT('Ctrl Pts',(-0.0818442132904599,-1.56055889476217,
9.86261126892046));
#266309=CARTESIAN_POINT('Ctrl Pts',(-0.231737247206432,-1.54542760266506,
9.85309825107761));
#266310=CARTESIAN_POINT('Ctrl Pts',(-0.414665255115307,-1.49970916326379,
9.84026833650741));
#266311=CARTESIAN_POINT('Ctrl Pts',(-0.451806187156601,-1.48894109772049,
9.83760231444335));
#266312=CARTESIAN_POINT('Ctrl Pts',(-0.498367017896825,-1.47353943476071,
9.83416273279154));
#266313=CARTESIAN_POINT('Ctrl Pts',(-0.508195841200293,-1.4701786041158,
9.8334310733035));
#266314=CARTESIAN_POINT('Ctrl Pts',(-0.523937362672284,-1.46461929249572,
9.83224992994934));
#266315=CARTESIAN_POINT('Ctrl Pts',(-0.529871756009032,-1.4624828040043,
9.83180250089712));
#266316=CARTESIAN_POINT('Ctrl Pts',(-0.541144691661499,-1.45834672485435,
9.83094838389672));
#266317=CARTESIAN_POINT('Ctrl Pts',(-0.546485569241593,-1.45635375792664,
9.83054192226394));
#266318=CARTESIAN_POINT('Ctrl Pts',(-0.558655647288737,-1.4517360794013,
9.82961155029829));
#266319=CARTESIAN_POINT('Ctrl Pts',(-0.565477481690202,-1.4490924714439,
9.82908701517361));
#266320=CARTESIAN_POINT('Ctrl Pts',(-0.583218917641197,-1.44207292758878,
9.82771482185608));
#266321=CARTESIAN_POINT('Ctrl Pts',(-0.594107792879591,-1.43762114295616,
9.82686463384183));
#266322=CARTESIAN_POINT('Ctrl Pts',(-0.678079545492833,-1.40217338642281,
9.82024461101965));
#266323=CARTESIAN_POINT('Ctrl Pts',(-0.748730734262422,-1.36575270583019,
9.81428974285974));
#266324=CARTESIAN_POINT('Ctrl Pts',(-0.90718489793107,-1.26806896540939,
9.80002539570256));
#266325=CARTESIAN_POINT('Ctrl Pts',(-0.992068713572339,-1.20282254056915,
9.79163998644903));
#266326=CARTESIAN_POINT('Ctrl Pts',(-1.09685968115574,-1.10357998845685,
9.7806568559953));
#266327=CARTESIAN_POINT('Ctrl Pts',(-1.12317979586336,-1.07678116415248,
9.77783793554676));
#266328=CARTESIAN_POINT('Ctrl Pts',(-1.15315574278301,-1.0439634116067,
9.77457992730635));
#266329=CARTESIAN_POINT('Ctrl Pts',(-1.15777113129653,-1.03884252135484,
9.77407689384493));
#266330=CARTESIAN_POINT('Ctrl Pts',(-1.16484691146803,-1.03088603299751,
9.77330375271329));
#266331=CARTESIAN_POINT('Ctrl Pts',(-1.16733126051641,-1.02807201557891,
9.77303192146778));
#266332=CARTESIAN_POINT('Ctrl Pts',(-1.17189930655405,-1.02285989138455,
9.77253144340425));
#266333=CARTESIAN_POINT('Ctrl Pts',(-1.17398583034206,-1.02046441027476,
9.77230259277415));
#266334=CARTESIAN_POINT('Ctrl Pts',(-1.17868709994172,-1.01503350692562,
9.77178637310993));
#266335=CARTESIAN_POINT('Ctrl Pts',(-1.18129746361163,-1.01199436914875,
9.77149932696935));
#266336=CARTESIAN_POINT('Ctrl Pts',(-1.18898785429494,-1.00297046566973,
9.77065230112957));
#266337=CARTESIAN_POINT('Ctrl Pts',(-1.19403445353265,-0.996957172249979,
9.7700946930963));
#266338=CARTESIAN_POINT('Ctrl Pts',(-1.23450839700174,-0.94798208819109,
9.7656057184469));
#266339=CARTESIAN_POINT('Ctrl Pts',(-1.26765569712896,-0.903178661932668,
9.76182260192153));
#266340=CARTESIAN_POINT('Ctrl Pts',(-1.37277829468245,-0.743862757981147,
9.74906930194352));
#266341=CARTESIAN_POINT('Ctrl Pts',(-1.43219874660425,-0.621819782193494,
9.74040512651302));
#266342=CARTESIAN_POINT('Ctrl Pts',(-1.48663399272524,-0.4591529194858,
9.72871071651736));
#266343=CARTESIAN_POINT('Ctrl Pts',(-1.49695835129795,-0.424284537689517,
9.72620009026614));
#266344=CARTESIAN_POINT('Ctrl Pts',(-1.50859712903308,-0.379234158149677,
9.72293561295762));
#266345=CARTESIAN_POINT('Ctrl Pts',(-1.51104622228774,-0.369355045692685,
9.72221851612086));
#266346=CARTESIAN_POINT('Ctrl Pts',(-1.51484499153238,-0.353361151494857,
9.72105525580279));
#266347=CARTESIAN_POINT('Ctrl Pts',(-1.51625503271118,-0.347260889605912,
9.72061103533954));
#266348=CARTESIAN_POINT('Ctrl Pts',(-1.51888094265229,-0.335579437573681,
9.71975928366385));
#266349=CARTESIAN_POINT('Ctrl Pts',(-1.52010297571201,-0.329999725008494,
9.7193519573891));
#266350=CARTESIAN_POINT('Ctrl Pts',(-1.52281322792954,-0.317290354479505,
9.71842299595069));
#266351=CARTESIAN_POINT('Ctrl Pts',(-1.5242821500401,-0.310156766697294,
9.71790075429078));
#266352=CARTESIAN_POINT('Ctrl Pts',(-1.52802243903776,-0.291324050560442,
9.71651971325704));
#266353=CARTESIAN_POINT('Ctrl Pts',(-1.53020950684352,-0.279608882365264,
9.71565826053547));
#266354=CARTESIAN_POINT('Ctrl Pts',(-1.54780879990943,-0.17893796457108,
9.70823388929048));
#266355=CARTESIAN_POINT('Ctrl Pts',(-1.555581235732,-0.0888385080196809,
9.70142856197073));
#266356=CARTESIAN_POINT('Ctrl Pts',(-1.55541935066541,0.0896033524905979,
9.68769192438867));
#266357=CARTESIAN_POINT('Ctrl Pts',(-1.54783931923097,0.177627251609025,
9.68079338785291));
#266358=CARTESIAN_POINT('Ctrl Pts',(-1.52999796541242,0.281008854757881,
9.67277117261743));
#266359=CARTESIAN_POINT('Ctrl Pts',(-1.52688927605936,0.297437267115137,
9.67149922133837));
#266360=CARTESIAN_POINT('Ctrl Pts',(-1.51775431724925,0.341786168768107,
9.66807830749043));
#266361=CARTESIAN_POINT('Ctrl Pts',(-1.51122257092077,0.369597845716856,
9.66594675006831));
#266362=CARTESIAN_POINT('Ctrl Pts',(-1.50223829838421,0.403613839664403,
9.66336902220448));
#266363=CARTESIAN_POINT('Ctrl Pts',(-1.50050767899166,0.410000909998151,
9.66288630213274));
#266364=CARTESIAN_POINT('Ctrl Pts',(-1.49773682393734,0.419974520795588,
9.66213474774306));
#266365=CARTESIAN_POINT('Ctrl Pts',(-1.49672437117302,0.423568588813101,
9.66186437361502));
#266366=CARTESIAN_POINT('Ctrl Pts',(-1.49482611716555,0.430215332498108,
9.66136523909301));
#266367=CARTESIAN_POINT('Ctrl Pts',(-1.49394390779455,0.433268916027962,
9.66113628362256));
#266368=CARTESIAN_POINT('Ctrl Pts',(-1.49192135315733,0.440189939157331,
9.66061813197997));
#266369=CARTESIAN_POINT('Ctrl Pts',(-1.49077532831515,0.444055658696583,
9.66032926924321));
#266370=CARTESIAN_POINT('Ctrl Pts',(-1.48724160960258,0.455807564853408,
9.65945266655478));
#266371=CARTESIAN_POINT('Ctrl Pts',(-1.48480622351122,0.463679445348387,
9.65886761190597));
#266372=CARTESIAN_POINT('Ctrl Pts',(-1.47902163853053,0.481863877358021,
9.65752023059936));
#266373=CARTESIAN_POINT('Ctrl Pts',(-1.47562689931451,0.492161633671748,
9.65676030541721));
#266374=CARTESIAN_POINT('Ctrl Pts',(-1.46362596516928,0.527324945947235,
9.65417330326446));
#266375=CARTESIAN_POINT('Ctrl Pts',(-1.45449626084364,0.55200848865195,
9.6523708787466));
#266376=CARTESIAN_POINT('Ctrl Pts',(-1.40057364947584,0.687153546254603,
9.64251576904411));
#266377=CARTESIAN_POINT('Ctrl Pts',(-1.34382377608123,0.792419283826056,
9.63486114319564));
#266378=CARTESIAN_POINT('Ctrl Pts',(-1.23788923570902,0.944221226886848,
9.62250620004183));
#266379=CARTESIAN_POINT('Ctrl Pts',(-1.19678263446667,0.995807730607634,
9.61803459043951));
#266380=CARTESIAN_POINT('Ctrl Pts',(-1.14489923276042,1.05305042924463,
9.6126343443291));
#266381=CARTESIAN_POINT('Ctrl Pts',(-1.1371735514339,1.06138860063923,9.61183608812386));
#266382=CARTESIAN_POINT('Ctrl Pts',(-1.12440860889715,1.07486618760146,
9.6105261244484));
#266383=CARTESIAN_POINT('Ctrl Pts',(-1.11942373693226,1.08005672770383,
9.61001674524638));
#266384=CARTESIAN_POINT('Ctrl Pts',(-1.11043540563666,1.0892868324814,9.60910202445981));
#266385=CARTESIAN_POINT('Ctrl Pts',(-1.10644544424069,1.0933394124673,9.60869727540878));
#266386=CARTESIAN_POINT('Ctrl Pts',(-1.09793578888721,1.10188833260888,
9.60783671878387));
#266387=CARTESIAN_POINT('Ctrl Pts',(-1.09341050841158,1.10637893685565,
9.60738066856671));
#266388=CARTESIAN_POINT('Ctrl Pts',(-1.08121946132528,1.11832872127012,
9.60615617554746));
#266389=CARTESIAN_POINT('Ctrl Pts',(-1.07350427129386,1.125736745982,9.60538552890128));
#266390=CARTESIAN_POINT('Ctrl Pts',(-1.03485889349432,1.16208498716031,
9.60154566508982));
#266391=CARTESIAN_POINT('Ctrl Pts',(-1.00283485146302,1.18983026800243,
9.59842656632351));
#266392=CARTESIAN_POINT('Ctrl Pts',(-0.846779639675462,1.3142555991856,
9.58349671095936));
#266393=CARTESIAN_POINT('Ctrl Pts',(-0.709716708672483,1.39305102056663,
9.57102424986713));
#266394=CARTESIAN_POINT('Ctrl Pts',(-0.536331559427122,1.46039686847863,
9.55696809261493));
#266395=CARTESIAN_POINT('Ctrl Pts',(-0.509184505099739,1.47008230223421,
9.55481711825901));
#266396=CARTESIAN_POINT('Ctrl Pts',(-0.475472072141567,1.48106400817749,
9.55221923524248));
#266397=CARTESIAN_POINT('Ctrl Pts',(-0.469149067865993,1.48307904174806,
9.55173511721245));
#266398=CARTESIAN_POINT('Ctrl Pts',(-0.459244309671248,1.48616583467769,
9.55098185849182));
#266399=CARTESIAN_POINT('Ctrl Pts',(-0.45567135978787,1.48726522073147,
9.55071116696772));
#266400=CARTESIAN_POINT('Ctrl Pts',(-0.449053517919327,1.4892754239568,
9.55021174171513));
#266401=CARTESIAN_POINT('Ctrl Pts',(-0.446009820069313,1.49018978359114,
9.54998281100287));
#266402=CARTESIAN_POINT('Ctrl Pts',(-0.439103712939263,1.49224139799925,
9.54946508886609));
#266403=CARTESIAN_POINT('Ctrl Pts',(-0.435239681428837,1.49337298800968,
9.5491766285439));
#266404=CARTESIAN_POINT('Ctrl Pts',(-0.423482380285726,1.49676662932743,
9.54830246331214));
#266405=CARTESIAN_POINT('Ctrl Pts',(-0.415575384644471,1.49898124624159,
9.54771942192633));
#266406=CARTESIAN_POINT('Ctrl Pts',(-0.319936120803106,1.52495325243211,
9.54072143669122));
#266407=CARTESIAN_POINT('Ctrl Pts',(-0.230286500239397,1.5410435690689,
9.53470551968568));
#266408=CARTESIAN_POINT('Ctrl Pts',(-0.0177832922187705,1.56021036104209,
9.52064810628876));
#266409=CARTESIAN_POINT('Ctrl Pts',(0.105020370939977,1.55677191647627,
9.51264851258683));
#266410=CARTESIAN_POINT('Ctrl Pts',(0.244019536252181,1.536346684342,9.50290022371281));
#266411=CARTESIAN_POINT('Ctrl Pts',(0.261846837541059,1.53340890009237,
9.50163758066318));
#266412=CARTESIAN_POINT('Ctrl Pts',(0.286751970780154,1.52885779125364,
9.49985443320377));
#266413=CARTESIAN_POINT('Ctrl Pts',(0.293876328611617,1.52750434988096,
9.49934213432499));
#266414=CARTESIAN_POINT('Ctrl Pts',(0.306228277737918,1.52506819176618,
9.49844996192172));
#266415=CARTESIAN_POINT('Ctrl Pts',(0.311460287824334,1.52400827932011,
9.49807081762084));
#266416=CARTESIAN_POINT('Ctrl Pts',(0.322357059308416,1.52174233032004,
9.49727852833045));
#266417=CARTESIAN_POINT('Ctrl Pts',(0.328020737820953,1.52053154767105,
9.49686523745411));
#266418=CARTESIAN_POINT('Ctrl Pts',(0.341410582989951,1.51759077149081,
9.49588454481544));
#266419=CARTESIAN_POINT('Ctrl Pts',(0.34913049802757,1.51583337703686,9.4953162749674));
#266420=CARTESIAN_POINT('Ctrl Pts',(0.374867717183696,1.5097674087971,9.49341197712675));
#266421=CARTESIAN_POINT('Ctrl Pts',(0.392820788270152,1.50519606936468,
9.49206758059581));
#266422=CARTESIAN_POINT('Ctrl Pts',(0.435360243601908,1.49355149905255,
9.48884226064361));
#266423=CARTESIAN_POINT('Ctrl Pts',(0.459861486105481,1.48619039687422,
9.48695250844848));
#266424=CARTESIAN_POINT('Ctrl Pts',(0.626579731903588,1.43158466077983,
9.47386860437107));
#266425=CARTESIAN_POINT('Ctrl Pts',(0.761494314389863,1.3646056987717,9.46203677239422));
#266426=CARTESIAN_POINT('Ctrl Pts',(0.916990895997634,1.25707924778209,
9.44762524639557));
#266427=CARTESIAN_POINT('Ctrl Pts',(0.948418356069569,1.23354116440051,
9.44467330728708));
#266428=CARTESIAN_POINT('Ctrl Pts',(0.984081462484981,1.20466093030836,
9.44130603679204));
#266429=CARTESIAN_POINT('Ctrl Pts',(0.989211620154896,1.20045185516356,
9.44082122096884));
#266430=CARTESIAN_POINT('Ctrl Pts',(0.997465580391936,1.19359099042189,
9.44004070619022));
#266431=CARTESIAN_POINT('Ctrl Pts',(1.00060604381264,1.19095952181927,9.43974362021254));
#266432=CARTESIAN_POINT('Ctrl Pts',(1.00616835225893,1.18626119946765,9.43921727788989));
#266433=CARTESIAN_POINT('Ctrl Pts',(1.00859428143507,1.18419929176145,9.4389876718591));
#266434=CARTESIAN_POINT('Ctrl Pts',(1.01381616451833,1.17973328797119,9.43849334226401));
#266435=CARTESIAN_POINT('Ctrl Pts',(1.01660990311454,1.17732669715817,9.43822880627326));
#266436=CARTESIAN_POINT('Ctrl Pts',(1.02437030589653,1.17059348741227,9.43749370800106));
#266437=CARTESIAN_POINT('Ctrl Pts',(1.02931816425105,1.16624515314938,9.4370247106712));
#266438=CARTESIAN_POINT('Ctrl Pts',(1.05795374878651,1.14075509224693,9.43430750979954));
#266439=CARTESIAN_POINT('Ctrl Pts',(1.0810194200989,1.11892166638026,9.43210718981094));
#266440=CARTESIAN_POINT('Ctrl Pts',(1.20615091865032,0.992990455380167,
9.41999162257703));
#266441=CARTESIAN_POINT('Ctrl Pts',(1.29386065716655,0.875650069229085,
9.41073992067343));
#266442=CARTESIAN_POINT('Ctrl Pts',(1.38760487917842,0.704665237915422,
9.39758699089129));
#266443=CARTESIAN_POINT('Ctrl Pts',(1.40919323568639,0.660434704966541,
9.39421755039785));
#266444=CARTESIAN_POINT('Ctrl Pts',(1.43064719267416,0.610618044335124,
9.39042104283477));
#266445=CARTESIAN_POINT('Ctrl Pts',(1.43262330446223,0.605967203421737,
9.39006660355166));
#266446=CARTESIAN_POINT('Ctrl Pts',(1.43457668359376,0.601306900749626,
9.38971141570882));
#266447=CARTESIAN_POINT('',(-1.55550041510621,0.000136228757878965,9.55740355867135));
#266448=CARTESIAN_POINT('Ctrl Pts',(1.43457655129078,0.601307216393289,
9.25009119722734));
#266449=CARTESIAN_POINT('Ctrl Pts',(1.39925071630394,0.685586288962663,
9.25611033277065));
#266450=CARTESIAN_POINT('Ctrl Pts',(1.35650306920638,0.766741828868003,
9.2621775061668));
#266451=CARTESIAN_POINT('Ctrl Pts',(1.29474908886411,0.862377045314231,
9.27004055526603));
#266452=CARTESIAN_POINT('Ctrl Pts',(1.28235765822098,0.880697520446168,
9.27158128126093));
#266453=CARTESIAN_POINT('Ctrl Pts',(1.26448653094339,0.905942486002453,
9.27375665296959));
#266454=CARTESIAN_POINT('Ctrl Pts',(1.25933167991373,0.91309456745673,9.27437897720188));
#266455=CARTESIAN_POINT('Ctrl Pts',(1.2509114597129,0.924570235499429,9.27538750389055));
#266456=CARTESIAN_POINT('Ctrl Pts',(1.24768375595191,0.928921333695101,
9.27577224738425));
#266457=CARTESIAN_POINT('Ctrl Pts',(1.24091876103452,0.937941999962577,
9.27657486403914));
#266458=CARTESIAN_POINT('Ctrl Pts',(1.23737769561372,0.94260861626253,9.27699288030599));
#266459=CARTESIAN_POINT('Ctrl Pts',(1.22895452807975,0.953579886961219,
9.27798235884503));
#266460=CARTESIAN_POINT('Ctrl Pts',(1.22405018088686,0.959867169553989,
9.27855469177296));
#266461=CARTESIAN_POINT('Ctrl Pts',(1.20760308448201,0.980621003952878,
9.28046182767233));
#266462=CARTESIAN_POINT('Ctrl Pts',(1.19585091354144,0.994918740762502,
9.28180494327615));
#266463=CARTESIAN_POINT('Ctrl Pts',(1.16732537036019,1.02838730456784,9.28502086956314));
#266464=CARTESIAN_POINT('Ctrl Pts',(1.15033115388183,1.04736195604734,9.28690235491231));
#266465=CARTESIAN_POINT('Ctrl Pts',(1.02987131190614,1.17539013727228,9.30001157764069));
#266466=CARTESIAN_POINT('Ctrl Pts',(0.911540348493249,1.26935278601737,
9.31188129206641));
#266467=CARTESIAN_POINT('Ctrl Pts',(0.74814260735315,1.36431735631842,9.32628221208198));
#266468=CARTESIAN_POINT('Ctrl Pts',(0.71395069661022,1.38251735329988,9.32919330152686));
#266469=CARTESIAN_POINT('Ctrl Pts',(0.673122833155897,1.40233028077393,
9.33252330485184));
#266470=CARTESIAN_POINT('Ctrl Pts',(0.667115096777648,1.40519821262707,
9.33300968509803));
#266471=CARTESIAN_POINT('Ctrl Pts',(0.657350513322305,1.40978282363793,
9.33379414786567));
#266472=CARTESIAN_POINT('Ctrl Pts',(0.653605000356183,1.41152322395584,
9.33409361630183));
#266473=CARTESIAN_POINT('Ctrl Pts',(0.646924438379127,1.41459513914092,
9.33462514272473));
#266474=CARTESIAN_POINT('Ctrl Pts',(0.643992146163158,1.41593246768541,
9.3348575506479));
#266475=CARTESIAN_POINT('Ctrl Pts',(0.637638114176911,1.41880652461627,
9.3353592180977));
#266476=CARTESIAN_POINT('Ctrl Pts',(0.634214969746228,1.42033999165668,
9.3356282782304));
#266477=CARTESIAN_POINT('Ctrl Pts',(0.624618154356527,1.42459746757173,
9.3363793131292));
#266478=CARTESIAN_POINT('Ctrl Pts',(0.618432155295258,1.42729375290562,
9.33685963829998));
#266479=CARTESIAN_POINT('Ctrl Pts',(0.581378974405374,1.44315795998708,
9.33971533143563));
#266480=CARTESIAN_POINT('Ctrl Pts',(0.550106972934137,1.45536564275558,
9.34203723514331));
#266481=CARTESIAN_POINT('Ctrl Pts',(0.356175812631202,1.52392495300936,
9.35604722185994));
#266482=CARTESIAN_POINT('Ctrl Pts',(0.185490220824298,1.55396684056293,
9.36686501370038));
#266483=CARTESIAN_POINT('Ctrl Pts',(-0.0120678110005505,1.55566063466285,
9.38046416801924));
#266484=CARTESIAN_POINT('Ctrl Pts',(-0.0374716295706017,1.55525605346374,
9.38222981017678));
#266485=CARTESIAN_POINT('Ctrl Pts',(-0.0721656983561482,1.55385302752024,
9.3846696218158));
#266486=CARTESIAN_POINT('Ctrl Pts',(-0.0814746903087904,1.55339273438509,
9.38532705890838));
#266487=CARTESIAN_POINT('Ctrl Pts',(-0.0962825259984223,1.55252707533458,
9.38637754027212));
#266488=CARTESIAN_POINT('Ctrl Pts',(-0.101784431729667,1.55217607651114,
9.38676888278129));
#266489=CARTESIAN_POINT('Ctrl Pts',(-0.113073418369649,1.55139560597441,
9.38757402947499));
#266490=CARTESIAN_POINT('Ctrl Pts',(-0.118860187128812,1.55096298421891,
9.38798792599675));
#266491=CARTESIAN_POINT('Ctrl Pts',(-0.132248435259629,1.54988670472818,
9.38894830748156));
#266492=CARTESIAN_POINT('Ctrl Pts',(-0.139847814388744,1.54921949093484,
9.38949552099795));
#266493=CARTESIAN_POINT('Ctrl Pts',(-0.163936856610407,1.54692582527297,
9.39123692584105));
#266494=CARTESIAN_POINT('Ctrl Pts',(-0.180405092044375,1.54509183066003,
9.39243756899137));
#266495=CARTESIAN_POINT('Ctrl Pts',(-0.262947097655967,1.5345619246884,
9.39850874866032));
#266496=CARTESIAN_POINT('Ctrl Pts',(-0.328433903797956,1.52189038212225,
9.4035019907975));
#266497=CARTESIAN_POINT('Ctrl Pts',(-0.476647727485408,1.48319893279626,
9.41519942571041));
#266498=CARTESIAN_POINT('Ctrl Pts',(-0.558422937732378,1.45438454627873,
9.42195336348554));
#266499=CARTESIAN_POINT('Ctrl Pts',(-0.694598924932757,1.39321516591301,
9.43347428204779));
#266500=CARTESIAN_POINT('Ctrl Pts',(-0.750227506234502,1.3640663126175,
9.43826323764434));
#266501=CARTESIAN_POINT('Ctrl Pts',(-0.810773125802581,1.32751298511043,
9.44346104725598));
#266502=CARTESIAN_POINT('Ctrl Pts',(-0.817565385733237,1.32334070988243,
9.44404391076425));
#266503=CARTESIAN_POINT('Ctrl Pts',(-0.8277340879076,1.31698621316253,9.44491579890265));
#266504=CARTESIAN_POINT('Ctrl Pts',(-0.831134496108052,1.31484290175978,
9.44520723584989));
#266505=CARTESIAN_POINT('Ctrl Pts',(-0.837195233256664,1.31098985169396,
9.44572640893649));
#266506=CARTESIAN_POINT('Ctrl Pts',(-0.839858691861754,1.30928515925039,
9.4459544683676));
#266507=CARTESIAN_POINT('Ctrl Pts',(-0.845068258151721,1.30592844375465,
9.44640033957755));
#266508=CARTESIAN_POINT('Ctrl Pts',(-0.847614717978009,1.30427709917736,
9.44661819421686));
#266509=CARTESIAN_POINT('Ctrl Pts',(-0.855013277450244,1.29944841497385,
9.44725094642093));
#266510=CARTESIAN_POINT('Ctrl Pts',(-0.859852533126146,1.29625133053721,
9.44766455468977));
#266511=CARTESIAN_POINT('Ctrl Pts',(-0.88188397542213,1.28151845156964,
9.44954692479818));
#266512=CARTESIAN_POINT('Ctrl Pts',(-0.89886369078421,1.26966651692676,
9.45099587553947));
#266513=CARTESIAN_POINT('Ctrl Pts',(-0.945886659920381,1.23542786647326,
9.45501907256936));
#266514=CARTESIAN_POINT('Ctrl Pts',(-0.975366516869028,1.21228881970871,
9.45755387958667));
#266515=CARTESIAN_POINT('Ctrl Pts',(-1.10670458390996,1.10130433638461,
9.46905320362962));
#266516=CARTESIAN_POINT('Ctrl Pts',(-1.19773202792704,1.00155159020856,
9.47767223554719));
#266517=CARTESIAN_POINT('Ctrl Pts',(-1.29606726630938,0.860911004548675,
9.48935687944838));
#266518=CARTESIAN_POINT('Ctrl Pts',(-1.316240197144,0.82974061218526,9.49191717714124));
#266519=CARTESIAN_POINT('Ctrl Pts',(-1.34079541171658,0.788646703524483,
9.49527281946354));
#266520=CARTESIAN_POINT('Ctrl Pts',(-1.34621697080266,0.779356026647765,
9.49603018461435));
#266521=CARTESIAN_POINT('Ctrl Pts',(-1.35472951465828,0.764414589223952,
9.49724653003967));
#266522=CARTESIAN_POINT('Ctrl Pts',(-1.35788258919811,0.758799442404477,
9.49770327383646));
#266523=CARTESIAN_POINT('Ctrl Pts',(-1.36351211466083,0.74862665376947,
9.49853015719919));
#266524=CARTESIAN_POINT('Ctrl Pts',(-1.36600082351253,0.744075871486197,
9.49889985258664));
#266525=CARTESIAN_POINT('Ctrl Pts',(-1.37181133849836,0.733323526834958,
9.49977290745003));
#266526=CARTESIAN_POINT('Ctrl Pts',(-1.37511390039701,0.727111753012827,
9.50027693937888));
#266527=CARTESIAN_POINT('Ctrl Pts',(-1.38464602345614,0.70888559788463,
9.5017549747366));
#266528=CARTESIAN_POINT('Ctrl Pts',(-1.39076092336078,0.696812337508565,
9.50273296704253));
#266529=CARTESIAN_POINT('Ctrl Pts',(-1.44694706164432,0.582191914322762,
9.51201021512522));
#266530=CARTESIAN_POINT('Ctrl Pts',(-1.48573717247729,0.474528771854461,
9.52070710677491));
#266531=CARTESIAN_POINT('Ctrl Pts',(-1.52957679191973,0.292185873805893,
9.53523409757297));
#266532=CARTESIAN_POINT('Ctrl Pts',(-1.54166922380741,0.219623954117895,
9.5409547588679));
#266533=CARTESIAN_POINT('Ctrl Pts',(-1.5500708800315,0.130799409081583,
9.54773268412755));
#266534=CARTESIAN_POINT('Ctrl Pts',(-1.55131563965779,0.115100141296424,
9.5489219718076));
#266535=CARTESIAN_POINT('Ctrl Pts',(-1.55366363609054,0.0784258028527149,
9.55167626828863));
#266536=CARTESIAN_POINT('Ctrl Pts',(-1.55458095330774,0.0574410695691954,
9.55323403154435));
#266537=CARTESIAN_POINT('Ctrl Pts',(-1.55521238816227,0.0304967721539908,
9.55520564980473));
#266538=CARTESIAN_POINT('Ctrl Pts',(-1.55531763178217,0.0245498015049972,
9.55563902857444));
#266539=CARTESIAN_POINT('Ctrl Pts',(-1.55543133538284,0.0150427069836612,
9.55632884370575));
#266540=CARTESIAN_POINT('Ctrl Pts',(-1.55546168833773,0.011482984387568,
9.55658645680835));
#266541=CARTESIAN_POINT('Ctrl Pts',(-1.55549033932317,0.00585819086112859,
9.55699242080158));
#266542=CARTESIAN_POINT('Ctrl Pts',(-1.55549674561761,0.00379323407447863,
9.5571412223948));
#266543=CARTESIAN_POINT('Ctrl Pts',(-1.55549962955002,0.00119753963184114,
9.5573279757493));
#266544=CARTESIAN_POINT('Ctrl Pts',(-1.55549994758783,0.000666849136197624,
9.55736614218525));
#266545=CARTESIAN_POINT('Ctrl Pts',(-1.55549999404086,0.000136157597505023,
9.55740429344755));
#266546=CARTESIAN_POINT('Ctrl Pts',(-1.55549999403006,0.000136280906002111,
9.55740428458294));
#266547=CARTESIAN_POINT('Ctrl Pts',(-1.55550006570921,-0.000681859550039542,
9.557463100469));
#266548=CARTESIAN_POINT('Ctrl Pts',(-1.55549949191725,-0.00150000170682517,
9.55752188023614));
#266549=CARTESIAN_POINT('Ctrl Pts',(-1.55549308453614,-0.00579941781312716,
9.55783058495101));
#266550=CARTESIAN_POINT('Ctrl Pts',(-1.55547620951391,-0.00928070896563226,
9.55807989708535));
#266551=CARTESIAN_POINT('Ctrl Pts',(-1.5553836847996,-0.0205577661163616,
9.55888548227781));
#266552=CARTESIAN_POINT('Ctrl Pts',(-1.55526111365173,-0.0283531966144095,
9.5594392283958));
#266553=CARTESIAN_POINT('Ctrl Pts',(-1.55394268147482,-0.0850725358237559,
9.56344768583682));
#266554=CARTESIAN_POINT('Ctrl Pts',(-1.55049704041156,-0.133922680817761,
9.56678882158552));
#266555=CARTESIAN_POINT('Ctrl Pts',(-1.53339288906358,-0.27867166500983,
9.57657273091826));
#266556=CARTESIAN_POINT('Ctrl Pts',(-1.51308294930104,-0.373541611719926,
9.58284323455126));
#266557=CARTESIAN_POINT('Ctrl Pts',(-1.4631520794489,-0.532588207295485,
9.59391411071522));
#266558=CARTESIAN_POINT('Ctrl Pts',(-1.43775269713861,-0.597770419429405,
9.59862255813638));
#266559=CARTESIAN_POINT('Ctrl Pts',(-1.40084422436254,-0.676390462343084,
9.60465938316445));
#266560=CARTESIAN_POINT('Ctrl Pts',(-1.39337715789063,-0.691641999031352,
9.60584769950275));
#266561=CARTESIAN_POINT('Ctrl Pts',(-1.38216170330981,-0.713630596333607,
9.60758770403325));
#266562=CARTESIAN_POINT('Ctrl Pts',(-1.37861036667116,-0.720467247820372,
9.60813252262895));
#266563=CARTESIAN_POINT('Ctrl Pts',(-1.37229002590633,-0.732416643203587,
9.60909165336074));
#266564=CARTESIAN_POINT('Ctrl Pts',(-1.36954284416077,-0.73754081295495,
9.60950518988078));
#266565=CARTESIAN_POINT('Ctrl Pts',(-1.36414606302589,-0.747473013212312,
9.61031117867769));
#266566=CARTESIAN_POINT('Ctrl Pts',(-1.3614996076125,-0.752282662166422,
9.61070351444077));
#266567=CARTESIAN_POINT('Ctrl Pts',(-1.35435075472932,-0.765113649228796,
9.61175570311962));
#266568=CARTESIAN_POINT('Ctrl Pts',(-1.34980263262482,-0.773109118614836,
9.61241718392743));
#266569=CARTESIAN_POINT('Ctrl Pts',(-1.33284229411428,-0.802318999292765,
9.61485561940009));
#266570=CARTESIAN_POINT('Ctrl Pts',(-1.31999927844321,-0.823277677706043,
9.61664801562009));
#266571=CARTESIAN_POINT('Ctrl Pts',(-1.30451222442658,-0.847256668671183,
9.61875041354431));
#266572=CARTESIAN_POINT('Ctrl Pts',(-1.30234591519674,-0.850582813682114,
9.61904321555013));
#266573=CARTESIAN_POINT('Ctrl Pts',(-1.22168218710971,-0.973403093064545,
9.62989889045855));
#266574=CARTESIAN_POINT('Ctrl Pts',(-1.12710574260796,-1.08149784058133,
9.64108519363977));
#266575=CARTESIAN_POINT('Ctrl Pts',(-0.989105531915848,-1.20117892341108,
9.65515452313245));
#266576=CARTESIAN_POINT('Ctrl Pts',(-0.958083469561142,-1.22606570119661,
9.65819115278687));
#266577=CARTESIAN_POINT('Ctrl Pts',(-0.908828346513758,-1.26256704799,9.66278675240287));
#266578=CARTESIAN_POINT('Ctrl Pts',(-0.891251083219132,-1.27503574316913,
9.66438489333406));
#266579=CARTESIAN_POINT('Ctrl Pts',(-0.868553741871806,-1.29043760852088,
9.66639051646606));
#266580=CARTESIAN_POINT('Ctrl Pts',(-0.863669434580082,-1.29371168919657,
9.66681876443209));
#266581=CARTESIAN_POINT('Ctrl Pts',(-0.856231437671663,-1.29863667736652,
9.66746571604367));
#266582=CARTESIAN_POINT('Ctrl Pts',(-0.853691355145765,-1.30030787325152,
9.66768573767221));
#266583=CARTESIAN_POINT('Ctrl Pts',(-0.848615468916188,-1.30362616528251,
9.66812356735667));
#266584=CARTESIAN_POINT('Ctrl Pts',(-0.846079791288125,-1.30527329704007,
9.6683413704027));
#266585=CARTESIAN_POINT('Ctrl Pts',(-0.840249403161727,-1.30903648631074,
9.66884009100542));
#266586=CARTESIAN_POINT('Ctrl Pts',(-0.836951497723282,-1.31114750252352,
9.66912067337497));
#266587=CARTESIAN_POINT('Ctrl Pts',(-0.827315327278335,-1.31726452150416,
9.66993621517443));
#266588=CARTESIAN_POINT('Ctrl Pts',(-0.820955906036507,-1.32123725223603,
9.67046904664975));
#266589=CARTESIAN_POINT('Ctrl Pts',(-0.776875434624696,-1.3483331707083,
9.6741271973021));
#266590=CARTESIAN_POINT('Ctrl Pts',(-0.738207254345492,-1.3698863903696,
9.67715964479529));
#266591=CARTESIAN_POINT('Ctrl Pts',(-0.621197293782455,-1.42871018188696,
9.68598506849212));
#266592=CARTESIAN_POINT('Ctrl Pts',(-0.54060113359116,-1.46111294880882,
9.69162587110098));
#266593=CARTESIAN_POINT('Ctrl Pts',(-0.37027140464894,-1.51355595170738,
9.70339885958134));
#266594=CARTESIAN_POINT('Ctrl Pts',(-0.280630773527694,-1.5327084213721,
9.7095218113252));
#266595=CARTESIAN_POINT('Ctrl Pts',(-0.176965063265548,-1.54545519503463,
9.71681927175854));
#266596=CARTESIAN_POINT('Ctrl Pts',(-0.164076045708595,-1.54687666826049,
9.71773004930059));
#266597=CARTESIAN_POINT('Ctrl Pts',(-0.144286528843685,-1.54880905757599,
9.71913442451726));
#266598=CARTESIAN_POINT('Ctrl Pts',(-0.137397653596425,-1.5494353749754,
9.71962440626672));
#266599=CARTESIAN_POINT('Ctrl Pts',(-0.124845041246703,-1.55049225315724,
9.7205193532912));
#266600=CARTESIAN_POINT('Ctrl Pts',(-0.119182655145225,-1.55093778230113,
9.72092384255929));
#266601=CARTESIAN_POINT('Ctrl Pts',(-0.106826879336625,-1.55184189883895,
9.7218082462049));
#266602=CARTESIAN_POINT('Ctrl Pts',(-0.100132735566828,-1.55228821222174,
9.72228853639637));
#266603=CARTESIAN_POINT('Ctrl Pts',(-0.081788762242601,-1.55339209409597,
9.72360790227887));
#266604=CARTESIAN_POINT('Ctrl Pts',(-0.0701343008674653,-1.55396189325335,
9.72444969784083));
#266605=CARTESIAN_POINT('Ctrl Pts',(-0.00891603221280406,-1.55626485655855,
9.72889111642858));
#266606=CARTESIAN_POINT('Ctrl Pts',(0.0406978766529117,-1.55575784430602,
9.73255959986612));
#266607=CARTESIAN_POINT('Ctrl Pts',(0.237230812759556,-1.5443423685084,
9.74737792992191));
#266608=CARTESIAN_POINT('Ctrl Pts',(0.382278354418441,-1.51496709974836,
9.75904126554015));
#266609=CARTESIAN_POINT('Ctrl Pts',(0.549010781067511,-1.45569567812998,
9.77241859469092));
#266610=CARTESIAN_POINT('Ctrl Pts',(0.576713291064678,-1.44494457729338,
9.77463643653261));
#266611=CARTESIAN_POINT('Ctrl Pts',(0.610097398241374,-1.43087521091526,
9.77728952885686));
#266612=CARTESIAN_POINT('Ctrl Pts',(0.616085866998809,-1.42830700938748,
9.77776465592653));
#266613=CARTESIAN_POINT('Ctrl Pts',(0.625449601076448,-1.42422144978071,
9.77850614488328));
#266614=CARTESIAN_POINT('Ctrl Pts',(0.628835797811732,-1.42272958838604,
9.77877399319462));
#266615=CARTESIAN_POINT('Ctrl Pts',(0.635168128936506,-1.41991272011558,
9.77927428318958));
#266616=CARTESIAN_POINT('Ctrl Pts',(0.638115428237316,-1.41859063344479,
9.7795068875135));
#266617=CARTESIAN_POINT('Ctrl Pts',(0.644828018557296,-1.41555437596949,
9.78003611097663));
#266618=CARTESIAN_POINT('Ctrl Pts',(0.648590604447967,-1.41383435866132,
9.78033236893495));
#266619=CARTESIAN_POINT('Ctrl Pts',(0.658545719602895,-1.4092354024515,
9.78111530670266));
#266620=CARTESIAN_POINT('Ctrl Pts',(0.66472632047392,-1.40633061820943,
9.78160045738315));
#266621=CARTESIAN_POINT('Ctrl Pts',(0.70927592023042,-1.38503369897656,
9.78509208769269));
#266622=CARTESIAN_POINT('Ctrl Pts',(0.746899326153401,-1.36511277164091,
9.78801234269924));
#266623=CARTESIAN_POINT('Ctrl Pts',(0.867674552347196,-1.29467370050598,
9.79744803569534));
#266624=CARTESIAN_POINT('Ctrl Pts',(0.946910897578922,-1.23790195036941,
9.80374979812193));
#266625=CARTESIAN_POINT('Ctrl Pts',(1.07727269227693,-1.12461329298098,
9.81519049687603));
#266626=CARTESIAN_POINT('Ctrl Pts',(1.13053296868357,-1.07105763208144,
9.82025538835076));
#266627=CARTESIAN_POINT('Ctrl Pts',(1.19120373928502,-1.00046275146492,
9.82672009022015));
#266628=CARTESIAN_POINT('Ctrl Pts',(1.20248388478312,-0.986876146266399,
9.82795511937148));
#266629=CARTESIAN_POINT('Ctrl Pts',(1.21842558041628,-0.966995655092733,
9.82975096597959));
#266630=CARTESIAN_POINT('Ctrl Pts',(1.22327502903952,-0.960853626356437,
9.83030426788144));
#266631=CARTESIAN_POINT('Ctrl Pts',(1.23165797599887,-0.950069948665049,
9.83127322520721));
#266632=CARTESIAN_POINT('Ctrl Pts',(1.23521212625693,-0.945444487345753,
9.83168805491645));
#266633=CARTESIAN_POINT('Ctrl Pts',(1.24203947258411,-0.93645499428858,
9.8324928149631));
#266634=CARTESIAN_POINT('Ctrl Pts',(1.24531589921918,-0.932093513301942,
9.83288261071643));
#266635=CARTESIAN_POINT('Ctrl Pts',(1.25394680562262,-0.920477569518755,
9.83391909000782));
#266636=CARTESIAN_POINT('Ctrl Pts',(1.25926119657258,-0.913193725215407,
9.83456731353236));
#266637=CARTESIAN_POINT('Ctrl Pts',(1.27814886649666,-0.886828093551,9.83690794903746));
#266638=CARTESIAN_POINT('Ctrl Pts',(1.29135354595389,-0.867487464491169,
9.83861424904));
#266639=CARTESIAN_POINT('Ctrl Pts',(1.39917182459066,-0.701648736084956,
9.85316505059864));
#266640=CARTESIAN_POINT('Ctrl Pts',(1.46895224824044,-0.54050297310002,
9.8669881214529));
#266641=CARTESIAN_POINT('Ctrl Pts',(1.51865727727712,-0.338250847533332,
9.88279201769263));
#266642=CARTESIAN_POINT('Ctrl Pts',(1.52568075238155,-0.305011875809233,
9.88533539302164));
#266643=CARTESIAN_POINT('Ctrl Pts',(1.5327928183653,-0.264900472378489,
9.88832049661821));
#266644=CARTESIAN_POINT('Ctrl Pts',(1.53393127173312,-0.258226533108866,
9.88881439758493));
#266645=CARTESIAN_POINT('Ctrl Pts',(1.53563348762522,-0.247838953554657,
9.88957859570405));
#266646=CARTESIAN_POINT('Ctrl Pts',(1.53622741708248,-0.244130454941157,
9.88985052883173));
#266647=CARTESIAN_POINT('Ctrl Pts',(1.53730595884031,-0.237236215816053,
9.89035435523716));
#266648=CARTESIAN_POINT('Ctrl Pts',(1.5377940999222,-0.234051147756886,
9.89058643647957));
#266649=CARTESIAN_POINT('Ctrl Pts',(1.53888431020765,-0.226786971484537,
9.89111421220874));
#266650=CARTESIAN_POINT('Ctrl Pts',(1.53948006016304,-0.222706973524559,
9.89140954872123));
#266651=CARTESIAN_POINT('Ctrl Pts',(1.54099201539908,-0.212056290805593,
9.89217777595388));
#266652=CARTESIAN_POINT('Ctrl Pts',(1.54188243379256,-0.205481937186603,
9.89264926517398));
#266653=CARTESIAN_POINT('Ctrl Pts',(1.54762235232947,-0.160961761497843,
9.89582498313843));
#266654=CARTESIAN_POINT('Ctrl Pts',(1.55111318153999,-0.122850056412527,
9.89845964745957));
#266655=CARTESIAN_POINT('Ctrl Pts',(1.56134100049507,0.0648263101851032,
9.91119418471039));
#266656=CARTESIAN_POINT('Ctrl Pts',(1.54786993121525,0.214693316810053,
9.92069523844469));
#266657=CARTESIAN_POINT('Ctrl Pts',(1.50404071096711,0.398749477501326,
9.93355995810379));
#266658=CARTESIAN_POINT('Ctrl Pts',(1.493434327872,0.436798654086403,9.93628159575215));
#266659=CARTESIAN_POINT('Ctrl Pts',(1.47817694821596,0.484442294591727,
9.9397895344268));
#266660=CARTESIAN_POINT('Ctrl Pts',(1.47485924787553,0.494450822895139,
9.94053210933116));
#266661=CARTESIAN_POINT('Ctrl Pts',(1.46936697264354,0.510472154154579,
9.94173028748855));
#266662=CARTESIAN_POINT('Ctrl Pts',(1.46725658702874,0.516506753167798,
9.94218377205813));
#266663=CARTESIAN_POINT('Ctrl Pts',(1.46316988138562,0.527965409064701,
9.94304909986741));
#266664=CARTESIAN_POINT('Ctrl Pts',(1.46120044398097,0.533391822043335,
9.94346070889015));
#266665=CARTESIAN_POINT('Ctrl Pts',(1.45663683796814,0.545751009800278,
9.94440241939294));
#266666=CARTESIAN_POINT('Ctrl Pts',(1.45402331359471,0.552676435575332,
9.94493315790384));
#266667=CARTESIAN_POINT('Ctrl Pts',(1.44708281771471,0.57067763389007,9.94632082704289));
#266668=CARTESIAN_POINT('Ctrl Pts',(1.44267816994791,0.581722723047897,
9.94718033638785));
#266669=CARTESIAN_POINT('Ctrl Pts',(1.43696565742733,0.595583384729583,
9.94826939717981));
#266670=CARTESIAN_POINT('Ctrl Pts',(1.43577539858722,0.598447049047754,
9.94849496736736));
#266671=CARTESIAN_POINT('Ctrl Pts',(1.4345766815454,0.601306905636538,9.94872080685755));
#266672=CARTESIAN_POINT('Origin',(0.,0.,-1.29405622560371));
#266673=CARTESIAN_POINT('',(1.43457669771236,0.601306867065985,10.7874266037958));
#266674=CARTESIAN_POINT('',(1.4345766806181,0.60130690784885,10.6508134549194));
#266675=CARTESIAN_POINT('',(1.43457668357355,0.601306900797845,-1.29405622560371));
#266676=CARTESIAN_POINT('',(-1.55549951249496,-0.000556301241264363,10.3953761425462));
#266677=CARTESIAN_POINT('Ctrl Pts',(1.43457669771236,0.601306867065985,
10.7874266037958));
#266678=CARTESIAN_POINT('Ctrl Pts',(1.45423156484639,0.554414978861378,
10.7835217661703));
#266679=CARTESIAN_POINT('Ctrl Pts',(1.47158201151098,0.506572022160425,
10.7796660057214));
#266680=CARTESIAN_POINT('Ctrl Pts',(1.48894631453756,0.450205259606307,
10.7753315281049));
#266681=CARTESIAN_POINT('Ctrl Pts',(1.49127132062371,0.442442944616008,
10.7747391284532));
#266682=CARTESIAN_POINT('Ctrl Pts',(1.49465467865279,0.430817454322671,
10.7738589749464));
#266683=CARTESIAN_POINT('Ctrl Pts',(1.49575889068674,0.426967948768711,
10.7735686866264));
#266684=CARTESIAN_POINT('Ctrl Pts',(1.49771233635579,0.420057256655038,
10.7730496755902));
#266685=CARTESIAN_POINT('Ctrl Pts',(1.49856706660349,0.416997708459551,
10.7728206417466));
#266686=CARTESIAN_POINT('Ctrl Pts',(1.5004116655524,0.410315955334787,10.7723220848118));
#266687=CARTESIAN_POINT('Ctrl Pts',(1.50139779219925,0.406692782963212,
10.7720527791139));
#266688=CARTESIAN_POINT('Ctrl Pts',(1.50415856681661,0.39640239146838,10.7712907504056));
#266689=CARTESIAN_POINT('Ctrl Pts',(1.50590202092662,0.38972677375402,10.7707997834689));
#266690=CARTESIAN_POINT('Ctrl Pts',(1.51687627530202,0.346533336744395,
10.7676435189769));
#266691=CARTESIAN_POINT('Ctrl Pts',(1.52482343111679,0.309698365693566,
10.7650460187595));
#266692=CARTESIAN_POINT('Ctrl Pts',(1.55028099038903,0.166685559859222,
10.755192700768));
#266693=CARTESIAN_POINT('Ctrl Pts',(1.55809744699292,0.0590862201464926,
10.7482481197342));
#266694=CARTESIAN_POINT('Ctrl Pts',(1.55229954441817,-0.126907574114333,
10.7359030453782));
#266695=CARTESIAN_POINT('Ctrl Pts',(1.54392189113161,-0.205041200641974,
10.7306151081072));
#266696=CARTESIAN_POINT('Ctrl Pts',(1.52755683722975,-0.293748557985828,
10.7243134914281));
#266697=CARTESIAN_POINT('Ctrl Pts',(1.52529610912158,-0.305270163163949,
10.7234893179022));
#266698=CARTESIAN_POINT('Ctrl Pts',(1.52141671298726,-0.323921075857665,
10.7221453592533));
#266699=CARTESIAN_POINT('Ctrl Pts',(1.51987780503289,-0.331066658570192,
10.7216281118342));
#266700=CARTESIAN_POINT('Ctrl Pts',(1.51704934517923,-0.343764486579375,
10.7207046467754));
#266701=CARTESIAN_POINT('Ctrl Pts',(1.51577952038416,-0.349321029917241,
10.7202990665875));
#266702=CARTESIAN_POINT('Ctrl Pts',(1.51303943261021,-0.361014893146869,
10.7194423424182));
#266703=CARTESIAN_POINT('Ctrl Pts',(1.51156230439561,-0.367150480687252,
10.7189909846686));
#266704=CARTESIAN_POINT('Ctrl Pts',(1.50755123974292,-0.383376775273461,
10.7177923180683));
#266705=CARTESIAN_POINT('Ctrl Pts',(1.50495337009474,-0.393451186720672,
10.717042965207));
#266706=CARTESIAN_POINT('Ctrl Pts',(1.49217747674197,-0.441016773887805,
10.7134799303669));
#266707=CARTESIAN_POINT('Ctrl Pts',(1.48069921710864,-0.478140929372599,
10.7106246429486));
#266708=CARTESIAN_POINT('Ctrl Pts',(1.41827547971653,-0.656131332688146,
10.6965558847399));
#266709=CARTESIAN_POINT('Ctrl Pts',(1.34855256554065,-0.789560131631482,
10.6847299266808));
#266710=CARTESIAN_POINT('Ctrl Pts',(1.23791751017579,-0.94269633478496,
10.6703291456549));
#266711=CARTESIAN_POINT('Ctrl Pts',(1.21377201115519,-0.973588356546316,
10.6673815396478));
#266712=CARTESIAN_POINT('Ctrl Pts',(1.18420383267967,-1.00860573210254,
10.6640186393697));
#266713=CARTESIAN_POINT('Ctrl Pts',(1.17989236849965,-1.01364601469693,
10.663534055731));
#266714=CARTESIAN_POINT('Ctrl Pts',(1.17286620103169,-1.02175432626998,
10.662753840621));
#266715=CARTESIAN_POINT('Ctrl Pts',(1.17017144758954,-1.02483940842595,
10.662456823813));
#266716=CARTESIAN_POINT('Ctrl Pts',(1.16536063210452,-1.03030334515677,
10.6619305570907));
#266717=CARTESIAN_POINT('Ctrl Pts',(1.16324942611813,-1.03268637990313,
10.6617009578816));
#266718=CARTESIAN_POINT('Ctrl Pts',(1.15867682209809,-1.0378159147098,10.661206589811));
#266719=CARTESIAN_POINT('Ctrl Pts',(1.15621297155535,-1.04056014533795,
10.6609420088091));
#266720=CARTESIAN_POINT('Ctrl Pts',(1.14931950436625,-1.04818335792989,
10.6602066578212));
#266721=CARTESIAN_POINT('Ctrl Pts',(1.14486853871365,-1.05304307041731,
10.6597374545337));
#266722=CARTESIAN_POINT('Ctrl Pts',(1.11876024108901,-1.08118776700141,
10.6570165531571));
#266723=CARTESIAN_POINT('Ctrl Pts',(1.09642194601422,-1.10383456618323,
10.65481289122));
#266724=CARTESIAN_POINT('Ctrl Pts',(0.967917785881114,-1.22635978958701,
10.6426962108693));
#266725=CARTESIAN_POINT('Ctrl Pts',(0.848814746059553,-1.31161924449267,
10.6334458568429));
#266726=CARTESIAN_POINT('Ctrl Pts',(0.675982332720464,-1.4018008306185,
10.6202961308335));
#266727=CARTESIAN_POINT('Ctrl Pts',(0.631342500743646,-1.42246388624232,
10.6169285277414));
#266728=CARTESIAN_POINT('Ctrl Pts',(0.575105366247022,-1.44532605818967,
10.6126793747554));
#266729=CARTESIAN_POINT('Ctrl Pts',(0.56436013137958,-1.44955552710602,
10.6118672651422));
#266730=CARTESIAN_POINT('Ctrl Pts',(0.547372449666443,-1.45602459372945,
10.6105825264636));
#266731=CARTESIAN_POINT('Ctrl Pts',(0.541160909247763,-1.45834463829094,
10.6101125891765));
#266732=CARTESIAN_POINT('Ctrl Pts',(0.529669175375238,-1.46255333597755,
10.6092427639186));
#266733=CARTESIAN_POINT('Ctrl Pts',(0.524393213671634,-1.46445329453189,
10.6088432597875));
#266734=CARTESIAN_POINT('Ctrl Pts',(0.51267685693432,-1.46860111035686,
10.6079556651249));
#266735=CARTESIAN_POINT('Ctrl Pts',(0.50623174893115,-1.47083520307617,
10.6074671280121));
#266736=CARTESIAN_POINT('Ctrl Pts',(0.487688518044741,-1.47712659723637,
10.6060606401153));
#266737=CARTESIAN_POINT('Ctrl Pts',(0.47555514305992,-1.48107743307225,
10.6051392143814));
#266738=CARTESIAN_POINT('Ctrl Pts',(0.380194303144987,-1.5108359742808,
10.5978868305215));
#266739=CARTESIAN_POINT('Ctrl Pts',(0.294995575051489,-1.52975343055046,
10.5913313192512));
#266740=CARTESIAN_POINT('Ctrl Pts',(0.117440681523819,-1.55379029920837,
10.5775589463255));
#266741=CARTESIAN_POINT('Ctrl Pts',(0.0252921300135777,-1.55801685828702,
10.5703521365794));
#266742=CARTESIAN_POINT('Ctrl Pts',(-0.0828976978068575,-1.55337421480202,
10.5620711461192));
#266743=CARTESIAN_POINT('Ctrl Pts',(-0.099095807129142,-1.55242504991223,
10.5608365252184));
#266744=CARTESIAN_POINT('Ctrl Pts',(-0.144255210267106,-1.5490691012917,
10.5574136872666));
#266745=CARTESIAN_POINT('Ctrl Pts',(-0.17317030581851,-1.54610380584979,
10.5552441312997));
#266746=CARTESIAN_POINT('Ctrl Pts',(-0.208585359246172,-1.5414657550715,
10.5526269787601));
#266747=CARTESIAN_POINT('Ctrl Pts',(-0.215177601349624,-1.54055935630778,
10.5521415363609));
#266748=CARTESIAN_POINT('Ctrl Pts',(-0.225468036437977,-1.53907713231616,
10.5513866633163));
#266749=CARTESIAN_POINT('Ctrl Pts',(-0.229170206918606,-1.53853023101168,
10.5511156713637));
#266750=CARTESIAN_POINT('Ctrl Pts',(-0.236012353000364,-1.53749423325551,
10.5506159699221));
#266751=CARTESIAN_POINT('Ctrl Pts',(-0.239152781415582,-1.53700887946959,
10.5503870616462));
#266752=CARTESIAN_POINT('Ctrl Pts',(-0.246263614445864,-1.53588757720398,
10.5498697415476));
#266753=CARTESIAN_POINT('Ctrl Pts',(-0.250233049780753,-1.53524585633393,
10.5495816586378));
#266754=CARTESIAN_POINT('Ctrl Pts',(-0.262274017403842,-1.53325130623887,
10.5487097760464));
#266755=CARTESIAN_POINT('Ctrl Pts',(-0.270337575309741,-1.53185013347118,
10.5481286195734));
#266756=CARTESIAN_POINT('Ctrl Pts',(-0.365255555363848,-1.51458375672526,
10.5413157704661));
#266757=CARTESIAN_POINT('Ctrl Pts',(-0.450633487045888,-1.49141217318771,
10.5354606363794));
#266758=CARTESIAN_POINT('Ctrl Pts',(-0.651402014909569,-1.41809205992767,
10.5213719735854));
#266759=CARTESIAN_POINT('Ctrl Pts',(-0.763557839278286,-1.36098661716113,
10.5131916845782));
#266760=CARTESIAN_POINT('Ctrl Pts',(-0.875587235721102,-1.28569786315884,
10.503823548588));
#266761=CARTESIAN_POINT('Ctrl Pts',(-0.883487782714621,-1.28028173990148,
10.5031561852251));
#266762=CARTESIAN_POINT('Ctrl Pts',(-0.900267479315245,-1.26854934545049,
10.5017239458047));
#266763=CARTESIAN_POINT('Ctrl Pts',(-0.909131245124481,-1.2622120838619,
10.5009583259423));
#266764=CARTESIAN_POINT('Ctrl Pts',(-0.923621547451472,-1.25162024290108,
10.4996912597618));
#266765=CARTESIAN_POINT('Ctrl Pts',(-0.92928712863231,-1.24741950640167,
10.4991918894905));
#266766=CARTESIAN_POINT('Ctrl Pts',(-0.939346742389795,-1.23985425473455,
10.4982980140685));
#266767=CARTESIAN_POINT('Ctrl Pts',(-0.943751787689046,-1.23650452373014,
10.4979040911938));
#266768=CARTESIAN_POINT('Ctrl Pts',(-0.948237323468547,-1.23305565317334,
10.4975003763098));
#266769=CARTESIAN_POINT('Ctrl Pts',(-0.9483358252886,-1.23297989761216,
10.4974915094956));
#266770=CARTESIAN_POINT('Ctrl Pts',(-0.948509900555364,-1.23284598699181,
10.4974758375341));
#266771=CARTESIAN_POINT('Ctrl Pts',(-0.948585477743541,-1.23278783677785,
10.4974690325783));
#266772=CARTESIAN_POINT('Ctrl Pts',(-0.948719391787902,-1.23268478171235,
10.4974569736416));
#266773=CARTESIAN_POINT('Ctrl Pts',(-0.948777730810681,-1.23263987966371,
10.4974517197715));
#266774=CARTESIAN_POINT('Ctrl Pts',(-0.948936255817107,-1.23251784911289,
10.4974374421699));
#266775=CARTESIAN_POINT('Ctrl Pts',(-0.949036435570715,-1.23244071254777,
10.4974284181197));
#266776=CARTESIAN_POINT('Ctrl Pts',(-0.949231601350095,-1.23229040058556,
10.4974108352688));
#266777=CARTESIAN_POINT('Ctrl Pts',(-0.949326588320262,-1.23221722641959,
10.497402276517));
#266778=CARTESIAN_POINT('Ctrl Pts',(-0.949511783623432,-1.2320745252345,
10.4973855872543));
#266779=CARTESIAN_POINT('Ctrl Pts',(-0.949601992787823,-1.23200499928569,
10.4973774567856));
#266780=CARTESIAN_POINT('Ctrl Pts',(-0.949778004265813,-1.23186931301664,
10.4973615909237));
#266781=CARTESIAN_POINT('Ctrl Pts',(-0.949863807306044,-1.23180315363669,
10.4973538555678));
#266782=CARTESIAN_POINT('Ctrl Pts',(-0.950031340495033,-1.23167394741138,
10.4973387501258));
#266783=CARTESIAN_POINT('Ctrl Pts',(-0.95011307128588,-1.23161090139152,
10.4973313800722));
#266784=CARTESIAN_POINT('Ctrl Pts',(-0.95027276081356,-1.2314876937074,
10.4973169783725));
#266785=CARTESIAN_POINT('Ctrl Pts',(-0.950350720114854,-1.23142753277412,
10.4973099467553));
#266786=CARTESIAN_POINT('Ctrl Pts',(-0.950503138376721,-1.23130988901431,
10.4972961976557));
#266787=CARTESIAN_POINT('Ctrl Pts',(-0.950577597837861,-1.23125240683509,
10.4972894801989));
#266788=CARTESIAN_POINT('Ctrl Pts',(-0.950723262457778,-1.23113993368578,
10.4972763374316));
#266789=CARTESIAN_POINT('Ctrl Pts',(-0.950794468061787,-1.23108494329079,
10.4972699121438));
#266790=CARTESIAN_POINT('Ctrl Pts',(-0.950933848294579,-1.23097728394535,
10.4972573337475));
#266791=CARTESIAN_POINT('Ctrl Pts',(-0.951002023322032,-1.23092461550625,
10.4972511806591));
#266792=CARTESIAN_POINT('Ctrl Pts',(-0.951135545596474,-1.23082144550847,
10.4972391284877));
#266793=CARTESIAN_POINT('Ctrl Pts',(-0.951200893196398,-1.23077094440966,
10.497233229423));
#266794=CARTESIAN_POINT('Ctrl Pts',(-0.951328945893783,-1.2306719680672,
10.4972216687212));
#266795=CARTESIAN_POINT('Ctrl Pts',(-0.951391651307561,-1.23062349323587,
10.4972160071006));
#266796=CARTESIAN_POINT('Ctrl Pts',(-0.951514588921246,-1.23052844049516,
10.4972049061347));
#266797=CARTESIAN_POINT('Ctrl Pts',(-0.95157482141183,-1.23048186295145,
10.4971994668036));
#266798=CARTESIAN_POINT('Ctrl Pts',(-0.957076944454097,-1.22622644763627,
10.4967025500275));
#266799=CARTESIAN_POINT('Ctrl Pts',(-0.962490774284427,-1.22198162223904,
10.4962096508706));
#266800=CARTESIAN_POINT('Ctrl Pts',(-0.973707354756502,-1.21306624778813,
10.4951800674235));
#266801=CARTESIAN_POINT('Ctrl Pts',(-0.979505058008557,-1.20838966065369,
10.4946431493827));
#266802=CARTESIAN_POINT('Ctrl Pts',(-0.994482310818171,-1.19612998810639,
10.4932436117579));
#266803=CARTESIAN_POINT('Ctrl Pts',(-1.00360862532356,-1.18848295213681,
10.4923784306437));
#266804=CARTESIAN_POINT('Ctrl Pts',(-1.03040524144025,-1.16550103536149,
10.4898005886437));
#266805=CARTESIAN_POINT('Ctrl Pts',(-1.04781764171479,-1.14987203934489,
10.4880761347964));
#266806=CARTESIAN_POINT('Ctrl Pts',(-1.16398244174426,-1.04077501920385,
10.476225214078));
#266807=CARTESIAN_POINT('Ctrl Pts',(-1.25045070465667,-0.935108740075265,
10.4655748212541));
#266808=CARTESIAN_POINT('Ctrl Pts',(-1.35161950553541,-0.771913652987544,
10.4507945694255));
#266809=CARTESIAN_POINT('Ctrl Pts',(-1.37857529808757,-0.722673998363168,
10.4465301019183));
#266810=CARTESIAN_POINT('Ctrl Pts',(-1.40621064075385,-0.66499147524461,
10.4418310332293));
#266811=CARTESIAN_POINT('Ctrl Pts',(-1.40955297142878,-0.657877234749755,
10.4412564719334));
#266812=CARTESIAN_POINT('Ctrl Pts',(-1.4145181939206,-0.647097052812373,
10.4403936880099));
#266813=CARTESIAN_POINT('Ctrl Pts',(-1.41618101010326,-0.643449814898415,
10.4401031306445));
#266814=CARTESIAN_POINT('Ctrl Pts',(-1.41913643646542,-0.636900398379603,
10.4395838335024));
#266815=CARTESIAN_POINT('Ctrl Pts',(-1.42043426527787,-0.634000663576762,
10.4393547810659));
#266816=CARTESIAN_POINT('Ctrl Pts',(-1.42324551271229,-0.627667538011124,
10.4388564098179));
#266817=CARTESIAN_POINT('Ctrl Pts',(-1.42475539376767,-0.624232646105482,
10.4385873071486));
#266818=CARTESIAN_POINT('Ctrl Pts',(-1.42900097619172,-0.614478539484409,
10.4378264313983));
#266819=CARTESIAN_POINT('Ctrl Pts',(-1.43170721266465,-0.608146468659603,
10.4373364060013));
#266820=CARTESIAN_POINT('Ctrl Pts',(-1.44883425489476,-0.567324463212259,
10.4342010367673));
#266821=CARTESIAN_POINT('Ctrl Pts',(-1.46205125233759,-0.532338664876566,
10.4316224594959));
#266822=CARTESIAN_POINT('Ctrl Pts',(-1.5279120355649,-0.336973133875317,
10.417633839255));
#266823=CARTESIAN_POINT('Ctrl Pts',(-1.5554393773208,-0.169340451667066,
10.4069999775086));
#266824=CARTESIAN_POINT('Ctrl Pts',(-1.55549989999529,-0.000557776525539587,
10.3953769175085));
#266825=CARTESIAN_POINT('Ctrl Pts',(-1.55549990054006,-0.000556255220122361,
10.3953768127452));
#266826=CARTESIAN_POINT('Ctrl Pts',(-1.55550868565946,0.0240102600394349,
10.3936850621365));
#266827=CARTESIAN_POINT('Ctrl Pts',(-1.55493549136123,0.0485725664847252,
10.3919773671645));
#266828=CARTESIAN_POINT('Ctrl Pts',(-1.55345097257562,0.0801224492624995,
10.3897584704002));
#266829=CARTESIAN_POINT('Ctrl Pts',(-1.55307356133013,0.0871323205925535,
10.3892638594744));
#266830=CARTESIAN_POINT('Ctrl Pts',(-1.55231571177791,0.099631608214045,
10.3883789309062));
#266831=CARTESIAN_POINT('Ctrl Pts',(-1.55195356875411,0.105122050068117,
10.3879891871315));
#266832=CARTESIAN_POINT('Ctrl Pts',(-1.55116860993205,0.116132882799388,
10.3872054483733));
#266833=CARTESIAN_POINT('Ctrl Pts',(-1.55074543641878,0.12165316634033,
10.3868114477975));
#266834=CARTESIAN_POINT('Ctrl Pts',(-1.54977582196752,0.133473362848572,
10.3859654443242));
#266835=CARTESIAN_POINT('Ctrl Pts',(-1.54922041869164,0.139772418854117,
10.3855131673219));
#266836=CARTESIAN_POINT('Ctrl Pts',(-1.54764428899439,0.156482713325616,
10.384309444217));
#266837=CARTESIAN_POINT('Ctrl Pts',(-1.54655693196448,0.166887180690696,
10.383555923194));
#266838=CARTESIAN_POINT('Ctrl Pts',(-1.54136714804898,0.212127053134722,
10.3802613356304));
#266839=CARTESIAN_POINT('Ctrl Pts',(-1.53619234332671,0.246826434431386,
10.3776869987059));
#266840=CARTESIAN_POINT('Ctrl Pts',(-1.50145063304191,0.43575653621164,
10.3633968995562));
#266841=CARTESIAN_POINT('Ctrl Pts',(-1.449827845268,0.584995434557289,10.3509748067582));
#266842=CARTESIAN_POINT('Ctrl Pts',(-1.35977738374537,0.756253455099173,
10.3362621216931));
#266843=CARTESIAN_POINT('Ctrl Pts',(-1.34164708027808,0.78797047579587,
10.3335223467886));
#266844=CARTESIAN_POINT('Ctrl Pts',(-1.31881158193795,0.824841258967402,
10.3303436974223));
#266845=CARTESIAN_POINT('Ctrl Pts',(-1.31516950369142,0.830636064929464,
10.3298443222486));
#266846=CARTESIAN_POINT('Ctrl Pts',(-1.30947654336594,0.839562649637762,
10.3290755932031));
#266847=CARTESIAN_POINT('Ctrl Pts',(-1.30745246664984,0.842711284216797,
10.3288045460241));
#266848=CARTESIAN_POINT('Ctrl Pts',(-1.30368905066121,0.848519420423827,
10.3283047937071));
#266849=CARTESIAN_POINT('Ctrl Pts',(-1.30195293989458,0.851180879904725,
10.3280758894511));
#266850=CARTESIAN_POINT('Ctrl Pts',(-1.29800203907194,0.857197244696896,
10.3275586427851));
#266851=CARTESIAN_POINT('Ctrl Pts',(-1.29578239472684,0.860548892422617,
10.3272706288879));
#266852=CARTESIAN_POINT('Ctrl Pts',(-1.2891542769947,0.870473513249677,
10.3264180762232));
#266853=CARTESIAN_POINT('Ctrl Pts',(-1.28470851609589,0.877021620517394,
10.3258559553043));
#266854=CARTESIAN_POINT('Ctrl Pts',(-1.2454890806787,0.933849234224909,
10.3209782069085));
#266855=CARTESIAN_POINT('Ctrl Pts',(-1.20782438305582,0.982079320103689,
10.3168417958582));
#266856=CARTESIAN_POINT('Ctrl Pts',(-1.089058024934,1.11695585114861,10.3048735161258));
#266857=CARTESIAN_POINT('Ctrl Pts',(-1.00078945260503,1.19668648460321,
10.29723070882));
#266858=CARTESIAN_POINT('Ctrl Pts',(-0.879712166781752,1.28319968722721,
10.2871627538557));
#266859=CARTESIAN_POINT('Ctrl Pts',(-0.854598475144424,1.30006007226175,
10.2850963465806));
#266860=CARTESIAN_POINT('Ctrl Pts',(-0.816925709653545,1.32378873608082,
10.2820160925));
#266861=CARTESIAN_POINT('Ctrl Pts',(-0.804736954557418,1.33123350467389,
10.2810224356398));
#266862=CARTESIAN_POINT('Ctrl Pts',(-0.785200706215637,1.34279969807468,
10.2794333336505));
#266863=CARTESIAN_POINT('Ctrl Pts',(-0.777919066964841,1.34703121661438,
10.2788418066149));
#266864=CARTESIAN_POINT('Ctrl Pts',(-0.764029017533328,1.35495283817906,
10.2777146668191));
#266865=CARTESIAN_POINT('Ctrl Pts',(-0.757427314795329,1.35865425788761,
10.2771794750982));
#266866=CARTESIAN_POINT('Ctrl Pts',(-0.745844118606342,1.36503802443247,
10.276241204718));
#266867=CARTESIAN_POINT('Ctrl Pts',(-0.740874470652498,1.3677416695397,
10.2758388934621));
#266868=CARTESIAN_POINT('Ctrl Pts',(-0.731163990606952,1.37295602526604,
10.2750532103122));
#266869=CARTESIAN_POINT('Ctrl Pts',(-0.726424695680042,1.37546944300873,
10.2746699413505));
#266870=CARTESIAN_POINT('Ctrl Pts',(-0.713888104391087,1.38203518161326,
10.2736565448411));
#266871=CARTESIAN_POINT('Ctrl Pts',(-0.706069404678794,1.38604598000914,
10.2730249684271));
#266872=CARTESIAN_POINT('Ctrl Pts',(-0.678245557197977,1.40002240284376,
10.2707786994315));
#266873=CARTESIAN_POINT('Ctrl Pts',(-0.658060950260043,1.40962245072208,
10.269151430898));
#266874=CARTESIAN_POINT('Ctrl Pts',(-0.476761938066386,1.49110793840217,
10.25454695146));
#266875=CARTESIAN_POINT('Ctrl Pts',(-0.30472376853314,1.5355188483371,10.2405573060793));
#266876=CARTESIAN_POINT('Ctrl Pts',(-0.0954235847670609,1.55293574567425,
10.2246241548186));
#266877=CARTESIAN_POINT('Ctrl Pts',(-0.0617670163658839,1.55463833700794,
10.2221018499259));
#266878=CARTESIAN_POINT('Ctrl Pts',(-0.0213826531515281,1.55536744330044,
10.2191425020006));
#266879=CARTESIAN_POINT('Ctrl Pts',(-0.0146857405561477,1.55544509222503,
10.2186539721346));
#266880=CARTESIAN_POINT('Ctrl Pts',(-0.00427714314134912,1.55549854697581,
10.2178983363767));
#266881=CARTESIAN_POINT('Ctrl Pts',(-0.000565803094649467,1.55550432472794,
10.2176296255618));
#266882=CARTESIAN_POINT('Ctrl Pts',(0.0063264062122905,1.55549038708562,
10.2171319962261));
#266883=CARTESIAN_POINT('Ctrl Pts',(0.00950716715387924,1.5554741983836,
10.2169028926674));
#266884=CARTESIAN_POINT('Ctrl Pts',(0.0167505299542766,1.55541511352609,
10.216382407332));
#266885=CARTESIAN_POINT('Ctrl Pts',(0.0208130249869358,1.55536605808523,
10.2160913715708));
#266886=CARTESIAN_POINT('Ctrl Pts',(0.0313956299772142,1.55519680086801,
10.2153354262995));
#266887=CARTESIAN_POINT('Ctrl Pts',(0.0379153478087279,1.55505151212667,
10.2148718693102));
#266888=CARTESIAN_POINT('Ctrl Pts',(0.0814357238219479,1.55380781000222,
10.2117908264832));
#266889=CARTESIAN_POINT('Ctrl Pts',(0.118391615239711,1.55142981376781,
10.2092385955489));
#266890=CARTESIAN_POINT('Ctrl Pts',(0.170475679911314,1.54620601174728,
10.2056876716411));
#266891=CARTESIAN_POINT('Ctrl Pts',(0.185697370728413,1.54445184470954,
10.2046555155841));
#266892=CARTESIAN_POINT('Ctrl Pts',(0.284967029825184,1.53152300422074,
10.1979467662469));
#266893=CARTESIAN_POINT('Ctrl Pts',(0.368009970509466,1.51371688609786,
10.1924332151657));
#266894=CARTESIAN_POINT('Ctrl Pts',(0.532008489798817,1.46425065810727,
10.1811003020359));
#266895=CARTESIAN_POINT('Ctrl Pts',(0.612585794477345,1.43240995287475,
10.1752946060289));
#266896=CARTESIAN_POINT('Ctrl Pts',(0.701514956133872,1.38838736140621,
10.1683596751497));
#266897=CARTESIAN_POINT('Ctrl Pts',(0.712867299509692,1.38259281614573,
10.1674642650704));
#266898=CARTESIAN_POINT('Ctrl Pts',(0.730181209905368,1.37348539832301,
10.1660823603076));
#266899=CARTESIAN_POINT('Ctrl Pts',(0.736194532796881,1.37027163216065,
10.1655993549946));
#266900=CARTESIAN_POINT('Ctrl Pts',(0.74711453404063,1.36434290695812,10.1647165472003));
#266901=CARTESIAN_POINT('Ctrl Pts',(0.752028057056082,1.36164073625601,
10.1643172045436));
#266902=CARTESIAN_POINT('Ctrl Pts',(0.762721903149051,1.35568416349133,
10.1634433734562));
#266903=CARTESIAN_POINT('Ctrl Pts',(0.768496211061508,1.35241924851249,
10.1629685143291));
#266904=CARTESIAN_POINT('Ctrl Pts',(0.784275318510369,1.34336372614142,
10.1616624688343));
#266905=CARTESIAN_POINT('Ctrl Pts',(0.794236549870784,1.33749847303368,
10.1608286047823));
#266906=CARTESIAN_POINT('Ctrl Pts',(0.846365062252937,1.30601710256412,
10.1564142768577));
#266907=CARTESIAN_POINT('Ctrl Pts',(0.887356654970115,1.27851932294011,
10.1527655450247));
#266908=CARTESIAN_POINT('Ctrl Pts',(1.04415641814986,1.16215893118084,10.1380716838586));
#266909=CARTESIAN_POINT('Ctrl Pts',(1.14850263419929,1.05915434891066,10.1265218396409));
#266910=CARTESIAN_POINT('Ctrl Pts',(1.25605792605177,0.918090689412616,
10.1130899706047));
#266911=CARTESIAN_POINT('Ctrl Pts',(1.27438937254133,0.892470792256993,
10.110735788307));
#266912=CARTESIAN_POINT('Ctrl Pts',(1.29559167976259,0.860851691204771,
10.1079473233843));
#266913=CARTESIAN_POINT('Ctrl Pts',(1.29921704342593,0.855370395282219,
10.1074680623674));
#266914=CARTESIAN_POINT('Ctrl Pts',(1.30482042377313,0.846780658309995,
10.1067236318135));
#266915=CARTESIAN_POINT('Ctrl Pts',(1.30682226218573,0.843687973960617,
10.1064569312944));
#266916=CARTESIAN_POINT('Ctrl Pts',(1.31053389849359,0.837908879611088,
10.1059610772914));
#266917=CARTESIAN_POINT('Ctrl Pts',(1.31224641838309,0.835224357510852,
10.1057317510052));
#266918=CARTESIAN_POINT('Ctrl Pts',(1.31614624573452,0.829069440312904,
10.1052082472807));
#266919=CARTESIAN_POINT('Ctrl Pts',(1.31832807651357,0.825595639971596,
10.1049144319132));
#266920=CARTESIAN_POINT('Ctrl Pts',(1.32401197095684,0.816466044553289,
10.1041464410459));
#266921=CARTESIAN_POINT('Ctrl Pts',(1.32749159018408,0.810796264991437,
10.1036736895829));
#266922=CARTESIAN_POINT('Ctrl Pts',(1.3514498300759,0.771190391188492,10.1003991098142));
#266923=CARTESIAN_POINT('Ctrl Pts',(1.37066332679176,0.736501170227816,
10.0976721869515));
#266924=CARTESIAN_POINT('Ctrl Pts',(1.40506730893587,0.668365085578623,
10.0925072917869));
#266925=CARTESIAN_POINT('Ctrl Pts',(1.4204227431959,0.635074885627405,10.0900670882858));
#266926=CARTESIAN_POINT('Ctrl Pts',(1.43457678342482,0.601306662576177,
10.0876445460468));
#266927=CARTESIAN_POINT('Ctrl Pts',(1.4345766815454,0.601306905636539,9.94872080685755));
#266928=CARTESIAN_POINT('Ctrl Pts',(1.39464986035857,0.69656289905012,9.95624305992229));
#266929=CARTESIAN_POINT('Ctrl Pts',(1.34534036199748,0.787592841149577,
9.96409078293215));
#266930=CARTESIAN_POINT('Ctrl Pts',(1.24095222318489,0.941520643270294,
9.97847524407404));
#266931=CARTESIAN_POINT('Ctrl Pts',(1.18913275716379,1.00617482597473,9.98493228383878));
#266932=CARTESIAN_POINT('Ctrl Pts',(1.10881976201145,1.09145938142171,9.99382504031493));
#266933=CARTESIAN_POINT('Ctrl Pts',(1.08439638207577,1.11572836726689,9.99640352829429));
#266934=CARTESIAN_POINT('Ctrl Pts',(1.05420923550547,1.14379600889694,9.99942416676281));
#266935=CARTESIAN_POINT('Ctrl Pts',(1.04920252577313,1.14839038948299,9.99991990651836));
#266936=CARTESIAN_POINT('Ctrl Pts',(1.04137798931262,1.1554766458844,10.000686325941));
#266937=CARTESIAN_POINT('Ctrl Pts',(1.0385810432954,1.15799128370229,10.0009586565537));
#266938=CARTESIAN_POINT('Ctrl Pts',(1.03337140330718,1.1626410331687,10.001462838238));
#266939=CARTESIAN_POINT('Ctrl Pts',(1.03096121709802,1.16477877657822,10.0016948797116));
#266940=CARTESIAN_POINT('Ctrl Pts',(1.02545687238681,1.16963045067171,10.002222078051));
#266941=CARTESIAN_POINT('Ctrl Pts',(1.02235857535066,1.17233959786527,10.002516880071));
#266942=CARTESIAN_POINT('Ctrl Pts',(1.01425702404123,1.17936704129483,10.0032827945205));
#266943=CARTESIAN_POINT('Ctrl Pts',(1.00923686757152,1.18366586423359,10.0037525192117));
#266944=CARTESIAN_POINT('Ctrl Pts',(0.975374681281018,1.2122904217217,10.0068896041933));
#266945=CARTESIAN_POINT('Ctrl Pts',(0.945680309356813,1.23559425786066,
10.0094893116133));
#266946=CARTESIAN_POINT('Ctrl Pts',(0.794622396906456,1.34550297979804,
10.0221527296009));
#266947=CARTESIAN_POINT('Ctrl Pts',(0.662096285572017,1.41542856750007,
10.0316152363526));
#266948=CARTESIAN_POINT('Ctrl Pts',(0.496438246775405,1.4743963622761,10.0435614534246));
#266949=CARTESIAN_POINT('Ctrl Pts',(0.471015719440541,1.48271360126234,
10.0453951352197));
#266950=CARTESIAN_POINT('Ctrl Pts',(0.42697878363117,1.49587389772509,10.0485813922596));
#266951=CARTESIAN_POINT('Ctrl Pts',(0.40846533711961,1.50103484675055,10.0499238569104));
#266952=CARTESIAN_POINT('Ctrl Pts',(0.382025576382251,1.50788004494536,
10.0518474689537));
#266953=CARTESIAN_POINT('Ctrl Pts',(0.374173856007484,1.50984757243412,
10.0524195059916));
#266954=CARTESIAN_POINT('Ctrl Pts',(0.360593369946202,1.51313820818275,
10.0534104394129));
#266955=CARTESIAN_POINT('Ctrl Pts',(0.354871740668333,1.51449029757679,
10.053828397696));
#266956=CARTESIAN_POINT('Ctrl Pts',(0.343889769620078,1.51701981959872,
10.0546315728696));
#266957=CARTESIAN_POINT('Ctrl Pts',(0.338630692480567,1.5182024105722,10.0550166179476));
#266958=CARTESIAN_POINT('Ctrl Pts',(0.326254977275459,1.52091779375944,
10.0559237465952));
#266959=CARTESIAN_POINT('Ctrl Pts',(0.319133568784506,1.5224279974781,10.0564465430711));
#266960=CARTESIAN_POINT('Ctrl Pts',(0.294442935494892,1.52748317517575,
10.0582620827262));
#266961=CARTESIAN_POINT('Ctrl Pts',(0.27682382777396,1.53077431752977,10.0595628245813));
#266962=CARTESIAN_POINT('Ctrl Pts',(0.135762045252824,1.55460888277475,
10.0700223573381));
#266963=CARTESIAN_POINT('Ctrl Pts',(0.0103314187981903,1.56048720632894,
10.0796562924481));
#266964=CARTESIAN_POINT('Ctrl Pts',(-0.199081856613034,1.54504168485567,
10.0959385487793));
#266965=CARTESIAN_POINT('Ctrl Pts',(-0.283103949734268,1.53187565082544,
10.1025091855824));
#266966=CARTESIAN_POINT('Ctrl Pts',(-0.37579258792469,1.50945993185414,
10.1095478713378));
#266967=CARTESIAN_POINT('Ctrl Pts',(-0.385920630206807,1.5069023319547,
10.1103139882301));
#266968=CARTESIAN_POINT('Ctrl Pts',(-0.400347308653118,1.50310421555012,
10.1114002492365));
#266969=CARTESIAN_POINT('Ctrl Pts',(-0.404667258260174,1.50194695704885,
10.1117248752355));
#266970=CARTESIAN_POINT('Ctrl Pts',(-0.41213379310469,1.49991221628383,
10.1122847645362));
#266971=CARTESIAN_POINT('Ctrl Pts',(-0.415282691695335,1.49904343059812,
10.1125205210313));
#266972=CARTESIAN_POINT('Ctrl Pts',(-0.4218602752194,1.49720634880885,10.1130121861267));
#266973=CARTESIAN_POINT('Ctrl Pts',(-0.425288384545355,1.49623618903792,
10.1132679854305));
#266974=CARTESIAN_POINT('Ctrl Pts',(-0.434378993801736,1.49362976676146,
10.113945197932));
#266975=CARTESIAN_POINT('Ctrl Pts',(-0.440035653118906,1.49197306188208,
10.1143654474963));
#266976=CARTESIAN_POINT('Ctrl Pts',(-0.464284288950538,1.48472128950693,
10.1161625644793));
#266977=CARTESIAN_POINT('Ctrl Pts',(-0.482781057108053,1.47881024862455,
10.1175223045462));
#266978=CARTESIAN_POINT('Ctrl Pts',(-0.659262807854901,1.41874712619837,
10.1304328637531));
#266979=CARTESIAN_POINT('Ctrl Pts',(-0.807683273884122,1.33982672490135,
10.1409098876283));
#266980=CARTESIAN_POINT('Ctrl Pts',(-0.975089262784055,1.21270068574397,
10.1551607716187));
#266981=CARTESIAN_POINT('Ctrl Pts',(-1.00834877594978,1.18518951783725,
10.1581282441116));
#266982=CARTESIAN_POINT('Ctrl Pts',(-1.04848212539614,1.14907924611275,
10.1619120696735));
#266983=CARTESIAN_POINT('Ctrl Pts',(-1.05646843059558,1.14174091882177,
10.1626756186984));
#266984=CARTESIAN_POINT('Ctrl Pts',(-1.06908762047572,1.12989983385748,
10.163899560269));
#266985=CARTESIAN_POINT('Ctrl Pts',(-1.07377042997215,1.12545059253557,
10.1643576663117));
#266986=CARTESIAN_POINT('Ctrl Pts',(-1.08257609821553,1.11697914766503,
10.1652266424887));
#266987=CARTESIAN_POINT('Ctrl Pts',(-1.08670460509117,1.11296294834169,
10.1656372481826));
#266988=CARTESIAN_POINT('Ctrl Pts',(-1.09600481999391,1.10381464429617,
10.1665695414669));
#266989=CARTESIAN_POINT('Ctrl Pts',(-1.10116293399881,1.09866897828989,
10.1670918194007));
#266990=CARTESIAN_POINT('Ctrl Pts',(-1.11437253156175,1.08530478638757,
10.1684429966065));
#266991=CARTESIAN_POINT('Ctrl Pts',(-1.12236919622339,1.07703295799389,
10.1692742567673));
#266992=CARTESIAN_POINT('Ctrl Pts',(-1.17646575132327,1.01981820408645,
10.1749908441597));
#266993=CARTESIAN_POINT('Ctrl Pts',(-1.2194351671807,0.968026999758387,
10.1800068724847));
#266994=CARTESIAN_POINT('Ctrl Pts',(-1.32794770583136,0.818504006184004,
10.194075021361));
#266995=CARTESIAN_POINT('Ctrl Pts',(-1.38597089553815,0.715874001236015,
10.2033193996353));
#266996=CARTESIAN_POINT('Ctrl Pts',(-1.44716184615487,0.571692611803612,
10.2152526904509));
#266997=CARTESIAN_POINT('Ctrl Pts',(-1.46107960670724,0.535123235047128,
10.2181923652023));
#266998=CARTESIAN_POINT('Ctrl Pts',(-1.4758551218457,0.491407455262296,
10.221575743023));
#266999=CARTESIAN_POINT('Ctrl Pts',(-1.4780600378127,0.484735141500817,
10.2220886071838));
#267000=CARTESIAN_POINT('Ctrl Pts',(-1.48139096232781,0.474421322198345,
10.2228756865157));
#267001=CARTESIAN_POINT('Ctrl Pts',(-1.48254889270473,0.470790352289202,
10.2231516948238));
#267002=CARTESIAN_POINT('Ctrl Pts',(-1.48465965686182,0.464086525332085,
10.223659246459));
#267003=CARTESIAN_POINT('Ctrl Pts',(-1.4856162972954,0.461014986000578,
10.223891002545));
#267004=CARTESIAN_POINT('Ctrl Pts',(-1.4877556515077,0.454070227034208,
10.2244132315157));
#267005=CARTESIAN_POINT('Ctrl Pts',(-1.48893277188251,0.450195348143785,
10.2247033768899));
#267006=CARTESIAN_POINT('Ctrl Pts',(-1.49236601180917,0.438732943758511,
10.225558140743));
#267007=CARTESIAN_POINT('Ctrl Pts',(-1.49457940735182,0.431132591298094,
10.2261203551612));
#267008=CARTESIAN_POINT('Ctrl Pts',(-1.51187526292265,0.370007767337685,
10.230607945371));
#267009=CARTESIAN_POINT('Ctrl Pts',(-1.52413761827353,0.315719351150575,
10.2343858584892));
#267010=CARTESIAN_POINT('Ctrl Pts',(-1.54805757830584,0.17511873879064,
10.2439157176547));
#267011=CARTESIAN_POINT('Ctrl Pts',(-1.55542813893534,0.0882786190245136,
10.2495683327449));
#267012=CARTESIAN_POINT('Ctrl Pts',(-1.55556419254695,-0.0776507360197793,
10.2605745051194));
#267013=CARTESIAN_POINT('Ctrl Pts',(-1.54962198720566,-0.156456241130258,
10.2658907513526));
#267014=CARTESIAN_POINT('Ctrl Pts',(-1.53594203793849,-0.24617611525238,
10.2722300465037));
#267015=CARTESIAN_POINT('Ctrl Pts',(-1.53402245979568,-0.257867607231571,
10.2730616198341));
#267016=CARTESIAN_POINT('Ctrl Pts',(-1.5306891459699,-0.27681327682575,
10.2744186468661));
#267017=CARTESIAN_POINT('Ctrl Pts',(-1.5293569129153,-0.284081469541231,
10.2749415250497));
#267018=CARTESIAN_POINT('Ctrl Pts',(-1.5268920309354,-0.297008893991048,
10.2758757213272));
#267019=CARTESIAN_POINT('Ctrl Pts',(-1.52577956852232,-0.302671874943031,
10.2762863916489));
#267020=CARTESIAN_POINT('Ctrl Pts',(-1.52336703235503,-0.314601485802336,
10.2771546063657));
#267021=CARTESIAN_POINT('Ctrl Pts',(-1.52205974849696,-0.320866529698587,
10.2776123734426));
#267022=CARTESIAN_POINT('Ctrl Pts',(-1.51848974320291,-0.337462588368844,
10.2788298992047));
#267023=CARTESIAN_POINT('Ctrl Pts',(-1.51616029397407,-0.347778739252849,
10.2795917734682));
#267024=CARTESIAN_POINT('Ctrl Pts',(-1.50455085403857,-0.396857144931691,
10.2832411836649));
#267025=CARTESIAN_POINT('Ctrl Pts',(-1.49388928610356,-0.435273628260907,
10.2861725227912));
#267026=CARTESIAN_POINT('Ctrl Pts',(-1.43628524530431,-0.615639856941075,
10.3003079185256));
#267027=CARTESIAN_POINT('Ctrl Pts',(-1.37051371152964,-0.750736944814589,
10.3121144984721));
#267028=CARTESIAN_POINT('Ctrl Pts',(-1.26511427957333,-0.905822977656985,
10.326395921319));
#267029=CARTESIAN_POINT('Ctrl Pts',(-1.24256571103544,-0.936515057905393,
10.3292569511393));
#267030=CARTESIAN_POINT('Ctrl Pts',(-1.21479543134976,-0.971543207076164,
10.3325367658213));
#267031=CARTESIAN_POINT('Ctrl Pts',(-1.21064631460267,-0.976708579031646,
10.3330207980656));
#267032=CARTESIAN_POINT('Ctrl Pts',(-1.20386332971184,-0.985043304530043,
10.3338022278515));
#267033=CARTESIAN_POINT('Ctrl Pts',(-1.20124970628607,-0.988228907001057,
10.3341009943053));
#267034=CARTESIAN_POINT('Ctrl Pts',(-1.19656983841324,-0.993886941911346,
10.3346317588914));
#267035=CARTESIAN_POINT('Ctrl Pts',(-1.19450854590318,-0.996363370448372,
10.3348641029391));
#267036=CARTESIAN_POINT('Ctrl Pts',(-1.19002663866141,-1.00171401551384,
10.3353661853621));
#267037=CARTESIAN_POINT('Ctrl Pts',(-1.18760330229603,-1.00458586829852,
10.3356357213107));
#267038=CARTESIAN_POINT('Ctrl Pts',(-1.18077904500518,-1.01261396928665,
10.3363894368417));
#267039=CARTESIAN_POINT('Ctrl Pts',(-1.17635471753991,-1.01775035589376,
10.3368719478006));
#267040=CARTESIAN_POINT('Ctrl Pts',(-1.14945929176624,-1.04856467363213,
10.339769538717));
#267041=CARTESIAN_POINT('Ctrl Pts',(-1.12617976056278,-1.07352882189692,
10.3421293104767));
#267042=CARTESIAN_POINT('Ctrl Pts',(-1.01426798997064,-1.18588779344111,
10.3529242729752));
#267043=CARTESIAN_POINT('Ctrl Pts',(-0.916169471450868,-1.26321352010279,
10.3609004667231));
#267044=CARTESIAN_POINT('Ctrl Pts',(-0.753694414430256,-1.36229888817716,
10.3736025517594));
#267045=CARTESIAN_POINT('Ctrl Pts',(-0.695381370771949,-1.39296680347772,
10.3780688738453));
#267046=CARTESIAN_POINT('Ctrl Pts',(-0.62485110076814,-1.42452537981127,
10.3834693352067));
#267047=CARTESIAN_POINT('Ctrl Pts',(-0.614344416196805,-1.42908795454396,
10.3842736644787));
#267048=CARTESIAN_POINT('Ctrl Pts',(-0.5970880679109,-1.43635613624648,
10.3855949479659));
#267049=CARTESIAN_POINT('Ctrl Pts',(-0.590367993864654,-1.43913124472895,
10.3861095483177));
#267050=CARTESIAN_POINT('Ctrl Pts',(-0.578291311789725,-1.44401958620469,
10.3870345659502));
#267051=CARTESIAN_POINT('Ctrl Pts',(-0.572941921310816,-1.44615039321894,
10.3874443832714));
#267052=CARTESIAN_POINT('Ctrl Pts',(-0.561558082033392,-1.45061180751835,
10.3883167324587));
#267053=CARTESIAN_POINT('Ctrl Pts',(-0.555520695701756,-1.45293456491392,
10.3887795181124));
#267054=CARTESIAN_POINT('Ctrl Pts',(-0.539282774045474,-1.4590657605718,
10.3900246812528));
#267055=CARTESIAN_POINT('Ctrl Pts',(-0.529056612271184,-1.46280480374804,
10.390809348187));
#267056=CARTESIAN_POINT('Ctrl Pts',(-0.477599061166027,-1.48100933389709,
10.3947610178785));
#267057=CARTESIAN_POINT('Ctrl Pts',(-0.435814267012427,-1.49383892505317,
10.3979811324152));
#267058=CARTESIAN_POINT('Ctrl Pts',(-0.243126762961555,-1.54422918050073,
10.4128964566057));
#267059=CARTESIAN_POINT('Ctrl Pts',(-0.0876918707412931,-1.56078535366454,
10.4252253702649));
#267060=CARTESIAN_POINT('Ctrl Pts',(0.0962735123591064,-1.55278314926884,
10.4391392515311));
#267061=CARTESIAN_POINT('Ctrl Pts',(0.12491161146944,-1.55074223002995,
10.4412817634017));
#267062=CARTESIAN_POINT('Ctrl Pts',(0.160127205521839,-1.54725051619652,
10.443874865253));
#267063=CARTESIAN_POINT('Ctrl Pts',(0.166771157396114,-1.5465485014074,
10.4443622614655));
#267064=CARTESIAN_POINT('Ctrl Pts',(0.177163521042644,-1.54538267071173,
10.4451215594705));
#267065=CARTESIAN_POINT('Ctrl Pts',(0.180915011287092,-1.54494798347355,
10.4453950257974));
#267066=CARTESIAN_POINT('Ctrl Pts',(0.187831694722515,-1.54412100438494,
10.4458980139329));
#267067=CARTESIAN_POINT('Ctrl Pts',(0.190997241653555,-1.54373264387433,
10.4461277440395));
#267068=CARTESIAN_POINT('Ctrl Pts',(0.198208031392311,-1.5428254789474,
10.4466499887457));
#267069=CARTESIAN_POINT('Ctrl Pts',(0.202252439393425,-1.54230050054513,
10.4469421537296));
#267070=CARTESIAN_POINT('Ctrl Pts',(0.214541910562755,-1.5406561106215,
10.4478277748135));
#267071=CARTESIAN_POINT('Ctrl Pts',(0.222780278108291,-1.53948642033404,
10.4484184994134));
#267072=CARTESIAN_POINT('Ctrl Pts',(0.241832981866239,-1.53662515190068,
10.4497786336488));
#267073=CARTESIAN_POINT('Ctrl Pts',(0.252639776186028,-1.53488540567801,
10.4505456036878));
#267074=CARTESIAN_POINT('Ctrl Pts',(0.289599371700655,-1.52853447342525,
10.4531560259521));
#267075=CARTESIAN_POINT('Ctrl Pts',(0.315653347597125,-1.5233675132306,
10.4549744646969));
#267076=CARTESIAN_POINT('Ctrl Pts',(0.460004865183639,-1.4908771634028,
10.4649923779096));
#267077=CARTESIAN_POINT('Ctrl Pts',(0.574923432398753,-1.45044352010272,
10.4727832366868));
#267078=CARTESIAN_POINT('Ctrl Pts',(0.740669605465649,-1.36929664955656,
10.4851193269967));
#267079=CARTESIAN_POINT('Ctrl Pts',(0.795613979223518,-1.33811867507471,
10.4894085406645));
#267080=CARTESIAN_POINT('Ctrl Pts',(0.858024250161843,-1.29749896124582,
10.4946138461831));
#267081=CARTESIAN_POINT('Ctrl Pts',(0.867472098024921,-1.29120150071172,
10.4954112278284));
#267082=CARTESIAN_POINT('Ctrl Pts',(0.882830063440128,-1.28072001155749,
10.4967233850599));
#267083=CARTESIAN_POINT('Ctrl Pts',(0.888781523963574,-1.27659706578813,
10.4972358618758));
#267084=CARTESIAN_POINT('Ctrl Pts',(0.899411747484894,-1.26912248441489,
10.4981585496682));
#267085=CARTESIAN_POINT('Ctrl Pts',(0.904101133471117,-1.26578612363553,
10.4985681729351));
#267086=CARTESIAN_POINT('Ctrl Pts',(0.914037243739115,-1.25863348852336,
10.4994417027001));
#267087=CARTESIAN_POINT('Ctrl Pts',(0.91927880801342,-1.25481026938627,
10.4999058714044));
#267088=CARTESIAN_POINT('Ctrl Pts',(0.933322070853899,-1.2444318388997,
10.5011586626093));
#267089=CARTESIAN_POINT('Ctrl Pts',(0.942078421389058,-1.23781619237101,
10.5019496235394));
#267090=CARTESIAN_POINT('Ctrl Pts',(0.986245343153725,-1.20370684429341,
10.5059902994799));
#267091=CARTESIAN_POINT('Ctrl Pts',(1.02052198049525,-1.17478686388855,
10.5092960539549));
#267092=CARTESIAN_POINT('Ctrl Pts',(1.11804221155345,-1.08501510988762,
10.5192312920522));
#267093=CARTESIAN_POINT('Ctrl Pts',(1.177435889796,-1.02025356956725,10.5260058840845));
#267094=CARTESIAN_POINT('Ctrl Pts',(1.28372048158515,-0.882647553728048,
10.5394891339913));
#267095=CARTESIAN_POINT('Ctrl Pts',(1.33064071179853,-0.810187338955744,
10.546171884293));
#267096=CARTESIAN_POINT('Ctrl Pts',(1.37715836679279,-0.723303554000018,
10.5534721554879));
#267097=CARTESIAN_POINT('Ctrl Pts',(1.38286579716953,-0.712330970263795,
10.5543816914596));
#267098=CARTESIAN_POINT('Ctrl Pts',(1.39066398095201,-0.696891836828856,
10.5556430317168));
#267099=CARTESIAN_POINT('Ctrl Pts',(1.39286509832849,-0.692482028503425,
10.5560012217619));
#267100=CARTESIAN_POINT('Ctrl Pts',(1.396380326652,-0.685354902790822,10.5565766932149));
#267101=CARTESIAN_POINT('Ctrl Pts',(1.39770752877413,-0.682644141463641,
10.5567947735125));
#267102=CARTESIAN_POINT('Ctrl Pts',(1.40048735842366,-0.676924348019211,
10.5572532265455));
#267103=CARTESIAN_POINT('Ctrl Pts',(1.40193819492123,-0.67391446940491,
10.5574934829998));
#267104=CARTESIAN_POINT('Ctrl Pts',(1.40548303788341,-0.666499414962702,
10.5580829940322));
#267105=CARTESIAN_POINT('Ctrl Pts',(1.40756606884171,-0.662088969467931,
10.5584315761637));
#267106=CARTESIAN_POINT('Ctrl Pts',(1.41511845772876,-0.645901394737934,
10.5597037222602));
#267107=CARTESIAN_POINT('Ctrl Pts',(1.4204612351256,-0.634065272658606,
10.5606199016087));
#267108=CARTESIAN_POINT('Ctrl Pts',(1.45525352133037,-0.554340504707602,
10.5667070284646));
#267109=CARTESIAN_POINT('Ctrl Pts',(1.47997839663625,-0.484482380529914,
10.5716382115629));
#267110=CARTESIAN_POINT('Ctrl Pts',(1.53515835677589,-0.284177835200355,
10.585359342164));
#267111=CARTESIAN_POINT('Ctrl Pts',(1.55389819801128,-0.151209515050148,
10.5940427568767));
#267112=CARTESIAN_POINT('Ctrl Pts',(1.55559805582344,-2.31852926990466E-5,
10.6045457699659));
#267113=CARTESIAN_POINT('Ctrl Pts',(1.55550024276892,0.0174431545606266,
10.6057675448385));
#267114=CARTESIAN_POINT('Ctrl Pts',(1.55495098829591,0.0419148854556453,
10.6074927050732));
#267115=CARTESIAN_POINT('Ctrl Pts',(1.55474621004683,0.0489249739294903,
10.6079884228675));
#267116=CARTESIAN_POINT('Ctrl Pts',(1.55428335251448,0.0617886671499064,
10.6089010100376));
#267117=CARTESIAN_POINT('Ctrl Pts',(1.55403958909289,0.0676426870412161,
10.6093174262123));
#267118=CARTESIAN_POINT('Ctrl Pts',(1.5534772801245,0.0795304799023775,
10.6101653781285));
#267119=CARTESIAN_POINT('Ctrl Pts',(1.55315664017382,0.0855640478401656,
10.6105969722121));
#267120=CARTESIAN_POINT('Ctrl Pts',(1.55227524764469,0.100506122771638,
10.6116689196459));
#267121=CARTESIAN_POINT('Ctrl Pts',(1.55167295628279,0.109411862899771,
10.6123105597758));
#267122=CARTESIAN_POINT('Ctrl Pts',(1.54911539442991,0.142939919334832,
10.6147368559119));
#267123=CARTESIAN_POINT('Ctrl Pts',(1.54665049890624,0.167518447209745,
10.6165372874127));
#267124=CARTESIAN_POINT('Ctrl Pts',(1.53899818124486,0.229031430577571,
10.6211009962873));
#267125=CARTESIAN_POINT('Ctrl Pts',(1.53306591292877,0.265855777746757,
10.6238858928683));
#267126=CARTESIAN_POINT('Ctrl Pts',(1.50548810790567,0.404991580091826,
10.634608373832));
#267127=CARTESIAN_POINT('Ctrl Pts',(1.47489605884916,0.505114366182903,
10.6427635453334));
#267128=CARTESIAN_POINT('Ctrl Pts',(1.43457668061803,0.601306907849032,
10.6508134549194));
#267129=CARTESIAN_POINT('Origin',(0.,0.,-1.29405622560371));
#267130=CARTESIAN_POINT('',(1.4345766883817,0.601306889326732,11.4896545509914));
#267131=CARTESIAN_POINT('',(1.43457668357355,0.601306900797848,11.3502242497076));
#267132=CARTESIAN_POINT('',(1.43457668357355,0.601306900797845,-1.29405622560371));
#267133=CARTESIAN_POINT('Ctrl Pts',(1.4345766883817,0.601306889326732,11.4896545509914));
#267134=CARTESIAN_POINT('Ctrl Pts',(1.44407323673688,0.578650360468923,
11.4878458824711));
#267135=CARTESIAN_POINT('Ctrl Pts',(1.45303230308892,0.555770666562326,
11.486019839339));
#267136=CARTESIAN_POINT('Ctrl Pts',(1.51303881084614,0.391140569784664,
11.4728827943302));
#267137=CARTESIAN_POINT('Ctrl Pts',(1.54378555080634,0.242881238893851,
11.4609546076149));
#267138=CARTESIAN_POINT('Ctrl Pts',(1.55466567521783,0.06030784464822,11.4470960617881));
#267139=CARTESIAN_POINT('Ctrl Pts',(1.55558260286277,0.0280276449396798,
11.4446814329925));
#267140=CARTESIAN_POINT('Ctrl Pts',(1.55547603854558,-0.0108784739935134,
11.4418313869187));
#267141=CARTESIAN_POINT('Ctrl Pts',(1.55541567678721,-0.0174964084788573,
11.4413486978236));
#267142=CARTESIAN_POINT('Ctrl Pts',(1.55525581052292,-0.0278075546564512,
11.4406001214563));
#267143=CARTESIAN_POINT('Ctrl Pts',(1.55518538509407,-0.0315010321067899,
11.4403326760263));
#267144=CARTESIAN_POINT('Ctrl Pts',(1.5550297856546,-0.0383763822669787,
11.4398361700344));
#267145=CARTESIAN_POINT('Ctrl Pts',(1.55494800430072,-0.0415582149089613,
11.4396069321225));
#267146=CARTESIAN_POINT('Ctrl Pts',(1.55473889694584,-0.048825377876731,
11.4390845733081));
#267147=CARTESIAN_POINT('Ctrl Pts',(1.55460523553539,-0.0529104704047821,
11.4387918084128));
#267148=CARTESIAN_POINT('Ctrl Pts',(1.55421354852023,-0.0635931526224319,
11.4380283766596));
#267149=CARTESIAN_POINT('Ctrl Pts',(1.553929612088,-0.0701898015677843,
11.4375591065679));
#267150=CARTESIAN_POINT('Ctrl Pts',(1.55169503418187,-0.115402625114617,
11.4343563135564));
#267151=CARTESIAN_POINT('Ctrl Pts',(1.54834695455523,-0.153940172523269,
11.4316940468738));
#267152=CARTESIAN_POINT('Ctrl Pts',(1.54228604730357,-0.202586017920447,
11.4283738711653));
#267153=CARTESIAN_POINT('Ctrl Pts',(1.54090408958628,-0.212842526626525,
11.4276761426403));
#267154=CARTESIAN_POINT('Ctrl Pts',(1.52547690141245,-0.319299504718612,
11.4204510722172));
#267155=CARTESIAN_POINT('Ctrl Pts',(1.50254410758542,-0.413998741802044,
11.414155311747));
#267156=CARTESIAN_POINT('Ctrl Pts',(1.45408005578147,-0.5548980010043,11.4042634206064));
#267157=CARTESIAN_POINT('Ctrl Pts',(1.43480839838853,-0.602979879718134,
11.4007904142757));
#267158=CARTESIAN_POINT('Ctrl Pts',(1.40015443874943,-0.678320687071308,
11.3951106087149));
#267159=CARTESIAN_POINT('Ctrl Pts',(1.38628492506799,-0.70623316468095,
11.3929516612066));
#267160=CARTESIAN_POINT('Ctrl Pts',(1.36703561190124,-0.742217626532354,
11.3900859592445));
#267161=CARTESIAN_POINT('Ctrl Pts',(1.3624049246891,-0.750683810293062,
11.3894056237435));
#267162=CARTESIAN_POINT('Ctrl Pts',(1.3546969688877,-0.764469838849435,
11.3882874544315));
#267163=CARTESIAN_POINT('Ctrl Pts',(1.35166636366483,-0.769815595703467,
11.3878512924443));
#267164=CARTESIAN_POINT('Ctrl Pts',(1.34573863050125,-0.780128743001058,
11.3870047651151));
#267165=CARTESIAN_POINT('Ctrl Pts',(1.34284547149433,-0.785098309342846,
11.3865945480933));
#267166=CARTESIAN_POINT('Ctrl Pts',(1.33609636553207,-0.796544769529156,
11.3856442839464));
#267167=CARTESIAN_POINT('Ctrl Pts',(1.33222078942502,-0.803009858200643,
11.3851035304211));
#267168=CARTESIAN_POINT('Ctrl Pts',(1.31953794558891,-0.823822355829706,
11.3833494461501));
#267169=CARTESIAN_POINT('Ctrl Pts',(1.31054498122841,-0.838054577330154,
11.3821293506623));
#267170=CARTESIAN_POINT('Ctrl Pts',(1.22533847775522,-0.968175817688255,
11.3707777778507));
#267171=CARTESIAN_POINT('Ctrl Pts',(1.13418955789108,-1.07350607508223,
11.360044561091));
#267172=CARTESIAN_POINT('Ctrl Pts',(0.977386715594308,-1.2121421210387,
11.3438318809266));
#267173=CARTESIAN_POINT('Ctrl Pts',(0.921314794587914,-1.25529067441546,
11.3383918477702));
#267174=CARTESIAN_POINT('Ctrl Pts',(0.851974596277352,-1.30149122473887,
11.332219528681));
#267175=CARTESIAN_POINT('Ctrl Pts',(0.84136676225202,-1.30837384554578,
11.3312897537226));
#267176=CARTESIAN_POINT('Ctrl Pts',(0.826625549404747,-1.31768486352746,
11.3300187403291));
#267177=CARTESIAN_POINT('Ctrl Pts',(0.822563496881006,-1.32022441037192,
11.3296706774395));
#267178=CARTESIAN_POINT('Ctrl Pts',(0.815688511890171,-1.324478521029,11.3290853278683));
#267179=CARTESIAN_POINT('Ctrl Pts',(0.812881774171896,-1.32620297204218,
11.3288474027228));
#267180=CARTESIAN_POINT('Ctrl Pts',(0.807522383677627,-1.32947235857583,
11.3283951108807));
#267181=CARTESIAN_POINT('Ctrl Pts',(0.804970742262437,-1.33101887923143,
11.3281806376976));
#267182=CARTESIAN_POINT('Ctrl Pts',(0.798229972451977,-1.3350779086275,
11.3276162913125));
#267183=CARTESIAN_POINT('Ctrl Pts',(0.794033385276217,-1.33757807092635,
11.3272672155987));
#267184=CARTESIAN_POINT('Ctrl Pts',(0.779216501427361,-1.34631108204241,
11.3260424403143));
#267185=CARTESIAN_POINT('Ctrl Pts',(0.768533674299746,-1.35243776283375,
11.3251732579917));
#267186=CARTESIAN_POINT('Ctrl Pts',(0.688036343535112,-1.3973416933008,
11.3187180951702));
#267187=CARTESIAN_POINT('Ctrl Pts',(0.615390781887192,-1.43082343273482,
11.3134156047808));
#267188=CARTESIAN_POINT('Ctrl Pts',(0.478582600796601,-1.48151849855804,
11.303794292087));
#267189=CARTESIAN_POINT('Ctrl Pts',(0.415283885472396,-1.50049238901889,
11.2994743813456));
#267190=CARTESIAN_POINT('Ctrl Pts',(0.288246899694262,-1.52991485862425,
11.2907889679189));
#267191=CARTESIAN_POINT('Ctrl Pts',(0.224687530253573,-1.54053227175699,
11.2864356435291));
#267192=CARTESIAN_POINT('Ctrl Pts',(0.144549789380137,-1.54885373694145,
11.2808302074974));
#267193=CARTESIAN_POINT('Ctrl Pts',(0.128416443673834,-1.5502747248807,
11.2796960868988));
#267194=CARTESIAN_POINT('Ctrl Pts',(0.104781346789404,-1.55198498967307,
11.2780250636582));
#267195=CARTESIAN_POINT('Ctrl Pts',(0.0972946267128872,-1.55247231565039,
11.2774943484672));
#267196=CARTESIAN_POINT('Ctrl Pts',(0.0840890679635162,-1.5532359953968,
11.2765556426064));
#267197=CARTESIAN_POINT('Ctrl Pts',(0.0783716345593125,-1.55353497354903,
11.2761483667232));
#267198=CARTESIAN_POINT('Ctrl Pts',(0.0672061926329519,-1.55405704770376,
11.2753512752644));
#267199=CARTESIAN_POINT('Ctrl Pts',(0.061758398629359,-1.55428307545546,
11.2749615574745));
#267200=CARTESIAN_POINT('Ctrl Pts',(0.0470666366396885,-1.55481527071458,
11.2739083236134));
#267201=CARTESIAN_POINT('Ctrl Pts',(0.0378210685758777,-1.55506763654793,
11.2732431377116));
#267202=CARTESIAN_POINT('Ctrl Pts',(0.0031911707828243,-1.55570388282549,
11.27074234781));
#267203=CARTESIAN_POINT('Ctrl Pts',(-0.0221977743906398,-1.55554873675841,
11.2688901144894));
#267204=CARTESIAN_POINT('Ctrl Pts',(-0.0507959154971018,-1.55467374063616,
11.2667812032219));
#267205=CARTESIAN_POINT('Ctrl Pts',(-0.0540212744564434,-1.55456500876575,
11.2665430336903));
#267206=CARTESIAN_POINT('Ctrl Pts',(-0.0629986478676237,-1.55423439523362,
11.2658792194824));
#267207=CARTESIAN_POINT('Ctrl Pts',(-0.0687497559886824,-1.55399062237622,
11.2654529363581));
#267208=CARTESIAN_POINT('Ctrl Pts',(-0.212927542232475,-1.5470774200656,
11.2547402956532));
#267209=CARTESIAN_POINT('Ctrl Pts',(-0.349831848842385,-1.52196936592823,
11.2438857029329));
#267210=CARTESIAN_POINT('Ctrl Pts',(-0.518444971914157,-1.46707173483673,
11.2302353683261));
#267211=CARTESIAN_POINT('Ctrl Pts',(-0.554867063694058,-1.45368760783786,
11.2272747462962));
#267212=CARTESIAN_POINT('Ctrl Pts',(-0.60380164124047,-1.43359784706473,
11.2233113733096));
#267213=CARTESIAN_POINT('Ctrl Pts',(-0.616777190795279,-1.42806342294545,
11.2222618923797));
#267214=CARTESIAN_POINT('Ctrl Pts',(-0.638925015790562,-1.41825857281392,
11.2204751350318));
#267215=CARTESIAN_POINT('Ctrl Pts',(-0.648134006366779,-1.41407385925245,
11.2197335912736));
#267216=CARTESIAN_POINT('Ctrl Pts',(-0.661273082173743,-1.40794792508543,
11.2186782375319));
#267217=CARTESIAN_POINT('Ctrl Pts',(-0.665236547327894,-1.40607958036795,
11.2183602344379));
#267218=CARTESIAN_POINT('Ctrl Pts',(-0.672098867875133,-1.40280922789103,
11.217810319532));
#267219=CARTESIAN_POINT('Ctrl Pts',(-0.675001339125067,-1.40141493179697,
11.2175779403438));
#267220=CARTESIAN_POINT('Ctrl Pts',(-0.681076971163145,-1.39847305035946,
11.217091976527));
#267221=CARTESIAN_POINT('Ctrl Pts',(-0.684249204104702,-1.39692367027999,
11.2168385052843));
#267222=CARTESIAN_POINT('Ctrl Pts',(-0.692686650013249,-1.39276702085703,
11.2161649529105));
#267223=CARTESIAN_POINT('Ctrl Pts',(-0.697942482336024,-1.39014066331589,
11.2157460369082));
#267224=CARTESIAN_POINT('Ctrl Pts',(-0.720706138202114,-1.37860393984384,
11.2139339433999));
#267225=CARTESIAN_POINT('Ctrl Pts',(-0.738060141838192,-1.36939164703411,
11.2125583737263));
#267226=CARTESIAN_POINT('Ctrl Pts',(-0.851175561927651,-1.30656951075313,
11.2036000671003));
#267227=CARTESIAN_POINT('Ctrl Pts',(-0.941219936408087,-1.24327602094947,
11.1964901497737));
#267228=CARTESIAN_POINT('Ctrl Pts',(-1.09643014097945,-1.10757107105275,
11.182888967164));
#267229=CARTESIAN_POINT('Ctrl Pts',(-1.16293430465464,-1.03752220304883,
11.1764562146549));
#267230=CARTESIAN_POINT('Ctrl Pts',(-1.23052721268062,-0.951604206502917,
11.168818201296));
#267231=CARTESIAN_POINT('Ctrl Pts',(-1.23840283314166,-0.941332136938379,
11.1679090591008));
#267232=CARTESIAN_POINT('Ctrl Pts',(-1.25025472662428,-0.9254676794188,
11.1665103906766));
#267233=CARTESIAN_POINT('Ctrl Pts',(-1.25432385285745,-0.919945094295435,
11.1660244892754));
#267234=CARTESIAN_POINT('Ctrl Pts',(-1.26136151039847,-0.910260141793547,
11.1651739842198));
#267235=CARTESIAN_POINT('Ctrl Pts',(-1.26434632226614,-0.906109685347741,
11.1648100160584));
#267236=CARTESIAN_POINT('Ctrl Pts',(-1.2710319110929,-0.896715852100479,
11.1639873428862));
#267237=CARTESIAN_POINT('Ctrl Pts',(-1.27472078673598,-0.891464161930384,
11.1635281909489));
#267238=CARTESIAN_POINT('Ctrl Pts',(-1.28458078595995,-0.877240577595905,
11.1622865958419));
#267239=CARTESIAN_POINT('Ctrl Pts',(-1.29069026893407,-0.868226609303773,
11.1615018402763));
#267240=CARTESIAN_POINT('Ctrl Pts',(-1.3184201045975,-0.826374284505443,
11.157867019056));
#267241=CARTESIAN_POINT('Ctrl Pts',(-1.33888334424869,-0.792790581932498,
11.1549746119441));
#267242=CARTESIAN_POINT('Ctrl Pts',(-1.43421910520561,-0.622090701509377,
11.1403767687332));
#267243=CARTESIAN_POINT('Ctrl Pts',(-1.48939342059203,-0.475050691549615,
11.1280030280243));
#267244=CARTESIAN_POINT('Ctrl Pts',(-1.52851215983715,-0.290339124693049,
11.1136920176644));
#267245=CARTESIAN_POINT('Ctrl Pts',(-1.53427002481038,-0.258190082007997,
11.1112492791146));
#267246=CARTESIAN_POINT('Ctrl Pts',(-1.5399761490847,-0.219312078202865,
11.1083706507332));
#267247=CARTESIAN_POINT('Ctrl Pts',(-1.5408981976906,-0.212737105385428,
11.1078864046954));
#267248=CARTESIAN_POINT('Ctrl Pts',(-1.54226834185423,-0.202490226695637,
11.1071359460143));
#267249=CARTESIAN_POINT('Ctrl Pts',(-1.54274547081239,-0.198822391234944,
11.1068681628043));
#267250=CARTESIAN_POINT('Ctrl Pts',(-1.54360877498709,-0.191995643337098,
11.1063713588623));
#267251=CARTESIAN_POINT('Ctrl Pts',(-1.54399833569566,-0.188837276424316,
11.1061421587234));
#267252=CARTESIAN_POINT('Ctrl Pts',(-1.54486530373876,-0.181626249050114,
11.105620308652));
#267253=CARTESIAN_POINT('Ctrl Pts',(-1.54533645842177,-0.177572893029326,
11.105328012022));
#267254=CARTESIAN_POINT('Ctrl Pts',(-1.54652572090355,-0.166978282939704,
11.1045666098808));
#267255=CARTESIAN_POINT('Ctrl Pts',(-1.54721829068781,-0.160434152887472,
11.1040988890746));
#267256=CARTESIAN_POINT('Ctrl Pts',(-1.55165291611642,-0.115828176337331,
11.1009271994944));
#267257=CARTESIAN_POINT('Ctrl Pts',(-1.55403203440442,-0.0776400661746127,
11.0982929362908));
#267258=CARTESIAN_POINT('Ctrl Pts',(-1.55532424691055,-0.026639391096279,
11.0948362395981));
#267259=CARTESIAN_POINT('Ctrl Pts',(-1.5554904855441,-0.0138756730603074,
11.0939762747276));
#267260=CARTESIAN_POINT('Ctrl Pts',(-1.55558217104781,0.114482777279392,
11.085366981832));
#267261=CARTESIAN_POINT('Ctrl Pts',(-1.54277988274089,0.229726903704349,
11.0779273206166));
#267262=CARTESIAN_POINT('Ctrl Pts',(-1.51279541076874,0.362565510575355,
11.0687948979185));
#267263=CARTESIAN_POINT('Ctrl Pts',(-1.50786677741873,0.382545991423653,
11.0674068982995));
#267264=CARTESIAN_POINT('Ctrl Pts',(-1.49229849522005,0.44067403895012,
11.0633178607757));
#267265=CARTESIAN_POINT('Ctrl Pts',(-1.48059747192315,0.478517587256855,
11.060590393756));
#267266=CARTESIAN_POINT('Ctrl Pts',(-1.4638461164133,0.52616913125099,11.0570508059872));
#267267=CARTESIAN_POINT('Ctrl Pts',(-1.4601177091598,0.536428626976604,
11.056282410341));
#267268=CARTESIAN_POINT('Ctrl Pts',(-1.45402424810548,0.552661740583099,
11.0550561429149));
#267269=CARTESIAN_POINT('Ctrl Pts',(-1.45172958267431,0.558661552393764,
11.0546006192035));
#267270=CARTESIAN_POINT('Ctrl Pts',(-1.44754235582564,0.569409787472199,
11.0537803750444));
#267271=CARTESIAN_POINT('Ctrl Pts',(-1.44566341540457,0.57416344902276,
11.0534161160298));
#267272=CARTESIAN_POINT('Ctrl Pts',(-1.44121105649753,0.585267365005433,
11.0525617211079));
#267273=CARTESIAN_POINT('Ctrl Pts',(-1.43861905941743,0.591610004150868,
11.0520709650014));
#267274=CARTESIAN_POINT('Ctrl Pts',(-1.43102437127428,0.609849204723922,
11.05065173194));
#267275=CARTESIAN_POINT('Ctrl Pts',(-1.42591552787011,0.621700645318622,
11.049719681143));
#267276=CARTESIAN_POINT('Ctrl Pts',(-1.38229536757299,0.719523382584035,
11.041942191734));
#267277=CARTESIAN_POINT('Ctrl Pts',(-1.33620236672565,0.801879836687392,
11.0348320434333));
#267278=CARTESIAN_POINT('Ctrl Pts',(-1.22750367541922,0.960433280597649,
11.0200160721238));
#267279=CARTESIAN_POINT('Ctrl Pts',(-1.16452767311637,1.03589252185072,
11.0123310771437));
#267280=CARTESIAN_POINT('Ctrl Pts',(-1.07236398676692,1.12721744724209,
11.0025004534834));
#267281=CARTESIAN_POINT('Ctrl Pts',(-1.04918473712791,1.14882350428654,
11.0001307017482));
#267282=CARTESIAN_POINT('Ctrl Pts',(-1.02067181916037,1.17381776763446,
10.997351212523));
#267283=CARTESIAN_POINT('Ctrl Pts',(-1.01595911612107,1.1778990584566,10.9968960808536));
#267284=CARTESIAN_POINT('Ctrl Pts',(-1.00820100259672,1.1845365313033,10.9961539745183));
#267285=CARTESIAN_POINT('Ctrl Pts',(-1.00517016372617,1.18710951413079,
10.9958658212058));
#267286=CARTESIAN_POINT('Ctrl Pts',(-0.999701081239196,1.19171644254419,
10.9953490674367));
#267287=CARTESIAN_POINT('Ctrl Pts',(-0.997266459579022,1.19375455620573,
10.9951201680369));
#267288=CARTESIAN_POINT('Ctrl Pts',(-0.991920916247426,1.19820174517085,
10.9946200783711));
#267289=CARTESIAN_POINT('Ctrl Pts',(-0.989007456346326,1.20060767044556,
10.994349115658));
#267290=CARTESIAN_POINT('Ctrl Pts',(-0.980664594257101,1.20744620122068,
10.9935776532084));
#267291=CARTESIAN_POINT('Ctrl Pts',(-0.975213866103736,1.21185283577421,
10.9930789788959));
#267292=CARTESIAN_POINT('Ctrl Pts',(-0.938377309305883,1.24122380776167,
10.989743218794));
#267293=CARTESIAN_POINT('Ctrl Pts',(-0.906062629495376,1.26500581859923,
10.9869831292336));
#267294=CARTESIAN_POINT('Ctrl Pts',(-0.768069859748684,1.35855705071681,
10.9757006456318));
#267295=CARTESIAN_POINT('Ctrl Pts',(-0.654993139874641,1.41654402629038,
10.9675940287547));
#267296=CARTESIAN_POINT('Ctrl Pts',(-0.515655655391122,1.46770408175223,
10.9576423940307));
#267297=CARTESIAN_POINT('Ctrl Pts',(-0.495024728406495,1.47479031893277,
10.9561710416941));
#267298=CARTESIAN_POINT('Ctrl Pts',(-0.43719224106788,1.4933041864229,10.952042502575));
#267299=CARTESIAN_POINT('Ctrl Pts',(-0.399703032479088,1.50377242428745,
10.9493612647338));
#267300=CARTESIAN_POINT('Ctrl Pts',(-0.351309944031713,1.51534792011397,
10.9458740173629));
#267301=CARTESIAN_POINT('Ctrl Pts',(-0.340730698574113,1.51776169942081,
10.9451101285128));
#267302=CARTESIAN_POINT('Ctrl Pts',(-0.323863890699692,1.521424829217,10.9438893965402));
#267303=CARTESIAN_POINT('Ctrl Pts',(-0.317592221534729,1.52274637062255,
10.9434348646361));
#267304=CARTESIAN_POINT('Ctrl Pts',(-0.306302687401168,1.52505247801854,
10.9426154723566));
#267305=CARTESIAN_POINT('Ctrl Pts',(-0.301287766335465,1.52605113863509,
10.9422510673386));
#267306=CARTESIAN_POINT('Ctrl Pts',(-0.289522475276183,1.52833379932475,
10.9413951131415));
#267307=CARTESIAN_POINT('Ctrl Pts',(-0.282768387655546,1.52959782360806,
10.94090293629));
#267308=CARTESIAN_POINT('Ctrl Pts',(-0.263213571276487,1.53312355615844,
10.9394755167559));
#267309=CARTESIAN_POINT('Ctrl Pts',(-0.250392860327313,1.53526955905738,
10.9385366360095));
#267310=CARTESIAN_POINT('Ctrl Pts',(-0.138710229148496,1.55252752479783,
10.9303296076239));
#267311=CARTESIAN_POINT('Ctrl Pts',(-0.0386513585304838,1.55823002918866,
10.9227609228349));
#267312=CARTESIAN_POINT('Ctrl Pts',(0.172465863355541,1.54991140647999,
10.9064468286025));
#267313=CARTESIAN_POINT('Ctrl Pts',(0.282901300586441,1.53360346747836,
10.8977099057263));
#267314=CARTESIAN_POINT('Ctrl Pts',(0.405596303157897,1.50176901048146,
10.888277423913));
#267315=CARTESIAN_POINT('Ctrl Pts',(0.420479874414671,1.49766993888031,
10.887138469811));
#267316=CARTESIAN_POINT('Ctrl Pts',(0.440440069687756,1.49185168580223,
10.8856203284504));
#267317=CARTESIAN_POINT('Ctrl Pts',(0.445571776325477,1.49032704526006,
10.8852308531077));
#267318=CARTESIAN_POINT('Ctrl Pts',(0.453638483437051,1.48788501925912,
10.8846200483424));
#267319=CARTESIAN_POINT('Ctrl Pts',(0.456578743310892,1.4869853919244,10.8843977132168));
#267320=CARTESIAN_POINT('Ctrl Pts',(0.462598888173646,1.48512387672494,
10.8839431255458));
#267321=CARTESIAN_POINT('Ctrl Pts',(0.465678452641179,1.48416112316659,
10.8837109335711));
#267322=CARTESIAN_POINT('Ctrl Pts',(0.472972262211009,1.48185594801787,
10.8831617854914));
#267323=CARTESIAN_POINT('Ctrl Pts',(0.477183859976159,1.48050510859362,
10.8828453189205));
#267324=CARTESIAN_POINT('Ctrl Pts',(0.491232995161731,1.47593277196518,
10.8817915451575));
#267325=CARTESIAN_POINT('Ctrl Pts',(0.501044410423555,1.47263095070723,
10.8810587501095));
#267326=CARTESIAN_POINT('Ctrl Pts',(0.590995037240804,1.44135690833052,
10.8743629192792));
#267327=CARTESIAN_POINT('Ctrl Pts',(0.668764723103699,1.40696237549458,
10.868734006899));
#267328=CARTESIAN_POINT('Ctrl Pts',(0.853659543376579,1.30637496902906,
10.8548593246367));
#267329=CARTESIAN_POINT('Ctrl Pts',(0.956283033878582,1.23323493667614,
10.8466693205959));
#267330=CARTESIAN_POINT('Ctrl Pts',(1.05605398054823,1.14211279316921,10.8372912555581));
#267331=CARTESIAN_POINT('Ctrl Pts',(1.06305317632791,1.13560097725169,10.8366252071394));
#267332=CARTESIAN_POINT('Ctrl Pts',(1.07790584279944,1.12152491303635,10.8351937877764));
#267333=CARTESIAN_POINT('Ctrl Pts',(1.08574064998974,1.11394181481536,10.8344276579514));
#267334=CARTESIAN_POINT('Ctrl Pts',(1.09851266645072,1.10131736970719,10.8331599207525));
#267335=CARTESIAN_POINT('Ctrl Pts',(1.10349653823666,1.09632359014344,10.8326603932683));
#267336=CARTESIAN_POINT('Ctrl Pts',(1.11242695528036,1.08725282897042,10.8317564165027));
#267337=CARTESIAN_POINT('Ctrl Pts',(1.11638551674112,1.08318780522391,10.8313525036097));
#267338=CARTESIAN_POINT('Ctrl Pts',(1.12480786157488,1.07444373641828,10.8304861593299));
#267339=CARTESIAN_POINT('Ctrl Pts',(1.12926487047949,1.06975834568157,10.8300234455558));
#267340=CARTESIAN_POINT('Ctrl Pts',(1.14130080463768,1.05694663980147,10.8287621655614));
#267341=CARTESIAN_POINT('Ctrl Pts',(1.14882194752271,1.04876682204764,10.8279611592821));
#267342=CARTESIAN_POINT('Ctrl Pts',(1.1883878531437,1.00479955658845,10.8236773523445));
#267343=CARTESIAN_POINT('Ctrl Pts',(1.21884616070218,0.967626451145882,
10.8201296762553));
#267344=CARTESIAN_POINT('Ctrl Pts',(1.31101578117956,0.843868250753702,
10.8085355798078));
#267345=CARTESIAN_POINT('Ctrl Pts',(1.36558856985246,0.75235531415365,10.8002588317065));
#267346=CARTESIAN_POINT('Ctrl Pts',(1.4188108695178,0.637929180241413,10.7904961005974));
#267347=CARTESIAN_POINT('Ctrl Pts',(1.42687088569456,0.619691121367997,
10.788957519497));
#267348=CARTESIAN_POINT('Ctrl Pts',(1.43457669771236,0.601306867065985,
10.7874266037958));
#267349=CARTESIAN_POINT('',(-1.55549978056836,-0.000826227440647477,10.9559437744364));
#267350=CARTESIAN_POINT('Ctrl Pts',(1.43457668061803,0.601306907849032,
10.6508134549194));
#267351=CARTESIAN_POINT('Ctrl Pts',(1.41619620423421,0.645158396090189,
10.6544831834601));
#267352=CARTESIAN_POINT('Ctrl Pts',(1.39579412672923,0.688193435945673,
10.6581266992052));
#267353=CARTESIAN_POINT('Ctrl Pts',(1.36438025897942,0.747273394627868,
10.66313110101));
#267354=CARTESIAN_POINT('Ctrl Pts',(1.35502484783335,0.764106517541768,
10.664557133452));
#267355=CARTESIAN_POINT('Ctrl Pts',(1.34240944669324,0.785844546997109,
10.6663948398768));
#267356=CARTESIAN_POINT('Ctrl Pts',(1.33943134897283,0.790909880445301,
10.6668227782386));
#267357=CARTESIAN_POINT('Ctrl Pts',(1.33460359699645,0.799015739870661,
10.6675069953127));
#267358=CARTESIAN_POINT('Ctrl Pts',(1.3327721261639,0.802066938659978,10.6677644108619));
#267359=CARTESIAN_POINT('Ctrl Pts',(1.32923864623555,0.807908133224289,
10.6682569032129));
#267360=CARTESIAN_POINT('Ctrl Pts',(1.32753830870945,0.810699062234914,
10.6684920785131));
#267361=CARTESIAN_POINT('Ctrl Pts',(1.32348534594304,0.817304640257065,
10.6690484062855));
#267362=CARTESIAN_POINT('Ctrl Pts',(1.32112498360486,0.821114556534951,
10.6693690562206));
#267363=CARTESIAN_POINT('Ctrl Pts',(1.31317939338839,0.833816764043849,
10.6704375349543));
#267364=CARTESIAN_POINT('Ctrl Pts',(1.30752043314011,0.84266295045385,10.6711807266092));
#267365=CARTESIAN_POINT('Ctrl Pts',(1.27544013593418,0.891710063610714,
10.6753001603434));
#267366=CARTESIAN_POINT('Ctrl Pts',(1.24725167629116,0.930730189131567,
10.678573390205));
#267367=CARTESIAN_POINT('Ctrl Pts',(1.13870618721888,1.06717600073408,10.6902522847122));
#267368=CARTESIAN_POINT('Ctrl Pts',(1.04838333350197,1.15603226635772,10.6983550752257));
#267369=CARTESIAN_POINT('Ctrl Pts',(0.911642673098545,1.26120099364639,
10.7100154772344));
#267370=CARTESIAN_POINT('Ctrl Pts',(0.873736669563318,1.28775146965589,
10.7131890168183));
#267371=CARTESIAN_POINT('Ctrl Pts',(0.825057760966379,1.31870796655941,
10.7172277215283));
#267372=CARTESIAN_POINT('Ctrl Pts',(0.815341442936844,1.32473745666391,
10.7180320394218));
#267373=CARTESIAN_POINT('Ctrl Pts',(0.799866058557581,1.33410600684216,
10.7193107236626));
#267374=CARTESIAN_POINT('Ctrl Pts',(0.794150378480177,1.33751625148603,
10.7197824880266));
#267375=CARTESIAN_POINT('Ctrl Pts',(0.783467090048704,1.34379778564043,
10.7206634307065));
#267376=CARTESIAN_POINT('Ctrl Pts',(0.778505121588518,1.34667848572849,
10.7210722594634));
#267377=CARTESIAN_POINT('Ctrl Pts',(0.767449830053376,1.35301518106417,
10.7219824570715));
#267378=CARTESIAN_POINT('Ctrl Pts',(0.761348901513619,1.35645758099316,
10.7224843036137));
#267379=CARTESIAN_POINT('Ctrl Pts',(0.743520845129856,1.3663587532309,10.7239496227149));
#267380=CARTESIAN_POINT('Ctrl Pts',(0.731733590657187,1.37270733266515,
10.7249169800991));
#267381=CARTESIAN_POINT('Ctrl Pts',(0.704910433859287,1.3867105560066,10.7271156282808));
#267382=CARTESIAN_POINT('Ctrl Pts',(0.689829203029044,1.39427418944725,
10.7283499498588));
#267383=CARTESIAN_POINT('Ctrl Pts',(0.640219855864595,1.41815268420438,
10.7324052391445));
#267384=CARTESIAN_POINT('Ctrl Pts',(0.605215845889956,1.43344056071235,
10.7352592707501));
#267385=CARTESIAN_POINT('Ctrl Pts',(0.495389114658614,1.47666693979708,
10.7441894641905));
#267386=CARTESIAN_POINT('Ctrl Pts',(0.418955618688625,1.50014320523994,
10.7503773161104));
#267387=CARTESIAN_POINT('Ctrl Pts',(0.323987695278868,1.52148566292954,
10.75792399371));
#267388=CARTESIAN_POINT('Ctrl Pts',(0.306845677700836,1.52503520927365,
10.7592802964974));
#267389=CARTESIAN_POINT('Ctrl Pts',(0.222367522555693,1.54104577788857,
10.7659275088472));
#267390=CARTESIAN_POINT('Ctrl Pts',(0.154309765543913,1.54934192275926,
10.771171496261));
#267391=CARTESIAN_POINT('Ctrl Pts',(0.0778710378401672,1.55357050533948,
10.7767980922308));
#267392=CARTESIAN_POINT('Ctrl Pts',(0.069819771137083,1.55395315908165,
10.7773874525756));
#267393=CARTESIAN_POINT('Ctrl Pts',(0.057688532344503,1.5544352455154,10.7782701666098));
#267394=CARTESIAN_POINT('Ctrl Pts',(0.0536107142970978,1.5545812270859,
10.7785659816501));
#267395=CARTESIAN_POINT('Ctrl Pts',(0.04631493491922,1.55481366690318,10.7790935665395));
#267396=CARTESIAN_POINT('Ctrl Pts',(0.0430972478866489,1.55490618362709,
10.7793256653622));
#267397=CARTESIAN_POINT('Ctrl Pts',(0.0360933107500557,1.55508580640662,
10.779829598358));
#267398=CARTESIAN_POINT('Ctrl Pts',(0.0323070271114213,1.55516907415071,
10.7801012169415));
#267399=CARTESIAN_POINT('Ctrl Pts',(0.0216060525305109,1.55536531177897,
10.7808667017652));
#267400=CARTESIAN_POINT('Ctrl Pts',(0.0146907420575159,1.55544600081099,
10.7813588146593));
#267401=CARTESIAN_POINT('Ctrl Pts',(-0.0289771161113971,1.55566427131,10.7844514434209));
#267402=CARTESIAN_POINT('Ctrl Pts',(-0.0657279399814517,1.55454539425717,
10.7869876301598));
#267403=CARTESIAN_POINT('Ctrl Pts',(-0.155184050603876,1.54864314198138,
10.7930740252757));
#267404=CARTESIAN_POINT('Ctrl Pts',(-0.207751720116059,1.54247128097895,
10.796577285723));
#267405=CARTESIAN_POINT('Ctrl Pts',(-0.384102111429581,1.51258504509691,
10.8083702762409));
#267406=CARTESIAN_POINT('Ctrl Pts',(-0.505265310789401,1.47653324469058,
10.816584091007));
#267407=CARTESIAN_POINT('Ctrl Pts',(-0.637115133483651,1.41914871414357,
10.8265641689815));
#267408=CARTESIAN_POINT('Ctrl Pts',(-0.653355044431452,1.41174569468414,
10.8278116380983));
#267409=CARTESIAN_POINT('Ctrl Pts',(-0.676022702163713,1.40093767222303,
10.8295804468908));
#267410=CARTESIAN_POINT('Ctrl Pts',(-0.682559881241098,1.39776430795671,
10.8300938323111));
#267411=CARTESIAN_POINT('Ctrl Pts',(-0.693904235807884,1.39215882114782,
10.8309905847092));
#267412=CARTESIAN_POINT('Ctrl Pts',(-0.698721498509973,1.38974729284195,
10.8313732321887));
#267413=CARTESIAN_POINT('Ctrl Pts',(-0.708667277923455,1.38470363921932,
10.8321671459282));
#267414=CARTESIAN_POINT('Ctrl Pts',(-0.71379387648419,1.38206793592603,
10.8325785327186));
#267415=CARTESIAN_POINT('Ctrl Pts',(-0.725868218104618,1.37577513599158,
10.8335526302688));
#267416=CARTESIAN_POINT('Ctrl Pts',(-0.732803098461349,1.37209384138383,
10.8341161865886));
#267417=CARTESIAN_POINT('Ctrl Pts',(-0.747448672841228,1.36417672069205,
10.835315176103));
#267418=CARTESIAN_POINT('Ctrl Pts',(-0.755151868301836,1.35992767958414,
10.8359510643873));
#267419=CARTESIAN_POINT('Ctrl Pts',(-0.776007003449739,1.34819226909533,
10.8376871758941));
#267420=CARTESIAN_POINT('Ctrl Pts',(-0.789086095040736,1.34057911688083,
10.838791871823));
#267421=CARTESIAN_POINT('Ctrl Pts',(-0.830058397803283,1.31592239523502,
10.8423040084776));
#267422=CARTESIAN_POINT('Ctrl Pts',(-0.857524971854549,1.29819079262242,
10.8447353642989));
#267423=CARTESIAN_POINT('Ctrl Pts',(-0.977590337987496,1.21520671318003,
10.8557146768537));
#267424=CARTESIAN_POINT('Ctrl Pts',(-1.06344862377193,1.14082484694671,
10.8645642374876));
#267425=CARTESIAN_POINT('Ctrl Pts',(-1.18253181884092,1.0124359648641,10.878074107562));
#267426=CARTESIAN_POINT('Ctrl Pts',(-1.22186727572909,0.964598587834279,
10.882794261092));
#267427=CARTESIAN_POINT('Ctrl Pts',(-1.26295003261908,0.908075608173471,
10.8879291829592));
#267428=CARTESIAN_POINT('Ctrl Pts',(-1.26759811018072,0.901575916603189,
10.8885133850766));
#267429=CARTESIAN_POINT('Ctrl Pts',(-1.27453536002879,0.891715422511863,
10.8893899022158));
#267430=CARTESIAN_POINT('Ctrl Pts',(-1.27686168479867,0.888381121829058,
10.8896846289766));
#267431=CARTESIAN_POINT('Ctrl Pts',(-1.28100591737691,0.882391322119793,
10.8902110514531));
#267432=CARTESIAN_POINT('Ctrl Pts',(-1.28282867426031,0.879739278912409,
10.8904430698793));
#267433=CARTESIAN_POINT('Ctrl Pts',(-1.28678506910476,0.873944428817586,
10.8909477306516));
#267434=CARTESIAN_POINT('Ctrl Pts',(-1.28891542699547,0.870799461196348,
10.8912201523769));
#267435=CARTESIAN_POINT('Ctrl Pts',(-1.29492122314751,0.861863002509983,
10.8919901923896));
#267436=CARTESIAN_POINT('Ctrl Pts',(-1.29876936068532,0.856053130275553,
10.8924860240214));
#267437=CARTESIAN_POINT('Ctrl Pts',(-1.32326487319759,0.818524700312995,
10.8956594763472));
#267438=CARTESIAN_POINT('Ctrl Pts',(-1.34278994909062,0.786084190293236,
10.8982688178962));
#267439=CARTESIAN_POINT('Ctrl Pts',(-1.4308626495039,0.626876648683413,
10.9106078912675));
#267440=CARTESIAN_POINT('Ctrl Pts',(-1.48275758416514,0.491709700680271,
10.9197701759167));
#267441=CARTESIAN_POINT('Ctrl Pts',(-1.52401123281862,0.313776118444744,
10.9321330785903));
#267442=CARTESIAN_POINT('Ctrl Pts',(-1.5313170344172,0.275922870364973,
10.9347746967179));
#267443=CARTESIAN_POINT('Ctrl Pts',(-1.53949692490965,0.223054491725705,
10.93850249068));
#267444=CARTESIAN_POINT('Ctrl Pts',(-1.5415710276318,0.208237430823827,
10.9395513283463));
#267445=CARTESIAN_POINT('Ctrl Pts',(-1.54434140756813,0.186127602853223,
10.9411234913082));
#267446=CARTESIAN_POINT('Ctrl Pts',(-1.54520046363276,0.178855784234435,
10.9416417062508));
#267447=CARTESIAN_POINT('Ctrl Pts',(-1.5466163139368,0.166098248394197,
10.9425529684043));
#267448=CARTESIAN_POINT('Ctrl Pts',(-1.54719534759494,0.160615085230751,
10.9429453107873));
#267449=CARTESIAN_POINT('Ctrl Pts',(-1.5482816790177,0.149776595957513,
10.9437222515601));
#267450=CARTESIAN_POINT('Ctrl Pts',(-1.54879037307705,0.144421484556476,
10.9441068003859));
#267451=CARTESIAN_POINT('Ctrl Pts',(-1.54982941478438,0.13284581735533,
10.9449395534471));
#267452=CARTESIAN_POINT('Ctrl Pts',(-1.55035010782426,0.126624512560305,
10.9453880537738));
#267453=CARTESIAN_POINT('Ctrl Pts',(-1.55152314351844,0.1115150612476,10.9464796663673));
#267454=CARTESIAN_POINT('Ctrl Pts',(-1.55213657237751,0.102624209138309,
10.9471239819166));
#267455=CARTESIAN_POINT('Ctrl Pts',(-1.55457598776545,0.0622138129656635,
10.9500618284598));
#267456=CARTESIAN_POINT('Ctrl Pts',(-1.55551832872089,0.0306508940191186,
10.9523824318058));
#267457=CARTESIAN_POINT('Ctrl Pts',(-1.55549973002184,-0.000916461665043444,
10.954730847374));
#267458=CARTESIAN_POINT('Ctrl Pts',(-1.55549978056836,-0.000826227440647477,
10.9559437744364));
#267459=CARTESIAN_POINT('Ctrl Pts',(-1.55546565861298,-0.0650660378110669,
10.9605241758682));
#267460=CARTESIAN_POINT('Ctrl Pts',(-1.55144787772679,-0.129166249084525,
10.9651045773));
#267461=CARTESIAN_POINT('Ctrl Pts',(-1.54352279076948,-0.19265939991392,
10.9696849787318));
#267462=CARTESIAN_POINT('Ctrl Pts',(-1.53556587820097,-0.256407526914957,
10.9742837741668));
#267463=CARTESIAN_POINT('Ctrl Pts',(-1.52367036163636,-0.319543413071712,
10.9788825696018));
#267464=CARTESIAN_POINT('Ctrl Pts',(-1.50796326206369,-0.381611124400532,
10.9834813650368));
#267465=CARTESIAN_POINT('Ctrl Pts',(-1.49217853217136,-0.443985597410511,
10.9881028894269));
#267466=CARTESIAN_POINT('Ctrl Pts',(-1.47254460406452,-0.505281027035107,
10.9927244138169));
#267467=CARTESIAN_POINT('Ctrl Pts',(-1.44923826450197,-0.565056371261592,
10.997345938207));
#267468=CARTESIAN_POINT('Ctrl Pts',(-1.44472395673645,-0.576634521485644,
10.9982411016618));
#267469=CARTESIAN_POINT('Ctrl Pts',(-1.44007200844342,-0.588155714178932,
10.9991362651166));
#267470=CARTESIAN_POINT('Ctrl Pts',(-1.43528390274065,-0.599616851442292,
11.0000314285715));
#267471=CARTESIAN_POINT('Ctrl Pts',(-1.41309670781834,-0.652725638565867,
11.0041794502094));
#267472=CARTESIAN_POINT('Ctrl Pts',(-1.38791123557696,-0.704712790082137,
11.0083274718473));
#267473=CARTESIAN_POINT('Ctrl Pts',(-1.35986268358359,-0.755217671798561,
11.0124754934853));
#267474=CARTESIAN_POINT('Ctrl Pts',(-1.33186400318891,-0.805632753542662,
11.0166161397525));
#267475=CARTESIAN_POINT('Ctrl Pts',(-1.30101259808066,-0.854570345106836,
11.0207567860196));
#267476=CARTESIAN_POINT('Ctrl Pts',(-1.2674912840762,-0.901690686871537,
11.0248974322868));
#267477=CARTESIAN_POINT('Ctrl Pts',(-1.23400331523107,-0.948764155912103,
11.0290339596668));
#267478=CARTESIAN_POINT('Ctrl Pts',(-1.1978509999251,-0.994023534493074,
11.0331704870468));
#267479=CARTESIAN_POINT('Ctrl Pts',(-1.15926163198756,-1.03715607244115,
11.0373070144269));
#267480=CARTESIAN_POINT('Ctrl Pts',(-1.12069581533763,-1.08026228638183,
11.0414410172632));
#267481=CARTESIAN_POINT('Ctrl Pts',(-1.07969624093573,-1.12124384537538,
11.0455750200995));
#267482=CARTESIAN_POINT('Ctrl Pts',(-1.03653046940682,-1.15982103619105,
11.0497090229358));
#267483=CARTESIAN_POINT('Ctrl Pts',(-0.993374448377873,-1.19838951299827,
11.0538420919629));
#267484=CARTESIAN_POINT('Ctrl Pts',(-0.948053589772702,-1.23455435295824,
11.05797516099));
#267485=CARTESIAN_POINT('Ctrl Pts',(-0.900870680298012,-1.26807423575254,
11.0621082300171));
#267486=CARTESIAN_POINT('Ctrl Pts',(-0.853645123206089,-1.30162441644808,
11.0662450348364));
#267487=CARTESIAN_POINT('Ctrl Pts',(-0.80455457673083,-1.33252455904199,
11.0703818396558));
#267488=CARTESIAN_POINT('Ctrl Pts',(-0.753932043950639,-1.36057587921601,
11.0745186444751));
#267489=CARTESIAN_POINT('Ctrl Pts',(-0.703288596590755,-1.38863878872661,
11.0786571584055));
#267490=CARTESIAN_POINT('Ctrl Pts',(-0.651112370525066,-1.41385030117597,
11.082795672336));
#267491=CARTESIAN_POINT('Ctrl Pts',(-0.597759394860077,-1.43605847926069,
11.0869341862665));
#267492=CARTESIAN_POINT('Ctrl Pts',(-0.544302397442401,-1.45830995640379,
11.0910807690153));
#267493=CARTESIAN_POINT('Ctrl Pts',(-0.489664558226208,-1.47754622284655,
11.0952273517642));
#267494=CARTESIAN_POINT('Ctrl Pts',(-0.434219362892345,-1.49366455233073,
11.0993739345131));
#267495=CARTESIAN_POINT('Ctrl Pts',(-0.381764104060325,-1.50891368509943,
11.103296908723));
#267496=CARTESIAN_POINT('Ctrl Pts',(-0.328586705854618,-1.52137244781314,
11.107219882933));
#267497=CARTESIAN_POINT('Ctrl Pts',(-0.27500985724936,-1.53099635153572,
11.1111428571429));
#267498=CARTESIAN_POINT('Ctrl Pts',(-0.2183594906108,-1.54117234524515,
11.1152908787808));
#267499=CARTESIAN_POINT('Ctrl Pts',(-0.161024631712135,-1.54822116712312,
11.1194389004188));
#267500=CARTESIAN_POINT('Ctrl Pts',(-0.103381573792702,-1.55206072696919,
11.1235869220567));
#267501=CARTESIAN_POINT('Ctrl Pts',(-0.0458410078468976,-1.55589345990357,
11.1277275683239));
#267502=CARTESIAN_POINT('Ctrl Pts',(0.0120061540690754,-1.55652822247625,
11.1318682145911));
#267503=CARTESIAN_POINT('Ctrl Pts',(0.0697753189408187,-1.55393425049669,
11.1360088608582));
#267504=CARTESIAN_POINT('Ctrl Pts',(0.127487018224909,-1.55134285885777,
11.1401453882382));
#267505=CARTESIAN_POINT('Ctrl Pts',(0.185120356531842,-1.5455291193456,
11.1442819156183));
#267506=CARTESIAN_POINT('Ctrl Pts',(0.242289298251249,-1.53651428433091,
11.1484184429983));
#267507=CARTESIAN_POINT('Ctrl Pts',(0.299423349474618,-1.5275049511159,
11.1525524458346));
#267508=CARTESIAN_POINT('Ctrl Pts',(0.356093052529829,-1.51529847601814,
11.1566864486709));
#267509=CARTESIAN_POINT('Ctrl Pts',(0.411918277242572,-1.49996786061352,
11.1608204515072));
#267510=CARTESIAN_POINT('Ctrl Pts',(0.467730891874893,-1.48464070816484,
11.1649535205343));
#267511=CARTESIAN_POINT('Ctrl Pts',(0.522698904886622,-1.46619095424824,
11.1690865895614));
#267512=CARTESIAN_POINT('Ctrl Pts',(0.576455325509742,-1.44474202115515,
11.1732196585885));
#267513=CARTESIAN_POINT('Ctrl Pts',(0.630260335405474,-1.42327370083267,
11.1773564634079));
#267514=CARTESIAN_POINT('Ctrl Pts',(0.682851079059476,-1.39880097627071,
11.1814932682272));
#267515=CARTESIAN_POINT('Ctrl Pts',(0.733879903405016,-1.37149572998907,
11.1856300730465));
#267516=CARTESIAN_POINT('Ctrl Pts',(0.784929810188654,-1.3441792026095,
11.189768586977));
#267517=CARTESIAN_POINT('Ctrl Pts',(0.834416064806619,-1.31402809101586,
11.1939071009074));
#267518=CARTESIAN_POINT('Ctrl Pts',(0.882017874341116,-1.28125903678483,
11.1980456148379));
#267519=CARTESIAN_POINT('Ctrl Pts',(0.929712492638306,-1.24842609306287,
11.2021921975868));
#267520=CARTESIAN_POINT('Ctrl Pts',(0.975514909601415,-1.21296532571064,
11.2063387803356));
#267521=CARTESIAN_POINT('Ctrl Pts',(1.01913619998497,-1.17513473945765,
11.2104853630845));
#267522=CARTESIAN_POINT('Ctrl Pts',(1.06040516952995,-1.13934420464734,
11.2144083372944));
#267523=CARTESIAN_POINT('Ctrl Pts',(1.0997219438703,-1.10143315475768,11.2183313115044));
#267524=CARTESIAN_POINT('Ctrl Pts',(1.13687407815269,-1.06164852019134,
11.2222542857143));
#267525=CARTESIAN_POINT('Ctrl Pts',(1.17615750155851,-1.01958157908816,
11.2264023073522));
#267526=CARTESIAN_POINT('Ctrl Pts',(1.21318538180509,-0.975243017775855,
11.2305503289902));
#267527=CARTESIAN_POINT('Ctrl Pts',(1.24768460527871,-0.928904395376887,
11.2346983506281));
#267528=CARTESIAN_POINT('Ctrl Pts',(1.28212248756693,-0.882648165152056,
11.2388389968953));
#267529=CARTESIAN_POINT('Ctrl Pts',(1.31404032867007,-0.834399346673556,
11.2429796431625));
#267530=CARTESIAN_POINT('Ctrl Pts',(1.34320362724052,-0.78446431771491,
11.2471202894296));
#267531=CARTESIAN_POINT('Ctrl Pts',(1.37233791576565,-0.734578961376423,
11.2512568168096));
#267532=CARTESIAN_POINT('Ctrl Pts',(1.39872282929431,-0.683011165324985,
11.2553933441897));
#267533=CARTESIAN_POINT('Ctrl Pts',(1.42216677914759,-0.630096740420842,
11.2595298715697));
#267534=CARTESIAN_POINT('Ctrl Pts',(1.44559642103898,-0.577214609459475,
11.263663874406));
#267535=CARTESIAN_POINT('Ctrl Pts',(1.46608844667386,-0.522987953983979,
11.2677978772423));
#267536=CARTESIAN_POINT('Ctrl Pts',(1.48349794208529,-0.467775700340131,
11.2719318800786));
#267537=CARTESIAN_POINT('Ctrl Pts',(1.500903504953,-0.412575918315756,11.2760649491057));
#267538=CARTESIAN_POINT('Ctrl Pts',(1.51522776338046,-0.356391476567678,
11.2801980181328));
#267539=CARTESIAN_POINT('Ctrl Pts',(1.52637528689117,-0.299597619429611,
11.2843310871599));
#267540=CARTESIAN_POINT('Ctrl Pts',(1.53753288640867,-0.242752427545375,
11.2884678919793));
#267541=CARTESIAN_POINT('Ctrl Pts',(1.54550791113036,-0.185297231555324,
11.2926046967986));
#267542=CARTESIAN_POINT('Ctrl Pts',(1.55025613005402,-0.127617323392752,
11.2967415016179));
#267543=CARTESIAN_POINT('Ctrl Pts',(1.5550063106931,-0.0699135849125411,
11.3008800155484));
#267544=CARTESIAN_POINT('Ctrl Pts',(1.55652701283117,-0.0119854709137854,
11.3050185294789));
#267545=CARTESIAN_POINT('Ctrl Pts',(1.55482617711243,0.0457800061812131,
11.3091570434093));
#267546=CARTESIAN_POINT('Ctrl Pts',(1.55312202529163,0.103658108037933,
11.3133036261582));
#267547=CARTESIAN_POINT('Ctrl Pts',(1.54818382720234,0.161372418399441,
11.317450208907));
#267548=CARTESIAN_POINT('Ctrl Pts',(1.54007155928367,0.218540253238526,
11.3215967916559));
#267549=CARTESIAN_POINT('Ctrl Pts',(1.53239675336362,0.272625256551814,
11.3255197658659));
#267550=CARTESIAN_POINT('Ctrl Pts',(1.52188150498649,0.326220834726039,
11.3294427400758));
#267551=CARTESIAN_POINT('Ctrl Pts',(1.50861798182058,0.379014557672403,
11.3333657142857));
#267552=CARTESIAN_POINT('Ctrl Pts',(1.49459539648248,0.434829628530324,
11.3375131975713));
#267553=CARTESIAN_POINT('Ctrl Pts',(1.4774416706778,0.489982606874012,11.3416606808568));
#267554=CARTESIAN_POINT('Ctrl Pts',(1.45723671095245,0.544096883149017,
11.3458081641423));
#267555=CARTESIAN_POINT('Ctrl Pts',(1.45006554835835,0.563303171065727,
11.3472801926641));
#267556=CARTESIAN_POINT('Ctrl Pts',(1.4425104980916,0.582378687427456,11.3487522211859));
#267557=CARTESIAN_POINT('Ctrl Pts',(1.43457668357355,0.601306900797849,
11.3502242497077));
#267558=CARTESIAN_POINT('Origin',(0.,0.,-1.29405622560371));
#267559=CARTESIAN_POINT('',(1.4345767274609,0.601306796092946,12.1885981050115));
#267560=CARTESIAN_POINT('',(1.43231976391824,0.600353038565383,12.0501913886179));
#267561=CARTESIAN_POINT('',(1.43457668357355,0.601306900797845,-1.29405622560371));
#267562=CARTESIAN_POINT('',(-1.55549949371246,0.00125501405145053,11.7935273087615));
#267563=CARTESIAN_POINT('Ctrl Pts',(1.43457672746074,0.601306796093334,
12.1885981050115));
#267564=CARTESIAN_POINT('Ctrl Pts',(1.45158204059095,0.56073611467368,12.1856920715499));
#267565=CARTESIAN_POINT('Ctrl Pts',(1.46687680900277,0.519419120084027,
12.1827654785763));
#267566=CARTESIAN_POINT('Ctrl Pts',(1.49549833502048,0.430675741285502,
12.1764757733554));
#267567=CARTESIAN_POINT('Ctrl Pts',(1.50835993112976,0.383205376732718,
12.1731087244595));
#267568=CARTESIAN_POINT('Ctrl Pts',(1.52144025862211,0.323933824353823,
12.1688601916985));
#267569=CARTESIAN_POINT('Ctrl Pts',(1.52380293781175,0.312631055912539,
12.168048123122));
#267570=CARTESIAN_POINT('Ctrl Pts',(1.527323859471,0.294798308515377,12.1667634352161));
#267571=CARTESIAN_POINT('Ctrl Pts',(1.52856658848981,0.288285269302204,
12.1662935073094));
#267572=CARTESIAN_POINT('Ctrl Pts',(1.53078339948072,0.27624966941998,12.1654236909974));
#267573=CARTESIAN_POINT('Ctrl Pts',(1.5317693356534,0.270729379308468,12.1650241863763));
#267574=CARTESIAN_POINT('Ctrl Pts',(1.53388841843068,0.258482306658949,
12.1641365802209));
#267575=CARTESIAN_POINT('Ctrl Pts',(1.53500720214617,0.25175319197037,12.1636480320448));
#267576=CARTESIAN_POINT('Ctrl Pts',(1.53809174235351,0.232415329622212,
12.1622414807255));
#267577=CARTESIAN_POINT('Ctrl Pts',(1.53994660646182,0.219789727999229,
12.1613200021437));
#267578=CARTESIAN_POINT('Ctrl Pts',(1.55325386263287,0.120751532516686,
12.1540652905653));
#267579=CARTESIAN_POINT('Ctrl Pts',(1.55757745999443,0.0335535934348645,
12.1475073349953));
#267580=CARTESIAN_POINT('Ctrl Pts',(1.55140191647346,-0.145780576912626,
12.1337143431608));
#267581=CARTESIAN_POINT('Ctrl Pts',(1.54002114670295,-0.237559200622337,
12.1264887818188));
#267582=CARTESIAN_POINT('Ctrl Pts',(1.51674661293645,-0.345527624136952,
12.1180440353607));
#267583=CARTESIAN_POINT('Ctrl Pts',(1.512611826786,-0.363201236993375,12.1166640550951));
#267584=CARTESIAN_POINT('Ctrl Pts',(1.50152803910009,-0.407098978642287,
12.113248257347));
#267585=CARTESIAN_POINT('Ctrl Pts',(1.49420019446831,-0.433222860636483,
12.1112260707693));
#267586=CARTESIAN_POINT('Ctrl Pts',(1.48427072885522,-0.465363330377416,
12.1087620280064));
#267587=CARTESIAN_POINT('Ctrl Pts',(1.48231017142485,-0.471570976102156,
12.1082872406096));
#267588=CARTESIAN_POINT('Ctrl Pts',(1.47917134528659,-0.481296312540366,
12.1075453632342));
#267589=CARTESIAN_POINT('Ctrl Pts',(1.47801939612779,-0.484822312434049,
12.1072767953699));
#267590=CARTESIAN_POINT('Ctrl Pts',(1.47585614512653,-0.491364435052166,
12.1067792939064));
#267591=CARTESIAN_POINT('Ctrl Pts',(1.47484821326013,-0.494381550339857,
12.1065501761354));
#267592=CARTESIAN_POINT('Ctrl Pts',(1.47253101675,-0.501247625872965,12.1060294835219));
#267593=CARTESIAN_POINT('Ctrl Pts',(1.47121591472639,-0.505094556499425,
12.1057382558047));
#267594=CARTESIAN_POINT('Ctrl Pts',(1.46713426563989,-0.51688298107644,
12.1048472520649));
#267595=CARTESIAN_POINT('Ctrl Pts',(1.46431832670959,-0.524807408475454,
12.1042502918418));
#267596=CARTESIAN_POINT('Ctrl Pts',(1.42882683372046,-0.622175085968407,
12.0969354181743));
#267597=CARTESIAN_POINT('Ctrl Pts',(1.38806298754657,-0.708473954905476,
12.0906540911223));
#267598=CARTESIAN_POINT('Ctrl Pts',(1.27999483179161,-0.891613013130005,
12.0766529068945));
#267599=CARTESIAN_POINT('Ctrl Pts',(1.20909331202946,-0.985621329517202,
12.0689615847856));
#267600=CARTESIAN_POINT('Ctrl Pts',(1.11567365197953,-1.08406132597586,
12.059548017591));
#267601=CARTESIAN_POINT('Ctrl Pts',(1.10281419048869,-1.09714058715052,
12.0582664915187));
#267602=CARTESIAN_POINT('Ctrl Pts',(1.08451914954465,-1.11510166583624,
12.0564609634516));
#267603=CARTESIAN_POINT('Ctrl Pts',(1.0792755318422,-1.12017759037847,12.0559454456617));
#267604=CARTESIAN_POINT('Ctrl Pts',(1.07012639839581,-1.1289102549915,12.0550492329253));
#267605=CARTESIAN_POINT('Ctrl Pts',(1.06623734177724,-1.13258412582228,
12.0546692836316));
#267606=CARTESIAN_POINT('Ctrl Pts',(1.0581051801526,-1.14018731827884,12.0538768278583));
#267607=CARTESIAN_POINT('Ctrl Pts',(1.05385896777574,-1.14411317945634,
12.0534641822785));
#267608=CARTESIAN_POINT('Ctrl Pts',(1.04378462695974,-1.15332380435742,
12.0524877582621));
#267609=CARTESIAN_POINT('Ctrl Pts',(1.03793814955025,-1.15858816611638,
12.0519231324301));
#267610=CARTESIAN_POINT('Ctrl Pts',(1.01841055371683,-1.17590502458872,
12.0500437070847));
#267611=CARTESIAN_POINT('Ctrl Pts',(1.00455794571759,-1.18776090351007,
12.0487208354279));
#267612=CARTESIAN_POINT('Ctrl Pts',(0.971178085517181,-1.21532768558087,
12.0455560488411));
#267613=CARTESIAN_POINT('Ctrl Pts',(0.951473759381031,-1.23081510007813,
12.0437057400017));
#267614=CARTESIAN_POINT('Ctrl Pts',(0.810956354033189,-1.33586936761816,
12.0306297007018));
#267615=CARTESIAN_POINT('Ctrl Pts',(0.678090337225914,-1.40796866756557,
12.0187571993409));
#267616=CARTESIAN_POINT('Ctrl Pts',(0.499803415034939,-1.47354912648907,
12.0042721454798));
#267617=CARTESIAN_POINT('Ctrl Pts',(0.46210021024975,-1.4858043403824,12.0012908798576));
#267618=CARTESIAN_POINT('Ctrl Pts',(0.417566453962252,-1.49842008525386,
11.9978944336353));
#267619=CARTESIAN_POINT('Ctrl Pts',(0.411154858918472,-1.50019204823291,
11.9974084291805));
#267620=CARTESIAN_POINT('Ctrl Pts',(0.400771283344013,-1.50299017109325,
11.9966263804856));
#267621=CARTESIAN_POINT('Ctrl Pts',(0.396806355850358,-1.50404181888666,
11.9963289405809));
#267622=CARTESIAN_POINT('Ctrl Pts',(0.389756246341952,-1.50588195345002,
11.9958022111291));
#267623=CARTESIAN_POINT('Ctrl Pts',(0.386672761823889,-1.50667666247869,
11.9955725698963));
#267624=CARTESIAN_POINT('Ctrl Pts',(0.380016490173102,-1.50837040856132,
11.9950784358204));
#267625=CARTESIAN_POINT('Ctrl Pts',(0.376442946894745,-1.5092662226142,
11.9948141290924));
#267626=CARTESIAN_POINT('Ctrl Pts',(0.366485884725922,-1.51172468938218,
11.9940803176299));
#267627=CARTESIAN_POINT('Ctrl Pts',(0.360095493960803,-1.51325962066001,
11.9936123689661));
#267628=CARTESIAN_POINT('Ctrl Pts',(0.323021315754391,-1.52191644977286,
11.9909139031385));
#267629=CARTESIAN_POINT('Ctrl Pts',(0.292133916195586,-1.52814612673749,
11.9887305008976));
#267630=CARTESIAN_POINT('Ctrl Pts',(0.117250866611674,-1.55792096940701,
11.9766204561852));
#267631=CARTESIAN_POINT('Ctrl Pts',(-0.0293126270151572,-1.56205465328092,
11.9673618405338));
#267632=CARTESIAN_POINT('Ctrl Pts',(-0.223339881178667,-1.5401731539439,
11.9541926636323));
#267633=CARTESIAN_POINT('Ctrl Pts',(-0.272067078029229,-1.53231612997555,
11.9508140042706));
#267634=CARTESIAN_POINT('Ctrl Pts',(-0.331646544503724,-1.51977775977022,
11.9465524758041));
#267635=CARTESIAN_POINT('Ctrl Pts',(-0.342931000125702,-1.51727129610168,
11.9457395465846));
#267636=CARTESIAN_POINT('Ctrl Pts',(-0.360645349920121,-1.51312893814528,
11.9444537938638));
#267637=CARTESIAN_POINT('Ctrl Pts',(-0.36709467127881,-1.51157723974608,
11.9439836692483));
#267638=CARTESIAN_POINT('Ctrl Pts',(-0.378977260688168,-1.50863777317442,
11.94311366523));
#267639=CARTESIAN_POINT('Ctrl Pts',(-0.384413352792178,-1.50726177801037,
11.9427141707757));
#267640=CARTESIAN_POINT('Ctrl Pts',(-0.39644254662691,-1.50414761472061,
11.9418268051065));
#267641=CARTESIAN_POINT('Ctrl Pts',(-0.403031866176009,-1.50239543787667,
11.9413384885164));
#267642=CARTESIAN_POINT('Ctrl Pts',(-0.421905386813321,-1.49724365156291,
11.9399332645514));
#267643=CARTESIAN_POINT('Ctrl Pts',(-0.434159346805522,-1.49373637271134,
11.9390128919615));
#267644=CARTESIAN_POINT('Ctrl Pts',(-0.50412808035066,-1.47277651889407,
11.9337103078438));
#267645=CARTESIAN_POINT('Ctrl Pts',(-0.560824812037048,-1.45213275769606,
11.9292248993702));
#267646=CARTESIAN_POINT('Ctrl Pts',(-0.736672458551097,-1.37626893498022,
11.9146979491392));
#267647=CARTESIAN_POINT('Ctrl Pts',(-0.850092936226315,-1.30925151295815,
11.9043396242968));
#267648=CARTESIAN_POINT('Ctrl Pts',(-0.979530552695255,-1.20878670771401,
11.8919146289656));
#267649=CARTESIAN_POINT('Ctrl Pts',(-1.0046788888164,-1.18796722702655,
11.8894713610034));
#267650=CARTESIAN_POINT('Ctrl Pts',(-1.03387257401732,-1.16220795157377,
11.8866169625753));
#267651=CARTESIAN_POINT('Ctrl Pts',(-1.03856433069995,-1.15801725228821,
11.8861576538563));
#267652=CARTESIAN_POINT('Ctrl Pts',(-1.0461923680452,-1.15112020313484,
11.8854101312503));
#267653=CARTESIAN_POINT('Ctrl Pts',(-1.04914381880209,-1.14843086054787,
11.8851207102606));
#267654=CARTESIAN_POINT('Ctrl Pts',(-1.05442426453674,-1.14358200726755,
11.8846026190701));
#267655=CARTESIAN_POINT('Ctrl Pts',(-1.05675701877295,-1.14142671288253,
11.8843736426868));
#267656=CARTESIAN_POINT('Ctrl Pts',(-1.06129282473143,-1.13721013527475,
11.8839282317697));
#267657=CARTESIAN_POINT('Ctrl Pts',(-1.06349646771223,-1.13514960035315,
11.8837117442681));
#267658=CARTESIAN_POINT('Ctrl Pts',(-1.06984292218618,-1.1291805924429,
11.8830879467235));
#267659=CARTESIAN_POINT('Ctrl Pts',(-1.07397034085452,-1.12525570345684,
11.8826818672655));
#267660=CARTESIAN_POINT('Ctrl Pts',(-1.09331004413161,-1.10666164108773,
11.8807767078342));
#267661=CARTESIAN_POINT('Ctrl Pts',(-1.10824484635721,-1.09170523433954,
11.8792984012521));
#267662=CARTESIAN_POINT('Ctrl Pts',(-1.14984497320157,-1.04831105564144,
11.8751432625112));
#267663=CARTESIAN_POINT('Ctrl Pts',(-1.17575386580629,-1.01916773046994,
11.8725096059014));
#267664=CARTESIAN_POINT('Ctrl Pts',(-1.2359450804774,-0.946107782794096,
11.8661877984875));
#267665=CARTESIAN_POINT('Ctrl Pts',(-1.26901637162586,-0.901264703617742,
11.8625349099386));
#267666=CARTESIAN_POINT('Ctrl Pts',(-1.35490827479823,-0.770668540126365,
11.8522449840749));
#267667=CARTESIAN_POINT('Ctrl Pts',(-1.40190742087495,-0.681438298097991,
11.8455890219725));
#267668=CARTESIAN_POINT('Ctrl Pts',(-1.44702596352617,-0.571003745377852,
11.8373174846453));
#267669=CARTESIAN_POINT('Ctrl Pts',(-1.45378059771936,-0.553580470949328,
11.8360122478373));
#267670=CARTESIAN_POINT('Ctrl Pts',(-1.46275448749065,-0.529134833582684,
11.8341786028953));
#267671=CARTESIAN_POINT('Ctrl Pts',(-1.46524042696315,-0.522211499911363,
11.8336590352217));
#267672=CARTESIAN_POINT('Ctrl Pts',(-1.46945426056182,-0.510208983951964,
11.8327577288438));
#267673=CARTESIAN_POINT('Ctrl Pts',(-1.47120517393833,-0.505137967342879,
11.8323767565876));
#267674=CARTESIAN_POINT('Ctrl Pts',(-1.47478559083017,-0.494591786325402,
11.8315840356302));
#267675=CARTESIAN_POINT('Ctrl Pts',(-1.4766109150612,-0.489115301221913,
11.8311721561985));
#267676=CARTESIAN_POINT('Ctrl Pts',(-1.48083291888741,-0.476209051969776,
11.83020088385));
#267677=CARTESIAN_POINT('Ctrl Pts',(-1.48320421352683,-0.468771214659952,
11.8296406684617));
#267678=CARTESIAN_POINT('Ctrl Pts',(-1.48807310557398,-0.453092517158042,
11.8284586276957));
#267679=CARTESIAN_POINT('Ctrl Pts',(-1.49055845382412,-0.444848161535628,
11.8278364227426));
#267680=CARTESIAN_POINT('Ctrl Pts',(-1.50050315548437,-0.410840499083276,
11.8252668929519));
#267681=CARTESIAN_POINT('Ctrl Pts',(-1.50736358380977,-0.384908426387242,
11.8233004664417));
#267682=CARTESIAN_POINT('Ctrl Pts',(-1.54152424155393,-0.240811636859674,
11.812328617889));
#267683=CARTESIAN_POINT('Ctrl Pts',(-1.55559729728022,-0.119965461492677,
11.8029143200534));
#267684=CARTESIAN_POINT('Ctrl Pts',(-1.55549949371246,0.00125501405145053,
11.7935273087615));
#267685=CARTESIAN_POINT('Ctrl Pts',(-1.55549949256107,0.00125644030590557,
11.793527198316));
#267686=CARTESIAN_POINT('Ctrl Pts',(-1.55543827476008,0.0770453639235173,
11.7876582936078));
#267687=CARTESIAN_POINT('Ctrl Pts',(-1.5498380746614,0.152741214403535,
11.7818321000103));
#267688=CARTESIAN_POINT('Ctrl Pts',(-1.53791872494753,0.233275774147497,
11.775851467811));
#267689=CARTESIAN_POINT('Ctrl Pts',(-1.53706917578888,0.238809427517005,
11.7754416727001));
#267690=CARTESIAN_POINT('Ctrl Pts',(-1.53560595715123,0.248008884992335,
11.7747624411622));
#267691=CARTESIAN_POINT('Ctrl Pts',(-1.53500900097402,0.251677234498533,
11.7744921321761));
#267692=CARTESIAN_POINT('Ctrl Pts',(-1.53390385571041,0.258318225709805,
11.774003798637));
#267693=CARTESIAN_POINT('Ctrl Pts',(-1.5334001613056,0.261291580473112,
11.7737855291795));
#267694=CARTESIAN_POINT('Ctrl Pts',(-1.53234817902121,0.267393713056188,
11.7733383686218));
#267695=CARTESIAN_POINT('Ctrl Pts',(-1.53179896062522,0.27052224333861,
11.7731095425681));
#267696=CARTESIAN_POINT('Ctrl Pts',(-1.53053654987904,0.277586229865394,
11.7725938285275));
#267697=CARTESIAN_POINT('Ctrl Pts',(-1.52981776157695,0.281520625991666,
11.7723072606542));
#267698=CARTESIAN_POINT('Ctrl Pts',(-1.5276016529063,0.293391668079941,
11.7714445086636));
#267699=CARTESIAN_POINT('Ctrl Pts',(-1.52605765506662,0.301319633833431,
11.770870887273));
#267700=CARTESIAN_POINT('Ctrl Pts',(-1.51121779730803,0.374476351867772,
11.7655983195444));
#267701=CARTESIAN_POINT('Ctrl Pts',(-1.49380714537275,0.438810412518146,
11.7611122629698));
#267702=CARTESIAN_POINT('Ctrl Pts',(-1.45370456831319,0.556465673460301,
11.7528579526875));
#267703=CARTESIAN_POINT('Ctrl Pts',(-1.43205907766077,0.610014816728726,
11.7490800359503));
#267704=CARTESIAN_POINT('Ctrl Pts',(-1.37969947215315,0.72129729323195,
11.7409688696035));
#267705=CARTESIAN_POINT('Ctrl Pts',(-1.34822414890071,0.778544112823092,
11.7366347880482));
#267706=CARTESIAN_POINT('Ctrl Pts',(-1.29337733083871,0.864945141752854,
11.7296625366397));
#267707=CARTESIAN_POINT('Ctrl Pts',(-1.27239475243753,0.89552567501197,
11.727103408162));
#267708=CARTESIAN_POINT('Ctrl Pts',(-1.24421543415836,0.933602828860798,
11.7237805921658));
#267709=CARTESIAN_POINT('Ctrl Pts',(-1.23800781260553,0.941818950493964,
11.7230551921094));
#267710=CARTESIAN_POINT('Ctrl Pts',(-1.2278793428984,0.954951360685005,
11.7218817361772));
#267711=CARTESIAN_POINT('Ctrl Pts',(-1.22400938351031,0.959906666795737,
11.7214356867553));
#267712=CARTESIAN_POINT('Ctrl Pts',(-1.21657069394242,0.96931344098426,
11.720582603928));
#267713=CARTESIAN_POINT('Ctrl Pts',(-1.2130072985851,0.973769013789738,
11.7201757877134));
#267714=CARTESIAN_POINT('Ctrl Pts',(-1.20479492207426,0.983922519613457,
11.7192423373674));
#267715=CARTESIAN_POINT('Ctrl Pts',(-1.20012991525647,0.989607251349276,
11.7187150634646));
#267716=CARTESIAN_POINT('Ctrl Pts',(-1.18781758867245,1.00439583103383,
11.7173309918827));
#267717=CARTESIAN_POINT('Ctrl Pts',(-1.18010602177053,1.01344529804828,
11.7164715921882));
#267718=CARTESIAN_POINT('Ctrl Pts',(-1.11557181185831,1.08744033771526,
11.7093391710308));
#267719=CARTESIAN_POINT('Ctrl Pts',(-1.05354923356515,1.14763061224681,
11.7028457507348));
#267720=CARTESIAN_POINT('Ctrl Pts',(-0.920477103875181,1.25685294142414,
11.6896133472452));
#267721=CARTESIAN_POINT('Ctrl Pts',(-0.849689080786751,1.30575089228336,
11.6828990233396));
#267722=CARTESIAN_POINT('Ctrl Pts',(-0.745583186768539,1.36559700999893,
11.6736841640721));
#267723=CARTESIAN_POINT('Ctrl Pts',(-0.715382226259641,1.38165773382522,
11.6710835797942));
#267724=CARTESIAN_POINT('Ctrl Pts',(-0.667305151858946,1.40522534427645,
11.6670802130565));
#267725=CARTESIAN_POINT('Ctrl Pts',(-0.649777569366639,1.413415592456,11.6656481795102));
#267726=CARTESIAN_POINT('Ctrl Pts',(-0.627090073541303,1.42350565929894,
11.6638336137261));
#267727=CARTESIAN_POINT('Ctrl Pts',(-0.622067587670371,1.42570762822903,
11.6634343354659));
#267728=CARTESIAN_POINT('Ctrl Pts',(-0.614275784233497,1.4290747131572,
11.6628187614712));
#267729=CARTESIAN_POINT('Ctrl Pts',(-0.61151462909365,1.43025841500837,
11.6626013692067));
#267730=CARTESIAN_POINT('Ctrl Pts',(-0.60582242021112,1.43267915674698,
11.6621547690777));
#267731=CARTESIAN_POINT('Ctrl Pts',(-0.602891038114204,1.43391518839084,
11.6619256324742));
#267732=CARTESIAN_POINT('Ctrl Pts',(-0.596201654091225,1.43671166010294,
11.6614046688441));
#267733=CARTESIAN_POINT('Ctrl Pts',(-0.59244131047902,1.43826635268745,
11.6611131903921));
#267734=CARTESIAN_POINT('Ctrl Pts',(-0.582619488955455,1.44228207296019,
11.6603553305582));
#267735=CARTESIAN_POINT('Ctrl Pts',(-0.57654842669666,1.44471968303848,
11.6598903129488));
#267736=CARTESIAN_POINT('Ctrl Pts',(-0.5356247164776,1.46085202807501,11.6567775543695));
#267737=CARTESIAN_POINT('Ctrl Pts',(-0.500299239638685,1.47332404016643,
11.6541966090801));
#267738=CARTESIAN_POINT('Ctrl Pts',(-0.455800175436651,1.48724933807806,
11.6510349228867));
#267739=CARTESIAN_POINT('Ctrl Pts',(-0.447021619980684,1.48991143046835,
11.6504154678147));
#267740=CARTESIAN_POINT('Ctrl Pts',(-0.352900817635657,1.51754675641406,
11.6438143804556));
#267741=CARTESIAN_POINT('Ctrl Pts',(-0.265586708613,1.53523697968682,11.6380369984889));
#267742=CARTESIAN_POINT('Ctrl Pts',(-0.118576690159297,1.55209726425564,
11.6282520010717));
#267743=CARTESIAN_POINT('Ctrl Pts',(-0.059587436677704,1.55547893964097,
11.6243123453095));
#267744=CARTESIAN_POINT('Ctrl Pts',(0.0327683210596626,1.55551173349886,
11.6180033995987));
#267745=CARTESIAN_POINT('Ctrl Pts',(0.0660784657661782,1.55445291811311,
11.6156998037777));
#267746=CARTESIAN_POINT('Ctrl Pts',(0.109642075689366,1.55166546088532,
11.6126379520989));
#267747=CARTESIAN_POINT('Ctrl Pts',(0.119950130040805,1.55090265471277,
11.6119098601358));
#267748=CARTESIAN_POINT('Ctrl Pts',(0.136523469858874,1.54950999724567,
11.6107330983032));
#267749=CARTESIAN_POINT('Ctrl Pts',(0.142793996735838,1.54894472521255,
11.6102864556283));
#267750=CARTESIAN_POINT('Ctrl Pts',(0.154737828945701,1.5477948769901,11.6094329311594));
#267751=CARTESIAN_POINT('Ctrl Pts',(0.160411702453959,1.54721713442772,
11.6090262704917));
#267752=CARTESIAN_POINT('Ctrl Pts',(0.173377735378919,1.54582477967243,
11.608094158825));
#267753=CARTESIAN_POINT('Ctrl Pts',(0.180667516446653,1.54498975195845,
11.607568074564));
#267754=CARTESIAN_POINT('Ctrl Pts',(0.199699069317484,1.54267319730258,
11.60618916652));
#267755=CARTESIAN_POINT('Ctrl Pts',(0.211430122289766,1.54110921123343,
11.6053337722227));
#267756=CARTESIAN_POINT('Ctrl Pts',(0.329677276358081,1.52396896471315,
11.5966547709806));
#267757=CARTESIAN_POINT('Ctrl Pts',(0.434298895567302,1.49751253877421,
11.5884785693645));
#267758=CARTESIAN_POINT('Ctrl Pts',(0.612358274561361,1.43224572763298,
11.5738061700983));
#267759=CARTESIAN_POINT('Ctrl Pts',(0.687032838892333,1.39796185575089,
11.5674035894142));
#267760=CARTESIAN_POINT('Ctrl Pts',(0.78851268001489,1.34126715350211,11.5585811930183));
#267761=CARTESIAN_POINT('Ctrl Pts',(0.817813109994618,1.32360567811974,
11.5560196353514));
#267762=CARTESIAN_POINT('Ctrl Pts',(0.852151860316267,1.30133111890856,
11.5530205637455));
#267763=CARTESIAN_POINT('Ctrl Pts',(0.85777006686341,1.29763476791207,11.5525299853492));
#267764=CARTESIAN_POINT('Ctrl Pts',(0.866456394970757,1.29183876079708,
11.5517718749555));
#267765=CARTESIAN_POINT('Ctrl Pts',(0.869541167959608,1.28976440728287,
11.551502721495));
#267766=CARTESIAN_POINT('Ctrl Pts',(0.87525113978003,1.28589494353712,11.5510046946817));
#267767=CARTESIAN_POINT('Ctrl Pts',(0.87787824824078,1.28410285612381,11.5507756336121));
#267768=CARTESIAN_POINT('Ctrl Pts',(0.883842210878091,1.28000766958513,
11.5502557832441));
#267769=CARTESIAN_POINT('Ctrl Pts',(0.887175565891035,1.27769957510366,
11.5499653365535));
#267770=CARTESIAN_POINT('Ctrl Pts',(0.895823995414858,1.271661033543,11.5492119366804));
#267771=CARTESIAN_POINT('Ctrl Pts',(0.901124875053817,1.26791024069463,
11.548750321127));
#267772=CARTESIAN_POINT('Ctrl Pts',(0.936027864489046,1.24288414308738,
11.5457108299805));
#267773=CARTESIAN_POINT('Ctrl Pts',(0.964900622201271,1.22060496353759,
11.5431962190013));
#267774=CARTESIAN_POINT('Ctrl Pts',(1.00555814454436,1.18688696401468,11.539611120718));
#267775=CARTESIAN_POINT('Ctrl Pts',(1.01798471773903,1.17624614493162,11.5385090748479));
#267776=CARTESIAN_POINT('Ctrl Pts',(1.0564829365996,1.14221311911377,11.5350665459296));
#267777=CARTESIAN_POINT('Ctrl Pts',(1.08193435620354,1.11813470954132,11.5327486011254));
#267778=CARTESIAN_POINT('Ctrl Pts',(1.16259766892338,1.03648745647425,11.5251800595548));
#267779=CARTESIAN_POINT('Ctrl Pts',(1.21419561020457,0.975534706193046,
11.51996903195));
#267780=CARTESIAN_POINT('Ctrl Pts',(1.28327766639522,0.879909085401753,
11.5120538558977));
#267781=CARTESIAN_POINT('Ctrl Pts',(1.30451201813904,0.848109434627519,
11.509461091908));
#267782=CARTESIAN_POINT('Ctrl Pts',(1.33337797176438,0.801228290341209,
11.5056682333747));
#267783=CARTESIAN_POINT('Ctrl Pts',(1.34196994117998,0.786752965749487,
11.5045010874051));
#267784=CARTESIAN_POINT('Ctrl Pts',(1.35694320883465,0.760567638537831,
11.5023946877119));
#267785=CARTESIAN_POINT('Ctrl Pts',(1.36341210969027,0.748909476842886,
11.5014585941772));
#267786=CARTESIAN_POINT('Ctrl Pts',(1.37301943071061,0.731058181902767,
11.5000270684353));
#267787=CARTESIAN_POINT('Ctrl Pts',(1.37626768900546,0.724924594567943,
11.4995355338475));
#267788=CARTESIAN_POINT('Ctrl Pts',(1.38209299733483,0.71374456396407,11.498640073186));
#267789=CARTESIAN_POINT('Ctrl Pts',(1.38468374345685,0.708705358325314,
11.4982366378726));
#267790=CARTESIAN_POINT('Ctrl Pts',(1.39021051287214,0.697809359022167,
11.49736463231));
#267791=CARTESIAN_POINT('Ctrl Pts',(1.39313717239279,0.6919479663299,11.496895743849));
#267792=CARTESIAN_POINT('Ctrl Pts',(1.40096698220504,0.676015700266734,
11.4956216520789));
#267793=CARTESIAN_POINT('Ctrl Pts',(1.40579843873033,0.665910241467936,
11.494813982745));
#267794=CARTESIAN_POINT('Ctrl Pts',(1.41888691716792,0.637757044987237,
11.4925646705203));
#267795=CARTESIAN_POINT('Ctrl Pts',(1.42690708914345,0.619604747661188,
11.4911152672628));
#267796=CARTESIAN_POINT('Ctrl Pts',(1.4345766883817,0.601306889326732,11.4896545509914));
#267797=CARTESIAN_POINT('',(-1.55549976470477,-0.000855571976022074,11.6559437432627));
#267798=CARTESIAN_POINT('Ctrl Pts',(1.43457668357355,0.601306900797849,
11.3502242497077));
#267799=CARTESIAN_POINT('Ctrl Pts',(1.41226865130244,0.654528613221381,
11.3543632498939));
#267800=CARTESIAN_POINT('Ctrl Pts',(1.38696253154565,0.706584446038729,
11.3585022500801));
#267801=CARTESIAN_POINT('Ctrl Pts',(1.35880582970744,0.757117538532215,
11.3626412502663));
#267802=CARTESIAN_POINT('Ctrl Pts',(1.33067329122353,0.80760726483087,11.3667766984695));
#267803=CARTESIAN_POINT('Ctrl Pts',(1.29969527071767,0.856576387070337,
11.3709121466726));
#267804=CARTESIAN_POINT('Ctrl Pts',(1.26606623022454,0.903690517093667,
11.3750475948758));
#267805=CARTESIAN_POINT('Ctrl Pts',(1.23245312122716,0.950782327165226,
11.3791810839426));
#267806=CARTESIAN_POINT('Ctrl Pts',(1.19619178468126,0.996020464185237,
11.3833145730094));
#267807=CARTESIAN_POINT('Ctrl Pts',(1.15752003742474,1.03909942400149,11.3874480620763));
#267808=CARTESIAN_POINT('Ctrl Pts',(1.11885174464237,1.08217453565562,11.3915811819063));
#267809=CARTESIAN_POINT('Ctrl Pts',(1.07777381780718,1.12309046680136,11.3957143017364));
#267810=CARTESIAN_POINT('Ctrl Pts',(1.03456293596234,1.16157642087509,11.3998474215664));
#267811=CARTESIAN_POINT('Ctrl Pts',(0.991308894315491,1.20010081540842,
11.4039846696305));
#267812=CARTESIAN_POINT('Ctrl Pts',(0.945918034130839,1.23619004022242,
11.4081219176946));
#267813=CARTESIAN_POINT('Ctrl Pts',(0.898701275092304,1.26961264492264,
11.4122591657587));
#267814=CARTESIAN_POINT('Ctrl Pts',(0.851459226604644,1.30305315087824,
11.4163986297462));
#267815=CARTESIAN_POINT('Ctrl Pts',(0.802389773687353,1.33382391591129,
11.4205380937338));
#267816=CARTESIAN_POINT('Ctrl Pts',(0.75183136726111,1.36173780339766,11.4246775577214));
#267817=CARTESIAN_POINT('Ctrl Pts',(0.701180318458949,1.38970283982327,
11.4288246067933));
#267818=CARTESIAN_POINT('Ctrl Pts',(0.649035338870661,1.41480032145479,
11.4329716558652));
#267819=CARTESIAN_POINT('Ctrl Pts',(0.595756836526051,1.43689040700134,
11.4371187049372));
#267820=CARTESIAN_POINT('Ctrl Pts',(0.564244746428948,1.44995580365031,
11.4395715175772));
#267821=CARTESIAN_POINT('Ctrl Pts',(0.532336468268933,1.46197007338129,
11.4420243302172));
#267822=CARTESIAN_POINT('Ctrl Pts',(0.500108798853076,1.47291257015131,
11.4444771428572));
#267823=CARTESIAN_POINT('Ctrl Pts',(0.445607664972614,1.49141773953708,
11.4486251644952));
#267824=CARTESIAN_POINT('Ctrl Pts',(0.389963628830703,1.50693267352437,
11.4527731861331));
#267825=CARTESIAN_POINT('Ctrl Pts',(0.33353654704593,1.51932011827155,11.456921207771));
#267826=CARTESIAN_POINT('Ctrl Pts',(0.277209795174015,1.53168553757966,
11.4610618540382));
#267827=CARTESIAN_POINT('Ctrl Pts',(0.220103265647797,1.54093439430489,
11.4652025003054));
#267828=CARTESIAN_POINT('Ctrl Pts',(0.162592671480833,1.54697895046466,
11.4693431465725));
#267829=CARTESIAN_POINT('Ctrl Pts',(0.105139285689614,1.55301749383243,
11.4734796739526));
#267830=CARTESIAN_POINT('Ctrl Pts',(0.0472831469573348,1.55585799774962,
11.4776162013326));
#267831=CARTESIAN_POINT('Ctrl Pts',(-0.0105908529907744,1.55546394488362,
11.4817527287126));
#267832=CARTESIAN_POINT('Ctrl Pts',(-0.0684295321422135,1.5550701325101,
11.4858867315489));
#267833=CARTESIAN_POINT('Ctrl Pts',(-0.126285531165076,1.55144568003564,
11.4900207343852));
#267834=CARTESIAN_POINT('Ctrl Pts',(-0.183772085437503,1.54460612151252,
11.4941547372215));
#267835=CARTESIAN_POINT('Ctrl Pts',(-0.241245654360086,1.53776810794302,
11.4982878062486));
#267836=CARTESIAN_POINT('Ctrl Pts',(-0.298349427291833,1.52771649160558,
11.5024208752757));
#267837=CARTESIAN_POINT('Ctrl Pts',(-0.354702117886104,1.51451862239033,
11.5065539443028));
#267838=CARTESIAN_POINT('Ctrl Pts',(-0.411105744465599,1.50130882390491,
11.5106907491222));
#267839=CARTESIAN_POINT('Ctrl Pts',(-0.466756423426883,1.48494720733713,
11.5148275539415));
#267840=CARTESIAN_POINT('Ctrl Pts',(-0.521284767950481,1.46555192357788,
11.5189643587608));
#267841=CARTESIAN_POINT('Ctrl Pts',(-0.575835640730655,1.44614862670301,
11.5231028726913));
#267842=CARTESIAN_POINT('Ctrl Pts',(-0.629262772949708,1.42370936492172,
11.5272413866217));
#267843=CARTESIAN_POINT('Ctrl Pts',(-0.681216667352735,1.39840055138749,
11.5313799005522));
#267844=CARTESIAN_POINT('Ctrl Pts',(-0.733271855733956,1.37304239351756,
11.535526483301));
#267845=CARTESIAN_POINT('Ctrl Pts',(-0.783847609271613,1.34480375730816,
11.5396730660499));
#267846=CARTESIAN_POINT('Ctrl Pts',(-0.832619777979761,1.31389670648683,
11.5438196487988));
#267847=CARTESIAN_POINT('Ctrl Pts',(-0.878761859687165,1.28465634867402,
11.5477426230087));
#267848=CARTESIAN_POINT('Ctrl Pts',(-0.923289576558216,1.25302821438636,
11.5516655972186));
#267849=CARTESIAN_POINT('Ctrl Pts',(-0.965956055322932,1.21922481486597,
11.5555885714286));
#267850=CARTESIAN_POINT('Ctrl Pts',(-1.0114338992033,1.18319405323478,11.5597700369217));
#267851=CARTESIAN_POINT('Ctrl Pts',(-1.05500203629591,1.14452862400283,
11.5639515024147));
#267852=CARTESIAN_POINT('Ctrl Pts',(-1.09633493644636,1.10346271215984,
11.5681329679078));
#267853=CARTESIAN_POINT('Ctrl Pts',(-1.13676231568373,1.06329647205179,
11.5722228258815));
#267854=CARTESIAN_POINT('Ctrl Pts',(-1.17505098592424,1.02083424380586,
11.5763126838553));
#267855=CARTESIAN_POINT('Ctrl Pts',(-1.21092769215217,0.976337223698363,
11.580402541829));
#267856=CARTESIAN_POINT('Ctrl Pts',(-1.2467695817939,0.931883385769461,
11.5844884307958));
#267857=CARTESIAN_POINT('Ctrl Pts',(-1.28020380750838,0.885399079675038,
11.5885743197627));
#267858=CARTESIAN_POINT('Ctrl Pts',(-1.3109950352659,0.837181143784403,
11.5926602087296));
#267859=CARTESIAN_POINT('Ctrl Pts',(-1.34176891796273,0.788990369624073,
11.5967437960671));
#267860=CARTESIAN_POINT('Ctrl Pts',(-1.36990246527459,0.739068350541516,
11.6008273834047));
#267861=CARTESIAN_POINT('Ctrl Pts',(-1.39520305183881,0.687741735057339,
11.6049109707423));
#267862=CARTESIAN_POINT('Ctrl Pts',(-1.42155159810529,0.634289152076536,
11.6091637017856));
#267863=CARTESIAN_POINT('Ctrl Pts',(-1.4448270044127,0.579313576673076,
11.613416432829));
#267864=CARTESIAN_POINT('Ctrl Pts',(-1.46486537546916,0.523210934281381,
11.6176691638724));
#267865=CARTESIAN_POINT('Ctrl Pts',(-1.48411993315168,0.46930278171604,
11.6217555466902));
#267866=CARTESIAN_POINT('Ctrl Pts',(-1.50038591659663,0.414354664111797,
11.6258419295081));
#267867=CARTESIAN_POINT('Ctrl Pts',(-1.51356867128985,0.35873406207089,
11.6299283123259));
#267868=CARTESIAN_POINT('Ctrl Pts',(-1.52675850798256,0.303083579698876,
11.6340168904179));
#267869=CARTESIAN_POINT('Ctrl Pts',(-1.53686172842426,0.246760420744384,
11.63810546851));
#267870=CARTESIAN_POINT('Ctrl Pts',(-1.54383509081983,0.190140638353125,
11.642194046602));
#267871=CARTESIAN_POINT('Ctrl Pts',(-1.55081899955752,0.133435225592786,
11.6462888081592));
#267872=CARTESIAN_POINT('Ctrl Pts',(-1.55466358298914,0.076432827428913,
11.6503835697164));
#267873=CARTESIAN_POINT('Ctrl Pts',(-1.55537762736568,0.0195111837242169,
11.6544783312735));
#267874=CARTESIAN_POINT('Ctrl Pts',(-1.55546280686274,0.0127209096986689,
11.6549668019366));
#267875=CARTESIAN_POINT('Ctrl Pts',(-1.55550349795349,0.00593177925652502,
11.6554552725996));
#267876=CARTESIAN_POINT('Ctrl Pts',(-1.55549976470477,-0.000855571976022074,
11.6559437432627));
#267877=CARTESIAN_POINT('Ctrl Pts',(-1.55745359230764,-0.000857079788619507,
11.6559437743963));
#267878=CARTESIAN_POINT('Ctrl Pts',(-1.55778429450171,-0.0507394822719253,
11.6595291829309));
#267879=CARTESIAN_POINT('Ctrl Pts',(-1.53298428568849,-0.61557232946888,
11.7001517343226));
#267880=CARTESIAN_POINT('Ctrl Pts',(-0.843887408158428,-1.63323853987322,
11.7778114285714));
#267881=CARTESIAN_POINT('Ctrl Pts',(0.914119296723934,-1.59499216209124,
11.8889228571429));
#267882=CARTESIAN_POINT('Ctrl Pts',(1.66724862260157,-0.371308863304057,
11.9797161771584));
#267883=CARTESIAN_POINT('Ctrl Pts',(1.52345377446436,0.384508855915243,
12.0334723543167));
#267884=CARTESIAN_POINT('Ctrl Pts',(1.43231976391824,0.600353038565383,
12.0501913886179));
#267885=CARTESIAN_POINT('Origin',(0.,0.,-1.29405622560371));
#267886=CARTESIAN_POINT('',(1.43457668357408,0.601306900796593,12.8868295753666));
#267887=CARTESIAN_POINT('',(1.43457658310325,0.601307140496281,12.749909041778));
#267888=CARTESIAN_POINT('',(1.43457668357355,0.601306900797845,-1.29405622560371));
#267889=CARTESIAN_POINT('Ctrl Pts',(1.43457668357408,0.601306900796593,
12.8868295753666));
#267890=CARTESIAN_POINT('Ctrl Pts',(1.43630803386767,0.597176306654078,
12.8865025089062));
#267891=CARTESIAN_POINT('Ctrl Pts',(1.43802156797068,0.593038178282737,
12.8861764329062));
#267892=CARTESIAN_POINT('Ctrl Pts',(1.4410954682343,0.585523145905051,12.8855872095809));
#267893=CARTESIAN_POINT('Ctrl Pts',(1.44246188697645,0.582148785377978,
12.8853237112177));
#267894=CARTESIAN_POINT('Ctrl Pts',(1.44500388949606,0.575807427749637,
12.884830574421));
#267895=CARTESIAN_POINT('Ctrl Pts',(1.44618217616257,0.572841643151802,
12.8846007829389));
#267896=CARTESIAN_POINT('Ctrl Pts',(1.44885376338895,0.56605639265347,12.8840769538399));
#267897=CARTESIAN_POINT('Ctrl Pts',(1.45034109317028,0.562234632383855,
12.883783275206));
#267898=CARTESIAN_POINT('Ctrl Pts',(1.45425306680089,0.552063814954083,
12.8830052188027));
#267899=CARTESIAN_POINT('Ctrl Pts',(1.45665128087403,0.545704579846847,
12.8825223643004));
#267900=CARTESIAN_POINT('Ctrl Pts',(1.47397588503568,0.498837638219103,
12.8789888702182));
#267901=CARTESIAN_POINT('Ctrl Pts',(1.48725353464925,0.457735361294269,
12.8760272387744));
#267902=CARTESIAN_POINT('Ctrl Pts',(1.52863014621185,0.308706085240282,
12.8655946795542));
#267903=CARTESIAN_POINT('Ctrl Pts',(1.54682145612325,0.198383237105034,
12.8584125802658));
#267904=CARTESIAN_POINT('Ctrl Pts',(1.55660052978561,0.0239302771643157,
12.8467669169518));
#267905=CARTESIAN_POINT('Ctrl Pts',(1.5562866564253,-0.0393471128764939,
12.8424887910578));
#267906=CARTESIAN_POINT('Ctrl Pts',(1.5510677913964,-0.118432824939837,
12.836973522802));
#267907=CARTESIAN_POINT('Ctrl Pts',(1.54976385617614,-0.134423153233905,
12.8358499251551));
#267908=CARTESIAN_POINT('Ctrl Pts',(1.54749025593567,-0.157829087226317,
12.8341915418417));
#267909=CARTESIAN_POINT('Ctrl Pts',(1.54671403800262,-0.165262803190695,
12.8336628091812));
#267910=CARTESIAN_POINT('Ctrl Pts',(1.54524911786642,-0.178376418299592,
12.8327263659454));
#267911=CARTESIAN_POINT('Ctrl Pts',(1.54458258992354,-0.184058697639912,
12.8323193587251));
#267912=CARTESIAN_POINT('Ctrl Pts',(1.54321848998383,-0.195158335282571,
12.8315218439678));
#267913=CARTESIAN_POINT('Ctrl Pts',(1.54252370083522,-0.200575957220771,
12.8311314297177));
#267914=CARTESIAN_POINT('Ctrl Pts',(1.54056908483936,-0.215205946379475,
12.8300739494174));
#267915=CARTESIAN_POINT('Ctrl Pts',(1.5392551837623,-0.224410732376552,
12.8294051893792));
#267916=CARTESIAN_POINT('Ctrl Pts',(1.53399549161855,-0.259036418208121,
12.8268762261096));
#267917=CARTESIAN_POINT('Ctrl Pts',(1.529502010323,-0.284368577793769,12.824998908354));
#267918=CARTESIAN_POINT('Ctrl Pts',(1.52398551699384,-0.311532305912606,
12.8229551370473));
#267919=CARTESIAN_POINT('Ctrl Pts',(1.52358452857621,-0.313487508284854,
12.8228078577438));
#267920=CARTESIAN_POINT('Ctrl Pts',(1.52198148458363,-0.321228154025933,
12.8222240969608));
#267921=CARTESIAN_POINT('Ctrl Pts',(1.52075024302148,-0.32700743568416,
12.8217867421423));
#267922=CARTESIAN_POINT('Ctrl Pts',(1.48978889966949,-0.468378321187837,
12.8110511573063));
#267923=CARTESIAN_POINT('Ctrl Pts',(1.44207641665855,-0.599375531415827,
12.8001811203944));
#267924=CARTESIAN_POINT('Ctrl Pts',(1.35950012202056,-0.756879461573442,
12.7864889022573));
#267925=CARTESIAN_POINT('Ctrl Pts',(1.34005725765543,-0.790793342407725,
12.7835056388749));
#267926=CARTESIAN_POINT('Ctrl Pts',(1.31184820494531,-0.835963784946403,
12.7795150063747));
#267927=CARTESIAN_POINT('Ctrl Pts',(1.30417580189023,-0.847883644583293,
12.7784602780913));
#267928=CARTESIAN_POINT('Ctrl Pts',(1.2907299311169,-0.86815872653338,12.7766654847704));
#267929=CARTESIAN_POINT('Ctrl Pts',(1.28503574504065,-0.876565159090118,
12.7759211035816));
#267930=CARTESIAN_POINT('Ctrl Pts',(1.27676295003602,-0.88852455059335,
12.7748624561391));
#267931=CARTESIAN_POINT('Ctrl Pts',(1.27425114019557,-0.892123052373519,
12.7745439615408));
#267932=CARTESIAN_POINT('Ctrl Pts',(1.26986933526257,-0.898344308237728,
12.7739934790093));
#267933=CARTESIAN_POINT('Ctrl Pts',(1.26800637511454,-0.900971951995269,
12.7737610209342));
#267934=CARTESIAN_POINT('Ctrl Pts',(1.26408617194305,-0.906465025305012,
12.7732751896025));
#267935=CARTESIAN_POINT('Ctrl Pts',(1.26202733731474,-0.909329254309723,
12.7730219282269));
#267936=CARTESIAN_POINT('Ctrl Pts',(1.25652115694188,-0.916934672921012,
12.772349536477));
#267937=CARTESIAN_POINT('Ctrl Pts',(1.253056677899,-0.921663483686224,12.7719315641689));
#267938=CARTESIAN_POINT('Ctrl Pts',(1.2379373998346,-0.942057573383563,
12.7701288464441));
#267939=CARTESIAN_POINT('Ctrl Pts',(1.22601431547814,-0.957523090808126,
12.7687614858435));
#267940=CARTESIAN_POINT('Ctrl Pts',(1.19976006815747,-0.990282907704105,
12.7658543679145));
#267941=CARTESIAN_POINT('Ctrl Pts',(1.18533915034077,-1.00749970940668,
12.7643198488392));
#267942=CARTESIAN_POINT('Ctrl Pts',(1.07182044809957,-1.13721408385789,
12.7526525542086));
#267943=CARTESIAN_POINT('Ctrl Pts',(0.957300501113441,-1.23516669992363,
12.7431369642283));
#267944=CARTESIAN_POINT('Ctrl Pts',(0.797890359839658,-1.33582968469954,
12.7303078577488));
#267945=CARTESIAN_POINT('Ctrl Pts',(0.764502373532948,-1.3552142526981,
12.7276460873808));
#267946=CARTESIAN_POINT('Ctrl Pts',(0.721264224917749,-1.37821114234835,
12.724211289038));
#267947=CARTESIAN_POINT('Ctrl Pts',(0.712049719733451,-1.38299429585679,
12.7234800155666));
#267948=CARTESIAN_POINT('Ctrl Pts',(0.697162481163887,-1.39053388717173,
12.72229934632));
#267949=CARTESIAN_POINT('Ctrl Pts',(0.691519545084185,-1.39334874785641,
12.7218520023628));
#267950=CARTESIAN_POINT('Ctrl Pts',(0.680742908817956,-1.3986428573648,
12.7209979498659));
#267951=CARTESIAN_POINT('Ctrl Pts',(0.675612377307309,-1.40112835400685,
12.7205914670816));
#267952=CARTESIAN_POINT('Ctrl Pts',(0.663864638601112,-1.4067400440466,
12.719660908738));
#267953=CARTESIAN_POINT('Ctrl Pts',(0.65723884301869,-1.40984783212392,
12.7191362074789));
#267954=CARTESIAN_POINT('Ctrl Pts',(0.639899226007944,-1.41783207545981,
12.7177632945459));
#267955=CARTESIAN_POINT('Ctrl Pts',(0.629151724697672,-1.42263379222711,
12.7169125487042));
#267956=CARTESIAN_POINT('Ctrl Pts',(0.545226050390564,-1.45899269118711,
12.7102695031969));
#267957=CARTESIAN_POINT('Ctrl Pts',(0.469787643090025,-1.48500058473315,
12.7042906659553));
#267958=CARTESIAN_POINT('Ctrl Pts',(0.289643495969261,-1.53200218576918,
12.6900219387361));
#267959=CARTESIAN_POINT('Ctrl Pts',(0.184102071200889,-1.54823434186491,
12.6816588031931));
#267960=CARTESIAN_POINT('Ctrl Pts',(0.0402743406402426,-1.55543075149596,
12.6707003078938));
#267961=CARTESIAN_POINT('Ctrl Pts',(0.00275707545095223,-1.55594981291119,
12.6678845757238));
#267962=CARTESIAN_POINT('Ctrl Pts',(-0.0416357872520772,-1.55495794351881,
12.6646297598777));
#267963=CARTESIAN_POINT('Ctrl Pts',(-0.0485247956830509,-1.55475821073372,
12.6641268709908));
#267964=CARTESIAN_POINT('Ctrl Pts',(-0.059163306185866,-1.55437898860908,
12.6633539041798));
#267965=CARTESIAN_POINT('Ctrl Pts',(-0.0629137507359866,-1.55423170660157,
12.663082103881));
#267966=CARTESIAN_POINT('Ctrl Pts',(-0.0698376003415167,-1.55393470000887,
12.6625816545831));
#267967=CARTESIAN_POINT('Ctrl Pts',(-0.073011059152898,-1.55378882990267,
12.662352801957));
#267968=CARTESIAN_POINT('Ctrl Pts',(-0.0801860862681806,-1.55343699441159,
12.6618365423015));
#267969=CARTESIAN_POINT('Ctrl Pts',(-0.0841873142209091,-1.55322528988408,
12.6615494583852));
#267970=CARTESIAN_POINT('Ctrl Pts',(-0.0960276280279973,-1.55255293201059,
12.6607022171312));
#267971=CARTESIAN_POINT('Ctrl Pts',(-0.103864250696702,-1.55204836790932,
12.6601444332513));
#267972=CARTESIAN_POINT('Ctrl Pts',(-0.167335707890344,-1.54747882997415,
12.6556483679543));
#267973=CARTESIAN_POINT('Ctrl Pts',(-0.222726367074404,-1.54048258065713,
12.6518588651193));
#267974=CARTESIAN_POINT('Ctrl Pts',(-0.410811867645751,-1.50636497978527,
12.6390875249788));
#267975=CARTESIAN_POINT('Ctrl Pts',(-0.540267839730735,-1.46492782110384,
12.6304116167841));
#267976=CARTESIAN_POINT('Ctrl Pts',(-0.695402089092766,-1.39186942844944,
12.618718676366));
#267977=CARTESIAN_POINT('Ctrl Pts',(-0.727527365184992,-1.37535019306935,
12.6162243236083));
#267978=CARTESIAN_POINT('Ctrl Pts',(-0.767910920675648,-1.35277352142793,
12.6129782187025));
#267979=CARTESIAN_POINT('Ctrl Pts',(-0.776726207233167,-1.34773134290876,
12.6122627026434));
#267980=CARTESIAN_POINT('Ctrl Pts',(-0.790891172584244,-1.33944411686298,
12.6111013830782));
#267981=CARTESIAN_POINT('Ctrl Pts',(-0.796271857019717,-1.33625241504336,
12.6106575106051));
#267982=CARTESIAN_POINT('Ctrl Pts',(-0.806529278766559,-1.33008398787893,
12.6098060067984));
#267983=CARTESIAN_POINT('Ctrl Pts',(-0.811409166832632,-1.32711267596163,
12.6093985780495));
#267984=CARTESIAN_POINT('Ctrl Pts',(-0.822480755730538,-1.32028741035984,
12.6084688028307));
#267985=CARTESIAN_POINT('Ctrl Pts',(-0.828661903223299,-1.3164166841432,
12.6079458460296));
#267986=CARTESIAN_POINT('Ctrl Pts',(-0.844899437422479,-1.30608882318844,
12.6065616640811));
#267987=CARTESIAN_POINT('Ctrl Pts',(-0.854908847816922,-1.29955912543796,
12.6056977661122));
#267988=CARTESIAN_POINT('Ctrl Pts',(-0.943520601362143,-1.24028597035465,
12.5979525768149));
#267989=CARTESIAN_POINT('Ctrl Pts',(-1.01721558217201,-1.18059580870191,
12.5908033683006));
#267990=CARTESIAN_POINT('Ctrl Pts',(-1.1513053586924,-1.05006382595058,
12.5763755618778));
#267991=CARTESIAN_POINT('Ctrl Pts',(-1.21170373049357,-0.979751296507427,
12.569134214758));
#267992=CARTESIAN_POINT('Ctrl Pts',(-1.28660532725679,-0.87495416411567,
12.5593411702552));
#267993=CARTESIAN_POINT('Ctrl Pts',(-1.30667574881821,-0.844687559676874,
12.5566180522283));
#267994=CARTESIAN_POINT('Ctrl Pts',(-1.32924517351526,-0.807919682708667,
12.5534561345351));
#267995=CARTESIAN_POINT('Ctrl Pts',(-1.33278165642756,-0.802072319646806,
12.552957548061));
#267996=CARTESIAN_POINT('Ctrl Pts',(-1.33819431581306,-0.792988156403571,
12.5521897705286));
#267997=CARTESIAN_POINT('Ctrl Pts',(-1.34009748406117,-0.789767672853815,
12.5519188926589));
#267998=CARTESIAN_POINT('Ctrl Pts',(-1.34359594194522,-0.783798630843553,
12.5514192962093));
#267999=CARTESIAN_POINT('Ctrl Pts',(-1.34519441523558,-0.781052069010605,
12.551190379527));
#268000=CARTESIAN_POINT('Ctrl Pts',(-1.34879739290478,-0.774817415126494,
12.5506729072732));
#268001=CARTESIAN_POINT('Ctrl Pts',(-1.35079678769415,-0.771326437528438,
12.5503846814438));
#268002=CARTESIAN_POINT('Ctrl Pts',(-1.35669631720515,-0.760932463389,12.5495309161395));
#268003=CARTESIAN_POINT('Ctrl Pts',(-1.36055732214704,-0.754007222224728,
12.5489678047051));
#268004=CARTESIAN_POINT('Ctrl Pts',(-1.3942431952972,-0.692485665568443,
12.5440130145136));
#268005=CARTESIAN_POINT('Ctrl Pts',(-1.42082499068629,-0.636167442836501,
12.5398070162856));
#268006=CARTESIAN_POINT('Ctrl Pts',(-1.47151872124608,-0.509611696999284,
12.5307333446788));
#268007=CARTESIAN_POINT('Ctrl Pts',(-1.49412287672159,-0.438940492438061,
12.52590187724));
#268008=CARTESIAN_POINT('Ctrl Pts',(-1.5300089804147,-0.29110256943578,
12.5158353021519));
#268009=CARTESIAN_POINT('Ctrl Pts',(-1.54268101829008,-0.214011724475579,
12.5106051451062));
#268010=CARTESIAN_POINT('Ctrl Pts',(-1.55108315050351,-0.118494252877623,
12.5039474662107));
#268011=CARTESIAN_POINT('Ctrl Pts',(-1.55234245265071,-0.100661270788728,
12.5026973619671));
#268012=CARTESIAN_POINT('Ctrl Pts',(-1.5537096531494,-0.0750166086789068,
12.5008876467063));
#268013=CARTESIAN_POINT('Ctrl Pts',(-1.55406652312781,-0.0672191606709169,
12.5003358010362));
#268014=CARTESIAN_POINT('Ctrl Pts',(-1.55458519307445,-0.0536511825652345,
12.4993726472811));
#268015=CARTESIAN_POINT('Ctrl Pts',(-1.55477358681539,-0.04788177122694,
12.4989621771955));
#268016=CARTESIAN_POINT('Ctrl Pts',(-1.5550751072852,-0.0367483988363213,
12.4981682570041));
#268017=CARTESIAN_POINT('Ctrl Pts',(-1.55519260473,-0.031384629643052,12.4977849494411));
#268018=CARTESIAN_POINT('Ctrl Pts',(-1.5554293939188,-0.0172313597589847,
12.4967713069122));
#268019=CARTESIAN_POINT('Ctrl Pts',(-1.55550193094502,-0.00844137850564686,
12.4961395216324));
#268020=CARTESIAN_POINT('Ctrl Pts',(-1.5554945369244,0.0245530928688604,
12.4937592320721));
#268021=CARTESIAN_POINT('Ctrl Pts',(-1.55492416102653,0.0487528198289879,
12.4919955828552));
#268022=CARTESIAN_POINT('Ctrl Pts',(-1.55208285740592,0.109288947594619,
12.4875362748412));
#268023=CARTESIAN_POINT('Ctrl Pts',(-1.54910057074156,0.145575781188323,
12.4848200657217));
#268024=CARTESIAN_POINT('Ctrl Pts',(-1.52851922446572,0.320541083888283,
12.4715152711997));
#268025=CARTESIAN_POINT('Ctrl Pts',(-1.49355764573315,0.456503787206729,
12.4604642924911));
#268026=CARTESIAN_POINT('Ctrl Pts',(-1.42905275071181,0.615125929149876,
12.4474923462506));
#268027=CARTESIAN_POINT('Ctrl Pts',(-1.41630761673484,0.643929161521702,
12.4451371633041));
#268028=CARTESIAN_POINT('Ctrl Pts',(-1.40000603838808,0.677939574099746,
12.4423725326169));
#268029=CARTESIAN_POINT('Ctrl Pts',(-1.39728265577096,0.683535044468746,
12.4419182337002));
#268030=CARTESIAN_POINT('Ctrl Pts',(-1.39276595690463,0.692675261253849,
12.4411772076144));
#268031=CARTESIAN_POINT('Ctrl Pts',(-1.39099254675416,0.696229677688026,
12.4408893074381));
#268032=CARTESIAN_POINT('Ctrl Pts',(-1.38777719660975,0.70261282565802,
12.4403728197065));
#268033=CARTESIAN_POINT('Ctrl Pts',(-1.38634020330007,0.705443953494621,
12.4401439346554));
#268034=CARTESIAN_POINT('Ctrl Pts',(-1.383172778194,0.711637276654677,12.4396436560727));
#268035=CARTESIAN_POINT('Ctrl Pts',(-1.38143875449403,0.714997563818882,
12.4393724913268));
#268036=CARTESIAN_POINT('Ctrl Pts',(-1.37644944839085,0.724580209153862,
12.4385998756825));
#268037=CARTESIAN_POINT('Ctrl Pts',(-1.37316420321775,0.730787000052084,
12.4381002587719));
#268038=CARTESIAN_POINT('Ctrl Pts',(-1.35068804593067,0.772564289207047,
12.434741440879));
#268039=CARTESIAN_POINT('Ctrl Pts',(-1.33015706013255,0.807401190602827,
12.4319604626095));
#268040=CARTESIAN_POINT('Ctrl Pts',(-1.2382332657067,0.950332811755104,
12.4204630777161));
#268041=CARTESIAN_POINT('Ctrl Pts',(-1.15484438834402,1.0500919243436,12.4121792712782));
#268042=CARTESIAN_POINT('Ctrl Pts',(-1.04178226039845,1.15537569561948,
12.4018018576025));
#268043=CARTESIAN_POINT('Ctrl Pts',(-1.02310931585939,1.17194304882542,
12.4001130309193));
#268044=CARTESIAN_POINT('Ctrl Pts',(-0.999862656680437,1.19158924342775,
12.3980341583902));
#268045=CARTESIAN_POINT('Ctrl Pts',(-0.995660168197325,1.19510296025012,
12.3976592610984));
#268046=CARTESIAN_POINT('Ctrl Pts',(-0.987583130098101,1.20178402997367,
12.3969403773389));
#268047=CARTESIAN_POINT('Ctrl Pts',(-0.983711678178769,1.20495503105514,
12.3965965241109));
#268048=CARTESIAN_POINT('Ctrl Pts',(-0.960203267982165,1.22402132531571,
12.3945126838423));
#268049=CARTESIAN_POINT('Ctrl Pts',(-0.94019774938797,1.23945414885604,
12.3927565572023));
#268050=CARTESIAN_POINT('Ctrl Pts',(-0.912382122166189,1.25985091384744,
12.3903326658022));
#268051=CARTESIAN_POINT('Ctrl Pts',(-0.904889700561335,1.26524309333065,
12.3896814884863));
#268052=CARTESIAN_POINT('Ctrl Pts',(-0.892898978778593,1.27371164539533,
12.3886418415372));
#268053=CARTESIAN_POINT('Ctrl Pts',(-0.888431651697082,1.27683168068718,
12.3882550464476));
#268054=CARTESIAN_POINT('Ctrl Pts',(-0.879235843593155,1.28318251913938,
12.3874598947281));
#268055=CARTESIAN_POINT('Ctrl Pts',(-0.874505735270798,1.28641080664344,
12.3870514507153));
#268056=CARTESIAN_POINT('Ctrl Pts',(-0.863529041839809,1.2938138551353,
12.3861048461946));
#268057=CARTESIAN_POINT('Ctrl Pts',(-0.857269866607893,1.29796959516599,
12.3855659822328));
#268058=CARTESIAN_POINT('Ctrl Pts',(-0.837376369323995,1.31097109273508,
12.3838560067863));
#268059=CARTESIAN_POINT('Ctrl Pts',(-0.823633793998572,1.31964833421932,
12.3826786944117));
#268060=CARTESIAN_POINT('Ctrl Pts',(-0.754410675375549,1.36185422149185,
12.3767657719777));
#268061=CARTESIAN_POINT('Ctrl Pts',(-0.697015739094113,1.39210247571934,
12.3719140591416));
#268062=CARTESIAN_POINT('Ctrl Pts',(-0.577998342048428,1.44561859389717,
12.3619601799778));
#268063=CARTESIAN_POINT('Ctrl Pts',(-0.51644491965093,1.46873376392769,
12.3568653268197));
#268064=CARTESIAN_POINT('Ctrl Pts',(-0.438410659311208,1.49252441701657,
12.3505396051291));
#268065=CARTESIAN_POINT('Ctrl Pts',(-0.423132024362915,1.49692763313344,
12.349307454213));
#268066=CARTESIAN_POINT('Ctrl Pts',(-0.340047883931425,1.51949831308055,
12.3426480818876));
#268067=CARTESIAN_POINT('Ctrl Pts',(-0.271129746806319,1.53329677022921,
12.3372674099411));
#268068=CARTESIAN_POINT('Ctrl Pts',(-0.193474224065011,1.54344212718842,
12.331512053412));
#268069=CARTESIAN_POINT('Ctrl Pts',(-0.185433228320604,1.54442882671571,
12.3309197816025));
#268070=CARTESIAN_POINT('Ctrl Pts',(-0.173406460593269,1.54580932977666,
12.3300397800865));
#268071=CARTESIAN_POINT('Ctrl Pts',(-0.16942645091503,1.54625061465036,
12.3297495171734));
#268072=CARTESIAN_POINT('Ctrl Pts',(-0.162286074448352,1.5470144056371,
12.3292305331364));
#268073=CARTESIAN_POINT('Ctrl Pts',(-0.159126398395019,1.54734260303603,
12.32900150103));
#268074=CARTESIAN_POINT('Ctrl Pts',(-0.152229386695192,1.54803764980117,
12.3285029264759));
#268075=CARTESIAN_POINT('Ctrl Pts',(-0.148491726274141,1.54840064563759,
12.3282336015401));
#268076=CARTESIAN_POINT('Ctrl Pts',(-0.137882127124026,1.54939226364097,
12.3274714635509));
#268077=CARTESIAN_POINT('Ctrl Pts',(-0.13100715221249,1.54998870912158,
12.3269804073676));
#268078=CARTESIAN_POINT('Ctrl Pts',(-0.0865553451291839,1.5535472937897,
12.323822151199));
#268079=CARTESIAN_POINT('Ctrl Pts',(-0.0488815495785679,1.55518879973118,
12.3212228472374));
#268080=CARTESIAN_POINT('Ctrl Pts',(0.0965865640621532,1.55623451500756,
12.3113554818272));
#268081=CARTESIAN_POINT('Ctrl Pts',(0.204150612941537,1.54580754830162,
12.3043996192563));
#268082=CARTESIAN_POINT('Ctrl Pts',(0.386488362420709,1.50875256398428,
12.2920547747426));
#268083=CARTESIAN_POINT('Ctrl Pts',(0.461900598502809,1.4873979624635,12.2867799282199));
#268084=CARTESIAN_POINT('Ctrl Pts',(0.546397930219472,1.45642277019431,
12.2804928178577));
#268085=CARTESIAN_POINT('Ctrl Pts',(0.557370543630846,1.45225894644588,
12.2796690059345));
#268086=CARTESIAN_POINT('Ctrl Pts',(0.575097428552243,1.44530156116565,
12.2783255211351));
#268087=CARTESIAN_POINT('Ctrl Pts',(0.581881118511559,1.44258379848928,
12.2778083829847));
#268088=CARTESIAN_POINT('Ctrl Pts',(0.593921055616238,1.43766147458029,
12.27688504024));
#268089=CARTESIAN_POINT('Ctrl Pts',(0.599184848635445,1.43547561852478,
12.2764794724726));
#268090=CARTESIAN_POINT('Ctrl Pts',(0.610252201690894,1.43080828161097,
12.2756226993501));
#268091=CARTESIAN_POINT('Ctrl Pts',(0.616052894984619,1.42832031309741,
12.2751712798409));
#268092=CARTESIAN_POINT('Ctrl Pts',(0.631378164445106,1.4216364463678,12.2739722735484));
#268093=CARTESIAN_POINT('Ctrl Pts',(0.640875901169038,1.41738020364727,
12.2732226406837));
#268094=CARTESIAN_POINT('Ctrl Pts',(0.685659775415312,1.39676895250205,
12.269656125898));
#268095=CARTESIAN_POINT('Ctrl Pts',(0.720364112563305,1.37919102408313,
12.2667975395383));
#268096=CARTESIAN_POINT('Ctrl Pts',(0.885331155445646,1.28770876644346,
12.2527271104533));
#268097=CARTESIAN_POINT('Ctrl Pts',(1.00510973220499,1.19655552789888,12.2409033206742));
#268098=CARTESIAN_POINT('Ctrl Pts',(1.1374259359383,1.06177997478218,12.2265065524647));
#268099=CARTESIAN_POINT('Ctrl Pts',(1.16380398059014,1.03279979177485,12.223560589531));
#268100=CARTESIAN_POINT('Ctrl Pts',(1.193337604329,0.997782335858556,12.2201993275371));
#268101=CARTESIAN_POINT('Ctrl Pts',(1.19758070379005,0.992685594615127,
12.21971481363));
#268102=CARTESIAN_POINT('Ctrl Pts',(1.20439160302388,0.984397223190089,
12.2189346885213));
#268103=CARTESIAN_POINT('Ctrl Pts',(1.20697955963501,0.981222385662177,
12.2186376924891));
#268104=CARTESIAN_POINT('Ctrl Pts',(1.2115567502596,0.975561698016046,12.2181114484705));
#268105=CARTESIAN_POINT('Ctrl Pts',(1.21355091970713,0.973079930794289,
12.2178818513066));
#268106=CARTESIAN_POINT('Ctrl Pts',(1.21783881333861,0.967709913679408,
12.2173874716625));
#268107=CARTESIAN_POINT('Ctrl Pts',(1.22012988688721,0.964819626768871,
12.2171228771278));
#268108=CARTESIAN_POINT('Ctrl Pts',(1.22648634399336,0.956741832763743,
12.2163874501555));
#268109=CARTESIAN_POINT('Ctrl Pts',(1.23052913546826,0.951536513991988,
12.2159181849416));
#268110=CARTESIAN_POINT('Ctrl Pts',(1.25389352929578,0.921055606847856,
12.2131961695598));
#268111=CARTESIAN_POINT('Ctrl Pts',(1.27247082443883,0.895215495728091,
12.2109915015328));
#268112=CARTESIAN_POINT('Ctrl Pts',(1.34702900787913,0.784492801423282,
12.2018823334935));
#268113=CARTESIAN_POINT('Ctrl Pts',(1.39535328556851,0.694884712183891,
12.1953009886188));
#268114=CARTESIAN_POINT('Ctrl Pts',(1.43457672746074,0.601306796093332,
12.1885981050115));
#268115=CARTESIAN_POINT('',(-1.55596490018789,0.0013805236815898,12.3559437743963));
#268116=CARTESIAN_POINT('Ctrl Pts',(1.43231976391824,0.600353038565383,
12.0501913886179));
#268117=CARTESIAN_POINT('Ctrl Pts',(1.32156751076454,0.862661581944224,
12.0705094971739));
#268118=CARTESIAN_POINT('Ctrl Pts',(0.815438458427758,1.52296397998904,
12.127864748587));
#268119=CARTESIAN_POINT('Ctrl Pts',(-0.666202740309759,1.7134141339966,
12.2222571428571));
#268120=CARTESIAN_POINT('Ctrl Pts',(-1.49941198544797,0.726802141234669,
12.3038564962274));
#268121=CARTESIAN_POINT('Ctrl Pts',(-1.55693100729208,0.106334549516482,
12.3484187067404));
#268122=CARTESIAN_POINT('Ctrl Pts',(-1.55596490018789,0.0013805236815898,
12.3559437743963));
#268123=CARTESIAN_POINT('Ctrl Pts',(-1.55549937226897,0.00139745155209831,
12.3562113151331));
#268124=CARTESIAN_POINT('Ctrl Pts',(-1.55560015022923,-0.110778211126,12.363603217017));
#268125=CARTESIAN_POINT('Ctrl Pts',(-1.54356710252479,-0.222627877494369,
12.3709328968758));
#268126=CARTESIAN_POINT('Ctrl Pts',(-1.51586618162988,-0.349338442814302,
12.3798584345126));
#268127=CARTESIAN_POINT('Ctrl Pts',(-1.51183262656993,-0.366401004801656,
12.3810729896259));
#268128=CARTESIAN_POINT('Ctrl Pts',(-1.50510967085173,-0.392835973703192,
12.3829765578517));
#268129=CARTESIAN_POINT('Ctrl Pts',(-1.50261901115177,-0.402257782188188,
12.3836593733796));
#268130=CARTESIAN_POINT('Ctrl Pts',(-1.49829769540081,-0.418004318998284,
12.3848081980143));
#268131=CARTESIAN_POINT('Ctrl Pts',(-1.49651509301103,-0.424342042170239,
12.3852726683186));
#268132=CARTESIAN_POINT('Ctrl Pts',(-1.49292509230952,-0.436801626793386,
12.3861900133275));
#268133=CARTESIAN_POINT('Ctrl Pts',(-1.49112013799867,-0.442924061511792,
12.3866428013252));
#268134=CARTESIAN_POINT('Ctrl Pts',(-1.48761046176979,-0.454564313554196,
12.3875076011396));
#268135=CARTESIAN_POINT('Ctrl Pts',(-1.48591258877012,-0.460084098841065,
12.3879193833788));
#268136=CARTESIAN_POINT('Ctrl Pts',(-1.48196280840128,-0.472674892616054,
12.3888626199935));
#268137=CARTESIAN_POINT('Ctrl Pts',(-1.47969097327655,-0.479739449769033,
12.389394718922));
#268138=CARTESIAN_POINT('Ctrl Pts',(-1.47362798022986,-0.498140248149313,
12.3907882834518));
#268139=CARTESIAN_POINT('Ctrl Pts',(-1.46975661181773,-0.509449328330971,
12.3916523638042));
#268140=CARTESIAN_POINT('Ctrl Pts',(-1.43078718406095,-0.619144528455941,
12.4001098086086));
#268141=CARTESIAN_POINT('Ctrl Pts',(-1.38600037386035,-0.713783199183425,
12.4080332552461));
#268142=CARTESIAN_POINT('Ctrl Pts',(-1.30096844084808,-0.854805318301572,
12.4207640374016));
#268143=CARTESIAN_POINT('Ctrl Pts',(-1.26688248342074,-0.904555059984803,
12.4254551433798));
#268144=CARTESIAN_POINT('Ctrl Pts',(-1.20606190559064,-0.983119351874199,
12.4331046737486));
#268145=CARTESIAN_POINT('Ctrl Pts',(-1.18096831486752,-1.01312550119775,
12.4360898880484));
#268146=CARTESIAN_POINT('Ctrl Pts',(-1.14055748614195,-1.05790301861601,
12.4406100633039));
#268147=CARTESIAN_POINT('Ctrl Pts',(-1.12602462218836,-1.07335867547891,
12.4421830873412));
#268148=CARTESIAN_POINT('Ctrl Pts',(-1.10715837982193,-1.09261776779837,
12.4441545208049));
#268149=CARTESIAN_POINT('Ctrl Pts',(-1.10311474859451,-1.09670010428365,
12.4445730684628));
#268150=CARTESIAN_POINT('Ctrl Pts',(-1.09688579431638,-1.10291937344725,
12.445211600245));
#268151=CARTESIAN_POINT('Ctrl Pts',(-1.09471669942804,-1.10507236800551,
12.4454328135893));
#268152=CARTESIAN_POINT('Ctrl Pts',(-1.09025148295789,-1.10947839179932,
12.4458858327158));
#268153=CARTESIAN_POINT('Ctrl Pts',(-1.08795474135719,-1.11173066842782,
12.4461175725733));
#268154=CARTESIAN_POINT('Ctrl Pts',(-1.08275423116946,-1.11679894593777,
12.4466394439839));
#268155=CARTESIAN_POINT('Ctrl Pts',(-1.07984645959039,-1.11961075176768,
12.4469292500253));
#268156=CARTESIAN_POINT('Ctrl Pts',(-1.07123211024121,-1.12787602147472,
12.4477820825379));
#268157=CARTESIAN_POINT('Ctrl Pts',(-1.06549483917688,-1.13329753748813,
12.4483427210811));
#268158=CARTESIAN_POINT('Ctrl Pts',(-1.01967757513187,-1.17593770515855,
12.4527644420004));
#268159=CARTESIAN_POINT('Ctrl Pts',(-0.977695839382554,-1.2110674012157,
12.456482916874));
#268160=CARTESIAN_POINT('Ctrl Pts',(-0.826268070246201,-1.32476095302283,
12.4691433913733));
#268161=CARTESIAN_POINT('Ctrl Pts',(-0.708554042657932,-1.39128103360543,
12.4777736621562));
#268162=CARTESIAN_POINT('Ctrl Pts',(-0.560840067834145,-1.45108550805223,
12.4886284562226));
#268163=CARTESIAN_POINT('Ctrl Pts',(-0.537721348907002,-1.45981039046095,
12.4903260643206));
#268164=CARTESIAN_POINT('Ctrl Pts',(-0.4975278368748,-1.4738948877594,12.4932824857116));
#268165=CARTESIAN_POINT('Ctrl Pts',(-0.480549933961462,-1.47951742255689,
12.4945327801255));
#268166=CARTESIAN_POINT('Ctrl Pts',(-0.455867104797492,-1.48722191573576,
12.4963544344436));
#268167=CARTESIAN_POINT('Ctrl Pts',(-0.448236720553013,-1.48953941940832,
12.4969181124094));
#268168=CARTESIAN_POINT('Ctrl Pts',(-0.434970716162959,-1.49345741293552,
12.4978991989121));
#268169=CARTESIAN_POINT('Ctrl Pts',(-0.429343195071929,-1.49508494317291,
12.4983157198108));
#268170=CARTESIAN_POINT('Ctrl Pts',(-0.418494099513277,-1.4981562960236,
12.49911942811));
#268171=CARTESIAN_POINT('Ctrl Pts',(-0.413273902823672,-1.499604707421,
12.499506459898));
#268172=CARTESIAN_POINT('Ctrl Pts',(-0.400917527316907,-1.50296372588632,
12.5004233782777));
#268173=CARTESIAN_POINT('Ctrl Pts',(-0.393775149091655,-1.50485080772348,
12.500954016322));
#268174=CARTESIAN_POINT('Ctrl Pts',(-0.36864354507519,-1.51129964155113,
12.5028235433987));
#268175=CARTESIAN_POINT('Ctrl Pts',(-0.350587023565802,-1.51559010073253,
12.5041710728761));
#268176=CARTESIAN_POINT('Ctrl Pts',(-0.221607200207151,-1.54380917537687,
12.5138313979138));
#268177=CARTESIAN_POINT('Ctrl Pts',(-0.108456652023515,-1.55585465976143,
12.5225259285749));
#268178=CARTESIAN_POINT('Ctrl Pts',(0.0758711805864795,-1.5552654049063,
12.5368163144409));
#268179=CARTESIAN_POINT('Ctrl Pts',(0.14667540519007,-1.55019173375234,
12.5423257713841));
#268180=CARTESIAN_POINT('Ctrl Pts',(0.237206617356653,-1.53744405456127,
12.5492439391433));
#268181=CARTESIAN_POINT('Ctrl Pts',(0.257465832132295,-1.53418142313367,
12.5507834746384));
#268182=CARTESIAN_POINT('Ctrl Pts',(0.290914021506309,-1.52811349442264,
12.5533049174963));
#268183=CARTESIAN_POINT('Ctrl Pts',(0.304141196931125,-1.52553596650936,
12.55429670792));
#268184=CARTESIAN_POINT('Ctrl Pts',(0.322178311086359,-1.52177720918438,
12.5556403758097));
#268185=CARTESIAN_POINT('Ctrl Pts',(0.327018071872729,-1.52074452851333,
12.5560000435315));
#268186=CARTESIAN_POINT('Ctrl Pts',(0.335131466829362,-1.51897281458054,
12.5566014408929));
#268187=CARTESIAN_POINT('Ctrl Pts',(0.338407748220145,-1.51824626070349,
12.5568438664806));
#268188=CARTESIAN_POINT('Ctrl Pts',(0.34461377601422,-1.51684891412099,
12.5573022363793));
#268189=CARTESIAN_POINT('Ctrl Pts',(0.347543962521087,-1.51618022590472,
12.5575183020249));
#268190=CARTESIAN_POINT('Ctrl Pts',(0.355206673937327,-1.51440816246543,
12.5580824503047));
#268191=CARTESIAN_POINT('Ctrl Pts',(0.359936050032937,-1.51329108414137,
12.5584297557633));
#268192=CARTESIAN_POINT('Ctrl Pts',(0.376282149870901,-1.5093491704708,
12.559627334812));
#268193=CARTESIAN_POINT('Ctrl Pts',(0.387871873844865,-1.50641249571743,
12.5604715234795));
#268194=CARTESIAN_POINT('Ctrl Pts',(0.497139595461702,-1.4773808628683,
12.5683940268733));
#268195=CARTESIAN_POINT('Ctrl Pts',(0.592104563507977,-1.44195031690323,
12.5750124333734));
#268196=CARTESIAN_POINT('Ctrl Pts',(0.785088731277806,-1.34764042850243,
12.589150483299));
#268197=CARTESIAN_POINT('Ctrl Pts',(0.881414400348714,-1.28670213965037,
12.59665331513));
#268198=CARTESIAN_POINT('Ctrl Pts',(0.980874254483286,-1.2073322528372,
12.6055359588512));
#268199=CARTESIAN_POINT('Ctrl Pts',(0.991399732746898,-1.19870430929726,
12.6064912615979));
#268200=CARTESIAN_POINT('Ctrl Pts',(1.00720419160567,-1.18539853262973,
12.6079499239553));
#268201=CARTESIAN_POINT('Ctrl Pts',(1.01256700482454,-1.18082091043928,
12.6084492122276));
#268202=CARTESIAN_POINT('Ctrl Pts',(1.02182186106105,-1.17281168823464,
12.6093185257271));
#268203=CARTESIAN_POINT('Ctrl Pts',(1.02572823297761,-1.16939675161193,
12.6096878596056));
#268204=CARTESIAN_POINT('Ctrl Pts',(1.03443682908957,-1.16170651878011,
12.6105166884413));
#268205=CARTESIAN_POINT('Ctrl Pts',(1.03922975382705,-1.157420885254,12.6109766105641));
#268206=CARTESIAN_POINT('Ctrl Pts',(1.05193526253678,-1.14591760428703,
12.6122059977293));
#268207=CARTESIAN_POINT('Ctrl Pts',(1.05979998088015,-1.13864785700074,
12.6129776522848));
#268208=CARTESIAN_POINT('Ctrl Pts',(1.09425187249814,-1.10613611732601,
12.6164061873442));
#268209=CARTESIAN_POINT('Ctrl Pts',(1.12001480381902,-1.08004198616461,
12.6190995049003));
#268210=CARTESIAN_POINT('Ctrl Pts',(1.24544129781082,-0.943685596223638,
12.6329017122115));
#268211=CARTESIAN_POINT('Ctrl Pts',(1.32984968312786,-0.820458237612204,
12.6446209043491));
#268212=CARTESIAN_POINT('Ctrl Pts',(1.41412675134025,-0.649312762034147,
12.6591871112096));
#268213=CARTESIAN_POINT('Ctrl Pts',(1.43122522815361,-0.61070177855176,
12.6623660977481));
#268214=CARTESIAN_POINT('Ctrl Pts',(1.44936349252139,-0.564780462295209,
12.6659872522042));
#268215=CARTESIAN_POINT('Ctrl Pts',(1.45194761012485,-0.558103616540816,
12.6665098856312));
#268216=CARTESIAN_POINT('Ctrl Pts',(1.45584659743324,-0.547819016650909,
12.6673087286485));
#268217=CARTESIAN_POINT('Ctrl Pts',(1.45719431623729,-0.544223957440305,
12.6675868147411));
#268218=CARTESIAN_POINT('Ctrl Pts',(1.45964624908201,-0.537608980658181,
12.668096330654));
#268219=CARTESIAN_POINT('Ctrl Pts',(1.46075440580217,-0.534590642363316,
12.6683279857228));
#268220=CARTESIAN_POINT('Ctrl Pts',(1.46322541888445,-0.527795174897882,
12.6688476787133));
#268221=CARTESIAN_POINT('Ctrl Pts',(1.46458301178637,-0.524016197918953,
12.6691354034082));
#268222=CARTESIAN_POINT('Ctrl Pts',(1.46802586889457,-0.514314806686216,
12.6698708830791));
#268223=CARTESIAN_POINT('Ctrl Pts',(1.47008996253747,-0.508384871633926,
12.6703174255542));
#268224=CARTESIAN_POINT('Ctrl Pts',(1.48231793395388,-0.472557847312886,
12.6729981019342));
#268225=CARTESIAN_POINT('Ctrl Pts',(1.49160628561459,-0.442366842251715,
12.6751850659997));
#268226=CARTESIAN_POINT('Ctrl Pts',(1.50358408076105,-0.398749859390128,
12.6782706054195));
#268227=CARTESIAN_POINT('Ctrl Pts',(1.50702511613622,-0.385540994223214,
12.6791954556755));
#268228=CARTESIAN_POINT('Ctrl Pts',(1.53473127644131,-0.273143149108765,
12.6869975334167));
#268229=CARTESIAN_POINT('Ctrl Pts',(1.54934979569201,-0.171828086244541,
12.6936003016814));
#268230=CARTESIAN_POINT('Ctrl Pts',(1.55707109430422,5.27306946508915E-5,
12.7050265026763));
#268231=CARTESIAN_POINT('Ctrl Pts',(1.55549462106469,0.0700354402682524,
12.7097378005632));
#268232=CARTESIAN_POINT('Ctrl Pts',(1.54769163906902,0.156586642653441,
12.7157780457768));
#268233=CARTESIAN_POINT('Ctrl Pts',(1.54588946824115,0.173477660584556,
12.7169667435368));
#268234=CARTESIAN_POINT('Ctrl Pts',(1.54286830441444,0.197982354900983,
12.7187072047668));
#268235=CARTESIAN_POINT('Ctrl Pts',(1.54186870435193,0.205622256365373,
12.7192520934816));
#268236=CARTESIAN_POINT('Ctrl Pts',(1.54001527695707,0.219013704964218,
12.720211305066));
#268237=CARTESIAN_POINT('Ctrl Pts',(1.53918587668273,0.224768528860726,
12.7206248519073));
#268238=CARTESIAN_POINT('Ctrl Pts',(1.53751073696963,0.235947276184699,
12.7214308290482));
#268239=CARTESIAN_POINT('Ctrl Pts',(1.53666851026494,0.2413716461636,12.7218231426811));
#268240=CARTESIAN_POINT('Ctrl Pts',(1.53433843416575,0.255871849796493,
12.7228751951929));
#268241=CARTESIAN_POINT('Ctrl Pts',(1.5327987951335,0.26493901368328,12.7235365611952));
#268242=CARTESIAN_POINT('Ctrl Pts',(1.52685157232671,0.298174539208212,
12.7259740270748));
#268243=CARTESIAN_POINT('Ctrl Pts',(1.52195223056001,0.322249995993279,
12.727765552245));
#268244=CARTESIAN_POINT('Ctrl Pts',(1.51537870829572,0.351044631417397,
12.7299408405132));
#268245=CARTESIAN_POINT('Ctrl Pts',(1.51424908402265,0.355885758789841,
12.7303076758378));
#268246=CARTESIAN_POINT('Ctrl Pts',(1.4934680278206,0.443054815944682,12.7369330502946));
#268247=CARTESIAN_POINT('Ctrl Pts',(1.46718470041356,0.523511886852931,
12.743384755441));
#268248=CARTESIAN_POINT('Ctrl Pts',(1.43457658310325,0.601307140496281,
12.749909041778));
#268249=CARTESIAN_POINT('Origin',(0.,0.,-1.29405622560371));
#268250=CARTESIAN_POINT('',(1.43457670670211,0.601306845618552,13.5890749702576));
#268251=CARTESIAN_POINT('',(1.43457668314421,0.601306901822156,13.4515605039018));
#268252=CARTESIAN_POINT('',(1.43457668357355,0.601306900797845,-1.29405622560371));
#268253=CARTESIAN_POINT('',(-1.55549936700331,-0.00142192595573973,13.1940429763088));
#268254=CARTESIAN_POINT('Ctrl Pts',(1.43457670670211,0.601306845618552,
13.5890749702576));
#268255=CARTESIAN_POINT('Ctrl Pts',(1.45865647660418,0.543858178177025,
13.5843171061907));
#268256=CARTESIAN_POINT('Ctrl Pts',(1.47926802300138,0.485004505948749,
13.5794850661721));
#268257=CARTESIAN_POINT('Ctrl Pts',(1.52008574292279,0.341318809516777,
13.5679023622844));
#268258=CARTESIAN_POINT('Ctrl Pts',(1.53680621093689,0.255714392750175,
13.5611697067846));
#268259=CARTESIAN_POINT('Ctrl Pts',(1.54713080553736,0.161333096143716,
13.5541942793966));
#268260=CARTESIAN_POINT('Ctrl Pts',(1.54792672424916,0.153508829286314,
13.553619393256));
#268261=CARTESIAN_POINT('Ctrl Pts',(1.5490387721051,0.141687002620586,13.5527562187289));
#268262=CARTESIAN_POINT('Ctrl Pts',(1.54939882710123,0.137693862439449,
13.5524655925377));
#268263=CARTESIAN_POINT('Ctrl Pts',(1.55001651315244,0.130534103140939,
13.5519462221477));
#268264=CARTESIAN_POINT('Ctrl Pts',(1.55027988470742,0.127368060485406,
13.5517171648972));
#268265=CARTESIAN_POINT('Ctrl Pts',(1.5508330899526,0.120461816918602,13.5512188408898));
#268266=CARTESIAN_POINT('Ctrl Pts',(1.55111909413622,0.116721372670901,
13.550949789956));
#268267=CARTESIAN_POINT('Ctrl Pts',(1.55189145955195,0.106115579625303,
13.5501892079015));
#268268=CARTESIAN_POINT('Ctrl Pts',(1.55234580020136,0.0992478702810322,
13.5496994223305));
#268269=CARTESIAN_POINT('Ctrl Pts',(1.55497038625052,0.0551315965832953,
13.5465693417098));
#268270=CARTESIAN_POINT('Ctrl Pts',(1.55584562602841,0.0178144299041783,
13.5439955536589));
#268271=CARTESIAN_POINT('Ctrl Pts',(1.55405865316281,-0.124707051753495,
13.5343239609659));
#268272=CARTESIAN_POINT('Ctrl Pts',(1.5420690022035,-0.229514357431623,
13.5275250686444));
#268273=CARTESIAN_POINT('Ctrl Pts',(1.5022580284579,-0.41155925816425,13.5151756968029));
#268274=CARTESIAN_POINT('Ctrl Pts',(1.47875894083323,-0.489315115857666,
13.5097181953477));
#268275=CARTESIAN_POINT('Ctrl Pts',(1.44502094592174,-0.575876790834559,
13.5032286048885));
#268276=CARTESIAN_POINT('Ctrl Pts',(1.44060894138887,-0.586826615692031,
13.502400002413));
#268277=CARTESIAN_POINT('Ctrl Pts',(1.43325670151859,-0.60449084873319,
13.5010502410663));
#268278=CARTESIAN_POINT('Ctrl Pts',(1.43039283032183,-0.611236702346225,
13.5005316565034));
#268279=CARTESIAN_POINT('Ctrl Pts',(1.42521611655373,-0.623194821552002,
13.4996066927768));
#268280=CARTESIAN_POINT('Ctrl Pts',(1.42292206433732,-0.628415118954393,
13.4992009587135));
#268281=CARTESIAN_POINT('Ctrl Pts',(1.4180328568701,-0.639376856903346,
13.4983448244155));
#268282=CARTESIAN_POINT('Ctrl Pts',(1.41543142234358,-0.645115365489947,
13.4978942151));
#268283=CARTESIAN_POINT('Ctrl Pts',(1.40846157284832,-0.660245048516545,
13.4966996648346));
#268284=CARTESIAN_POINT('Ctrl Pts',(1.40403416509097,-0.669608527343406,
13.4959537049001));
#268285=CARTESIAN_POINT('Ctrl Pts',(1.38278833447639,-0.713403862462427,
13.4924325196657));
#268286=CARTESIAN_POINT('Ctrl Pts',(1.36479619656187,-0.74724795975849,
13.4896168695039));
#268287=CARTESIAN_POINT('Ctrl Pts',(1.27025692406576,-0.910255563427451,
13.4755678538875));
#268288=CARTESIAN_POINT('Ctrl Pts',(1.17653771174988,-1.02852426048133,
13.4637154610322));
#268289=CARTESIAN_POINT('Ctrl Pts',(1.03867740986663,-1.15857033205153,
13.4492663910669));
#268290=CARTESIAN_POINT('Ctrl Pts',(1.00896372847602,-1.18453738778254,
13.4462993004457));
#268291=CARTESIAN_POINT('Ctrl Pts',(0.973126711431908,-1.21352741692326,
13.4429169777336));
#268292=CARTESIAN_POINT('Ctrl Pts',(0.967934653940546,-1.2176727384809,
13.4424315698324));
#268293=CARTESIAN_POINT('Ctrl Pts',(0.959496052635796,-1.22432200875417,
13.4416502909437));
#268294=CARTESIAN_POINT('Ctrl Pts',(0.956265963444916,-1.22684655289302,
13.441353028632));
#268295=CARTESIAN_POINT('Ctrl Pts',(0.950509470250032,-1.23130911424539,
13.4408264934953));
#268296=CARTESIAN_POINT('Ctrl Pts',(0.947987063070771,-1.23325217081216,
13.440596869988));
#268297=CARTESIAN_POINT('Ctrl Pts',(0.942531918220844,-1.23742774227772,
13.4401026380868));
#268298=CARTESIAN_POINT('Ctrl Pts',(0.939597210115723,-1.23965758083888,
13.4398382165388));
#268299=CARTESIAN_POINT('Ctrl Pts',(0.931401722497112,-1.24583882171926,
13.4391037606934));
#268300=CARTESIAN_POINT('Ctrl Pts',(0.926123673893443,-1.24976737161002,
13.4386352869109));
#268301=CARTESIAN_POINT('Ctrl Pts',(0.895332820379853,-1.27238339338094,
13.4359274617279));
#268302=CARTESIAN_POINT('Ctrl Pts',(0.869277570227663,-1.29032446616473,
13.4337356084054));
#268303=CARTESIAN_POINT('Ctrl Pts',(0.720112008040473,-1.38646543964895,
13.4216228284471));
#268304=CARTESIAN_POINT('Ctrl Pts',(0.587024807379808,-1.44784598767101,
13.412367685377));
#268305=CARTESIAN_POINT('Ctrl Pts',(0.400140260560503,-1.50395978040451,
13.3992066305443));
#268306=CARTESIAN_POINT('Ctrl Pts',(0.352314943247857,-1.51587618345896,
13.3958325591057));
#268307=CARTESIAN_POINT('Ctrl Pts',(0.292676964265228,-1.52776109089081,
13.3915761664699));
#268308=CARTESIAN_POINT('Ctrl Pts',(0.281320765834508,-1.52989292769967,
13.3907635776079));
#268309=CARTESIAN_POINT('Ctrl Pts',(0.263410496588431,-1.53304897095434,
13.3894782459837));
#268310=CARTESIAN_POINT('Ctrl Pts',(0.256871654844472,-1.53415813641352,
13.3890081991548));
#268311=CARTESIAN_POINT('Ctrl Pts',(0.244791494970911,-1.53612786552186,
13.3881382693904));
#268312=CARTESIAN_POINT('Ctrl Pts',(0.23925220739389,-1.53700034970343,
13.3877387709431));
#268313=CARTESIAN_POINT('Ctrl Pts',(0.226966212681123,-1.53886747158078,
13.3868513103064));
#268314=CARTESIAN_POINT('Ctrl Pts',(0.220217472080572,-1.53984772592532,
13.3863629022416));
#268315=CARTESIAN_POINT('Ctrl Pts',(0.201296294613768,-1.54246909591618,
13.3849908658806));
#268316=CARTESIAN_POINT('Ctrl Pts',(0.189110784996112,-1.54401042903936,
13.3841041200772));
#268317=CARTESIAN_POINT('Ctrl Pts',(0.16152054228375,-1.54716878856753,
13.3820888176029));
#268318=CARTESIAN_POINT('Ctrl Pts',(0.146107547853411,-1.54870032554592,
13.3809576847575));
#268319=CARTESIAN_POINT('Ctrl Pts',(0.0968600525073427,-1.55285219559935,
13.377325733894));
#268320=CARTESIAN_POINT('Ctrl Pts',(0.0629636142149593,-1.5545954713363,
13.3747989674912));
#268321=CARTESIAN_POINT('Ctrl Pts',(-0.0953325866465109,-1.55755120588528,
13.3628732576448));
#268322=CARTESIAN_POINT('Ctrl Pts',(-0.219527562206013,-1.5449449237587,
13.3531061291233));
#268323=CARTESIAN_POINT('Ctrl Pts',(-0.352018721021943,-1.51518765062239,
13.342687590316));
#268324=CARTESIAN_POINT('Ctrl Pts',(-0.363139000214201,-1.51256103130583,
13.3418135695069));
#268325=CARTESIAN_POINT('Ctrl Pts',(-0.411836161330166,-1.50049071033415,
13.3379904815714));
#268326=CARTESIAN_POINT('Ctrl Pts',(-0.449085440557114,-1.48976652035185,
13.3350773271913));
#268327=CARTESIAN_POINT('Ctrl Pts',(-0.492175702757902,-1.47559716263511,
13.3317491872374));
#268328=CARTESIAN_POINT('Ctrl Pts',(-0.498439469931759,-1.4734931312073,
13.3312664547501));
#268329=CARTESIAN_POINT('Ctrl Pts',(-0.508557276873416,-1.47002260644851,
13.3304886292608));
#268330=CARTESIAN_POINT('Ctrl Pts',(-0.512419581614434,-1.46868074840852,
13.3301921643284));
#268331=CARTESIAN_POINT('Ctrl Pts',(-0.519279189064021,-1.46626720122315,
13.3296665001026));
#268332=CARTESIAN_POINT('Ctrl Pts',(-0.522278531743087,-1.465201527966,
13.3294369546342));
#268333=CARTESIAN_POINT('Ctrl Pts',(-0.528750797503353,-1.46287951754892,
13.3289422764567));
#268334=CARTESIAN_POINT('Ctrl Pts',(-0.532222520104307,-1.4616200185369,
13.3286773339011));
#268335=CARTESIAN_POINT('Ctrl Pts',(-0.541535111472556,-1.45820394274807,
13.3279676467945));
#268336=CARTESIAN_POINT('Ctrl Pts',(-0.547367654961516,-1.4560246115361,
13.3275242221131));
#268337=CARTESIAN_POINT('Ctrl Pts',(-0.579679529621522,-1.44372967031622,
13.3250727221209));
#268338=CARTESIAN_POINT('Ctrl Pts',(-0.605893714508587,-1.43292595510251,
13.3231026946037));
#268339=CARTESIAN_POINT('Ctrl Pts',(-0.766692546522229,-1.36145280517023,
13.3110482023596));
#268340=CARTESIAN_POINT('Ctrl Pts',(-0.892374016857767,-1.28259484816741,
13.3016908299711));
#268341=CARTESIAN_POINT('Ctrl Pts',(-1.04390505051855,-1.15431033337945,
13.2883149588975));
#268342=CARTESIAN_POINT('Ctrl Pts',(-1.08110490532008,-1.11954516731242,
13.2848327703219));
#268343=CARTESIAN_POINT('Ctrl Pts',(-1.12465509032343,-1.0746475286691,
13.28045542583));
#268344=CARTESIAN_POINT('Ctrl Pts',(-1.13268401615312,-1.06618164001697,
13.2796349847631));
#268345=CARTESIAN_POINT('Ctrl Pts',(-1.14514371580149,-1.05274424683791,
13.2783399397987));
#268346=CARTESIAN_POINT('Ctrl Pts',(-1.1496392187029,-1.04783311811135,
13.2778681003129));
#268347=CARTESIAN_POINT('Ctrl Pts',(-1.15751891709497,-1.03911316271139,
13.2770328255442));
#268348=CARTESIAN_POINT('Ctrl Pts',(-1.16091621203529,-1.03531625885682,
13.2766699490089));
#268349=CARTESIAN_POINT('Ctrl Pts',(-1.16866084484423,-1.02657460969551,
13.2758363287833));
#268350=CARTESIAN_POINT('Ctrl Pts',(-1.1729955378379,-1.02161884540701,
13.2753650678692));
#268351=CARTESIAN_POINT('Ctrl Pts',(-1.18180904725329,-1.01141250377658,
13.2743971375996));
#268352=CARTESIAN_POINT('Ctrl Pts',(-1.18628463796444,-1.00615934714186,
13.273900349496));
#268353=CARTESIAN_POINT('Ctrl Pts',(-1.20780594330266,-0.980555835174825,
13.2714855962354));
#268354=CARTESIAN_POINT('Ctrl Pts',(-1.22436279966232,-0.959802331887778,
13.2695480587677));
#268355=CARTESIAN_POINT('Ctrl Pts',(-1.27644531427125,-0.890976870139557,
13.2631810105464));
#268356=CARTESIAN_POINT('Ctrl Pts',(-1.30972975110126,-0.841284036024207,
13.2586708795457));
#268357=CARTESIAN_POINT('Ctrl Pts',(-1.36744771550181,-0.743353417773102,
13.2499609303454));
#268358=CARTESIAN_POINT('Ctrl Pts',(-1.39239043495957,-0.695511298393266,
13.2457800708118));
#268359=CARTESIAN_POINT('Ctrl Pts',(-1.44893884953429,-0.571755834475074,
13.2352284161469));
#268360=CARTESIAN_POINT('Ctrl Pts',(-1.47711133093812,-0.494442798788441,
13.2288690966019));
#268361=CARTESIAN_POINT('Ctrl Pts',(-1.50233780352053,-0.403377446876232,
13.2218699021356));
#268362=CARTESIAN_POINT('Ctrl Pts',(-1.50548779756471,-0.391457223010544,
13.2209632748028));
#268363=CARTESIAN_POINT('Ctrl Pts',(-1.50968822552226,-0.374760719961676,
13.2197078315613));
#268364=CARTESIAN_POINT('Ctrl Pts',(-1.51085826887459,-0.370015443763787,
13.2193526469601));
#268365=CARTESIAN_POINT('Ctrl Pts',(-1.51270669089005,-0.362363936520089,
13.218782625625));
#268366=CARTESIAN_POINT('Ctrl Pts',(-1.51339909257423,-0.359461183108582,
13.2185669996639));
#268367=CARTESIAN_POINT('Ctrl Pts',(-1.51483812258624,-0.35335047817249,
13.218114412214));
#268368=CARTESIAN_POINT('Ctrl Pts',(-1.51558292238446,-0.350142119451603,
13.2178775611972));
#268369=CARTESIAN_POINT('Ctrl Pts',(-1.51705901456637,-0.343690629268269,
13.2174028042245));
#268370=CARTESIAN_POINT('Ctrl Pts',(-1.51779011399703,-0.340447459570058,
13.2171649094264));
#268371=CARTESIAN_POINT('Ctrl Pts',(-1.51951374458998,-0.33268548827976,
13.2165973242223));
#268372=CARTESIAN_POINT('Ctrl Pts',(-1.52049653203074,-0.328164519125983,
13.2162681699804));
#268373=CARTESIAN_POINT('Ctrl Pts',(-1.52308642920974,-0.315989160648673,
13.2153854226322));
#268374=CARTESIAN_POINT('Ctrl Pts',(-1.52465603060778,-0.308326799373177,
13.2148337991552));
#268375=CARTESIAN_POINT('Ctrl Pts',(-1.54558199302605,-0.202102815742466,
13.2072365938642));
#268376=CARTESIAN_POINT('Ctrl Pts',(-1.55540751071694,-0.101891035777499,
13.2006549036526));
#268377=CARTESIAN_POINT('Ctrl Pts',(-1.55549935012108,-0.00142189060349853,
13.1940429475177));
#268378=CARTESIAN_POINT('Ctrl Pts',(-1.5554993500872,-0.00142192767448274,
13.1940429499574));
#268379=CARTESIAN_POINT('Ctrl Pts',(-1.55560532666497,0.114509776029417,
13.1864133902736));
#268380=CARTESIAN_POINT('Ctrl Pts',(-1.54275149737557,0.230076481554751,
13.1787694472679));
#268381=CARTESIAN_POINT('Ctrl Pts',(-1.51509323349481,0.352366628040915,
13.1700144932057));
#268382=CARTESIAN_POINT('Ctrl Pts',(-1.51292222855975,0.361574432401795,
13.1693513464451));
#268383=CARTESIAN_POINT('Ctrl Pts',(-1.50913380558097,0.377010350794123,
13.1682327101714));
#268384=CARTESIAN_POINT('Ctrl Pts',(-1.50756146729406,0.383249354671272,
13.1677786567778));
#268385=CARTESIAN_POINT('Ctrl Pts',(-1.50438393824964,0.395535535725688,
13.166880629426));
#268386=CARTESIAN_POINT('Ctrl Pts',(-1.50278087943554,0.401583142086659,
13.1664367313259));
#268387=CARTESIAN_POINT('Ctrl Pts',(-1.49964423762699,0.413134423311204,
13.1655852093262));
#268388=CARTESIAN_POINT('Ctrl Pts',(-1.49811672757471,0.418639654275458,
13.1651777881848));
#268389=CARTESIAN_POINT('Ctrl Pts',(-1.49457053617927,0.431152341152361,
13.1642480731838));
#268390=CARTESIAN_POINT('Ctrl Pts',(-1.49253284844343,0.438154221544365,
13.1637251692766));
#268391=CARTESIAN_POINT('Ctrl Pts',(-1.48702672798701,0.456590105710933,
13.1623412197185));
#268392=CARTESIAN_POINT('Ctrl Pts',(-1.48347571470457,0.467998721624268,
13.161477502689));
#268393=CARTESIAN_POINT('Ctrl Pts',(-1.45067209494675,0.569263081057521,
13.1537442097845));
#268394=CARTESIAN_POINT('Ctrl Pts',(-1.41342513761139,0.656302509391999,
13.146607677695));
#268395=CARTESIAN_POINT('Ctrl Pts',(-1.34146758101601,0.789483469408031,
13.134937233164));
#268396=CARTESIAN_POINT('Ctrl Pts',(-1.31168601895308,0.838032817961845,
13.1305093920219));
#268397=CARTESIAN_POINT('Ctrl Pts',(-1.24454219641953,0.935110167357172,
13.1213801067369));
#268398=CARTESIAN_POINT('Ctrl Pts',(-1.20683566660835,0.983293241526527,
13.1166901917138));
#268399=CARTESIAN_POINT('Ctrl Pts',(-1.15705682664943,1.03971083680104,
13.1111023098393));
#268400=CARTESIAN_POINT('Ctrl Pts',(-1.14758278044537,1.0501585232005,13.1100632427421));
#268401=CARTESIAN_POINT('Ctrl Pts',(-1.13532145456876,1.0633158085424,13.1087507584632));
#268402=CARTESIAN_POINT('Ctrl Pts',(-1.13266473845105,1.06614534892473,
13.1084682657019));
#268403=CARTESIAN_POINT('Ctrl Pts',(-1.12747518450364,1.07163120002392,
13.107920164797));
#268404=CARTESIAN_POINT('Ctrl Pts',(-1.12494348322294,1.07428854636398,
13.1076544755705));
#268405=CARTESIAN_POINT('Ctrl Pts',(-1.12019636800393,1.07923607219256,
13.107159495127));
#268406=CARTESIAN_POINT('Ctrl Pts',(-1.11798334561292,1.08152838226147,
13.1069300373096));
#268407=CARTESIAN_POINT('Ctrl Pts',(-1.11289058649208,1.08677126864311,
13.1064049268886));
#268408=CARTESIAN_POINT('Ctrl Pts',(-1.1100061521652,1.08971720692291,13.1061096448164));
#268409=CARTESIAN_POINT('Ctrl Pts',(-1.1023884202592,1.0974357390234,13.1053352742));
#268410=CARTESIAN_POINT('Ctrl Pts',(-1.09763577379955,1.10218924999249,
13.1048576482712));
#268411=CARTESIAN_POINT('Ctrl Pts',(-1.06349102594555,1.1359003044778,13.1014638391734));
#268412=CARTESIAN_POINT('Ctrl Pts',(-1.03298465154647,1.16371221366005,
13.0986288910756));
#268413=CARTESIAN_POINT('Ctrl Pts',(-0.986915767935382,1.20247081242974,
13.0945611493805));
#268414=CARTESIAN_POINT('Ctrl Pts',(-0.972204664422465,1.21439570218504,
13.0932919754945));
#268415=CARTESIAN_POINT('Ctrl Pts',(-0.872144057891693,1.29252136973191,
13.0848289421818));
#268416=CARTESIAN_POINT('Ctrl Pts',(-0.780318232993791,1.34994478672804,
13.0778515516041));
#268417=CARTESIAN_POINT('Ctrl Pts',(-0.64948818760217,1.41391670476706,
13.0680745669525));
#268418=CARTESIAN_POINT('Ctrl Pts',(-0.615107885555045,1.42920862997314,
13.06552176588));
#268419=CARTESIAN_POINT('Ctrl Pts',(-0.564764787435561,1.44944750182462,
13.0617826480369));
#268420=CARTESIAN_POINT('Ctrl Pts',(-0.549222369575856,1.45540787372533,
13.0606281985852));
#268421=CARTESIAN_POINT('Ctrl Pts',(-0.521376076388962,1.46557710503839,
13.0585577064921));
#268422=CARTESIAN_POINT('Ctrl Pts',(-0.509109280853314,1.46988332393,13.0576448914661));
#268423=CARTESIAN_POINT('Ctrl Pts',(-0.491435989831771,1.47583970761921,
13.0563280784612));
#268424=CARTESIAN_POINT('Ctrl Pts',(-0.486071981170295,1.47761503859665,
13.0559281939286));
#268425=CARTESIAN_POINT('Ctrl Pts',(-0.475223985267353,1.48113994892571,
13.055118973102));
#268426=CARTESIAN_POINT('Ctrl Pts',(-0.469739724351119,1.48288838899446,
13.0547096068622));
#268427=CARTESIAN_POINT('Ctrl Pts',(-0.459100580465859,1.48621531774945,
13.0539148968668));
#268428=CARTESIAN_POINT('Ctrl Pts',(-0.453946939829438,1.48779752929173,
13.0535296816134));
#268429=CARTESIAN_POINT('Ctrl Pts',(-0.44164454600721,1.49150459746582,
13.0526094627482));
#268430=CARTESIAN_POINT('Ctrl Pts',(-0.434488589985751,1.49360487775552,
13.0520736669071));
#268431=CARTESIAN_POINT('Ctrl Pts',(-0.408750275005844,1.50095848114298,
13.0501444417567));
#268432=CARTESIAN_POINT('Ctrl Pts',(-0.390086268774325,1.50591692664642,
13.0487415466751));
#268433=CARTESIAN_POINT('Ctrl Pts',(-0.231012431485575,1.54502234670856,
13.0367459444016));
#268434=CARTESIAN_POINT('Ctrl Pts',(-0.0865916555847983,1.55978968356651,
13.0255025276203));
#268435=CARTESIAN_POINT('Ctrl Pts',(0.104580207163462,1.55268793576817,
13.010716817981));
#268436=CARTESIAN_POINT('Ctrl Pts',(0.151316968064041,1.54883204359739,
13.0071192403454));
#268437=CARTESIAN_POINT('Ctrl Pts',(0.213631181874183,1.54084273850421,
13.002397335285));
#268438=CARTESIAN_POINT('Ctrl Pts',(0.229419505095176,1.53857120893022,
13.0012075346182));
#268439=CARTESIAN_POINT('Ctrl Pts',(0.256073786931493,1.53431690627593,
12.9992129705051));
#268440=CARTESIAN_POINT('Ctrl Pts',(0.266958344467703,1.53246057508004,
12.9984024702484));
#268441=CARTESIAN_POINT('Ctrl Pts',(0.282278053802187,1.52967965775119,
12.9972682135915));
#268442=CARTESIAN_POINT('Ctrl Pts',(0.286730009584213,1.52885141789327,
12.9969393718969));
#268443=CARTESIAN_POINT('Ctrl Pts',(0.2943819094531,1.52739326199613,12.9963755778687));
#268444=CARTESIAN_POINT('Ctrl Pts',(0.297583585667985,1.52677270599082,
12.9961401035246));
#268445=CARTESIAN_POINT('Ctrl Pts',(0.303746662533513,1.52555804127153,
12.9956876750254));
#268446=CARTESIAN_POINT('Ctrl Pts',(0.306708298186996,1.52496537420939,
12.9954706377838));
#268447=CARTESIAN_POINT('Ctrl Pts',(0.314642991614519,1.52335347423595,
12.9948901198869));
#268448=CARTESIAN_POINT('Ctrl Pts',(0.319612876292937,1.52231850507107,
12.99452752485));
#268449=CARTESIAN_POINT('Ctrl Pts',(0.337809312421182,1.51843609151781,
12.9932033508101));
#268450=CARTESIAN_POINT('Ctrl Pts',(0.351004128039468,1.51544034215433,
12.9922497638899));
#268451=CARTESIAN_POINT('Ctrl Pts',(0.519034662137245,1.47497820036408,
12.9801710586475));
#268452=CARTESIAN_POINT('Ctrl Pts',(0.66728645537411,1.41410911376194,12.9701384119536));
#268453=CARTESIAN_POINT('Ctrl Pts',(0.852479784879324,1.30234451359323,
12.9556166853679));
#268454=CARTESIAN_POINT('Ctrl Pts',(0.89957653346717,1.27026920346239,12.9517306723403));
#268455=CARTESIAN_POINT('Ctrl Pts',(0.954059686325388,1.22861144325625,
12.9469298716769));
#268456=CARTESIAN_POINT('Ctrl Pts',(0.963234115898543,1.22143194181302,
12.9461105072023));
#268457=CARTESIAN_POINT('Ctrl Pts',(0.977465937982646,1.21003468478247,
12.9448216800265));
#268458=CARTESIAN_POINT('Ctrl Pts',(0.9825787994208,1.20588660279634,12.9443549993826));
#268459=CARTESIAN_POINT('Ctrl Pts',(0.991601206928114,1.19847121565272,
12.9435248545138));
#268460=CARTESIAN_POINT('Ctrl Pts',(0.995521350429314,1.19521690417903,
12.9431619195307));
#268461=CARTESIAN_POINT('Ctrl Pts',(1.00452734580211,1.1876655219114,12.9423228769869));
#268462=CARTESIAN_POINT('Ctrl Pts',(1.00960170512964,1.18335496570163,12.9418462227313));
#268463=CARTESIAN_POINT('Ctrl Pts',(1.02349211450505,1.17140099234914,12.9405305301814));
#268464=CARTESIAN_POINT('Ctrl Pts',(1.03224991886995,1.1636908887341,12.9396887487776));
#268465=CARTESIAN_POINT('Ctrl Pts',(1.07874143173811,1.12182338561223,12.935152800035));
#268466=CARTESIAN_POINT('Ctrl Pts',(1.11486400381476,1.08593183256602,12.9313857880437));
#268467=CARTESIAN_POINT('Ctrl Pts',(1.24867531701197,0.939251589313107,
12.9164274177818));
#268468=CARTESIAN_POINT('Ctrl Pts',(1.33213542888772,0.816571739045674,
12.9047271564757));
#268469=CARTESIAN_POINT('Ctrl Pts',(1.40952661595457,0.658498329059338,
12.8914388014644));
#268470=CARTESIAN_POINT('Ctrl Pts',(1.42130463026261,0.632675864308015,
12.889322724023));
#268471=CARTESIAN_POINT('Ctrl Pts',(1.4331090631311,0.604799347628273,12.8871063962525));
#268472=CARTESIAN_POINT('Ctrl Pts',(1.43384446664119,0.603053797993081,
12.8869678972309));
#268473=CARTESIAN_POINT('Ctrl Pts',(1.43457668357408,0.601306900796593,
12.8868295753666));
#268474=CARTESIAN_POINT('Ctrl Pts',(1.43457658310325,0.601307140496281,
12.749909041778));
#268475=CARTESIAN_POINT('Ctrl Pts',(1.40228372079604,0.6783502702836,12.7563702513696));
#268476=CARTESIAN_POINT('Ctrl Pts',(1.36378817913178,0.752783104809556,
12.7629010726667));
#268477=CARTESIAN_POINT('Ctrl Pts',(1.30172901177612,0.852171572957744,
12.7717880182731));
#268478=CARTESIAN_POINT('Ctrl Pts',(1.2831381829391,0.879915697305408,12.7742872593444));
#268479=CARTESIAN_POINT('Ctrl Pts',(1.25973790685436,0.912516333320734,
12.7772276251402));
#268480=CARTESIAN_POINT('Ctrl Pts',(1.25577314197408,0.917964853837816,
12.7777191667732));
#268481=CARTESIAN_POINT('Ctrl Pts',(1.24954763807542,0.926404341162586,
12.7784805139681));
#268482=CARTESIAN_POINT('Ctrl Pts',(1.24731134518913,0.929413100894063,
12.7787519363812));
#268483=CARTESIAN_POINT('Ctrl Pts',(1.24313212303325,0.934993670167423,
12.7792553090446));
#268484=CARTESIAN_POINT('Ctrl Pts',(1.2411920948355,0.937567502968436,12.7794874441212));
#268485=CARTESIAN_POINT('Ctrl Pts',(1.23674603205329,0.943428102332941,
12.7800159740925));
#268486=CARTESIAN_POINT('Ctrl Pts',(1.23423488992615,0.946710921889629,
12.7803120069392));
#268487=CARTESIAN_POINT('Ctrl Pts',(1.2276389665983,0.955262930364784,12.7810832504053));
#268488=CARTESIAN_POINT('Ctrl Pts',(1.22353328455597,0.960516009361563,
12.7815570414815));
#268489=CARTESIAN_POINT('Ctrl Pts',(1.19524232048095,0.996237562853903,
12.7847805233195));
#268490=CARTESIAN_POINT('Ctrl Pts',(1.16995276655549,1.02581901059186,12.7874582599539));
#268491=CARTESIAN_POINT('Ctrl Pts',(1.04152227898642,1.16510860655659,12.8002870147671));
#268492=CARTESIAN_POINT('Ctrl Pts',(0.923937739193306,1.26039358871116,
12.8098415741555));
#268493=CARTESIAN_POINT('Ctrl Pts',(0.772806328867017,1.35018016463913,
12.8218075618696));
#268494=CARTESIAN_POINT('Ctrl Pts',(0.750818561725533,1.36252980584718,
12.8235391458762));
#268495=CARTESIAN_POINT('Ctrl Pts',(0.712315887237081,1.38294019052209,
12.8265631473355));
#268496=CARTESIAN_POINT('Ctrl Pts',(0.695940054740942,1.39125299074903,
12.8278468097822));
#268497=CARTESIAN_POINT('Ctrl Pts',(0.672270587057553,1.40274577125392,
12.829700605158));
#268498=CARTESIAN_POINT('Ctrl Pts',(0.665093305691609,1.40616298184091,
12.8302625195112));
#268499=CARTESIAN_POINT('Ctrl Pts',(0.652585778977298,1.41200082098948,
12.8312415366845));
#268500=CARTESIAN_POINT('Ctrl Pts',(0.647267426161632,1.41444667439876,
12.8316577624454));
#268501=CARTESIAN_POINT('Ctrl Pts',(0.636995343196801,1.41910062965395,
12.8324616174887));
#268502=CARTESIAN_POINT('Ctrl Pts',(0.63204361292717,1.42131296142817,12.832849094657));
#268503=CARTESIAN_POINT('Ctrl Pts',(0.6202980466784,1.42648712279473,12.8337681877066));
#268504=CARTESIAN_POINT('Ctrl Pts',(0.613494466018343,1.42942635866672,
12.8343005636465));
#268505=CARTESIAN_POINT('Ctrl Pts',(0.58945120747819,1.439610089999,12.8361820993049));
#268506=CARTESIAN_POINT('Ctrl Pts',(0.57210278054025,1.44659195667141,12.8375400454521));
#268507=CARTESIAN_POINT('Ctrl Pts',(0.45366101912095,1.49179501438343,12.8468173264569));
#268508=CARTESIAN_POINT('Ctrl Pts',(0.34896724615083,1.51969531058973,12.8550794889915));
#268509=CARTESIAN_POINT('Ctrl Pts',(0.168152024005762,1.54820285716115,
12.8692633673445));
#268510=CARTESIAN_POINT('Ctrl Pts',(0.093302731761542,1.55451052067063,
12.8751018308152));
#268511=CARTESIAN_POINT('Ctrl Pts',(-0.0134353899226439,1.5557654713372,
12.8831863143454));
#268512=CARTESIAN_POINT('Ctrl Pts',(-0.0451649484647025,1.55516790270789,
12.8855583847279));
#268513=CARTESIAN_POINT('Ctrl Pts',(-0.0834904111891236,1.55327193833299,
12.8883693715831));
#268514=CARTESIAN_POINT('Ctrl Pts',(-0.0901220650063386,1.55290127852089,
12.8888538007289));
#268515=CARTESIAN_POINT('Ctrl Pts',(-0.100471855152008,1.55225627800856,
12.8896065482265));
#268516=CARTESIAN_POINT('Ctrl Pts',(-0.104191618366901,1.55201103531839,
12.8898764263521));
#268517=CARTESIAN_POINT('Ctrl Pts',(-0.111128678421574,1.55152862476989,
12.8903784465026));
#268518=CARTESIAN_POINT('Ctrl Pts',(-0.114346088047813,1.55129482340083,
12.8906107638171));
#268519=CARTESIAN_POINT('Ctrl Pts',(-0.121714770198221,1.55073630970753,
12.8911416624902));
#268520=CARTESIAN_POINT('Ctrl Pts',(-0.125865481649582,1.55040493715256,
12.8914398690967));
#268521=CARTESIAN_POINT('Ctrl Pts',(-0.136760923365318,1.54949105487974,
12.8922205517017));
#268522=CARTESIAN_POINT('Ctrl Pts',(-0.143503365503485,1.54888116645628,
12.8927015509941));
#268523=CARTESIAN_POINT('Ctrl Pts',(-0.1911323947483,1.54425919012869,12.896085804839));
#268524=CARTESIAN_POINT('Ctrl Pts',(-0.231854302044268,1.53867226965545,
12.8989087314909));
#268525=CARTESIAN_POINT('Ctrl Pts',(-0.31308739480184,1.52422825958511,
12.9044841285828));
#268526=CARTESIAN_POINT('Ctrl Pts',(-0.35355983257934,1.51535187651162,
12.9072336623691));
#268527=CARTESIAN_POINT('Ctrl Pts',(-0.439317677535034,1.4929200410687,
12.9130868951461));
#268528=CARTESIAN_POINT('Ctrl Pts',(-0.484435839807965,1.47889560521561,
12.9161833770986));
#268529=CARTESIAN_POINT('Ctrl Pts',(-0.616204196510021,1.43125870218765,
12.925435586729));
#268530=CARTESIAN_POINT('Ctrl Pts',(-0.700544290145323,1.39192056937093,
12.9316466269394));
#268531=CARTESIAN_POINT('Ctrl Pts',(-0.792103182272308,1.33877617675636,
12.9390429035172));
#268532=CARTESIAN_POINT('Ctrl Pts',(-0.803259054430659,1.33211259895255,
12.9399555749378));
#268533=CARTESIAN_POINT('Ctrl Pts',(-0.820228387576899,1.3216858820524,
12.9413622624499));
#268534=CARTESIAN_POINT('Ctrl Pts',(-0.826102583131821,1.3180222676205,
12.9418526437559));
#268535=CARTESIAN_POINT('Ctrl Pts',(-0.836751465092908,1.31128162479135,
12.9427480034049));
#268536=CARTESIAN_POINT('Ctrl Pts',(-0.841534152912501,1.30821740615402,
12.9431525034268));
#268537=CARTESIAN_POINT('Ctrl Pts',(-0.851924833250524,1.30147964730193,
12.944036554533));
#268538=CARTESIAN_POINT('Ctrl Pts',(-0.857526051997652,1.29779592440225,
12.9445164793394));
#268539=CARTESIAN_POINT('Ctrl Pts',(-0.87279218017388,1.28761395480967,
12.9458338847357));
#268540=CARTESIAN_POINT('Ctrl Pts',(-0.882408024098973,1.28104330593842,
12.9466740718866));
#268541=CARTESIAN_POINT('Ctrl Pts',(-0.932315867409602,1.24611200146705,
12.9510904273366));
#268542=CARTESIAN_POINT('Ctrl Pts',(-0.971312976945295,1.21595974625617,
12.9547345262802));
#268543=CARTESIAN_POINT('Ctrl Pts',(-1.1206553678197,1.08871590608621,12.9694993093467));
#268544=CARTESIAN_POINT('Ctrl Pts',(-1.21841436714455,0.978073296096773,
12.9811327007383));
#268545=CARTESIAN_POINT('Ctrl Pts',(-1.31032144964198,0.838479084850347,
12.9937749190824));
#268546=CARTESIAN_POINT('Ctrl Pts',(-1.32111561701813,0.821366601300952,
12.9952923480351));
#268547=CARTESIAN_POINT('Ctrl Pts',(-1.3384657430439,0.792633265348912,
12.9977814551326));
#268548=CARTESIAN_POINT('Ctrl Pts',(-1.3452113011274,0.781130351486874,
12.9987627146716));
#268549=CARTESIAN_POINT('Ctrl Pts',(-1.35424656077656,0.765258643229806,
13.0000945341625));
#268550=CARTESIAN_POINT('Ctrl Pts',(-1.35666439424859,0.760964034351721,
13.000452711198));
#268551=CARTESIAN_POINT('Ctrl Pts',(-1.36069218683463,0.75372956429974,
13.0010523159055));
#268552=CARTESIAN_POINT('Ctrl Pts',(-1.36231311079477,0.75079589256053,
13.001294430726));
#268553=CARTESIAN_POINT('Ctrl Pts',(-1.36537122967589,0.745218564666876,
13.0017527367919));
#268554=CARTESIAN_POINT('Ctrl Pts',(-1.3668102515783,0.742575949350076,
13.00196904677));
#268555=CARTESIAN_POINT('Ctrl Pts',(-1.37056229000855,0.735637859191506,
13.0025348024319));
#268556=CARTESIAN_POINT('Ctrl Pts',(-1.37286280772509,0.731335602550337,
13.0028834622806));
#268557=CARTESIAN_POINT('Ctrl Pts',(-1.3807844238112,0.716352083656887,
13.0040905093476));
#268558=CARTESIAN_POINT('Ctrl Pts',(-1.38630160289683,0.70561591698935,
13.0049426829418));
#268559=CARTESIAN_POINT('Ctrl Pts',(-1.43569331840376,0.606685970181726,
13.0126895163759));
#268560=CARTESIAN_POINT('Ctrl Pts',(-1.47122953742331,0.514560931490708,
13.019148654988));
#268561=CARTESIAN_POINT('Ctrl Pts',(-1.52836752342796,0.310638897373222,
13.0330874556989));
#268562=CARTESIAN_POINT('Ctrl Pts',(-1.54691801183598,0.198603903938476,
13.0405499501285));
#268563=CARTESIAN_POINT('Ctrl Pts',(-1.55399221543649,0.0701820582762164,
13.0495071809115));
#268564=CARTESIAN_POINT('Ctrl Pts',(-1.55461075640187,0.0547968371795999,
13.0505861641577));
#268565=CARTESIAN_POINT('Ctrl Pts',(-1.55518843906608,0.0320005674855285,
13.0521947456539));
#268566=CARTESIAN_POINT('Ctrl Pts',(-1.55532318863349,0.0245945685074745,
13.052718874717));
#268567=CARTESIAN_POINT('Ctrl Pts',(-1.55546882978987,0.0114149699964946,
13.0536544703676));
#268568=CARTESIAN_POINT('Ctrl Pts',(-1.55550048266985,0.00564169813958446,
13.0540652819445));
#268569=CARTESIAN_POINT('Ctrl Pts',(-1.55549945402464,-0.00652181833482271,
13.0549329319355));
#268570=CARTESIAN_POINT('Ctrl Pts',(-1.55545953505878,-0.0129119375274382,
13.0553899885487));
#268571=CARTESIAN_POINT('Ctrl Pts',(-1.55524955990949,-0.0298324091756489,
13.0566036052685));
#268572=CARTESIAN_POINT('Ctrl Pts',(-1.55501193277288,-0.0403614300648564,
13.0573622568114));
#268573=CARTESIAN_POINT('Ctrl Pts',(-1.55338021559916,-0.0902126302264806,
13.060971255883));
#268574=CARTESIAN_POINT('Ctrl Pts',(-1.5506014901205,-0.129471681614499,
13.0638642355735));
#268575=CARTESIAN_POINT('Ctrl Pts',(-1.53010224199153,-0.317505513036257,
13.0779791742268));
#268576=CARTESIAN_POINT('Ctrl Pts',(-1.4924357582644,-0.463296811112938,
13.0898098144486));
#268577=CARTESIAN_POINT('Ctrl Pts',(-1.41971519652966,-0.636755720839577,
13.1041377016585));
#268578=CARTESIAN_POINT('Ctrl Pts',(-1.40359444342355,-0.671544733435485,
13.1070186084021));
#268579=CARTESIAN_POINT('Ctrl Pts',(-1.38319186676609,-0.711621084039836,
13.110318338441));
#268580=CARTESIAN_POINT('Ctrl Pts',(-1.38014259583502,-0.717517056865483,
13.1108032868958));
#268581=CARTESIAN_POINT('Ctrl Pts',(-1.37513761686939,-0.727044561098761,
13.1115859003218));
#268582=CARTESIAN_POINT('Ctrl Pts',(-1.3732050856552,-0.730688068156672,
13.1118849408291));
#268583=CARTESIAN_POINT('Ctrl Pts',(-1.36973684543953,-0.737164573033759,
13.1124160025907));
#268584=CARTESIAN_POINT('Ctrl Pts',(-1.36820680607999,-0.740000520266559,
13.1126483713304));
#268585=CARTESIAN_POINT('Ctrl Pts',(-1.36487473067632,-0.746130899563447,
13.1131502906357));
#268586=CARTESIAN_POINT('Ctrl Pts',(-1.36306957720293,-0.749423563969802,
13.1134196399628));
#268587=CARTESIAN_POINT('Ctrl Pts',(-1.35797805621914,-0.758631424012251,
13.1141723037586));
#268588=CARTESIAN_POINT('Ctrl Pts',(-1.35466493426856,-0.764531856101368,
13.1146539570812));
#268589=CARTESIAN_POINT('Ctrl Pts',(-1.33452370832511,-0.799859908895218,
13.1175350047483));
#268590=CARTESIAN_POINT('Ctrl Pts',(-1.3167742547823,-0.828755333186258,
13.1198798229291));
#268591=CARTESIAN_POINT('Ctrl Pts',(-1.19860182111201,-1.00773995271303,
13.1344828563475));
#268592=CARTESIAN_POINT('Ctrl Pts',(-1.07363450604211,-1.13995934047877,
13.1458004310081));
#268593=CARTESIAN_POINT('Ctrl Pts',(-0.913524684104517,-1.25913202035108,
13.1596344340926));
#268594=CARTESIAN_POINT('Ctrl Pts',(-0.898087159556186,-1.27018903801665,
13.1609604101024));
#268595=CARTESIAN_POINT('Ctrl Pts',(-0.876308517177886,-1.28519231286381,
13.1628223429951));
#268596=CARTESIAN_POINT('Ctrl Pts',(-0.870135092921735,-1.28938001183234,
13.1633491748046));
#268597=CARTESIAN_POINT('Ctrl Pts',(-0.859411517584092,-1.29654218679491,
13.1642627994264));
#268598=CARTESIAN_POINT('Ctrl Pts',(-0.854875412625818,-1.29953754321188,
13.1646488033143));
#268599=CARTESIAN_POINT('Ctrl Pts',(-0.845429072877646,-1.3057044463902,
13.1654517482956));
#268600=CARTESIAN_POINT('Ctrl Pts',(-0.840516482678021,-1.30887220889639,
13.165868822067));
#268601=CARTESIAN_POINT('Ctrl Pts',(-0.828923445072133,-1.31625551116972,
13.1668519598735));
#268602=CARTESIAN_POINT('Ctrl Pts',(-0.822228564445755,-1.32044796641858,
13.1674188635305));
#268603=CARTESIAN_POINT('Ctrl Pts',(-0.800109270553225,-1.33406602411455,
13.1692892962143));
#268604=CARTESIAN_POINT('Ctrl Pts',(-0.784552993855251,-1.34327344579654,
13.170600704567));
#268605=CARTESIAN_POINT('Ctrl Pts',(-0.700157411333412,-1.39125923226449,
13.1776968519611));
#268606=CARTESIAN_POINT('Ctrl Pts',(-0.628610409128113,-1.42501505368135,
13.1836563499679));
#268607=CARTESIAN_POINT('Ctrl Pts',(-0.467641120586529,-1.4864723626952,
13.1969004302794));
#268608=CARTESIAN_POINT('Ctrl Pts',(-0.377646270198764,-1.5118436641429,
13.2042063044731));
#268609=CARTESIAN_POINT('Ctrl Pts',(-0.244307568042703,-1.53677789588288,
13.2145691006185));
#268610=CARTESIAN_POINT('Ctrl Pts',(-0.202388976565711,-1.54285837769939,
13.2177601288857));
#268611=CARTESIAN_POINT('Ctrl Pts',(-0.153485974857522,-1.54792403750036,
13.2213691483664));
#268612=CARTESIAN_POINT('Ctrl Pts',(-0.146696977286281,-1.54858218114044,
13.2218676346047));
#268613=CARTESIAN_POINT('Ctrl Pts',(-0.135741630765942,-1.54957152910898,
13.2226677156232));
#268614=CARTESIAN_POINT('Ctrl Pts',(-0.131577991333384,-1.5499306266571,
13.2229707853996));
#268615=CARTESIAN_POINT('Ctrl Pts',(-0.124196362446616,-1.55053730348172,
13.2235062512743));
#268616=CARTESIAN_POINT('Ctrl Pts',(-0.12097900062946,-1.55079165205646,
13.2237390178965));
#268617=CARTESIAN_POINT('Ctrl Pts',(-0.114053647445887,-1.55131745220483,
13.2242386974867));
#268618=CARTESIAN_POINT('Ctrl Pts',(-0.1103454706002,-1.55158562442216,
13.2245054260738));
#268619=CARTESIAN_POINT('Ctrl Pts',(-0.100055748635186,-1.55229269324437,
13.2252433668086));
#268620=CARTESIAN_POINT('Ctrl Pts',(-0.0934722156499973,-1.55270303257786,
13.2257130208875));
#268621=CARTESIAN_POINT('Ctrl Pts',(-0.0559602116824918,-1.55480163031358,
13.2283758781633));
#268622=CARTESIAN_POINT('Ctrl Pts',(-0.0249867336084995,-1.55560781052316,
13.2305236779858));
#268623=CARTESIAN_POINT('Ctrl Pts',(0.077771935132967,-1.5552119128537,
13.2375422152561));
#268624=CARTESIAN_POINT('Ctrl Pts',(0.149452456779749,-1.54996721677447,
13.2422675205366));
#268625=CARTESIAN_POINT('Ctrl Pts',(0.331671817486694,-1.52387080190935,
13.2543847265251));
#268626=CARTESIAN_POINT('Ctrl Pts',(0.440758015238778,-1.49596672539899,
13.2617628725647));
#268627=CARTESIAN_POINT('Ctrl Pts',(0.563299726462704,-1.45004122688803,
13.2708374029218));
#268628=CARTESIAN_POINT('Ctrl Pts',(0.580595879495543,-1.44320286680382,
13.2721365701282));
#268629=CARTESIAN_POINT('Ctrl Pts',(0.604590995475178,-1.43321479595762,
13.2739667132268));
#268630=CARTESIAN_POINT('Ctrl Pts',(0.611396890022277,-1.43032470531911,
13.2744889727128));
#268631=CARTESIAN_POINT('Ctrl Pts',(0.623154609822524,-1.425232594751,13.2753968456621));
#268632=CARTESIAN_POINT('Ctrl Pts',(0.628116056753881,-1.42305299788104,
13.2757816939791));
#268633=CARTESIAN_POINT('Ctrl Pts',(0.63841590050243,-1.41846384934235,
13.2765843346048));
#268634=CARTESIAN_POINT('Ctrl Pts',(0.643752270606257,-1.41604998720707,
13.2770022691362));
#268635=CARTESIAN_POINT('Ctrl Pts',(0.656315508413264,-1.41028142028259,
13.2779912033803));
#268636=CARTESIAN_POINT('Ctrl Pts',(0.663530424017184,-1.40690124138273,
13.278563071082));
#268637=CARTESIAN_POINT('Ctrl Pts',(0.687383602986294,-1.39550176287826,
13.2804670420124));
#268638=CARTESIAN_POINT('Ctrl Pts',(0.70390440777325,-1.38724183832221,
13.2818074200295));
#268639=CARTESIAN_POINT('Ctrl Pts',(0.742789816014992,-1.3669268061881,
13.2850156524628));
#268640=CARTESIAN_POINT('Ctrl Pts',(0.765013231729733,-1.3546144184417,
13.2868921262663));
#268641=CARTESIAN_POINT('Ctrl Pts',(0.916648346407024,-1.2656827440796,
13.3000002758974));
#268642=CARTESIAN_POINT('Ctrl Pts',(1.0346452553648,-1.17119236350077,13.3118750782068));
#268643=CARTESIAN_POINT('Ctrl Pts',(1.16366683825793,-1.03293874591521,
13.3262852912839));
#268644=CARTESIAN_POINT('Ctrl Pts',(1.18904931408387,-1.00361611867614,
13.32920012223));
#268645=CARTESIAN_POINT('Ctrl Pts',(1.21747914611102,-0.968178251894301,
13.3325338878714));
#268646=CARTESIAN_POINT('Ctrl Pts',(1.22161309324011,-0.962956932221121,
13.333020455665));
#268647=CARTESIAN_POINT('Ctrl Pts',(1.22825677660456,-0.954454087009126,
13.3338051606405));
#268648=CARTESIAN_POINT('Ctrl Pts',(1.23078713955892,-0.951188904291931,
13.3341046850991));
#268649=CARTESIAN_POINT('Ctrl Pts',(1.2352685219935,-0.945358300140465,
13.3346362724096));
#268650=CARTESIAN_POINT('Ctrl Pts',(1.23722460088262,-0.942796862932915,
13.3348686855186));
#268651=CARTESIAN_POINT('Ctrl Pts',(1.24143966535341,-0.937241629584523,
13.3353703202518));
#268652=CARTESIAN_POINT('Ctrl Pts',(1.24369578712206,-0.934245741140031,
13.3356393427225));
#268653=CARTESIAN_POINT('Ctrl Pts',(1.2499793873529,-0.925838690796355,
13.3363901655692));
#268654=CARTESIAN_POINT('Ctrl Pts',(1.25398260134742,-0.920409360077848,
13.3368703178509));
#268655=CARTESIAN_POINT('Ctrl Pts',(1.27766374703624,-0.887850666032035,
13.3397227338609));
#268656=CARTESIAN_POINT('Ctrl Pts',(1.29649783208754,-0.860114673723011,
13.3420416761633));
#268657=CARTESIAN_POINT('Ctrl Pts',(1.40594706755979,-0.687159132722282,
13.3559831089664));
#268658=CARTESIAN_POINT('Ctrl Pts',(1.47297832753361,-0.528413330252782,
13.3667433474358));
#268659=CARTESIAN_POINT('Ctrl Pts',(1.51304023146319,-0.360957743978504,
13.3785859300394));
#268660=CARTESIAN_POINT('Ctrl Pts',(1.513270224476,-0.359992309183792,13.3786542167928));
#268661=CARTESIAN_POINT('Ctrl Pts',(1.51936667205013,-0.334292353703326,
13.3804723022116));
#268662=CARTESIAN_POINT('Ctrl Pts',(1.52462653278502,-0.30941924589726,
13.3822390451271));
#268663=CARTESIAN_POINT('Ctrl Pts',(1.53097905397723,-0.275264054449133,
13.3846801459928));
#268664=CARTESIAN_POINT('Ctrl Pts',(1.53260128702239,-0.266083542612564,
13.3853377482856));
#268665=CARTESIAN_POINT('Ctrl Pts',(1.53505142806947,-0.251451312763804,
13.3863884277084));
#268666=CARTESIAN_POINT('Ctrl Pts',(1.53593305956365,-0.246008708431925,
13.3867798019021));
#268667=CARTESIAN_POINT('Ctrl Pts',(1.53768313315552,-0.234828669009878,
13.3875849649422));
#268668=CARTESIAN_POINT('Ctrl Pts',(1.53854844178735,-0.229090838701217,
13.3879988459015));
#268669=CARTESIAN_POINT('Ctrl Pts',(1.54047677735189,-0.215800191937193,
13.3889591088162));
#268670=CARTESIAN_POINT('Ctrl Pts',(1.54151638962109,-0.20824418621481,
13.3895062187461));
#268671=CARTESIAN_POINT('Ctrl Pts',(1.54463708680179,-0.184257473754559,
13.3912469609415));
#268672=CARTESIAN_POINT('Ctrl Pts',(1.54651128561639,-0.167801521536852,
13.3924470380808));
#268673=CARTESIAN_POINT('Ctrl Pts',(1.55459948495729,-0.0850525451355771,
13.3985132266329));
#268674=CARTESIAN_POINT('Ctrl Pts',(1.55681433074755,-0.0184479522290053,
13.4035018149905));
#268675=CARTESIAN_POINT('Ctrl Pts',(1.55183858713221,0.142433535765555,
13.4157927330419));
#268676=CARTESIAN_POINT('Ctrl Pts',(1.54033839074952,0.236318001884554,
13.4231738493771));
#268677=CARTESIAN_POINT('Ctrl Pts',(1.50874237150909,0.382522225760758,
13.4346829770609));
#268678=CARTESIAN_POINT('Ctrl Pts',(1.49421843576441,0.43582058583104,13.4388775548485));
#268679=CARTESIAN_POINT('Ctrl Pts',(1.47440688443156,0.495749071166107,
13.4435151061474));
#268680=CARTESIAN_POINT('Ctrl Pts',(1.47186710097608,0.503239551856673,
13.4440932914642));
#268681=CARTESIAN_POINT('Ctrl Pts',(1.46794109286813,0.514534338862254,
13.4449625738269));
#268682=CARTESIAN_POINT('Ctrl Pts',(1.46659701925061,0.518352989893866,
13.4452560253135));
#268683=CARTESIAN_POINT('Ctrl Pts',(1.46415812027924,0.525196722987202,
13.4457810929504));
#268684=CARTESIAN_POINT('Ctrl Pts',(1.46306881013627,0.528223680334259,
13.4460130244597));
#268685=CARTESIAN_POINT('Ctrl Pts',(1.460668102007,0.534830327114244,13.446518571043));
#268686=CARTESIAN_POINT('Ctrl Pts',(1.45935293452879,0.538408577520192,
13.4467919594709));
#268687=CARTESIAN_POINT('Ctrl Pts',(1.4555743387941,0.548573648448143,13.4475674951338));
#268688=CARTESIAN_POINT('Ctrl Pts',(1.45307933713432,0.555148762501953,
13.4480678151394));
#268689=CARTESIAN_POINT('Ctrl Pts',(1.44539993475487,0.574979885537125,
13.4495734757298));
#268690=CARTESIAN_POINT('Ctrl Pts',(1.44007838871623,0.588181127766952,
13.4505712215658));
#268691=CARTESIAN_POINT('Ctrl Pts',(1.43457668314421,0.601306901822155,
13.4515605039018));
#268692=CARTESIAN_POINT('Origin',(0.,0.,-1.29405622560371));
#268693=CARTESIAN_POINT('',(1.43457668360422,0.601306900724687,14.2893889670083));
#268694=CARTESIAN_POINT('',(1.43457666475166,0.601306945702447,14.1492791259731));
#268695=CARTESIAN_POINT('',(1.43457668357355,0.601306900797845,-1.29405622560371));
#268696=CARTESIAN_POINT('Ctrl Pts',(1.43457668360422,0.601306900724687,
14.2893889670083));
#268697=CARTESIAN_POINT('Ctrl Pts',(1.43510642363156,0.600043065750092,
14.2892958059463));
#268698=CARTESIAN_POINT('Ctrl Pts',(1.43563451927348,0.598778469337572,
14.2892025954736));
#268699=CARTESIAN_POINT('Ctrl Pts',(1.45097763803968,0.561900302523962,
14.2864845633064));
#268700=CARTESIAN_POINT('Ctrl Pts',(1.46446337624145,0.525751513059345,
14.2838244665163));
#268701=CARTESIAN_POINT('Ctrl Pts',(1.47985501929301,0.479288129934118,
14.2803915511198));
#268702=CARTESIAN_POINT('Ctrl Pts',(1.48302025483501,0.469402709922828,
14.2796604297811));
#268703=CARTESIAN_POINT('Ctrl Pts',(1.48794888988238,0.453462359550888,
14.2784799473835));
#268704=CARTESIAN_POINT('Ctrl Pts',(1.48977485404067,0.447426968980638,
14.2780326369627));
#268705=CARTESIAN_POINT('Ctrl Pts',(1.49318173919188,0.435914034364007,
14.2771786098615));
#268706=CARTESIAN_POINT('Ctrl Pts',(1.49476934501179,0.430438561508871,
14.2767721187157));
#268707=CARTESIAN_POINT('Ctrl Pts',(1.49832640831333,0.417913624157321,
14.2758414867958));
#268708=CARTESIAN_POINT('Ctrl Pts',(1.50027626746597,0.410858784730702,
14.2753167199634));
#268709=CARTESIAN_POINT('Ctrl Pts',(1.50523271448447,0.392419876782316,
14.2739435229652));
#268710=CARTESIAN_POINT('Ctrl Pts',(1.50815991158616,0.381015158950399,
14.273092556915));
#268711=CARTESIAN_POINT('Ctrl Pts',(1.52992096659911,0.292048901328185,
14.2664403349478));
#268712=CARTESIAN_POINT('Ctrl Pts',(1.54288608418305,0.213188381740176,
14.2604519398788));
#268713=CARTESIAN_POINT('Ctrl Pts',(1.55888861657664,0.0276904145284185,
14.2461814623007));
#268714=CARTESIAN_POINT('Ctrl Pts',(1.55713325312661,-0.0789659695126312,
14.2378271995628));
#268715=CARTESIAN_POINT('Ctrl Pts',(1.5400575459802,-0.221829575670318,
14.2268785210513));
#268716=CARTESIAN_POINT('Ctrl Pts',(1.5342638068842,-0.258883665635753,
14.2240640623603));
#268717=CARTESIAN_POINT('Ctrl Pts',(1.52582604833923,-0.302460913689011,
14.220810521741));
#268718=CARTESIAN_POINT('Ctrl Pts',(1.52447114190434,-0.3092175227038,14.2203076906654));
#268719=CARTESIAN_POINT('Ctrl Pts',(1.52230898694001,-0.319639928743608,
14.2195347935613));
#268720=CARTESIAN_POINT('Ctrl Pts',(1.52153331987344,-0.323312067652006,
14.2192630056382));
#268721=CARTESIAN_POINT('Ctrl Pts',(1.5200765526474,-0.330087286165561,
14.218762567841));
#268722=CARTESIAN_POINT('Ctrl Pts',(1.5193992418032,-0.333191066476965,
14.2185337144139));
#268723=CARTESIAN_POINT('Ctrl Pts',(1.51784611682222,-0.340205043173597,
14.2180174387534));
#268724=CARTESIAN_POINT('Ctrl Pts',(1.51696470090874,-0.344113938868705,
14.217730339721));
#268725=CARTESIAN_POINT('Ctrl Pts',(1.51431107086636,-0.3556738793492,14.2168830122607));
#268726=CARTESIAN_POINT('Ctrl Pts',(1.51249597187433,-0.36331511079172,
14.2163251580079));
#268727=CARTESIAN_POINT('Ctrl Pts',(1.49731099727027,-0.425154273493698,
14.21182623971));
#268728=CARTESIAN_POINT('Ctrl Pts',(1.4810885217557,-0.478617613667169,
14.2080341671923));
#268729=CARTESIAN_POINT('Ctrl Pts',(1.41578279436657,-0.658392935595339,
14.1952554988008));
#268730=CARTESIAN_POINT('Ctrl Pts',(1.35311839352551,-0.779098067013249,
14.1865748042326));
#268731=CARTESIAN_POINT('Ctrl Pts',(1.25500069965703,-0.919701455304375,
14.1748824273492));
#268732=CARTESIAN_POINT('Ctrl Pts',(1.23337076002019,-0.948511330104299,
14.1723946758144));
#268733=CARTESIAN_POINT('Ctrl Pts',(1.20439214639933,-0.98444032425386,
14.1691560255389));
#268734=CARTESIAN_POINT('Ctrl Pts',(1.19794541529606,-0.992275147130088,
14.1684411538262));
#268735=CARTESIAN_POINT('Ctrl Pts',(1.18740182208363,-1.00483644263579,
14.1672806253067));
#268736=CARTESIAN_POINT('Ctrl Pts',(1.18335221288825,-1.00960234830909,
14.166836894656));
#268737=CARTESIAN_POINT('Ctrl Pts',(1.17554798188747,-1.01867553272687,
14.1659854913553));
#268738=CARTESIAN_POINT('Ctrl Pts',(1.17179814339994,-1.02298680745084,
14.1655780203292));
#268739=CARTESIAN_POINT('Ctrl Pts',(1.16320552875811,-1.03275669749077,
14.1646479110233));
#268740=CARTESIAN_POINT('Ctrl Pts',(1.15834795537023,-1.03820205609117,
14.1641246608388));
#268741=CARTESIAN_POINT('Ctrl Pts',(1.14542507174974,-1.05248506220085,
14.1627391896757));
#268742=CARTESIAN_POINT('Ctrl Pts',(1.13729593924475,-1.06126402598284,
14.1618742878627));
#268743=CARTESIAN_POINT('Ctrl Pts',(1.06344518721115,-1.13919529438871,
14.1540739772809));
#268744=CARTESIAN_POINT('Ctrl Pts',(0.991605851365938,-1.20224492947703,
14.146866192723));
#268745=CARTESIAN_POINT('Ctrl Pts',(0.840141542172154,-1.31231958673576,
14.1324267164581));
#268746=CARTESIAN_POINT('Ctrl Pts',(0.761184553683046,-1.35963932549793,
14.125236452795));
#268747=CARTESIAN_POINT('Ctrl Pts',(0.645953894423232,-1.41549742045255,
14.1155018825313));
#268748=CARTESIAN_POINT('Ctrl Pts',(0.612851497056703,-1.4301408838063,
14.1127879729051));
#268749=CARTESIAN_POINT('Ctrl Pts',(0.572928962189321,-1.44616018064728,
14.1096353094923));
#268750=CARTESIAN_POINT('Ctrl Pts',(0.566575779084717,-1.4486610214193,
14.1091371619));
#268751=CARTESIAN_POINT('Ctrl Pts',(0.556717660917583,-1.45246675676604,
14.1083699138952));
#268752=CARTESIAN_POINT('Ctrl Pts',(0.553224246933727,-1.45380093784985,
14.1080991302809));
#268753=CARTESIAN_POINT('Ctrl Pts',(0.546753090118514,-1.45624565513195,
14.107599620471));
#268754=CARTESIAN_POINT('Ctrl Pts',(0.543776776856625,-1.45735965600731,
14.1073706967387));
#268755=CARTESIAN_POINT('Ctrl Pts',(0.537023444886674,-1.45986378372471,
14.1068530983014));
#268756=CARTESIAN_POINT('Ctrl Pts',(0.533244436396847,-1.46124837704856,
14.1065647540256));
#268757=CARTESIAN_POINT('Ctrl Pts',(0.523446873793777,-1.46479504253782,
14.1058204183328));
#268758=CARTESIAN_POINT('Ctrl Pts',(0.517420204688105,-1.46693472310291,
14.1053657121367));
#268759=CARTESIAN_POINT('Ctrl Pts',(0.478761759015114,-1.48039195215472,
14.1024680292886));
#268760=CARTESIAN_POINT('Ctrl Pts',(0.445770819136474,-1.49065824034146,
14.1000817686897));
#268761=CARTESIAN_POINT('Ctrl Pts',(0.393489843388598,-1.50503593705312,
14.0963943809113));
#268762=CARTESIAN_POINT('Ctrl Pts',(0.374419364428812,-1.50989324912639,
14.0950686171438));
#268763=CARTESIAN_POINT('Ctrl Pts',(0.274226625088214,-1.53339753127321,
14.0881796074168));
#268764=CARTESIAN_POINT('Ctrl Pts',(0.191794339524217,-1.5458732989144,
14.0827648639141));
#268765=CARTESIAN_POINT('Ctrl Pts',(0.0225543798508679,-1.55773519677699,
14.0715401863919));
#268766=CARTESIAN_POINT('Ctrl Pts',(-0.063988810093637,-1.55658269572875,
14.0657401640109));
#268767=CARTESIAN_POINT('Ctrl Pts',(-0.162664829078716,-1.54702385202516,
14.0588115741827));
#268768=CARTESIAN_POINT('Ctrl Pts',(-0.175332975959581,-1.54563934211039,
14.0579163100236));
#268769=CARTESIAN_POINT('Ctrl Pts',(-0.194750207432216,-1.54327544183502,
14.0565345834734));
#268770=CARTESIAN_POINT('Ctrl Pts',(-0.201512468268516,-1.54240703289295,
14.0560516090263));
#268771=CARTESIAN_POINT('Ctrl Pts',(-0.213825760922436,-1.54074340451008,
14.0551688329878));
#268772=CARTESIAN_POINT('Ctrl Pts',(-0.219378648311558,-1.53996256504178,
14.0547694910442));
#268773=CARTESIAN_POINT('Ctrl Pts',(-0.231491250414504,-1.53819246484057,
14.0538956321503));
#268774=CARTESIAN_POINT('Ctrl Pts',(-0.238049075273868,-1.53719123506156,
14.0534207443418));
#268775=CARTESIAN_POINT('Ctrl Pts',(-0.256017765360416,-1.53433008826178,
14.0521145448663));
#268776=CARTESIAN_POINT('Ctrl Pts',(-0.267414409566224,-1.53238488509148,
14.0512805544763));
#268777=CARTESIAN_POINT('Ctrl Pts',(-0.327351064457082,-1.5214657963856,
14.0468643284272));
#268778=CARTESIAN_POINT('Ctrl Pts',(-0.375459893498453,-1.51031313222582,
14.0432137546576));
#268779=CARTESIAN_POINT('Ctrl Pts',(-0.563406098753759,-1.45720826746905,
14.0285161612423));
#268780=CARTESIAN_POINT('Ctrl Pts',(-0.697549418085453,-1.39796187754212,
14.0169644034898));
#268781=CARTESIAN_POINT('Ctrl Pts',(-0.848166289265676,-1.3042941307266,
14.0035347745476));
#268782=CARTESIAN_POINT('Ctrl Pts',(-0.874364157900145,-1.28687874797435,
14.0011839877682));
#268783=CARTESIAN_POINT('Ctrl Pts',(-0.905375794037493,-1.26487867861151,
13.9983989869758));
#268784=CARTESIAN_POINT('Ctrl Pts',(-0.910709420163506,-1.26104391525003,
13.9979199218419));
#268785=CARTESIAN_POINT('Ctrl Pts',(-0.918995678434938,-1.25500627900246,
13.9971757282376));
#268786=CARTESIAN_POINT('Ctrl Pts',(-0.921964965607764,-1.25282657230593,
13.9969090703319));
#268787=CARTESIAN_POINT('Ctrl Pts',(-0.927486778227432,-1.24874283435745,
13.9964132534112));
#268788=CARTESIAN_POINT('Ctrl Pts',(-0.930041174895956,-1.24684153100951,
13.9961839218546));
#268789=CARTESIAN_POINT('Ctrl Pts',(-0.93587354453081,-1.24247245150107,
13.9956603516606));
#268790=CARTESIAN_POINT('Ctrl Pts',(-0.939147603576829,-1.23999954186706,
13.9953664754453));
#268791=CARTESIAN_POINT('Ctrl Pts',(-0.94770645285149,-1.23348166531379,
13.9945982202367));
#268792=CARTESIAN_POINT('Ctrl Pts',(-0.952975210616525,-1.22941563012079,
13.9941252668691));
#268793=CARTESIAN_POINT('Ctrl Pts',(-0.989492067658269,-1.20085882590092,
13.9908458626741));
#268794=CARTESIAN_POINT('Ctrl Pts',(-1.01982188986394,-1.17521081263067,
13.9881145682104));
#268795=CARTESIAN_POINT('Ctrl Pts',(-1.16023542700811,-1.04693676537881,
13.9752463257933));
#268796=CARTESIAN_POINT('Ctrl Pts',(-1.25601908796069,-0.929862827458389,
13.9656960119448));
#268797=CARTESIAN_POINT('Ctrl Pts',(-1.35294289368544,-0.768473671828879,
13.952876749384));
#268798=CARTESIAN_POINT('Ctrl Pts',(-1.37119805597474,-0.735405841287683,
13.9502712236113));
#268799=CARTESIAN_POINT('Ctrl Pts',(-1.39288081512394,-0.692509589513686,
13.9468997415392));
#268800=CARTESIAN_POINT('Ctrl Pts',(-1.39743907059523,-0.683264613150348,
13.9461736392021));
#268801=CARTESIAN_POINT('Ctrl Pts',(-1.40463023514552,-0.668306600677126,
13.9449993208265));
#268802=CARTESIAN_POINT('Ctrl Pts',(-1.40732101430308,-0.662621589281365,
13.9445531166446));
#268803=CARTESIAN_POINT('Ctrl Pts',(-1.41238643843066,-0.651749447734409,
13.9436999190605));
#268804=CARTESIAN_POINT('Ctrl Pts',(-1.4147671764514,-0.646565254963968,
13.9432931438775));
#268805=CARTESIAN_POINT('Ctrl Pts',(-1.42014969815926,-0.634672435659164,
13.9423600449609));
#268806=CARTESIAN_POINT('Ctrl Pts',(-1.42313254027963,-0.627955440400696,
13.9418330831641));
#268807=CARTESIAN_POINT('Ctrl Pts',(-1.4308101664857,-0.610330677333528,
13.9404503668461));
#268808=CARTESIAN_POINT('Ctrl Pts',(-1.43542775780959,-0.599390028089579,
13.9395920185953));
#268809=CARTESIAN_POINT('Ctrl Pts',(-1.47209461872559,-0.509659367487536,
13.9325505508937));
#268810=CARTESIAN_POINT('Ctrl Pts',(-1.49775130286952,-0.428429134032381,
13.9261536139243));
#268811=CARTESIAN_POINT('Ctrl Pts',(-1.53228263841126,-0.276857080910632,
13.9142108919993));
#268812=CARTESIAN_POINT('Ctrl Pts',(-1.54324448647616,-0.207209614375265,
13.9087240440755));
#268813=CARTESIAN_POINT('Ctrl Pts',(-1.55349617243896,-0.0913174537903301,
13.8997352703765));
#268814=CARTESIAN_POINT('Ctrl Pts',(-1.55551523355228,-0.0454119413306816,
13.8962123141049));
#268815=CARTESIAN_POINT('Ctrl Pts',(-1.55549869742765,0.00416514605386303,
13.8924873319056));
#268816=CARTESIAN_POINT('Ctrl Pts',(-1.55548466003159,0.00781139927385783,
13.8922138397129));
#268817=CARTESIAN_POINT('Ctrl Pts',(-1.55530944731517,0.0315978658981645,
13.8904329013735));
#268818=CARTESIAN_POINT('Ctrl Pts',(-1.55476992860723,0.0517346559627735,
13.8889401577351));
#268819=CARTESIAN_POINT('Ctrl Pts',(-1.55356545931134,0.0777803327808232,
13.8870333551244));
#268820=CARTESIAN_POINT('Ctrl Pts',(-1.55325763646708,0.0837026544015386,
13.8866013896784));
#268821=CARTESIAN_POINT('Ctrl Pts',(-1.55271183589274,0.0931598309754612,
13.885914316331));
#268822=CARTESIAN_POINT('Ctrl Pts',(-1.55249564301516,0.0966958041096516,
13.8856580319886));
#268823=CARTESIAN_POINT('Ctrl Pts',(-1.55206014726408,0.103440279047142,
13.8851703964523));
#268824=CARTESIAN_POINT('Ctrl Pts',(-1.55184297704861,0.10664880147417,
13.884938938198));
#268825=CARTESIAN_POINT('Ctrl Pts',(-1.55130828652724,0.114200768753752,
13.8843953433217));
#268826=CARTESIAN_POINT('Ctrl Pts',(-1.55098247404556,0.118543586394214,
13.8840836718114));
#268827=CARTESIAN_POINT('Ctrl Pts',(-1.54985135725508,0.132816707213509,
13.8830622087196));
#268828=CARTESIAN_POINT('Ctrl Pts',(-1.54896886718134,0.142740917409205,
13.882356559669));
#268829=CARTESIAN_POINT('Ctrl Pts',(-1.546633599569,0.166421389750078,13.8806822542213));
#268830=CARTESIAN_POINT('Ctrl Pts',(-1.54509254556125,0.180168331531759,
13.8797179345087));
#268831=CARTESIAN_POINT('Ctrl Pts',(-1.53867436904587,0.231256235348058,
13.8761565459136));
#268832=CARTESIAN_POINT('Ctrl Pts',(-1.53262489373753,0.268439267809651,
13.8736088610586));
#268833=CARTESIAN_POINT('Ctrl Pts',(-1.49826252131152,0.440069658214332,
13.8619052633682));
#268834=CARTESIAN_POINT('Ctrl Pts',(-1.45357114256359,0.570599769147444,
13.8531082460646));
#268835=CARTESIAN_POINT('Ctrl Pts',(-1.37680317210424,0.724709481668072,
13.841361226969));
#268836=CARTESIAN_POINT('Ctrl Pts',(-1.36025022100336,0.755321011010828,
13.8389578045322));
#268837=CARTESIAN_POINT('Ctrl Pts',(-1.33741841882751,0.794355760157811,
13.8357863967801));
#268838=CARTESIAN_POINT('Ctrl Pts',(-1.33206051093637,0.803308089395746,
13.8350515628939));
#268839=CARTESIAN_POINT('Ctrl Pts',(-1.32331445159441,0.817593432724739,
13.8338665206161));
#268840=CARTESIAN_POINT('Ctrl Pts',(-1.3199830903128,0.822960994325506,
13.8334183917417));
#268841=CARTESIAN_POINT('Ctrl Pts',(-1.31358475367028,0.833131332217873,
13.8325637407926));
#268842=CARTESIAN_POINT('Ctrl Pts',(-1.31052389448628,0.837937851030816,
13.8321574496257));
#268843=CARTESIAN_POINT('Ctrl Pts',(-1.30348310073282,0.848861184646816,
13.8312285935015));
#268844=CARTESIAN_POINT('Ctrl Pts',(-1.29948641831693,0.85496698763336,
13.8307054111437));
#268845=CARTESIAN_POINT('Ctrl Pts',(-1.28707968511959,0.873633000769312,
13.8290935498743));
#268846=CARTESIAN_POINT('Ctrl Pts',(-1.27852962089448,0.886098591796523,
13.8279996375153));
#268847=CARTESIAN_POINT('Ctrl Pts',(-1.25840919810705,0.914535641405829,
13.8254626644934));
#268848=CARTESIAN_POINT('Ctrl Pts',(-1.24671425993316,0.930415304044121,
13.8240150046247));
#268849=CARTESIAN_POINT('Ctrl Pts',(-1.20543176783678,0.984293438906693,
13.8189937299405));
#268850=CARTESIAN_POINT('Ctrl Pts',(-1.17438601061904,1.021134656924,13.8153666864828));
#268851=CARTESIAN_POINT('Ctrl Pts',(-1.0811288902787,1.1219135072548,13.8048860701825));
#268852=CARTESIAN_POINT('Ctrl Pts',(-1.01506091612326,1.18202336306852,
13.7979248322068));
#268853=CARTESIAN_POINT('Ctrl Pts',(-0.895377679050786,1.27344245844416,
13.7863069990047));
#268854=CARTESIAN_POINT('Ctrl Pts',(-0.844366127486653,1.30782441175503,
13.7816197385012));
#268855=CARTESIAN_POINT('Ctrl Pts',(-0.784630385465915,1.34312996941277,
13.7765212468718));
#268856=CARTESIAN_POINT('Ctrl Pts',(-0.777782423342916,1.34710707279357,
13.7759423328059));
#268857=CARTESIAN_POINT('Ctrl Pts',(-0.767411880095811,1.3530245465355,
13.775074316669));
#268858=CARTESIAN_POINT('Ctrl Pts',(-0.763911797365107,1.35500375795572,
13.7747828386143));
#268859=CARTESIAN_POINT('Ctrl Pts',(-0.757631889322544,1.35852282577063,
13.7742625597066));
#268860=CARTESIAN_POINT('Ctrl Pts',(-0.75485499515718,1.36006775007228,
13.774033440954));
#268861=CARTESIAN_POINT('Ctrl Pts',(-0.748797470660418,1.36341358467278,
13.7735356929672));
#268862=CARTESIAN_POINT('Ctrl Pts',(-0.745515074148207,1.36521116679979,
13.7732672756406));
#268863=CARTESIAN_POINT('Ctrl Pts',(-0.736214431294065,1.37026105427154,
13.7725102872313));
#268864=CARTESIAN_POINT('Ctrl Pts',(-0.730181072184381,1.37348558497319,
13.7720234356829));
#268865=CARTESIAN_POINT('Ctrl Pts',(-0.691866477595388,1.39363900378096,
13.7689569757977));
#268866=CARTESIAN_POINT('Ctrl Pts',(-0.659016668405864,1.40947027716365,
13.7664407937663));
#268867=CARTESIAN_POINT('Ctrl Pts',(-0.577698982879933,1.44519402812156,
13.760408867415));
#268868=CARTESIAN_POINT('Ctrl Pts',(-0.528724072290274,1.4638215390211,
13.7569393300948));
#268869=CARTESIAN_POINT('Ctrl Pts',(-0.357779981470167,1.51913788168171,
13.7450920664581));
#268870=CARTESIAN_POINT('Ctrl Pts',(-0.232323442074437,1.54331064014915,
13.7367975492238));
#268871=CARTESIAN_POINT('Ctrl Pts',(-0.0876692729125478,1.55312835300434,
13.7267329859269));
#268872=CARTESIAN_POINT('Ctrl Pts',(-0.0699901918887989,1.55402538935513,
13.725495536695));
#268873=CARTESIAN_POINT('Ctrl Pts',(-0.0451148681929885,1.55486224052582,
13.7237422908924));
#268874=CARTESIAN_POINT('Ctrl Pts',(-0.0379279934085873,1.55505414778454,
13.7232343353313));
#268875=CARTESIAN_POINT('Ctrl Pts',(-0.0254184584830591,1.55530141241899,
13.7223476022687));
#268876=CARTESIAN_POINT('Ctrl Pts',(-0.0200963196289022,1.55537928434101,
13.7219695319587));
#268877=CARTESIAN_POINT('Ctrl Pts',(-0.00897005928959219,1.55548496494596,
13.7211774011916));
#268878=CARTESIAN_POINT('Ctrl Pts',(-0.00316598331366182,1.55550760621891,
13.7207631854895));
#268879=CARTESIAN_POINT('Ctrl Pts',(0.0106258773889423,1.55548421622053,
13.7197764733789));
#268880=CARTESIAN_POINT('Ctrl Pts',(0.0186133790661768,1.55540914035031,
13.7192030796356));
#268881=CARTESIAN_POINT('Ctrl Pts',(0.0455390572294313,1.55494863072896,
13.7172634051839));
#268882=CARTESIAN_POINT('Ctrl Pts',(0.0644699897829865,1.55427880749964,
13.7158883246744));
#268883=CARTESIAN_POINT('Ctrl Pts',(0.10967387793181,1.55185214542411,13.7125762551443));
#268884=CARTESIAN_POINT('Ctrl Pts',(0.135922932076452,1.54977361096245,
13.7106297922839));
#268885=CARTESIAN_POINT('Ctrl Pts',(0.310417488702593,1.53148923671992,
13.6975320383032));
#268886=CARTESIAN_POINT('Ctrl Pts',(0.455716652937254,1.49469953382833,
13.685755728808));
#268887=CARTESIAN_POINT('Ctrl Pts',(0.629278418229681,1.42305510441386,
13.6714481623336));
#268888=CARTESIAN_POINT('Ctrl Pts',(0.664481824163188,1.40696186281549,
13.6685392375838));
#268889=CARTESIAN_POINT('Ctrl Pts',(0.70495127858869,1.38660288399937,13.6652153954514));
#268890=CARTESIAN_POINT('Ctrl Pts',(0.710832011863789,1.38359738296306,
13.6647329185618));
#268891=CARTESIAN_POINT('Ctrl Pts',(0.720321475707622,1.37867107407236,
13.6639554230796));
#268892=CARTESIAN_POINT('Ctrl Pts',(0.723942006627118,1.37677337674962,
13.6636590344032));
#268893=CARTESIAN_POINT('Ctrl Pts',(0.730368362679882,1.37337265000639,
13.6631334533313));
#268894=CARTESIAN_POINT('Ctrl Pts',(0.733177091196946,1.37187526205131,
13.6629039151919));
#268895=CARTESIAN_POINT('Ctrl Pts',(0.739235442990032,1.36862151591274,
13.6624091937249));
#268896=CARTESIAN_POINT('Ctrl Pts',(0.742483408793337,1.36686220316036,
13.6621442008693));
#268897=CARTESIAN_POINT('Ctrl Pts',(0.751531759605301,1.36191924992618,
13.6614065363533));
#268898=CARTESIAN_POINT('Ctrl Pts',(0.757318236863859,1.35871009465218,
13.6609354474234));
#268899=CARTESIAN_POINT('Ctrl Pts',(0.791193813306958,1.33963919614724,
13.6581803409233));
#268900=CARTESIAN_POINT('Ctrl Pts',(0.818806991269441,1.32294229676711,
13.6559457822308));
#268901=CARTESIAN_POINT('Ctrl Pts',(0.971991577838283,1.22368033191457,
13.6434955326567));
#268902=CARTESIAN_POINT('Ctrl Pts',(1.08560070714567,1.12411788947292,13.6339761488987));
#268903=CARTESIAN_POINT('Ctrl Pts',(1.21222105476563,0.975757562258376,
13.6207765181854));
#268904=CARTESIAN_POINT('Ctrl Pts',(1.23978604282488,0.940485320867346,
13.6177037630854));
#268905=CARTESIAN_POINT('Ctrl Pts',(1.2723151556437,0.894941571335043,13.6137844018349));
#268906=CARTESIAN_POINT('Ctrl Pts',(1.27874056979808,0.885736312250796,
13.6129946273594));
#268907=CARTESIAN_POINT('Ctrl Pts',(1.28876034967867,0.871045353410482,
13.6117375346395));
#268908=CARTESIAN_POINT('Ctrl Pts',(1.29242071696767,0.865604952946545,
13.6112727176601));
#268909=CARTESIAN_POINT('Ctrl Pts',(1.29917953367074,0.855420885069376,
13.61040384407));
#268910=CARTESIAN_POINT('Ctrl Pts',(1.30228668646884,0.850683099637103,
13.6100001225079));
#268911=CARTESIAN_POINT('Ctrl Pts',(1.30913843912789,0.840110033934366,
13.6091001848727));
#268912=CARTESIAN_POINT('Ctrl Pts',(1.31287002766012,0.834266509881198,
13.608603495805));
#268913=CARTESIAN_POINT('Ctrl Pts',(1.3236440530544,0.81714349543857,13.607149936131));
#268914=CARTESIAN_POINT('Ctrl Pts',(1.330580913642,0.805798661670588,13.6061892187042));
#268915=CARTESIAN_POINT('Ctrl Pts',(1.34593906480333,0.779942149024446,
13.6040042634589));
#268916=CARTESIAN_POINT('Ctrl Pts',(1.35427260094002,0.765380561398834,
13.6027770111668));
#268917=CARTESIAN_POINT('Ctrl Pts',(1.38072989315217,0.7173651296398,13.5987397398097));
#268918=CARTESIAN_POINT('Ctrl Pts',(1.39786086528448,0.683383006565913,
13.5958968047415));
#268919=CARTESIAN_POINT('Ctrl Pts',(1.42094296181424,0.633088123108505,
13.5917105661335));
#268920=CARTESIAN_POINT('Ctrl Pts',(1.42789341460871,0.617251608647841,
13.5903955059367));
#268921=CARTESIAN_POINT('Ctrl Pts',(1.43457670670211,0.601306845618552,
13.5890749702576));
#268922=CARTESIAN_POINT('',(-1.55549951545175,-0.00134136213463568,13.7562673034149));
#268923=CARTESIAN_POINT('Ctrl Pts',(1.43457668314421,0.601306901822155,
13.4515605039018));
#268924=CARTESIAN_POINT('Ctrl Pts',(1.42491482403355,0.624357822664694,
13.4532978390657));
#268925=CARTESIAN_POINT('Ctrl Pts',(1.41469733731682,0.647175991875524,
13.4550090885635));
#268926=CARTESIAN_POINT('Ctrl Pts',(1.35292712151481,0.776660653332891,
13.4647256675113));
#268927=CARTESIAN_POINT('Ctrl Pts',(1.28987237647954,0.877409177485551,
13.4723368859934));
#268928=CARTESIAN_POINT('Ctrl Pts',(1.17468647016616,1.02180141387318,13.4846626878756));
#268929=CARTESIAN_POINT('Ctrl Pts',(1.13012664881844,1.07087739654077,13.4891551949743));
#268930=CARTESIAN_POINT('Ctrl Pts',(1.07434407638805,1.12494292997761,13.4945845415706));
#268931=CARTESIAN_POINT('Ctrl Pts',(1.06602061085322,1.13283354251355,13.4953898810427));
#268932=CARTESIAN_POINT('Ctrl Pts',(1.05227617988597,1.14557759080823,13.4967124911391));
#268933=CARTESIAN_POINT('Ctrl Pts',(1.04690696526504,1.15048640937279,13.4972273998412));
#268934=CARTESIAN_POINT('Ctrl Pts',(1.03722633739703,1.1592130679131,13.4981527566677));
#268935=CARTESIAN_POINT('Ctrl Pts',(1.03292775444979,1.16304499666431,13.4985626030537));
#268936=CARTESIAN_POINT('Ctrl Pts',(1.02375751441355,1.17112877698053,13.4994347851006));
#268937=CARTESIAN_POINT('Ctrl Pts',(1.01888043804736,1.1753742855888,13.4998973733425));
#268938=CARTESIAN_POINT('Ctrl Pts',(1.00572949336778,1.18667886239086,13.501141448177));
#268939=CARTESIAN_POINT('Ctrl Pts',(0.997407957952652,1.1936816537615,13.5019252172642));
#268940=CARTESIAN_POINT('Ctrl Pts',(0.955411117453664,1.22827733973371,
13.5058643974196));
#268941=CARTESIAN_POINT('Ctrl Pts',(0.92066447964419,1.254532522117,13.5090725162834));
#268942=CARTESIAN_POINT('Ctrl Pts',(0.742060889928688,1.37806955984452,
13.5253335989984));
#268943=CARTESIAN_POINT('Ctrl Pts',(0.583761386538825,1.45221755675548,
13.5392159625137));
#268944=CARTESIAN_POINT('Ctrl Pts',(0.403116580464746,1.50242156626473,
13.5531371381978));
#268945=CARTESIAN_POINT('Ctrl Pts',(0.38967143678975,1.50596472321581,13.5541613548444));
#268946=CARTESIAN_POINT('Ctrl Pts',(0.371163106854808,1.510577681094,13.5555533471034));
#268947=CARTESIAN_POINT('Ctrl Pts',(0.366139932036013,1.51180307405809,
13.5559293338634));
#268948=CARTESIAN_POINT('Ctrl Pts',(0.358129953326154,1.51371482689133,
13.5565259192799));
#268949=CARTESIAN_POINT('Ctrl Pts',(0.355147130667341,1.51441743143822,
13.5567474276248));
#268950=CARTESIAN_POINT('Ctrl Pts',(0.348948164385919,1.51585827727611,
13.5572063882515));
#268951=CARTESIAN_POINT('Ctrl Pts',(0.345731731505761,1.51659510361663,
13.5574437519777));
#268952=CARTESIAN_POINT('Ctrl Pts',(0.337963820233271,1.5183485947983,13.5580151822512));
#268953=CARTESIAN_POINT('Ctrl Pts',(0.333410015257791,1.5193550481537,13.5583486695394));
#268954=CARTESIAN_POINT('Ctrl Pts',(0.317519410930875,1.52279220583716,
13.5595073655911));
#268955=CARTESIAN_POINT('Ctrl Pts',(0.306159649201728,1.52511670663915,
13.5603268032607));
#268956=CARTESIAN_POINT('Ctrl Pts',(0.237248552546934,1.53841667915043,
13.5652500041482));
#268957=CARTESIAN_POINT('Ctrl Pts',(0.179133733721364,1.54626180991327,
13.5692018582337));
#268958=CARTESIAN_POINT('Ctrl Pts',(0.0185697998232404,1.55875939697581,
13.5799122249702));
#268959=CARTESIAN_POINT('Ctrl Pts',(-0.0841022821022617,1.55659974997274,
13.5865459877373));
#268960=CARTESIAN_POINT('Ctrl Pts',(-0.203457621590718,1.54223893461175,
13.5946132004922));
#268961=CARTESIAN_POINT('Ctrl Pts',(-0.221059791182818,1.53981442767176,
13.5958115598582));
#268962=CARTESIAN_POINT('Ctrl Pts',(-0.27913610129727,1.53079872051998,
13.5998004262197));
#268963=CARTESIAN_POINT('Ctrl Pts',(-0.319388137313364,1.52290919163844,
13.6026221209597));
#268964=CARTESIAN_POINT('Ctrl Pts',(-0.370107750335763,1.51086874961113,
13.6062740927559));
#268965=CARTESIAN_POINT('Ctrl Pts',(-0.380908571754019,1.50818194325879,
13.6070573859803));
#268966=CARTESIAN_POINT('Ctrl Pts',(-0.39799116808154,1.50373728279574,
13.6083055786646));
#268967=CARTESIAN_POINT('Ctrl Pts',(-0.404292470219306,1.50205538570144,
13.6087680288113));
#268968=CARTESIAN_POINT('Ctrl Pts',(-0.415574630332352,1.49896789819568,
13.6095997475955));
#268969=CARTESIAN_POINT('Ctrl Pts',(-0.420559433272976,1.49757697468096,
13.6099685364776));
#268970=CARTESIAN_POINT('Ctrl Pts',(-0.432192535520679,1.4942682957153,
13.6108323005173));
#268971=CARTESIAN_POINT('Ctrl Pts',(-0.438835117795961,1.49233101685513,
13.6113279032667));
#268972=CARTESIAN_POINT('Ctrl Pts',(-0.457380899882402,1.48678769520407,
13.6127184234272));
#268973=CARTESIAN_POINT('Ctrl Pts',(-0.469253864524501,1.48308318449054,
13.6136165280138));
#268974=CARTESIAN_POINT('Ctrl Pts',(-0.534842717663971,1.46175222579179,
13.6186229929478));
#268975=CARTESIAN_POINT('Ctrl Pts',(-0.587604483824374,1.44135207249496,
13.6228215111518));
#268976=CARTESIAN_POINT('Ctrl Pts',(-0.751116181933909,1.36765930924143,
13.6363935101631));
#268977=CARTESIAN_POINT('Ctrl Pts',(-0.856723480656026,1.30410393245719,
13.6460516803294));
#268978=CARTESIAN_POINT('Ctrl Pts',(-0.96664430687877,1.21878870492784,
13.65669105786));
#268979=CARTESIAN_POINT('Ctrl Pts',(-0.979391380448577,1.20856927108453,
13.6579340177806));
#268980=CARTESIAN_POINT('Ctrl Pts',(-1.01418380355451,1.17976385065839,
13.6613475059728));
#268981=CARTESIAN_POINT('Ctrl Pts',(-1.03587852485889,1.16076160029383,
13.6634998755578));
#268982=CARTESIAN_POINT('Ctrl Pts',(-1.06194243707086,1.13661922900806,
13.6661032157693));
#268983=CARTESIAN_POINT('Ctrl Pts',(-1.06682146717324,1.132041065035,13.6665913274712));
#268984=CARTESIAN_POINT('Ctrl Pts',(-1.0744097607285,1.1248280734704,13.6673514978763));
#268985=CARTESIAN_POINT('Ctrl Pts',(-1.07713914210445,1.1222146845356,13.6676251267921));
#268986=CARTESIAN_POINT('Ctrl Pts',(-1.08217652191016,1.11735607247166,
13.668130481512));
#268987=CARTESIAN_POINT('Ctrl Pts',(-1.08448705553333,1.11511364622996,
13.6683624056499));
#268988=CARTESIAN_POINT('Ctrl Pts',(-1.08902927520813,1.11067784630976,
13.6688186115888));
#268989=CARTESIAN_POINT('Ctrl Pts',(-1.09126129507027,1.10848492406989,
13.6690429224655));
#268990=CARTESIAN_POINT('Ctrl Pts',(-1.09801008749208,1.10181420801552,
13.6697216205818));
#268991=CARTESIAN_POINT('Ctrl Pts',(-1.10250610512266,1.09731535717561,
13.6701744032067));
#268992=CARTESIAN_POINT('Ctrl Pts',(-1.12848152482335,1.07100274917494,
13.6727949887573));
#268993=CARTESIAN_POINT('Ctrl Pts',(-1.14934262608573,1.04858442651917,
13.6749183423942));
#268994=CARTESIAN_POINT('Ctrl Pts',(-1.21594893668811,0.972628012759765,
13.6818208369414));
#268995=CARTESIAN_POINT('Ctrl Pts',(-1.25872456846244,0.916597678142573,
13.6864598008834));
#268996=CARTESIAN_POINT('Ctrl Pts',(-1.36049882817829,0.762658125252066,
13.6986087720395));
#268997=CARTESIAN_POINT('Ctrl Pts',(-1.41276211104518,0.660835304177493,
13.7060999184273));
#268998=CARTESIAN_POINT('Ctrl Pts',(-1.46002081698805,0.536901277587853,
13.7152981382997));
#268999=CARTESIAN_POINT('Ctrl Pts',(-1.46631419443058,0.519467419739277,
13.7165929077524));
#269000=CARTESIAN_POINT('Ctrl Pts',(-1.47467681327628,0.494937431694128,
13.7184178410167));
#269001=CARTESIAN_POINT('Ctrl Pts',(-1.47700945658193,0.487932194779434,
13.7189393546206));
#269002=CARTESIAN_POINT('Ctrl Pts',(-1.48096668264113,0.475759679229069,
13.7198462906411));
#269003=CARTESIAN_POINT('Ctrl Pts',(-1.48261432658778,0.470599983763692,
13.7202309517733));
#269004=CARTESIAN_POINT('Ctrl Pts',(-1.48598805829119,0.459841350453832,
13.7210335500361));
#269005=CARTESIAN_POINT('Ctrl Pts',(-1.48770952472348,0.454241065174517,
13.7214516309685));
#269006=CARTESIAN_POINT('Ctrl Pts',(-1.49170054395539,0.440991383826819,
13.7224415394216));
#269007=CARTESIAN_POINT('Ctrl Pts',(-1.49394294040363,0.433334051129318,
13.723014239705));
#269008=CARTESIAN_POINT('Ctrl Pts',(-1.4985407327796,0.417173549614107,
13.7242243169945));
#269009=CARTESIAN_POINT('Ctrl Pts',(-1.50088288159451,0.408666940270814,
13.7248621014086));
#269010=CARTESIAN_POINT('Ctrl Pts',(-1.51057966231786,0.372240432773733,
13.7275969994662));
#269011=CARTESIAN_POINT('Ctrl Pts',(-1.51722809949493,0.34414029899846,
13.7297164446371));
#269012=CARTESIAN_POINT('Ctrl Pts',(-1.54473528368205,0.21150498246949,
13.7397716978657));
#269013=CARTESIAN_POINT('Ctrl Pts',(-1.55559124031108,0.105207658855261,
13.7480058999189));
#269014=CARTESIAN_POINT('Ctrl Pts',(-1.55549942243246,-0.00134045226759553,
13.7562673955592));
#269015=CARTESIAN_POINT('Ctrl Pts',(-1.555499421659,-0.00134134951378047,
13.7562674651297));
#269016=CARTESIAN_POINT('Ctrl Pts',(-1.55542394797204,-0.0888646051650332,
13.7630538171062));
#269017=CARTESIAN_POINT('Ctrl Pts',(-1.54796158042164,-0.176239683107133,
13.769824279052));
#269018=CARTESIAN_POINT('Ctrl Pts',(-1.53222541744419,-0.268137709402849,
13.7766750956072));
#269019=CARTESIAN_POINT('Ctrl Pts',(-1.53123530937207,-0.273735257118771,
13.7770912617309));
#269020=CARTESIAN_POINT('Ctrl Pts',(-1.52953758398736,-0.283035756747498,
13.7777807331157));
#269021=CARTESIAN_POINT('Ctrl Pts',(-1.52884716097948,-0.286741729761807,
13.7780549372045));
#269022=CARTESIAN_POINT('Ctrl Pts',(-1.52757271702178,-0.293447066589199,
13.7785500596778));
#269023=CARTESIAN_POINT('Ctrl Pts',(-1.5269933206881,-0.296447273035847,
13.7787712305849));
#269024=CARTESIAN_POINT('Ctrl Pts',(-1.52578578452506,-0.302602608692982,
13.7792242176254));
#269025=CARTESIAN_POINT('Ctrl Pts',(-1.52515670426852,-0.305757464130997,
13.7794559675518));
#269026=CARTESIAN_POINT('Ctrl Pts',(-1.52371394955127,-0.312877667828354,
13.7799780624258));
#269027=CARTESIAN_POINT('Ctrl Pts',(-1.52289458257793,-0.316841800336313,
13.7802680806119));
#269028=CARTESIAN_POINT('Ctrl Pts',(-1.52037515790309,-0.328795297816436,
13.7811407524533));
#269029=CARTESIAN_POINT('Ctrl Pts',(-1.51862760042459,-0.336774683673459,
13.7817207901984));
#269030=CARTESIAN_POINT('Ctrl Pts',(-1.50002669118191,-0.418616553269739,
13.7876478157671));
#269031=CARTESIAN_POINT('Ctrl Pts',(-1.47785858246025,-0.491179692018681,
13.7927186950357));
#269032=CARTESIAN_POINT('Ctrl Pts',(-1.42971047402387,-0.615480554534184,
13.8015367829861));
#269033=CARTESIAN_POINT('Ctrl Pts',(-1.40597689187837,-0.667920211683963,
13.805301279978));
#269034=CARTESIAN_POINT('Ctrl Pts',(-1.34490607878004,-0.785096086708805,
13.8140380613771));
#269035=CARTESIAN_POINT('Ctrl Pts',(-1.30570601163146,-0.848691935995779,
13.8190280247341));
#269036=CARTESIAN_POINT('Ctrl Pts',(-1.24924637175966,-0.927063712846012,
13.8257022261241));
#269037=CARTESIAN_POINT('Ctrl Pts',(-1.23601901106091,-0.944627199154691,
13.8272344172082));
#269038=CARTESIAN_POINT('Ctrl Pts',(-1.21834382729615,-0.967089505732215,
13.829245279046));
#269039=CARTESIAN_POINT('Ctrl Pts',(-1.21423032916878,-0.972249195904546,
13.8297107932177));
#269040=CARTESIAN_POINT('Ctrl Pts',(-1.20606691872174,-0.982356205174639,
13.8306299122717));
#269041=CARTESIAN_POINT('Ctrl Pts',(-1.2020190850422,-0.987305040632434,
13.8310834284625));
#269042=CARTESIAN_POINT('Ctrl Pts',(-1.19425861286853,-0.996674440019329,
13.8319487803847));
#269043=CARTESIAN_POINT('Ctrl Pts',(-1.19055164083243,-1.00109957679535,
13.8323603816892));
#269044=CARTESIAN_POINT('Ctrl Pts',(-1.18203579936579,-1.01115102679588,
13.8333020236178));
#269045=CARTESIAN_POINT('Ctrl Pts',(-1.1772112645467,-1.01676381972,13.8338327009346));
#269046=CARTESIAN_POINT('Ctrl Pts',(-1.16453357234536,-1.03130167038854,
13.8352201050721));
#269047=CARTESIAN_POINT('Ctrl Pts',(-1.15661796188794,-1.04017135709515,
13.8360794089955));
#269048=CARTESIAN_POINT('Ctrl Pts',(-1.09426903235366,-1.10844356984625,
13.8427959279096));
#269049=CARTESIAN_POINT('Ctrl Pts',(-1.03540586685138,-1.1636161245161,
13.848843685773));
#269050=CARTESIAN_POINT('Ctrl Pts',(-0.897708902440449,-1.27392848768245,
13.8623716080388));
#269051=CARTESIAN_POINT('Ctrl Pts',(-0.817493066480184,-1.32683052556791,
13.8698808194894));
#269052=CARTESIAN_POINT('Ctrl Pts',(-0.705432959993615,-1.38669234473495,
13.8796062008373));
#269053=CARTESIAN_POINT('Ctrl Pts',(-0.677509894960468,-1.4005470125059,
13.8819700809562));
#269054=CARTESIAN_POINT('Ctrl Pts',(-0.632673719022722,-1.42113843186653,
13.8856537936808));
#269055=CARTESIAN_POINT('Ctrl Pts',(-0.61602722266824,-1.42843306309832,
13.8869977175083));
#269056=CARTESIAN_POINT('Ctrl Pts',(-0.594271376189781,-1.43751554964689,
13.8887201536663));
#269057=CARTESIAN_POINT('Ctrl Pts',(-0.589276085943536,-1.43957046402505,
13.8891133392763));
#269058=CARTESIAN_POINT('Ctrl Pts',(-0.581460023397564,-1.44273825927916,
13.8897248604344));
#269059=CARTESIAN_POINT('Ctrl Pts',(-0.578646595453798,-1.44386895582517,
13.889944236981));
#269060=CARTESIAN_POINT('Ctrl Pts',(-0.572829285119295,-1.44618715705759,
13.8903962810099));
#269061=CARTESIAN_POINT('Ctrl Pts',(-0.569825053464294,-1.44737351497923,
13.8906288685618));
#269062=CARTESIAN_POINT('Ctrl Pts',(-0.562966613211537,-1.45005721901695,
13.8911579136427));
#269063=CARTESIAN_POINT('Ctrl Pts',(-0.559110114859249,-1.45154856155106,
13.8914540109092));
#269064=CARTESIAN_POINT('Ctrl Pts',(-0.54887583830307,-1.45545940953836,
13.8922362408763));
#269065=CARTESIAN_POINT('Ctrl Pts',(-0.54248791948583,-1.45785240693218,
13.8927208488526));
#269066=CARTESIAN_POINT('Ctrl Pts',(-0.49632850963146,-1.47479890636588,
13.8961979446267));
#269067=CARTESIAN_POINT('Ctrl Pts',(-0.455988706641099,-1.48776641226626,
13.8991050194487));
#269068=CARTESIAN_POINT('Ctrl Pts',(-0.31782043230741,-1.52603188908608,
13.9087822336986));
#269069=CARTESIAN_POINT('Ctrl Pts',(-0.218075711322604,-1.54344701824852,
13.9153173802451));
#269070=CARTESIAN_POINT('Ctrl Pts',(-0.0642819751277782,-1.55508183062603,
13.9255477747706));
#269071=CARTESIAN_POINT('Ctrl Pts',(-0.0110557105183446,-1.55637035341085,
13.9291132382103));
#269072=CARTESIAN_POINT('Ctrl Pts',(0.0632624219517054,-1.55435680552894,
13.9342018805486));
#269073=CARTESIAN_POINT('Ctrl Pts',(0.0843814181962754,-1.55335344310347,
13.9356601720196));
#269074=CARTESIAN_POINT('Ctrl Pts',(0.121065411833475,-1.5508603014553,
13.9382188935981));
#269075=CARTESIAN_POINT('Ctrl Pts',(0.136640844848652,-1.54956566726711,
13.9393133453624));
#269076=CARTESIAN_POINT('Ctrl Pts',(0.159817376257911,-1.54728709012976,
13.9409551451811));
#269077=CARTESIAN_POINT('Ctrl Pts',(0.167435339975332,-1.54648127572977,
13.9414969280022));
#269078=CARTESIAN_POINT('Ctrl Pts',(0.180817647551001,-1.5449656814214,
13.9424525645731));
#269079=CARTESIAN_POINT('Ctrl Pts',(0.186584597428597,-1.54427982074695,
13.9428656605312));
#269080=CARTESIAN_POINT('Ctrl Pts',(0.197808293237889,-1.54288120490314,
13.9436721794718));
#269081=CARTESIAN_POINT('Ctrl Pts',(0.20326537082163,-1.54217175467155,
13.944065492624));
#269082=CARTESIAN_POINT('Ctrl Pts',(0.217902694031781,-1.54018978109164,
13.9451236843625));
#269083=CARTESIAN_POINT('Ctrl Pts',(0.227075396453182,-1.53886416010994,
13.9457902248465));
#269084=CARTESIAN_POINT('Ctrl Pts',(0.260995846663186,-1.53365216587991,
13.9482680823758));
#269085=CARTESIAN_POINT('Ctrl Pts',(0.285659229486592,-1.52925029577789,
13.9500954971752));
#269086=CARTESIAN_POINT('Ctrl Pts',(0.479353219575773,-1.48983123210039,
13.964660750462));
#269087=CARTESIAN_POINT('Ctrl Pts',(0.641580781174021,-1.42748861649259,
13.9783450837591));
#269088=CARTESIAN_POINT('Ctrl Pts',(0.819120240931761,-1.32278107627788,
13.9939805151973));
#269089=CARTESIAN_POINT('Ctrl Pts',(0.847485929812238,-1.30478955056603,
13.9964945686221));
#269090=CARTESIAN_POINT('Ctrl Pts',(0.880828612054437,-1.28209467455352,
13.999449958471));
#269091=CARTESIAN_POINT('Ctrl Pts',(0.886383160992166,-1.2782608085616,
13.9999422980049));
#269092=CARTESIAN_POINT('Ctrl Pts',(0.894985918576415,-1.27223996411929,
14.0007046094499));
#269093=CARTESIAN_POINT('Ctrl Pts',(0.898051375772499,-1.27007796927322,
14.0009762046691));
#269094=CARTESIAN_POINT('Ctrl Pts',(0.903735999749112,-1.26603786652385,
14.0014797305121));
#269095=CARTESIAN_POINT('Ctrl Pts',(0.906357127918199,-1.26416272438452,
14.0017118470248));
#269096=CARTESIAN_POINT('Ctrl Pts',(0.91232370999698,-1.25986616453107,
14.0022401202137));
#269097=CARTESIAN_POINT('Ctrl Pts',(0.9156653598114,-1.2574395628645,14.0025359162271));
#269098=CARTESIAN_POINT('Ctrl Pts',(0.924367352814728,-1.25106736298631,
14.0033061334268));
#269099=CARTESIAN_POINT('Ctrl Pts',(0.929712180830482,-1.2471005631822,
14.0037791412212));
#269100=CARTESIAN_POINT('Ctrl Pts',(0.965954529295828,-1.21983988279399,
14.0069873430414));
#269101=CARTESIAN_POINT('Ctrl Pts',(0.996002166994366,-1.19543205529874,
14.0096513480871));
#269102=CARTESIAN_POINT('Ctrl Pts',(1.13812891129731,-1.07089798544751,
14.0224491256689));
#269103=CARTESIAN_POINT('Ctrl Pts',(1.23620420906182,-0.956015343843199,
14.0319857622665));
#269104=CARTESIAN_POINT('Ctrl Pts',(1.33684677620992,-0.796184803320936,
14.0448378869267));
#269105=CARTESIAN_POINT('Ctrl Pts',(1.35618599479533,-0.7627769461492,14.0474991020282));
#269106=CARTESIAN_POINT('Ctrl Pts',(1.37916437902502,-0.719441022950661,
14.0509390434279));
#269107=CARTESIAN_POINT('Ctrl Pts',(1.38397333559117,-0.710146158717262,
14.0516761341921));
#269108=CARTESIAN_POINT('Ctrl Pts',(1.39156045790689,-0.695111782705513,
14.0528675768741));
#269109=CARTESIAN_POINT('Ctrl Pts',(1.39439782002678,-0.689402361304805,
14.053319853124));
#269110=CARTESIAN_POINT('Ctrl Pts',(1.39973897550416,-0.67848686165099,
14.0541842689806));
#269111=CARTESIAN_POINT('Ctrl Pts',(1.40224902971585,-0.673283950488848,
14.0545961824337));
#269112=CARTESIAN_POINT('Ctrl Pts',(1.40792318031783,-0.661353041222404,
14.0555405594739));
#269113=CARTESIAN_POINT('Ctrl Pts',(1.41106811619982,-0.654616143019086,
14.0560736732287));
#269114=CARTESIAN_POINT('Ctrl Pts',(1.41916247491842,-0.636947499641706,
14.0574716406558));
#269115=CARTESIAN_POINT('Ctrl Pts',(1.42403382068632,-0.625980758538256,
14.0583391361447));
#269116=CARTESIAN_POINT('Ctrl Pts',(1.46362193219472,-0.534002908640036,
14.0656146311728));
#269117=CARTESIAN_POINT('Ctrl Pts',(1.49151614713888,-0.450247279612979,
14.0722526854534));
#269118=CARTESIAN_POINT('Ctrl Pts',(1.51437955710908,-0.355420693444977,
14.0797556027548));
#269119=CARTESIAN_POINT('Ctrl Pts',(1.51650801132852,-0.346226458405174,
14.0804827849193));
#269120=CARTESIAN_POINT('Ctrl Pts',(1.53799900059489,-0.249389988913261,
14.0881371409923));
#269121=CARTESIAN_POINT('Ctrl Pts',(1.54982507646817,-0.160247161293668,
14.0951572699393));
#269122=CARTESIAN_POINT('Ctrl Pts',(1.55552459876715,-0.034766945670613,
14.104703441249));
#269123=CARTESIAN_POINT('Ctrl Pts',(1.55591285957617,0.00109598353668149,
14.1073920035592));
#269124=CARTESIAN_POINT('Ctrl Pts',(1.55489805662046,0.0438119126565924,
14.1105237168089));
#269125=CARTESIAN_POINT('Ctrl Pts',(1.5546893807644,0.0506792285990876,
14.1110250102522));
#269126=CARTESIAN_POINT('Ctrl Pts',(1.55429546432879,0.0613198828896375,
14.1117981353413));
#269127=CARTESIAN_POINT('Ctrl Pts',(1.55414197076843,0.0650941932193456,
14.1120716634984));
#269128=CARTESIAN_POINT('Ctrl Pts',(1.5538321676789,0.0720847613072222,
14.1125769265078));
#269129=CARTESIAN_POINT('Ctrl Pts',(1.55367962191105,0.0753010687049443,
14.11280885908));
#269130=CARTESIAN_POINT('Ctrl Pts',(1.55331046554904,0.082605103211132,
14.1133343671755));
#269131=CARTESIAN_POINT('Ctrl Pts',(1.55308770642234,0.0866924602037214,
14.1136275970647));
#269132=CARTESIAN_POINT('Ctrl Pts',(1.55246741763863,0.0973030110623689,
14.1143867208042));
#269133=CARTESIAN_POINT('Ctrl Pts',(1.55204490385286,0.10382475230554,14.1148512669579));
#269134=CARTESIAN_POINT('Ctrl Pts',(1.54901116597825,0.146483165649293,
14.1178775920443));
#269135=CARTESIAN_POINT('Ctrl Pts',(1.54517892804341,0.182525373289272,
14.1203770470608));
#269136=CARTESIAN_POINT('Ctrl Pts',(1.53875895622177,0.227796197206829,
14.1234810896471));
#269137=CARTESIAN_POINT('Ctrl Pts',(1.53734114932868,0.237175947248667,
14.124122286209));
#269138=CARTESIAN_POINT('Ctrl Pts',(1.51983133250108,0.346253514021789,
14.1315622405307));
#269139=CARTESIAN_POINT('Ctrl Pts',(1.4941523090723,0.444173292909463,14.1380947421775));
#269140=CARTESIAN_POINT('Ctrl Pts',(1.45141285026689,0.559893776997534,
14.1462866907977));
#269141=CARTESIAN_POINT('Ctrl Pts',(1.44321615033215,0.58069516914172,14.1477780500171));
#269142=CARTESIAN_POINT('Ctrl Pts',(1.43457666475166,0.601306945702447,
14.1492791259731));
#269143=CARTESIAN_POINT('Origin',(0.,0.,-1.29405622560371));
#269144=CARTESIAN_POINT('',(1.4345766844093,0.601306898803946,14.987048570644));
#269145=CARTESIAN_POINT('',(1.43457662445949,0.601307041830064,14.8491341039362));
#269146=CARTESIAN_POINT('',(1.43457668357355,0.601306900797845,-1.29405622560371));
#269147=CARTESIAN_POINT('',(-1.55549959649185,0.00112040782065311,14.5950894464761));
#269148=CARTESIAN_POINT('Ctrl Pts',(1.4345766844093,0.601306898803942,14.987048570644));
#269149=CARTESIAN_POINT('Ctrl Pts',(1.49486490206182,0.457473406188229,
14.976439209092));
#269150=CARTESIAN_POINT('Ctrl Pts',(1.53318843830475,0.305373873929638,
14.9665756914561));
#269151=CARTESIAN_POINT('Ctrl Pts',(1.55186059850538,0.112762420484539,
14.9534032965279));
#269152=CARTESIAN_POINT('Ctrl Pts',(1.55412782937726,0.0753192035225039,
14.9508170288459));
#269153=CARTESIAN_POINT('Ctrl Pts',(1.55530042438738,0.0271224202641314,
14.9474374879375));
#269154=CARTESIAN_POINT('Ctrl Pts',(1.55545033675133,0.0164096155206039,
14.9466831401705));
#269155=CARTESIAN_POINT('Ctrl Pts',(1.55551293087773,-0.000682820512163463,
14.9454741278517));
#269156=CARTESIAN_POINT('Ctrl Pts',(1.55549704933952,-0.00706198732699898,
14.9450216973144));
#269157=CARTESIAN_POINT('Ctrl Pts',(1.55539770759106,-0.0185583587751548,
14.9442040810712));
#269158=CARTESIAN_POINT('Ctrl Pts',(1.55532823072722,-0.0236756206461456,
14.9438393377651));
#269159=CARTESIAN_POINT('Ctrl Pts',(1.55510551932437,-0.0357054738714125,
14.9429799409452));
#269160=CARTESIAN_POINT('Ctrl Pts',(1.55493144578642,-0.0426175215637954,
14.9424846433416));
#269161=CARTESIAN_POINT('Ctrl Pts',(1.55429084062506,-0.0627264404817726,
14.9410391678639));
#269162=CARTESIAN_POINT('Ctrl Pts',(1.55370234646703,-0.0759185232106978,
14.9400852083322));
#269163=CARTESIAN_POINT('Ctrl Pts',(1.55199334469202,-0.105704756185604,
14.9379178593878));
#269164=CARTESIAN_POINT('Ctrl Pts',(1.55077451958072,-0.122291403380222,
14.9367015250704));
#269165=CARTESIAN_POINT('Ctrl Pts',(1.54593622038812,-0.17627536209115,
14.9327109837878));
#269166=CARTESIAN_POINT('Ctrl Pts',(1.54122803732576,-0.213559167661376,
14.9299047078128));
#269167=CARTESIAN_POINT('Ctrl Pts',(1.50962398916305,-0.407139761776606,
14.9150739528187));
#269168=CARTESIAN_POINT('Ctrl Pts',(1.46029687605994,-0.55879555238969,
14.9024383936853));
#269169=CARTESIAN_POINT('Ctrl Pts',(1.3825376542555,-0.713000734108949,
14.8896108510062));
#269170=CARTESIAN_POINT('Ctrl Pts',(1.37599517880621,-0.725546496153935,
14.8885683386006));
#269171=CARTESIAN_POINT('Ctrl Pts',(1.36682924517354,-0.74255288928872,
14.8871583950433));
#269172=CARTESIAN_POINT('Ctrl Pts',(1.36435363637782,-0.747091785398318,
14.8867824091287));
#269173=CARTESIAN_POINT('Ctrl Pts',(1.36038715102502,-0.754278650312392,
14.8861876821429));
#269174=CARTESIAN_POINT('Ctrl Pts',(1.35891109661614,-0.756934683390036,
14.8859680227311));
#269175=CARTESIAN_POINT('Ctrl Pts',(1.35584117107055,-0.762420827647948,
14.8855146083494));
#269176=CARTESIAN_POINT('Ctrl Pts',(1.3542462126083,-0.765250282898886,
14.8852809324592));
#269177=CARTESIAN_POINT('Ctrl Pts',(1.35039637250112,-0.772030165909536,
14.8847213672156));
#269178=CARTESIAN_POINT('Ctrl Pts',(1.34813297822836,-0.775975782069383,
14.8843960196119));
#269179=CARTESIAN_POINT('Ctrl Pts',(1.34028754759362,-0.789514229579249,
14.8832804854181));
#269180=CARTESIAN_POINT('Ctrl Pts',(1.33461999815095,-0.799057512441261,
14.8824955637599));
#269181=CARTESIAN_POINT('Ctrl Pts',(1.30067556034983,-0.854845851685494,
14.8779103999651));
#269182=CARTESIAN_POINT('Ctrl Pts',(1.270095811652,-0.899653488003313,14.874240872608));
#269183=CARTESIAN_POINT('Ctrl Pts',(1.18031980704884,-1.0174692048576,14.8643632437778));
#269184=CARTESIAN_POINT('Ctrl Pts',(1.11675754865631,-1.08685408867507,
14.8582744560472));
#269185=CARTESIAN_POINT('Ctrl Pts',(0.995846956086833,-1.19696136337736,
14.8473810357873));
#269186=CARTESIAN_POINT('Ctrl Pts',(0.941287329985927,-1.24032406775073,
14.8426667396948));
#269187=CARTESIAN_POINT('Ctrl Pts',(0.874552777073934,-1.28641745353404,
14.8369986175241));
#269188=CARTESIAN_POINT('Ctrl Pts',(0.865021222204317,-1.29284596813049,
14.8361913775601));
#269189=CARTESIAN_POINT('Ctrl Pts',(0.84937607011585,-1.30314730509912,
14.8348696227709));
#269190=CARTESIAN_POINT('Ctrl Pts',(0.843305037361686,-1.30708424289972,
14.8343575078911));
#269191=CARTESIAN_POINT('Ctrl Pts',(0.832410176387109,-1.31404183327217,
14.833439761891));
#269192=CARTESIAN_POINT('Ctrl Pts',(0.827596787547885,-1.31707866014364,
14.8330347389075));
#269193=CARTESIAN_POINT('Ctrl Pts',(0.817376138388073,-1.32344884581364,
14.8321755877951));
#269194=CARTESIAN_POINT('Ctrl Pts',(0.811964922446482,-1.32677562594298,
14.8317212273248));
#269195=CARTESIAN_POINT('Ctrl Pts',(0.797477704479851,-1.33556045313757,
14.8305060392756));
#269196=CARTESIAN_POINT('Ctrl Pts',(0.788366222054037,-1.34095902351144,
14.8297430660026));
#269197=CARTESIAN_POINT('Ctrl Pts',(0.743669932872061,-1.36682866862723,
14.8260059052544));
#269198=CARTESIAN_POINT('Ctrl Pts',(0.707342550418044,-1.3859767350806,
14.8229850016968));
#269199=CARTESIAN_POINT('Ctrl Pts',(0.536369388325766,-1.4676229683982,
14.8088271239949));
#269200=CARTESIAN_POINT('Ctrl Pts',(0.393975421402373,-1.51207780353708,
14.7971040263131));
#269201=CARTESIAN_POINT('Ctrl Pts',(0.209887098955397,-1.54174519951429,
14.7829022388443));
#269202=CARTESIAN_POINT('Ctrl Pts',(0.172071569920612,-1.54642258921192,
14.7800398705558));
#269203=CARTESIAN_POINT('Ctrl Pts',(0.127570565130129,-1.5502739118521,
14.7767628341066));
#269204=CARTESIAN_POINT('Ctrl Pts',(0.121018624993018,-1.5507991318482,
14.7762826707616));
#269205=CARTESIAN_POINT('Ctrl Pts',(0.110396207315975,-1.55158292060797,
14.7755081630059));
#269206=CARTESIAN_POINT('Ctrl Pts',(0.106327787713946,-1.55186703190108,
14.7752124651791));
#269207=CARTESIAN_POINT('Ctrl Pts',(0.0990830193210822,-1.5523443339152,
14.7746876363614));
#269208=CARTESIAN_POINT('Ctrl Pts',(0.0959071563343846,-1.55254378160758,
14.7744581635346));
#269209=CARTESIAN_POINT('Ctrl Pts',(0.0890368977889373,-1.55295407948584,
14.7739630449436));
#269210=CARTESIAN_POINT('Ctrl Pts',(0.0853423595391087,-1.55316149340679,
14.773697592557));
#269211=CARTESIAN_POINT('Ctrl Pts',(0.0750097057204092,-1.55370459556713,
14.7729573441526));
#269212=CARTESIAN_POINT('Ctrl Pts',(0.0683700202281368,-1.55401093008039,
14.7724841488582));
#269213=CARTESIAN_POINT('Ctrl Pts',(0.0289741863571047,-1.55557554567858,
14.7696901239696));
#269214=CARTESIAN_POINT('Ctrl Pts',(-0.00381608135986826,-1.55584080807551,
14.7674203988275));
#269215=CARTESIAN_POINT('Ctrl Pts',(-0.194838050308205,-1.55134576804175,
14.7543948445618));
#269216=CARTESIAN_POINT('Ctrl Pts',(-0.351594185123817,-1.52349160191971,
14.7443993367283));
#269217=CARTESIAN_POINT('Ctrl Pts',(-0.536872277991188,-1.46039304176426,
14.7310752183441));
#269218=CARTESIAN_POINT('Ctrl Pts',(-0.571834710660903,-1.44706059220272,
14.7284952494209));
#269219=CARTESIAN_POINT('Ctrl Pts',(-0.616138326706858,-1.42830962991474,
14.7251228610801));
#269220=CARTESIAN_POINT('Ctrl Pts',(-0.625952705227407,-1.42403582721424,
14.7243691599743));
#269221=CARTESIAN_POINT('Ctrl Pts',(-0.641542237557301,-1.41705485979598,
14.7231609419995));
#269222=CARTESIAN_POINT('Ctrl Pts',(-0.647346334614583,-1.41441282485061,
14.722708653952));
#269223=CARTESIAN_POINT('Ctrl Pts',(-0.658184564721687,-1.40939855877366,
14.7218593758202));
#269224=CARTESIAN_POINT('Ctrl Pts',(-0.663222548960715,-1.40703484952657,
14.7214626844791));
#269225=CARTESIAN_POINT('Ctrl Pts',(-0.67455919067198,-1.40164153738495,
14.7205656396141));
#269226=CARTESIAN_POINT('Ctrl Pts',(-0.680850293412602,-1.39859643072956,
14.7200647553006));
#269227=CARTESIAN_POINT('Ctrl Pts',(-0.699458354821174,-1.3894341960119,
14.7185739050948));
#269228=CARTESIAN_POINT('Ctrl Pts',(-0.711714656474277,-1.38319615396487,
14.7175797482935));
#269229=CARTESIAN_POINT('Ctrl Pts',(-0.739531135586624,-1.36857092359856,
14.7152947410611));
#269230=CARTESIAN_POINT('Ctrl Pts',(-0.755034030115011,-1.36007949747804,
14.7140003393474));
#269231=CARTESIAN_POINT('Ctrl Pts',(-0.806025673564585,-1.3310092631534,
14.709671635109));
#269232=CARTESIAN_POINT('Ctrl Pts',(-0.840842318597159,-1.30929244409194,
14.7065988758501));
#269233=CARTESIAN_POINT('Ctrl Pts',(-0.963608840547663,-1.22579944926369,
14.695335402881));
#269234=CARTESIAN_POINT('Ctrl Pts',(-1.04595565381527,-1.15633015067891,
14.6869212469262));
#269235=CARTESIAN_POINT('Ctrl Pts',(-1.15829691523965,-1.03966416688124,
14.6744628789054));
#269236=CARTESIAN_POINT('Ctrl Pts',(-1.19403128661577,-0.998420798811307,
14.6703210304767));
#269237=CARTESIAN_POINT('Ctrl Pts',(-1.23233290277162,-0.949208637463735,
14.6657398916192));
#269238=CARTESIAN_POINT('Ctrl Pts',(-1.23709014440016,-0.943000213237792,
14.6651681972039));
#269239=CARTESIAN_POINT('Ctrl Pts',(-1.24420940695368,-0.933562639616464,
14.6643088613918));
#269240=CARTESIAN_POINT('Ctrl Pts',(-1.2466060371625,-0.930359951590167,
14.6640189122466));
#269241=CARTESIAN_POINT('Ctrl Pts',(-1.25088360745399,-0.924597501727867,
14.6635002613761));
#269242=CARTESIAN_POINT('Ctrl Pts',(-1.25276907636123,-0.922041203816691,
14.6632712504563));
#269243=CARTESIAN_POINT('Ctrl Pts',(-1.25686849950748,-0.916447462607108,
14.6627724571021));
#269244=CARTESIAN_POINT('Ctrl Pts',(-1.25907927652511,-0.913407769294506,
14.6625028936473));
#269245=CARTESIAN_POINT('Ctrl Pts',(-1.26532682650846,-0.904751959004491,
14.6617394002847));
#269246=CARTESIAN_POINT('Ctrl Pts',(-1.26933725965174,-0.899116795093998,
14.6612472371353));
#269247=CARTESIAN_POINT('Ctrl Pts',(-1.29515400094594,-0.86232398593046,
14.6580641158906));
#269248=CARTESIAN_POINT('Ctrl Pts',(-1.31585122304527,-0.830399122665444,
14.6554422922447));
#269249=CARTESIAN_POINT('Ctrl Pts',(-1.40070831188263,-0.688355256619558,
14.6442227513191));
#269250=CARTESIAN_POINT('Ctrl Pts',(-1.45237240917423,-0.571345816022819,
14.6360675361225));
#269251=CARTESIAN_POINT('Ctrl Pts',(-1.49991869317795,-0.413768607775255,
14.625041205455));
#269252=CARTESIAN_POINT('Ctrl Pts',(-1.50937247641969,-0.377829277982698,
14.6225269189865));
#269253=CARTESIAN_POINT('Ctrl Pts',(-1.51809288682723,-0.33908819225072,
14.6197992313694));
#269254=CARTESIAN_POINT('Ctrl Pts',(-1.51864937869788,-0.33658710554306,
14.6196230597135));
#269255=CARTESIAN_POINT('Ctrl Pts',(-1.52468852810913,-0.309124983517292,
14.6176878101906));
#269256=CARTESIAN_POINT('Ctrl Pts',(-1.52956113490112,-0.284035152648691,
14.6159117445361));
#269257=CARTESIAN_POINT('Ctrl Pts',(-1.53535643518452,-0.249693546340576,
14.6134645256988));
#269258=CARTESIAN_POINT('Ctrl Pts',(-1.53681774573789,-0.24053577670269,
14.612810382294));
#269259=CARTESIAN_POINT('Ctrl Pts',(-1.53900877225638,-0.225969092511054,
14.611767177405));
#269260=CARTESIAN_POINT('Ctrl Pts',(-1.53979207450111,-0.220568351705099,
14.6113798114108));
#269261=CARTESIAN_POINT('Ctrl Pts',(-1.54130551109226,-0.209732320819259,
14.6106013692436));
#269262=CARTESIAN_POINT('Ctrl Pts',(-1.54203535326286,-0.204297069951322,
14.6102102898128));
#269263=CARTESIAN_POINT('Ctrl Pts',(-1.54344536599304,-0.193358226605947,
14.609421916275));
#269264=CARTESIAN_POINT('Ctrl Pts',(-1.54412487755364,-0.187854631687998,
14.6090246074517));
#269265=CARTESIAN_POINT('Ctrl Pts',(-1.54561366289956,-0.175242244892861,
14.6081125469229));
#269266=CARTESIAN_POINT('Ctrl Pts',(-1.54640334242745,-0.168131313815164,
14.607597187089));
#269267=CARTESIAN_POINT('Ctrl Pts',(-1.54915474553508,-0.14169397103447,
14.6056767814503));
#269268=CARTESIAN_POINT('Ctrl Pts',(-1.55080336398481,-0.122337524634641,
14.6042620218949));
#269269=CARTESIAN_POINT('Ctrl Pts',(-1.55438730032399,-0.0683087702370583,
14.6002871583492));
#269270=CARTESIAN_POINT('Ctrl Pts',(-1.5555246032339,-0.03359728732884,
14.5977035516453));
#269271=CARTESIAN_POINT('Ctrl Pts',(-1.55549959649185,0.00112040782065311,
14.5950894464761));
#269272=CARTESIAN_POINT('Ctrl Pts',(-1.55549959789313,0.00111846069355959,
14.595089593087));
#269273=CARTESIAN_POINT('Ctrl Pts',(-1.55548425053835,0.0224627996720666,
14.5934824494409));
#269274=CARTESIAN_POINT('Ctrl Pts',(-1.55502958043063,0.0438039458821249,
14.5918642772033));
#269275=CARTESIAN_POINT('Ctrl Pts',(-1.54822857536825,0.206093876730948,
14.5794785918082));
#269276=CARTESIAN_POINT('Ctrl Pts',(-1.52317170858574,0.345589628889972,
14.5682926697141));
#269277=CARTESIAN_POINT('Ctrl Pts',(-1.47623606221595,0.490336843701623,
14.5569574948509));
#269278=CARTESIAN_POINT('Ctrl Pts',(-1.47270410090153,0.500845066095354,
14.556136665006));
#269279=CARTESIAN_POINT('Ctrl Pts',(-1.46630393991913,0.519233379449804,
14.5547049940083));
#269280=CARTESIAN_POINT('Ctrl Pts',(-1.4634838404652,0.527129589049032,
14.5540917494566));
#269281=CARTESIAN_POINT('Ctrl Pts',(-1.45920337267358,0.53881560366164,
14.553186856077));
#269282=CARTESIAN_POINT('Ctrl Pts',(-1.45779185164148,0.542622940793565,
14.552892463875));
#269283=CARTESIAN_POINT('Ctrl Pts',(-1.4552481092326,0.549402681953135,
14.5523690512611));
#269284=CARTESIAN_POINT('Ctrl Pts',(-1.45412166770451,0.552377174174578,
14.5521396964069));
#269285=CARTESIAN_POINT('Ctrl Pts',(-1.4516604967155,0.558816461569717,
14.5516438024714));
#269286=CARTESIAN_POINT('Ctrl Pts',(-1.45032248508607,0.562279935157498,
14.5513774623542));
#269287=CARTESIAN_POINT('Ctrl Pts',(-1.44659886112226,0.571816895843875,
14.5506450453363));
#269288=CARTESIAN_POINT('Ctrl Pts',(-1.44418737740314,0.577880307963531,
14.5501804797453));
#269289=CARTESIAN_POINT('Ctrl Pts',(-1.43148204040952,0.609250182459884,
14.5477817516802));
#269290=CARTESIAN_POINT('Ctrl Pts',(-1.42056017349597,0.634299338453912,
14.5458824696654));
#269291=CARTESIAN_POINT('Ctrl Pts',(-1.40137663391961,0.675311851633021,
14.5427786767828));
#269292=CARTESIAN_POINT('Ctrl Pts',(-1.39348878267914,0.691441703119032,
14.5415595310115));
#269293=CARTESIAN_POINT('Ctrl Pts',(-1.37812298516231,0.721531656444259,
14.5392815105495));
#269294=CARTESIAN_POINT('Ctrl Pts',(-1.37070779423519,0.735520945336393,
14.5382208704523));
#269295=CARTESIAN_POINT('Ctrl Pts',(-1.3128730877119,0.840716934861597,
14.5302153703065));
#269296=CARTESIAN_POINT('Ctrl Pts',(-1.25361624668274,0.926762009243754,
14.523477239618));
#269297=CARTESIAN_POINT('Ctrl Pts',(-1.1601289333121,1.03696926908142,14.5137991470962));
#269298=CARTESIAN_POINT('Ctrl Pts',(-1.13287604875944,1.06667514548298,
14.5110706280556));
#269299=CARTESIAN_POINT('Ctrl Pts',(-1.09220755453749,1.10768577517916,
14.5070956276272));
#269300=CARTESIAN_POINT('Ctrl Pts',(-1.0797054981399,1.11987549097028,14.5058859072131));
#269301=CARTESIAN_POINT('Ctrl Pts',(-1.05711322117367,1.14117332294881,
14.5037189025745));
#269302=CARTESIAN_POINT('Ctrl Pts',(-1.04710369134614,1.15036461802958,
14.502765204596));
#269303=CARTESIAN_POINT('Ctrl Pts',(-1.03177921489796,1.16407065873604,
14.5013138782989));
#269304=CARTESIAN_POINT('Ctrl Pts',(-1.0265520285847,1.16868292388205,14.5008203401368));
#269305=CARTESIAN_POINT('Ctrl Pts',(-1.01709071019442,1.17691877098868,
14.4999296178954));
#269306=CARTESIAN_POINT('Ctrl Pts',(-1.01286774664155,1.18055505276195,
14.4995329684991));
#269307=CARTESIAN_POINT('Ctrl Pts',(-1.00375940665784,1.18831315708249,
14.4986793481202));
#269308=CARTESIAN_POINT('Ctrl Pts',(-0.998867997074274,1.19242770343379,
14.4982220891621));
#269309=CARTESIAN_POINT('Ctrl Pts',(-0.985666066209812,1.20339464642037,
14.4969909351986));
#269310=CARTESIAN_POINT('Ctrl Pts',(-0.977309631316976,1.21019095302896,
14.4962147943293));
#269311=CARTESIAN_POINT('Ctrl Pts',(-0.939088544590627,1.24062220169355,
14.4926783033393));
#269312=CARTESIAN_POINT('Ctrl Pts',(-0.908435058600292,1.26324028518734,
14.4898783585339));
#269313=CARTESIAN_POINT('Ctrl Pts',(-0.746840842708807,1.3735498360812,
14.4752854896071));
#269314=CARTESIAN_POINT('Ctrl Pts',(-0.603987886157338,1.44207934776766,
14.4628021748968));
#269315=CARTESIAN_POINT('Ctrl Pts',(-0.42198731154876,1.49752411697499,
14.4483801948711));
#269316=CARTESIAN_POINT('Ctrl Pts',(-0.390377653254265,1.50607352411901,
14.4459309631188));
#269317=CARTESIAN_POINT('Ctrl Pts',(-0.352053900359383,1.51515096369368,
14.4430457372718));
#269318=CARTESIAN_POINT('Ctrl Pts',(-0.345578969477129,1.51664088421181,
14.4425611348744));
#269319=CARTESIAN_POINT('Ctrl Pts',(-0.335483792140536,1.51889583684061,
14.4418102454153));
#269320=CARTESIAN_POINT('Ctrl Pts',(-0.331870130960391,1.51968949292715,
14.4415423849408));
#269321=CARTESIAN_POINT('Ctrl Pts',(-0.325143076801083,1.52114179354025,
14.4410455126465));
#269322=CARTESIAN_POINT('Ctrl Pts',(-0.322030522570498,1.52180377161487,
14.4408163209499));
#269323=CARTESIAN_POINT('Ctrl Pts',(-0.31492345624512,1.52329252130051,
14.4402945863532));
#269324=CARTESIAN_POINT('Ctrl Pts',(-0.310927711278263,1.52411313495032,
14.4400023961408));
#269325=CARTESIAN_POINT('Ctrl Pts',(-0.298616267675917,1.52659112759011,
14.4391054935858));
#269326=CARTESIAN_POINT('Ctrl Pts',(-0.290290022620433,1.52819627584766,
14.4385036513972));
#269327=CARTESIAN_POINT('Ctrl Pts',(-0.273236051650089,1.53133955650659,
14.4372798288425));
#269328=CARTESIAN_POINT('Ctrl Pts',(-0.264507469498146,1.53287135294408,
14.4366581863243));
#269329=CARTESIAN_POINT('Ctrl Pts',(-0.0999070888177371,1.56030953543648,
14.4250162901345));
#269330=CARTESIAN_POINT('Ctrl Pts',(0.0590233411496406,1.56239584489408,
14.4150581402861));
#269331=CARTESIAN_POINT('Ctrl Pts',(0.271872446521253,1.53261167114947,
14.4006284059027));
#269332=CARTESIAN_POINT('Ctrl Pts',(0.327701868486181,1.5216515452454,14.3967481133074));
#269333=CARTESIAN_POINT('Ctrl Pts',(0.39408833510564,1.50479574678,14.3919536637725));
#269334=CARTESIAN_POINT('Ctrl Pts',(0.40534235679344,1.50180338797677,14.3911346217553));
#269335=CARTESIAN_POINT('Ctrl Pts',(0.422903946645971,1.49692212120169,
14.3898461900224));
#269336=CARTESIAN_POINT('Ctrl Pts',(0.42923509350274,1.49511899764551,14.3893795795179));
#269337=CARTESIAN_POINT('Ctrl Pts',(0.440445613630258,1.49184914435426,
14.3885495061347));
#269338=CARTESIAN_POINT('Ctrl Pts',(0.445329617618472,1.49039851671121,
14.3881865721065));
#269339=CARTESIAN_POINT('Ctrl Pts',(0.456580491852915,1.48699658667121,
14.3873474548923));
#269340=CARTESIAN_POINT('Ctrl Pts',(0.462942094221371,1.48502835298161,
14.386870724586));
#269341=CARTESIAN_POINT('Ctrl Pts',(0.480419513925493,1.47949774966963,
14.3855546228983));
#269342=CARTESIAN_POINT('Ctrl Pts',(0.491507972831767,1.47585107631614,
14.384712505617));
#269343=CARTESIAN_POINT('Ctrl Pts',(0.550780845115496,1.4556158839497,14.3801716684024));
#269344=CARTESIAN_POINT('Ctrl Pts',(0.598163740691983,1.43679371633505,
14.3763999178132));
#269345=CARTESIAN_POINT('Ctrl Pts',(0.755750221888889,1.36504762113438,
14.3633542651999));
#269346=CARTESIAN_POINT('Ctrl Pts',(0.860606315382178,1.30148514922372,
14.3537661588909));
#269347=CARTESIAN_POINT('Ctrl Pts',(0.984670651486607,1.20467523565277,
14.341681222052));
#269348=CARTESIAN_POINT('Ctrl Pts',(1.01167461188462,1.18208864292561,14.3390025534003));
#269349=CARTESIAN_POINT('Ctrl Pts',(1.04773862492915,1.14978207713126,14.3353806394628));
#269350=CARTESIAN_POINT('Ctrl Pts',(1.05747390685733,1.14083478899139,14.3343982469418));
#269351=CARTESIAN_POINT('Ctrl Pts',(1.07409403817436,1.12516434364419,14.3327146580435));
#269352=CARTESIAN_POINT('Ctrl Pts',(1.08103262876914,1.1184995624049,14.3320097947228));
#269353=CARTESIAN_POINT('Ctrl Pts',(1.09097799732966,1.10876764691982,14.3309971478179));
#269354=CARTESIAN_POINT('Ctrl Pts',(1.09403443020287,1.10575193974056,14.330685614288));
#269355=CARTESIAN_POINT('Ctrl Pts',(1.09935182797519,1.10046176336163,14.3301431205011));
#269356=CARTESIAN_POINT('Ctrl Pts',(1.10161829732988,1.09819290750213,14.3299117292382));
#269357=CARTESIAN_POINT('Ctrl Pts',(1.10639456503801,1.09338194473567,14.3294237829629));
#269358=CARTESIAN_POINT('Ctrl Pts',(1.10890262941845,1.09083819597026,14.3291673620266));
#269359=CARTESIAN_POINT('Ctrl Pts',(1.11564441217541,1.08395321181499,14.3284774847724));
#269360=CARTESIAN_POINT('Ctrl Pts',(1.11986160421642,1.07959576252823,14.3280452947567));
#269361=CARTESIAN_POINT('Ctrl Pts',(1.13884623476006,1.05974878955028,14.3260960940857));
#269362=CARTESIAN_POINT('Ctrl Pts',(1.15331943010993,1.043979241614,14.3246001274156));
#269363=CARTESIAN_POINT('Ctrl Pts',(1.17030921405807,1.02468294497131,14.3228244102407));
#269364=CARTESIAN_POINT('Ctrl Pts',(1.17314152807511,1.02143905846759,14.3225277091567));
#269365=CARTESIAN_POINT('Ctrl Pts',(1.18637016239279,1.00616052474135,14.3211385094828));
#269366=CARTESIAN_POINT('Ctrl Pts',(1.19659534262965,0.993978262325523,
14.3200547128902));
#269367=CARTESIAN_POINT('Ctrl Pts',(1.30038614212316,0.866398690485069,
14.3089227094254));
#269368=CARTESIAN_POINT('Ctrl Pts',(1.37714534498762,0.738324552090829,
14.2994889485436));
#269369=CARTESIAN_POINT('Ctrl Pts',(1.43457668360422,0.601306900724686,
14.2893889670083));
#269370=CARTESIAN_POINT('Ctrl Pts',(1.43457666475166,0.601306945702447,
14.1492791259731));
#269371=CARTESIAN_POINT('Ctrl Pts',(1.41615095798171,0.645266339740121,
14.1524805185963));
#269372=CARTESIAN_POINT('Ctrl Pts',(1.39571127249006,0.688363216504817,
14.1557269862668));
#269373=CARTESIAN_POINT('Ctrl Pts',(1.36533555092534,0.745471761040895,
14.1602228695212));
#269374=CARTESIAN_POINT('Ctrl Pts',(1.3571062184931,0.760349909706468,14.1614126364628));
#269375=CARTESIAN_POINT('Ctrl Pts',(1.34479420304447,0.781772481299565,
14.1631543778237));
#269376=CARTESIAN_POINT('Ctrl Pts',(1.34090390144716,0.788426524346289,
14.1636994630176));
#269377=CARTESIAN_POINT('Ctrl Pts',(1.33399232294111,0.800049088212788,
14.1646589011918));
#269378=CARTESIAN_POINT('Ctrl Pts',(1.33099231371677,0.805030136308535,
14.1650724769881));
#269379=CARTESIAN_POINT('Ctrl Pts',(1.32510643631638,0.814679879830104,
14.1658784216071));
#269380=CARTESIAN_POINT('Ctrl Pts',(1.32222364325466,0.819350358492522,
14.1662706733348));
#269381=CARTESIAN_POINT('Ctrl Pts',(1.31444659519299,0.831802200864574,
14.1673223448837));
#269382=CARTESIAN_POINT('Ctrl Pts',(1.30950804419281,0.839555494556103,
14.1679833896785));
#269383=CARTESIAN_POINT('Ctrl Pts',(1.29113768537945,0.867839645452182,
14.1704181551143));
#269384=CARTESIAN_POINT('Ctrl Pts',(1.27729005128138,0.888094685551313,
14.1722072558396));
#269385=CARTESIAN_POINT('Ctrl Pts',(1.26033577187772,0.911676672489267,
14.174346283534));
#269386=CARTESIAN_POINT('Ctrl Pts',(1.25768569959545,0.915329062849927,
14.1746792037951));
#269387=CARTESIAN_POINT('Ctrl Pts',(1.15521085351981,1.0552770301321,14.1874984922414));
#269388=CARTESIAN_POINT('Ctrl Pts',(1.03386376484364,1.1744034179853,14.2008904314514));
#269389=CARTESIAN_POINT('Ctrl Pts',(0.86849596856837,1.29089546984202,14.2162325932811));
#269390=CARTESIAN_POINT('Ctrl Pts',(0.840568560973116,1.30925218258257,
14.2187336155123));
#269391=CARTESIAN_POINT('Ctrl Pts',(0.806320926591495,1.33021510796637,
14.2216757884163));
#269392=CARTESIAN_POINT('Ctrl Pts',(0.800549860318849,1.33369621567632,
14.2221674263225));
#269393=CARTESIAN_POINT('Ctrl Pts',(0.791533462962841,1.33905529470563,
14.2229288898673));
#269394=CARTESIAN_POINT('Ctrl Pts',(0.788303753806995,1.34095917082117,
14.2232003331356));
#269395=CARTESIAN_POINT('Ctrl Pts',(0.782284672796656,1.34447808797766,
14.2237037242665));
#269396=CARTESIAN_POINT('Ctrl Pts',(0.779497189324543,1.34609612231607,
14.2239358570836));
#269397=CARTESIAN_POINT('Ctrl Pts',(0.773124038606977,1.3497690727102,14.2244643559788));
#269398=CARTESIAN_POINT('Ctrl Pts',(0.769535199760015,1.35181837023764,
14.2247603601764));
#269399=CARTESIAN_POINT('Ctrl Pts',(0.760136659553227,1.3571355640577,14.2255314794755));
#269400=CARTESIAN_POINT('Ctrl Pts',(0.754313963980703,1.36038050867561,
14.2260051757787));
#269401=CARTESIAN_POINT('Ctrl Pts',(0.714390058465094,1.38229465252935,
14.2292269138871));
#269402=CARTESIAN_POINT('Ctrl Pts',(0.679616700559208,1.39971905520224,
14.2319030886684));
#269403=CARTESIAN_POINT('Ctrl Pts',(0.557680721110371,1.45520196238738,
14.2409742755611));
#269404=CARTESIAN_POINT('Ctrl Pts',(0.467704087879769,1.48656518539461,
14.2471443532155));
#269405=CARTESIAN_POINT('Ctrl Pts',(0.297105345708217,1.52899358283808,
14.2587657909073));
#269406=CARTESIAN_POINT('Ctrl Pts',(0.217402974511302,1.5423444173344,14.2641658962156));
#269407=CARTESIAN_POINT('Ctrl Pts',(0.118831885331883,1.55106190972053,
14.2710334748072));
#269408=CARTESIAN_POINT('Ctrl Pts',(0.100606077109826,1.55235061536784,
14.272310690932));
#269409=CARTESIAN_POINT('Ctrl Pts',(0.0744404945306592,1.55373800769298,
14.2741568161015));
#269410=CARTESIAN_POINT('Ctrl Pts',(0.0665155791580642,1.55409744138275,
14.2747176015493));
#269411=CARTESIAN_POINT('Ctrl Pts',(0.0527414603637865,1.5546166162528,
14.2756952957193));
#269412=CARTESIAN_POINT('Ctrl Pts',(0.0468934065256717,1.55480400433193,
14.2761113341421));
#269413=CARTESIAN_POINT('Ctrl Pts',(0.0356189492305106,1.55510160363929,
14.2769152897417));
#269414=CARTESIAN_POINT('Ctrl Pts',(0.0301927434527061,1.55521641711133,
14.2773030570594));
#269415=CARTESIAN_POINT('Ctrl Pts',(0.0173401977181681,1.55542107665724,
14.2782235632367));
#269416=CARTESIAN_POINT('Ctrl Pts',(0.00991365484985559,1.55548613753573,
14.2787570677559));
#269417=CARTESIAN_POINT('Ctrl Pts',(-0.0163044721599605,1.55552805707598,
14.2806463886457));
#269418=CARTESIAN_POINT('Ctrl Pts',(-0.0350941927334791,1.55521757717389,
14.2820110866454));
#269419=CARTESIAN_POINT('Ctrl Pts',(-0.155588080260383,1.55104190617281,
14.2908350002324));
#269420=CARTESIAN_POINT('Ctrl Pts',(-0.256692252927695,1.53754360718377,
14.2985947740687));
#269421=CARTESIAN_POINT('Ctrl Pts',(-0.401040464613895,1.50363312636605,
14.3100734624229));
#269422=CARTESIAN_POINT('Ctrl Pts',(-0.445844737903421,1.49096228745882,
14.3136906990146));
#269423=CARTESIAN_POINT('Ctrl Pts',(-0.545740143620875,1.45780503420672,
14.3218166073789));
#269424=CARTESIAN_POINT('Ctrl Pts',(-0.600381412745239,1.43616558094254,
14.3263052277747));
#269425=CARTESIAN_POINT('Ctrl Pts',(-0.664205836612502,1.4066078258431,
14.3315070239361));
#269426=CARTESIAN_POINT('Ctrl Pts',(-0.674683584151132,1.40161230441675,
14.332359535248));
#269427=CARTESIAN_POINT('Ctrl Pts',(-0.689293537626307,1.39444484898514,
14.33354524951));
#269428=CARTESIAN_POINT('Ctrl Pts',(-0.693473040825964,1.39237105724174,
14.3338841005771));
#269429=CARTESIAN_POINT('Ctrl Pts',(-0.700592755273029,1.38879837688395,
14.3344606518894));
#269430=CARTESIAN_POINT('Ctrl Pts',(-0.70353762133428,1.38730889011528,
14.334698926757));
#269431=CARTESIAN_POINT('Ctrl Pts',(-0.709207460892252,1.38441843927126,
14.335157271851));
#269432=CARTESIAN_POINT('Ctrl Pts',(-0.711933047831652,1.38301878997667,
14.3353774245943));
#269433=CARTESIAN_POINT('Ctrl Pts',(-0.718480108061998,1.37963224638834,
14.3359058540576));
#269434=CARTESIAN_POINT('Ctrl Pts',(-0.722297528208144,1.37763750053657,
14.3362136437028));
#269435=CARTESIAN_POINT('Ctrl Pts',(-0.736257871888219,1.37026871559943,
14.337338228532));
#269436=CARTESIAN_POINT('Ctrl Pts',(-0.746349844426033,1.36479813053238,
14.3381492425614));
#269437=CARTESIAN_POINT('Ctrl Pts',(-0.851897287926064,1.3060627679079,
14.3466206333362));
#269438=CARTESIAN_POINT('Ctrl Pts',(-0.941561329325435,1.24297994671131,
14.353738743941));
#269439=CARTESIAN_POINT('Ctrl Pts',(-1.10359824444006,1.10130144245127,
14.3679136434628));
#269440=CARTESIAN_POINT('Ctrl Pts',(-1.17597910480945,1.02365144088429,
14.3749353706486));
#269441=CARTESIAN_POINT('Ctrl Pts',(-1.2482033916897,0.928308826371025,
14.3832834447503));
#269442=CARTESIAN_POINT('Ctrl Pts',(-1.25635317904375,0.91724895881205,
14.3842476420301));
#269443=CARTESIAN_POINT('Ctrl Pts',(-1.26847768455944,0.900330328751975,
14.3857171296547));
#269444=CARTESIAN_POINT('Ctrl Pts',(-1.27256081592829,0.894549777188648,
14.3862182546709));
#269445=CARTESIAN_POINT('Ctrl Pts',(-1.27988490520559,0.884029325193976,
14.3871286875832));
#269446=CARTESIAN_POINT('Ctrl Pts',(-1.28313935497527,0.879298932372164,
14.387537473274));
#269447=CARTESIAN_POINT('Ctrl Pts',(-1.29007807956924,0.869092834607,14.3884182765239));
#269448=CARTESIAN_POINT('Ctrl Pts',(-1.29375383228069,0.863611501503633,
14.3888906048745));
#269449=CARTESIAN_POINT('Ctrl Pts',(-1.30356805931941,0.848773113891189,
14.3901674117379));
#269450=CARTESIAN_POINT('Ctrl Pts',(-1.30964051764068,0.839373091380753,
14.3909743276963));
#269451=CARTESIAN_POINT('Ctrl Pts',(-1.33861049025997,0.793448502152106,
14.394908063641));
#269452=CARTESIAN_POINT('Ctrl Pts',(-1.36008223339606,0.756051728565129,
14.3980862297483));
#269453=CARTESIAN_POINT('Ctrl Pts',(-1.44996338279417,0.583258649341762,
14.4126746345461));
#269454=CARTESIAN_POINT('Ctrl Pts',(-1.49988575723115,0.439220128545266,
14.424682208944));
#269455=CARTESIAN_POINT('Ctrl Pts',(-1.53422623095591,0.258418640860106,
14.4386285103538));
#269456=CARTESIAN_POINT('Ctrl Pts',(-1.53927720453619,0.226398758163,14.4410526389676));
#269457=CARTESIAN_POINT('Ctrl Pts',(-1.54415888398919,0.187611940616024,
14.4439166738966));
#269458=CARTESIAN_POINT('Ctrl Pts',(-1.5449505865198,0.180976763181725,
14.4444040725565));
#269459=CARTESIAN_POINT('Ctrl Pts',(-1.54611830821319,0.170623529340433,
14.4451604114354));
#269460=CARTESIAN_POINT('Ctrl Pts',(-1.54652371647945,0.166908977954843,
14.4454309351536));
#269461=CARTESIAN_POINT('Ctrl Pts',(-1.54725405719984,0.159986034503915,
14.4459335170802));
#269462=CARTESIAN_POINT('Ctrl Pts',(-1.54758239499378,0.156778122789219,
14.4461657545738));
#269463=CARTESIAN_POINT('Ctrl Pts',(-1.54831055686672,0.149438611141913,
14.4466956465444));
#269464=CARTESIAN_POINT('Ctrl Pts',(-1.5487038209897,0.145306417391493,
14.4469929316527));
#269465=CARTESIAN_POINT('Ctrl Pts',(-1.54969098754791,0.134474286099981,
14.4477696084757));
#269466=CARTESIAN_POINT('Ctrl Pts',(-1.55025799118575,0.127771888903843,
14.4482475478732));
#269467=CARTESIAN_POINT('Ctrl Pts',(-1.55390021025738,0.0811172353033317,
14.4515574724266));
#269468=CARTESIAN_POINT('Ctrl Pts',(-1.55547444188554,0.0410586581403037,
14.4543130783304));
#269469=CARTESIAN_POINT('Ctrl Pts',(-1.55558242940234,-0.130350922880776,
14.4659067034203));
#269470=CARTESIAN_POINT('Ctrl Pts',(-1.53903344529269,-0.261167877420479,
14.4743024819735));
#269471=CARTESIAN_POINT('Ctrl Pts',(-1.50026039181661,-0.411549096672414,
14.4847494019014));
#269472=CARTESIAN_POINT('Ctrl Pts',(-1.49374598462802,-0.434599529382573,
14.4863721093593));
#269473=CARTESIAN_POINT('Ctrl Pts',(-1.48505329777108,-0.462848124196335,
14.4883928726107));
#269474=CARTESIAN_POINT('Ctrl Pts',(-1.48337541042363,-0.468197686673823,
14.4887769860116));
#269475=CARTESIAN_POINT('Ctrl Pts',(-1.48031806823913,-0.477763905217369,
14.4894665281685));
#269476=CARTESIAN_POINT('Ctrl Pts',(-1.47894941925461,-0.481983969584611,
14.4897716462491));
#269477=CARTESIAN_POINT('Ctrl Pts',(-1.46989365726946,-0.509504556147677,
14.4917676833024));
#269478=CARTESIAN_POINT('Ctrl Pts',(-1.46167459625255,-0.532625117546181,
14.4934739866947));
#269479=CARTESIAN_POINT('Ctrl Pts',(-1.44962939782763,-0.564127083508641,
14.4958443460546));
#269480=CARTESIAN_POINT('Ctrl Pts',(-1.44627024113819,-0.572684154233286,
14.4964929005276));
#269481=CARTESIAN_POINT('Ctrl Pts',(-1.44078469007477,-0.586301843356348,
14.4975327403878));
#269482=CARTESIAN_POINT('Ctrl Pts',(-1.43870697567624,-0.591381950529767,
14.4979223867085));
#269483=CARTESIAN_POINT('Ctrl Pts',(-1.43437281002033,-0.601821155173974,
14.4987267096439));
#269484=CARTESIAN_POINT('Ctrl Pts',(-1.432113110824,-0.607178801556033,
14.4991414908342));
#269485=CARTESIAN_POINT('Ctrl Pts',(-1.42678831983815,-0.619608545011971,
14.5001084770268));
#269486=CARTESIAN_POINT('Ctrl Pts',(-1.42370061995286,-0.626670726508734,
14.5006614428106));
#269487=CARTESIAN_POINT('Ctrl Pts',(-1.4136344050101,-0.649235746098329,
14.5024399033955));
#269488=CARTESIAN_POINT('Ctrl Pts',(-1.40645438714995,-0.664646747761118,
14.5036722448325));
#269489=CARTESIAN_POINT('Ctrl Pts',(-1.36840372830881,-0.742939016893913,
14.5100267867545));
#269490=CARTESIAN_POINT('Ctrl Pts',(-1.33356790150155,-0.803791727598661,
14.5152850630738));
#269491=CARTESIAN_POINT('Ctrl Pts',(-1.23851960288269,-0.946544050852793,
14.5284073457598));
#269492=CARTESIAN_POINT('Ctrl Pts',(-1.17415745957458,-1.0252947383269,
14.536361339362));
#269493=CARTESIAN_POINT('Ctrl Pts',(-1.09485814420198,-1.10498233822317,
14.544962019682));
#269494=CARTESIAN_POINT('Ctrl Pts',(-1.08704672058147,-1.11266785748559,
14.5457976340851));
#269495=CARTESIAN_POINT('Ctrl Pts',(-1.05433096190226,-1.14418289378781,
14.5492476559074));
#269496=CARTESIAN_POINT('Ctrl Pts',(-1.02871693580132,-1.1672661190051,
14.5518315425071));
#269497=CARTESIAN_POINT('Ctrl Pts',(-0.997427498539236,-1.1936331729162,
14.5548324502846));
#269498=CARTESIAN_POINT('Ctrl Pts',(-0.992474468967387,-1.19775464875928,
14.5553030330538));
#269499=CARTESIAN_POINT('Ctrl Pts',(-0.984354670153629,-1.20442627908317,
14.5560670665393));
#269500=CARTESIAN_POINT('Ctrl Pts',(-0.981203326836895,-1.20699495062057,
14.5563617904985));
#269501=CARTESIAN_POINT('Ctrl Pts',(-0.975539574888806,-1.21157465453732,
14.5568882099897));
#269502=CARTESIAN_POINT('Ctrl Pts',(-0.973030974179026,-1.21359026431431,
14.5571202282162));
#269503=CARTESIAN_POINT('Ctrl Pts',(-0.967547555823956,-1.21796814661827,
14.5576248908952));
#269504=CARTESIAN_POINT('Ctrl Pts',(-0.96457033851482,-1.22032730931075,
14.5578973147137));
#269505=CARTESIAN_POINT('Ctrl Pts',(-0.956106922599905,-1.22698344069285,
14.558667366611));
#269506=CARTESIAN_POINT('Ctrl Pts',(-0.9506003554593,-1.23125455541696,
14.5591632079469));
#269507=CARTESIAN_POINT('Ctrl Pts',(-0.915002416928547,-1.2584845677591,
14.5623368753823));
#269508=CARTESIAN_POINT('Ctrl Pts',(-0.884107216886533,-1.2803780111328,
14.5649464116578));
#269509=CARTESIAN_POINT('Ctrl Pts',(-0.7618847624684,-1.36045291495877,
14.5748557419773));
#269510=CARTESIAN_POINT('Ctrl Pts',(-0.665376606737659,-1.41016953035004,
14.5818423690219));
#269511=CARTESIAN_POINT('Ctrl Pts',(-0.492474356317959,-1.4775048468549,
14.5941585880479));
#269512=CARTESIAN_POINT('Ctrl Pts',(-0.41848837780569,-1.50013880604874,
14.5993683872779));
#269513=CARTESIAN_POINT('Ctrl Pts',(-0.33162037720998,-1.51978535423363,
14.6055897154412));
#269514=CARTESIAN_POINT('Ctrl Pts',(-0.320077636616072,-1.52225815504397,
14.6064182853689));
#269515=CARTESIAN_POINT('Ctrl Pts',(-0.301278406107025,-1.5260622468872,
14.607771375509));
#269516=CARTESIAN_POINT('Ctrl Pts',(-0.294038468768413,-1.52747374277408,
14.6082933450789));
#269517=CARTESIAN_POINT('Ctrl Pts',(-0.281118076337098,-1.52989743667297,
14.609226526818));
#269518=CARTESIAN_POINT('Ctrl Pts',(-0.275441471715819,-1.53092963051871,
14.6096370964701));
#269519=CARTESIAN_POINT('Ctrl Pts',(-0.263449222806274,-1.53304135921232,
14.6105057308185));
#269520=CARTESIAN_POINT('Ctrl Pts',(-0.257132403957094,-1.53411349861104,
14.6109640214866));
#269521=CARTESIAN_POINT('Ctrl Pts',(-0.24033961603682,-1.53685707128588,
14.6121844284579));
#269522=CARTESIAN_POINT('Ctrl Pts',(-0.229853027484549,-1.53846038752966,
14.6129486782045));
#269523=CARTESIAN_POINT('Ctrl Pts',(-0.1795144870316,-1.54563060021993,
14.6166282252176));
#269524=CARTESIAN_POINT('Ctrl Pts',(-0.139476420704787,-1.54975649087051,
14.6195882101971));
#269525=CARTESIAN_POINT('Ctrl Pts',(0.049628203695662,-1.56185648608417,
14.6337392620499));
#269526=CARTESIAN_POINT('Ctrl Pts',(0.199172829396593,-1.54989517817302,
14.6455283080303));
#269527=CARTESIAN_POINT('Ctrl Pts',(0.381606903810736,-1.50843981305747,
14.6597751057999));
#269528=CARTESIAN_POINT('Ctrl Pts',(0.418222052045253,-1.49870123723444,
14.6626209922974));
#269529=CARTESIAN_POINT('Ctrl Pts',(0.460775739576232,-1.48570176561497,
14.665885632442));
#269530=CARTESIAN_POINT('Ctrl Pts',(0.46709063242107,-1.48372853439972,
14.6663689680884));
#269531=CARTESIAN_POINT('Ctrl Pts',(0.477315224547363,-1.48046188113127,
14.6671494978251));
#269532=CARTESIAN_POINT('Ctrl Pts',(0.481232627321724,-1.47919314645751,
14.6674480558005));
#269533=CARTESIAN_POINT('Ctrl Pts',(0.488206099426863,-1.47690400314015,
14.6679785945315));
#269534=CARTESIAN_POINT('Ctrl Pts',(0.491264073349703,-1.47588964389191,
14.6682109200075));
#269535=CARTESIAN_POINT('Ctrl Pts',(0.49788370355583,-1.47367099535311,
14.668713127481));
#269536=CARTESIAN_POINT('Ctrl Pts',(0.501444148246857,-1.47246329387548,
14.6689828061441));
#269537=CARTESIAN_POINT('Ctrl Pts',(0.511420793187353,-1.46903883639715,
14.6697373262768));
#269538=CARTESIAN_POINT('Ctrl Pts',(0.517827017720188,-1.46679293520486,
14.6702204933922));
#269539=CARTESIAN_POINT('Ctrl Pts',(0.556505600512279,-1.45294796594852,
14.6731308331912));
#269540=CARTESIAN_POINT('Ctrl Pts',(0.588404848215433,-1.4403251237996,
14.6755021300159));
#269541=CARTESIAN_POINT('Ctrl Pts',(0.695198042385484,-1.3939248848908,
14.6834267708379));
#269542=CARTESIAN_POINT('Ctrl Pts',(0.767827976580619,-1.35527465416929,
14.6887973520171));
#269543=CARTESIAN_POINT('Ctrl Pts',(0.927342274078477,-1.25343026065,14.7012603782791));
#269544=CARTESIAN_POINT('Ctrl Pts',(1.01140602005964,-1.18663557705038,
14.7083614280825));
#269545=CARTESIAN_POINT('Ctrl Pts',(1.09644066819439,-1.10342179916349,
14.7166712186744));
#269546=CARTESIAN_POINT('Ctrl Pts',(1.10484821117991,-1.09500329780913,
14.7175062382373));
#269547=CARTESIAN_POINT('Ctrl Pts',(1.1183298878144,-1.08119070234061,14.7188677815361));
#269548=CARTESIAN_POINT('Ctrl Pts',(1.12346363989359,-1.07585525012657,
14.719391701076));
#269549=CARTESIAN_POINT('Ctrl Pts',(1.13253197711948,-1.06629493978487,
14.7203270621179));
#269550=CARTESIAN_POINT('Ctrl Pts',(1.13648153107041,-1.0620844155251,14.7207378498221));
#269551=CARTESIAN_POINT('Ctrl Pts',(1.14475445392842,-1.05316586846507,
14.7216055933696));
#269552=CARTESIAN_POINT('Ctrl Pts',(1.14907241419645,-1.04845299893241,
14.7220627681592));
#269553=CARTESIAN_POINT('Ctrl Pts',(1.16043265078725,-1.03589931173692,
14.7232770350641));
#269554=CARTESIAN_POINT('Ctrl Pts',(1.16742438936073,-1.02801342697538,
14.7240362226237));
#269555=CARTESIAN_POINT('Ctrl Pts',(1.20019323418368,-0.990288475774633,
14.7276519056707));
#269556=CARTESIAN_POINT('Ctrl Pts',(1.22490753008888,-0.959549940723327,
14.73055122582));
#269557=CARTESIAN_POINT('Ctrl Pts',(1.3377594085566,-0.807716854184142,
14.7446695056808));
#269558=CARTESIAN_POINT('Ctrl Pts',(1.40926154753768,-0.675258831606486,
14.7564961230062));
#269559=CARTESIAN_POINT('Ctrl Pts',(1.47387977250682,-0.49872264221895,
14.7708163227759));
#269560=CARTESIAN_POINT('Ctrl Pts',(1.48570861944867,-0.462294665066724,
14.7736939763001));
#269561=CARTESIAN_POINT('Ctrl Pts',(1.49799705850008,-0.41908124900415,
14.7769904466823));
#269562=CARTESIAN_POINT('Ctrl Pts',(1.49977121346047,-0.41268703881596,
14.7774752447048));
#269563=CARTESIAN_POINT('Ctrl Pts',(1.50258148288639,-0.402301058156212,
14.7782576638021));
#269564=CARTESIAN_POINT('Ctrl Pts',(1.50364271259795,-0.398316266326904,
14.7785566593244));
#269565=CARTESIAN_POINT('Ctrl Pts',(1.50550496739803,-0.391210207308202,
14.7790876722839));
#269566=CARTESIAN_POINT('Ctrl Pts',(1.50631215039805,-0.388090633013378,
14.7793200369489));
#269567=CARTESIAN_POINT('Ctrl Pts',(1.50803907472301,-0.381329912391649,
14.7798219829311));
#269568=CARTESIAN_POINT('Ctrl Pts',(1.50895532511103,-0.3776879407694,14.7800913628154));
#269569=CARTESIAN_POINT('Ctrl Pts',(1.51148602956775,-0.367472513426196,
14.780844198789));
#269570=CARTESIAN_POINT('Ctrl Pts',(1.51307080689287,-0.360891678338084,
14.7813259925093));
#269571=CARTESIAN_POINT('Ctrl Pts',(1.52234218360128,-0.321257124619396,
14.7842097390996));
#269572=CARTESIAN_POINT('Ctrl Pts',(1.52898909699851,-0.287966395677746,
14.7865569967321));
#269573=CARTESIAN_POINT('Ctrl Pts',(1.56425065248389,-0.0753368845034653,
14.8012314348214));
#269574=CARTESIAN_POINT('Ctrl Pts',(1.56236500970744,0.107627522009729,
14.8126094172263));
#269575=CARTESIAN_POINT('Ctrl Pts',(1.52558848064339,0.30412905366778,14.8264773773804));
#269576=CARTESIAN_POINT('Ctrl Pts',(1.52190760050675,0.32204332017638,14.8277552236677));
#269577=CARTESIAN_POINT('Ctrl Pts',(1.51631020672089,0.347040828788507,
14.8295592702533));
#269578=CARTESIAN_POINT('Ctrl Pts',(1.51465801938965,0.354182242426665,
14.8300770675531));
#269579=CARTESIAN_POINT('Ctrl Pts',(1.5117004432393,0.366566790541964,14.8309793413134));
#269580=CARTESIAN_POINT('Ctrl Pts',(1.5104180852256,0.371815341937226,14.8313630756621));
#269581=CARTESIAN_POINT('Ctrl Pts',(1.50768574108579,0.382751097149428,
14.8321654947747));
#269582=CARTESIAN_POINT('Ctrl Pts',(1.50623086172509,0.388436977761936,
14.8325843313073));
#269583=CARTESIAN_POINT('Ctrl Pts',(1.50270745449472,0.401889480763949,
14.8335792191401));
#269584=CARTESIAN_POINT('Ctrl Pts',(1.50061085754058,0.409648505770617,
14.8341561676337));
#269585=CARTESIAN_POINT('Ctrl Pts',(1.49338844329536,0.43557734120893,14.8360949095229));
#269586=CARTESIAN_POINT('Ctrl Pts',(1.48799217319954,0.45366936966431,14.8374653984487));
#269587=CARTESIAN_POINT('Ctrl Pts',(1.47434382819559,0.49656169427142,14.8407584907405));
#269588=CARTESIAN_POINT('Ctrl Pts',(1.46579357257349,0.521260293856361,
14.8426903343373));
#269589=CARTESIAN_POINT('Ctrl Pts',(1.44962853802406,0.564406873256468,
14.8461292864136));
#269590=CARTESIAN_POINT('Ctrl Pts',(1.44227704762217,0.58293565034592,14.8476274724982));
#269591=CARTESIAN_POINT('Ctrl Pts',(1.43457662445954,0.601307041829941,
14.8491341039362));
#269592=CARTESIAN_POINT('Origin',(0.,0.,-1.29405622560371));
#269593=CARTESIAN_POINT('',(1.4345766974292,0.601306867741532,15.6881535475172));
#269594=CARTESIAN_POINT('',(1.43457668274383,0.601306902777371,15.5515012983457));
#269595=CARTESIAN_POINT('',(1.43457668357355,0.601306900797845,-1.29405622560371));
#269596=CARTESIAN_POINT('Ctrl Pts',(1.43457669742932,0.601306867741247,
15.6881535475172));
#269597=CARTESIAN_POINT('Ctrl Pts',(1.45874319013863,0.543651302572655,
15.6833052102356));
#269598=CARTESIAN_POINT('Ctrl Pts',(1.47944557503403,0.484511145403499,
15.6784494417411));
#269599=CARTESIAN_POINT('Ctrl Pts',(1.50559969200234,0.392241097227874,
15.6711766387542));
#269600=CARTESIAN_POINT('Ctrl Pts',(1.51363277875958,0.359999636504437,
15.6686905268506));
#269601=CARTESIAN_POINT('Ctrl Pts',(1.52203249339847,0.321001310937034,
15.6657678630902));
#269602=CARTESIAN_POINT('Ctrl Pts',(1.52339519752378,0.314470712569572,
15.6652812596447));
#269603=CARTESIAN_POINT('Ctrl Pts',(1.52544945226465,0.304299112998734,
15.664527951634));
#269604=CARTESIAN_POINT('Ctrl Pts',(1.52617005541673,0.300664171984863,
15.6642596576344));
#269605=CARTESIAN_POINT('Ctrl Pts',(1.52748518643701,0.293903686810627,
15.6637624004689));
#269606=CARTESIAN_POINT('Ctrl Pts',(1.52808311002675,0.290778921319678,
15.6635332547922));
#269607=CARTESIAN_POINT('Ctrl Pts',(1.52942423314351,0.28365178556088,15.6630121620093));
#269608=CARTESIAN_POINT('Ctrl Pts',(1.53016131116095,0.279648320617172,
15.6627205641679));
#269609=CARTESIAN_POINT('Ctrl Pts',(1.53204293262263,0.269198018218926,
15.6619621877474));
#269610=CARTESIAN_POINT('Ctrl Pts',(1.53316251837995,0.262746677708289,
15.6614967759841));
#269611=CARTESIAN_POINT('Ctrl Pts',(1.5403882809248,0.219490456809539,15.6583934791403));
#269612=CARTESIAN_POINT('Ctrl Pts',(1.54520998398117,0.182479554578232,
15.6558218672983));
#269613=CARTESIAN_POINT('Ctrl Pts',(1.55007179064466,0.13066923654386,15.6522928750845));
#269614=CARTESIAN_POINT('Ctrl Pts',(1.55123915758606,0.115991829365177,
15.6513010396435));
#269615=CARTESIAN_POINT('Ctrl Pts',(1.55446740582268,0.066525925349292,
15.6479784306287));
#269616=CARTESIAN_POINT('Ctrl Pts',(1.55556770599653,0.0316844245101462,
15.6456713653327));
#269617=CARTESIAN_POINT('Ctrl Pts',(1.55533385693495,-0.0832171977139087,
15.6380928381742));
#269618=CARTESIAN_POINT('Ctrl Pts',(1.54899173983458,-0.163133326739185,
15.6328632538657));
#269619=CARTESIAN_POINT('Ctrl Pts',(1.52743741979106,-0.299872221051706,
15.6235783621063));
#269620=CARTESIAN_POINT('Ctrl Pts',(1.51510906566858,-0.35697567083628,
15.6195976743679));
#269621=CARTESIAN_POINT('Ctrl Pts',(1.49648750822896,-0.424550190407996,
15.6146917783434));
#269622=CARTESIAN_POINT('Ctrl Pts',(1.49324491219919,-0.435818018605811,
15.6138671772992));
#269623=CARTESIAN_POINT('Ctrl Pts',(1.48797841216963,-0.453369671088375,
15.6125719290709));
#269624=CARTESIAN_POINT('Ctrl Pts',(1.48604131186894,-0.45967926941373,
15.6121041103411));
#269625=CARTESIAN_POINT('Ctrl Pts',(1.48253773367707,-0.470837637753408,
15.6112728021752));
#269626=CARTESIAN_POINT('Ctrl Pts',(1.48098746588687,-0.475691431133484,
15.6109098483265));
#269627=CARTESIAN_POINT('Ctrl Pts',(1.47736169311522,-0.486853967185574,
15.6100719995129));
#269628=CARTESIAN_POINT('Ctrl Pts',(1.47526958917049,-0.49315717006524,
15.6095965646843));
#269629=CARTESIAN_POINT('Ctrl Pts',(1.46941443471303,-0.510427173155055,
15.6082874275026));
#269630=CARTESIAN_POINT('Ctrl Pts',(1.4655690989699,-0.521365402229734,
15.6074510265751));
#269631=CARTESIAN_POINT('Ctrl Pts',(1.4445469761717,-0.579092852828204,
15.6029973999521));
#269632=CARTESIAN_POINT('Ctrl Pts',(1.4252528747187,-0.625074166119957,
15.5993104422468));
#269633=CARTESIAN_POINT('Ctrl Pts',(1.34071975863937,-0.802176257105888,
15.5845370711677));
#269634=CARTESIAN_POINT('Ctrl Pts',(1.25932694589711,-0.924717371307711,
15.5729452342796));
#269635=CARTESIAN_POINT('Ctrl Pts',(1.14170867403552,-1.05688925041815,
15.5595596940166));
#269636=CARTESIAN_POINT('Ctrl Pts',(1.12072945446215,-1.07911046959223,
15.5572775288031));
#269637=CARTESIAN_POINT('Ctrl Pts',(1.09449795302527,-1.10530399214629,
15.5545626498978));
#269638=CARTESIAN_POINT('Ctrl Pts',(1.08985943469471,-1.10987796665545,
15.5540876214665));
#269639=CARTESIAN_POINT('Ctrl Pts',(1.08256184439132,-1.11698414604593,
15.5533483121491));
#269640=CARTESIAN_POINT('Ctrl Pts',(1.0799223819164,-1.11953623400272,15.5530825335575));
#269641=CARTESIAN_POINT('Ctrl Pts',(1.07497553912838,-1.12428554713978,
15.5525874764719));
#269642=CARTESIAN_POINT('Ctrl Pts',(1.07267046762741,-1.12648500629478,
15.5523580308282));
#269643=CARTESIAN_POINT('Ctrl Pts',(1.06736838415157,-1.13151313072728,
15.5518330648835));
#269644=CARTESIAN_POINT('Ctrl Pts',(1.06436687829317,-1.13433697900724,
15.5515379143555));
#269645=CARTESIAN_POINT('Ctrl Pts',(1.05644484613809,-1.14173098127667,
15.5507641165993));
#269646=CARTESIAN_POINT('Ctrl Pts',(1.05150581517116,-1.14628132301999,
15.5502869285026));
#269647=CARTESIAN_POINT('Ctrl Pts',(1.01612399830472,-1.17845755209012,
15.5469042260504));
#269648=CARTESIAN_POINT('Ctrl Pts',(0.984622792796408,-1.20490201808363,
15.5440793453098));
#269649=CARTESIAN_POINT('Ctrl Pts',(0.937125174460898,-1.24166646384064,
15.5400205568663));
#269650=CARTESIAN_POINT('Ctrl Pts',(0.921931851616002,-1.25298878865298,
15.5387505126898));
#269651=CARTESIAN_POINT('Ctrl Pts',(0.84913468415556,-1.30519730260713,
15.5327778772585));
#269652=CARTESIAN_POINT('Ctrl Pts',(0.788995506759633,-1.34240693759025,
15.5281670272871));
#269653=CARTESIAN_POINT('Ctrl Pts',(0.644868598726049,-1.41853971744403,
15.5174026723607));
#269654=CARTESIAN_POINT('Ctrl Pts',(0.559536182516225,-1.45431283344704,
15.5112248625628));
#269655=CARTESIAN_POINT('Ctrl Pts',(0.459277692117528,-1.48620655328027,
15.5038732748825));
#269656=CARTESIAN_POINT('Ctrl Pts',(0.446964546459356,-1.48995590343311,
15.502969153361));
#269657=CARTESIAN_POINT('Ctrl Pts',(0.428034545496895,-1.49546431824363,
15.5015766122785));
#269658=CARTESIAN_POINT('Ctrl Pts',(0.421450027597146,-1.49733328648135,
15.5010917677439));
#269659=CARTESIAN_POINT('Ctrl Pts',(0.409448089354381,-1.5006545131494,
15.5002070608285));
#269660=CARTESIAN_POINT('Ctrl Pts',(0.404034710841987,-1.50212105259046,
15.4998076687979));
#269661=CARTESIAN_POINT('Ctrl Pts',(0.392223973644245,-1.50525223838375,
15.4989354612995));
#269662=CARTESIAN_POINT('Ctrl Pts',(0.385823722875915,-1.50690543798597,
15.4984622846564));
#269663=CARTESIAN_POINT('Ctrl Pts',(0.368300978655044,-1.51131265209707,
15.4971652633676));
#269664=CARTESIAN_POINT('Ctrl Pts',(0.357158480000599,-1.51398459383233,
15.4963388015963));
#269665=CARTESIAN_POINT('Ctrl Pts',(0.299308195396958,-1.52718278220831,
15.4920382400436));
#269666=CARTESIAN_POINT('Ctrl Pts',(0.25216701831684,-1.53567038326185,
15.4885000213669));
#269667=CARTESIAN_POINT('Ctrl Pts',(0.0589964587991515,-1.5613159558735,
15.4738516603627));
#269668=CARTESIAN_POINT('Ctrl Pts',(-0.0886988826687305,-1.55990710361526,
15.4622176580609));
#269669=CARTESIAN_POINT('Ctrl Pts',(-0.265642821647463,-1.53298382783339,
15.4486590115296));
#269670=CARTESIAN_POINT('Ctrl Pts',(-0.297145130524926,-1.52719045093759,
15.4462644710532));
#269671=CARTESIAN_POINT('Ctrl Pts',(-0.334902683999179,-1.51903391601913,
15.4434348722881));
#269672=CARTESIAN_POINT('Ctrl Pts',(-0.341347735255132,-1.51759862071411,
15.4429533101879));
#269673=CARTESIAN_POINT('Ctrl Pts',(-0.351380932425219,-1.51529710355211,
15.4422060965731));
#269674=CARTESIAN_POINT('Ctrl Pts',(-0.354975362517023,-1.51445909963988,
15.4419388958567));
#269675=CARTESIAN_POINT('Ctrl Pts',(-0.361664450821116,-1.51287448546476,
15.4414426048312));
#269676=CARTESIAN_POINT('Ctrl Pts',(-0.364759770699785,-1.5121311761055,
15.4412133386642));
#269677=CARTESIAN_POINT('Ctrl Pts',(-0.37182885646169,-1.51041063832276,
15.4406906072505));
#269678=CARTESIAN_POINT('Ctrl Pts',(-0.375801061018894,-1.50942722859638,
15.4403974999877));
#269679=CARTESIAN_POINT('Ctrl Pts',(-0.386187800823735,-1.50681221112393,
15.4396325832598));
#269680=CARTESIAN_POINT('Ctrl Pts',(-0.392595973949335,-1.5051552951318,
15.4391621794159));
#269681=CARTESIAN_POINT('Ctrl Pts',(-0.436585958248702,-1.49348105818434,
15.4359422059889));
#269682=CARTESIAN_POINT('Ctrl Pts',(-0.473795007339837,-1.4820971271957,
15.4332647348821));
#269683=CARTESIAN_POINT('Ctrl Pts',(-0.651630998362606,-1.42030517264415,
15.4205167036886));
#269684=CARTESIAN_POINT('Ctrl Pts',(-0.784926791220451,-1.35121643419585,
15.4110354358585));
#269685=CARTESIAN_POINT('Ctrl Pts',(-0.938398929554399,-1.24118668534751,
15.3981945814172));
#269686=CARTESIAN_POINT('Ctrl Pts',(-0.969575602328509,-1.21698793761691,
15.3954750300494));
#269687=CARTESIAN_POINT('Ctrl Pts',(-1.00780723286618,-1.18491103934747,
15.3919752602722));
#269688=CARTESIAN_POINT('Ctrl Pts',(-1.01574960983595,-1.17810963429126,
15.3912387983172));
#269689=CARTESIAN_POINT('Ctrl Pts',(-1.02838324571956,-1.16706817461973,
15.3900517563115));
#269690=CARTESIAN_POINT('Ctrl Pts',(-1.03311837379139,-1.16287860410109,
15.3896032684935));
#269691=CARTESIAN_POINT('Ctrl Pts',(-1.04207156308504,-1.15485911112617,
15.3887483413132));
#269692=CARTESIAN_POINT('Ctrl Pts',(-1.04629439177707,-1.15103464469578,
15.3883421352048));
#269693=CARTESIAN_POINT('Ctrl Pts',(-1.05587111589086,-1.14226509796828,
15.3874140450346));
#269694=CARTESIAN_POINT('Ctrl Pts',(-1.06121142277729,-1.13730544719794,
15.3868915473111));
#269695=CARTESIAN_POINT('Ctrl Pts',(-1.07501193334228,-1.12430680488447,
15.3855281694956));
#269696=CARTESIAN_POINT('Ctrl Pts',(-1.08341672904834,-1.11620993802489,
15.3846848125416));
#269697=CARTESIAN_POINT('Ctrl Pts',(-1.14571810467919,-1.05482451451753,
15.3783333393166));
#269698=CARTESIAN_POINT('Ctrl Pts',(-1.19573762981428,-0.99776391126455,
15.3726572283521));
#269699=CARTESIAN_POINT('Ctrl Pts',(-1.30770259268482,-0.84947259958713,
15.3584431895774));
#269700=CARTESIAN_POINT('Ctrl Pts',(-1.36450092300531,-0.754867889450489,
15.3497967750708));
#269701=CARTESIAN_POINT('Ctrl Pts',(-1.42685128866542,-0.620581257784346,
15.3385258350334));
#269702=CARTESIAN_POINT('Ctrl Pts',(-1.44159425794493,-0.585518821829499,
15.3356704585475));
#269703=CARTESIAN_POINT('Ctrl Pts',(-1.45748376826084,-0.543478742268391,
15.3323759735027));
#269704=CARTESIAN_POINT('Ctrl Pts',(-1.45988573846608,-0.536993215470201,
15.3318713032008));
#269705=CARTESIAN_POINT('Ctrl Pts',(-1.46352622396099,-0.526958601521506,
15.3310961887023));
#269706=CARTESIAN_POINT('Ctrl Pts',(-1.4647952240991,-0.523420794588629,
15.3308240073131));
#269707=CARTESIAN_POINT('Ctrl Pts',(-1.4671130372656,-0.516884586438547,
15.3303232031027));
#269708=CARTESIAN_POINT('Ctrl Pts',(-1.46816548251521,-0.513887590961846,
15.3300943743779));
#269709=CARTESIAN_POINT('Ctrl Pts',(-1.47052259306265,-0.50710901673015,
15.3295786041296));
#269710=CARTESIAN_POINT('Ctrl Pts',(-1.47182185447659,-0.503325621452828,
15.3292919830291));
#269711=CARTESIAN_POINT('Ctrl Pts',(-1.47561844614545,-0.492129690548404,
15.3284473791682));
#269712=CARTESIAN_POINT('Ctrl Pts',(-1.47807452733873,-0.484703135271742,
15.3278917479743));
#269713=CARTESIAN_POINT('Ctrl Pts',(-1.49720752986677,-0.425351770622989,
15.3234855812468));
#269714=CARTESIAN_POINT('Ctrl Pts',(-1.51120137157454,-0.372594262487917,
15.3197771830265));
#269715=CARTESIAN_POINT('Ctrl Pts',(-1.54432950799412,-0.214594635733381,
15.3089825340143));
#269716=CARTESIAN_POINT('Ctrl Pts',(-1.55542317921802,-0.108002426917552,
15.3020810023186));
#269717=CARTESIAN_POINT('Ctrl Pts',(-1.55554364612096,0.0604900793579502,
15.2908079468492));
#269718=CARTESIAN_POINT('Ctrl Pts',(-1.55192830998767,0.122033232736486,
15.2866182755));
#269719=CARTESIAN_POINT('Ctrl Pts',(-1.54335429864604,0.194328221685656,
15.2815282007728));
#269720=CARTESIAN_POINT('Ctrl Pts',(-1.54191358888956,0.20544688294018,
15.2807407189313));
#269721=CARTESIAN_POINT('Ctrl Pts',(-1.5393575461247,0.223628506224607,
15.2794449065531));
#269722=CARTESIAN_POINT('Ctrl Pts',(-1.53831346354665,0.230701210213163,
15.278938819604));
#269723=CARTESIAN_POINT('Ctrl Pts',(-1.53635209310862,0.243381974614483,
15.2780277165559));
#269724=CARTESIAN_POINT('Ctrl Pts',(-1.53545275543261,0.24899271842983,
15.2776232742252));
#269725=CARTESIAN_POINT('Ctrl Pts',(-1.53347446136182,0.260916351390305,
15.2767609151204));
#269726=CARTESIAN_POINT('Ctrl Pts',(-1.53238722239672,0.267227738903957,
15.2763027429033));
#269727=CARTESIAN_POINT('Ctrl Pts',(-1.52935693959747,0.284191573321525,
15.2750665532301));
#269728=CARTESIAN_POINT('Ctrl Pts',(-1.52734161963906,0.294830569878293,
15.2742862579238));
#269729=CARTESIAN_POINT('Ctrl Pts',(-1.516561721348,0.348658713670287,15.2703121351901));
#269730=CARTESIAN_POINT('Ctrl Pts',(-1.5060764796557,0.391478314807975,
15.2670641173678));
#269731=CARTESIAN_POINT('Ctrl Pts',(-1.46997649866109,0.515790941422989,
15.2573676720175));
#269732=CARTESIAN_POINT('Ctrl Pts',(-1.43945549096516,0.595680884742685,
15.2507820542005));
#269733=CARTESIAN_POINT('Ctrl Pts',(-1.3637243425151,0.75358673667765,15.2372012571951));
#269734=CARTESIAN_POINT('Ctrl Pts',(-1.31797239318387,0.831017008048588,
15.2302280801331));
#269735=CARTESIAN_POINT('Ctrl Pts',(-1.25864283021201,0.914084116088655,
15.2226674671));
#269736=CARTESIAN_POINT('Ctrl Pts',(-1.25137502440972,0.924008722347184,
15.2217629455501));
#269737=CARTESIAN_POINT('Ctrl Pts',(-1.24105881129791,0.937751094122978,
15.220509937278));
#269738=CARTESIAN_POINT('Ctrl Pts',(-1.23810924729513,0.941641960157849,
15.2201551131706));
#269739=CARTESIAN_POINT('Ctrl Pts',(-1.23332798399747,0.947887774778778,
15.2195855181641));
#269740=CARTESIAN_POINT('Ctrl Pts',(-1.2315077772983,0.950251411234026,
15.2193699602193));
#269741=CARTESIAN_POINT('Ctrl Pts',(-1.22766310470639,0.955214324486042,
15.218917373492));
#269742=CARTESIAN_POINT('Ctrl Pts',(-1.22563716274456,0.957812429464149,
15.2186804557609));
#269743=CARTESIAN_POINT('Ctrl Pts',(-1.22064377818878,0.964174251663145,
15.2181003081391));
#269744=CARTESIAN_POINT('Ctrl Pts',(-1.21766713184873,0.967930771519231,
15.2177577244571));
#269745=CARTESIAN_POINT('Ctrl Pts',(-1.20676503242662,0.981559306768895,
15.2165145200226));
#269746=CARTESIAN_POINT('Ctrl Pts',(-1.19873621960749,0.991348586182511,
15.2156209163984));
#269747=CARTESIAN_POINT('Ctrl Pts',(-1.14499794164625,1.05526234211818,
15.209774072517));
#269748=CARTESIAN_POINT('Ctrl Pts',(-1.09574989498326,1.10631541773307,
15.2050416775706));
#269749=CARTESIAN_POINT('Ctrl Pts',(-0.940501273564758,1.24667580500327,
15.1912054139043));
#269750=CARTESIAN_POINT('Ctrl Pts',(-0.825897460497674,1.3253801349975,
15.1822415339958));
#269751=CARTESIAN_POINT('Ctrl Pts',(-0.687346865705255,1.39549957638931,
15.1714467712168));
#269752=CARTESIAN_POINT('Ctrl Pts',(-0.672174104878261,1.40287088337617,
15.1702662195884));
#269753=CARTESIAN_POINT('Ctrl Pts',(-0.650046934092668,1.41317944399814,
15.1685453510928));
#269754=CARTESIAN_POINT('Ctrl Pts',(-0.643185918573314,1.41631529964121,
15.1680118689332));
#269755=CARTESIAN_POINT('Ctrl Pts',(-0.631054302493441,1.42175377466758,
15.1670686258953));
#269756=CARTESIAN_POINT('Ctrl Pts',(-0.6257931901356,1.42407731883909,15.1666595892612));
#269757=CARTESIAN_POINT('Ctrl Pts',(-0.614886628560528,1.4288220380778,
15.165811610362));
#269758=CARTESIAN_POINT('Ctrl Pts',(-0.609239490368795,1.43123905196035,
15.1653725350727));
#269759=CARTESIAN_POINT('Ctrl Pts',(-0.594694651887369,1.43736266409605,
15.1642415257729));
#269760=CARTESIAN_POINT('Ctrl Pts',(-0.585776663793272,1.44102007255408,
15.1635479439251));
#269761=CARTESIAN_POINT('Ctrl Pts',(-0.547976510140223,1.45611364630161,
15.1606071377234));
#269762=CARTESIAN_POINT('Ctrl Pts',(-0.518791056587234,1.46676541729477,
15.1583339879914));
#269763=CARTESIAN_POINT('Ctrl Pts',(-0.440390766161352,1.49274643600657,
15.1522157299155));
#269764=CARTESIAN_POINT('Ctrl Pts',(-0.390703055321786,1.50651454524288,
15.1483248642517));
#269765=CARTESIAN_POINT('Ctrl Pts',(-0.240313958295305,1.54024561565479,
15.1365307090132));
#269766=CARTESIAN_POINT('Ctrl Pts',(-0.138229735688819,1.55273902845089,
15.1284846707027));
#269767=CARTESIAN_POINT('Ctrl Pts',(-0.0175972229059484,1.55550541326658,
15.1192587878866));
#269768=CARTESIAN_POINT('Ctrl Pts',(0.000473968940785682,1.55560489128815,
15.1178847968187));
#269769=CARTESIAN_POINT('Ctrl Pts',(0.0457456455514533,1.55506515963206,
15.1144687695645));
#269770=CARTESIAN_POINT('Ctrl Pts',(0.072936920072047,1.55402727128559,
15.112440578103));
#269771=CARTESIAN_POINT('Ctrl Pts',(0.106591520627368,1.55185725999964,
15.1099702603373));
#269772=CARTESIAN_POINT('Ctrl Pts',(0.113091430064516,1.55139712522477,
15.1094950090082));
#269773=CARTESIAN_POINT('Ctrl Pts',(0.123288201764571,1.55061086000439,
15.1087525654169));
#269774=CARTESIAN_POINT('Ctrl Pts',(0.126987014839802,1.55031232940424,
15.1084838916767));
#269775=CARTESIAN_POINT('Ctrl Pts',(0.133854425822546,1.54973331924651,
15.1079862955285));
#269776=CARTESIAN_POINT('Ctrl Pts',(0.137023204588303,1.5494563594474,15.1077571883069));
#269777=CARTESIAN_POINT('Ctrl Pts',(0.144238087354764,1.54880345283545,
15.107236649318));
#269778=CARTESIAN_POINT('Ctrl Pts',(0.148283579395924,1.54842137109197,
15.1069455638534));
#269779=CARTESIAN_POINT('Ctrl Pts',(0.160686439678187,1.54720091294515,
15.1060554300551));
#269780=CARTESIAN_POINT('Ctrl Pts',(0.169038738122006,1.5463106771559,15.1054591895492));
#269781=CARTESIAN_POINT('Ctrl Pts',(0.188421523624302,1.54408581985507,
15.1040820738031));
#269782=CARTESIAN_POINT('Ctrl Pts',(0.199445880900395,1.54270056960888,
15.1033037498686));
#269783=CARTESIAN_POINT('Ctrl Pts',(0.350170938178949,1.52211863828171,
15.0927184195491));
#269784=CARTESIAN_POINT('Ctrl Pts',(0.486664105689321,1.48412785667841,
15.0837429924393));
#269785=CARTESIAN_POINT('Ctrl Pts',(0.680184039657533,1.4006386337053,15.0697040846656));
#269786=CARTESIAN_POINT('Ctrl Pts',(0.742249293970187,1.36875960454969,
15.0649845273215));
#269787=CARTESIAN_POINT('Ctrl Pts',(0.811814943939734,1.32690201440155,
15.0593106753447));
#269788=CARTESIAN_POINT('Ctrl Pts',(0.821600919005587,1.32086501068108,
15.0585033318073));
#269789=CARTESIAN_POINT('Ctrl Pts',(0.837435001934042,1.31085286410948,
15.057181441124));
#269790=CARTESIAN_POINT('Ctrl Pts',(0.843524006988558,1.30694294452568,
15.0566692947554));
#269791=CARTESIAN_POINT('Ctrl Pts',(0.854352904769364,1.29988220851742,
15.0557515138373));
#269792=CARTESIAN_POINT('Ctrl Pts',(0.859103237023871,1.29674757314841,
15.0553464876042));
#269793=CARTESIAN_POINT('Ctrl Pts',(0.869118521100297,1.29005953042814,
15.0544873522016));
#269794=CARTESIAN_POINT('Ctrl Pts',(0.874379110490841,1.28649981138507,
15.0540330108076));
#269795=CARTESIAN_POINT('Ctrl Pts',(0.888351451172761,1.27691976536659,
15.0528179277687));
#269796=CARTESIAN_POINT('Ctrl Pts',(0.897023639451311,1.27084262123153,
15.052055041082));
#269797=CARTESIAN_POINT('Ctrl Pts',(0.938998517390703,1.24078450014822,
15.0483190196218));
#269798=CARTESIAN_POINT('Ctrl Pts',(0.971402342309505,1.21558269846498,
15.0452992032494));
#269799=CARTESIAN_POINT('Ctrl Pts',(1.11623973692998,1.09344439369855,15.0311419453224));
#269800=CARTESIAN_POINT('Ctrl Pts',(1.21542313736418,0.982010693103723,
15.0194182120874));
#269801=CARTESIAN_POINT('Ctrl Pts',(1.31831441699774,0.826485654502356,
15.0052151198238));
#269802=CARTESIAN_POINT('Ctrl Pts',(1.33816130453385,0.793949845767243,
15.0023521594732));
#269803=CARTESIAN_POINT('Ctrl Pts',(1.36000973884674,0.754981434198667,
14.99907452962));
#269804=CARTESIAN_POINT('Ctrl Pts',(1.36318800909648,0.749227543326059,
14.9985943387916));
#269805=CARTESIAN_POINT('Ctrl Pts',(1.36827904239983,0.739871167942625,
14.9978197955366));
#269806=CARTESIAN_POINT('Ctrl Pts',(1.3702142346257,0.736281084425017,14.9975240894964));
#269807=CARTESIAN_POINT('Ctrl Pts',(1.37363417527809,0.729876378796892,
14.9969992517469));
#269808=CARTESIAN_POINT('Ctrl Pts',(1.37512442547233,0.727064777702217,
14.9967697781553));
#269809=CARTESIAN_POINT('Ctrl Pts',(1.37832891954686,0.720973876865821,
14.9962746643382));
#269810=CARTESIAN_POINT('Ctrl Pts',(1.38004009172385,0.717693031588492,
14.9960092174557));
#269811=CARTESIAN_POINT('Ctrl Pts',(1.38479199670207,0.708502326980686,
14.9952690000166));
#269812=CARTESIAN_POINT('Ctrl Pts',(1.38780663353652,0.70257894475651,14.9947958299672));
#269813=CARTESIAN_POINT('Ctrl Pts',(1.40546111689658,0.667333062475629,
14.9920022760485));
#269814=CARTESIAN_POINT('Ctrl Pts',(1.4192105620845,0.637570504649129,14.9897329765469));
#269815=CARTESIAN_POINT('Ctrl Pts',(1.43287024456846,0.605365972271906,
14.9873482618096));
#269816=CARTESIAN_POINT('Ctrl Pts',(1.43372565284231,0.603337259749617,
14.9871983329348));
#269817=CARTESIAN_POINT('Ctrl Pts',(1.4345766844093,0.601306898803946,14.987048570644));
#269818=CARTESIAN_POINT('',(-1.55549984403819,0.000696560963701701,15.1547003707517));
#269819=CARTESIAN_POINT('Ctrl Pts',(1.43457662445954,0.601307041829938,
14.8491341039362));
#269820=CARTESIAN_POINT('Ctrl Pts',(1.38448969431034,0.720802630912524,
14.8589338957143));
#269821=CARTESIAN_POINT('Ctrl Pts',(1.31964055215274,0.833634866082474,
14.8691504652631));
#269822=CARTESIAN_POINT('Ctrl Pts',(1.21848667811269,0.967641878853461,
14.8819394954867));
#269823=CARTESIAN_POINT('Ctrl Pts',(1.19434505119975,0.997286863375022,
14.8848118360002));
#269824=CARTESIAN_POINT('Ctrl Pts',(1.16475882936822,1.03100005139464,14.8881029831226));
#269825=CARTESIAN_POINT('Ctrl Pts',(1.16035223328545,1.03595701429165,14.8885875360038));
#269826=CARTESIAN_POINT('Ctrl Pts',(1.15315526016599,1.0439493243621,14.8893696384163));
#269827=CARTESIAN_POINT('Ctrl Pts',(1.15038434562817,1.04700196001743,14.8896685606221));
#269828=CARTESIAN_POINT('Ctrl Pts',(1.14542612551546,1.05242083959573,14.8901994940623));
#269829=CARTESIAN_POINT('Ctrl Pts',(1.14324357754077,1.05479133279857,14.8904318521045));
#269830=CARTESIAN_POINT('Ctrl Pts',(1.13850087716068,1.05991042592819,14.8909338416474));
#269831=CARTESIAN_POINT('Ctrl Pts',(1.1359381333817,1.06265653728012,14.8912032713976));
#269832=CARTESIAN_POINT('Ctrl Pts',(1.12872715883814,1.07032757169798,14.891956388374));
#269833=CARTESIAN_POINT('Ctrl Pts',(1.12405660107506,1.07523154338236,14.892438411234));
#269834=CARTESIAN_POINT('Ctrl Pts',(1.0957488184019,1.10456798008782,14.8953265704348));
#269835=CARTESIAN_POINT('Ctrl Pts',(1.07134569053159,1.12825296314354,14.8976778165618));
#269836=CARTESIAN_POINT('Ctrl Pts',(0.927480651971162,1.25900308988499,
14.9109128215768));
#269837=CARTESIAN_POINT('Ctrl Pts',(0.792802869301842,1.34788057355433,
14.9210388921652));
#269838=CARTESIAN_POINT('Ctrl Pts',(0.615733697305195,1.42885514108345,
14.9343289472299));
#269839=CARTESIAN_POINT('Ctrl Pts',(0.584103290076188,1.44207421660871,
14.9366971743447));
#269840=CARTESIAN_POINT('Ctrl Pts',(0.542289363653755,1.45794780756784,
14.93983381778));
#269841=CARTESIAN_POINT('Ctrl Pts',(0.532477746629139,1.46155978440423,
14.9405702227141));
#269842=CARTESIAN_POINT('Ctrl Pts',(0.51662774534732,1.46721390515693,14.9417608231288));
#269843=CARTESIAN_POINT('Ctrl Pts',(0.510611796395492,1.46931836643203,
14.9422129482956));
#269844=CARTESIAN_POINT('Ctrl Pts',(0.499118294731389,1.47325983954268,
14.9430772514466));
#269845=CARTESIAN_POINT('Ctrl Pts',(0.49364309527527,1.47510342680706,14.9434892042906));
#269846=CARTESIAN_POINT('Ctrl Pts',(0.481094645621458,1.47925100322241,
14.9444339211938));
#269847=CARTESIAN_POINT('Ctrl Pts',(0.474014931033483,1.48153482246555,
14.9449673370929));
#269848=CARTESIAN_POINT('Ctrl Pts',(0.452074583423186,1.48843911734937,
14.9466218710701));
#269849=CARTESIAN_POINT('Ctrl Pts',(0.437161201218259,1.4928872986568,14.9477485626628));
#269850=CARTESIAN_POINT('Ctrl Pts',(0.402548498640975,1.5026480536672,14.9503691628947));
#269851=CARTESIAN_POINT('Ctrl Pts',(0.382806774185083,1.50779818558583,
14.9518680474685));
#269852=CARTESIAN_POINT('Ctrl Pts',(0.313925902983509,1.52432760448762,
14.9571138143134));
#269853=CARTESIAN_POINT('Ctrl Pts',(0.264343080126861,1.53370333366798,
14.960919225385));
#269854=CARTESIAN_POINT('Ctrl Pts',(0.152232272556627,1.54930463864472,
14.9695743258279));
#269855=CARTESIAN_POINT('Ctrl Pts',(0.0896038512857674,1.55418464920886,
14.9744451851052));
#269856=CARTESIAN_POINT('Ctrl Pts',(-0.0208512102421502,1.55609192854191,
14.9830088027057));
#269857=CARTESIAN_POINT('Ctrl Pts',(-0.0685730245939707,1.55472024897298,
14.9866988749557));
#269858=CARTESIAN_POINT('Ctrl Pts',(-0.153498866993543,1.54836057822019,
14.9931821261876));
#269859=CARTESIAN_POINT('Ctrl Pts',(-0.19073015469002,1.54421661622696,
14.9959951332856));
#269860=CARTESIAN_POINT('Ctrl Pts',(-0.234303190953112,1.53776648477042,
14.9992268080692));
#269861=CARTESIAN_POINT('Ctrl Pts',(-0.240821267417033,1.53675920958705,
14.9997086234692));
#269862=CARTESIAN_POINT('Ctrl Pts',(-0.251392046586988,1.53505673935006,
15.0004871885796));
#269863=CARTESIAN_POINT('Ctrl Pts',(-0.255448655956028,1.53438689362732,
15.0007852912315));
#269864=CARTESIAN_POINT('Ctrl Pts',(-0.262678785810304,1.53316355366678,
15.0013153373323));
#269865=CARTESIAN_POINT('Ctrl Pts',(-0.265853279859228,1.53261627979498,
15.0015476228913));
#269866=CARTESIAN_POINT('Ctrl Pts',(-0.272733504773122,1.53140812772971,
15.0020501064023));
#269867=CARTESIAN_POINT('Ctrl Pts',(-0.27643853982599,1.53074366006012,
15.0023200990262));
#269868=CARTESIAN_POINT('Ctrl Pts',(-0.286838659520395,1.52883949233657,
15.0030763901819));
#269869=CARTESIAN_POINT('Ctrl Pts',(-0.293528179994305,1.52756925277144,
15.0035610017138));
#269870=CARTESIAN_POINT('Ctrl Pts',(-0.334232320751749,1.51956288351313,
15.006499692045));
#269871=CARTESIAN_POINT('Ctrl Pts',(-0.368025405070559,1.51173422558794,
15.0088966216291));
#269872=CARTESIAN_POINT('Ctrl Pts',(-0.48261977840887,1.48111549350689,
15.0169662237786));
#269873=CARTESIAN_POINT('Ctrl Pts',(-0.561828097148201,1.4529199965584,
15.0224485455255));
#269874=CARTESIAN_POINT('Ctrl Pts',(-0.733949938914209,1.37545679150609,
15.034881696169));
#269875=CARTESIAN_POINT('Ctrl Pts',(-0.824913647769721,1.32290459063556,
15.0418393207345));
#269876=CARTESIAN_POINT('Ctrl Pts',(-0.919583364846484,1.25462716070336,
15.049991123783));
#269877=CARTESIAN_POINT('Ctrl Pts',(-0.929188635688008,1.24753009689229,
15.0508292545906));
#269878=CARTESIAN_POINT('Ctrl Pts',(-0.944625733258137,1.23584687422173,
15.0521948741498));
#269879=CARTESIAN_POINT('Ctrl Pts',(-0.950508272640006,1.23132826356852,
15.0527197326911));
#269880=CARTESIAN_POINT('Ctrl Pts',(-0.960746214092261,1.22334701491011,
15.0536411845617));
#269881=CARTESIAN_POINT('Ctrl Pts',(-0.965115812586305,1.21990273120727,
15.0540370474519));
#269882=CARTESIAN_POINT('Ctrl Pts',(-0.974240211873082,1.21263082502837,
15.0548691684647));
#269883=CARTESIAN_POINT('Ctrl Pts',(-0.978991139004057,1.20879851755018,
15.055305609471));
#269884=CARTESIAN_POINT('Ctrl Pts',(-0.991250914205855,1.19878955956145,
15.0564401869939));
#269885=CARTESIAN_POINT('Ctrl Pts',(-0.998724523954861,1.19257037541106,
15.0571400328213));
#269886=CARTESIAN_POINT('Ctrl Pts',(-1.0149204122241,1.17883390937404,15.0586749524786));
#269887=CARTESIAN_POINT('Ctrl Pts',(-1.02361844768952,1.17128907164764,
15.0595111295317));
#269888=CARTESIAN_POINT('Ctrl Pts',(-1.04884775792436,1.1489090377648,15.0619719599693));
#269889=CARTESIAN_POINT('Ctrl Pts',(-1.06514537533249,1.13381604911318,
15.0636071132973));
#269890=CARTESIAN_POINT('Ctrl Pts',(-1.18729733638274,1.01573441430448,
15.0762212365456));
#269891=CARTESIAN_POINT('Ctrl Pts',(-1.27831057499782,0.898497496166772,
15.0878392077257));
#269892=CARTESIAN_POINT('Ctrl Pts',(-1.35603553146169,0.762125324186883,
15.0998637405688));
#269893=CARTESIAN_POINT('Ctrl Pts',(-1.36058439655371,0.753974454513514,
15.1005769159044));
#269894=CARTESIAN_POINT('Ctrl Pts',(-1.38331157793251,0.712375277228548,
15.1041872379123));
#269895=CARTESIAN_POINT('Ctrl Pts',(-1.40033284258663,0.678305226233278,
15.1070483184058));
#269896=CARTESIAN_POINT('Ctrl Pts',(-1.41882961088583,0.637610130828309,
15.1103281838581));
#269897=CARTESIAN_POINT('Ctrl Pts',(-1.42153253067859,0.631561091308568,
15.1108122184314));
#269898=CARTESIAN_POINT('Ctrl Pts',(-1.42585370940418,0.621722146847599,
15.1115936512264));
#269899=CARTESIAN_POINT('Ctrl Pts',(-1.42749566525312,0.6179428414073,15.111892418377));
#269900=CARTESIAN_POINT('Ctrl Pts',(-1.43039476312056,0.611196738492991,
15.1124231837184));
#269901=CARTESIAN_POINT('Ctrl Pts',(-1.4316577206618,0.608232523860307,
15.1126555278285));
#269902=CARTESIAN_POINT('Ctrl Pts',(-1.43437362509822,0.601802852413072,
15.1131576098349));
#269903=CARTESIAN_POINT('Ctrl Pts',(-1.43582322681121,0.598336052489105,
15.1134271453076));
#269904=CARTESIAN_POINT('Ctrl Pts',(-1.43985270173415,0.588600374451776,
15.1141808581556));
#269905=CARTESIAN_POINT('Ctrl Pts',(-1.44240422124614,0.582319732200108,
15.1146633669266));
#269906=CARTESIAN_POINT('Ctrl Pts',(-1.45755016023219,0.544327134834577,
15.1175609154676));
#269907=CARTESIAN_POINT('Ctrl Pts',(-1.46914057516394,0.512221549746112,
15.1199206489215));
#269908=CARTESIAN_POINT('Ctrl Pts',(-1.52983774872017,0.325019611299663,
15.1333167815798));
#269909=CARTESIAN_POINT('Ctrl Pts',(-1.55542699587216,0.163374799902079,
15.1435769870656));
#269910=CARTESIAN_POINT('Ctrl Pts',(-1.55549984403819,0.000696560963701701,
15.1547003707517));
#269911=CARTESIAN_POINT('Ctrl Pts',(-1.55549984481413,0.000694826046350984,
15.1547004893794));
#269912=CARTESIAN_POINT('Ctrl Pts',(-1.5555125263787,-0.0276952606902724,
15.1566417076067));
#269913=CARTESIAN_POINT('Ctrl Pts',(-1.55474797027491,-0.0560791253254835,
15.1586030095658));
#269914=CARTESIAN_POINT('Ctrl Pts',(-1.55272661854127,-0.0932668495106141,
15.1612072810071));
#269915=CARTESIAN_POINT('Ctrl Pts',(-1.55217054284928,-0.102104149637935,
15.1618287195237));
#269916=CARTESIAN_POINT('Ctrl Pts',(-1.55109545149386,-0.117140254106849,
15.1628906597484));
#269917=CARTESIAN_POINT('Ctrl Pts',(-1.55061464422912,-0.123341646914341,
15.1633299738422));
#269918=CARTESIAN_POINT('Ctrl Pts',(-1.54964882427644,-0.134898813301272,
15.1641512696402));
#269919=CARTESIAN_POINT('Ctrl Pts',(-1.54917320490023,-0.140255296904652,
15.1645329532254));
#269920=CARTESIAN_POINT('Ctrl Pts',(-1.5481508749264,-0.151128594537193,
15.1653098945114));
#269921=CARTESIAN_POINT('Ctrl Pts',(-1.54760242799074,-0.15664516282932,
15.1657052011876));
#269922=CARTESIAN_POINT('Ctrl Pts',(-1.54625519666379,-0.169498009803029,
15.1666288974961));
#269923=CARTESIAN_POINT('Ctrl Pts',(-1.54543367674206,-0.176831716199418,
15.167157992624));
#269924=CARTESIAN_POINT('Ctrl Pts',(-1.54316113496428,-0.195891733163291,
15.168538550544));
#269925=CARTESIAN_POINT('Ctrl Pts',(-1.54162865432939,-0.207607652601354,
15.1693925489004));
#269926=CARTESIAN_POINT('Ctrl Pts',(-1.53448962018521,-0.257738126566052,
15.1730705592355));
#269927=CARTESIAN_POINT('Ctrl Pts',(-1.52757997202731,-0.295949785225794,
15.1759348782609));
#269928=CARTESIAN_POINT('Ctrl Pts',(-1.50111487761445,-0.416380676512976,
15.1851631176065));
#269929=CARTESIAN_POINT('Ctrl Pts',(-1.47628969611336,-0.497276726124052,
15.1916730715154));
#269930=CARTESIAN_POINT('Ctrl Pts',(-1.40972685877153,-0.66433771623309,
15.2056158623732));
#269931=CARTESIAN_POINT('Ctrl Pts',(-1.36635336422968,-0.749504521562905,
15.2130316495414));
#269932=CARTESIAN_POINT('Ctrl Pts',(-1.31014347492284,-0.838572033497492,
15.2207985692926));
#269933=CARTESIAN_POINT('Ctrl Pts',(-1.30475989519401,-0.846924205501031,
15.2215268778759));
#269934=CARTESIAN_POINT('Ctrl Pts',(-1.29688681294401,-0.858885354798602,
15.2225692238688));
#269935=CARTESIAN_POINT('Ctrl Pts',(-1.29446165980958,-0.862536069290741,
15.2228872723498));
#269936=CARTESIAN_POINT('Ctrl Pts',(-1.29020977881723,-0.868878332722819,
15.2234395825227));
#269937=CARTESIAN_POINT('Ctrl Pts',(-1.28838999463197,-0.871574467851273,
15.2236742999759));
#269938=CARTESIAN_POINT('Ctrl Pts',(-1.28453639272768,-0.877245399413548,
15.2241678190269));
#269939=CARTESIAN_POINT('Ctrl Pts',(-1.28250068969525,-0.880218845902813,
15.2244264906434));
#269940=CARTESIAN_POINT('Ctrl Pts',(-1.27700388052335,-0.888188198847021,
15.2251195965164));
#269941=CARTESIAN_POINT('Ctrl Pts',(-1.2735237492052,-0.893171008775414,
15.2255527685777));
#269942=CARTESIAN_POINT('Ctrl Pts',(-1.25783899046606,-0.915350197077298,
15.2274806577308));
#269943=CARTESIAN_POINT('Ctrl Pts',(-1.2453139168844,-0.932318761945474,
15.2289550292966));
#269944=CARTESIAN_POINT('Ctrl Pts',(-1.13170546163315,-1.07985530960747,
15.2418208956206));
#269945=CARTESIAN_POINT('Ctrl Pts',(-1.01076733014357,-1.19382155551633,
15.2521922598749));
#269946=CARTESIAN_POINT('Ctrl Pts',(-0.85066970897933,-1.30259240762529,
15.26531550409));
#269947=CARTESIAN_POINT('Ctrl Pts',(-0.82676027028175,-1.31789727644882,
15.2672583379683));
#269948=CARTESIAN_POINT('Ctrl Pts',(-0.790710977032655,-1.33960593890161,
15.2701726471617));
#269949=CARTESIAN_POINT('Ctrl Pts',(-0.77888278058075,-1.34651755079651,
15.2711265250598));
#269950=CARTESIAN_POINT('Ctrl Pts',(-0.757194135280786,-1.35880956373169,
15.2728724540265));
#269951=CARTESIAN_POINT('Ctrl Pts',(-0.747363663911357,-1.36424115579042,
15.2736626513386));
#269952=CARTESIAN_POINT('Ctrl Pts',(-0.731770183702935,-1.37263783879527,
15.2749147297762));
#269953=CARTESIAN_POINT('Ctrl Pts',(-0.726045845280711,-1.37567425886233,
15.275374078512));
#269954=CARTESIAN_POINT('Ctrl Pts',(-0.720239872991005,-1.37870764863017,
15.275839736497));
#269955=CARTESIAN_POINT('Ctrl Pts',(-0.720176964191238,-1.37874051049707,
15.2758447819601));
#269956=CARTESIAN_POINT('Ctrl Pts',(-0.720044566835006,-1.37880965978515,
15.2758554005412));
#269957=CARTESIAN_POINT('Ctrl Pts',(-0.719975077788481,-1.37884594625683,
15.2758609736923));
#269958=CARTESIAN_POINT('Ctrl Pts',(-0.719828835990497,-1.3789222981636,
15.2758727024839));
#269959=CARTESIAN_POINT('Ctrl Pts',(-0.719752082636228,-1.37896236244396,
15.2758788581652));
#269960=CARTESIAN_POINT('Ctrl Pts',(-0.719590559099501,-1.37904665852802,
15.275891812395));
#269961=CARTESIAN_POINT('Ctrl Pts',(-0.719505788184481,-1.37909088892337,
15.2758986109929));
#269962=CARTESIAN_POINT('Ctrl Pts',(-0.719327401019969,-1.37918394396459,
15.2759129174733));
#269963=CARTESIAN_POINT('Ctrl Pts',(-0.719233783880984,-1.37923276689328,
15.2759204254159));
#269964=CARTESIAN_POINT('Ctrl Pts',(-0.719036792794181,-1.37933547558167,
15.2759362236498));
#269965=CARTESIAN_POINT('Ctrl Pts',(-0.71893341776129,-1.37938935925073,
15.2759445140145));
#269966=CARTESIAN_POINT('Ctrl Pts',(-0.718715918409621,-1.37950269850554,
15.2759619566442));
#269967=CARTESIAN_POINT('Ctrl Pts',(-0.718601789401949,-1.37956215330405,
15.2759711092687));
#269968=CARTESIAN_POINT('Ctrl Pts',(-0.718392146452066,-1.37967133242328,
15.2759879215053));
#269969=CARTESIAN_POINT('Ctrl Pts',(-0.718296636739827,-1.37972105994079,
15.2759955808057));
#269970=CARTESIAN_POINT('Ctrl Pts',(-0.718046176039664,-1.37985143025878,
15.2760156660685));
#269971=CARTESIAN_POINT('Ctrl Pts',(-0.717891219256346,-1.37993205551082,
15.2760280923907));
#269972=CARTESIAN_POINT('Ctrl Pts',(-0.712795492074503,-1.38258231245329,
15.2764367243206));
#269973=CARTESIAN_POINT('Ctrl Pts',(-0.707841029936725,-1.3851253874963,
15.2768338571734));
#269974=CARTESIAN_POINT('Ctrl Pts',(-0.696247099781216,-1.39099798482353,
15.2777628515641));
#269975=CARTESIAN_POINT('Ctrl Pts',(-0.689597277286889,-1.39430664107737,
15.2782954313772));
#269976=CARTESIAN_POINT('Ctrl Pts',(-0.67216463462957,-1.40282513638577,
15.2796910817107));
#269977=CARTESIAN_POINT('Ctrl Pts',(-0.661345081613867,-1.40795821224977,
15.2805567797875));
#269978=CARTESIAN_POINT('Ctrl Pts',(-0.556443296402479,-1.45625040579505,
15.2889471079586));
#269979=CARTESIAN_POINT('Ctrl Pts',(-0.458353207163089,-1.49003305843016,
15.2967954051994));
#269980=CARTESIAN_POINT('Ctrl Pts',(-0.274985716201144,-1.53335546002276,
15.3113583425522));
#269981=CARTESIAN_POINT('Ctrl Pts',(-0.190852682925785,-1.54608286829337,
15.3179933058857));
#269982=CARTESIAN_POINT('Ctrl Pts',(-0.0712949703106406,-1.55425682309582,
15.3270936693173));
#269983=CARTESIAN_POINT('Ctrl Pts',(-0.0364170491154879,-1.55546504859568,
15.3297080553145));
#269984=CARTESIAN_POINT('Ctrl Pts',(0.00529519210871108,-1.55550593812472,
15.3327649713313));
#269985=CARTESIAN_POINT('Ctrl Pts',(0.0121153435057373,-1.5554677706894,
15.3332625568429));
#269986=CARTESIAN_POINT('Ctrl Pts',(0.0227014169890424,-1.5553388962645,
15.3340312054375));
#269987=CARTESIAN_POINT('Ctrl Pts',(0.0264675192671187,-1.55527936648302,
15.3343039345515));
#269988=CARTESIAN_POINT('Ctrl Pts',(0.0334538907940433,-1.55514355045724,
15.3348084742616));
#269989=CARTESIAN_POINT('Ctrl Pts',(0.0366741134858062,-1.55507094214065,
15.3350404776992));
#269990=CARTESIAN_POINT('Ctrl Pts',(0.0440009473277864,-1.55488296769438,
15.3355671054639));
#269991=CARTESIAN_POINT('Ctrl Pts',(0.048107339048445,-1.55476133588665,
15.3358613780457));
#269992=CARTESIAN_POINT('Ctrl Pts',(0.0587936721339433,-1.5544024268926,
15.3366250036344));
#269993=CARTESIAN_POINT('Ctrl Pts',(0.0653727646067616,-1.55413963540062,
15.3370929824602));
#269994=CARTESIAN_POINT('Ctrl Pts',(0.109126931100659,-1.55211360405198,
15.340192151669));
#269995=CARTESIAN_POINT('Ctrl Pts',(0.146233800687356,-1.5490582827536,
15.3427575391598));
#269996=CARTESIAN_POINT('Ctrl Pts',(0.230623835750005,-1.53904959577818,
15.3485210706069));
#269997=CARTESIAN_POINT('Ctrl Pts',(0.277767677739557,-1.53124351483212,
15.3516899932918));
#269998=CARTESIAN_POINT('Ctrl Pts',(0.385565986350445,-1.50825075848853,
15.3589639980438));
#269999=CARTESIAN_POINT('Ctrl Pts',(0.445810583517784,-1.49155431539201,
15.3630516468424));
#270000=CARTESIAN_POINT('Ctrl Pts',(0.570453894172218,-1.44878147799923,
15.371805766872));
#270001=CARTESIAN_POINT('Ctrl Pts',(0.634434822829089,-1.4219268594508,
15.376477754972));
#270002=CARTESIAN_POINT('Ctrl Pts',(0.71152724343633,-1.38332757430809,
15.3824708352682));
#270003=CARTESIAN_POINT('Ctrl Pts',(0.726522788193741,-1.37551110325834,
15.3836542615365));
#270004=CARTESIAN_POINT('Ctrl Pts',(0.748148751208125,-1.36378621835699,
15.3853884098071));
#270005=CARTESIAN_POINT('Ctrl Pts',(0.754882680674469,-1.36007041652513,
15.3859323281794));
#270006=CARTESIAN_POINT('Ctrl Pts',(0.766656568833255,-1.35345917454319,
15.3868904214634));
#270007=CARTESIAN_POINT('Ctrl Pts',(0.771708415055184,-1.35058511473642,
15.38730382605));
#270008=CARTESIAN_POINT('Ctrl Pts',(0.781503614782134,-1.34493960074805,
15.3881099668274));
#270009=CARTESIAN_POINT('Ctrl Pts',(0.786248633459315,-1.34217119419752,
15.3885025884737));
#270010=CARTESIAN_POINT('Ctrl Pts',(0.798916838421896,-1.33468989773695,
15.3895565351928));
#270011=CARTESIAN_POINT('Ctrl Pts',(0.80681285082437,-1.3299316729776,15.3902194980925));
#270012=CARTESIAN_POINT('Ctrl Pts',(0.835726756589508,-1.3121555732434,
15.3926698929321));
#270013=CARTESIAN_POINT('Ctrl Pts',(0.856474693350269,-1.29870798471957,
15.3944729657176));
#270014=CARTESIAN_POINT('Ctrl Pts',(0.881379653929259,-1.28170966765153,
15.396694085811));
#270015=CARTESIAN_POINT('Ctrl Pts',(0.885850862663507,-1.27862348417631,
15.397095126387));
#270016=CARTESIAN_POINT('Ctrl Pts',(0.894739849751391,-1.27241899204902,
15.3978969935394));
#270017=CARTESIAN_POINT('Ctrl Pts',(0.899157719173715,-1.26930094335778,
15.3982978068634));
#270018=CARTESIAN_POINT('Ctrl Pts',(1.03517479679167,-1.1722362083094,15.4107088706492));
#270019=CARTESIAN_POINT('Ctrl Pts',(1.15130595135913,-1.05839497997946,
15.4235134913719));
#270020=CARTESIAN_POINT('Ctrl Pts',(1.26810612266311,-0.901466873722713,
15.4383581420086));
#270021=CARTESIAN_POINT('Ctrl Pts',(1.28750393421204,-0.873538621993595,
15.4409038897354));
#270022=CARTESIAN_POINT('Ctrl Pts',(1.30965124679445,-0.839309072424249,
15.4438913958631));
#270023=CARTESIAN_POINT('Ctrl Pts',(1.31329281778026,-0.833599476102055,
15.4443854221251));
#270024=CARTESIAN_POINT('Ctrl Pts',(1.31889611845211,-0.824686235311817,
15.4451497716214));
#270025=CARTESIAN_POINT('Ctrl Pts',(1.32088366779136,-0.821499053531846,
15.4454217318491));
#270026=CARTESIAN_POINT('Ctrl Pts',(1.32455481675404,-0.815564326289604,
15.4459255824182));
#270027=CARTESIAN_POINT('Ctrl Pts',(1.32624140965404,-0.812818772275222,
15.4461576608905));
#270028=CARTESIAN_POINT('Ctrl Pts',(1.33006649676801,-0.806548424171424,
15.4466853969884));
#270029=CARTESIAN_POINT('Ctrl Pts',(1.33219951637633,-0.803020358385821,
15.4469806968542));
#270030=CARTESIAN_POINT('Ctrl Pts',(1.3377274009304,-0.793794456961812,
15.4477487654474));
#270031=CARTESIAN_POINT('Ctrl Pts',(1.34109994250851,-0.788083236376625,
15.4482201336208));
#270032=CARTESIAN_POINT('Ctrl Pts',(1.36365813520844,-0.749317944644559,
15.4513932065983));
#270033=CARTESIAN_POINT('Ctrl Pts',(1.38165842701888,-0.715584715891151,
15.4540254786558));
#270034=CARTESIAN_POINT('Ctrl Pts',(1.46393663406337,-0.546684918543369,
15.4667550113932));
#270035=CARTESIAN_POINT('Ctrl Pts',(1.50971968806793,-0.403395233726827,
15.4762533022922));
#270036=CARTESIAN_POINT('Ctrl Pts',(1.5408337241483,-0.216741045405577,
15.4891191015357));
#270037=CARTESIAN_POINT('Ctrl Pts',(1.54584687883676,-0.177488650248184,
15.4918455413033));
#270038=CARTESIAN_POINT('Ctrl Pts',(1.55029494254361,-0.127581929092454,
15.4953588806552));
#270039=CARTESIAN_POINT('Ctrl Pts',(1.55112458913943,-0.117064327345026,
15.4961018856068));
#270040=CARTESIAN_POINT('Ctrl Pts',(1.55228512741467,-0.100159977558526,
15.4973005919637));
#270041=CARTESIAN_POINT('Ctrl Pts',(1.5526837436891,-0.0937780772025266,
15.4977541712973));
#270042=CARTESIAN_POINT('Ctrl Pts',(1.55336731394945,-0.0816306280322024,
15.4986195714066));
#270043=CARTESIAN_POINT('Ctrl Pts',(1.55365954550481,-0.0758655817320582,
15.499031157336));
#270044=CARTESIAN_POINT('Ctrl Pts',(1.55425314618952,-0.0627069589700235,
15.4999726625137));
#270045=CARTESIAN_POINT('Ctrl Pts',(1.55453385730008,-0.0553126400381016,
15.5005032177799));
#270046=CARTESIAN_POINT('Ctrl Pts',(1.55512783124167,-0.0360398672224341,
15.5018900934238));
#270047=CARTESIAN_POINT('Ctrl Pts',(1.55535775502189,-0.0241595294448888,
15.5027489876862));
#270048=CARTESIAN_POINT('Ctrl Pts',(1.55629621137896,0.0947295848169169,
15.5113857622986));
#270049=CARTESIAN_POINT('Ctrl Pts',(1.54609636708754,0.201515767774227,
15.5195113411043));
#270050=CARTESIAN_POINT('Ctrl Pts',(1.50882657284367,0.387023167389231,
15.5341474368718));
#270051=CARTESIAN_POINT('Ctrl Pts',(1.48625653958619,0.466247815391386,
15.5405661445793));
#270052=CARTESIAN_POINT('Ctrl Pts',(1.45026520959079,0.562799534624391,
15.5483874352204));
#270053=CARTESIAN_POINT('Ctrl Pts',(1.44261352366488,0.582132892741886,
15.5499529745773));
#270054=CARTESIAN_POINT('Ctrl Pts',(1.43457668274383,0.601306902777371,
15.5515012983457));
#270055=CARTESIAN_POINT('Origin',(0.,0.,-1.29405622560371));
#270056=CARTESIAN_POINT('',(1.43457668357428,0.601306900796103,16.3897484311226));
#270057=CARTESIAN_POINT('',(1.43457653793677,0.601307248252799,16.2500928067243));
#270058=CARTESIAN_POINT('',(1.43457668357355,0.601306900797845,-1.29405622560371));
#270059=CARTESIAN_POINT('',(-1.555499922686,-0.000490432305788335,15.9926617964138));
#270060=CARTESIAN_POINT('Ctrl Pts',(1.43457668357428,0.601306900796103,
16.3897484311226));
#270061=CARTESIAN_POINT('Ctrl Pts',(1.43622124916671,0.597383354516543,
16.3894460676227));
#270062=CARTESIAN_POINT('Ctrl Pts',(1.43784969886007,0.593453108296744,
16.3891431618272));
#270063=CARTESIAN_POINT('Ctrl Pts',(1.44185258584415,0.583678986602261,
16.3883897712346));
#270064=CARTESIAN_POINT('Ctrl Pts',(1.44420761711323,0.577827305700601,
16.3879386389247));
#270065=CARTESIAN_POINT('Ctrl Pts',(1.4503473683068,0.562299486109962,16.3867412122664));
#270066=CARTESIAN_POINT('Ctrl Pts',(1.45407078622349,0.552599619749088,
16.3859928814586));
#270067=CARTESIAN_POINT('Ctrl Pts',(1.47119863463307,0.506607924974705,
16.3824425147161));
#270068=CARTESIAN_POINT('Ctrl Pts',(1.48334209387819,0.469864612056201,
16.3795992326525));
#270069=CARTESIAN_POINT('Ctrl Pts',(1.53579686969054,0.28874363162374,16.3655365191552));
#270070=CARTESIAN_POINT('Ctrl Pts',(1.55645950951083,0.139514110338311,
16.3537026292281));
#270071=CARTESIAN_POINT('Ctrl Pts',(1.55520547888475,-0.0495653299290125,
16.3392885804976));
#270072=CARTESIAN_POINT('Ctrl Pts',(1.55345967028794,-0.0887947076208234,
16.3363363303646));
#270073=CARTESIAN_POINT('Ctrl Pts',(1.54968469411606,-0.134542785712773,
16.3329680120167));
#270074=CARTESIAN_POINT('Ctrl Pts',(1.54909573938789,-0.141162341969934,
16.3324824692211));
#270075=CARTESIAN_POINT('Ctrl Pts',(1.54807484319533,-0.151859607825807,
16.3317010162551));
#270076=CARTESIAN_POINT('Ctrl Pts',(1.54766917921796,-0.155939646554834,
16.3314037137795));
#270077=CARTESIAN_POINT('Ctrl Pts',(1.54691983009985,-0.163185254925248,
16.3308771347085));
#270078=CARTESIAN_POINT('Ctrl Pts',(1.54658255368569,-0.16635141574489,
16.3306475072039));
#270079=CARTESIAN_POINT('Ctrl Pts',(1.54583392657445,-0.173179972737344,
16.3301532974776));
#270080=CARTESIAN_POINT('Ctrl Pts',(1.54541928246134,-0.176841945440848,
16.3298889019365));
#270081=CARTESIAN_POINT('Ctrl Pts',(1.54422833614253,-0.187035723799553,
16.3291545920577));
#270082=CARTESIAN_POINT('Ctrl Pts',(1.54342359950181,-0.193564234129192,
16.3286862372278));
#270083=CARTESIAN_POINT('Ctrl Pts',(1.53851317896824,-0.231421173267933,
16.3259805360574));
#270084=CARTESIAN_POINT('Ctrl Pts',(1.53349477728767,-0.262626524767828,
16.3237906006973));
#270085=CARTESIAN_POINT('Ctrl Pts',(1.49999444498925,-0.436884888645756,
16.3116784456318));
#270086=CARTESIAN_POINT('Ctrl Pts',(1.45245317451607,-0.575534479184962,
16.3024225177903));
#270087=CARTESIAN_POINT('Ctrl Pts',(1.36393426180833,-0.749461223127075,
16.2892596207072));
#270088=CARTESIAN_POINT('Ctrl Pts',(1.33950949241042,-0.79228927050142,
16.2858845049917));
#270089=CARTESIAN_POINT('Ctrl Pts',(1.30690068846105,-0.843637583639098,
16.2816269434337));
#270090=CARTESIAN_POINT('Ctrl Pts',(1.30059752645406,-0.853322824885235,
16.2808142771389));
#270091=CARTESIAN_POINT('Ctrl Pts',(1.29050769501656,-0.868455024471865,
16.2795288497129));
#270092=CARTESIAN_POINT('Ctrl Pts',(1.28679299744938,-0.873949666554983,
16.2790587851867));
#270093=CARTESIAN_POINT('Ctrl Pts',(1.27987300396394,-0.884045693874743,
16.2781888385319));
#270094=CARTESIAN_POINT('Ctrl Pts',(1.27667773322361,-0.888653846620655,
16.2777893409963));
#270095=CARTESIAN_POINT('Ctrl Pts',(1.26954167458808,-0.898827396873072,
16.2769019019813));
#270096=CARTESIAN_POINT('Ctrl Pts',(1.26558908437035,-0.904384331834199,
16.2764135147403));
#270097=CARTESIAN_POINT('Ctrl Pts',(1.25414152922805,-0.92025640440821,
16.2750078858892));
#270098=CARTESIAN_POINT('Ctrl Pts',(1.24655626077617,-0.930505398104111,
16.2740871759472));
#270099=CARTESIAN_POINT('Ctrl Pts',(1.18640577760831,-1.00972340706203,
16.2668660946348));
#270100=CARTESIAN_POINT('Ctrl Pts',(1.12829217320694,-1.07426801437701,
16.2603434412624));
#270101=CARTESIAN_POINT('Ctrl Pts',(1.00108949750904,-1.19378314426523,
16.2469295933528));
#270102=CARTESIAN_POINT('Ctrl Pts',(0.932084566585866,-1.24840548094538,
16.2400591007981));
#270103=CARTESIAN_POINT('Ctrl Pts',(0.848937209399679,-1.30346726204182,
16.2324127972949));
#270104=CARTESIAN_POINT('Ctrl Pts',(0.838960542287971,-1.30991087834649,
16.2315051394349));
#270105=CARTESIAN_POINT('Ctrl Pts',(0.797454687077481,-1.33604947061021,
16.2277718414017));
#270106=CARTESIAN_POINT('Ctrl Pts',(0.765295191208394,-1.35472727669639,
16.2249798438761));
#270107=CARTESIAN_POINT('Ctrl Pts',(0.726734595774218,-1.37531076566749,
16.2217733536623));
#270108=CARTESIAN_POINT('Ctrl Pts',(0.720955586806194,-1.37834898364336,
16.2212964412069));
#270109=CARTESIAN_POINT('Ctrl Pts',(0.711547574183233,-1.38321973093594,
16.2205261336903));
#270110=CARTESIAN_POINT('Ctrl Pts',(0.707930294861838,-1.38507453698824,
16.2202314084864));
#270111=CARTESIAN_POINT('Ctrl Pts',(0.70146949582348,-1.38835547145709,
16.2197076353591));
#270112=CARTESIAN_POINT('Ctrl Pts',(0.698628840221144,-1.38978707469345,
16.2194782511067));
#270113=CARTESIAN_POINT('Ctrl Pts',(0.69246590248059,-1.3928693353179,16.2189825580635));
#270114=CARTESIAN_POINT('Ctrl Pts',(0.689142105309287,-1.39451682343256,
16.2187164467997));
#270115=CARTESIAN_POINT('Ctrl Pts',(0.67980815278537,-1.39910181017468,
16.2179724888132));
#270116=CARTESIAN_POINT('Ctrl Pts',(0.673784798076448,-1.40201249995334,
16.2174962688064));
#270117=CARTESIAN_POINT('Ctrl Pts',(0.637442093168647,-1.41928621852338,
16.214644996229));
#270118=CARTESIAN_POINT('Ctrl Pts',(0.606680555216482,-1.43270545586184,
16.2123235206432));
#270119=CARTESIAN_POINT('Ctrl Pts',(0.414697011581696,-1.50916117926978,
16.1982478450922));
#270120=CARTESIAN_POINT('Ctrl Pts',(0.244324212070338,-1.54591657966354,
16.1873755292736));
#270121=CARTESIAN_POINT('Ctrl Pts',(0.0464991820170724,-1.5550043521393,
16.1737368210692));
#270122=CARTESIAN_POINT('Ctrl Pts',(0.0215938335854684,-1.55554951540799,
16.1720049393561));
#270123=CARTESIAN_POINT('Ctrl Pts',(-0.0124914097454679,-1.55547692482545,
16.1696094418835));
#270124=CARTESIAN_POINT('Ctrl Pts',(-0.0216695802801524,-1.55537613515637,
16.168961907389));
#270125=CARTESIAN_POINT('Ctrl Pts',(-0.0362840079143223,-1.55508626857893,
16.1679266279421));
#270126=CARTESIAN_POINT('Ctrl Pts',(-0.0417212009102184,-1.55494989371981,
16.1675405319428));
#270127=CARTESIAN_POINT('Ctrl Pts',(-0.0528862023635586,-1.5546112529404,
16.1667457420892));
#270128=CARTESIAN_POINT('Ctrl Pts',(-0.0586138245277649,-1.55440584022524,
16.1663369559689));
#270129=CARTESIAN_POINT('Ctrl Pts',(-0.0718781794081574,-1.55385671707094,
16.1653877418562));
#270130=CARTESIAN_POINT('Ctrl Pts',(-0.0794137522707384,-1.55348982040239,
16.1648465978156));
#270131=CARTESIAN_POINT('Ctrl Pts',(-0.103342343882475,-1.55215021337,16.1631220543335));
#270132=CARTESIAN_POINT('Ctrl Pts',(-0.119722277857939,-1.55097274722946,
16.1619323031679));
#270133=CARTESIAN_POINT('Ctrl Pts',(-0.20195809291009,-1.54375081592702,
16.1559103961131));
#270134=CARTESIAN_POINT('Ctrl Pts',(-0.267390634171013,-1.53377105005858,
16.1509572296355));
#270135=CARTESIAN_POINT('Ctrl Pts',(-0.395241876496527,-1.50584093383744,
16.1409670568313));
#270136=CARTESIAN_POINT('Ctrl Pts',(-0.457573954285048,-1.48808542459818,
16.1359437441298));
#270137=CARTESIAN_POINT('Ctrl Pts',(-0.599424521885813,-1.43792123016951,
16.1242776453891));
#270138=CARTESIAN_POINT('Ctrl Pts',(-0.6777453710834,-1.40270892192832,
16.1176534644634));
#270139=CARTESIAN_POINT('Ctrl Pts',(-0.759654392830792,-1.35741197616246,
16.1107768516612));
#270140=CARTESIAN_POINT('Ctrl Pts',(-0.766506144926125,-1.35355472971061,
16.1102020962037));
#270141=CARTESIAN_POINT('Ctrl Pts',(-0.776806897008622,-1.34765253902365,
16.1093390788116));
#270142=CARTESIAN_POINT('Ctrl Pts',(-0.780277584656725,-1.34564602070483,
16.1090484803062));
#270143=CARTESIAN_POINT('Ctrl Pts',(-0.786384154429284,-1.34208404292978,
16.1085375554856));
#270144=CARTESIAN_POINT('Ctrl Pts',(-0.789023229894871,-1.34053420691248,
16.1083168761084));
#270145=CARTESIAN_POINT('Ctrl Pts',(-0.794773538276345,-1.3371343890138,
16.1078363187212));
#270146=CARTESIAN_POINT('Ctrl Pts',(-0.797882889462375,-1.33528133621917,
16.1075766434577));
#270147=CARTESIAN_POINT('Ctrl Pts',(-0.804324903347557,-1.33141160909593,
16.1070389462636));
#270148=CARTESIAN_POINT('Ctrl Pts',(-0.80765652127111,-1.32939323283044,
16.106761034654));
#270149=CARTESIAN_POINT('Ctrl Pts',(-0.816127845920436,-1.32421749481746,
16.1060547249551));
#270150=CARTESIAN_POINT('Ctrl Pts',(-0.821256893698819,-1.32104267609436,
16.105627401268));
#270151=CARTESIAN_POINT('Ctrl Pts',(-0.836070685458236,-1.31175349563657,
16.1043937247262));
#270152=CARTESIAN_POINT('Ctrl Pts',(-0.845706772380946,-1.3055617558416,
16.1035918981216));
#270153=CARTESIAN_POINT('Ctrl Pts',(-0.976461631052707,-1.21948900371196,
16.0927078148246));
#270154=CARTESIAN_POINT('Ctrl Pts',(-1.08590940391926,-1.12314059161889,
16.0834962595416));
#270155=CARTESIAN_POINT('Ctrl Pts',(-1.22293597596988,-0.963467028996656,
16.0694479952498));
#270156=CARTESIAN_POINT('Ctrl Pts',(-1.26228043043216,-0.911310868972647,
16.0650174533412));
#270157=CARTESIAN_POINT('Ctrl Pts',(-1.30447885558593,-0.847374686860039,
16.0596624793527));
#270158=CARTESIAN_POINT('Ctrl Pts',(-1.3106239526464,-0.837838759763592,
16.0588657945625));
#270159=CARTESIAN_POINT('Ctrl Pts',(-1.32049227288281,-0.822150898163259,
16.0575578941453));
#270160=CARTESIAN_POINT('Ctrl Pts',(-1.32427819042192,-0.816038732739042,
16.0570489943488));
#270161=CARTESIAN_POINT('Ctrl Pts',(-1.3309822859232,-0.805045799915239,
16.0561348019584));
#270162=CARTESIAN_POINT('Ctrl Pts',(-1.33391634949332,-0.80017482863684,
16.0557300991647));
#270163=CARTESIAN_POINT('Ctrl Pts',(-1.34008524180136,-0.789805350546408,
16.054869287775));
#270164=CARTESIAN_POINT('Ctrl Pts',(-1.3433130759484,-0.784302827223577,
16.0544129346997));
#270165=CARTESIAN_POINT('Ctrl Pts',(-1.351871410928,-0.769505519530362,
16.0531867731405));
#270166=CARTESIAN_POINT('Ctrl Pts',(-1.35713978827913,-0.760175401246038,
16.0524147503176));
#270167=CARTESIAN_POINT('Ctrl Pts',(-1.38287156433815,-0.713485111054437,
16.0485560946431));
#270168=CARTESIAN_POINT('Ctrl Pts',(-1.40188874034638,-0.675353296657955,
16.0454189887703));
#270169=CARTESIAN_POINT('Ctrl Pts',(-1.48483081101455,-0.490400613932409,
16.0302534114448));
#270170=CARTESIAN_POINT('Ctrl Pts',(-1.52738494115264,-0.33510522985144,
16.0175353988927));
#270171=CARTESIAN_POINT('Ctrl Pts',(-1.54848231151036,-0.149918712130985,
16.0034886715258));
#270172=CARTESIAN_POINT('Ctrl Pts',(-1.55079768980039,-0.123692497960716,
16.001528261944));
#270173=CARTESIAN_POINT('Ctrl Pts',(-1.55283995640408,-0.0911471365309453,
15.9991409602467));
#270174=CARTESIAN_POINT('Ctrl Pts',(-1.55319548055527,-0.0848736325823962,
15.9986828695023));
#270175=CARTESIAN_POINT('Ctrl Pts',(-1.55369778872703,-0.0749453617730281,
15.9979613907529));
#270176=CARTESIAN_POINT('Ctrl Pts',(-1.55386970929931,-0.0712920277401801,
15.997696651721));
#270177=CARTESIAN_POINT('Ctrl Pts',(-1.55416497753361,-0.0645080476316434,
15.9972064757795));
#270178=CARTESIAN_POINT('Ctrl Pts',(-1.55429175119681,-0.0613776672525384,
15.9969808586445));
#270179=CARTESIAN_POINT('Ctrl Pts',(-1.55452553951862,-0.0551386554779275,
15.9965323038761));
#270180=CARTESIAN_POINT('Ctrl Pts',(-1.55463268773893,-0.0520300971929322,
15.9963093609128));
#270181=CARTESIAN_POINT('Ctrl Pts',(-1.55485755933656,-0.0448836101606422,
15.9957980359545));
#270182=CARTESIAN_POINT('Ctrl Pts',(-1.55496887945015,-0.0408454794407842,
15.995510002288));
#270183=CARTESIAN_POINT('Ctrl Pts',(-1.55535093414078,-0.0247039502565554,
15.9943620471943));
#270184=CARTESIAN_POINT('Ctrl Pts',(-1.55549610541594,-0.0125976349117609,
15.9935086974294));
#270185=CARTESIAN_POINT('Ctrl Pts',(-1.555499922686,-0.000490432305788335,
15.9926617964138));
#270186=CARTESIAN_POINT('Ctrl Pts',(-1.5554999222446,-0.000491830301829164,
15.9926618942039));
#270187=CARTESIAN_POINT('Ctrl Pts',(-1.55554030562071,0.127227706631577,
15.9837278841703));
#270188=CARTESIAN_POINT('Ctrl Pts',(-1.5398505335658,0.254495564010868,
15.9755208537055));
#270189=CARTESIAN_POINT('Ctrl Pts',(-1.48952695169905,0.455128082193538,
15.9618391493048));
#270190=CARTESIAN_POINT('Ctrl Pts',(-1.46447355021139,0.530232798088373,
15.9565425441433));
#270191=CARTESIAN_POINT('Ctrl Pts',(-1.42684502869873,0.619691391172787,
15.9498050035162));
#270192=CARTESIAN_POINT('Ctrl Pts',(-1.41957991519656,0.636157978547014,
15.948546584934));
#270193=CARTESIAN_POINT('Ctrl Pts',(-1.40874790931139,0.659598995112758,
15.9467269703452));
#270194=CARTESIAN_POINT('Ctrl Pts',(-1.40541130331365,0.666678761345963,
15.9461736595929));
#270195=CARTESIAN_POINT('Ctrl Pts',(-1.39951968555009,0.678939071313797,
15.9452087912896));
#270196=CARTESIAN_POINT('Ctrl Pts',(-1.39698895894683,0.684131171438668,
15.9447980803877));
#270197=CARTESIAN_POINT('Ctrl Pts',(-1.39205422289453,0.694113836870691,
15.944004300602));
#270198=CARTESIAN_POINT('Ctrl Pts',(-1.38965425108613,0.698906316415611,
15.943621377177));
#270199=CARTESIAN_POINT('Ctrl Pts',(-1.3839105396724,0.710229326492192,
15.9427122219029));
#270200=CARTESIAN_POINT('Ctrl Pts',(-1.38054529681994,0.716748741213035,
15.9421852414407));
#270201=CARTESIAN_POINT('Ctrl Pts',(-1.3684995150176,0.739685201061264,
15.9403185794652));
#270202=CARTESIAN_POINT('Ctrl Pts',(-1.35957154558131,0.755969758789627,
15.9389702124151));
#270203=CARTESIAN_POINT('Ctrl Pts',(-1.29519000225675,0.868570511218385,
15.929480064824));
#270204=CARTESIAN_POINT('Ctrl Pts',(-1.2298553969229,0.958842089365959,
15.9209731408593));
#270205=CARTESIAN_POINT('Ctrl Pts',(-1.09333104534222,1.11032665730706,
15.9051649285799));
#270206=CARTESIAN_POINT('Ctrl Pts',(-1.02512803857659,1.17359015713718,
15.8979363380555));
#270207=CARTESIAN_POINT('Ctrl Pts',(-0.944018339322086,1.23632663234336,
15.8903209042197));
#270208=CARTESIAN_POINT('Ctrl Pts',(-0.93629723493177,1.24218423213741,
15.8896050853797));
#270209=CARTESIAN_POINT('Ctrl Pts',(-0.924217891554731,1.25117157686216,
15.8884999080377));
#270210=CARTESIAN_POINT('Ctrl Pts',(-0.919897516201082,1.2543514609951,
15.8881075003065));
#270211=CARTESIAN_POINT('Ctrl Pts',(-0.911793773768553,1.26025159221254,
15.8873769453647));
#270212=CARTESIAN_POINT('Ctrl Pts',(-0.908014481900579,1.26297730135247,
15.8870384474337));
#270213=CARTESIAN_POINT('Ctrl Pts',(-0.901600430749328,1.26755958478693,
15.8864677617847));
#270214=CARTESIAN_POINT('Ctrl Pts',(-0.898972069865703,1.26942500999133,
15.8862349761029));
#270215=CARTESIAN_POINT('Ctrl Pts',(-0.893903015961476,1.27299902743729,
15.8857881109913));
#270216=CARTESIAN_POINT('Ctrl Pts',(-0.891463190891873,1.27470879242905,
15.8855739490452));
#270217=CARTESIAN_POINT('Ctrl Pts',(-0.885029707953356,1.27918970216261,
15.8850116115073));
#270218=CARTESIAN_POINT('Ctrl Pts',(-0.881027902956447,1.28194918541921,
15.8846642226194));
#270219=CARTESIAN_POINT('Ctrl Pts',(-0.867036088347509,1.29150091098132,
15.8834577085358));
#270220=CARTESIAN_POINT('Ctrl Pts',(-0.856979609319309,1.29819573045059,
15.8826048244042));
#270221=CARTESIAN_POINT('Ctrl Pts',(-0.765874142598457,1.35732653583144,
15.8749956956541));
#270222=CARTESIAN_POINT('Ctrl Pts',(-0.680172933462574,1.40223719870668,
15.8686579403287));
#270223=CARTESIAN_POINT('Ctrl Pts',(-0.481580870613016,1.48378322846103,
15.8545291965505));
#270224=CARTESIAN_POINT('Ctrl Pts',(-0.367575910434226,1.51605252721111,
15.8467542408138));
#270225=CARTESIAN_POINT('Ctrl Pts',(-0.237554502424209,1.53731403682826,
15.8375580332332));
#270226=CARTESIAN_POINT('Ctrl Pts',(-0.224054784418524,1.53933947594232,
15.8365998990486));
#270227=CARTESIAN_POINT('Ctrl Pts',(-0.203589011586023,1.54213515884334,
15.8351415475675));
#270228=CARTESIAN_POINT('Ctrl Pts',(-0.19664127367615,1.5430364676057,15.8346454578352));
#270229=CARTESIAN_POINT('Ctrl Pts',(-0.184059758045968,1.5445822763151,
15.8337451680965));
#270230=CARTESIAN_POINT('Ctrl Pts',(-0.178428060747985,1.54524296743774,
15.8333414848725));
#270231=CARTESIAN_POINT('Ctrl Pts',(-0.166331305626079,1.54659510577575,
15.8324728220715));
#270232=CARTESIAN_POINT('Ctrl Pts',(-0.159865293933973,1.54727683685333,
15.8320075451354));
#270233=CARTESIAN_POINT('Ctrl Pts',(-0.142463626944474,1.54900130398847,
15.8307526948474));
#270234=CARTESIAN_POINT('Ctrl Pts',(-0.131521065255699,1.54996874892331,
15.8299607792273));
#270235=CARTESIAN_POINT('Ctrl Pts',(-0.0791205196508659,1.554042660268,
15.8261542349543));
#270236=CARTESIAN_POINT('Ctrl Pts',(-0.037563078176485,1.55560183088846,
15.823091915796));
#270237=CARTESIAN_POINT('Ctrl Pts',(0.147616518815006,1.55512522061724,
15.8092397272847));
#270238=CARTESIAN_POINT('Ctrl Pts',(0.290479054988182,1.53486643416447,
15.7979142255212));
#270239=CARTESIAN_POINT('Ctrl Pts',(0.468613472780923,1.4838204924963,15.7837699061838));
#270240=CARTESIAN_POINT('Ctrl Pts',(0.508256883953022,1.4707132774537,15.7806276780636));
#270241=CARTESIAN_POINT('Ctrl Pts',(0.553953404949826,1.4535356749029,15.7770477936374));
#270242=CARTESIAN_POINT('Ctrl Pts',(0.560560874023978,1.45100029107967,
15.7765312228227));
#270243=CARTESIAN_POINT('Ctrl Pts',(0.570682756067301,1.44703691309852,
15.7757417753155));
#270244=CARTESIAN_POINT('Ctrl Pts',(0.574209517190068,1.44564105750517,
15.775467061043));
#270245=CARTESIAN_POINT('Ctrl Pts',(0.580678461139734,1.44305330850844,
15.7749638618381));
#270246=CARTESIAN_POINT('Ctrl Pts',(0.583622088372616,1.4418653143792,15.7747351559546));
#270247=CARTESIAN_POINT('Ctrl Pts',(0.590228337269242,1.4391756073858,15.7742224761117));
#270248=CARTESIAN_POINT('Ctrl Pts',(0.593888869289395,1.43766892255628,
15.7739388053781));
#270249=CARTESIAN_POINT('Ctrl Pts',(0.604585858185119,1.43321818572596,
15.773110924296));
#270250=CARTESIAN_POINT('Ctrl Pts',(0.611606595866989,1.43023627628909,
15.7725689290351));
#270251=CARTESIAN_POINT('Ctrl Pts',(0.662621819692862,1.40812428991122,
15.7686385510335));
#270252=CARTESIAN_POINT('Ctrl Pts',(0.705737631372396,1.38701737455483,
15.7653598328581));
#270253=CARTESIAN_POINT('Ctrl Pts',(0.830884781060122,1.31840281325852,
15.7557708201339));
#270254=CARTESIAN_POINT('Ctrl Pts',(0.909624761125001,1.26536163017004,
15.7496301680889));
#270255=CARTESIAN_POINT('Ctrl Pts',(1.04118128410883,1.15807940032096,15.7383734959797));
#270256=CARTESIAN_POINT('Ctrl Pts',(1.09579828535327,1.10653972841146,15.7333275347108));
#270257=CARTESIAN_POINT('Ctrl Pts',(1.1572552109425,1.03951661073784,15.7269989430662));
#270258=CARTESIAN_POINT('Ctrl Pts',(1.1678479961554,1.02760178680621,15.725882299104));
#270259=CARTESIAN_POINT('Ctrl Pts',(1.18312271699436,1.00987943227182,15.7242322736868));
#270260=CARTESIAN_POINT('Ctrl Pts',(1.1879492446031,1.00419740088748,15.723704857187));
#270261=CARTESIAN_POINT('Ctrl Pts',(1.19640548705963,0.994096003161028,
15.722769912651));
#270262=CARTESIAN_POINT('Ctrl Pts',(1.20005205446257,0.989690869892641,
15.7223630803908));
#270263=CARTESIAN_POINT('Ctrl Pts',(1.20713797849269,0.981034176317199,
15.7215652709919));
#270264=CARTESIAN_POINT('Ctrl Pts',(1.2105793729228,0.976784384941612,15.7211743841208));
#270265=CARTESIAN_POINT('Ctrl Pts',(1.21983230208397,0.965233898349809,
15.7201140267467));
#270266=CARTESIAN_POINT('Ctrl Pts',(1.225600586333,0.957899013185116,15.7194428458201));
#270267=CARTESIAN_POINT('Ctrl Pts',(1.24716338059975,0.929966385597103,
15.7168946474326));
#270268=CARTESIAN_POINT('Ctrl Pts',(1.26250664122506,0.909027395911184,
15.7150001798617));
#270269=CARTESIAN_POINT('Ctrl Pts',(1.28071860612345,0.882822522779436,
15.7126466390402));
#270270=CARTESIAN_POINT('Ctrl Pts',(1.28409095564,0.877910115374345,15.7122061771278));
#270271=CARTESIAN_POINT('Ctrl Pts',(1.34546691838573,0.78739521878424,15.7041036790209));
#270272=CARTESIAN_POINT('Ctrl Pts',(1.39473129640741,0.696368618857575,
15.6961474234014));
#270273=CARTESIAN_POINT('Ctrl Pts',(1.43457669742932,0.601306867741246,
15.6881535475172));
#270274=CARTESIAN_POINT('Ctrl Pts',(1.43457668274383,0.601306902777371,
15.5515012983457));
#270275=CARTESIAN_POINT('Ctrl Pts',(1.42934844806766,0.613780239643622,
15.5525085349074));
#270276=CARTESIAN_POINT('Ctrl Pts',(1.42395721819853,0.626186141922541,
15.5535084794065));
#270277=CARTESIAN_POINT('Ctrl Pts',(1.41561724659483,0.644712461489998,
15.5549973208906));
#270278=CARTESIAN_POINT('Ctrl Pts',(1.41278964660618,0.650885370738069,
15.5554926512506));
#270279=CARTESIAN_POINT('Ctrl Pts',(1.40833348086355,0.660447721965127,
15.55625857616));
#270280=CARTESIAN_POINT('Ctrl Pts',(1.40673293767129,0.663850005388352,
15.556530818317));
#270281=CARTESIAN_POINT('Ctrl Pts',(1.40373802512826,0.670156837512861,
15.5570349207783));
#270282=CARTESIAN_POINT('Ctrl Pts',(1.40234698007989,0.673062833517404,
15.5572669709428));
#270283=CARTESIAN_POINT('Ctrl Pts',(1.39915764745773,0.679672773936283,
15.5577942970538));
#270284=CARTESIAN_POINT('Ctrl Pts',(1.39735367740164,0.683373911833856,
15.5580892174614));
#270285=CARTESIAN_POINT('Ctrl Pts',(1.3926133340234,0.693002239854106,15.5588556440012));
#270286=CARTESIAN_POINT('Ctrl Pts',(1.38965377158621,0.698918022213251,
15.5593257593537));
#270287=CARTESIAN_POINT('Ctrl Pts',(1.36962984442554,0.738313201347103,
15.5624523506666));
#270288=CARTESIAN_POINT('Ctrl Pts',(1.3513931545769,0.771187014485425,15.5650417529206));
#270289=CARTESIAN_POINT('Ctrl Pts',(1.25506506696459,0.930898075588822,
15.5776864907652));
#270290=CARTESIAN_POINT('Ctrl Pts',(1.16023235582736,1.04672200712425,15.5871399182306));
#270291=CARTESIAN_POINT('Ctrl Pts',(1.03052492131856,1.16547098614687,15.5990848128733));
#270292=CARTESIAN_POINT('Ctrl Pts',(1.0102118927016,1.1831213073835,15.6009292642349));
#270293=CARTESIAN_POINT('Ctrl Pts',(0.974554263842389,1.21251681484336,
15.604132582659));
#270294=CARTESIAN_POINT('Ctrl Pts',(0.959429485372816,1.22451951576753,
15.6054811898572));
#270295=CARTESIAN_POINT('Ctrl Pts',(0.937640810738469,1.24115902391904,
15.6074120797511));
#270296=CARTESIAN_POINT('Ctrl Pts',(0.931157555623165,1.246030342628,15.6079851562898));
#270297=CARTESIAN_POINT('Ctrl Pts',(0.919906685743735,1.25434705585255,
15.6089773184488));
#270298=CARTESIAN_POINT('Ctrl Pts',(0.915157022637549,1.25781654830282,
15.6093954596554));
#270299=CARTESIAN_POINT('Ctrl Pts',(0.906019661718658,1.26441197601966,
15.6101985862839));
#270300=CARTESIAN_POINT('Ctrl Pts',(0.901635169418222,1.26754222511353,
15.6105833979205));
#270301=CARTESIAN_POINT('Ctrl Pts',(0.891298315762892,1.2748413123673,15.6114893657844));
#270302=CARTESIAN_POINT('Ctrl Pts',(0.885332870111243,1.27899130770212,
15.6120112303675));
#270303=CARTESIAN_POINT('Ctrl Pts',(0.864615643544258,1.29318931902059,
15.6138204236947));
#270304=CARTESIAN_POINT('Ctrl Pts',(0.849720648974535,1.30302478692408,
15.615115677387));
#270305=CARTESIAN_POINT('Ctrl Pts',(0.728275641506958,1.3802495425295,15.6256369559465));
#270306=CARTESIAN_POINT('Ctrl Pts',(0.61408279200549,1.43469969242128,15.6353461738357));
#270307=CARTESIAN_POINT('Ctrl Pts',(0.444520143592107,1.49156719770015,
15.6492135003694));
#270308=CARTESIAN_POINT('Ctrl Pts',(0.393609754801732,1.50580304159952,
15.6533033741496));
#270309=CARTESIAN_POINT('Ctrl Pts',(0.306242534213506,1.52549818145962,
15.6601144994287));
#270310=CARTESIAN_POINT('Ctrl Pts',(0.270135121165863,1.53230439260416,
15.6628705570639));
#270311=CARTESIAN_POINT('Ctrl Pts',(0.226981413298368,1.53886565228877,
15.6660701444033));
#270312=CARTESIAN_POINT('Ctrl Pts',(0.220138631157557,1.53985942398576,
15.6665746924036));
#270313=CARTESIAN_POINT('Ctrl Pts',(0.209538179049052,1.54132681216738,
15.6673517447645));
#270314=CARTESIAN_POINT('Ctrl Pts',(0.205785139586706,1.54183237335995,
15.6676259725834));
#270315=CARTESIAN_POINT('Ctrl Pts',(0.198838445709416,1.54274232613377,
15.6681318746976));
#270316=CARTESIAN_POINT('Ctrl Pts',(0.195645404825771,1.54315050733253,
15.6683637509709));
#270317=CARTESIAN_POINT('Ctrl Pts',(0.188401678718804,1.54405366148103,
15.6688883046321));
#270318=CARTESIAN_POINT('Ctrl Pts',(0.184350302424393,1.54454260837944,
15.6691806416247));
#270319=CARTESIAN_POINT('Ctrl Pts',(0.172289696565317,1.54595003162697,
15.670047929346));
#270320=CARTESIAN_POINT('Ctrl Pts',(0.164275035421767,1.54682221343174,
15.6706203700988));
#270321=CARTESIAN_POINT('Ctrl Pts',(0.0878890321656346,1.55453438098304,
15.6760422108649));
#270322=CARTESIAN_POINT('Ctrl Pts',(0.0191314642421557,1.5569002588872,
15.6806650907233));
#270323=CARTESIAN_POINT('Ctrl Pts',(-0.123717841429334,1.5523460265859,
15.6901466418542));
#270324=CARTESIAN_POINT('Ctrl Pts',(-0.197605372077892,1.54468010560252,
15.6949846986021));
#270325=CARTESIAN_POINT('Ctrl Pts',(-0.341552558709919,1.51924459721154,
15.7046827646893));
#270326=CARTESIAN_POINT('Ctrl Pts',(-0.411477035943539,1.5018145355335,
15.7095263283126));
#270327=CARTESIAN_POINT('Ctrl Pts',(-0.496337524567553,1.47428849324218,
15.715725298707));
#270328=CARTESIAN_POINT('Ctrl Pts',(-0.512647105714802,1.46869683845198,
15.7169315538374));
#270329=CARTESIAN_POINT('Ctrl Pts',(-0.536149195959212,1.46020011284151,
15.7186930244006));
#270330=CARTESIAN_POINT('Ctrl Pts',(-0.543418644266888,1.45751037835709,
15.7192411255614));
#270331=CARTESIAN_POINT('Ctrl Pts',(-0.556111993204555,1.45270561019864,
15.7202040481441));
#270332=CARTESIAN_POINT('Ctrl Pts',(-0.561544736460079,1.45061423064821,
15.720618074617));
#270333=CARTESIAN_POINT('Ctrl Pts',(-0.572064696659957,1.44649653224233,
15.7214235453037));
#270334=CARTESIAN_POINT('Ctrl Pts',(-0.577153212239487,1.44447374608946,
15.7218148659096));
#270335=CARTESIAN_POINT('Ctrl Pts',(-0.589291257647919,1.43957425460287,
15.7227524766097));
#270336=CARTESIAN_POINT('Ctrl Pts',(-0.596330495111955,1.43667259931803,
15.7232996007539));
#270337=CARTESIAN_POINT('Ctrl Pts',(-0.621749120791783,1.42597575204317,
15.7252877228035));
#270338=CARTESIAN_POINT('Ctrl Pts',(-0.639998589627072,1.41787889153704,
15.7267388683028));
#270339=CARTESIAN_POINT('Ctrl Pts',(-0.820527571616443,1.33358709687311,
15.7413401328465));
#270340=CARTESIAN_POINT('Ctrl Pts',(-0.968618873358817,1.23022956974228,
15.7555528068988));
#270341=CARTESIAN_POINT('Ctrl Pts',(-1.11981784811301,1.08015464159224,
15.771716709502));
#270342=CARTESIAN_POINT('Ctrl Pts',(-1.14306003135819,1.05552842900918,
15.774251600495));
#270343=CARTESIAN_POINT('Ctrl Pts',(-1.16996165699715,1.025093031421,15.7772281100735));
#270344=CARTESIAN_POINT('Ctrl Pts',(-1.17440826799998,1.01999569923434,
15.7777215616844));
#270345=CARTESIAN_POINT('Ctrl Pts',(-1.18127109364515,1.01202418380928,
15.778485216888));
#270346=CARTESIAN_POINT('Ctrl Pts',(-1.18371031895236,1.00917006837892,
15.7787570528064));
#270347=CARTESIAN_POINT('Ctrl Pts',(-1.18822393676091,1.00384984449521,
15.7792607926071));
#270348=CARTESIAN_POINT('Ctrl Pts',(-1.19030098197612,1.00138614271979,
15.7794928838574));
#270349=CARTESIAN_POINT('Ctrl Pts',(-1.19501945585576,0.995753868258473,
15.7800208020681));
#270350=CARTESIAN_POINT('Ctrl Pts',(-1.19765594509,0.992581233086318,15.7803162702837));
#270351=CARTESIAN_POINT('Ctrl Pts',(-1.20450351664006,0.98427416034673,
15.7810850677255));
#270352=CARTESIAN_POINT('Ctrl Pts',(-1.20869445583477,0.97912310815566,
15.7815569920491));
#270353=CARTESIAN_POINT('Ctrl Pts',(-1.23688489886833,0.944017597118781,
15.7847421845554));
#270354=CARTESIAN_POINT('Ctrl Pts',(-1.25980400446532,0.913207510243438,
15.787385415763));
#270355=CARTESIAN_POINT('Ctrl Pts',(-1.36649169966915,0.758114147660761,
15.8001380528514));
#270356=CARTESIAN_POINT('Ctrl Pts',(-1.43313778581445,0.623024121988957,
15.8096491627439));
#270357=CARTESIAN_POINT('Ctrl Pts',(-1.49155088772275,0.443165068054534,
15.8225100803645));
#270358=CARTESIAN_POINT('Ctrl Pts',(-1.50225208250412,0.405410368434929,
15.8252143780538));
#270359=CARTESIAN_POINT('Ctrl Pts',(-1.51399866275157,0.357070026138771,
15.8287028112708));
#270360=CARTESIAN_POINT('Ctrl Pts',(-1.51637923511729,0.346821221994342,
15.8294438262542));
#270361=CARTESIAN_POINT('Ctrl Pts',(-1.520037726189,0.330312531122009,15.8306400884911));
#270362=CARTESIAN_POINT('Ctrl Pts',(-1.5213813999129,0.324067417434184,
15.8310932293327));
#270363=CARTESIAN_POINT('Ctrl Pts',(-1.52386624949489,0.312162203669072,
15.8319582958353));
#270364=CARTESIAN_POINT('Ctrl Pts',(-1.5250144553291,0.306503665778198,
15.8323699895656));
#270365=CARTESIAN_POINT('Ctrl Pts',(-1.52756450164253,0.293567491085846,
15.8333124494089));
#270366=CARTESIAN_POINT('Ctrl Pts',(-1.52894587651818,0.286286013732919,
15.8338438562475));
#270367=CARTESIAN_POINT('Ctrl Pts',(-1.53241339035425,0.267266858826115,
15.8352344206141));
#270368=CARTESIAN_POINT('Ctrl Pts',(-1.53441668264626,0.255514778583605,
15.836096174526));
#270369=CARTESIAN_POINT('Ctrl Pts',(-1.54914924951,0.162656358876138,15.8429265024275));
#270370=CARTESIAN_POINT('Ctrl Pts',(-1.55557208489254,0.0806950259623673,
15.8490932619655));
#270371=CARTESIAN_POINT('Ctrl Pts',(-1.5554120703512,-0.0999616197188796,
15.8629544420336));
#270372=CARTESIAN_POINT('Ctrl Pts',(-1.54595327256803,-0.198309895053453,
15.870680526702));
#270373=CARTESIAN_POINT('Ctrl Pts',(-1.5193725451513,-0.335874966079489,
15.8813781973874));
#270374=CARTESIAN_POINT('Ctrl Pts',(-1.50986320948355,-0.376322676413595,
15.8845068123646));
#270375=CARTESIAN_POINT('Ctrl Pts',(-1.49692813352857,-0.422885912252754,
15.8880540353352));
#270376=CARTESIAN_POINT('Ctrl Pts',(-1.4950683214219,-0.429414776749792,
15.888550136866));
#270377=CARTESIAN_POINT('Ctrl Pts',(-1.49199730164097,-0.439933728839646,
15.8893471438969));
#270378=CARTESIAN_POINT('Ctrl Pts',(-1.49081271558257,-0.443931393381345,
15.8896495066573));
#270379=CARTESIAN_POINT('Ctrl Pts',(-1.48868296448025,-0.451014069723026,
15.8901841951944));
#270380=CARTESIAN_POINT('Ctrl Pts',(-1.48774426167838,-0.454100949576394,
15.8904168874582));
#270381=CARTESIAN_POINT('Ctrl Pts',(-1.4857013661754,-0.460744581512379,
15.890916939358));
#270382=CARTESIAN_POINT('Ctrl Pts',(-1.48459400439268,-0.464300292653457,
15.891184111735));
#270383=CARTESIAN_POINT('Ctrl Pts',(-1.48148127871369,-0.474170180518937,
15.8919245397757));
#270384=CARTESIAN_POINT('Ctrl Pts',(-1.4794482989959,-0.480475674788657,
15.8923962201653));
#270385=CARTESIAN_POINT('Ctrl Pts',(-1.4675348760013,-0.516633739557499,
15.8950942856192));
#270386=CARTESIAN_POINT('Ctrl Pts',(-1.45679045193464,-0.546196822495111,
15.8972738476213));
#270387=CARTESIAN_POINT('Ctrl Pts',(-1.41785960741151,-0.643971496555455,
15.9044581095223));
#270388=CARTESIAN_POINT('Ctrl Pts',(-1.38571700242618,-0.710503683917368,
15.9093094563308));
#270389=CARTESIAN_POINT('Ctrl Pts',(-1.29437567048341,-0.869594070895327,
15.9213839861234));
#270390=CARTESIAN_POINT('Ctrl Pts',(-1.22988950761889,-0.958629108956368,
15.9285993075028));
#270391=CARTESIAN_POINT('Ctrl Pts',(-1.14410059163391,-1.05402212292164,
15.9374948780266));
#270392=CARTESIAN_POINT('Ctrl Pts',(-1.13136816714337,-1.06767730036343,
15.9387989510139));
#270393=CARTESIAN_POINT('Ctrl Pts',(-1.11324609141095,-1.08642452184601,
15.9406349142027));
#270394=CARTESIAN_POINT('Ctrl Pts',(-1.10806077413058,-1.09171260830882,
15.9411580139155));
#270395=CARTESIAN_POINT('Ctrl Pts',(-1.09901415828145,-1.10080767166477,
15.9420669427638));
#270396=CARTESIAN_POINT('Ctrl Pts',(-1.09517031658875,-1.10463189633755,
15.942452002397));
#270397=CARTESIAN_POINT('Ctrl Pts',(-1.08713454834094,-1.11254348322454,
15.9432546932393));
#270398=CARTESIAN_POINT('Ctrl Pts',(-1.08293938958395,-1.11662742444639,
15.9436724648996));
#270399=CARTESIAN_POINT('Ctrl Pts',(-1.07299021366747,-1.12620403516568,
15.9446603115157));
#270400=CARTESIAN_POINT('Ctrl Pts',(-1.0672169687623,-1.13167639574182,
15.9452312491333));
#270401=CARTESIAN_POINT('Ctrl Pts',(-1.04795443279522,-1.14965653971391,
15.9471289039081));
#270402=CARTESIAN_POINT('Ctrl Pts',(-1.03428571218525,-1.16196887400984,
15.9484638206013));
#270403=CARTESIAN_POINT('Ctrl Pts',(-1.00132795128539,-1.19061381683405,
15.9516567169589));
#270404=CARTESIAN_POINT('Ctrl Pts',(-0.981853395783587,-1.20672395402667,
15.9535232064232));
#270405=CARTESIAN_POINT('Ctrl Pts',(-0.843711303932902,-1.31544237099492,
15.966629289372));
#270406=CARTESIAN_POINT('Ctrl Pts',(-0.712545280346618,-1.39086371500204,
15.9785143108742));
#270407=CARTESIAN_POINT('Ctrl Pts',(-0.53650775481938,-1.46056489265463,
15.9929430332127));
#270408=CARTESIAN_POINT('Ctrl Pts',(-0.499849217277457,-1.47351340759649,
15.9958652416534));
#270409=CARTESIAN_POINT('Ctrl Pts',(-0.456377607788493,-1.48705889158308,
15.9992064405419));
#270410=CARTESIAN_POINT('Ctrl Pts',(-0.450001837833795,-1.4890006776742,
15.9996933928782));
#270411=CARTESIAN_POINT('Ctrl Pts',(-0.439652887823633,-1.49207997929655,
16.0004785944465));
#270412=CARTESIAN_POINT('Ctrl Pts',(-0.435687399434212,-1.49324271886152,
16.0007782337497));
#270413=CARTESIAN_POINT('Ctrl Pts',(-0.428620852744101,-1.4952841878815,
16.0013099459183));
#270414=CARTESIAN_POINT('Ctrl Pts',(-0.425521657526806,-1.49616909392795,
16.0015423696985));
#270415=CARTESIAN_POINT('Ctrl Pts',(-0.418811303747745,-1.49806254829275,
16.0020439375468));
#270416=CARTESIAN_POINT('Ctrl Pts',(-0.415199246348476,-1.4990676747164,
16.0023128829537));
#270417=CARTESIAN_POINT('Ctrl Pts',(-0.40508342294535,-1.50184323509203,
16.0030632719579));
#270418=CARTESIAN_POINT('Ctrl Pts',(-0.39857162590491,-1.50358449904523,
16.0035430705299));
#270419=CARTESIAN_POINT('Ctrl Pts',(-0.359703204987075,-1.51370771449768,
16.0063887985263));
#270420=CARTESIAN_POINT('Ctrl Pts',(-0.327091621469221,-1.52108807554105,
16.008701697389));
#270421=CARTESIAN_POINT('Ctrl Pts',(-0.128081056059097,-1.55942857772257,
16.0225077268172));
#270422=CARTESIAN_POINT('Ctrl Pts',(0.0422172938819871,-1.56411338524212,
16.0331544213128));
#270423=CARTESIAN_POINT('Ctrl Pts',(0.214032242580014,-1.54071006648652,
16.045062626977));
#270424=CARTESIAN_POINT('Ctrl Pts',(0.218122538668752,-1.54013631456753,
16.0453467197997));
#270425=CARTESIAN_POINT('Ctrl Pts',(0.246516970173361,-1.53603800322895,
16.0473231770209));
#270426=CARTESIAN_POINT('Ctrl Pts',(0.270735733481293,-1.531954767939,16.0490310229766));
#270427=CARTESIAN_POINT('Ctrl Pts',(0.303875700185424,-1.5255570694587,
16.0514031683096));
#270428=CARTESIAN_POINT('Ctrl Pts',(0.312889008325581,-1.5237339909968,
16.0520519346301));
#270429=CARTESIAN_POINT('Ctrl Pts',(0.32725581576149,-1.52069523972461,
16.0530920280967));
#270430=CARTESIAN_POINT('Ctrl Pts',(0.332620066055354,-1.51953093792877,
16.0534817146912));
#270431=CARTESIAN_POINT('Ctrl Pts',(0.343653491025345,-1.51707492748415,
16.054286055969));
#270432=CARTESIAN_POINT('Ctrl Pts',(0.349321802615655,-1.51577977754852,
16.0547008149319));
#270433=CARTESIAN_POINT('Ctrl Pts',(0.362485064934866,-1.51269435326561,
16.0556676381989));
#270434=CARTESIAN_POINT('Ctrl Pts',(0.369974181756807,-1.51088011753997,
16.05622046249));
#270435=CARTESIAN_POINT('Ctrl Pts',(0.393931925753363,-1.50488755703987,
16.0579980054344));
#270436=CARTESIAN_POINT('Ctrl Pts',(0.410345176873168,-1.50049515652697,
16.0592295607999));
#270437=CARTESIAN_POINT('Ctrl Pts',(0.493962508726928,-1.47664355403327,
16.0655769830527));
#270438=CARTESIAN_POINT('Ctrl Pts',(0.559860743095888,-1.4529378671706,
16.07082858045));
#270439=CARTESIAN_POINT('Ctrl Pts',(0.717574364942324,-1.38387771829978,
16.0840015443296));
#270440=CARTESIAN_POINT('Ctrl Pts',(0.806940907251016,-1.33374490097917,
16.0920163453326));
#270441=CARTESIAN_POINT('Ctrl Pts',(0.902666854512966,-1.26687979351112,
16.1009460085624));
#270442=CARTESIAN_POINT('Ctrl Pts',(0.914475397680684,-1.25838254646261,
16.102053628093));
#270443=CARTESIAN_POINT('Ctrl Pts',(0.950787795580712,-1.23147156331882,
16.1054749978316));
#270444=CARTESIAN_POINT('Ctrl Pts',(0.974869746746093,-1.21249699033323,
16.1077662230733));
#270445=CARTESIAN_POINT('Ctrl Pts',(1.00360837571268,-1.18844310502144,
16.110513249889));
#270446=CARTESIAN_POINT('Ctrl Pts',(1.00881081194145,-1.18403020906588,
16.111011057188));
#270447=CARTESIAN_POINT('Ctrl Pts',(1.01687233312155,-1.17710042620274,
16.1117830414109));
#270448=CARTESIAN_POINT('Ctrl Pts',(1.01975140515304,-1.17460709506081,
16.1120588663488));
#270449=CARTESIAN_POINT('Ctrl Pts',(1.02504562078543,-1.1699880666837,16.1125662466186));
#270450=CARTESIAN_POINT('Ctrl Pts',(1.02746331299255,-1.16786546388028,
16.1127980136026));
#270451=CARTESIAN_POINT('Ctrl Pts',(1.03291174020139,-1.16305202460563,
16.1133204753159));
#270452=CARTESIAN_POINT('Ctrl Pts',(1.03593855155773,-1.16035683881633,
16.1136108412362));
#270453=CARTESIAN_POINT('Ctrl Pts',(1.04505212702312,-1.15217768719108,
16.1144856035957));
#270454=CARTESIAN_POINT('Ctrl Pts',(1.05110626241287,-1.14665731757139,
16.1150673656332));
#270455=CARTESIAN_POINT('Ctrl Pts',(1.12538028097479,-1.07784911003095,
16.1222170814118));
#270456=CARTESIAN_POINT('Ctrl Pts',(1.18784364608688,-1.00859946737058,
16.1283670068836));
#270457=CARTESIAN_POINT('Ctrl Pts',(1.31571249277058,-0.838355549884314,
16.1423918693914));
#270458=CARTESIAN_POINT('Ctrl Pts',(1.37635565566783,-0.734561096730959,
16.1502323200143));
#270459=CARTESIAN_POINT('Ctrl Pts',(1.43183283736425,-0.60808692592948,
16.159812664107));
#270460=CARTESIAN_POINT('Ctrl Pts',(1.43888574261177,-0.591204494469641,
16.1610910562212));
#270461=CARTESIAN_POINT('Ctrl Pts',(1.44834531423227,-0.567388623149606,
16.1628957474056));
#270462=CARTESIAN_POINT('Ctrl Pts',(1.4510033914926,-0.56055611094073,16.1634136353778));
#270463=CARTESIAN_POINT('Ctrl Pts',(1.45553641666728,-0.548655798566441,
16.1643160227701));
#270464=CARTESIAN_POINT('Ctrl Pts',(1.45743345924851,-0.543596501153376,
16.1646997796119));
#270465=CARTESIAN_POINT('Ctrl Pts',(1.46133592356034,-0.533021586576347,
16.1655022024487));
#270466=CARTESIAN_POINT('Ctrl Pts',(1.46333656278031,-0.527504308549459,
16.1659210200159));
#270467=CARTESIAN_POINT('Ctrl Pts',(1.46800248658415,-0.514405991977171,
16.1669157838157));
#270468=CARTESIAN_POINT('Ctrl Pts',(1.47064031787978,-0.506815426101302,
16.1674926266324));
#270469=CARTESIAN_POINT('Ctrl Pts',(1.47927520391315,-0.481332743861357,
16.1694306406548));
#270470=CARTESIAN_POINT('Ctrl Pts',(1.48500525660034,-0.463352639903636,
16.1708004984707));
#270471=CARTESIAN_POINT('Ctrl Pts',(1.49788326072202,-0.42024775313346,
16.1740918068332));
#270472=CARTESIAN_POINT('Ctrl Pts',(1.50472800136901,-0.395039150347152,
16.1760224843062));
#270473=CARTESIAN_POINT('Ctrl Pts',(1.54650760837292,-0.224276054029034,
16.189143502219));
#270474=CARTESIAN_POINT('Ctrl Pts',(1.56090331708873,-0.0745135463966356,
16.2009647394349));
#270475=CARTESIAN_POINT('Ctrl Pts',(1.55185140635719,0.113131397764378,
16.2152746077481));
#270476=CARTESIAN_POINT('Ctrl Pts',(1.54860247285123,0.151236506442244,
16.2181478669469));
#270477=CARTESIAN_POINT('Ctrl Pts',(1.54314555494617,0.195770376752052,
16.2214399345214));
#270478=CARTESIAN_POINT('Ctrl Pts',(1.54229672266842,0.202348875941217,
16.2219245297602));
#270479=CARTESIAN_POINT('Ctrl Pts',(1.54085207858474,0.21300732200163,16.2227066868933));
#270480=CARTESIAN_POINT('Ctrl Pts',(1.54028209219645,0.217090591289451,
16.2230056217683));
#270481=CARTESIAN_POINT('Ctrl Pts',(1.53923771138108,0.224361094183342,
16.2235365689481));
#270482=CARTESIAN_POINT('Ctrl Pts',(1.53876964281009,0.227549159070106,
16.2237689281331));
#270483=CARTESIAN_POINT('Ctrl Pts',(1.53773451178213,0.234450269018181,
16.2242709101417));
#270484=CARTESIAN_POINT('Ctrl Pts',(1.53716390735117,0.238162717723234,
16.2245403312696));
#270485=CARTESIAN_POINT('Ctrl Pts',(1.53552692771861,0.248562178244353,
16.2252933996548));
#270486=CARTESIAN_POINT('Ctrl Pts',(1.53443030930661,0.255244456456546,
16.2257753828915));
#270487=CARTESIAN_POINT('Ctrl Pts',(1.5275676521542,0.295418796690088,16.2286627783639));
#270488=CARTESIAN_POINT('Ctrl Pts',(1.52074838454615,0.328724793222004,
16.2310133341582));
#270489=CARTESIAN_POINT('Ctrl Pts',(1.49324451285637,0.443735601225883,
16.2390641417353));
#270490=CARTESIAN_POINT('Ctrl Pts',(1.46705034582479,0.523832441439846,
16.2445596914745));
#270491=CARTESIAN_POINT('Ctrl Pts',(1.43457653793677,0.601307248252799,
16.2500928067243));
#270492=CARTESIAN_POINT('Origin',(0.,0.,-1.29405622560371));
#270493=CARTESIAN_POINT('',(1.43457668369174,0.601306900515888,17.0878643847065));
#270494=CARTESIAN_POINT('',(1.4345766824505,0.601306903477194,16.9487204703706));
#270495=CARTESIAN_POINT('',(1.43457668357355,0.601306900797845,-1.29405622560371));
#270496=CARTESIAN_POINT('Ctrl Pts',(1.43457668369174,0.601306900515888,
17.0878643847065));
#270497=CARTESIAN_POINT('Ctrl Pts',(1.46485147221303,0.529078383465645,
17.0827019053849));
#270498=CARTESIAN_POINT('Ctrl Pts',(1.48962766213377,0.454668124152851,
17.0775806645933));
#270499=CARTESIAN_POINT('Ctrl Pts',(1.51793983480686,0.341878389690674,
17.0697763105215));
#270500=CARTESIAN_POINT('Ctrl Pts',(1.52583248471291,0.304724565586252,
17.067200233606));
#270501=CARTESIAN_POINT('Ctrl Pts',(1.535236909699,0.250815869464161,17.0634298083927));
#270502=CARTESIAN_POINT('Ctrl Pts',(1.53784933366876,0.234265575817172,
17.0622679549121));
#270503=CARTESIAN_POINT('Ctrl Pts',(1.54205269612597,0.204524271440075,
17.060170295671));
#270504=CARTESIAN_POINT('Ctrl Pts',(1.54374295426395,0.191348810213299,
17.0592376115309));
#270505=CARTESIAN_POINT('Ctrl Pts',(1.5460579799202,0.171268806576169,17.0578102390323));
#270506=CARTESIAN_POINT('Ctrl Pts',(1.5468057028868,0.164378818842778,17.0573194132758));
#270507=CARTESIAN_POINT('Ctrl Pts',(1.54808095594149,0.151847632093962,
17.0564246979273));
#270508=CARTESIAN_POINT('Ctrl Pts',(1.54862375870161,0.146208077577833,
17.0560212950401));
#270509=CARTESIAN_POINT('Ctrl Pts',(1.54972849489882,0.134033089691732,
17.0551487397923));
#270510=CARTESIAN_POINT('Ctrl Pts',(1.55027992016421,0.127496838124804,
17.054679265863));
#270511=CARTESIAN_POINT('Ctrl Pts',(1.55166370731226,0.109755356467329,
17.0534020490485));
#270512=CARTESIAN_POINT('Ctrl Pts',(1.55241601186724,0.0985444703630529,
17.0525918197777));
#270513=CARTESIAN_POINT('Ctrl Pts',(1.55556657379776,0.0425138312444026,
17.0485258351188));
#270514=CARTESIAN_POINT('Ctrl Pts',(1.55614535237466,-0.00238242058257087,
17.0452140644875));
#270515=CARTESIAN_POINT('Ctrl Pts',(1.55022249010626,-0.197330826533279,
17.0305862958485));
#270516=CARTESIAN_POINT('Ctrl Pts',(1.52395590129271,-0.345941650565378,
17.0186976790508));
#270517=CARTESIAN_POINT('Ctrl Pts',(1.46668625166107,-0.519087295236012,
17.0048794168187));
#270518=CARTESIAN_POINT('Ctrl Pts',(1.45560886776008,-0.549384554985741,
17.0024674184821));
#270519=CARTESIAN_POINT('Ctrl Pts',(1.44113246698195,-0.585458140215961,
16.9996200489091));
#270520=CARTESIAN_POINT('Ctrl Pts',(1.43862925210175,-0.591582539082508,
16.9991375067435));
#270521=CARTESIAN_POINT('Ctrl Pts',(1.43466771577604,-0.601101021765354,
16.9983891080523));
#270522=CARTESIAN_POINT('Ctrl Pts',(1.43323629207973,-0.604506099965401,
16.9981216945372));
#270523=CARTESIAN_POINT('Ctrl Pts',(1.43054879111752,-0.610835933435642,
16.9976252166475));
#270524=CARTESIAN_POINT('Ctrl Pts',(1.42929587756749,-0.613761904999399,
16.9973959751171));
#270525=CARTESIAN_POINT('Ctrl Pts',(1.42641331820236,-0.620436947642356,
16.9968735679961));
#270526=CARTESIAN_POINT('Ctrl Pts',(1.42477787000566,-0.624183452615307,
16.996580758669));
#270527=CARTESIAN_POINT('Ctrl Pts',(1.42046149163215,-0.633966104729296,
16.99581713422));
#270528=CARTESIAN_POINT('Ctrl Pts',(1.41775681636755,-0.639991785030695,
16.995347717012));
#270529=CARTESIAN_POINT('Ctrl Pts',(1.39894172088783,-0.681204805565765,
16.9921423413064));
#270530=CARTESIAN_POINT('Ctrl Pts',(1.38155974331485,-0.715801107936104,
16.9894777671423));
#270531=CARTESIAN_POINT('Ctrl Pts',(1.29103514846456,-0.880365057652797,
16.976757524794));
#270532=CARTESIAN_POINT('Ctrl Pts',(1.20075460499769,-1.00000449689836,
16.9672919631132));
#270533=CARTESIAN_POINT('Ctrl Pts',(1.07612343688604,-1.12349058272458,
16.9553656978949));
#270534=CARTESIAN_POINT('Ctrl Pts',(1.05696402724497,-1.14153390531805,
16.9535606220944));
#270535=CARTESIAN_POINT('Ctrl Pts',(1.0232478454372,-1.17170927270085,16.950422798444));
#270536=CARTESIAN_POINT('Ctrl Pts',(1.00890981438683,-1.18407757555334,
16.9490998309626));
#270537=CARTESIAN_POINT('Ctrl Pts',(0.988208376135252,-1.20128607833971,
16.9472035492496));
#270538=CARTESIAN_POINT('Ctrl Pts',(0.982027507472763,-1.20634406657612,
16.9466390822869));
#270539=CARTESIAN_POINT('Ctrl Pts',(0.971288221787149,-1.21499511349565,
16.9456610902617));
#270540=CARTESIAN_POINT('Ctrl Pts',(0.966748093993297,-1.21861070760625,
16.9452484782359));
#270541=CARTESIAN_POINT('Ctrl Pts',(0.958005463364686,-1.2254934175481,
16.9444554847823));
#270542=CARTESIAN_POINT('Ctrl Pts',(0.953806207871142,-1.22876454246446,
16.9440752703585));
#270543=CARTESIAN_POINT('Ctrl Pts',(0.94389513623882,-1.23640362556131,
16.9431794188314));
#270544=CARTESIAN_POINT('Ctrl Pts',(0.93816970111598,-1.24075362671324,
16.9426630849868));
#270545=CARTESIAN_POINT('Ctrl Pts',(0.918240942793458,-1.25567805275695,
16.9408697642755));
#270546=CARTESIAN_POINT('Ctrl Pts',(0.903887842906313,-1.26604917775412,
16.9395849603637));
#270547=CARTESIAN_POINT('Ctrl Pts',(0.78496497359218,-1.34892621341377,
16.9289901837927));
#270548=CARTESIAN_POINT('Ctrl Pts',(0.672056801019739,-1.40858009442183,
16.9191860684388));
#270549=CARTESIAN_POINT('Ctrl Pts',(0.504199142671074,-1.47245028350452,
16.9052594361015));
#270550=CARTESIAN_POINT('Ctrl Pts',(0.454306101138838,-1.48860107349504,
16.9012028041132));
#270551=CARTESIAN_POINT('Ctrl Pts',(0.368472821598813,-1.51166725673301,
16.8944448835673));
#270552=CARTESIAN_POINT('Ctrl Pts',(0.332929393732065,-1.51989100569227,
16.8917090163716));
#270553=CARTESIAN_POINT('Ctrl Pts',(0.290410768648681,-1.5281651227565,
16.888534291323));
#270554=CARTESIAN_POINT('Ctrl Pts',(0.283686466091494,-1.52942768726112,
16.8880351005877));
#270555=CARTESIAN_POINT('Ctrl Pts',(0.273271190817226,-1.53131221915521,
16.887266594048));
#270556=CARTESIAN_POINT('Ctrl Pts',(0.269586049045342,-1.53196528003321,
16.8869955864562));
#270557=CARTESIAN_POINT('Ctrl Pts',(0.262767579194244,-1.53314824699708,
16.8864958706089));
#270558=CARTESIAN_POINT('Ctrl Pts',(0.259635006466371,-1.53368184827483,
16.8862669634726));
#270559=CARTESIAN_POINT('Ctrl Pts',(0.252535145957948,-1.5348688593619,
16.8857496641785));
#270560=CARTESIAN_POINT('Ctrl Pts',(0.248566950899842,-1.5355164887707,
16.8854616008202));
#270561=CARTESIAN_POINT('Ctrl Pts',(0.238293718029,-1.53715226398202,16.884718473888));
#270562=CARTESIAN_POINT('Ctrl Pts',(0.231984947042247,-1.53811701985817,
16.8842646886189));
#270563=CARTESIAN_POINT('Ctrl Pts',(0.191740365933215,-1.54401809343218,
16.8813852305919));
#270564=CARTESIAN_POINT('Ctrl Pts',(0.15765191133053,-1.5478703322816,16.8790154595782));
#270565=CARTESIAN_POINT('Ctrl Pts',(0.103435768649945,-1.55218711416128,
16.8753158601897));
#270566=CARTESIAN_POINT('Ctrl Pts',(0.08338094353823,-1.55339353450533,
16.8739623380437));
#270567=CARTESIAN_POINT('Ctrl Pts',(-0.0197240895592042,-1.5575933109998,
16.8670553858614));
#270568=CARTESIAN_POINT('Ctrl Pts',(-0.102896028625891,-1.55431639394722,
16.861649172063));
#270569=CARTESIAN_POINT('Ctrl Pts',(-0.271201494249236,-1.53411086464129,
16.8504338057363));
#270570=CARTESIAN_POINT('Ctrl Pts',(-0.355972126701788,-1.51668284563349,
16.8446342439596));
#270571=CARTESIAN_POINT('Ctrl Pts',(-0.451075661100523,-1.48871534853524,
16.8377061688898));
#270572=CARTESIAN_POINT('Ctrl Pts',(-0.463256287901399,-1.48497011273172,
16.836810916571));
#270573=CARTESIAN_POINT('Ctrl Pts',(-0.481880793068728,-1.47899210053651,
16.8354292044706));
#270574=CARTESIAN_POINT('Ctrl Pts',(-0.488358509778034,-1.47686583528251,
16.8349462325171));
#270575=CARTESIAN_POINT('Ctrl Pts',(-0.50013819919708,-1.4729132616241,
16.8340634590291));
#270576=CARTESIAN_POINT('Ctrl Pts',(-0.505444702032444,-1.47110072606917,
16.8336641171281));
#270577=CARTESIAN_POINT('Ctrl Pts',(-0.517007306063693,-1.46708135555474,
16.8327902559369));
#270578=CARTESIAN_POINT('Ctrl Pts',(-0.52325929717968,-1.46486312115931,
16.8323153657752));
#270579=CARTESIAN_POINT('Ctrl Pts',(-0.540367899222976,-1.45866941171774,
16.8310091537131));
#270580=CARTESIAN_POINT('Ctrl Pts',(-0.551194482331632,-1.45461285172834,
16.830175153005));
#270581=CARTESIAN_POINT('Ctrl Pts',(-0.608004639160203,-1.43260163452344,
16.8257587722325));
#270582=CARTESIAN_POINT('Ctrl Pts',(-0.653154387550186,-1.41258820270241,
16.8221080483415));
#270583=CARTESIAN_POINT('Ctrl Pts',(-0.82774098791286,-1.32503877398737,
16.807410148088));
#270584=CARTESIAN_POINT('Ctrl Pts',(-0.948328741761421,-1.24159000017251,
16.7958582314524));
#270585=CARTESIAN_POINT('Ctrl Pts',(-1.07861014055851,-1.12123555442892,
16.782428785693));
#270586=CARTESIAN_POINT('Ctrl Pts',(-1.10105712124808,-1.09920088172291,
16.7800782784836));
#270587=CARTESIAN_POINT('Ctrl Pts',(-1.12736840889186,-1.07175737356725,
16.7772935629172));
#270588=CARTESIAN_POINT('Ctrl Pts',(-1.13188433666563,-1.06698699603247,
16.7768145139129));
#270589=CARTESIAN_POINT('Ctrl Pts',(-1.13888521816745,-1.05949718112267,
16.7760703398128));
#270590=CARTESIAN_POINT('Ctrl Pts',(-1.14139088962725,-1.05679735749544,
16.775803685409));
#270591=CARTESIAN_POINT('Ctrl Pts',(-1.14604487670847,-1.05174689481779,
16.7753078715292));
#270592=CARTESIAN_POINT('Ctrl Pts',(-1.14819554348618,-1.04939858224281,
16.7750785395331));
#270593=CARTESIAN_POINT('Ctrl Pts',(-1.15310087881565,-1.0440093141107,
16.7745549638485));
#270594=CARTESIAN_POINT('Ctrl Pts',(-1.15585073639902,-1.04096405359845,
16.7742610826111));
#270595=CARTESIAN_POINT('Ctrl Pts',(-1.16302928511924,-1.03295083356297,
16.7734928055837));
#270596=CARTESIAN_POINT('Ctrl Pts',(-1.1674382613916,-1.02796520010947,
16.7730198355505));
#270597=CARTESIAN_POINT('Ctrl Pts',(-1.19792797539884,-0.993038502859575,
16.769740032826));
#270598=CARTESIAN_POINT('Ctrl Pts',(-1.22288862889438,-0.962133552808118,
16.7670083772452));
#270599=CARTESIAN_POINT('Ctrl Pts',(-1.33664116407618,-0.809700973999434,
16.7541392857221));
#270600=CARTESIAN_POINT('Ctrl Pts',(-1.40866637824048,-0.676675914152685,
16.7445884700309));
#270601=CARTESIAN_POINT('Ctrl Pts',(-1.47345893538007,-0.499924124621506,
16.7317693357119));
#270602=CARTESIAN_POINT('Ctrl Pts',(-1.48515627741034,-0.464021334520767,
16.7291646076415));
#270603=CARTESIAN_POINT('Ctrl Pts',(-1.49836959416402,-0.417821773003317,
16.7257940241061));
#270604=CARTESIAN_POINT('Ctrl Pts',(-1.50110506510699,-0.407884847873317,
16.7250679959893));
#270605=CARTESIAN_POINT('Ctrl Pts',(-1.50535046715196,-0.391841521636461,
16.7238937687649));
#270606=CARTESIAN_POINT('Ctrl Pts',(-1.50692249265256,-0.385751741484423,
16.7234475809426));
#270607=CARTESIAN_POINT('Ctrl Pts',(-1.50984989893882,-0.374120404957784,
16.7225943955109));
#270608=CARTESIAN_POINT('Ctrl Pts',(-1.51121181353593,-0.368580585173296,
16.7221876160121));
#270609=CARTESIAN_POINT('Ctrl Pts',(-1.5142585999138,-0.3558864495967,16.7212544800439));
#270610=CARTESIAN_POINT('Ctrl Pts',(-1.51592328743781,-0.348727480400935,
16.7207274853312));
#270611=CARTESIAN_POINT('Ctrl Pts',(-1.52014502174021,-0.329970327526181,
16.7193446260913));
#270612=CARTESIAN_POINT('Ctrl Pts',(-1.5226200371931,-0.318354381078791,
16.7184861669611));
#270613=CARTESIAN_POINT('Ctrl Pts',(-1.54536881320966,-0.205248058170481,
16.710105289614));
#270614=CARTESIAN_POINT('Ctrl Pts',(-1.55559463716222,-0.102022711011283,
16.7022588051956));
#270615=CARTESIAN_POINT('Ctrl Pts',(-1.55539500295535,0.114702355763758,
16.6855071832301));
#270616=CARTESIAN_POINT('Ctrl Pts',(-1.54291906605899,0.227629022166531,
16.6766211945832));
#270617=CARTESIAN_POINT('Ctrl Pts',(-1.51586821381248,0.349066783705029,
16.6674237523592));
#270618=CARTESIAN_POINT('Ctrl Pts',(-1.51333234485893,0.359901784005148,
16.6666066131679));
#270619=CARTESIAN_POINT('Ctrl Pts',(-1.50967322038962,0.374813120533336,
16.6654877136615));
#270620=CARTESIAN_POINT('Ctrl Pts',(-1.50864937693395,0.378913138187209,
16.6651806549299));
#270621=CARTESIAN_POINT('Ctrl Pts',(-1.50686564642258,0.385934299246099,
16.6646559031947));
#270622=CARTESIAN_POINT('Ctrl Pts',(-1.50611395011581,0.388857466683658,
16.6644377506967));
#270623=CARTESIAN_POINT('Ctrl Pts',(-1.50453193483721,0.394936138309345,
16.663984801268));
#270624=CARTESIAN_POINT('Ctrl Pts',(-1.50370019119181,0.39809123523306,
16.6637500945618));
#270625=CARTESIAN_POINT('Ctrl Pts',(-1.50166427583753,0.405716757071498,
16.663183738763));
#270626=CARTESIAN_POINT('Ctrl Pts',(-1.50045004779117,0.41018451928302,
16.662852665635));
#270627=CARTESIAN_POINT('Ctrl Pts',(-1.49612362863004,0.425827314932196,
16.6616959145881));
#270628=CARTESIAN_POINT('Ctrl Pts',(-1.49290629471815,0.436973260888894,
16.6608760381759));
#270629=CARTESIAN_POINT('Ctrl Pts',(-1.47250438771779,0.504795476639918,
16.6559077510363));
#270630=CARTESIAN_POINT('Ctrl Pts',(-1.45221710042606,0.560495240825511,
16.6519149120071));
#270631=CARTESIAN_POINT('Ctrl Pts',(-1.40607871372675,0.667702278374972,
16.6441561599367));
#270632=CARTESIAN_POINT('Ctrl Pts',(-1.38044884964969,0.719197440059563,
16.6403926960556));
#270633=CARTESIAN_POINT('Ctrl Pts',(-1.34613548323605,0.779513621113158,
16.6358182669723));
#270634=CARTESIAN_POINT('Ctrl Pts',(-1.34012488293191,0.789802202578729,
16.6350319409928));
#270635=CARTESIAN_POINT('Ctrl Pts',(-1.2889156826116,0.875191130038503,
16.6284486981176));
#270636=CARTESIAN_POINT('Ctrl Pts',(-1.23756866300656,0.946405567453251,
16.6225729910319));
#270637=CARTESIAN_POINT('Ctrl Pts',(-1.17275402907612,1.02194416898097,
16.6156213096609));
#270638=CARTESIAN_POINT('Ctrl Pts',(-1.1649007450776,1.03088706342611,16.614786034343));
#270639=CARTESIAN_POINT('Ctrl Pts',(-1.15202788055219,1.04521105261589,
16.6134275341423));
#270640=CARTESIAN_POINT('Ctrl Pts',(-1.14707127330378,1.05064831065563,
16.6129069391673));
#270641=CARTESIAN_POINT('Ctrl Pts',(-1.13820265226072,1.0602393728886,16.6119797157614));
#270642=CARTESIAN_POINT('Ctrl Pts',(-1.13430597700229,1.06440723146045,
16.611573743941));
#270643=CARTESIAN_POINT('Ctrl Pts',(-1.1260686182145,1.07312125388745,16.6107184652592));
#270644=CARTESIAN_POINT('Ctrl Pts',(-1.12172314282997,1.07766272421838,
16.6102689562537));
#270645=CARTESIAN_POINT('Ctrl Pts',(-1.11019213510238,1.08956850966515,
16.6090804571449));
#270646=CARTESIAN_POINT('Ctrl Pts',(-1.1029609595622,1.09688797346021,16.6083394846244));
#270647=CARTESIAN_POINT('Ctrl Pts',(-1.06899859592078,1.13058958667524,
16.6048787703327));
#270648=CARTESIAN_POINT('Ctrl Pts',(-1.04139229346829,1.15606766786562,
16.6021202771157));
#270649=CARTESIAN_POINT('Ctrl Pts',(-0.898566181413095,1.27861333074479,
16.5880986431829));
#270650=CARTESIAN_POINT('Ctrl Pts',(-0.770600720303237,1.35957076732516,
16.5762068811241));
#270651=CARTESIAN_POINT('Ctrl Pts',(-0.596693210522621,1.43705293595673,
16.5616879313495));
#270652=CARTESIAN_POINT('Ctrl Pts',(-0.559730291076118,1.45184937140861,
16.5586935816575));
#270653=CARTESIAN_POINT('Ctrl Pts',(-0.515964199725549,1.46744864940867,
16.5552841035713));
#270654=CARTESIAN_POINT('Ctrl Pts',(-0.5096771450536,1.46964410865359,16.5547975507935));
#270655=CARTESIAN_POINT('Ctrl Pts',(-0.4994927147271,1.47312732718678,16.5540147946011));
#270656=CARTESIAN_POINT('Ctrl Pts',(-0.49560409132311,1.47444012421066,
16.5537171915272));
#270657=CARTESIAN_POINT('Ctrl Pts',(-0.488689114795489,1.4767441686675,
16.5531902834324));
#270658=CARTESIAN_POINT('Ctrl Pts',(-0.485664872710304,1.47774152771564,
16.5529606258042));
#270659=CARTESIAN_POINT('Ctrl Pts',(-0.47913668864465,1.4798722393654,16.5524665811086));
#270660=CARTESIAN_POINT('Ctrl Pts',(-0.475631782245464,1.48100243744932,
16.5522023794871));
#270661=CARTESIAN_POINT('Ctrl Pts',(-0.465867457944091,1.48411281985807,
16.5514691577558));
#270662=CARTESIAN_POINT('Ctrl Pts',(-0.45959936930184,1.48606587144153,
16.5510016896542));
#270663=CARTESIAN_POINT('Ctrl Pts',(-0.423296203274179,1.49712577940899,
16.5483117503545));
#270664=CARTESIAN_POINT('Ctrl Pts',(-0.393000756460136,1.50536242681236,
16.5461360464508));
#270665=CARTESIAN_POINT('Ctrl Pts',(-0.220541367577036,1.54668787780174,
16.5340284524399));
#270666=CARTESIAN_POINT('Ctrl Pts',(-0.0745197199249979,1.56055669520138,
16.5247666406067));
#270667=CARTESIAN_POINT('Ctrl Pts',(0.120650740593084,1.55160033741761,
16.5115900508908));
#270668=CARTESIAN_POINT('Ctrl Pts',(0.169854034310815,1.54698706618201,
16.5082072384773));
#270669=CARTESIAN_POINT('Ctrl Pts',(0.230199618560858,1.53841545335448,
16.5039410627464));
#270670=CARTESIAN_POINT('Ctrl Pts',(0.241629728667893,1.53666165207661,
16.5031278275039));
#270671=CARTESIAN_POINT('Ctrl Pts',(0.25958497877861,1.53370137379655,16.5018416961694));
#270672=CARTESIAN_POINT('Ctrl Pts',(0.266123937588478,1.53258027932054,
16.5013715016191));
#270673=CARTESIAN_POINT('Ctrl Pts',(0.278176142391241,1.53043448998946,
16.5005014308093));
#270674=CARTESIAN_POINT('Ctrl Pts',(0.283691428426807,1.52942174244735,
16.5001019399123));
#270675=CARTESIAN_POINT('Ctrl Pts',(0.295899394574699,1.52711174199839,
16.4992146594712));
#270676=CARTESIAN_POINT('Ctrl Pts',(0.302589231843184,1.52580027470608,
16.4987264250012));
#270677=CARTESIAN_POINT('Ctrl Pts',(0.321756296771107,1.52191177681647,
16.4973216715952));
#270678=CARTESIAN_POINT('Ctrl Pts',(0.334210508786813,1.51922542394985,
16.4964016910652));
#270679=CARTESIAN_POINT('Ctrl Pts',(0.430754504023246,1.4971564831268,16.4892120874183));
#270680=CARTESIAN_POINT('Ctrl Pts',(0.513117067217718,1.47096325188963,
16.4827224524802));
#270681=CARTESIAN_POINT('Ctrl Pts',(0.667557380823319,1.40729297229781,
16.4698865239128));
#270682=CARTESIAN_POINT('Ctrl Pts',(0.739728905204007,1.3707322643646,16.4635786113087));
#270683=CARTESIAN_POINT('Ctrl Pts',(0.856058764237086,1.29992809980425,
16.4530988785788));
#270684=CARTESIAN_POINT('Ctrl Pts',(0.901817872054727,1.26861173610823,
16.4488881690252));
#270685=CARTESIAN_POINT('Ctrl Pts',(0.952044217633804,1.23014375657088,
16.4442403209255));
#270686=CARTESIAN_POINT('Ctrl Pts',(0.958239394602735,1.2253240892562,16.4436665799035));
#270687=CARTESIAN_POINT('Ctrl Pts',(0.967541105962813,1.21797393486456,
16.4428047823928));
#270688=CARTESIAN_POINT('Ctrl Pts',(0.970674657794897,1.21547809829273,
16.442514398903));
#270689=CARTESIAN_POINT('Ctrl Pts',(0.976275803966315,1.21098137740805,
16.4419952867025));
#270690=CARTESIAN_POINT('Ctrl Pts',(0.978746931192432,1.20898502354244,
16.4417662463225));
#270691=CARTESIAN_POINT('Ctrl Pts',(0.984124807308284,1.20461309361595,
16.4412677552552));
#270692=CARTESIAN_POINT('Ctrl Pts',(0.987029074315152,1.20223456485563,
16.4409985215179));
#270693=CARTESIAN_POINT('Ctrl Pts',(0.995242888944374,1.19545781046219,
16.4402369015307));
#270694=CARTESIAN_POINT('Ctrl Pts',(1.00053193537072,1.19103469118462,16.4397462683783));
#270695=CARTESIAN_POINT('Ctrl Pts',(1.03444744237669,1.16228649729511,16.4365974357485));
#270696=CARTESIAN_POINT('Ctrl Pts',(1.06221705469526,1.13696390578309,16.4340066660361));
#270697=CARTESIAN_POINT('Ctrl Pts',(1.16537743360218,1.03581098158832,16.4242054798981));
#270698=CARTESIAN_POINT('Ctrl Pts',(1.23379573212081,0.953289370161784,
16.4173027414172));
#270699=CARTESIAN_POINT('Ctrl Pts',(1.337243725789,0.798522168580856,16.4049566985637));
#270700=CARTESIAN_POINT('Ctrl Pts',(1.37617118222644,0.729389158769463,
16.3996201717271));
#270701=CARTESIAN_POINT('Ctrl Pts',(1.41463274000653,0.646941084534134,
16.3932646970309));
#270702=CARTESIAN_POINT('Ctrl Pts',(1.41948336477519,0.636227569154962,
16.392439198595));
#270703=CARTESIAN_POINT('Ctrl Pts',(1.42715333419177,0.618762573683803,
16.3910935038768));
#270704=CARTESIAN_POINT('Ctrl Pts',(1.43004740958704,0.612044250784941,
16.3905758562236));
#270705=CARTESIAN_POINT('Ctrl Pts',(1.43345671918452,0.603973654829153,
16.3899539384062));
#270706=CARTESIAN_POINT('Ctrl Pts',(1.434017632541,0.602640664929218,16.3898512160938));
#270707=CARTESIAN_POINT('Ctrl Pts',(1.43457668357428,0.601306900796103,
16.3897484311226));
#270708=CARTESIAN_POINT('',(-1.55550041526741,0.000134513367580657,16.5574036059057));
#270709=CARTESIAN_POINT('Ctrl Pts',(1.43457653793677,0.601307248252799,
16.2500928067243));
#270710=CARTESIAN_POINT('Ctrl Pts',(1.40375589294166,0.674838000330927,
16.2553442444805));
#270711=CARTESIAN_POINT('Ctrl Pts',(1.3672790165716,0.746006945298649,16.2606305819942));
#270712=CARTESIAN_POINT('Ctrl Pts',(1.32228285271093,0.819258241307971,
16.2665149389514));
#270713=CARTESIAN_POINT('Ctrl Pts',(1.31912362583802,0.824335409140046,
16.2669251564596));
#270714=CARTESIAN_POINT('Ctrl Pts',(1.31502854246759,0.830832759401978,
16.2674532434056));
#270715=CARTESIAN_POINT('Ctrl Pts',(1.31411949431617,0.83226984579663,16.2675702432442));
#270716=CARTESIAN_POINT('Ctrl Pts',(1.29971672369564,0.854956317759878,
16.2694203970959));
#270717=CARTESIAN_POINT('Ctrl Pts',(1.28571221442915,0.875875473284353,
16.271170144239));
#270718=CARTESIAN_POINT('Ctrl Pts',(1.2658554292215,0.90403346813135,16.2735913319866));
#270719=CARTESIAN_POINT('Ctrl Pts',(1.2604361248971,0.911574049415152,16.2742463743444));
#270720=CARTESIAN_POINT('Ctrl Pts',(1.25169623176006,0.923508048038257,
16.2752939852326));
#270721=CARTESIAN_POINT('Ctrl Pts',(1.24841920170457,0.927933223238932,
16.27568486899));
#270722=CARTESIAN_POINT('Ctrl Pts',(1.24163876797836,0.936988329373549,
16.2764897828329));
#270723=CARTESIAN_POINT('Ctrl Pts',(1.23813280443094,0.941616225668033,
16.2769039085194));
#270724=CARTESIAN_POINT('Ctrl Pts',(1.22994782061302,0.952295711886498,
16.2778660258924));
#270725=CARTESIAN_POINT('Ctrl Pts',(1.22524994015833,0.958332585576827,
16.2784147546055));
#270726=CARTESIAN_POINT('Ctrl Pts',(1.21016541601565,0.977424280486823,
16.2801658708772));
#270727=CARTESIAN_POINT('Ctrl Pts',(1.19961351132416,0.99034637445705,16.2813748125574));
#270728=CARTESIAN_POINT('Ctrl Pts',(1.14531153710402,1.05470437279876,16.2875194427389));
#270729=CARTESIAN_POINT('Ctrl Pts',(1.09845911430131,1.10341515587118,16.2925812292881));
#270730=CARTESIAN_POINT('Ctrl Pts',(0.975081264765485,1.21601944539658,
16.3053435603302));
#270731=CARTESIAN_POINT('Ctrl Pts',(0.895300707009709,1.27590033556052,
16.313138458457));
#270732=CARTESIAN_POINT('Ctrl Pts',(0.795860468760591,1.33659062846146,
16.322075392268));
#270733=CARTESIAN_POINT('Ctrl Pts',(0.781226830362618,1.34519629397978,
16.3233718038171));
#270734=CARTESIAN_POINT('Ctrl Pts',(0.737317315515137,1.37006008694333,
16.327201053015));
#270735=CARTESIAN_POINT('Ctrl Pts',(0.707651817970889,1.38561567217687,
16.3297094558764));
#270736=CARTESIAN_POINT('Ctrl Pts',(0.671753476962848,1.40298550796603,
16.3326338633877));
#270737=CARTESIAN_POINT('Ctrl Pts',(0.665985111905587,1.40573287072954,
16.3331004309786));
#270738=CARTESIAN_POINT('Ctrl Pts',(0.656533633349744,1.41016319365411,
16.3338592634462));
#270739=CARTESIAN_POINT('Ctrl Pts',(0.652860662763911,1.41186741604147,
16.3341527735727));
#270740=CARTESIAN_POINT('Ctrl Pts',(0.646257550609289,1.41489991786983,
16.3346779033301));
#270741=CARTESIAN_POINT('Ctrl Pts',(0.643329919531836,1.41623346048127,
16.3349098386584));
#270742=CARTESIAN_POINT('Ctrl Pts',(0.636924512140874,1.41912717681864,
16.3354153437078));
#270743=CARTESIAN_POINT('Ctrl Pts',(0.633445136290934,1.42068365173367,
16.3356886870629));
#270744=CARTESIAN_POINT('Ctrl Pts',(0.623532948312553,1.42507414682746,
16.3364639661754));
#270745=CARTESIAN_POINT('Ctrl Pts',(0.617086487388842,1.42787742248762,
16.336964076607));
#270746=CARTESIAN_POINT('Ctrl Pts',(0.574601452153752,1.44601078457249,
16.3402346133114));
#270747=CARTESIAN_POINT('Ctrl Pts',(0.538010166588153,1.46002045463908,
16.3429318510077));
#270748=CARTESIAN_POINT('Ctrl Pts',(0.389271906533926,1.51061462838705,
16.3535731808969));
#270749=CARTESIAN_POINT('Ctrl Pts',(0.273655694459271,1.53577529529139,
16.3611522460564));
#270750=CARTESIAN_POINT('Ctrl Pts',(0.0898508929878587,1.55433829059288,
16.3734765024534));
#270751=CARTESIAN_POINT('Ctrl Pts',(0.0230473944813672,1.55676192536714,
16.3780054870758));
#270752=CARTESIAN_POINT('Ctrl Pts',(-0.0551838605018441,1.55456328063912,
16.3834750801024));
#270753=CARTESIAN_POINT('Ctrl Pts',(-0.0666643294699243,1.55411328631946,
16.3842818128188));
#270754=CARTESIAN_POINT('Ctrl Pts',(-0.0854103796816846,1.55317041277752,
16.3856062523885));
#270755=CARTESIAN_POINT('Ctrl Pts',(-0.0926794929868463,1.55275360969185,
16.3861215861844));
#270756=CARTESIAN_POINT('Ctrl Pts',(-0.105692655121872,1.55191574566971,
16.3870474109874));
#270757=CARTESIAN_POINT('Ctrl Pts',(-0.111437837002576,1.55151378526135,
16.3874572978031));
#270758=CARTESIAN_POINT('Ctrl Pts',(-0.123624618541308,1.55059310145363,
16.3883292511753));
#270759=CARTESIAN_POINT('Ctrl Pts',(-0.130065465214612,1.55006612278847,
16.3887915686556));
#270760=CARTESIAN_POINT('Ctrl Pts',(-0.147319935784709,1.54854609426637,
16.3900341510085));
#270761=CARTESIAN_POINT('Ctrl Pts',(-0.158126581764484,1.54747993285136,
16.3908166888547));
#270762=CARTESIAN_POINT('Ctrl Pts',(-0.211983531035931,1.54159649394849,
16.3947388239744));
#270763=CARTESIAN_POINT('Ctrl Pts',(-0.254826497700319,1.53509593843784,
16.3979305804161));
#270764=CARTESIAN_POINT('Ctrl Pts',(-0.463972099294807,1.49436604351247,
16.4138826266288));
#270765=CARTESIAN_POINT('Ctrl Pts',(-0.624130871568306,1.4348673470839,
16.4274299238938));
#270766=CARTESIAN_POINT('Ctrl Pts',(-0.786332168583866,1.34221969835758,
16.4413616221168));
#270767=CARTESIAN_POINT('Ctrl Pts',(-0.801024131977854,1.33350380681095,
16.4426240225975));
#270768=CARTESIAN_POINT('Ctrl Pts',(-0.820256344781417,1.32166185643422,
16.444274295303));
#270769=CARTESIAN_POINT('Ctrl Pts',(-0.824927107367844,1.31875160811054,
16.4446749039408));
#270770=CARTESIAN_POINT('Ctrl Pts',(-0.832505625629978,1.31397358232262,
16.4453244940857));
#270771=CARTESIAN_POINT('Ctrl Pts',(-0.835422720002956,1.31212082952986,
16.4455744309721));
#270772=CARTESIAN_POINT('Ctrl Pts',(-0.84103537413148,1.30852972334829,
16.4460550923816));
#270773=CARTESIAN_POINT('Ctrl Pts',(-0.843731742235814,1.30679274744793,
16.4462858982283));
#270774=CARTESIAN_POINT('Ctrl Pts',(-0.849143965876476,1.30328250782357,
16.4467489946652));
#270775=CARTESIAN_POINT('Ctrl Pts',(-0.851859693212711,1.30150906012126,
16.4469812733594));
#270776=CARTESIAN_POINT('Ctrl Pts',(-0.861273974911252,1.29531917488499,
16.4477862390695));
#270777=CARTESIAN_POINT('Ctrl Pts',(-0.867944048445492,1.29085931098709,
16.4483561267084));
#270778=CARTESIAN_POINT('Ctrl Pts',(-0.946266740737118,1.23760822646027,
16.4550466516388));
#270779=CARTESIAN_POINT('Ctrl Pts',(-1.01376677756615,1.18295257977444,
16.4608037035514));
#270780=CARTESIAN_POINT('Ctrl Pts',(-1.16823942158121,1.03488728743512,
16.474914989481));
#270781=CARTESIAN_POINT('Ctrl Pts',(-1.2489451727583,0.935898778966701,
16.4832070053746));
#270782=CARTESIAN_POINT('Ctrl Pts',(-1.32614104473809,0.813169809459138,
16.4932710172997));
#270783=CARTESIAN_POINT('Ctrl Pts',(-1.33533196633021,0.797987283337744,
16.4945116056877));
#270784=CARTESIAN_POINT('Ctrl Pts',(-1.34790840246709,0.776386336854409,
16.4962722362941));
#270785=CARTESIAN_POINT('Ctrl Pts',(-1.35151210513657,0.770095988803044,
16.4967844230542));
#270786=CARTESIAN_POINT('Ctrl Pts',(-1.3577147769389,0.759091437493524,
16.4976796780455));
#270787=CARTESIAN_POINT('Ctrl Pts',(-1.3603335127657,0.754388466715651,
16.4980620328953));
#270788=CARTESIAN_POINT('Ctrl Pts',(-1.36576433631322,0.744515055892219,
16.4988642878019));
#270789=CARTESIAN_POINT('Ctrl Pts',(-1.36857158905733,0.739342068780553,
16.4992843519822));
#270790=CARTESIAN_POINT('Ctrl Pts',(-1.37518653562031,0.726985790614702,
16.5002871749432));
#270791=CARTESIAN_POINT('Ctrl Pts',(-1.37896736907099,0.719788397998064,
16.5008708699764));
#270792=CARTESIAN_POINT('Ctrl Pts',(-1.39159306338327,0.695288852579852,
16.5028564974421));
#270793=CARTESIAN_POINT('Ctrl Pts',(-1.40016974301459,0.677851362622899,
16.5042677101531));
#270794=CARTESIAN_POINT('Ctrl Pts',(-1.41993378502312,0.635692092658565,
16.5076763978822));
#270795=CARTESIAN_POINT('Ctrl Pts',(-1.43080497558965,0.61083004732621,
16.5096839985814));
#270796=CARTESIAN_POINT('Ctrl Pts',(-1.49703028996313,0.447892783368919,
16.522828012903));
#270797=CARTESIAN_POINT('Ctrl Pts',(-1.53297886410841,0.302770674755422,
16.5345787089787));
#270798=CARTESIAN_POINT('Ctrl Pts',(-1.54793564095542,0.153225353892046,
16.5460196773578));
#270799=CARTESIAN_POINT('Ctrl Pts',(-1.54809082728922,0.151649425026329,
16.5461401588464));
#270800=CARTESIAN_POINT('Ctrl Pts',(-1.54980250097743,0.133990796826681,
16.5474892108777));
#270801=CARTESIAN_POINT('Ctrl Pts',(-1.5511107748881,0.117884391851123,
16.5487106811146));
#270802=CARTESIAN_POINT('Ctrl Pts',(-1.55359029641752,0.0800636724071525,
16.5515538065943));
#270803=CARTESIAN_POINT('Ctrl Pts',(-1.55455773496866,0.0583384735902952,
16.553167623083));
#270804=CARTESIAN_POINT('Ctrl Pts',(-1.5552111032702,0.0305770339096044,
16.5551994321998));
#270805=CARTESIAN_POINT('Ctrl Pts',(-1.55531784954197,0.0245544462477771,
16.5556383875253));
#270806=CARTESIAN_POINT('Ctrl Pts',(-1.55543223145612,0.014953995409549,
16.5563350456703));
#270807=CARTESIAN_POINT('Ctrl Pts',(-1.55546251112997,0.0113765461869869,
16.5565939646384));
#270808=CARTESIAN_POINT('Ctrl Pts',(-1.55549071071321,0.00575223046998475,
16.5569999255921));
#270809=CARTESIAN_POINT('Ctrl Pts',(-1.55549693308948,0.00370547598347781,
16.5571474292398));
#270810=CARTESIAN_POINT('Ctrl Pts',(-1.555499657428,0.00115060015537671,
16.5573312652292));
#270811=CARTESIAN_POINT('Ctrl Pts',(-1.55549995027406,0.000642525155756949,
16.5573678096748));
#270812=CARTESIAN_POINT('Ctrl Pts',(-1.55549999418946,0.000134449200880738,
16.5574043402006));
#270813=CARTESIAN_POINT('Ctrl Pts',(-1.5554999941794,0.000134565524924873,
16.557404331837));
#270814=CARTESIAN_POINT('Ctrl Pts',(-1.55550005631452,-0.000583680669580982,
16.5574559735501));
#270815=CARTESIAN_POINT('Ctrl Pts',(-1.55549962097871,-0.00130192819956115,
16.5575075874042));
#270816=CARTESIAN_POINT('Ctrl Pts',(-1.55549439591342,-0.00532513151133239,
16.5577965427963));
#270817=CARTESIAN_POINT('Ctrl Pts',(-1.55547957060547,-0.00863010535305416,
16.5580333263913));
#270818=CARTESIAN_POINT('Ctrl Pts',(-1.55539859988764,-0.0191827435514825,
16.5587875644079));
#270819=CARTESIAN_POINT('Ctrl Pts',(-1.55529233098782,-0.0264301491038218,
16.559302850863));
#270820=CARTESIAN_POINT('Ctrl Pts',(-1.55430327163282,-0.0721032610949992,
16.5625345873586));
#270821=CARTESIAN_POINT('Ctrl Pts',(-1.55204708527963,-0.11048980600777,
16.565181236402));
#270822=CARTESIAN_POINT('Ctrl Pts',(-1.53402892344551,-0.298035761655428,
16.5779439561759));
#270823=CARTESIAN_POINT('Ctrl Pts',(-1.49817646609508,-0.444458831348207,
16.587461995549));
#270824=CARTESIAN_POINT('Ctrl Pts',(-1.4272635103738,-0.619697063958071,
16.6003204069466));
#270825=CARTESIAN_POINT('Ctrl Pts',(-1.41125605076399,-0.655333122806546,
16.603012879769));
#270826=CARTESIAN_POINT('Ctrl Pts',(-1.38926318635584,-0.699741687877563,
16.6064880075852));
#270827=CARTESIAN_POINT('Ctrl Pts',(-1.38450539084191,-0.709108908298952,
16.607227952405));
#270828=CARTESIAN_POINT('Ctrl Pts',(-1.37670433675246,-0.724089899864763,
16.6084229002773));
#270829=CARTESIAN_POINT('Ctrl Pts',(-1.37372070382062,-0.729734499394515,
16.6088758053203));
#270830=CARTESIAN_POINT('Ctrl Pts',(-1.36797248394207,-0.740449106850769,
16.6097406934233));
#270831=CARTESIAN_POINT('Ctrl Pts',(-1.36521424190891,-0.745522413275524,
16.6101524461245));
#270832=CARTESIAN_POINT('Ctrl Pts',(-1.35884855105654,-0.757077200767418,
16.6110954242065));
#270833=CARTESIAN_POINT('Ctrl Pts',(-1.35522288469019,-0.763548428007948,
16.6116272928666));
#270834=CARTESIAN_POINT('Ctrl Pts',(-1.34563932637681,-0.780370220919685,
16.613019858976));
#270835=CARTESIAN_POINT('Ctrl Pts',(-1.33960837148295,-0.790678363595692,
16.613883165057));
#270836=CARTESIAN_POINT('Ctrl Pts',(-1.28085517119875,-0.888497652019422,
16.6221730921203));
#270837=CARTESIAN_POINT('Ctrl Pts',(-1.21976152713595,-0.970665722630313,
16.6299145302193));
#270838=CARTESIAN_POINT('Ctrl Pts',(-1.10228510645782,-1.09991301332591,
16.6434092977767));
#270839=CARTESIAN_POINT('Ctrl Pts',(-1.04980530641377,-1.1501087559358,
16.6490656360401));
#270840=CARTESIAN_POINT('Ctrl Pts',(-0.969187023403972,-1.21708610632094,
16.6570963760611));
#270841=CARTESIAN_POINT('Ctrl Pts',(-0.943722108275766,-1.23693611598278,
16.6595472649625));
#270842=CARTESIAN_POINT('Ctrl Pts',(-0.907554751915153,-1.26336104618176,
16.662893468804));
#270843=CARTESIAN_POINT('Ctrl Pts',(-0.897364204209617,-1.27061964019404,
16.6638220292012));
#270844=CARTESIAN_POINT('Ctrl Pts',(-0.879498454045766,-1.28302301490749,
16.6654238787073));
#270845=CARTESIAN_POINT('Ctrl Pts',(-0.871863075041391,-1.28822372938218,
16.6661003608773));
#270846=CARTESIAN_POINT('Ctrl Pts',(-0.86137966774159,-1.29522842525874,
16.6670176914443));
#270847=CARTESIAN_POINT('Ctrl Pts',(-0.858571652746082,-1.29709148608409,
16.6672622886862));
#270848=CARTESIAN_POINT('Ctrl Pts',(-0.853245960579193,-1.30060010259783,
16.6677240583768));
#270849=CARTESIAN_POINT('Ctrl Pts',(-0.850729527833492,-1.30224750605124,
16.6679413518457));
#270850=CARTESIAN_POINT('Ctrl Pts',(-0.845528973077091,-1.30563058420997,
16.6683885473436));
#270851=CARTESIAN_POINT('Ctrl Pts',(-0.842844250581885,-1.30736530335068,
16.6686183826911));
#270852=CARTESIAN_POINT('Ctrl Pts',(-0.836231292345833,-1.31160939429937,
16.6691820470341));
#270853=CARTESIAN_POINT('Ctrl Pts',(-0.832297047013893,-1.31410943400867,
16.6695152624206));
#270854=CARTESIAN_POINT('Ctrl Pts',(-0.818824551861958,-1.32258583676254,
16.6706493115965));
#270855=CARTESIAN_POINT('Ctrl Pts',(-0.8092324042918,-1.3284765250317,16.671444780997));
#270856=CARTESIAN_POINT('Ctrl Pts',(-0.704420550919519,-1.39128658470135,
16.6800176144275));
#270857=CARTESIAN_POINT('Ctrl Pts',(-0.603420639387468,-1.43797721376659,
16.6872345086983));
#270858=CARTESIAN_POINT('Ctrl Pts',(-0.401632461431591,-1.50621520461431,
16.7012649782695));
#270859=CARTESIAN_POINT('Ctrl Pts',(-0.302000648323582,-1.5293083800525,
16.7080346195901));
#270860=CARTESIAN_POINT('Ctrl Pts',(-0.185652149056219,-1.54445715874957,
16.7162067707985));
#270861=CARTESIAN_POINT('Ctrl Pts',(-0.170442768572791,-1.54620951657286,
16.7172796966736));
#270862=CARTESIAN_POINT('Ctrl Pts',(-0.147857038815427,-1.54847446304233,
16.7188809667008));
#270863=CARTESIAN_POINT('Ctrl Pts',(-0.14049857011486,-1.54915945435491,
16.7194039147117));
#270864=CARTESIAN_POINT('Ctrl Pts',(-0.127385429832946,-1.55028594487522,
16.7203381890206));
#270865=CARTESIAN_POINT('Ctrl Pts',(-0.121632614303835,-1.55074790475653,
16.7207488671424));
#270866=CARTESIAN_POINT('Ctrl Pts',(-0.109495750635575,-1.5516545632689,
16.7216170499274));
#270867=CARTESIAN_POINT('Ctrl Pts',(-0.103111278205868,-1.55209189971729,
16.7220747770206));
#270868=CARTESIAN_POINT('Ctrl Pts',(-0.0861714662690325,-1.55314729648499,
16.7232920827909));
#270869=CARTESIAN_POINT('Ctrl Pts',(-0.0756123759146554,-1.5536971405432,
16.7240537756847));
#270870=CARTESIAN_POINT('Ctrl Pts',(-0.0522965277171016,-1.55467302895351,
16.7257424232621));
#270871=CARTESIAN_POINT('Ctrl Pts',(-0.0395385943510725,-1.55504978548417,
16.7266708588757));
#270872=CARTESIAN_POINT('Ctrl Pts',(0.0964432028722504,-1.55739104874265,
16.7366159310021));
#270873=CARTESIAN_POINT('Ctrl Pts',(0.219454959696569,-1.54486089523714,
16.7460964634013));
#270874=CARTESIAN_POINT('Ctrl Pts',(0.392965155545203,-1.50603491758828,
16.7598840688127));
#270875=CARTESIAN_POINT('Ctrl Pts',(0.445597437267887,-1.49131026441339,
16.7641155303527));
#270876=CARTESIAN_POINT('Ctrl Pts',(0.532776837083353,-1.4618916493064,
16.7711165372224));
#270877=CARTESIAN_POINT('Ctrl Pts',(0.567766425841591,-1.44866152311005,
16.7739236689726));
#270878=CARTESIAN_POINT('Ctrl Pts',(0.608653300959912,-1.43149211163754,
16.7771745023783));
#270879=CARTESIAN_POINT('Ctrl Pts',(0.615040266671612,-1.42875959548013,
16.7776814405567));
#270880=CARTESIAN_POINT('Ctrl Pts',(0.62488682302739,-1.4244687085434,16.7784613760123));
#270881=CARTESIAN_POINT('Ctrl Pts',(0.628359269315785,-1.42294036161469,
16.7787361166533));
#270882=CARTESIAN_POINT('Ctrl Pts',(0.634767120984724,-1.42009200776305,
16.7792424905287));
#270883=CARTESIAN_POINT('Ctrl Pts',(0.637704001739351,-1.41877560415379,
16.779474328854));
#270884=CARTESIAN_POINT('Ctrl Pts',(0.644347103606848,-1.4157731590593,
16.7799981979163));
#270885=CARTESIAN_POINT('Ctrl Pts',(0.648050799832014,-1.41408167716587,
16.7802898920336));
#270886=CARTESIAN_POINT('Ctrl Pts',(0.659028760119822,-1.40901584199773,
16.7811534969775));
#270887=CARTESIAN_POINT('Ctrl Pts',(0.666283769100503,-1.40559969265221,
16.7817229292086));
#270888=CARTESIAN_POINT('Ctrl Pts',(0.730371797147227,-1.37481499476078,
16.7867444012345));
#270889=CARTESIAN_POINT('Ctrl Pts',(0.785525727972356,-1.34406503529633,
16.7910059989779));
#270890=CARTESIAN_POINT('Ctrl Pts',(0.912255095560012,-1.26293530584869,
16.8010163641911));
#270891=CARTESIAN_POINT('Ctrl Pts',(0.981743908824223,-1.20970835957524,
16.8066944160147));
#270892=CARTESIAN_POINT('Ctrl Pts',(1.09500324685008,-1.10673558929196,
16.8168825926789));
#270893=CARTESIAN_POINT('Ctrl Pts',(1.14075585346209,-1.05951413465942,
16.8213203466108));
#270894=CARTESIAN_POINT('Ctrl Pts',(1.1940578583454,-0.997033896665379,
16.8270324458937));
#270895=CARTESIAN_POINT('Ctrl Pts',(1.20453287609112,-0.984353226540621,
16.8281839410511));
#270896=CARTESIAN_POINT('Ctrl Pts',(1.21955493493162,-0.965569190443507,
16.8298797995177));
#270897=CARTESIAN_POINT('Ctrl Pts',(1.22426164324301,-0.959594459150302,
16.8304177822563));
#270898=CARTESIAN_POINT('Ctrl Pts',(1.2324797119608,-0.949003501514645,
16.8313690631042));
#270899=CARTESIAN_POINT('Ctrl Pts',(1.23600945557266,-0.944401667910239,
16.8317816256643));
#270900=CARTESIAN_POINT('Ctrl Pts',(1.24284862292754,-0.935381219693552,
16.8325888812655));
#270901=CARTESIAN_POINT('Ctrl Pts',(1.24616042553597,-0.930964509553055,
16.8329834730188));
#270902=CARTESIAN_POINT('Ctrl Pts',(1.25502295768887,-0.919013169942722,
16.834049488398));
#270903=CARTESIAN_POINT('Ctrl Pts',(1.26052923912267,-0.911446027511432,
16.8347226185924));
#270904=CARTESIAN_POINT('Ctrl Pts',(1.28087932618228,-0.882942282508785,
16.837251727528));
#270905=CARTESIAN_POINT('Ctrl Pts',(1.29527175601318,-0.861690115472988,
16.8391246756498));
#270906=CARTESIAN_POINT('Ctrl Pts',(1.31238370166954,-0.835024274253569,
16.8414608468509));
#270907=CARTESIAN_POINT('Ctrl Pts',(1.31560675529061,-0.829936975084977,
16.8419059259617));
#270908=CARTESIAN_POINT('Ctrl Pts',(1.40686814550163,-0.684021614678269,
16.8546544950382));
#270909=CARTESIAN_POINT('Ctrl Pts',(1.47180837690826,-0.530020496406353,
16.8678184023214));
#270910=CARTESIAN_POINT('Ctrl Pts',(1.51904880942607,-0.336418749923332,
16.8829314001696));
#270911=CARTESIAN_POINT('Ctrl Pts',(1.52589659067416,-0.303853372962476,
16.8854214974098));
#270912=CARTESIAN_POINT('Ctrl Pts',(1.53286834057281,-0.264462119343719,
16.8883525840522));
#270913=CARTESIAN_POINT('Ctrl Pts',(1.53399847463748,-0.257826000118732,
16.8888436300476));
#270914=CARTESIAN_POINT('Ctrl Pts',(1.53569063447191,-0.247484479117746,
16.8896043782268));
#270915=CARTESIAN_POINT('Ctrl Pts',(1.53628239178288,-0.243784137531892,
16.8898756932562));
#270916=CARTESIAN_POINT('Ctrl Pts',(1.53735827748471,-0.236896953102605,
16.890378970915));
#270917=CARTESIAN_POINT('Ctrl Pts',(1.53784586841758,-0.233710772246146,
16.8906111177098));
#270918=CARTESIAN_POINT('Ctrl Pts',(1.53893638871303,-0.22643352418955,
16.8911398080761));
#270919=CARTESIAN_POINT('Ctrl Pts',(1.53953291078763,-0.22234155493375,
16.8914359887352));
#270920=CARTESIAN_POINT('Ctrl Pts',(1.54104951580669,-0.211639271602126,
16.8922078729318));
#270921=CARTESIAN_POINT('Ctrl Pts',(1.54194339974385,-0.205025236647381,
16.8926821530798));
#270922=CARTESIAN_POINT('Ctrl Pts',(1.54777078982401,-0.159711640484578,
16.8959140059561));
#270923=CARTESIAN_POINT('Ctrl Pts',(1.55128995472198,-0.120840139787276,
16.8985992083349));
#270924=CARTESIAN_POINT('Ctrl Pts',(1.56091952725396,0.0618566635447943,
16.9109856866003));
#270925=CARTESIAN_POINT('Ctrl Pts',(1.54851151526834,0.205946077313584,
16.920141896236));
#270926=CARTESIAN_POINT('Ctrl Pts',(1.506730076061,0.388918033882374,16.9328600800483));
#270927=CARTESIAN_POINT('Ctrl Pts',(1.49520169161464,0.431119545182808,
16.9358666928964));
#270928=CARTESIAN_POINT('Ctrl Pts',(1.47860161689127,0.483152280035275,
16.9396943425542));
#270929=CARTESIAN_POINT('Ctrl Pts',(1.47518257109654,0.493492896011304,
16.9404610441578));
#270930=CARTESIAN_POINT('Ctrl Pts',(1.4695599631504,0.509917266403414,16.9416888582295));
#270931=CARTESIAN_POINT('Ctrl Pts',(1.46742649515984,0.516024789016074,
16.9421476585144));
#270932=CARTESIAN_POINT('Ctrl Pts',(1.46332226468621,0.527542751909619,
16.9430172029556));
#270933=CARTESIAN_POINT('Ctrl Pts',(1.46135943255118,0.53295592001184,16.9434276782068));
#270934=CARTESIAN_POINT('Ctrl Pts',(1.45685063793552,0.545178241116116,
16.9443586550454));
#270935=CARTESIAN_POINT('Ctrl Pts',(1.45428692194885,0.551980652892509,
16.9448797404049));
#270936=CARTESIAN_POINT('Ctrl Pts',(1.44756221276699,0.569451505920662,
16.9462257969949));
#270937=CARTESIAN_POINT('Ctrl Pts',(1.44333098934203,0.580092250937445,
16.9470530992632));
#270938=CARTESIAN_POINT('Ctrl Pts',(1.43752707603031,0.594231310765164,
16.9481626327223));
#270939=CARTESIAN_POINT('Ctrl Pts',(1.43605836754101,0.597771951742406,
16.9484413407064));
#270940=CARTESIAN_POINT('Ctrl Pts',(1.4345766824505,0.601306903477194,16.9487204703706));
#270941=CARTESIAN_POINT('Origin',(0.,0.,-1.29405622560371));
#270942=CARTESIAN_POINT('',(1.43457675882331,0.601306721269597,17.7872340762022));
#270943=CARTESIAN_POINT('',(1.43457667260785,0.601306926959429,17.650811911463));
#270944=CARTESIAN_POINT('',(1.43457668357355,0.601306900797845,-1.29405622560371));
#270945=CARTESIAN_POINT('',(-1.5554999603012,-0.000351429880857887,17.395456864983));
#270946=CARTESIAN_POINT('Ctrl Pts',(1.43457675882332,0.601306721269597,
17.7872340762022));
#270947=CARTESIAN_POINT('Ctrl Pts',(1.44690679487224,0.57189014812056,17.7848031153696));
#270948=CARTESIAN_POINT('Ctrl Pts',(1.45833584107452,0.542085259084417,
17.7823974315995));
#270949=CARTESIAN_POINT('Ctrl Pts',(1.47275577373232,0.500711392614961,
17.7791544208958));
#270950=CARTESIAN_POINT('Ctrl Pts',(1.47653821205348,0.489444990848641,
17.7782809671412));
#270951=CARTESIAN_POINT('Ctrl Pts',(1.4816705060036,0.473556669248412,17.7770637326209));
#270952=CARTESIAN_POINT('Ctrl Pts',(1.48312847097578,0.468970518901122,
17.7767140701249));
#270953=CARTESIAN_POINT('Ctrl Pts',(1.48545190330485,0.461542755981358,
17.7761505671935));
#270954=CARTESIAN_POINT('Ctrl Pts',(1.4863305400394,0.458705350725448,17.7759359707686));
#270955=CARTESIAN_POINT('Ctrl Pts',(1.48817082176006,0.452701673250632,
17.775483328293));
#270956=CARTESIAN_POINT('Ctrl Pts',(1.48913050113314,0.449534815929342,
17.7752454017436));
#270957=CARTESIAN_POINT('Ctrl Pts',(1.49147575321705,0.44170576507869,17.7746592111106));
#270958=CARTESIAN_POINT('Ctrl Pts',(1.49284959472888,0.437040037713588,
17.7743116244073));
#270959=CARTESIAN_POINT('Ctrl Pts',(1.49785472595556,0.41974301921536,17.7730292501083));
#270960=CARTESIAN_POINT('Ctrl Pts',(1.50134790722727,0.407071829227247,
17.7721020710032));
#270961=CARTESIAN_POINT('Ctrl Pts',(1.50972741120255,0.375099623352245,
17.7697896832));
#270962=CARTESIAN_POINT('Ctrl Pts',(1.51440471423828,0.355745739213263,
17.7684145389477));
#270963=CARTESIAN_POINT('Ctrl Pts',(1.55043747873432,0.193027148764359,
17.7570169255336));
#270964=CARTESIAN_POINT('Ctrl Pts',(1.56173358295706,0.0459693221400361,
17.7477094026532));
#270965=CARTESIAN_POINT('Ctrl Pts',(1.54900674702494,-0.150590046290445,
17.7344327353212));
#270966=CARTESIAN_POINT('Ctrl Pts',(1.54334205350967,-0.20048366796201,
17.7309971157239));
#270967=CARTESIAN_POINT('Ctrl Pts',(1.53340914686726,-0.261479683018524,
17.7266719271998));
#270968=CARTESIAN_POINT('Ctrl Pts',(1.53141337830653,-0.272925425943734,
17.725854904451));
#270969=CARTESIAN_POINT('Ctrl Pts',(1.52807458283947,-0.290882277453159,
17.724564087975));
#270970=CARTESIAN_POINT('Ctrl Pts',(1.52681768155549,-0.297409137147886,
17.7240930287585));
#270971=CARTESIAN_POINT('Ctrl Pts',(1.52452345518529,-0.308924660432629,
17.7232585099452));
#270972=CARTESIAN_POINT('Ctrl Pts',(1.52350337030061,-0.313916694017427,
17.7228956045271));
#270973=CARTESIAN_POINT('Ctrl Pts',(1.52110672131121,-0.325358395022645,
17.7220611678649));
#270974=CARTESIAN_POINT('Ctrl Pts',(1.51971363750734,-0.331804460980519,
17.7215891151783));
#270975=CARTESIAN_POINT('Ctrl Pts',(1.51573542085201,-0.349661664745591,
17.7202758974049));
#270976=CARTESIAN_POINT('Ctrl Pts',(1.51306251269409,-0.361052578698618,
17.7194319411809));
#270977=CARTESIAN_POINT('Ctrl Pts',(1.49639841718896,-0.428631342342926,
17.714386524882));
#270978=CARTESIAN_POINT('Ctrl Pts',(1.47940900194819,-0.484025270831817,
17.7100893632637));
#270979=CARTESIAN_POINT('Ctrl Pts',(1.43175498639562,-0.613210113420364,
17.6996710425956));
#270980=CARTESIAN_POINT('Ctrl Pts',(1.39841703382149,-0.685840068163576,
17.6934861479448));
#270981=CARTESIAN_POINT('Ctrl Pts',(1.32085659472172,-0.825408402874694,
17.6811050806827));
#270982=CARTESIAN_POINT('Ctrl Pts',(1.27672902221003,-0.892147458294287,
17.6749280062949));
#270983=CARTESIAN_POINT('Ctrl Pts',(1.22010249534743,-0.964925794909212,
17.6680979772779));
#270984=CARTESIAN_POINT('Ctrl Pts',(1.21242510087692,-0.974554918432606,
17.6671924145254));
#270985=CARTESIAN_POINT('Ctrl Pts',(1.20154346927468,-0.987875195851234,
17.6659382034851));
#270986=CARTESIAN_POINT('Ctrl Pts',(1.1984352340874,-0.991643636884611,
17.6655832022986));
#270987=CARTESIAN_POINT('Ctrl Pts',(1.19339992479924,-0.997690218357838,
17.6650133985101));
#270988=CARTESIAN_POINT('Ctrl Pts',(1.1914839927223,-0.999977523655699,
17.6647978077846));
#270989=CARTESIAN_POINT('Ctrl Pts',(1.18743896637812,-1.00477848418966,
17.6643452224476));
#270990=CARTESIAN_POINT('Ctrl Pts',(1.18530844978136,-1.00729091151195,
17.6641083386001));
#270991=CARTESIAN_POINT('Ctrl Pts',(1.18006011939083,-1.01344033502069,
17.6635283936405));
#270992=CARTESIAN_POINT('Ctrl Pts',(1.17693341921679,-1.0170697745923,17.6631859777038));
#270993=CARTESIAN_POINT('Ctrl Pts',(1.16549340833,-1.03022581461333,17.6619440652548));
#270994=CARTESIAN_POINT('Ctrl Pts',(1.15708049465765,-1.03966574920664,
17.6610515668366));
#270995=CARTESIAN_POINT('Ctrl Pts',(1.10090314421147,-1.10117434486033,
17.655218655124));
#270996=CARTESIAN_POINT('Ctrl Pts',(1.04974697676919,-1.15004638052301,
17.6504979634673));
#270997=CARTESIAN_POINT('Ctrl Pts',(0.888867301873258,-1.28402865935836,
17.6366559401494));
#270998=CARTESIAN_POINT('Ctrl Pts',(0.770920378940911,-1.35812089762546,
17.6276766423771));
#270999=CARTESIAN_POINT('Ctrl Pts',(0.629398982446087,-1.42257532779914,
17.6168658550513));
#271000=CARTESIAN_POINT('Ctrl Pts',(0.613967085195139,-1.42930333452608,
17.6156876356169));
#271001=CARTESIAN_POINT('Ctrl Pts',(0.591472048558315,-1.43867921435167,
17.6139695534218));
#271002=CARTESIAN_POINT('Ctrl Pts',(0.584493675976079,-1.4415284267653,
17.6134364939884));
#271003=CARTESIAN_POINT('Ctrl Pts',(0.572155581096667,-1.44646165104697,
17.612493744104));
#271004=CARTESIAN_POINT('Ctrl Pts',(0.566804451279021,-1.44856688810552,
17.6120847754956));
#271005=CARTESIAN_POINT('Ctrl Pts',(0.555710975706681,-1.45286039378464,
17.6112366882273));
#271006=CARTESIAN_POINT('Ctrl Pts',(0.549967098930028,-1.45504439810024,
17.6107974352973));
#271007=CARTESIAN_POINT('Ctrl Pts',(0.535170371209446,-1.46057045238012,
17.609665440056));
#271008=CARTESIAN_POINT('Ctrl Pts',(0.526099207623039,-1.4638623529982,
17.6089710443485));
#271009=CARTESIAN_POINT('Ctrl Pts',(0.487604731311496,-1.47742788181399,
17.6060220445099));
#271010=CARTESIAN_POINT('Ctrl Pts',(0.457908732017132,-1.48689974570038,
17.6037413341823));
#271011=CARTESIAN_POINT('Ctrl Pts',(0.378171027456508,-1.5097177915959,
17.5975969243279));
#271012=CARTESIAN_POINT('Ctrl Pts',(0.327716807777019,-1.52146699633172,
17.5936869752201));
#271013=CARTESIAN_POINT('Ctrl Pts',(0.180535503645951,-1.54808014006072,
17.5822395797291));
#271014=CARTESIAN_POINT('Ctrl Pts',(0.082874869517439,-1.55636614997997,
17.5745794231732));
#271015=CARTESIAN_POINT('Ctrl Pts',(-0.0250205497408982,-1.55533159461845,
17.5663084949911));
#271016=CARTESIAN_POINT('Ctrl Pts',(-0.0351258713253945,-1.55513619263152,
17.5655359054609));
#271017=CARTESIAN_POINT('Ctrl Pts',(-0.0835731852144278,-1.55372691060975,
17.5618436516246));
#271018=CARTESIAN_POINT('Ctrl Pts',(-0.121867350590717,-1.55119332944801,
17.5589601508508));
#271019=CARTESIAN_POINT('Ctrl Pts',(-0.166583549676007,-1.54656831366107,
17.5556619228482));
#271020=CARTESIAN_POINT('Ctrl Pts',(-0.173130572719318,-1.54584909895374,
17.5551807649105));
#271021=CARTESIAN_POINT('Ctrl Pts',(-0.183727945077796,-1.54461676711698,
17.5544049728898));
#271022=CARTESIAN_POINT('Ctrl Pts',(-0.187781097753289,-1.54412926124093,
17.5541089782319));
#271023=CARTESIAN_POINT('Ctrl Pts',(-0.194990500014386,-1.54323332094478,
17.5535838265887));
#271024=CARTESIAN_POINT('Ctrl Pts',(-0.198147454703101,-1.54283115241295,
17.5533543260882));
#271025=CARTESIAN_POINT('Ctrl Pts',(-0.204969632960233,-1.54194078061221,
17.5528593795015));
#271026=CARTESIAN_POINT('Ctrl Pts',(-0.208634352565216,-1.54144919768787,
17.5525941255405));
#271027=CARTESIAN_POINT('Ctrl Pts',(-0.218868836227695,-1.54003918353441,
17.5518549939548));
#271028=CARTESIAN_POINT('Ctrl Pts',(-0.225434634864877,-1.53909177241289,
17.5513827092611));
#271029=CARTESIAN_POINT('Ctrl Pts',(-0.264183175652776,-1.53324727083779,
17.5486056083556));
#271030=CARTESIAN_POINT('Ctrl Pts',(-0.296214714029169,-1.52738246035465,
17.5463511774142));
#271031=CARTESIAN_POINT('Ctrl Pts',(-0.47921709607514,-1.48790088970543,
17.5335857949565));
#271032=CARTESIAN_POINT('Ctrl Pts',(-0.624691046510996,-1.43292301553589,
17.5238059666347));
#271033=CARTESIAN_POINT('Ctrl Pts',(-0.795181463123512,-1.33750606586419,
17.5105419518066));
#271034=CARTESIAN_POINT('Ctrl Pts',(-0.829893632763427,-1.31624925673716,
17.5077411410696));
#271035=CARTESIAN_POINT('Ctrl Pts',(-0.872892158193993,-1.28754063568279,
17.5041186230854));
#271036=CARTESIAN_POINT('Ctrl Pts',(-0.881988573871251,-1.28132655980388,
17.503343252725));
#271037=CARTESIAN_POINT('Ctrl Pts',(-0.896301460054811,-1.27132430559928,
17.5021084189028));
#271038=CARTESIAN_POINT('Ctrl Pts',(-0.901561831072859,-1.26759932935658,
17.5016513610177));
#271039=CARTESIAN_POINT('Ctrl Pts',(-0.911235620088362,-1.26065844449219,
17.5008047695889));
#271040=CARTESIAN_POINT('Ctrl Pts',(-0.91565556631832,-1.25745176903959,
17.5004155956519));
#271041=CARTESIAN_POINT('Ctrl Pts',(-0.920127347815195,-1.25417140818013,
17.5000194188615));
#271042=CARTESIAN_POINT('Ctrl Pts',(-0.920196206647987,-1.25412088674282,
17.5000133177343));
#271043=CARTESIAN_POINT('Ctrl Pts',(-0.920331683582465,-1.25402147071847,
17.5000013128558));
#271044=CARTESIAN_POINT('Ctrl Pts',(-0.92039830195099,-1.25397257649216,
17.4999954091186));
#271045=CARTESIAN_POINT('Ctrl Pts',(-0.926044458638076,-1.24982791502793,
17.4994949984296));
#271046=CARTESIAN_POINT('Ctrl Pts',(-0.931596516533388,-1.24569502048958,
17.4989990523982));
#271047=CARTESIAN_POINT('Ctrl Pts',(-0.943112681260327,-1.23700245748673,
17.4979621404227));
#271048=CARTESIAN_POINT('Ctrl Pts',(-0.949071717140402,-1.23243640056207,
17.4974209320286));
#271049=CARTESIAN_POINT('Ctrl Pts',(-0.964507341940575,-1.22043065742354,
17.4960067155646));
#271050=CARTESIAN_POINT('Ctrl Pts',(-0.973930799545166,-1.21292381655863,
17.4951310719277));
#271051=CARTESIAN_POINT('Ctrl Pts',(-1.00169890515288,-1.19027116684355,
17.4925135380778));
#271052=CARTESIAN_POINT('Ctrl Pts',(-1.01978359084261,-1.17481379879,17.490759424453));
#271053=CARTESIAN_POINT('Ctrl Pts',(-1.13845847377506,-1.06857449830548,
17.4789082507005));
#271054=CARTESIAN_POINT('Ctrl Pts',(-1.22715853292402,-0.965406078891215,
17.468293690062));
#271055=CARTESIAN_POINT('Ctrl Pts',(-1.33194779482776,-0.805365730683185,
17.4535700699966));
#271056=CARTESIAN_POINT('Ctrl Pts',(-1.36000478742733,-0.757025386093227,
17.4493246277061));
#271057=CARTESIAN_POINT('Ctrl Pts',(-1.38897448861438,-0.700279803433184,
17.4446438484717));
#271058=CARTESIAN_POINT('Ctrl Pts',(-1.392492655234,-0.693257632608618,
17.4440697354421));
#271059=CARTESIAN_POINT('Ctrl Pts',(-1.39772528710097,-0.682612868450967,
17.4432074901694));
#271060=CARTESIAN_POINT('Ctrl Pts',(-1.39947911843154,-0.679009944278098,
17.4429170274254));
#271061=CARTESIAN_POINT('Ctrl Pts',(-1.40259842032801,-0.672538484829419,
17.4423978306542));
#271062=CARTESIAN_POINT('Ctrl Pts',(-1.40396903753513,-0.669672520383105,
17.4421687845073));
#271063=CARTESIAN_POINT('Ctrl Pts',(-1.40693974057702,-0.663411562876161,
17.4416703472381));
#271064=CARTESIAN_POINT('Ctrl Pts',(-1.40853632080669,-0.660014976456627,
17.441401172699));
#271065=CARTESIAN_POINT('Ctrl Pts',(-1.41302930741365,-0.650365979357112,
17.4406398890738));
#271066=CARTESIAN_POINT('Ctrl Pts',(-1.4158965325938,-0.644099949082936,
17.4401495306365));
#271067=CARTESIAN_POINT('Ctrl Pts',(-1.43409150073586,-0.603628014989925,
17.4370067962985));
#271068=CARTESIAN_POINT('Ctrl Pts',(-1.4482217931586,-0.56889316116657,
17.4344215493099));
#271069=CARTESIAN_POINT('Ctrl Pts',(-1.48807801336718,-0.459776275902577,
17.4265402540847));
#271070=CARTESIAN_POINT('Ctrl Pts',(-1.50942778119496,-0.383927164863786,
17.4213940892309));
#271071=CARTESIAN_POINT('Ctrl Pts',(-1.54524553084811,-0.205885544366946,
17.4094361640154));
#271072=CARTESIAN_POINT('Ctrl Pts',(-1.55547671460093,-0.103241615985641,
17.4026172025359));
#271073=CARTESIAN_POINT('Ctrl Pts',(-1.5554999603012,-0.000351429880857887,
17.395456864983));
#271074=CARTESIAN_POINT('Ctrl Pts',(-1.55549996055179,-0.000350318978951627,
17.3954567876731));
#271075=CARTESIAN_POINT('Ctrl Pts',(-1.5555020360747,0.00886549862816396,
17.394815439967));
#271076=CARTESIAN_POINT('Ctrl Pts',(-1.55542221061676,0.0180810189639046,
17.394171699026));
#271077=CARTESIAN_POINT('Ctrl Pts',(-1.55511197823933,0.035757859119276,
17.3929319368728));
#271078=CARTESIAN_POINT('Ctrl Pts',(-1.55489438855453,0.0442190544186781,
17.3923363295072));
#271079=CARTESIAN_POINT('Ctrl Pts',(-1.55441798831586,0.0582783737622305,
17.3913428268625));
#271080=CARTESIAN_POINT('Ctrl Pts',(-1.55419795658096,0.063877707554238,
17.3909461401424));
#271081=CARTESIAN_POINT('Ctrl Pts',(-1.55370512290485,0.0749008154391519,
17.390163154582));
#271082=CARTESIAN_POINT('Ctrl Pts',(-1.55343416312172,0.0803245950657222,
17.38977691865));
#271083=CARTESIAN_POINT('Ctrl Pts',(-1.55279782395194,0.0918506312577073,
17.3889539969631));
#271084=CARTESIAN_POINT('Ctrl Pts',(-1.55242486257448,0.0979523589495593,
17.3885170804876));
#271085=CARTESIAN_POINT('Ctrl Pts',(-1.55138024292207,0.113533720313811,
17.3873980333919));
#271086=CARTESIAN_POINT('Ctrl Pts',(-1.55065766795671,0.123009565221441,
17.3867143217273));
#271087=CARTESIAN_POINT('Ctrl Pts',(-1.54752617426158,0.15964463058344,
17.3840583411605));
#271088=CARTESIAN_POINT('Ctrl Pts',(-1.54449028669734,0.186743803352096,
17.3820666525217));
#271089=CARTESIAN_POINT('Ctrl Pts',(-1.5205575959555,0.359256320838537,
17.369205188255));
#271090=CARTESIAN_POINT('Ctrl Pts',(-1.47986110201174,0.501152983121043,
17.3576922870742));
#271091=CARTESIAN_POINT('Ctrl Pts',(-1.40454160001679,0.669520086941398,
17.3435043038259));
#271092=CARTESIAN_POINT('Ctrl Pts',(-1.38794532269747,0.703279787160669,
17.3406366122605));
#271093=CARTESIAN_POINT('Ctrl Pts',(-1.36359833980893,0.748579172761733,
17.3367853698398));
#271094=CARTESIAN_POINT('Ctrl Pts',(-1.35689401465341,0.760664101502796,
17.3357576404983));
#271095=CARTESIAN_POINT('Ctrl Pts',(-1.34508406620527,0.781299057773077,
17.3340042454211));
#271096=CARTESIAN_POINT('Ctrl Pts',(-1.34005586931038,0.789892172249686,
17.3332745118182));
#271097=CARTESIAN_POINT('Ctrl Pts',(-1.33271061932318,0.802173054509789,
17.3322328826455));
#271098=CARTESIAN_POINT('Ctrl Pts',(-1.33046018325886,0.805900059713476,
17.3319169391457));
#271099=CARTESIAN_POINT('Ctrl Pts',(-1.32652038913346,0.812363371652627,
17.3313693973018));
#271100=CARTESIAN_POINT('Ctrl Pts',(-1.32483815312171,0.815103956097704,
17.3311373431652));
#271101=CARTESIAN_POINT('Ctrl Pts',(-1.32128451516139,0.820853235135281,
17.330650797765));
#271102=CARTESIAN_POINT('Ctrl Pts',(-1.31941132680581,0.823860761911189,
17.330396426292));
#271103=CARTESIAN_POINT('Ctrl Pts',(-1.31437412876736,0.831887070408513,
17.3297178942402));
#271104=CARTESIAN_POINT('Ctrl Pts',(-1.3111916124328,0.836894262626329,
17.3292949292892));
#271105=CARTESIAN_POINT('Ctrl Pts',(-1.29706636013733,0.858839769150748,
17.3274420626684));
#271106=CARTESIAN_POINT('Ctrl Pts',(-1.28582286786256,0.875583546451696,
17.3260307564443));
#271107=CARTESIAN_POINT('Ctrl Pts',(-1.27208265307508,0.895209661101148,
17.3243732442507));
#271108=CARTESIAN_POINT('Ctrl Pts',(-1.26989770293045,0.898306427817408,
17.3241116105747));
#271109=CARTESIAN_POINT('Ctrl Pts',(-1.18257179152736,1.02111957571539,
17.3137303524027));
#271110=CARTESIAN_POINT('Ctrl Pts',(-1.08090336990349,1.12819340188835,
17.3044171457754));
#271111=CARTESIAN_POINT('Ctrl Pts',(-0.936139129157414,1.2428380922563,
17.2920211506613));
#271112=CARTESIAN_POINT('Ctrl Pts',(-0.90572941557981,1.26517069249233,
17.2894616971732));
#271113=CARTESIAN_POINT('Ctrl Pts',(-0.860748393691952,1.29575096702797,
17.2857136295249));
#271114=CARTESIAN_POINT('Ctrl Pts',(-0.846807500938753,1.30490435911294,
17.2845570613963));
#271115=CARTESIAN_POINT('Ctrl Pts',(-0.824802832481698,1.3188511881578,
17.2827375503216));
#271116=CARTESIAN_POINT('Ctrl Pts',(-0.816838021323161,1.3237990063342,
17.2820801748405));
#271117=CARTESIAN_POINT('Ctrl Pts',(-0.803362652134913,1.33200212273425,
17.2809697267821));
#271118=CARTESIAN_POINT('Ctrl Pts',(-0.797875780186113,1.33529601325457,
17.2805180568162));
#271119=CARTESIAN_POINT('Ctrl Pts',(-0.787097128068209,1.34167652206558,
17.2796316157982));
#271120=CARTESIAN_POINT('Ctrl Pts',(-0.781807125893892,1.34476592566285,
17.2791969552695));
#271121=CARTESIAN_POINT('Ctrl Pts',(-0.771696678839268,1.3505906869611,
17.2783668845521));
#271122=CARTESIAN_POINT('Ctrl Pts',(-0.766879582402399,1.35333169344035,
17.277971685855));
#271123=CARTESIAN_POINT('Ctrl Pts',(-0.755677478716684,1.3596268598496,
17.2770532567584));
#271124=CARTESIAN_POINT('Ctrl Pts',(-0.749281914841805,1.36316186074075,
17.2765293514285));
#271125=CARTESIAN_POINT('Ctrl Pts',(-0.732551637641446,1.37225582690031,
17.2751598847431));
#271126=CARTESIAN_POINT('Ctrl Pts',(-0.722178678292795,1.37774304529251,
17.2743118100013));
#271127=CARTESIAN_POINT('Ctrl Pts',(-0.642088156542963,1.41895735732056,
17.267770104671));
#271128=CARTESIAN_POINT('Ctrl Pts',(-0.56983531290357,1.44948305707374,
17.2618964892526));
#271129=CARTESIAN_POINT('Ctrl Pts',(-0.393482747641707,1.5087604785845,
17.2476466391434));
#271130=CARTESIAN_POINT('Ctrl Pts',(-0.288079069319143,1.53238252900044,
17.239185215477));
#271131=CARTESIAN_POINT('Ctrl Pts',(-0.143652882207271,1.54931092245702,
17.2281181003721));
#271132=CARTESIAN_POINT('Ctrl Pts',(-0.1060720383946,1.55233688085673,17.2252883913725));
#271133=CARTESIAN_POINT('Ctrl Pts',(-0.0615212249774581,1.55429823452016,
17.2220195834915));
#271134=CARTESIAN_POINT('Ctrl Pts',(-0.0546255714621406,1.55455585768492,
17.2215160625967));
#271135=CARTESIAN_POINT('Ctrl Pts',(-0.0439749222149352,1.55488281135439,
17.2207423338028));
#271136=CARTESIAN_POINT('Ctrl Pts',(-0.0402211242258011,1.55498444133869,
17.2204703982776));
#271137=CARTESIAN_POINT('Ctrl Pts',(-0.0332911163985541,1.55514695221371,
17.2199698232113));
#271138=CARTESIAN_POINT('Ctrl Pts',(-0.0301151084918541,1.55521169685317,
17.219740979235));
#271139=CARTESIAN_POINT('Ctrl Pts',(-0.0229350133192406,1.55533606352476,
17.2192248940198));
#271140=CARTESIAN_POINT('Ctrl Pts',(-0.0189308857210311,1.55538995363686,
17.218937974936));
#271141=CARTESIAN_POINT('Ctrl Pts',(-0.00682550035110079,1.55550612192181,
17.2180731110734));
#271142=CARTESIAN_POINT('Ctrl Pts',(0.00127624944527889,1.55552057572554,
17.2174977475247));
#271143=CARTESIAN_POINT('Ctrl Pts',(0.0796879713836924,1.55504782971908,
17.2119594379467));
#271144=CARTESIAN_POINT('Ctrl Pts',(0.149899444054184,1.54985711091355,
17.2072343336937));
#271145=CARTESIAN_POINT('Ctrl Pts',(0.284973747043006,1.53060132227121,
17.1981896154152));
#271146=CARTESIAN_POINT('Ctrl Pts',(0.349758562626398,1.51710895594546,
17.1938712486912));
#271147=CARTESIAN_POINT('Ctrl Pts',(0.488520571526831,1.47884607062597,
17.1843459079556));
#271148=CARTESIAN_POINT('Ctrl Pts',(0.561883860438447,1.45255710583265,
17.1791280738521));
#271149=CARTESIAN_POINT('Ctrl Pts',(0.649275351134604,1.41362673401151,
17.1724852028277));
#271150=CARTESIAN_POINT('Ctrl Pts',(0.665457651816556,1.40608146723739,
17.171236647396));
#271151=CARTESIAN_POINT('Ctrl Pts',(0.688518990003329,1.3948414666327,17.1694287767374));
#271152=CARTESIAN_POINT('Ctrl Pts',(0.695506115592836,1.39137067520223,
17.1688772046197));
#271153=CARTESIAN_POINT('Ctrl Pts',(0.707616486990826,1.38524094354631,
17.1679143706662));
#271154=CARTESIAN_POINT('Ctrl Pts',(0.712751638764899,1.38260575151938,
17.1675039452158));
#271155=CARTESIAN_POINT('Ctrl Pts',(0.722632385487544,1.37746560036033,
17.166709997566));
#271156=CARTESIAN_POINT('Ctrl Pts',(0.727379925897033,1.37496454019816,
17.1663266173624));
#271157=CARTESIAN_POINT('Ctrl Pts',(0.738609140058618,1.36897442394996,
17.1654152447034));
#271158=CARTESIAN_POINT('Ctrl Pts',(0.745079124051548,1.36546385182905,
17.1648864949309));
#271159=CARTESIAN_POINT('Ctrl Pts',(0.767910039065515,1.35286536296374,
17.1630075452129));
#271160=CARTESIAN_POINT('Ctrl Pts',(0.784131011321175,1.34352857009894,
17.1616485097875));
#271161=CARTESIAN_POINT('Ctrl Pts',(0.916605468070933,1.26405999604718,
17.1503437468259));
#271162=CARTESIAN_POINT('Ctrl Pts',(1.02336450301627,1.17928887908859,17.1398304470286));
#271163=CARTESIAN_POINT('Ctrl Pts',(1.16665034876433,1.03123845142085,17.1238719145491));
#271164=CARTESIAN_POINT('Ctrl Pts',(1.21208015275551,0.977440421709085,
17.1184588642416));
#271165=CARTESIAN_POINT('Ctrl Pts',(1.26118415251025,0.910578894214684,
17.1123139481622));
#271166=CARTESIAN_POINT('Ctrl Pts',(1.26852772644086,0.900320400611983,
17.1113863331313));
#271167=CARTESIAN_POINT('Ctrl Pts',(1.27848436177573,0.886047907182715,
17.1101177638395));
#271168=CARTESIAN_POINT('Ctrl Pts',(1.28120465031244,0.882109858683324,
17.109770018682));
#271169=CARTESIAN_POINT('Ctrl Pts',(1.28576596562492,0.875441018587189,
17.1091850494671));
#271170=CARTESIAN_POINT('Ctrl Pts',(1.28761655759249,0.872716847974279,
17.1089471887841));
#271171=CARTESIAN_POINT('Ctrl Pts',(1.29112774842616,0.867512705720129,
17.1084949024555));
#271172=CARTESIAN_POINT('Ctrl Pts',(1.29278987578452,0.865033811375427,
17.1082803708945));
#271173=CARTESIAN_POINT('Ctrl Pts',(1.29715604002407,0.858481428153496,
17.1077156491046));
#271174=CARTESIAN_POINT('Ctrl Pts',(1.29984805371944,0.854399902640539,
17.1073662583828));
#271175=CARTESIAN_POINT('Ctrl Pts',(1.30926623911597,0.839972876048405,
17.1061393582122));
#271176=CARTESIAN_POINT('Ctrl Pts',(1.31588873938611,0.82955974362176,17.1052683954196));
#271177=CARTESIAN_POINT('Ctrl Pts',(1.36481324392354,0.750571081033337,
17.0987618315329));
#271178=CARTESIAN_POINT('Ctrl Pts',(1.40185983736245,0.678870315930969,
17.0934147810645));
#271179=CARTESIAN_POINT('Ctrl Pts',(1.43365138259542,0.603510887816935,
17.0880219605327));
#271180=CARTESIAN_POINT('Ctrl Pts',(1.43411467340915,0.602409148267333,
17.0879431670415));
#271181=CARTESIAN_POINT('Ctrl Pts',(1.43457668369174,0.601306900515888,
17.0878643847065));
#271182=CARTESIAN_POINT('Ctrl Pts',(1.4345766824505,0.601306903477194,16.9487204703706));
#271183=CARTESIAN_POINT('Ctrl Pts',(1.41065121726306,0.658387429704644,
16.9532277081806));
#271184=CARTESIAN_POINT('Ctrl Pts',(1.38334239509286,0.71398433722006,16.9578483572576));
#271185=CARTESIAN_POINT('Ctrl Pts',(1.30587879174838,0.850467794813364,
16.9697880774579));
#271186=CARTESIAN_POINT('Ctrl Pts',(1.25148488824473,0.928653887924648,
16.9772109967927));
#271187=CARTESIAN_POINT('Ctrl Pts',(1.1539314621347,1.04461207454308,16.9888998715124));
#271188=CARTESIAN_POINT('Ctrl Pts',(1.11522752055849,1.08583665850537,16.9932128911011));
#271189=CARTESIAN_POINT('Ctrl Pts',(1.06612735060895,1.13273226376113,16.998232468779));
#271190=CARTESIAN_POINT('Ctrl Pts',(1.05780649673004,1.1405066176505,16.9990685990261));
#271191=CARTESIAN_POINT('Ctrl Pts',(1.0459830347572,1.15131280648582,17.0002355480977));
#271192=CARTESIAN_POINT('Ctrl Pts',(1.04255138244816,1.1544211986196,17.0005717842922));
#271193=CARTESIAN_POINT('Ctrl Pts',(1.0366549692451,1.15971443563753,17.0011452493219));
#271194=CARTESIAN_POINT('Ctrl Pts',(1.03419707232768,1.16190684391341,17.0013830377421));
#271195=CARTESIAN_POINT('Ctrl Pts',(1.0294325236598,1.16612965479541,17.0018415296063));
#271196=CARTESIAN_POINT('Ctrl Pts',(1.0271268104418,1.16816103696411,17.0020623102749));
#271197=CARTESIAN_POINT('Ctrl Pts',(1.02154979698476,1.1730452257836,17.0025937325973));
#271198=CARTESIAN_POINT('Ctrl Pts',(1.01827252123555,1.17589122080303,17.002903875017));
#271199=CARTESIAN_POINT('Ctrl Pts',(1.00610862330614,1.18636539347976,17.0040472911871));
#271200=CARTESIAN_POINT('Ctrl Pts',(0.997147549874596,1.19390711290743,
17.0048745272426));
#271201=CARTESIAN_POINT('Ctrl Pts',(0.905928195060317,1.2689345560661,17.0131546221594));
#271202=CARTESIAN_POINT('Ctrl Pts',(0.817022862169967,1.32792389058456,
17.0200957731965));
#271203=CARTESIAN_POINT('Ctrl Pts',(0.62700283298634,1.4276366287111,17.034224400446));
#271204=CARTESIAN_POINT('Ctrl Pts',(0.52626293681144,1.46776063342804,17.0413851160088));
#271205=CARTESIAN_POINT('Ctrl Pts',(0.408769510776668,1.50089373899557,
17.0499029942113));
#271206=CARTESIAN_POINT('Ctrl Pts',(0.395304485573703,1.50449621809098,
17.0508810629107));
#271207=CARTESIAN_POINT('Ctrl Pts',(0.374892880614281,1.50966428237514,
17.0523674197553));
#271208=CARTESIAN_POINT('Ctrl Pts',(0.367980713570848,1.51136398951791,
17.052871393978));
#271209=CARTESIAN_POINT('Ctrl Pts',(0.355469431700181,1.51434960779717,
17.05378486863));
#271210=CARTESIAN_POINT('Ctrl Pts',(0.349874362541732,1.51565206440121,
17.0541938303977));
#271211=CARTESIAN_POINT('Ctrl Pts',(0.337865366384993,1.51837755746418,
17.0550726439349));
#271212=CARTESIAN_POINT('Ctrl Pts',(0.33144940221459,1.51979100673046,17.0555427936852));
#271213=CARTESIAN_POINT('Ctrl Pts',(0.314208083979798,1.52347493322075,
17.0568080067576));
#271214=CARTESIAN_POINT('Ctrl Pts',(0.303367324910997,1.525670621931,17.0576054329312));
#271215=CARTESIAN_POINT('Ctrl Pts',(0.251809559381007,1.53554191302735,
17.0614076889888));
#271216=CARTESIAN_POINT('Ctrl Pts',(0.21082363738004,1.54170354353255,17.0644597575803));
#271217=CARTESIAN_POINT('Ctrl Pts',(0.152765132844512,1.54807344495159,
17.0688286024449));
#271218=CARTESIAN_POINT('Ctrl Pts',(0.135857591844307,1.54964875220432,
17.0701061697115));
#271219=CARTESIAN_POINT('Ctrl Pts',(-0.00857402935856209,1.56072391446616,
17.0810630422577));
#271220=CARTESIAN_POINT('Ctrl Pts',(-0.136776883644167,1.55474078191262,
17.0911333588831));
#271221=CARTESIAN_POINT('Ctrl Pts',(-0.302537509833343,1.52632806506721,
17.1039577965584));
#271222=CARTESIAN_POINT('Ctrl Pts',(-0.34200676025461,1.51797179791216,
17.10699125915));
#271223=CARTESIAN_POINT('Ctrl Pts',(-0.387975284496668,1.5063550589897,
17.110468052147));
#271224=CARTESIAN_POINT('Ctrl Pts',(-0.394828341840151,1.5045733517298,
17.1109848813355));
#271225=CARTESIAN_POINT('Ctrl Pts',(-0.405362076225008,1.50175778641549,
17.1117767371911));
#271226=CARTESIAN_POINT('Ctrl Pts',(-0.409051388150394,1.50075708381014,
17.1120535906333));
#271227=CARTESIAN_POINT('Ctrl Pts',(-0.415838059003677,1.49888935662649,
17.1125619363595));
#271228=CARTESIAN_POINT('Ctrl Pts',(-0.41893640170209,1.49802633036415,
17.1127936464935));
#271229=CARTESIAN_POINT('Ctrl Pts',(-0.425916234884315,1.49605878755416,
17.1133148219938));
#271230=CARTESIAN_POINT('Ctrl Pts',(-0.42979611204794,1.49494877437938,
17.1136039657528));
#271231=CARTESIAN_POINT('Ctrl Pts',(-0.439764656422691,1.49205480800695,
17.1143455205239));
#271232=CARTESIAN_POINT('Ctrl Pts',(-0.445846887197351,1.49024865709088,
17.1147966849212));
#271233=CARTESIAN_POINT('Ctrl Pts',(-0.483091837997484,1.4789401345226,
17.1175524811405));
#271234=CARTESIAN_POINT('Ctrl Pts',(-0.51396349263689,1.46849704245836,
17.1198068679091));
#271235=CARTESIAN_POINT('Ctrl Pts',(-0.556369258735124,1.45265081832783,
17.122891631052));
#271236=CARTESIAN_POINT('Ctrl Pts',(-0.56819702318692,1.44806536843342,
17.1237507116978));
#271237=CARTESIAN_POINT('Ctrl Pts',(-0.593487451078253,1.43790305407977,
17.1255874441537));
#271238=CARTESIAN_POINT('Ctrl Pts',(-0.606930548159199,1.43228065560838,
17.1265636503821));
#271239=CARTESIAN_POINT('Ctrl Pts',(-0.731178810506834,1.37825195711156,
17.1356023516139));
#271240=CARTESIAN_POINT('Ctrl Pts',(-0.836061665654816,1.31727086162147,
17.1433872438295));
#271241=CARTESIAN_POINT('Ctrl Pts',(-0.969733356535987,1.21709686757906,
17.1546861510329));
#271242=CARTESIAN_POINT('Ctrl Pts',(-1.00539032086086,1.18781192853032,
17.1578527409197));
#271243=CARTESIAN_POINT('Ctrl Pts',(-1.04792466465391,1.1495897878392,17.1618592656355));
#271244=CARTESIAN_POINT('Ctrl Pts',(-1.05607878154922,1.1421034887585,17.162638357859));
#271245=CARTESIAN_POINT('Ctrl Pts',(-1.06889932089553,1.13007825144332,
17.1638813911792));
#271246=CARTESIAN_POINT('Ctrl Pts',(-1.07361846144058,1.12559584643604,
17.1643429180008));
#271247=CARTESIAN_POINT('Ctrl Pts',(-1.08245495395808,1.11709650863134,
17.1652147407189));
#271248=CARTESIAN_POINT('Ctrl Pts',(-1.08657843861664,1.11308608474222,
17.1656247503448));
#271249=CARTESIAN_POINT('Ctrl Pts',(-1.09581847478791,1.10399912589227,
17.1665507822077));
#271250=CARTESIAN_POINT('Ctrl Pts',(-1.10092214563348,1.09890974409878,
17.1670673634063));
#271251=CARTESIAN_POINT('Ctrl Pts',(-1.11389916599741,1.08578791933433,
17.1683941292419));
#271252=CARTESIAN_POINT('Ctrl Pts',(-1.12172097738593,1.07770533742928,
17.1692065340253));
#271253=CARTESIAN_POINT('Ctrl Pts',(-1.1708443051417,1.02583012727984,17.1743912778714));
#271254=CARTESIAN_POINT('Ctrl Pts',(-1.20965656967211,0.979761730200339,
17.1788674967194));
#271255=CARTESIAN_POINT('Ctrl Pts',(-1.32008634431358,0.832094091443326,
17.1928491228821));
#271256=CARTESIAN_POINT('Ctrl Pts',(-1.38228342693806,0.724083098582645,
17.2026270303946));
#271257=CARTESIAN_POINT('Ctrl Pts',(-1.44662201997292,0.573112824702904,
17.2151374687387));
#271258=CARTESIAN_POINT('Ctrl Pts',(-1.46085374442986,0.535799023713378,
17.2181394134452));
#271259=CARTESIAN_POINT('Ctrl Pts',(-1.47589636177564,0.491284096185955,
17.2215848475293));
#271260=CARTESIAN_POINT('Ctrl Pts',(-1.47811191100088,0.484577462867704,
17.2221003645994));
#271261=CARTESIAN_POINT('Ctrl Pts',(-1.48145489454376,0.474221707980983,
17.222890640125));
#271262=CARTESIAN_POINT('Ctrl Pts',(-1.48261466186322,0.470583253172999,
17.2231672141938));
#271263=CARTESIAN_POINT('Ctrl Pts',(-1.48472660558073,0.463872291670716,
17.22367529662));
#271264=CARTESIAN_POINT('Ctrl Pts',(-1.48568264617349,0.460801119318555,
17.2239070211465));
#271265=CARTESIAN_POINT('Ctrl Pts',(-1.48781804113083,0.45386567286715,
17.2244285413521));
#271266=CARTESIAN_POINT('Ctrl Pts',(-1.48899186972508,0.449999761568095,
17.2247180134872));
#271267=CARTESIAN_POINT('Ctrl Pts',(-1.49240815865066,0.438588752321901,
17.2255689477027));
#271268=CARTESIAN_POINT('Ctrl Pts',(-1.49460847194814,0.431031006024629,
17.2261280376584));
#271269=CARTESIAN_POINT('Ctrl Pts',(-1.51144754253984,0.371511570518042,
17.2304981492817));
#271270=CARTESIAN_POINT('Ctrl Pts',(-1.52343154515495,0.318829667591794,
17.2341702780645));
#271271=CARTESIAN_POINT('Ctrl Pts',(-1.54778284418114,0.178322931254887,
17.243709188987));
#271272=CARTESIAN_POINT('Ctrl Pts',(-1.55542678203105,0.0898856949061964,
17.2494634277349));
#271273=CARTESIAN_POINT('Ctrl Pts',(-1.5555643000369,-0.0777392159181324,
17.2605816601617));
#271274=CARTESIAN_POINT('Ctrl Pts',(-1.54960862271705,-0.15663349341355,
17.2659036460172));
#271275=CARTESIAN_POINT('Ctrl Pts',(-1.53589951286607,-0.246441400897236,
17.2722493047636));
#271276=CARTESIAN_POINT('Ctrl Pts',(-1.53397753675704,-0.258134811300338,
17.2730810360388));
#271277=CARTESIAN_POINT('Ctrl Pts',(-1.53064038076691,-0.277082815583653,
17.2744382700025));
#271278=CARTESIAN_POINT('Ctrl Pts',(-1.5293067428239,-0.284351446066126,
17.2749611958606));
#271279=CARTESIAN_POINT('Ctrl Pts',(-1.52683942996924,-0.297279184021857,
17.275895445311));
#271280=CARTESIAN_POINT('Ctrl Pts',(-1.52572594961302,-0.302942045937434,
17.2763061208544));
#271281=CARTESIAN_POINT('Ctrl Pts',(-1.52331135952387,-0.31487093745215,
17.2771743134407));
#271282=CARTESIAN_POINT('Ctrl Pts',(-1.5220030453951,-0.321135380883416,
17.2776320529928));
#271283=CARTESIAN_POINT('Ctrl Pts',(-1.51843055118434,-0.33772877269013,
17.2788494276892));
#271284=CARTESIAN_POINT('Ctrl Pts',(-1.51609967535642,-0.348042851960356,
17.2796111774784));
#271285=CARTESIAN_POINT('Ctrl Pts',(-1.5044867037265,-0.397098278603461,
17.2832590184124));
#271286=CARTESIAN_POINT('Ctrl Pts',(-1.49382453463064,-0.435493983656121,
17.286188866976));
#271287=CARTESIAN_POINT('Ctrl Pts',(-1.43619853328125,-0.615845046848618,
17.3003234502519));
#271288=CARTESIAN_POINT('Ctrl Pts',(-1.37040185280259,-0.750943510157263,
17.3121309454437));
#271289=CARTESIAN_POINT('Ctrl Pts',(-1.26496539288794,-0.90603131375259,
17.3264141750078));
#271290=CARTESIAN_POINT('Ctrl Pts',(-1.24240560334809,-0.936727866878998,
17.3292759945909));
#271291=CARTESIAN_POINT('Ctrl Pts',(-1.21462243135818,-0.971759486173735,
17.3325566004207));
#271292=CARTESIAN_POINT('Ctrl Pts',(-1.21047208769491,-0.976924500056415,
17.3330406688579));
#271293=CARTESIAN_POINT('Ctrl Pts',(-1.20368721237451,-0.985258506381139,
17.3338221453396));
#271294=CARTESIAN_POINT('Ctrl Pts',(-1.20107292650043,-0.988443754554928,
17.3341209225585));
#271295=CARTESIAN_POINT('Ctrl Pts',(-1.19639194625467,-0.994101072580532,
17.3346516986926));
#271296=CARTESIAN_POINT('Ctrl Pts',(-1.19433020394037,-0.996577140129893,
17.3348840435856));
#271297=CARTESIAN_POINT('Ctrl Pts',(-1.18984740224431,-1.00192690759184,
17.3353861191417));
#271298=CARTESIAN_POINT('Ctrl Pts',(-1.18742362230327,-1.00479824382265,
17.335655647426));
#271299=CARTESIAN_POINT('Ctrl Pts',(-1.18059831963597,-1.01282466641958,
17.3364093203394));
#271300=CARTESIAN_POINT('Ctrl Pts',(-1.17617339823225,-1.01795989066736,
17.3368917966454));
#271301=CARTESIAN_POINT('Ctrl Pts',(-1.14927871464012,-1.04876230029075,
17.3397887209236));
#271302=CARTESIAN_POINT('Ctrl Pts',(-1.12600108223504,-1.0737159471893,
17.3421478902356));
#271303=CARTESIAN_POINT('Ctrl Pts',(-1.01257864251097,-1.18755506920908,
17.3530869096874));
#271304=CARTESIAN_POINT('Ctrl Pts',(-0.912621221041073,-1.26599002033087,
17.361191472381));
#271305=CARTESIAN_POINT('Ctrl Pts',(-0.749595222740299,-1.36446512563377,
17.3739176921002));
#271306=CARTESIAN_POINT('Ctrl Pts',(-0.692960729870463,-1.39408101267082,
17.378255078321));
#271307=CARTESIAN_POINT('Ctrl Pts',(-0.624280775254326,-1.42477482558215,
17.3835134132907));
#271308=CARTESIAN_POINT('Ctrl Pts',(-0.613839299660503,-1.42930440846725,
17.3843126891726));
#271309=CARTESIAN_POINT('Ctrl Pts',(-0.596668376026993,-1.43653041680071,
17.3856273349851));
#271310=CARTESIAN_POINT('Ctrl Pts',(-0.589967989060717,-1.43929516014522,
17.3861403911803));
#271311=CARTESIAN_POINT('Ctrl Pts',(-0.577912598806179,-1.44417118423408,
17.3870637134475));
#271312=CARTESIAN_POINT('Ctrl Pts',(-0.572564701082553,-1.44629977621355,
17.387473388467));
#271313=CARTESIAN_POINT('Ctrl Pts',(-0.561168972070333,-1.45076244032229,
17.3883465905612));
#271314=CARTESIAN_POINT('Ctrl Pts',(-0.555118134554774,-1.45308847900039,
17.3888103775251));
#271315=CARTESIAN_POINT('Ctrl Pts',(-0.538807193992186,-1.45924191802844,
17.3900610630777));
#271316=CARTESIAN_POINT('Ctrl Pts',(-0.5285210885085,-1.46299884321139,
17.3908502865333));
#271317=CARTESIAN_POINT('Ctrl Pts',(-0.476225403894931,-1.48147598227702,
17.394866136168));
#271318=CARTESIAN_POINT('Ctrl Pts',(-0.433641533703983,-1.49449523301362,
17.3981479766127));
#271319=CARTESIAN_POINT('Ctrl Pts',(-0.306706351760254,-1.52742146809097,
17.4079748907209));
#271320=CARTESIAN_POINT('Ctrl Pts',(-0.221190032584251,-1.54212730821209,
17.4146610622803));
#271321=CARTESIAN_POINT('Ctrl Pts',(-0.0476035777568375,-1.55723908488537,
17.428172722137));
#271322=CARTESIAN_POINT('Ctrl Pts',(0.0401942170759024,-1.55744900950112,
17.4349737173638));
#271323=CARTESIAN_POINT('Ctrl Pts',(0.139870214339904,-1.54924800501987,
17.4423820589408));
#271324=CARTESIAN_POINT('Ctrl Pts',(0.152178138610366,-1.54808749679548,
17.4432911709351));
#271325=CARTESIAN_POINT('Ctrl Pts',(0.169371344039356,-1.54625931798855,
17.444552022568));
#271326=CARTESIAN_POINT('Ctrl Pts',(0.174268848550884,-1.54571501282018,
17.4449101416354));
#271327=CARTESIAN_POINT('Ctrl Pts',(0.182161693362209,-1.54479981739838,
17.4454855292806));
#271328=CARTESIAN_POINT('Ctrl Pts',(0.185158630688581,-1.5444434726692,
17.4457035963151));
#271329=CARTESIAN_POINT('Ctrl Pts',(0.191471477455945,-1.54367421715733,
17.4461620503212));
#271330=CARTESIAN_POINT('Ctrl Pts',(0.194787125711285,-1.54325934031195,
17.4464023208941));
#271331=CARTESIAN_POINT('Ctrl Pts',(0.202940182094938,-1.54221247949117,
17.4469919150714));
#271332=CARTESIAN_POINT('Ctrl Pts',(0.207776058966439,-1.54156840926714,
17.4473405658007));
#271333=CARTESIAN_POINT('Ctrl Pts',(0.225478575423955,-1.53912586990373,
17.4486132439202));
#271334=CARTESIAN_POINT('Ctrl Pts',(0.238326048206005,-1.53718891341575,
17.4495298786573));
#271335=CARTESIAN_POINT('Ctrl Pts',(0.324254962320279,-1.52313052945659,
17.4556229183146));
#271336=CARTESIAN_POINT('Ctrl Pts',(0.396424431272561,-1.50596101982678,
17.4605590621444));
#271337=CARTESIAN_POINT('Ctrl Pts',(0.594575958919266,-1.44357866735489,
17.47427807543));
#271338=CARTESIAN_POINT('Ctrl Pts',(0.716329082674257,-1.38719439360538,
17.4829551333107));
#271339=CARTESIAN_POINT('Ctrl Pts',(0.844160802090589,-1.30662858782822,
17.4934514732183));
#271340=CARTESIAN_POINT('Ctrl Pts',(0.858788368133264,-1.29706137945197,
17.4946740659064));
#271341=CARTESIAN_POINT('Ctrl Pts',(0.879056386197448,-1.28331186013718,
17.4964001889486));
#271342=CARTESIAN_POINT('Ctrl Pts',(0.884834852460365,-1.27933449162295,
17.496896040153));
#271343=CARTESIAN_POINT('Ctrl Pts',(0.895390292746814,-1.27196336767508,
17.4978087951101));
#271344=CARTESIAN_POINT('Ctrl Pts',(0.900175396133304,-1.26858142802688,
17.4982252450285));
#271345=CARTESIAN_POINT('Ctrl Pts',(0.909855076808487,-1.26165783341647,
17.4990731844213));
#271346=CARTESIAN_POINT('Ctrl Pts',(0.914748352841473,-1.25811454108599,
17.4995047318337));
#271347=CARTESIAN_POINT('Ctrl Pts',(0.926817386233817,-1.24926754642543,
17.500576408885));
#271348=CARTESIAN_POINT('Ctrl Pts',(0.93396830432656,-1.2439304925656,17.5012178238799));
#271349=CARTESIAN_POINT('Ctrl Pts',(0.960721416522171,-1.22360270198446,
17.5036422559697));
#271350=CARTESIAN_POINT('Ctrl Pts',(0.98001089325329,-1.20820848037454,
17.5054410171653));
#271351=CARTESIAN_POINT('Ctrl Pts',(1.02747424977924,-1.1684451312156,17.5099995636182));
#271352=CARTESIAN_POINT('Ctrl Pts',(1.05515294055462,-1.14351179353789,
17.512780905484));
#271353=CARTESIAN_POINT('Ctrl Pts',(1.19069544862219,-1.01229926667695,
17.527041030381));
#271354=CARTESIAN_POINT('Ctrl Pts',(1.28350849502977,-0.891685862471345,
17.5390689531139));
#271355=CARTESIAN_POINT('Ctrl Pts',(1.36718971042241,-0.74214001425734,
17.5518969241535));
#271356=CARTESIAN_POINT('Ctrl Pts',(1.37661069057193,-0.724515432997913,
17.5533777007348));
#271357=CARTESIAN_POINT('Ctrl Pts',(1.38839684147589,-0.701405700235204,
17.555274906769));
#271358=CARTESIAN_POINT('Ctrl Pts',(1.39107321793935,-0.696082646801564,
17.5557088932698));
#271359=CARTESIAN_POINT('Ctrl Pts',(1.39530736332402,-0.687539384901019,
17.5564004617379));
#271360=CARTESIAN_POINT('Ctrl Pts',(1.39688468770652,-0.684329024586538,
17.5566592232629));
#271361=CARTESIAN_POINT('Ctrl Pts',(1.39987904725894,-0.678181052562585,
17.5571525961916));
#271362=CARTESIAN_POINT('Ctrl Pts',(1.40129790137036,-0.675244458583352,
17.5573873116029));
#271363=CARTESIAN_POINT('Ctrl Pts',(1.40462650090365,-0.668299599985734,
17.5579402098999));
#271364=CARTESIAN_POINT('Ctrl Pts',(1.40652833724146,-0.66428758849565,
17.5582579041266));
#271365=CARTESIAN_POINT('Ctrl Pts',(1.41276789502226,-0.650978020280832,
17.5593063566281));
#271366=CARTESIAN_POINT('Ctrl Pts',(1.4170309323208,-0.6416454315532,17.5600327118311));
#271367=CARTESIAN_POINT('Ctrl Pts',(1.4270234861773,-0.619184442842082,
17.5617614557874));
#271368=CARTESIAN_POINT('Ctrl Pts',(1.43266472277255,-0.606017517396869,
17.5627591650315));
#271369=CARTESIAN_POINT('Ctrl Pts',(1.45318464212921,-0.556234330639917,
17.5664796694373));
#271370=CARTESIAN_POINT('Ctrl Pts',(1.46684894186761,-0.519130922979059,
17.5691485122344));
#271371=CARTESIAN_POINT('Ctrl Pts',(1.52248940548107,-0.348228695388594,
17.5811458693348));
#271372=CARTESIAN_POINT('Ctrl Pts',(1.54766876886642,-0.209664333579345,
17.5901294631626));
#271373=CARTESIAN_POINT('Ctrl Pts',(1.55420874426898,-0.0636469458925181,
17.6001448968772));
#271374=CARTESIAN_POINT('Ctrl Pts',(1.55444114672544,-0.0576929314050126,
17.6005540967318));
#271375=CARTESIAN_POINT('Ctrl Pts',(1.55548393915306,-0.0263586577107222,
17.6027121701981));
#271376=CARTESIAN_POINT('Ctrl Pts',(1.55570691560009,-0.000963988855314317,
17.6044770347516));
#271377=CARTESIAN_POINT('Ctrl Pts',(1.55516192950211,0.0337410831718555,
17.6069159347291));
#271378=CARTESIAN_POINT('Ctrl Pts',(1.55493189003653,0.043056918905161,
17.6075732541421));
#271379=CARTESIAN_POINT('Ctrl Pts',(1.5544325627692,0.0578796041006588,
17.6086235937809));
#271380=CARTESIAN_POINT('Ctrl Pts',(1.55421767434555,0.0633881700060483,
17.6090149130737));
#271381=CARTESIAN_POINT('Ctrl Pts',(1.55371648378194,0.0746927957007798,
17.6098200463262));
#271382=CARTESIAN_POINT('Ctrl Pts',(1.55342701982006,0.0804886210664853,
17.6102339527805));
#271383=CARTESIAN_POINT('Ctrl Pts',(1.55268192440377,0.093900493853736,
17.6111944152708));
#271384=CARTESIAN_POINT('Ctrl Pts',(1.55220267921316,0.101515023115226,
17.6117417002655));
#271385=CARTESIAN_POINT('Ctrl Pts',(1.55050463073375,0.125659739615937,
17.6134835666887));
#271386=CARTESIAN_POINT('Ctrl Pts',(1.54907766158329,0.142173622688831,
17.6146846048149));
#271387=CARTESIAN_POINT('Ctrl Pts',(1.54058531952777,0.224997650445406,
17.6207592771234));
#271388=CARTESIAN_POINT('Ctrl Pts',(1.52952584874133,0.290818553216241,
17.6257557775075));
#271389=CARTESIAN_POINT('Ctrl Pts',(1.49455995587657,0.439666811062609,
17.6374320639716));
#271390=CARTESIAN_POINT('Ctrl Pts',(1.46789682906557,0.521812883171184,
17.6441592130327));
#271391=CARTESIAN_POINT('Ctrl Pts',(1.43457667260785,0.601306926959429,
17.650811911463));
#271392=CARTESIAN_POINT('Origin',(0.,0.,-1.29405622560371));
#271393=CARTESIAN_POINT('',(1.4345766894261,0.601306886835045,18.4895593986216));
#271394=CARTESIAN_POINT('',(1.43457668357356,0.601306900797837,18.3502241513278));
#271395=CARTESIAN_POINT('',(1.43457668357355,0.601306900797845,-1.29405622560371));
#271396=CARTESIAN_POINT('Ctrl Pts',(1.4345766894261,0.601306886835045,18.4895593986216));
#271397=CARTESIAN_POINT('Ctrl Pts',(1.44099262732833,0.585999969257908,
18.4883253124721));
#271398=CARTESIAN_POINT('Ctrl Pts',(1.44716375031046,0.570589955881822,
18.4870836263227));
#271399=CARTESIAN_POINT('Ctrl Pts',(1.50521501525075,0.418624171181762,
18.47484644818));
#271400=CARTESIAN_POINT('Ctrl Pts',(1.53785299730756,0.275529789507252,
18.4632869760968));
#271401=CARTESIAN_POINT('Ctrl Pts',(1.55271006181731,0.0983794845858045,
18.4498238883417));
#271402=CARTESIAN_POINT('Ctrl Pts',(1.55439400902584,0.0666835145531882,
18.4474515840324));
#271403=CARTESIAN_POINT('Ctrl Pts',(1.55525525106296,0.028368393556693,
18.4446443741028));
#271404=CARTESIAN_POINT('Ctrl Pts',(1.55536146467843,0.0217802678371933,
18.4441638484235));
#271405=CARTESIAN_POINT('Ctrl Pts',(1.55546184680569,0.0115023590345889,
18.4434177712575));
#271406=CARTESIAN_POINT('Ctrl Pts',(1.55548475348198,0.00781303948000507,
18.4431506805459));
#271407=CARTESIAN_POINT('Ctrl Pts',(1.55550297799219,0.000938469125552495,
18.4426543727589));
#271408=CARTESIAN_POINT('Ctrl Pts',(1.55550163873953,-0.00224665648035469,
18.4424249810905));
#271409=CARTESIAN_POINT('Ctrl Pts',(1.55547620170596,-0.00953092583499308,
18.4419016242649));
#271410=CARTESIAN_POINT('Ctrl Pts',(1.5554456843582,-0.0136299916416392,
18.4416080194258));
#271411=CARTESIAN_POINT('Ctrl Pts',(1.55532327272769,-0.0243694262571884,
18.4408410355608));
#271412=CARTESIAN_POINT('Ctrl Pts',(1.55520505607159,-0.0310095043566609,
18.4403690738874));
#271413=CARTESIAN_POINT('Ctrl Pts',(1.55409443362784,-0.0768826299381814,
18.4371228343138));
#271414=CARTESIAN_POINT('Ctrl Pts',(1.55165997838199,-0.116070700703275,
18.4344219490485));
#271415=CARTESIAN_POINT('Ctrl Pts',(1.53278910478316,-0.304348693341901,
18.4216134252618));
#271416=CARTESIAN_POINT('Ctrl Pts',(1.49633371708744,-0.450624091519519,
18.4120945941951));
#271417=CARTESIAN_POINT('Ctrl Pts',(1.42487850704468,-0.6251320705219,18.3992626610119));
#271418=CARTESIAN_POINT('Ctrl Pts',(1.40893616252026,-0.660278223834177,
18.3966018427199));
#271419=CARTESIAN_POINT('Ctrl Pts',(1.38706817648677,-0.704080880216519,
18.3931681062349));
#271420=CARTESIAN_POINT('Ctrl Pts',(1.38233861890689,-0.713321768556348,
18.3924369064952));
#271421=CARTESIAN_POINT('Ctrl Pts',(1.37458797847935,-0.72809882861183,
18.3912563192389));
#271422=CARTESIAN_POINT('Ctrl Pts',(1.37162504272376,-0.733665288023133,
18.3908089828107));
#271423=CARTESIAN_POINT('Ctrl Pts',(1.36591905692746,-0.744229724501757,
18.389954920219));
#271424=CARTESIAN_POINT('Ctrl Pts',(1.36318220897893,-0.749230950002752,
18.3895484196763));
#271425=CARTESIAN_POINT('Ctrl Pts',(1.35686907877674,-0.760618251300391,
18.3886177862348));
#271426=CARTESIAN_POINT('Ctrl Pts',(1.35327511571427,-0.766994314807492,
18.3880930273882));
#271427=CARTESIAN_POINT('Ctrl Pts',(1.34378293520718,-0.783560009482311,
18.3867198940818));
#271428=CARTESIAN_POINT('Ctrl Pts',(1.33781389059965,-0.79370828731514,
18.3858689842551));
#271429=CARTESIAN_POINT('Ctrl Pts',(1.29051723935601,-0.87207026867969,
18.379221095764));
#271430=CARTESIAN_POINT('Ctrl Pts',(1.24412093999459,-0.937070127111359,
18.373237264182));
#271431=CARTESIAN_POINT('Ctrl Pts',(1.12461686025537,-1.0798875346337,18.3589644413066));
#271432=CARTESIAN_POINT('Ctrl Pts',(1.04807677573844,-1.15431986270894,
18.3506025653542));
#271433=CARTESIAN_POINT('Ctrl Pts',(0.935112393364499,-1.24360426880536,
18.3396454061971));
#271434=CARTESIAN_POINT('Ctrl Pts',(0.904854885140763,-1.26579025872893,
18.336829731358));
#271435=CARTESIAN_POINT('Ctrl Pts',(0.868120824893188,-1.29073388894021,
18.3335750105203));
#271436=CARTESIAN_POINT('Ctrl Pts',(0.862393938066913,-1.29456727867069,
18.3330721523315));
#271437=CARTESIAN_POINT('Ctrl Pts',(0.853509059394139,-1.30042939840533,
18.3322992375892));
#271438=CARTESIAN_POINT('Ctrl Pts',(0.850368981347824,-1.30248490627538,
18.3320274586255));
#271439=CARTESIAN_POINT('Ctrl Pts',(0.844557515507106,-1.30625914072608,
18.3315270591057));
#271440=CARTESIAN_POINT('Ctrl Pts',(0.841888319921899,-1.30798103842754,
18.3312982348637));
#271441=CARTESIAN_POINT('Ctrl Pts',(0.835840795634892,-1.31185611356475,
18.3307820535295));
#271442=CARTESIAN_POINT('Ctrl Pts',(0.8324594165039,-1.31400442129854,18.3304950194327));
#271443=CARTESIAN_POINT('Ctrl Pts',(0.822427045266144,-1.32032406610473,
18.3296479518456));
#271444=CARTESIAN_POINT('Ctrl Pts',(0.815752597956168,-1.3244582251277,
18.3290902910988));
#271445=CARTESIAN_POINT('Ctrl Pts',(0.761437172958825,-1.35753488813396,
18.3245971366684));
#271446=CARTESIAN_POINT('Ctrl Pts',(0.71229676877724,-1.38395176898821,
18.3208102353864));
#271447=CARTESIAN_POINT('Ctrl Pts',(0.539473415545995,-1.46520700576085,
18.3080508928008));
#271448=CARTESIAN_POINT('Ctrl Pts',(0.410135161450797,-1.50653686145066,
18.2993841477549));
#271449=CARTESIAN_POINT('Ctrl Pts',(0.241384635176272,-1.53708477167178,
18.2876917611887));
#271450=CARTESIAN_POINT('Ctrl Pts',(0.205477170021583,-1.54229533969842,
18.2851866318275));
#271451=CARTESIAN_POINT('Ctrl Pts',(0.159313589844035,-1.54735349898748,
18.281928418628));
#271452=CARTESIAN_POINT('Ctrl Pts',(0.149194093412839,-1.54836196817265,
18.2812119192598));
#271453=CARTESIAN_POINT('Ctrl Pts',(0.132832027352404,-1.54983065965365,
18.2800494334376));
#271454=CARTESIAN_POINT('Ctrl Pts',(0.126595172320891,-1.55035256679105,
18.2796053859526));
#271455=CARTESIAN_POINT('Ctrl Pts',(0.114660944160205,-1.55127874356464,
18.2787538357524));
#271456=CARTESIAN_POINT('Ctrl Pts',(0.108964148856134,-1.55168930041261,
18.2783465372102));
#271457=CARTESIAN_POINT('Ctrl Pts',(0.0959960805833042,-1.55255211759448,
18.2774174598443));
#271458=CARTESIAN_POINT('Ctrl Pts',(0.0887236790606858,-1.55298468465123,
18.2768950734314));
#271459=CARTESIAN_POINT('Ctrl Pts',(0.0695389104639085,-1.55399061164669,
18.2755132662739));
#271460=CARTESIAN_POINT('Ctrl Pts',(0.057622730851717,-1.55447807553019,
18.274651186594));
#271461=CARTESIAN_POINT('Ctrl Pts',(-0.0464485217667476,-1.55753713248777,
18.2670873490543));
#271462=CARTESIAN_POINT('Ctrl Pts',(-0.138639676173716,-1.55204783098059,
18.2601321836644));
#271463=CARTESIAN_POINT('Ctrl Pts',(-0.32250845557302,-1.52458440797311,
18.2458108166579));
#271464=CARTESIAN_POINT('Ctrl Pts',(-0.413787248841978,-1.50238134171011,
18.2384695942592));
#271465=CARTESIAN_POINT('Ctrl Pts',(-0.537984195734153,-1.45998567522091,
18.2284832640889));
#271466=CARTESIAN_POINT('Ctrl Pts',(-0.57301114219307,-1.4465973777693,
18.2256692454341));
#271467=CARTESIAN_POINT('Ctrl Pts',(-0.613866109633851,-1.42926418844628,
18.2224162056396));
#271468=CARTESIAN_POINT('Ctrl Pts',(-0.620191007168949,-1.42653105129318,
18.2219134445991));
#271469=CARTESIAN_POINT('Ctrl Pts',(-0.629932434868032,-1.42224451458921,
18.2211406559713));
#271470=CARTESIAN_POINT('Ctrl Pts',(-0.633361747014747,-1.42072067275909,
18.2208689067071));
#271471=CARTESIAN_POINT('Ctrl Pts',(-0.639683885475553,-1.4178839403086,
18.2203685175538));
#271472=CARTESIAN_POINT('Ctrl Pts',(-0.642578185280274,-1.41657460717597,
18.2201396742988));
#271473=CARTESIAN_POINT('Ctrl Pts',(-0.649114309721366,-1.41359361886664,
18.2196234032342));
#271474=CARTESIAN_POINT('Ctrl Pts',(-0.652753694096921,-1.41191675469987,
18.2193362987182));
#271475=CARTESIAN_POINT('Ctrl Pts',(-0.663506702440633,-1.4069117898032,
18.2184889630306));
#271476=CARTESIAN_POINT('Ctrl Pts',(-0.670601789610282,-1.4035437916603,
18.2179311059489));
#271477=CARTESIAN_POINT('Ctrl Pts',(-0.727913745657558,-1.37580430717528,
18.2134324804981));
#271478=CARTESIAN_POINT('Ctrl Pts',(-0.776817761694269,-1.34879639978296,
18.2096406754315));
#271479=CARTESIAN_POINT('Ctrl Pts',(-0.939025099630886,-1.24745851724816,
18.1968625482307));
#271480=CARTESIAN_POINT('Ctrl Pts',(-1.04401443246632,-1.16101497075151,
18.1881821369283));
#271481=CARTESIAN_POINT('Ctrl Pts',(-1.16108416153649,-1.03574219593744,
18.1764894060544));
#271482=CARTESIAN_POINT('Ctrl Pts',(-1.18476015245662,-1.00857392364514,
18.1740008957899));
#271483=CARTESIAN_POINT('Ctrl Pts',(-1.21386745043356,-0.972732768074702,
18.170761357718));
#271484=CARTESIAN_POINT('Ctrl Pts',(-1.22018731831987,-0.964793306792589,
18.1700463785509));
#271485=CARTESIAN_POINT('Ctrl Pts',(-1.23027621267952,-0.951861235651385,
18.1688856971323));
#271486=CARTESIAN_POINT('Ctrl Pts',(-1.23409367329407,-0.946906634720758,
18.1684419216164));
#271487=CARTESIAN_POINT('Ctrl Pts',(-1.24134136563078,-0.937381734916853,
18.1675904464395));
#271488=CARTESIAN_POINT('Ctrl Pts',(-1.24477650538448,-0.932815283441667,
18.1671829484996));
#271489=CARTESIAN_POINT('Ctrl Pts',(-1.25254099298447,-0.922374415461869,
18.166252797018));
#271490=CARTESIAN_POINT('Ctrl Pts',(-1.25685429177768,-0.916488290859181,
18.1657295316527));
#271491=CARTESIAN_POINT('Ctrl Pts',(-1.26812975415566,-0.900871979136829,
18.1643440601856));
#271492=CARTESIAN_POINT('Ctrl Pts',(-1.27502122562983,-0.891091608917545,
18.1634791736943));
#271493=CARTESIAN_POINT('Ctrl Pts',(-1.33583058462001,-0.802641244987016,
18.1556808901109));
#271494=CARTESIAN_POINT('Ctrl Pts',(-1.38250890604917,-0.719262747387282,
18.1484753071038));
#271495=CARTESIAN_POINT('Ctrl Pts',(-1.45859351186842,-0.548203239973813,
18.1340376678064));
#271496=CARTESIAN_POINT('Ctrl Pts',(-1.48842150298396,-0.46111144524232,
18.1268469235825));
#271497=CARTESIAN_POINT('Ctrl Pts',(-1.51903955266582,-0.33676149716116,
18.1171117755219));
#271498=CARTESIAN_POINT('Ctrl Pts',(-1.52646272842221,-0.301332924161396,
18.1143977850868));
#271499=CARTESIAN_POINT('Ctrl Pts',(-1.53381012171295,-0.258946677652709,
18.1112449967756));
#271500=CARTESIAN_POINT('Ctrl Pts',(-1.53493203790112,-0.252211250704046,
18.1107468094738));
#271501=CARTESIAN_POINT('Ctrl Pts',(-1.53659976130025,-0.241775535931313,
18.1099794957395));
#271502=CARTESIAN_POINT('Ctrl Pts',(-1.53717661765396,-0.238080413183043,
18.1097086860612));
#271503=CARTESIAN_POINT('Ctrl Pts',(-1.53821903976589,-0.231241295104207,
18.1092091366221));
#271504=CARTESIAN_POINT('Ctrl Pts',(-1.53868829352599,-0.228097975855216,
18.108980199246));
#271505=CARTESIAN_POINT('Ctrl Pts',(-1.53972997980427,-0.220970672634736,
18.1084625742004));
#271506=CARTESIAN_POINT('Ctrl Pts',(-1.54029658535265,-0.216985895878232,
18.1081742169543));
#271507=CARTESIAN_POINT('Ctrl Pts',(-1.54193456342525,-0.205136657505268,
18.1073197168071));
#271508=CARTESIAN_POINT('Ctrl Pts',(-1.54296123858723,-0.197265986512507,
18.1067560080165));
#271509=CARTESIAN_POINT('Ctrl Pts',(-1.55158387649242,-0.126972417229791,
18.101753254382));
#271510=CARTESIAN_POINT('Ctrl Pts',(-1.55544934855044,-0.0641411672581848,
18.0975039681037));
#271511=CARTESIAN_POINT('Ctrl Pts',(-1.55557649265697,0.0953077447216411,
18.086895551804));
#271512=CARTESIAN_POINT('Ctrl Pts',(-1.54666464037744,0.191652626258326,
18.080636899838));
#271513=CARTESIAN_POINT('Ctrl Pts',(-1.51722265917634,0.348739012408554,
18.0699541997557));
#271514=CARTESIAN_POINT('Ctrl Pts',(-1.5017850109423,0.410150797896472,
18.0656549407979));
#271515=CARTESIAN_POINT('Ctrl Pts',(-1.47924411408363,0.481190341075226,
18.0604445189198));
#271516=CARTESIAN_POINT('Ctrl Pts',(-1.47571860479897,0.491896209664127,
18.0596528927329));
#271517=CARTESIAN_POINT('Ctrl Pts',(-1.46976139478114,0.509345723631646,
18.0583516364342));
#271518=CARTESIAN_POINT('Ctrl Pts',(-1.46739882868512,0.516112679786625,
18.0578442823139));
#271519=CARTESIAN_POINT('Ctrl Pts',(-1.46307895049382,0.528216380201834,
18.056931790686));
#271520=CARTESIAN_POINT('Ctrl Pts',(-1.46113898069707,0.533559216215017,
18.0565272341718));
#271521=CARTESIAN_POINT('Ctrl Pts',(-1.45695499241949,0.544888309948024,
18.0556655862453));
#271522=CARTESIAN_POINT('Ctrl Pts',(-1.45470327195844,0.550871589894027,
18.0552082443756));
#271523=CARTESIAN_POINT('Ctrl Pts',(-1.44855700065793,0.566902987328941,
18.0539766305722));
#271524=CARTESIAN_POINT('Ctrl Pts',(-1.44459486962785,0.576924633703933,
18.0532001098454));
#271525=CARTESIAN_POINT('Ctrl Pts',(-1.42415751167201,0.627087187710649,
18.0492792102401));
#271526=CARTESIAN_POINT('Ctrl Pts',(-1.40611350201907,0.666563643426204,
18.0460823718672));
#271527=CARTESIAN_POINT('Ctrl Pts',(-1.30859408566014,0.858281378753664,
18.0299791444942));
#271528=CARTESIAN_POINT('Ctrl Pts',(-1.20596047058541,0.9973504821537,18.0162626550089));
#271529=CARTESIAN_POINT('Ctrl Pts',(-1.07140623721043,1.12779282998613,
18.0023113678841));
#271530=CARTESIAN_POINT('Ctrl Pts',(-1.0599389199155,1.13857697586493,18.0011496421168));
#271531=CARTESIAN_POINT('Ctrl Pts',(-1.04432374498317,1.15282143830702,
17.9996061082658));
#271532=CARTESIAN_POINT('Ctrl Pts',(-1.04031922357721,1.15643645235584,
17.9992135808113));
#271533=CARTESIAN_POINT('Ctrl Pts',(-1.03399674381684,1.16208454444556,
17.9985991382254));
#271534=CARTESIAN_POINT('Ctrl Pts',(-1.0316914626088,1.16413164251117,17.998376197177));
#271535=CARTESIAN_POINT('Ctrl Pts',(-1.02696427770189,1.16830432923321,
17.9979212975794));
#271536=CARTESIAN_POINT('Ctrl Pts',(-1.02454188864819,1.17042921699715,
17.9976893990028));
#271537=CARTESIAN_POINT('Ctrl Pts',(-1.01879854225242,1.17543571148285,
17.9971423927193));
#271538=CARTESIAN_POINT('Ctrl Pts',(-1.01547194286804,1.17831078924332,
17.9968277672999));
#271539=CARTESIAN_POINT('Ctrl Pts',(-1.00438672081637,1.18780959450976,
17.9957864605753));
#271540=CARTESIAN_POINT('Ctrl Pts',(-0.996574914238254,1.19437128764136,
17.995064147019));
#271541=CARTESIAN_POINT('Ctrl Pts',(-0.977688205756535,1.20992125257977,
17.993343548437));
#271542=CARTESIAN_POINT('Ctrl Pts',(-0.96655293761215,1.2188351481963,17.992349926939));
#271543=CARTESIAN_POINT('Ctrl Pts',(-0.924167320144902,1.25181900548173,
17.9886384379965));
#271544=CARTESIAN_POINT('Ctrl Pts',(-0.892125765467794,1.27485221686184,
17.9859745206246));
#271545=CARTESIAN_POINT('Ctrl Pts',(-0.74230372613235,1.3741340559806,17.9739763288162));
#271546=CARTESIAN_POINT('Ctrl Pts',(-0.615428649756594,1.43544676418496,
17.9649902542972));
#271547=CARTESIAN_POINT('Ctrl Pts',(-0.476515378732291,1.48072524226858,
17.9549813409096));
#271548=CARTESIAN_POINT('Ctrl Pts',(-0.470969682316836,1.48249846751525,
17.9545816218799));
#271549=CARTESIAN_POINT('Ctrl Pts',(-0.440813428220075,1.49195458292039,
17.952406962847));
#271550=CARTESIAN_POINT('Ctrl Pts',(-0.416025975249983,1.49905543951122,
17.9506154867378));
#271551=CARTESIAN_POINT('Ctrl Pts',(-0.38206743833399,1.50787642984636,
17.9481502600115));
#271552=CARTESIAN_POINT('Ctrl Pts',(-0.373039533313863,1.51013521082684,
17.9474938497226));
#271553=CARTESIAN_POINT('Ctrl Pts',(-0.358680243632234,1.5135912866127,
17.9464479295517));
#271554=CARTESIAN_POINT('Ctrl Pts',(-0.353361774722541,1.5148417590165,
17.9460601312896));
#271555=CARTESIAN_POINT('Ctrl Pts',(-0.34246141974605,1.51734411063948,
17.9452644434042));
#271556=CARTESIAN_POINT('Ctrl Pts',(-0.336879001227993,1.5185932671491,
17.9448564733315));
#271557=CARTESIAN_POINT('Ctrl Pts',(-0.32399197203918,1.52140239328206,
17.9439135178281));
#271558=CARTESIAN_POINT('Ctrl Pts',(-0.316682813591592,1.52294058721888,
17.9433778464958));
#271559=CARTESIAN_POINT('Ctrl Pts',(-0.29366551257478,1.527611657187,17.9416881050753));
#271560=CARTESIAN_POINT('Ctrl Pts',(-0.277920348728082,1.53055449185459,
17.9405280402885));
#271561=CARTESIAN_POINT('Ctrl Pts',(-0.19999858621564,1.54387640563394,
17.9347643142724));
#271562=CARTESIAN_POINT('Ctrl Pts',(-0.137284555786867,1.55071104944769,
17.9300510861638));
#271563=CARTESIAN_POINT('Ctrl Pts',(0.0361201960514034,1.55900742080409,
17.9168239847331));
#271564=CARTESIAN_POINT('Ctrl Pts',(0.146815121103837,1.55249844714107,
17.9081425744055));
#271565=CARTESIAN_POINT('Ctrl Pts',(0.269268730094863,1.53207664963422,
17.8986468272466));
#271566=CARTESIAN_POINT('Ctrl Pts',(0.282628592492905,1.52966846341167,
17.8976127506854));
#271567=CARTESIAN_POINT('Ctrl Pts',(0.327151869831379,1.52103966651652,
17.8941762651607));
#271568=CARTESIAN_POINT('Ctrl Pts',(0.358158504806672,1.51403859420429,
17.8917988869589));
#271569=CARTESIAN_POINT('Ctrl Pts',(0.394973212107597,1.50453160422406,
17.8890116289492));
#271570=CARTESIAN_POINT('Ctrl Pts',(0.401005607914505,1.50293502598157,
17.88855606867));
#271571=CARTESIAN_POINT('Ctrl Pts',(0.410867149888422,1.50026139541515,
17.8878134090439));
#271572=CARTESIAN_POINT('Ctrl Pts',(0.414701984828125,1.49920590119147,
17.88752512811));
#271573=CARTESIAN_POINT('Ctrl Pts',(0.421590857204795,1.49728136327028,
17.8870082415381));
#271574=CARTESIAN_POINT('Ctrl Pts',(0.424646302092774,1.49641767244223,
17.886779336226));
#271575=CARTESIAN_POINT('Ctrl Pts',(0.431330511419027,1.49450610738197,
17.8862793453093));
#271576=CARTESIAN_POINT('Ctrl Pts',(0.434958105813315,1.49345437228297,
17.8860084866318));
#271577=CARTESIAN_POINT('Ctrl Pts',(0.445299775302416,1.49041517296627,
17.885237622148));
#271578=CARTESIAN_POINT('Ctrl Pts',(0.452004426932,1.48839553904711,17.8847394373079));
#271579=CARTESIAN_POINT('Ctrl Pts',(0.496860322581334,1.47455259494447,
17.8814155974756));
#271580=CARTESIAN_POINT('Ctrl Pts',(0.534561657787864,1.4613076527429,17.8786663079853));
#271581=CARTESIAN_POINT('Ctrl Pts',(0.688105264841811,1.40062625548094,
17.8674914553822));
#271582=CARTESIAN_POINT('Ctrl Pts',(0.798524167917304,1.34074840299653,
17.8594733432572));
#271583=CARTESIAN_POINT('Ctrl Pts',(0.922297338057383,1.25285966460046,
17.8493050660907));
#271584=CARTESIAN_POINT('Ctrl Pts',(0.943614365476525,1.23688380156222,
17.8475078655875));
#271585=CARTESIAN_POINT('Ctrl Pts',(0.99292362052183,1.19791258758639,17.8432249904034));
#271586=CARTESIAN_POINT('Ctrl Pts',(1.02054225539802,1.17447223755887,17.8407254398259));
#271587=CARTESIAN_POINT('Ctrl Pts',(1.05514124593311,1.14296509702396,17.8374444712517));
#271588=CARTESIAN_POINT('Ctrl Pts',(1.06289331718636,1.13575967894952,17.8366991783033));
#271589=CARTESIAN_POINT('Ctrl Pts',(1.07517826454215,1.12410510146682,17.8355012855254));
#271590=CARTESIAN_POINT('Ctrl Pts',(1.07975856652805,1.11970621839984,17.8350508474147));
#271591=CARTESIAN_POINT('Ctrl Pts',(1.08798451491493,1.11170867816885,17.8342348713813));
#271592=CARTESIAN_POINT('Ctrl Pts',(1.09163958553006,1.10811980577965,17.8338697634288));
#271593=CARTESIAN_POINT('Ctrl Pts',(1.10021689213668,1.09961422434851,17.8330068972699));
#271594=CARTESIAN_POINT('Ctrl Pts',(1.10512396492404,1.09468245229901,17.8325084785688));
#271595=CARTESIAN_POINT('Ctrl Pts',(1.11939387742573,1.08014697590798,17.8310448570047));
#271596=CARTESIAN_POINT('Ctrl Pts',(1.12866557302372,1.07045511147971,17.8300757255545));
#271597=CARTESIAN_POINT('Ctrl Pts',(1.21529253635949,0.977525729089931,
17.8208441503756));
#271598=CARTESIAN_POINT('Ctrl Pts',(1.28341652657203,0.886185021926734,
17.8121871100004));
#271599=CARTESIAN_POINT('Ctrl Pts',(1.37635065837062,0.728087679216828,
17.7979817476697));
#271600=CARTESIAN_POINT('Ctrl Pts',(1.4076174574621,0.66562528914666,17.7925493084874));
#271601=CARTESIAN_POINT('Ctrl Pts',(1.43457675882332,0.601306721269597,
17.7872340762022));
#271602=CARTESIAN_POINT('',(-1.55549978108786,-0.000825248823992286,17.9559437744364));
#271603=CARTESIAN_POINT('Ctrl Pts',(1.43457667260785,0.601306926959429,
17.650811911463));
#271604=CARTESIAN_POINT('Ctrl Pts',(1.43113399608224,0.609520342128201,
17.651499275844));
#271605=CARTESIAN_POINT('Ctrl Pts',(1.42762025295567,0.617705455986721,
17.6521857231963));
#271606=CARTESIAN_POINT('Ctrl Pts',(1.4021602503384,0.675635147384968,17.6570526399232));
#271607=CARTESIAN_POINT('Ctrl Pts',(1.37768732429456,0.724234300833138,
17.6611822828632));
#271608=CARTESIAN_POINT('Ctrl Pts',(1.34680672295463,0.778302022177472,
17.6657568881588));
#271609=CARTESIAN_POINT('Ctrl Pts',(1.34284518487173,0.785117318104389,
17.6663331255922));
#271610=CARTESIAN_POINT('Ctrl Pts',(1.33677383223619,0.795381866662972,
17.6672000637687));
#271611=CARTESIAN_POINT('Ctrl Pts',(1.33470217901971,0.798853357438681,
17.6674931005432));
#271612=CARTESIAN_POINT('Ctrl Pts',(1.33095784951244,0.805072543159744,
17.6680177285659));
#271613=CARTESIAN_POINT('Ctrl Pts',(1.32929017148378,0.807823147454503,
17.6682496327848));
#271614=CARTESIAN_POINT('Ctrl Pts',(1.32562502644105,0.813826214088698,
17.6687554725779));
#271615=CARTESIAN_POINT('Ctrl Pts',(1.32362412003024,0.817076500203668,
17.6690291795223));
#271616=CARTESIAN_POINT('Ctrl Pts',(1.31789148072096,0.826312317648029,
17.6698065323808));
#271617=CARTESIAN_POINT('Ctrl Pts',(1.31413090669652,0.832279980745032,
17.6703083375393));
#271618=CARTESIAN_POINT('Ctrl Pts',(1.28893439363693,0.871667805203456,
17.6736186503033));
#271619=CARTESIAN_POINT('Ctrl Pts',(1.26626397475577,0.904285825314207,
17.6763519054269));
#271620=CARTESIAN_POINT('Ctrl Pts',(1.16873821955681,1.03373279638744,17.6873240216271));
#271621=CARTESIAN_POINT('Ctrl Pts',(1.08383150223828,1.12243752577813,17.6951732857353));
#271622=CARTESIAN_POINT('Ctrl Pts',(0.941467757430883,1.23978923026179,
17.7075132449342));
#271623=CARTESIAN_POINT('Ctrl Pts',(0.89121749146488,1.27638894317095,17.7117364742955));
#271624=CARTESIAN_POINT('Ctrl Pts',(0.829388377278725,1.31598755565156,
17.7168692343652));
#271625=CARTESIAN_POINT('Ctrl Pts',(0.819792158598439,1.32198681226502,
17.7176640451095));
#271626=CARTESIAN_POINT('Ctrl Pts',(0.803960559703583,1.33164556993064,
17.7189728238172));
#271627=CARTESIAN_POINT('Ctrl Pts',(0.797763494663612,1.33536733106362,
17.7194845132424));
#271628=CARTESIAN_POINT('Ctrl Pts',(0.786587428259023,1.34197376172988,
17.7204063394339));
#271629=CARTESIAN_POINT('Ctrl Pts',(0.781617903023633,1.34487427349591,
17.7208158930284));
#271630=CARTESIAN_POINT('Ctrl Pts',(0.771004975045411,1.35098991959559,
17.7216898723472));
#271631=CARTESIAN_POINT('Ctrl Pts',(0.765357315606547,1.35419740491497,
17.7221545634451));
#271632=CARTESIAN_POINT('Ctrl Pts',(0.750084715597447,1.36274514349672,
17.7234102393004));
#271633=CARTESIAN_POINT('Ctrl Pts',(0.740423065030309,1.36801866942586,
17.7242035811303));
#271634=CARTESIAN_POINT('Ctrl Pts',(0.690742500299907,1.39445487636839,
17.7282786178758));
#271635=CARTESIAN_POINT('Ctrl Pts',(0.64987342773491,1.41396370334272,17.7316175054669));
#271636=CARTESIAN_POINT('Ctrl Pts',(0.526052398128402,1.46656684796264,
17.7417048207064));
#271637=CARTESIAN_POINT('Ctrl Pts',(0.441046210272524,1.49433061930852,
17.7486041154104));
#271638=CARTESIAN_POINT('Ctrl Pts',(0.312158981485861,1.52446574335081,
17.7588683380363));
#271639=CARTESIAN_POINT('Ctrl Pts',(0.269786358485031,1.5325320825178,17.7622098542381));
#271640=CARTESIAN_POINT('Ctrl Pts',(0.217100737758217,1.54030852184419,
17.7662925857506));
#271641=CARTESIAN_POINT('Ctrl Pts',(0.20705484337072,1.54169107540618,17.7670678256692));
#271642=CARTESIAN_POINT('Ctrl Pts',(0.158748951216467,1.54785842372358,
17.7707781516433));
#271643=CARTESIAN_POINT('Ctrl Pts',(0.120329485984408,1.55131826431919,
17.773676970177));
#271644=CARTESIAN_POINT('Ctrl Pts',(0.0751777223401169,1.55369648523671,
17.776994655763));
#271645=CARTESIAN_POINT('Ctrl Pts',(0.0685356704071852,1.55400364358276,
17.7774804427378));
#271646=CARTESIAN_POINT('Ctrl Pts',(0.057767335211512,1.55443244379102,
17.7782641396524));
#271647=CARTESIAN_POINT('Ctrl Pts',(0.0536422719712951,1.55458026330299,
17.7785634311973));
#271648=CARTESIAN_POINT('Ctrl Pts',(0.0462955853778806,1.55481425072788,
17.7790947671676));
#271649=CARTESIAN_POINT('Ctrl Pts',(0.0430742423888775,1.55490682867004,
17.7793271605005));
#271650=CARTESIAN_POINT('Ctrl Pts',(0.0361011483696269,1.55508554081373,
17.7798289384273));
#271651=CARTESIAN_POINT('Ctrl Pts',(0.0323493702975275,1.55516811027254,
17.7800981228477));
#271652=CARTESIAN_POINT('Ctrl Pts',(0.0218426313284958,1.55536130532916,
17.780849845549));
#271653=CARTESIAN_POINT('Ctrl Pts',(0.0150870844119887,1.55544150484054,
17.7813307294216));
#271654=CARTESIAN_POINT('Ctrl Pts',(-0.025368272809293,1.55565818184316,
17.7841969575686));
#271655=CARTESIAN_POINT('Ctrl Pts',(-0.059067829802532,1.55474350001894,
17.7865283783039));
#271656=CARTESIAN_POINT('Ctrl Pts',(-0.267821558628838,1.54227876786996,
17.8007700496928));
#271657=CARTESIAN_POINT('Ctrl Pts',(-0.439902145632824,1.50228153164371,
17.8117827128674));
#271658=CARTESIAN_POINT('Ctrl Pts',(-0.62275574276581,1.4255795557092,17.825468268183));
#271659=CARTESIAN_POINT('Ctrl Pts',(-0.643617041614602,1.41628344441866,
17.8270583972346));
#271660=CARTESIAN_POINT('Ctrl Pts',(-0.672336860873234,1.40271988573675,
17.829291769397));
#271661=CARTESIAN_POINT('Ctrl Pts',(-0.680375361178384,1.39883855190258,
17.8299217786094));
#271662=CARTESIAN_POINT('Ctrl Pts',(-0.693256533989951,1.39248167024186,
17.8309394626847));
#271663=CARTESIAN_POINT('Ctrl Pts',(-0.698120494706753,1.39004949458005,
17.8313256266196));
#271664=CARTESIAN_POINT('Ctrl Pts',(-0.708080530036251,1.3850036151129,
17.8321203162579));
#271665=CARTESIAN_POINT('Ctrl Pts',(-0.713175116901813,1.38238717511097,
17.8325289329897));
#271666=CARTESIAN_POINT('Ctrl Pts',(-0.725032372407305,1.37621462278791,
17.8334850103942));
#271667=CARTESIAN_POINT('Ctrl Pts',(-0.731783467495394,1.37263672610601,
17.8340332316358));
#271668=CARTESIAN_POINT('Ctrl Pts',(-0.745991264066383,1.36497237430686,
17.8351952957927));
#271669=CARTESIAN_POINT('Ctrl Pts',(-0.753441341533812,1.36087423673705,
17.8358095404717));
#271670=CARTESIAN_POINT('Ctrl Pts',(-0.773418794734829,1.34967071355989,
17.8374700792865));
#271671=CARTESIAN_POINT('Ctrl Pts',(-0.78588143304076,1.34245223919781,
17.8385203643568));
#271672=CARTESIAN_POINT('Ctrl Pts',(-0.824391243673544,1.31942698949943,
17.8418116476528));
#271673=CARTESIAN_POINT('Ctrl Pts',(-0.850074070661018,1.3030281449115,
17.8440732757223));
#271674=CARTESIAN_POINT('Ctrl Pts',(-0.976087522835685,1.21725527815718,
17.8555111960299));
#271675=CARTESIAN_POINT('Ctrl Pts',(-1.06848669106969,1.13700741940009,
17.8650590748476));
#271676=CARTESIAN_POINT('Ctrl Pts',(-1.15155213513869,1.04571035665813,
17.8745639570488));
#271677=CARTESIAN_POINT('Ctrl Pts',(-1.15255325501982,1.04460684677261,
17.8746786575593));
#271678=CARTESIAN_POINT('Ctrl Pts',(-1.19086295786352,1.00225688587125,
17.8790734425361));
#271679=CARTESIAN_POINT('Ctrl Pts',(-1.22593911208545,0.959035083441107,
17.8833010737216));
#271680=CARTESIAN_POINT('Ctrl Pts',(-1.26327927075591,0.90761687570065,
17.8879701280684));
#271681=CARTESIAN_POINT('Ctrl Pts',(-1.26788178564335,0.901176283363509,
17.888548811554));
#271682=CARTESIAN_POINT('Ctrl Pts',(-1.27476436756329,0.891387938531102,
17.8894186941819));
#271683=CARTESIAN_POINT('Ctrl Pts',(-1.27708076411719,0.888066085771792,
17.8897122524698));
#271684=CARTESIAN_POINT('Ctrl Pts',(-1.2812139900587,0.882089174140487,
17.8902374322009));
#271685=CARTESIAN_POINT('Ctrl Pts',(-1.28303557102551,0.879437504082222,
17.8904693696341));
#271686=CARTESIAN_POINT('Ctrl Pts',(-1.28699709807433,0.873632212847786,
17.8909748359383));
#271687=CARTESIAN_POINT('Ctrl Pts',(-1.28913368283199,0.870476376708512,
17.8912481386878));
#271688=CARTESIAN_POINT('Ctrl Pts',(-1.29517669275266,0.861479518671514,
17.8920232002549));
#271689=CARTESIAN_POINT('Ctrl Pts',(-1.29905523447166,0.855619734056771,
17.8925231352883));
#271690=CARTESIAN_POINT('Ctrl Pts',(-1.32425891917043,0.816975003872333,
17.8957897358448));
#271691=CARTESIAN_POINT('Ctrl Pts',(-1.34438303107358,0.783418633132571,
17.8984834134827));
#271692=CARTESIAN_POINT('Ctrl Pts',(-1.43199947549411,0.623980637876081,
17.9108063631384));
#271693=CARTESIAN_POINT('Ctrl Pts',(-1.48321658409031,0.489947597489042,
17.9198939126238));
#271694=CARTESIAN_POINT('Ctrl Pts',(-1.52412099448071,0.313243439519537,
17.9321711032087));
#271695=CARTESIAN_POINT('Ctrl Pts',(-1.53141486931275,0.275380383841871,
17.9348134062791));
#271696=CARTESIAN_POINT('Ctrl Pts',(-1.53956781459652,0.222560673256452,
17.9385378446545));
#271697=CARTESIAN_POINT('Ctrl Pts',(-1.54162920738253,0.207801994766207,
17.9395825620292));
#271698=CARTESIAN_POINT('Ctrl Pts',(-1.54438533709497,0.185762283358565,
17.9411497354098));
#271699=CARTESIAN_POINT('Ctrl Pts',(-1.5452413216916,0.178501960203745,
17.9416671290568));
#271700=CARTESIAN_POINT('Ctrl Pts',(-1.54665236575565,0.165762002719634,
17.9425771300317));
#271701=CARTESIAN_POINT('Ctrl Pts',(-1.54722956586231,0.160284906143858,
17.9429690356483));
#271702=CARTESIAN_POINT('Ctrl Pts',(-1.54831303645293,0.149452100981205,
17.9437455629745));
#271703=CARTESIAN_POINT('Ctrl Pts',(-1.54882063450804,0.144096599955775,
17.944130137285));
#271704=CARTESIAN_POINT('Ctrl Pts',(-1.54985769130544,0.13251574111988,
17.9449632594407));
#271705=CARTESIAN_POINT('Ctrl Pts',(-1.55037744169917,0.126289631802385,
17.9454121050563));
#271706=CARTESIAN_POINT('Ctrl Pts',(-1.55154844155662,0.111163472316023,
17.9465049253662));
#271707=CARTESIAN_POINT('Ctrl Pts',(-1.55216063089044,0.102260714930382,
17.9471501078678));
#271708=CARTESIAN_POINT('Ctrl Pts',(-1.55458343907947,0.0619634477458824,
17.9500797668325));
#271709=CARTESIAN_POINT('Ctrl Pts',(-1.55551823661414,0.0305261394203842,
17.9523910747632));
#271710=CARTESIAN_POINT('Ctrl Pts',(-1.55549973056384,-0.000915541269661115,
17.9547299826528));
#271711=CARTESIAN_POINT('Ctrl Pts',(-1.55549978108786,-0.000825248823992286,
17.9559437744364));
#271712=CARTESIAN_POINT('Ctrl Pts',(-1.55546570367139,-0.0650572868587075,
17.9605236044809));
#271713=CARTESIAN_POINT('Ctrl Pts',(-1.55144892983626,-0.12914984215493,
17.9651034345255));
#271714=CARTESIAN_POINT('Ctrl Pts',(-1.54352576552891,-0.192635565637285,
17.9696832645701));
#271715=CARTESIAN_POINT('Ctrl Pts',(-1.53557083843072,-0.256375793971246,
17.9742814544742));
#271716=CARTESIAN_POINT('Ctrl Pts',(-1.52367828485016,-0.319504020046929,
17.9788796443784));
#271717=CARTESIAN_POINT('Ctrl Pts',(-1.5079750791896,-0.381564425154021,
17.9834778342825));
#271718=CARTESIAN_POINT('Ctrl Pts',(-1.492194322415,-0.443931318863357,
17.9880987325913));
#271719=CARTESIAN_POINT('Ctrl Pts',(-1.47256533691098,-0.505219534397231,
17.9927196309002));
#271720=CARTESIAN_POINT('Ctrl Pts',(-1.44926486241833,-0.56498814904349,
17.997340529209));
#271721=CARTESIAN_POINT('Ctrl Pts',(-1.44470837165074,-0.576676114492983,
17.9982441623299));
#271722=CARTESIAN_POINT('Ctrl Pts',(-1.44001162060527,-0.588306042235484,
17.9991477954507));
#271723=CARTESIAN_POINT('Ctrl Pts',(-1.43517613547869,-0.599874745386444,
18.0000514285715));
#271724=CARTESIAN_POINT('Ctrl Pts',(-1.4129793509677,-0.652979657136013,
18.0041994611131));
#271725=CARTESIAN_POINT('Ctrl Pts',(-1.38778447851346,-0.704962388747883,
18.0083474936548));
#271726=CARTESIAN_POINT('Ctrl Pts',(-1.35972678115222,-0.755462329052493,
18.0124955261964));
#271727=CARTESIAN_POINT('Ctrl Pts',(-1.33171897319288,-0.805872475394861,
18.0166361831199));
#271728=CARTESIAN_POINT('Ctrl Pts',(-1.30085869485994,-0.854804612100729,
18.0207768400434));
#271729=CARTESIAN_POINT('Ctrl Pts',(-1.26732882366757,-0.901919011165288,
18.0249174969668));
#271730=CARTESIAN_POINT('Ctrl Pts',(-1.23383230732935,-0.948986541755466,
18.0290540348465));
#271731=CARTESIAN_POINT('Ctrl Pts',(-1.19767176020619,-0.99423949518981,
18.0331905727262));
#271732=CARTESIAN_POINT('Ctrl Pts',(-1.15907453297798,-1.03736516087725,
18.0373271106059));
#271733=CARTESIAN_POINT('Ctrl Pts',(-1.12050086338133,-1.08046450502254,
18.0414611237696));
#271734=CARTESIAN_POINT('Ctrl Pts',(-1.07949380837069,-1.12143874788174,
18.0455951369333));
#271735=CARTESIAN_POINT('Ctrl Pts',(-1.03632097951966,-1.1600082229913,
18.049729150097));
#271736=CARTESIAN_POINT('Ctrl Pts',(-0.993157904702015,-1.19856898410276,
18.0538622292635));
#271737=CARTESIAN_POINT('Ctrl Pts',(-0.947830415658562,-1.2347257092607,
18.05799530843));
#271738=CARTESIAN_POINT('Ctrl Pts',(-0.900641343215095,-1.26823713117528,
18.0621283875965));
#271739=CARTESIAN_POINT('Ctrl Pts',(-0.853409621944049,-1.30177884024707,
18.0662652021825));
#271740=CARTESIAN_POINT('Ctrl Pts',(-0.804313379998956,-1.33267016508006,
18.0704020167685));
#271741=CARTESIAN_POINT('Ctrl Pts',(-0.753685657002759,-1.3607123797586,
18.0745388313545));
#271742=CARTESIAN_POINT('Ctrl Pts',(-0.703037019623535,-1.38876617871517,
18.0786773548643));
#271743=CARTESIAN_POINT('Ctrl Pts',(-0.650856109387414,-1.41396829298555,
18.0828158783742));
#271744=CARTESIAN_POINT('Ctrl Pts',(-0.597498983686705,-1.43616684772117,
18.086954401884));
#271745=CARTESIAN_POINT('Ctrl Pts',(-0.544037834057248,-1.45840868029167,
18.0911009937722));
#271746=CARTESIAN_POINT('Ctrl Pts',(-0.489396379134149,-1.47763507686832,
18.0952475856603));
#271747=CARTESIAN_POINT('Ctrl Pts',(-0.433948124184827,-1.49374337672723,
18.0993941775485));
#271748=CARTESIAN_POINT('Ctrl Pts',(-0.381491169641016,-1.50898267243183,
18.1033170707466));
#271749=CARTESIAN_POINT('Ctrl Pts',(-0.328312606387049,-1.52143158288161,
18.1072399639447));
#271750=CARTESIAN_POINT('Ctrl Pts',(-0.274735110446107,-1.53104567831537,
18.1111628571429));
#271751=CARTESIAN_POINT('Ctrl Pts',(-0.21808230386972,-1.54121161607431,
18.1153109216552));
#271752=CARTESIAN_POINT('Ctrl Pts',(-0.160745571050524,-1.54825018790437,
18.1194589861676));
#271753=CARTESIAN_POINT('Ctrl Pts',(-0.103101228021132,-1.55207937515468,
18.1236070506799));
#271754=CARTESIAN_POINT('Ctrl Pts',(-0.0455593729887791,-1.55590175435217,
18.1277477401958));
#271755=CARTESIAN_POINT('Ctrl Pts',(0.0122884913517671,-1.55652604048254,
18.1318884297118));
#271756=CARTESIAN_POINT('Ctrl Pts',(0.070057759223516,-1.55392154254086,
18.1360291192277));
#271757=CARTESIAN_POINT('Ctrl Pts',(0.127769564769916,-1.55131963525878,
18.1401656900546));
#271758=CARTESIAN_POINT('Ctrl Pts',(0.185402411102989,-1.54549533040801,
18.1443022608815));
#271759=CARTESIAN_POINT('Ctrl Pts',(0.242570259876582,-1.53646995383034,
18.1484388317085));
#271760=CARTESIAN_POINT('Ctrl Pts',(0.299703220892861,-1.52745008515885,
18.1525728781151));
#271761=CARTESIAN_POINT('Ctrl Pts',(0.356371233489937,-1.51523309821701,
18.1567069245217));
#271762=CARTESIAN_POINT('Ctrl Pts',(0.412194174568351,-1.49989206693412,
18.1608409709283));
#271763=CARTESIAN_POINT('Ctrl Pts',(0.468004506875572,-1.48455450074192,
18.1649740835746));
#271764=CARTESIAN_POINT('Ctrl Pts',(0.522969644665716,-1.46609442900677,
18.1691071962209));
#271765=CARTESIAN_POINT('Ctrl Pts',(0.576722613642818,-1.44463534392351,
18.1732403088673));
#271766=CARTESIAN_POINT('Ctrl Pts',(0.630524164682245,-1.42315686406767,
18.1773771570307));
#271767=CARTESIAN_POINT('Ctrl Pts',(0.683110872245827,-1.39867414664148,
18.1815140051942));
#271768=CARTESIAN_POINT('Ctrl Pts',(0.734135108671954,-1.37135914049355,
18.1856508533576));
#271769=CARTESIAN_POINT('Ctrl Pts',(0.785180424456432,-1.34403284984941,
18.1897894105541));
#271770=CARTESIAN_POINT('Ctrl Pts',(0.834661535923235,-1.31387220838579,
18.1939279677506));
#271771=CARTESIAN_POINT('Ctrl Pts',(0.882257683604024,-1.28109391916505,
18.198066524947));
#271772=CARTESIAN_POINT('Ctrl Pts',(0.929946619950204,-1.24825172868635,
18.2022131502586));
#271773=CARTESIAN_POINT('Ctrl Pts',(0.975742835023639,-1.21278201166987,
18.2063597755702));
#271774=CARTESIAN_POINT('Ctrl Pts',(1.01935744443746,-1.17494282859632,
18.2105064008818));
#271775=CARTESIAN_POINT('Ctrl Pts',(1.06061603120207,-1.13914768474603,
18.2144290291593));
#271776=CARTESIAN_POINT('Ctrl Pts',(1.09992237905076,-1.10123275944642,
18.2183516574368));
#271777=CARTESIAN_POINT('Ctrl Pts',(1.13706414369385,-1.06144495058659,
18.2222742857143));
#271778=CARTESIAN_POINT('Ctrl Pts',(1.17633885422906,-1.01937224104206,
18.2264221793757));
#271779=CARTESIAN_POINT('Ctrl Pts',(1.21335778128719,-0.975028418356394,
18.2305700730371));
#271780=CARTESIAN_POINT('Ctrl Pts',(1.24784786515699,-0.928685067944537,
18.2347179666985));
#271781=CARTESIAN_POINT('Ctrl Pts',(1.28227662322299,-0.882424119281116,
18.2388584851121));
#271782=CARTESIAN_POINT('Ctrl Pts',(1.31418515450624,-0.83417111400729,
18.2429990035258));
#271783=CARTESIAN_POINT('Ctrl Pts',(1.34333901653407,-0.784232450653037,
18.2471395219395));
#271784=CARTESIAN_POINT('Ctrl Pts',(1.37246387812037,-0.734343463162846,
18.251275921624));
#271785=CARTESIAN_POINT('Ctrl Pts',(1.39883923824252,-0.682772587311995,
18.2554123213084));
#271786=CARTESIAN_POINT('Ctrl Pts',(1.42227357161143,-0.629855648141438,
18.2595487209929));
#271787=CARTESIAN_POINT('Ctrl Pts',(1.44569360453453,-0.576971000728829,
18.2636825965024));
#271788=CARTESIAN_POINT('Ctrl Pts',(1.46617595784719,-0.522742393527044,
18.2678164720118));
#271789=CARTESIAN_POINT('Ctrl Pts',(1.48357578473478,-0.467528759488206,
18.2719503475212));
#271790=CARTESIAN_POINT('Ctrl Pts',(1.50097168358037,-0.412327590025899,
18.2760832898009));
#271791=CARTESIAN_POINT('Ctrl Pts',(1.5152862810371,-0.35614233171361,18.2802162320805));
#271792=CARTESIAN_POINT('Ctrl Pts',(1.52642421658827,-0.299348227008068,
18.2843491743602));
#271793=CARTESIAN_POINT('Ctrl Pts',(1.53757222495343,-0.242502759422096,
18.2884858543486));
#271794=CARTESIAN_POINT('Ctrl Pts',(1.54553772862851,-0.185047857209864,
18.2926225343369));
#271795=CARTESIAN_POINT('Ctrl Pts',(1.5502765683613,-0.127368801477861,
18.2967592143253));
#271796=CARTESIAN_POINT('Ctrl Pts',(1.55501736695423,-0.0696659033688531,
18.3008976042634));
#271797=CARTESIAN_POINT('Ctrl Pts',(1.55652882773326,-0.011739188796491,
18.3050359942014));
#271798=CARTESIAN_POINT('Ctrl Pts',(1.55481896346577,0.0460243505900421,
18.3091743841395));
#271799=CARTESIAN_POINT('Ctrl Pts',(1.55310576413567,0.103900556826267,
18.3133208459402));
#271800=CARTESIAN_POINT('Ctrl Pts',(1.5481587271621,0.161612430901385,18.317467307741));
#271801=CARTESIAN_POINT('Ctrl Pts',(1.54003790034462,0.218777319441797,
18.3216137695417));
#271802=CARTESIAN_POINT('Ctrl Pts',(1.53235280003774,0.272875000914189,
18.3255377511231));
#271803=CARTESIAN_POINT('Ctrl Pts',(1.52182588147778,0.326482519924142,
18.3294617327044));
#271804=CARTESIAN_POINT('Ctrl Pts',(1.50854945504498,0.379287215291371,
18.3333857142858));
#271805=CARTESIAN_POINT('Ctrl Pts',(1.49451645174172,0.435101064618002,
18.3375333097831));
#271806=CARTESIAN_POINT('Ctrl Pts',(1.4773522856722,0.490252203646958,18.3416809052804));
#271807=CARTESIAN_POINT('Ctrl Pts',(1.45713693966284,0.544364022571303,
18.3458285007778));
#271808=CARTESIAN_POINT('Ctrl Pts',(1.44999548490416,0.563480049899223,
18.3472937176278));
#271809=CARTESIAN_POINT('Ctrl Pts',(1.44247371498061,0.582466443269449,
18.3487589344778));
#271810=CARTESIAN_POINT('Ctrl Pts',(1.43457668357356,0.601306900797837,
18.3502241513278));
#271811=CARTESIAN_POINT('Origin',(0.,0.,-1.29405622560371));
#271812=CARTESIAN_POINT('',(1.43457668357355,0.601306900797844,19.188224604057));
#271813=CARTESIAN_POINT('',(1.43457668357356,0.601306900797836,19.0501843444911));
#271814=CARTESIAN_POINT('',(1.43457668357355,0.601306900797845,-1.29405622560371));
#271815=CARTESIAN_POINT('',(-1.55549954655085,0.00118772054205428,18.7940562256531));
#271816=CARTESIAN_POINT('Ctrl Pts',(-1.55549954655085,0.00118772054205428,
18.7940562256531));
#271817=CARTESIAN_POINT('Ctrl Pts',(-1.55554293531709,-0.0556364260569684,
18.7981393593524));
#271818=CARTESIAN_POINT('Ctrl Pts',(-1.55246831755618,-0.112576373261054,
18.8022224930517));
#271819=CARTESIAN_POINT('Ctrl Pts',(-1.54626410196496,-0.169255951075549,
18.8063056267509));
#271820=CARTESIAN_POINT('Ctrl Pts',(-1.54006667370066,-0.225873522207911,
18.8103842935578));
#271821=CARTESIAN_POINT('Ctrl Pts',(-1.53074648102143,-0.282230757233944,
18.8144629603647));
#271822=CARTESIAN_POINT('Ctrl Pts',(-1.51834394447829,-0.33795253552255,
18.8185416271716));
#271823=CARTESIAN_POINT('Ctrl Pts',(-1.50594988631056,-0.393636222397049,
18.8226175058014));
#271824=CARTESIAN_POINT('Ctrl Pts',(-1.49047777290168,-0.44868478979142,
18.8266933844312));
#271825=CARTESIAN_POINT('Ctrl Pts',(-1.47201938618257,-0.502731714438912,
18.830769263061));
#271826=CARTESIAN_POINT('Ctrl Pts',(-1.45356604480038,-0.556763866129879,
18.8348440276075));
#271827=CARTESIAN_POINT('Ctrl Pts',(-1.43212822258919,-0.60979441012812,
18.838918792154));
#271828=CARTESIAN_POINT('Ctrl Pts',(-1.40784729205727,-0.661472790254456,
18.8429935567004));
#271829=CARTESIAN_POINT('Ctrl Pts',(-1.38354594597962,-0.713194621859364,
18.8470717473323));
#271830=CARTESIAN_POINT('Ctrl Pts',(-1.35639694404575,-0.763561530749342,
18.8511499379642));
#271831=CARTESIAN_POINT('Ctrl Pts',(-1.32658881136516,-0.81224526810612,
18.8552281285961));
#271832=CARTESIAN_POINT('Ctrl Pts',(-1.29676823386543,-0.860949330798692,
18.8593080218621));
#271833=CARTESIAN_POINT('Ctrl Pts',(-1.2642866209274,-0.907968380249418,
18.8633879151282));
#271834=CARTESIAN_POINT('Ctrl Pts',(-1.22937539611821,-0.953003874818558,
18.8674678083942));
#271835=CARTESIAN_POINT('Ctrl Pts',(-1.19439986236409,-0.9981223279535,
18.8715552171121));
#271836=CARTESIAN_POINT('Ctrl Pts',(-1.15698613404714,-1.04124952517296,
18.8756426258301));
#271837=CARTESIAN_POINT('Ctrl Pts',(-1.11740452834311,-1.08212169834928,
18.879730034548));
#271838=CARTESIAN_POINT('Ctrl Pts',(-1.08838209309471,-1.11209041685809,
18.8827270467395));
#271839=CARTESIAN_POINT('Ctrl Pts',(-1.05819496421084,-1.14084751914303,
18.8857240589309));
#271840=CARTESIAN_POINT('Ctrl Pts',(-1.02696061094917,-1.16830310859764,
18.8887210711223));
#271841=CARTESIAN_POINT('Ctrl Pts',(-0.983795291387467,-1.20624624392158,
18.8928628885593));
#271842=CARTESIAN_POINT('Ctrl Pts',(-0.938431985387361,-1.24187503920902,
18.8970047059963));
#271843=CARTESIAN_POINT('Ctrl Pts',(-0.89114917915262,-1.27492485680357,
18.9011465234333));
#271844=CARTESIAN_POINT('Ctrl Pts',(-0.843950718407869,-1.30791571844181,
18.9052809524843));
#271845=CARTESIAN_POINT('Ctrl Pts',(-0.79483997769596,-1.33833643592707,
18.9094153815354));
#271846=CARTESIAN_POINT('Ctrl Pts',(-0.744129160547715,-1.36596194764809,
18.9135498105864));
#271847=CARTESIAN_POINT('Ctrl Pts',(-0.693468916016077,-1.39355990914429,
18.9176801164758));
#271848=CARTESIAN_POINT('Ctrl Pts',(-0.641212212707886,-1.41836793849242,
18.9218104223653));
#271849=CARTESIAN_POINT('Ctrl Pts',(-0.587699447516429,-1.44020471093136,
18.9259407282547));
#271850=CARTESIAN_POINT('Ctrl Pts',(-0.534219314459006,-1.46202816728614,
18.9300685154797));
#271851=CARTESIAN_POINT('Ctrl Pts',(-0.479485120448245,-1.48088376089469,
18.9341963027048));
#271852=CARTESIAN_POINT('Ctrl Pts',(-0.423859012247329,-1.49663749376284,
18.9383240899298));
#271853=CARTESIAN_POINT('Ctrl Pts',(-0.36824527219923,-1.51238772387695,
18.9424509593646));
#271854=CARTESIAN_POINT('Ctrl Pts',(-0.311740514143425,-1.52503731999041,
18.9465778287993));
#271855=CARTESIAN_POINT('Ctrl Pts',(-0.254721736165568,-1.53450222780053,
18.950704698234));
#271856=CARTESIAN_POINT('Ctrl Pts',(-0.197650249626981,-1.54397588503823,
18.954835382576));
#271857=CARTESIAN_POINT('Ctrl Pts',(-0.140064310195615,-1.55025888399788,
18.958966066918));
#271858=CARTESIAN_POINT('Ctrl Pts',(-0.0823494398928511,-1.55331864720325,
18.9630967512599));
#271859=CARTESIAN_POINT('Ctrl Pts',(-0.0246102727265254,-1.55637969851078,
18.9672291745415));
#271860=CARTESIAN_POINT('Ctrl Pts',(0.0332574098223974,-1.55621480986918,
18.9713615978231));
#271861=CARTESIAN_POINT('Ctrl Pts',(0.0908679535572635,-1.55284360610343,
18.9754940211046));
#271862=CARTESIAN_POINT('Ctrl Pts',(0.148592996712049,-1.54946570216007,
18.9796346574673));
#271863=CARTESIAN_POINT('Ctrl Pts',(0.206059358632892,-1.54286880761442,
18.98377529383));
#271864=CARTESIAN_POINT('Ctrl Pts',(0.262887291216128,-1.53312443138744,
18.9879159301927));
#271865=CARTESIAN_POINT('Ctrl Pts',(0.317606314807269,-1.52374167314853,
18.9919029057611));
#271866=CARTESIAN_POINT('Ctrl Pts',(0.371733071489943,-1.51144114537106,
18.9958898813295));
#271867=CARTESIAN_POINT('Ctrl Pts',(0.424942317006753,-1.4963302700998,
18.9998768568979));
#271868=CARTESIAN_POINT('Ctrl Pts',(0.48040560926309,-1.48057926887287,
19.0040327284766));
#271869=CARTESIAN_POINT('Ctrl Pts',(0.535106637496891,-1.46170783515026,
19.0081886000553));
#271870=CARTESIAN_POINT('Ctrl Pts',(0.588670275789439,-1.43980816652844,
19.0123444716341));
#271871=CARTESIAN_POINT('Ctrl Pts',(0.642137947017385,-1.41794773435471,
19.0164928973632));
#271872=CARTESIAN_POINT('Ctrl Pts',(0.694471797372421,-1.3930700323487,
19.0206413230923));
#271873=CARTESIAN_POINT('Ctrl Pts',(0.745311852489109,-1.36531699342653,
19.0247897488214));
#271874=CARTESIAN_POINT('Ctrl Pts',(0.796100836951593,-1.33759183342484,
19.0289340073084));
#271875=CARTESIAN_POINT('Ctrl Pts',(0.845398546695094,-1.30699730735699,
19.0330782657954));
#271876=CARTESIAN_POINT('Ctrl Pts',(0.892866584321714,-1.27372269847156,
19.0372225242825));
#271877=CARTESIAN_POINT('Ctrl Pts',(0.940305006694703,-1.24046884957603,
19.0413641971715));
#271878=CARTESIAN_POINT('Ctrl Pts',(0.985915596241511,-1.20453853002213,
19.0455058700604));
#271879=CARTESIAN_POINT('Ctrl Pts',(1.02938799067036,-1.1661649174382,19.0496475429494));
#271880=CARTESIAN_POINT('Ctrl Pts',(1.07284980880515,-1.12780064067798,
19.0537882082208));
#271881=CARTESIAN_POINT('Ctrl Pts',(1.11417407590801,-1.08699459410041,
19.0579288734921));
#271882=CARTESIAN_POINT('Ctrl Pts',(1.15308435880024,-1.04401949765809,
19.0620695387635));
#271883=CARTESIAN_POINT('Ctrl Pts',(1.19202813818442,-1.00100740546901,
19.0662137685877));
#271884=CARTESIAN_POINT('Ctrl Pts',(1.22855343011921,-0.955822916064633,
19.070357998412));
#271885=CARTESIAN_POINT('Ctrl Pts',(1.26242243533336,-0.908773813865138,
19.0745022282362));
#271886=CARTESIAN_POINT('Ctrl Pts',(1.29630471826431,-0.861706266935699,
19.0786480827291));
#271887=CARTESIAN_POINT('Ctrl Pts',(1.32752835665271,-0.812773086740959,
19.0827939372219));
#271888=CARTESIAN_POINT('Ctrl Pts',(1.35589929068108,-0.762310542712448,
19.0869397917148));
#271889=CARTESIAN_POINT('Ctrl Pts',(1.38432390192683,-0.711752524599698,
19.0910934900782));
#271890=CARTESIAN_POINT('Ctrl Pts',(1.40988479167735,-0.659659826671731,
19.0952471884416));
#271891=CARTESIAN_POINT('Ctrl Pts',(1.43243465760223,-0.606391953854926,
19.0994008868049));
#271892=CARTESIAN_POINT('Ctrl Pts',(1.45348373341846,-0.556669286002903,
19.1032781387611));
#271893=CARTESIAN_POINT('Ctrl Pts',(1.47190961747841,-0.505923193972485,
19.1071553907173));
#271894=CARTESIAN_POINT('Ctrl Pts',(1.48763200304815,-0.454457119547008,
19.1110326426734));
#271895=CARTESIAN_POINT('Ctrl Pts',(1.50447220800571,-0.399331945454153,
19.1151855568304));
#271896=CARTESIAN_POINT('Ctrl Pts',(1.51827854514202,-0.343157182743916,
19.1193384709874));
#271897=CARTESIAN_POINT('Ctrl Pts',(1.52892569376488,-0.286297874504137,
19.1234913851443));
#271898=CARTESIAN_POINT('Ctrl Pts',(1.5395574624503,-0.229520700236023,
19.1276383003656));
#271899=CARTESIAN_POINT('Ctrl Pts',(1.5470389930162,-0.172061446218813,
19.1317852155869));
#271900=CARTESIAN_POINT('Ctrl Pts',(1.5512948910046,-0.1142996550433,19.1359321308082));
#271901=CARTESIAN_POINT('Ctrl Pts',(1.55576711955347,-0.0536017876994527,
19.1402898369122));
#271902=CARTESIAN_POINT('Ctrl Pts',(1.55667684533764,0.00742962794439894,
19.1446475430163));
#271903=CARTESIAN_POINT('Ctrl Pts',(1.55399785510563,0.0683441023578467,
19.1490052491204));
#271904=CARTESIAN_POINT('Ctrl Pts',(1.55145262355544,0.12621719210948,19.1531453803273));
#271905=CARTESIAN_POINT('Ctrl Pts',(1.54566854178028,0.183984161633242,
19.1572855115342));
#271906=CARTESIAN_POINT('Ctrl Pts',(1.53667653344422,0.241258122271234,
19.1614256427411));
#271907=CARTESIAN_POINT('Ctrl Pts',(1.52768705099214,0.298515994470013,
19.1655646109719));
#271908=CARTESIAN_POINT('Ctrl Pts',(1.51549151678963,0.355280621099329,
19.1697035792027));
#271909=CARTESIAN_POINT('Ctrl Pts',(1.5001723928256,0.411172763937408,19.1738425474335));
#271910=CARTESIAN_POINT('Ctrl Pts',(1.48484781488213,0.467084805733029,
19.1779829892373));
#271911=CARTESIAN_POINT('Ctrl Pts',(1.4663975721555,0.522123245313919,19.1821234310411));
#271912=CARTESIAN_POINT('Ctrl Pts',(1.44495416056346,0.575923366317395,
19.1862638728448));
#271913=CARTESIAN_POINT('Ctrl Pts',(1.44156927489217,0.584415823682041,
19.1869174499156));
#271914=CARTESIAN_POINT('Ctrl Pts',(1.43810990577921,0.59287746453593,19.1875710269863));
#271915=CARTESIAN_POINT('Ctrl Pts',(1.43457668357355,0.601306900797844,
19.188224604057));
#271916=CARTESIAN_POINT('Ctrl Pts',(-1.55549958889311,0.00113090820362872,
18.7933196395821));
#271917=CARTESIAN_POINT('Ctrl Pts',(-1.55545428746057,0.063440439139176,
18.7885137489814));
#271918=CARTESIAN_POINT('Ctrl Pts',(-1.55166503816927,0.125700707766695,
18.7837601818246));
#271919=CARTESIAN_POINT('Ctrl Pts',(-1.54346157201289,0.193233343957606,
18.7787617229099));
#271920=CARTESIAN_POINT('Ctrl Pts',(-1.54274300200048,0.198888868159507,
18.7783443600553));
#271921=CARTESIAN_POINT('Ctrl Pts',(-1.54149823805131,0.208272918818632,
18.7776540288749));
#271922=CARTESIAN_POINT('Ctrl Pts',(-1.54098957760577,0.212003653569252,
18.7773801549248));
#271923=CARTESIAN_POINT('Ctrl Pts',(-1.54004607427961,0.218740866127462,
18.776886657891));
#271924=CARTESIAN_POINT('Ctrl Pts',(-1.53961596361043,0.221747970547353,
18.7766667795202));
#271925=CARTESIAN_POINT('Ctrl Pts',(-1.53871697917945,0.227904467166324,
18.7762174447576));
#271926=CARTESIAN_POINT('Ctrl Pts',(-1.53824724718087,0.231053663042422,
18.7759880469244));
#271927=CARTESIAN_POINT('Ctrl Pts',(-1.53717053254376,0.238123375196727,
18.7754740648235));
#271928=CARTESIAN_POINT('Ctrl Pts',(-1.53655822097506,0.242043017735181,
18.775189783164));
#271929=CARTESIAN_POINT('Ctrl Pts',(-1.53495114962413,0.252078581312601,
18.7744635825857));
#271930=CARTESIAN_POINT('Ctrl Pts',(-1.53393481770518,0.258191055855722,
18.7740228424643));
#271931=CARTESIAN_POINT('Ctrl Pts',(-1.52762155742059,0.294806935424441,
18.7713912110674));
#271932=CARTESIAN_POINT('Ctrl Pts',(-1.52145098600253,0.325155329425654,
18.7692456656695));
#271933=CARTESIAN_POINT('Ctrl Pts',(-1.50885764965102,0.378831015110621,
18.7654817713843));
#271934=CARTESIAN_POINT('Ctrl Pts',(-1.50278939559762,0.402229391684932,
18.7638516212343));
#271935=CARTESIAN_POINT('Ctrl Pts',(-1.48360231947615,0.469700075827315,
18.75915720477));
#271936=CARTESIAN_POINT('Ctrl Pts',(-1.46907165424801,0.513344718846042,
18.7561278793318));
#271937=CARTESIAN_POINT('Ctrl Pts',(-1.43787516749469,0.594808476515452,
18.7503850315676));
#271938=CARTESIAN_POINT('Ctrl Pts',(-1.42159527624399,0.632731304633764,
18.7476734337654));
#271939=CARTESIAN_POINT('Ctrl Pts',(-1.36862436450953,0.743725771684251,
18.7395218517367));
#271940=CARTESIAN_POINT('Ctrl Pts',(-1.32766740394668,0.814590050468797,
18.7340215262471));
#271941=CARTESIAN_POINT('Ctrl Pts',(-1.27412831319303,0.892378285496051,
18.7274212817382));
#271942=CARTESIAN_POINT('Ctrl Pts',(-1.26679052298963,0.902764485826335,
18.7265278421246));
#271943=CARTESIAN_POINT('Ctrl Pts',(-1.2553265552259,0.918576030052865,
18.7251481951955));
#271944=CARTESIAN_POINT('Ctrl Pts',(-1.25129055835476,0.924066349966369,
18.7246654547836));
#271945=CARTESIAN_POINT('Ctrl Pts',(-1.24386621855829,0.934028133105149,
18.7237827167207));
#271946=CARTESIAN_POINT('Ctrl Pts',(-1.24048949255047,0.938508146188682,
18.72338317615));
#271947=CARTESIAN_POINT('Ctrl Pts',(-1.23306131330517,0.94825322686272,
18.7225084160979));
#271948=CARTESIAN_POINT('Ctrl Pts',(-1.22900023325334,0.95351078061902,
18.7220328229874));
#271949=CARTESIAN_POINT('Ctrl Pts',(-1.21775923065159,0.967872482167281,
18.7207234875946));
#271950=CARTESIAN_POINT('Ctrl Pts',(-1.21051112748825,0.976922454580197,
18.7198870483512));
#271951=CARTESIAN_POINT('Ctrl Pts',(-1.17161032374428,1.02439629118279,
18.7154376524296));
#271952=CARTESIAN_POINT('Ctrl Pts',(-1.13823128300075,1.06136093455897,
18.7117551572179));
#271953=CARTESIAN_POINT('Ctrl Pts',(-1.0004780880754,1.19992842391073,18.697046120097));
#271954=CARTESIAN_POINT('Ctrl Pts',(-0.88384303124947,1.28825327817098,
18.6855202920137));
#271955=CARTESIAN_POINT('Ctrl Pts',(-0.738245916070925,1.36931245208684,
18.6729008077676));
#271956=CARTESIAN_POINT('Ctrl Pts',(-0.719641346799062,1.37918093686114,
18.6713197796696));
#271957=CARTESIAN_POINT('Ctrl Pts',(-0.692556218430453,1.39285040720813,
18.6690686115381));
#271958=CARTESIAN_POINT('Ctrl Pts',(-0.684233811270484,1.39695757794949,
18.6683836446252));
#271959=CARTESIAN_POINT('Ctrl Pts',(-0.669385714753562,1.4041206944867,
18.6671741451085));
#271960=CARTESIAN_POINT('Ctrl Pts',(-0.662874693880398,1.40720620571879,
18.6666480110027));
#271961=CARTESIAN_POINT('Ctrl Pts',(-0.652888222664744,1.41185400577409,
18.6658477589511));
#271962=CARTESIAN_POINT('Ctrl Pts',(-0.649428199112855,1.41344889541703,
18.6655717200872));
#271963=CARTESIAN_POINT('Ctrl Pts',(-0.645953593567903,1.41503505435319,
18.66529576954));
#271964=CARTESIAN_POINT('Ctrl Pts',(-0.645944886371479,1.41503902909501,
18.6652950780289));
#271965=CARTESIAN_POINT('Ctrl Pts',(-0.645927441107565,1.4150469924764,
18.6652936925708));
#271966=CARTESIAN_POINT('Ctrl Pts',(-0.645918703058556,1.41505098110684,
18.6652929986252));
#271967=CARTESIAN_POINT('Ctrl Pts',(-0.645901195925661,1.41505897233816,
18.6652916082853));
#271968=CARTESIAN_POINT('Ctrl Pts',(-0.645892426791781,1.41506297496117,
18.6652909118871));
#271969=CARTESIAN_POINT('Ctrl Pts',(-0.645874857233824,1.41507099429208,
18.6652895166216));
#271970=CARTESIAN_POINT('Ctrl Pts',(-0.64586605689437,1.41507501096066,
18.6652888177612));
#271971=CARTESIAN_POINT('Ctrl Pts',(-0.645848424741837,1.41508305846432,
18.6652874175571));
#271972=CARTESIAN_POINT('Ctrl Pts',(-0.645839592936646,1.4150870892951,
18.6652867162141));
#271973=CARTESIAN_POINT('Ctrl Pts',(-0.645821897664302,1.41509516520699,
18.66528531103));
#271974=CARTESIAN_POINT('Ctrl Pts',(-0.645813034239644,1.415099210268,18.6652846071923));
#271975=CARTESIAN_POINT('Ctrl Pts',(-0.645795275620331,1.4151073146875,
18.6652831970104));
#271976=CARTESIAN_POINT('Ctrl Pts',(-0.645786380324565,1.41511137409142,
18.6652824906583));
#271977=CARTESIAN_POINT('Ctrl Pts',(-0.645768557719544,1.4151195073057,
18.6652810754283));
#271978=CARTESIAN_POINT('Ctrl Pts',(-0.645759630456149,1.4151235810944,
18.6652803665542));
#271979=CARTESIAN_POINT('Ctrl Pts',(-0.645741743715666,1.41513174316741,
18.6652789462647));
#271980=CARTESIAN_POINT('Ctrl Pts',(-0.645732784219057,1.4151358314599,
18.6652782348477));
#271981=CARTESIAN_POINT('Ctrl Pts',(-0.645714832802365,1.41514402263399,
18.6652768094559));
#271982=CARTESIAN_POINT('Ctrl Pts',(-0.645705840916108,1.41514812549942,
18.6652760954838));
#271983=CARTESIAN_POINT('Ctrl Pts',(-0.645687824520127,1.41515634590842,
18.6652746649661));
#271984=CARTESIAN_POINT('Ctrl Pts',(-0.645678800021557,1.41516046344615,
18.6652739484215));
#271985=CARTESIAN_POINT('Ctrl Pts',(-0.645660718250003,1.41516871326637,
18.6652725127468));
#271986=CARTESIAN_POINT('Ctrl Pts',(-0.645651660928029,1.41517284557046,
18.6652717936129));
#271987=CARTESIAN_POINT('Ctrl Pts',(-0.64563351330241,1.41518112501567,
18.6652703527436));
#271988=CARTESIAN_POINT('Ctrl Pts',(-0.645624422990814,1.41518527215966,
18.6652696310076));
#271989=CARTESIAN_POINT('Ctrl Pts',(-0.645606209148752,1.4151935813906,
18.6652681849152));
#271990=CARTESIAN_POINT('Ctrl Pts',(-0.645597085643688,1.41519774346518,
18.665267460561));
#271991=CARTESIAN_POINT('Ctrl Pts',(-0.645578805209261,1.4152060826487,
18.6652660092161));
#271992=CARTESIAN_POINT('Ctrl Pts',(-0.645569648292943,1.41521025975091,
18.6652652822266));
#271993=CARTESIAN_POINT('Ctrl Pts',(-0.645551300862317,1.41521862906655,
18.6652638255976));
#271994=CARTESIAN_POINT('Ctrl Pts',(-0.645542110321833,1.41522282129115,
18.6652630959561));
#271995=CARTESIAN_POINT('Ctrl Pts',(-0.645523695448889,1.4152312209377,
18.6652616340079));
#271996=CARTESIAN_POINT('Ctrl Pts',(-0.64551447109297,1.41523542836955,
18.6652609016994));
#271997=CARTESIAN_POINT('Ctrl Pts',(-0.645495988347904,1.41524385853828,
18.6652594343982));
#271998=CARTESIAN_POINT('Ctrl Pts',(-0.645486729985911,1.41524808126196,
18.6652586994078));
#271999=CARTESIAN_POINT('Ctrl Pts',(-0.64546817901382,1.41525654210991,
18.6652572267259));
#272000=CARTESIAN_POINT('Ctrl Pts',(-0.645458886415928,1.41526078022781,
18.6652564890355));
#272001=CARTESIAN_POINT('Ctrl Pts',(-0.64544026675778,1.41526927195949,
18.6652550109368));
#272002=CARTESIAN_POINT('Ctrl Pts',(-0.645430939724615,1.41527352556009,
18.6652542705308));
#272003=CARTESIAN_POINT('Ctrl Pts',(-0.645412251023805,1.41528204833321,
18.6652527869875));
#272004=CARTESIAN_POINT('Ctrl Pts',(-0.645402889317873,1.41528631752236,
18.6652520438472));
#272005=CARTESIAN_POINT('Ctrl Pts',(-0.645384131052972,1.41529487156976,
18.6652505548182));
#272006=CARTESIAN_POINT('Ctrl Pts',(-0.645374734498175,1.41529915642526,
18.6652498089299));
#272007=CARTESIAN_POINT('Ctrl Pts',(-0.645355906318788,1.41530774190171,
18.6652483143878));
#272008=CARTESIAN_POINT('Ctrl Pts',(-0.645346474682014,1.41531204252735,
18.6652475657332));
#272009=CARTESIAN_POINT('Ctrl Pts',(-0.645327576142191,1.41532065963113,
18.6652460656431));
#272010=CARTESIAN_POINT('Ctrl Pts',(-0.645318109207583,1.4153249761228,
18.6652453142052));
#272011=CARTESIAN_POINT('Ctrl Pts',(-0.645299139822707,1.41533362506977,
18.665243808529));
#272012=CARTESIAN_POINT('Ctrl Pts',(-0.645289637400272,1.41533795751152,
18.6652430542929));
#272013=CARTESIAN_POINT('Ctrl Pts',(-0.645270596835231,1.41534663844932,
18.6652415430044));
#272014=CARTESIAN_POINT('Ctrl Pts',(-0.645261058670962,1.41535098695437,
18.6652407859503));
#272015=CARTESIAN_POINT('Ctrl Pts',(-0.645241946389719,1.41535970012217,
18.6652392690074));
#272016=CARTESIAN_POINT('Ctrl Pts',(-0.645232372296066,1.41536406477341,
18.6652385091205));
#272017=CARTESIAN_POINT('Ctrl Pts',(-0.645213187967082,1.41537281031709,
18.6652369864973));
#272018=CARTESIAN_POINT('Ctrl Pts',(-0.645203577685199,1.41537719122988,
18.6652362237574));
#272019=CARTESIAN_POINT('Ctrl Pts',(-0.645184320694549,1.415385969424,18.6652346954056));
#272020=CARTESIAN_POINT('Ctrl Pts',(-0.645174674069118,1.41539036666645,
18.6652339298005));
#272021=CARTESIAN_POINT('Ctrl Pts',(-0.645155060872781,1.41539930675065,
18.6652323732173));
#272022=CARTESIAN_POINT('Ctrl Pts',(-0.645145094260424,1.41540384960324,
18.6652315822367));
#272023=CARTESIAN_POINT('Ctrl Pts',(-0.645124990212183,1.41541301291455,
18.6652299867392));
#272024=CARTESIAN_POINT('Ctrl Pts',(-0.645114852758563,1.41541763337695,
18.6652291822212));
#272025=CARTESIAN_POINT('Ctrl Pts',(-0.64509440382662,1.41542695335365,
18.6652275593961));
#272026=CARTESIAN_POINT('Ctrl Pts',(-0.645084092352085,1.41543165286166,
18.6652267410896));
#272027=CARTESIAN_POINT('Ctrl Pts',(-0.645063292137594,1.41544113239282,
18.6652250904313));
#272028=CARTESIAN_POINT('Ctrl Pts',(-0.645052803384069,1.41544591241743,
18.6652242580788));
#272029=CARTESIAN_POINT('Ctrl Pts',(-0.645031645273522,1.4154555544888,
18.6652225790647));
#272030=CARTESIAN_POINT('Ctrl Pts',(-0.645020975950331,1.41546041651526,
18.6652217324062));
#272031=CARTESIAN_POINT('Ctrl Pts',(-0.644999453313102,1.4154702241192,
18.6652200245126));
#272032=CARTESIAN_POINT('Ctrl Pts',(-0.644988600018616,1.4154751696827,
18.6652191632795));
#272033=CARTESIAN_POINT('Ctrl Pts',(-0.644966706038322,1.41548514589496,
18.6652174259679));
#272034=CARTESIAN_POINT('Ctrl Pts',(-0.64495566530293,1.41549017656106,
18.665216549886));
#272035=CARTESIAN_POINT('Ctrl Pts',(-0.644933392913297,1.41550032456997,
18.6652147825984));
#272036=CARTESIAN_POINT('Ctrl Pts',(-0.644922161250578,1.4155054419112,
18.6652138913924));
#272037=CARTESIAN_POINT('Ctrl Pts',(-0.644899503383262,1.41551576490468,
18.6652120935704));
#272038=CARTESIAN_POINT('Ctrl Pts',(-0.644888077189239,1.41552097054647,
18.6652111869557));
#272039=CARTESIAN_POINT('Ctrl Pts',(-0.644865026554577,1.41553147181189,
18.6652093580237));
#272040=CARTESIAN_POINT('Ctrl Pts',(-0.644853402164402,1.41553676740668,
18.6652084357109));
#272041=CARTESIAN_POINT('Ctrl Pts',(-0.644829951437513,1.41554745024601,
18.6652065750905));
#272042=CARTESIAN_POINT('Ctrl Pts',(-0.644818125058231,1.41555283750388,
18.6652056367801));
#272043=CARTESIAN_POINT('Ctrl Pts',(-0.644794266521604,1.41556370539643,
18.6652037438621));
#272044=CARTESIAN_POINT('Ctrl Pts',(-0.644782234374757,1.41556918602006,
18.6652027892559));
#272045=CARTESIAN_POINT('Ctrl Pts',(-0.644757960379225,1.41558024241248,
18.6652008634363));
#272046=CARTESIAN_POINT('Ctrl Pts',(-0.644745718539001,1.4155858181709,
18.6651998922243));
#272047=CARTESIAN_POINT('Ctrl Pts',(-0.641838847815903,1.41690975732146,
18.6649692779887));
#272048=CARTESIAN_POINT('Ctrl Pts',(-0.638940222190832,1.41821922133179,
18.6647401934099));
#272049=CARTESIAN_POINT('Ctrl Pts',(-0.632310924005199,1.42118957951864,
18.6642182422463));
#272050=CARTESIAN_POINT('Ctrl Pts',(-0.628577716537844,1.42284467910259,
18.6639257311539));
#272051=CARTESIAN_POINT('Ctrl Pts',(-0.618796535415627,1.42713510902408,
18.6631629317355));
#272052=CARTESIAN_POINT('Ctrl Pts',(-0.612738154290542,1.42974673632314,
18.6626940396309));
#272053=CARTESIAN_POINT('Ctrl Pts',(-0.571081476420635,1.44739054284323,
18.6594932335859));
#272054=CARTESIAN_POINT('Ctrl Pts',(-0.534946735748217,1.46113177000206,
18.656832577638));
#272055=CARTESIAN_POINT('Ctrl Pts',(-0.489602866938786,1.47646680798279,
18.6535907030145));
#272056=CARTESIAN_POINT('Ctrl Pts',(-0.48084548258812,1.47934202605214,
18.652968986519));
#272057=CARTESIAN_POINT('Ctrl Pts',(-0.369158319168309,1.51491450453478,
18.645089650469));
#272058=CARTESIAN_POINT('Ctrl Pts',(-0.263117194499882,1.53688497405591,
18.6381235289083));
#272059=CARTESIAN_POINT('Ctrl Pts',(-0.0897978240626272,1.55431563052022,
18.6265095832142));
#272060=CARTESIAN_POINT('Ctrl Pts',(-0.0235973980838778,1.55672801854881,
18.622025469096));
#272061=CARTESIAN_POINT('Ctrl Pts',(0.0561733953246495,1.55454512464419,
18.6164553414199));
#272062=CARTESIAN_POINT('Ctrl Pts',(0.0697912386742956,1.55399329379031,
18.6154987509854));
#272063=CARTESIAN_POINT('Ctrl Pts',(0.0903868226196514,1.55288745017551,
18.6140425859668));
#272064=CARTESIAN_POINT('Ctrl Pts',(0.0973712280972347,1.55246515312185,
18.613547128563));
#272065=CARTESIAN_POINT('Ctrl Pts',(0.110004004127844,1.55161575578494,
18.6126479096249));
#272066=CARTESIAN_POINT('Ctrl Pts',(0.115653376373959,1.55120489604063,
18.6122446636767));
#272067=CARTESIAN_POINT('Ctrl Pts',(0.127776636086444,1.55025661768673,
18.6113768607707));
#272068=CARTESIAN_POINT('Ctrl Pts',(0.134249632152219,1.54970948351902,
18.6109120063419));
#272069=CARTESIAN_POINT('Ctrl Pts',(0.151651893589408,1.54812869922284,
18.6096581134512));
#272070=CARTESIAN_POINT('Ctrl Pts',(0.162573777559015,1.54701988401345,
18.6088667328782));
#272071=CARTESIAN_POINT('Ctrl Pts',(0.21479461266815,1.5411592033393,18.6050609760018));
#272072=CARTESIAN_POINT('Ctrl Pts',(0.255900017248029,1.53486904679568,
18.601998861258));
#272073=CARTESIAN_POINT('Ctrl Pts',(0.44768543244785,1.49760310761251,18.5873839826503));
#272074=CARTESIAN_POINT('Ctrl Pts',(0.593449121149683,1.44604338696173,
18.5752010628627));
#272075=CARTESIAN_POINT('Ctrl Pts',(0.757969857199383,1.35871923474111,
18.5610844278182));
#272076=CARTESIAN_POINT('Ctrl Pts',(0.786191786473468,1.34258673130148,
18.5586533335845));
#272077=CARTESIAN_POINT('Ctrl Pts',(0.819535986366454,1.32211380430319,
18.5557869729577));
#272078=CARTESIAN_POINT('Ctrl Pts',(0.825159919884402,1.31861110845188,
18.5553037393027));
#272079=CARTESIAN_POINT('Ctrl Pts',(0.833883730356905,1.3131000774609,18.5545546917192));
#272080=CARTESIAN_POINT('Ctrl Pts',(0.836999034648797,1.31111651120397,
18.5542873126004));
#272081=CARTESIAN_POINT('Ctrl Pts',(0.842784809381132,1.30740358596413,
18.5537909786182));
#272082=CARTESIAN_POINT('Ctrl Pts',(0.845457012337971,1.30567714696205,
18.553561846256));
#272083=CARTESIAN_POINT('Ctrl Pts',(0.85154647669686,1.30171637349602,18.5530399076791));
#272084=CARTESIAN_POINT('Ctrl Pts',(0.854960249953708,1.29947677587154,
18.5527474561279));
#272085=CARTESIAN_POINT('Ctrl Pts',(0.863858386379808,1.29358893197377,
18.5519854476243));
#272086=CARTESIAN_POINT('Ctrl Pts',(0.869328540350324,1.28991919500765,
18.5515172785256));
#272087=CARTESIAN_POINT('Ctrl Pts',(0.906496109011111,1.26464093326206,
18.5483369267465));
#272088=CARTESIAN_POINT('Ctrl Pts',(0.937411287606931,1.24189877760512,
18.5456948677055));
#272089=CARTESIAN_POINT('Ctrl Pts',(1.04309024184874,1.15796040031711,18.5365516675918));
#272090=CARTESIAN_POINT('Ctrl Pts',(1.11296910070648,1.09096842337835,18.5302878316224));
#272091=CARTESIAN_POINT('Ctrl Pts',(1.23412181179439,0.950979269136698,
18.5180474601914));
#272092=CARTESIAN_POINT('Ctrl Pts',(1.28622808701608,0.879222361561054,
18.5121123890196));
#272093=CARTESIAN_POINT('Ctrl Pts',(1.33855487551464,0.792473872806984,
18.5050325516305));
#272094=CARTESIAN_POINT('Ctrl Pts',(1.34502862181958,0.781435847087287,
18.5041336176649));
#272095=CARTESIAN_POINT('Ctrl Pts',(1.35474805469087,0.764385124250459,
18.5027472769333));
#272096=CARTESIAN_POINT('Ctrl Pts',(1.35809164917245,0.758428625262346,
18.5022633919723));
#272097=CARTESIAN_POINT('Ctrl Pts',(1.36410983615106,0.747540020506673,
18.501379498948));
#272098=CARTESIAN_POINT('Ctrl Pts',(1.36679719827266,0.742615071638851,
18.5009799547102));
#272099=CARTESIAN_POINT('Ctrl Pts',(1.37260117237279,0.731840286449427,
18.5001063013854));
#272100=CARTESIAN_POINT('Ctrl Pts',(1.3757071423129,0.725984875424026,18.4996318248346));
#272101=CARTESIAN_POINT('Ctrl Pts',(1.3841127159513,0.70989094334789,18.4983284014019));
#272102=CARTESIAN_POINT('Ctrl Pts',(1.38933597134251,0.69961325554501,18.4974967973479));
#272103=CARTESIAN_POINT('Ctrl Pts',(1.40873301588408,0.660372090505318,
18.4943238944194));
#272104=CARTESIAN_POINT('Ctrl Pts',(1.42211652744284,0.631033900310215,
18.4919560728974));
#272105=CARTESIAN_POINT('Ctrl Pts',(1.4345766894261,0.601306886835045,18.4895593986216));
#272106=CARTESIAN_POINT('',(-1.5554997549337,-0.000873155876330299,18.655943774337));
#272107=CARTESIAN_POINT('Ctrl Pts',(1.43457668357356,0.601306900797837,
18.3502241513278));
#272108=CARTESIAN_POINT('Ctrl Pts',(1.41226823356769,0.654529609838117,
18.3543632657824));
#272109=CARTESIAN_POINT('Ctrl Pts',(1.38696156950888,0.706586430174956,
18.3585023802371));
#272110=CARTESIAN_POINT('Ctrl Pts',(1.35880418892424,0.757120483253445,
18.3626414946918));
#272111=CARTESIAN_POINT('Ctrl Pts',(1.33067099704232,0.807611124865335,
18.3667770534248));
#272112=CARTESIAN_POINT('Ctrl Pts',(1.29969219388313,0.856581138214668,
18.3709126121577));
#272113=CARTESIAN_POINT('Ctrl Pts',(1.26606223462692,0.903696114881263,
18.3750481708907));
#272114=CARTESIAN_POINT('Ctrl Pts',(1.23244823856831,0.950788727391055,
18.3791817665901));
#272115=CARTESIAN_POINT('Ctrl Pts',(1.19618588385133,0.996027625870422,
18.3833153622894));
#272116=CARTESIAN_POINT('Ctrl Pts',(1.15751298206812,1.03910728336576,18.3874489579887));
#272117=CARTESIAN_POINT('Ctrl Pts',(1.11884357276049,1.08218305041986,18.391582180391));
#272118=CARTESIAN_POINT('Ctrl Pts',(1.07776439773428,1.12309957741441,18.3957154027932));
#272119=CARTESIAN_POINT('Ctrl Pts',(1.03455213303515,1.16158604245765,18.3998486251955));
#272120=CARTESIAN_POINT('Ctrl Pts',(0.991296757475191,1.20011090365184,
18.4039859711209));
#272121=CARTESIAN_POINT('Ctrl Pts',(0.945904433359631,1.23620051571814,
18.4081233170463));
#272122=CARTESIAN_POINT('Ctrl Pts',(0.898686080166107,1.26962340058605,
18.4122606629718));
#272123=CARTESIAN_POINT('Ctrl Pts',(0.851442481341058,1.3030641552393,18.4164002209589));
#272124=CARTESIAN_POINT('Ctrl Pts',(0.802371351123281,1.33383506677874,
18.4205397789461));
#272125=CARTESIAN_POINT('Ctrl Pts',(0.751811143945473,1.3617489687308,18.4246793369332));
#272126=CARTESIAN_POINT('Ctrl Pts',(0.701158309541624,1.38971400946274,
18.4288264786664));
#272127=CARTESIAN_POINT('Ctrl Pts',(0.64901142148413,1.41481136490602,18.4329736203997));
#272128=CARTESIAN_POINT('Ctrl Pts',(0.595730896403694,1.43690116190017,
18.4371207621329));
#272129=CARTESIAN_POINT('Ctrl Pts',(0.564141473819204,1.44999795347646,
18.4395795557077));
#272130=CARTESIAN_POINT('Ctrl Pts',(0.532153905931037,1.46203847331314,
18.4420383492824));
#272131=CARTESIAN_POINT('Ctrl Pts',(0.499845551780331,1.47300192612414,
18.4444971428572));
#272132=CARTESIAN_POINT('Ctrl Pts',(0.445337743066455,1.49149849781201,
18.4486454027536));
#272133=CARTESIAN_POINT('Ctrl Pts',(0.389687539204677,1.5070042221029,18.4527936626499));
#272134=CARTESIAN_POINT('Ctrl Pts',(0.333254870821266,1.51938192732239,
18.4569419225463));
#272135=CARTESIAN_POINT('Ctrl Pts',(0.276922497358692,1.53173763427384,
18.4610828099507));
#272136=CARTESIAN_POINT('Ctrl Pts',(0.219810924045607,1.54097624588835,
18.465223697355));
#272137=CARTESIAN_POINT('Ctrl Pts',(0.162295924297699,1.54701011081258,
18.4693645847593));
#272138=CARTESIAN_POINT('Ctrl Pts',(0.104838111984474,1.55303797623655,
18.4735013548598));
#272139=CARTESIAN_POINT('Ctrl Pts',(0.0469781832756797,1.55586735430706,
18.4776381249604));
#272140=CARTESIAN_POINT('Ctrl Pts',(-0.0108989230934016,1.55546181678478,
18.4817748950609));
#272141=CARTESIAN_POINT('Ctrl Pts',(-0.0687407250667601,1.55505652663591,
18.4859091417773));
#272142=CARTESIAN_POINT('Ctrl Pts',(-0.126599164262136,1.55142023610591,
18.4900433884938));
#272143=CARTESIAN_POINT('Ctrl Pts',(-0.184087441730226,1.54456856882342,
18.4941776352102));
#272144=CARTESIAN_POINT('Ctrl Pts',(-0.241562744488456,1.53771844791523,
18.4983109488555));
#272145=CARTESIAN_POINT('Ctrl Pts',(-0.298667534541657,1.5276544525376,
18.5024442625009));
#272146=CARTESIAN_POINT('Ctrl Pts',(-0.355020502908433,1.51444402092472,
18.5065775761462));
#272147=CARTESIAN_POINT('Ctrl Pts',(-0.411424393247191,1.50122165203067,
18.5107146247586));
#272148=CARTESIAN_POINT('Ctrl Pts',(-0.46707459575755,1.48484728305153,
18.514851673371));
#272149=CARTESIAN_POINT('Ctrl Pts',(-0.521601711801954,1.46543915064573,
18.5189887219834));
#272150=CARTESIAN_POINT('Ctrl Pts',(-0.57615135366955,1.44602300050139,
18.5231274796615));
#272151=CARTESIAN_POINT('Ctrl Pts',(-0.629576502509719,1.42357078941286,
18.5272662373396));
#272152=CARTESIAN_POINT('Ctrl Pts',(-0.681527658364044,1.39824901247411,
18.5314049950178));
#272153=CARTESIAN_POINT('Ctrl Pts',(-0.733580055445961,1.37287788903401,
18.5355518182125));
#272154=CARTESIAN_POINT('Ctrl Pts',(-0.784152262372308,1.34462627839229,
18.5396986414072));
#272155=CARTESIAN_POINT('Ctrl Pts',(-0.832920134865223,1.31370632141895,
18.5438454646019));
#272156=CARTESIAN_POINT('Ctrl Pts',(-0.87903267828431,1.28446990437703,
18.5477665002108));
#272157=CARTESIAN_POINT('Ctrl Pts',(-0.923531971664942,1.25284841053402,
18.5516875358197));
#272158=CARTESIAN_POINT('Ctrl Pts',(-0.966171551974055,1.21905405218803,
18.5556085714287));
#272159=CARTESIAN_POINT('Ctrl Pts',(-1.01163414749869,1.18302228936671,
18.5597892048832));
#272160=CARTESIAN_POINT('Ctrl Pts',(-1.05518758759132,1.14435700776817,
18.5639698383377));
#272161=CARTESIAN_POINT('Ctrl Pts',(-1.09650642551172,1.10329230433803,
18.5681504717922));
#272162=CARTESIAN_POINT('Ctrl Pts',(-1.13691930318326,1.06312798898295,
18.5722394403327));
#272163=CARTESIAN_POINT('Ctrl Pts',(-1.1751941580597,1.02066878544996,18.5763284088732));
#272164=CARTESIAN_POINT('Ctrl Pts',(-1.21105782752621,0.97617579789068,
18.5804173774137));
#272165=CARTESIAN_POINT('Ctrl Pts',(-1.24688668618988,0.931725997117362,
18.5845023770275));
#272166=CARTESIAN_POINT('Ctrl Pts',(-1.28030865878357,0.885246734994203,
18.5885873766412));
#272167=CARTESIAN_POINT('Ctrl Pts',(-1.31108850350603,0.83703475792486,
18.592672376255));
#272168=CARTESIAN_POINT('Ctrl Pts',(-1.34185101365334,0.788849932848869,
18.596755075281));
#272169=CARTESIAN_POINT('Ctrl Pts',(-1.36997405671991,0.738934776415113,
18.600837774307));
#272170=CARTESIAN_POINT('Ctrl Pts',(-1.39526510124146,0.687615842791343,
18.604920473333));
#272171=CARTESIAN_POINT('Ctrl Pts',(-1.42160455154756,0.63416955271055,
18.6091724150834));
#272172=CARTESIAN_POINT('Ctrl Pts',(-1.44487170883023,0.579201061646552,
18.6134243568337));
#272173=CARTESIAN_POINT('Ctrl Pts',(-1.4649027724697,0.523106219816391,
18.617676298584));
#272174=CARTESIAN_POINT('Ctrl Pts',(-1.48414973309998,0.469207174229017,
18.6217618008291));
#272175=CARTESIAN_POINT('Ctrl Pts',(-1.50040916787234,0.414268887386565,
18.6258473030742));
#272176=CARTESIAN_POINT('Ctrl Pts',(-1.51358652346675,0.358658731916363,
18.6299328053194));
#272177=CARTESIAN_POINT('Ctrl Pts',(-1.52677097037022,0.303018650199013,
18.6340205061512));
#272178=CARTESIAN_POINT('Ctrl Pts',(-1.53686994623477,0.246706507368367,
18.638108206983));
#272179=CARTESIAN_POINT('Ctrl Pts',(-1.54384031258021,0.190098235794666,
18.6421959078149));
#272180=CARTESIAN_POINT('Ctrl Pts',(-1.55082123451994,0.133404239322336,
18.6462897988682));
#272181=CARTESIAN_POINT('Ctrl Pts',(-1.5546640712529,0.0764137526860417,
18.6503836899215));
#272182=CARTESIAN_POINT('Ctrl Pts',(-1.55537771270569,0.0195043794678024,
18.6544775809749));
#272183=CARTESIAN_POINT('Ctrl Pts',(-1.55546290764187,0.012710505036345,
18.6549663120956));
#272184=CARTESIAN_POINT('Ctrl Pts',(-1.55550356692172,0.00591778098874543,
18.6554550432163));
#272185=CARTESIAN_POINT('Ctrl Pts',(-1.55549975493371,-0.000873155876329073,
18.655943774337));
#272186=CARTESIAN_POINT('Ctrl Pts',(-1.55549975493324,-0.0008731566999196,
18.6559437743963));
#272187=CARTESIAN_POINT('Ctrl Pts',(-1.55547173756343,-0.0507851734952812,
18.6595358495975));
#272188=CARTESIAN_POINT('Ctrl Pts',(-1.55304159676454,-0.100629236248426,
18.6631279247988));
#272189=CARTESIAN_POINT('Ctrl Pts',(-1.54822763866007,-0.150237907630056,
18.66672));
#272190=CARTESIAN_POINT('Ctrl Pts',(-1.54266732521047,-0.207537900009354,
18.6708689900037));
#272191=CARTESIAN_POINT('Ctrl Pts',(-1.53391005274538,-0.264648874929275,
18.6750179800073));
#272192=CARTESIAN_POINT('Ctrl Pts',(-1.52197885983842,-0.32118623912761,
18.679166970011));
#272193=CARTESIAN_POINT('Ctrl Pts',(-1.51006890548561,-0.377622961933217,
18.683308574454));
#272194=CARTESIAN_POINT('Ctrl Pts',(-1.49499635161617,-0.433487595602833,
18.687450178897));
#272195=CARTESIAN_POINT('Ctrl Pts',(-1.47683588997844,-0.488401478367519,
18.69159178334));
#272196=CARTESIAN_POINT('Ctrl Pts',(-1.45869351899637,-0.543260658329841,
18.6957292620983));
#272197=CARTESIAN_POINT('Ctrl Pts',(-1.43746949749457,-0.597170472162358,
18.6998667408565));
#272198=CARTESIAN_POINT('Ctrl Pts',(-1.41328897637056,-0.649764972331879,
18.7040042196148));
#272199=CARTESIAN_POINT('Ctrl Pts',(-1.38912325789126,-0.702327275606414,
18.7081391655232));
#272200=CARTESIAN_POINT('Ctrl Pts',(-1.36200484454982,-0.75357538937617,
18.7122741114317));
#272201=CARTESIAN_POINT('Ctrl Pts',(-1.33210709816146,-0.803163077480445,
18.7164090573401));
#272202=CARTESIAN_POINT('Ctrl Pts',(-1.30221617470249,-0.852739449236975,
18.7205430596175));
#272203=CARTESIAN_POINT('Ctrl Pts',(-1.26954744603632,-0.900655702012691,
18.7246770618948));
#272204=CARTESIAN_POINT('Ctrl Pts',(-1.23431924712162,-0.946591911113297,
18.7288110641721));
#272205=CARTESIAN_POINT('Ctrl Pts',(-1.19905940702001,-0.992569379098057,
18.7329487795186));
#272206=CARTESIAN_POINT('Ctrl Pts',(-1.16123581917785,-1.0365628345512,
18.7370864948651));
#272207=CARTESIAN_POINT('Ctrl Pts',(-1.12110822496951,-1.07828409888383,
18.7412242102116));
#272208=CARTESIAN_POINT('Ctrl Pts',(-1.08096416148368,-1.12002248657243,
18.7453636237706));
#272209=CARTESIAN_POINT('Ctrl Pts',(-1.03851458757045,-1.15948646774434,
18.7495030373296));
#272210=CARTESIAN_POINT('Ctrl Pts',(-0.994055054977217,-1.19642584294817,
18.7536424508885));
#272211=CARTESIAN_POINT('Ctrl Pts',(-0.949509182631559,-1.2334369538704,
18.7577899031272));
#272212=CARTESIAN_POINT('Ctrl Pts',(-0.90294597044219,-1.26791334933861,
18.7619373553659));
#272213=CARTESIAN_POINT('Ctrl Pts',(-0.854692154271789,-1.29964671023561,
18.7660848076046));
#272214=CARTESIAN_POINT('Ctrl Pts',(-0.809136533122573,-1.32960564574675,
18.7700003479269));
#272215=CARTESIAN_POINT('Ctrl Pts',(-0.762074664077149,-1.35711994382657,
18.7739158882492));
#272216=CARTESIAN_POINT('Ctrl Pts',(-0.713800020992557,-1.38205274140715,
18.7778314285715));
#272217=CARTESIAN_POINT('Ctrl Pts',(-0.662644162089899,-1.40847362395714,
18.7819806633551));
#272218=CARTESIAN_POINT('Ctrl Pts',(-0.609912578938574,-1.43210558658674,
18.7861298981388));
#272219=CARTESIAN_POINT('Ctrl Pts',(-0.555940967516389,-1.45275940562673,
18.7902791329224));
#272220=CARTESIAN_POINT('Ctrl Pts',(-0.502065012393167,-1.47337661898021,
18.7944210138319));
#272221=CARTESIAN_POINT('Ctrl Pts',(-0.446953873401568,-1.49102598110697,
18.7985628947413));
#272222=CARTESIAN_POINT('Ctrl Pts',(-0.390966271700142,-1.50556488548083,
18.8027047756507));
#272223=CARTESIAN_POINT('Ctrl Pts',(-0.335034182048991,-1.52008937444187,
18.8068425498598));
#272224=CARTESIAN_POINT('Ctrl Pts',(-0.278227852725018,-1.53150938602532,
18.8109803240689));
#272225=CARTESIAN_POINT('Ctrl Pts',(-0.22092268181058,-1.5397316060475,
18.815118098278));
#272226=CARTESIAN_POINT('Ctrl Pts',(-0.163652336157003,-1.54794882929623,
18.8192533578961));
#272227=CARTESIAN_POINT('Ctrl Pts',(-0.105884263995698,-1.55297203957189,
18.8233886175142));
#272228=CARTESIAN_POINT('Ctrl Pts',(-0.0480034433414906,-1.55475911942248,
18.8275238771323));
#272229=CARTESIAN_POINT('Ctrl Pts',(0.00986441513524329,-1.5565457990637,
18.8316582106756));
#272230=CARTESIAN_POINT('Ctrl Pts',(0.0678444520235309,-1.55509777102806,
18.835792544219));
#272231=CARTESIAN_POINT('Ctrl Pts',(0.125549409195623,-1.55042497266093,
18.8399268777623));
#272232=CARTESIAN_POINT('Ctrl Pts',(0.183306533597198,-1.54574794992631,
18.8440649488827));
#272233=CARTESIAN_POINT('Ctrl Pts',(0.240787561214699,-1.53784037190848,
18.8482030200031));
#272234=CARTESIAN_POINT('Ctrl Pts',(0.297609450539051,-1.52676418118511,
18.8523410911236));
#272235=CARTESIAN_POINT('Ctrl Pts',(0.35445485067309,-1.51568340754106,
18.8564808744257));
#272236=CARTESIAN_POINT('Ctrl Pts',(0.410640062912466,-1.5014315344574,
18.8606206577279));
#272237=CARTESIAN_POINT('Ctrl Pts',(0.465794535428237,-1.48412118803189,
18.8647604410301));
#272238=CARTESIAN_POINT('Ctrl Pts',(0.521056353633815,-1.46677715093737,
18.868908281483));
#272239=CARTESIAN_POINT('Ctrl Pts',(0.575282933874055,-1.44636292780657,
18.8730561219358));
#272240=CARTESIAN_POINT('Ctrl Pts',(0.628121997755228,-1.42304005774117,
18.8772039623886));
#272241=CARTESIAN_POINT('Ctrl Pts',(0.677968997808009,-1.40103786807339,
18.8811169273067));
#272242=CARTESIAN_POINT('Ctrl Pts',(0.726581039451729,-1.37644771635597,
18.8850298922248));
#272243=CARTESIAN_POINT('Ctrl Pts',(0.773684537451322,-1.34944154616224,
18.8889428571429));
#272244=CARTESIAN_POINT('Ctrl Pts',(0.823545450020095,-1.32085444864224,
18.8930848850167));
#272245=CARTESIAN_POINT('Ctrl Pts',(0.871926305188375,-1.28943906380778,
18.8972269128904));
#272246=CARTESIAN_POINT('Ctrl Pts',(0.918486649111735,-1.25537346053017,
18.9013689407642));
#272247=CARTESIAN_POINT('Ctrl Pts',(0.9649640126152,-1.22136856939139,18.9055035866647));
#272248=CARTESIAN_POINT('Ctrl Pts',(1.00962688604308,-1.18472313970499,
18.9096382325652));
#272249=CARTESIAN_POINT('Ctrl Pts',(1.05216137632172,-1.14565993566014,
18.9137728784657));
#272250=CARTESIAN_POINT('Ctrl Pts',(1.0946534911311,-1.10663564877618,18.9179034051783));
#272251=CARTESIAN_POINT('Ctrl Pts',(1.13502104061593,-1.06519871093113,
18.9220339318909));
#272252=CARTESIAN_POINT('Ctrl Pts',(1.17298241452074,-1.02161269824973,
18.9261644586034));
#272253=CARTESIAN_POINT('Ctrl Pts',(1.2109206738195,-0.978053225005893,
18.9302924702464));
#272254=CARTESIAN_POINT('Ctrl Pts',(1.2464553190132,-0.93234766373174,18.9344204818894));
#272255=CARTESIAN_POINT('Ctrl Pts',(1.27934250116004,-0.88479546491015,
18.9385484935323));
#272256=CARTESIAN_POINT('Ctrl Pts',(1.31222239708508,-0.837253801374514,
18.9426755906059));
#272257=CARTESIAN_POINT('Ctrl Pts',(1.34245569726827,-0.787866741951971,
18.9468026876796));
#272258=CARTESIAN_POINT('Ctrl Pts',(1.36984101896112,-0.736963929084426,
18.9509297847532));
#272259=CARTESIAN_POINT('Ctrl Pts',(1.39725164353726,-0.686014084162731,
18.9550606950906));
#272260=CARTESIAN_POINT('Ctrl Pts',(1.42180878200753,-0.63354614784719,
18.959191605428));
#272261=CARTESIAN_POINT('Ctrl Pts',(1.44335701313008,-0.579914461492563,
18.9633225157654));
#272262=CARTESIAN_POINT('Ctrl Pts',(1.46491432766989,-0.526260167296834,
18.9674551674421));
#272263=CARTESIAN_POINT('Ctrl Pts',(1.48346003794147,-0.471441640916516,
18.9715878191189));
#272264=CARTESIAN_POINT('Ctrl Pts',(1.49888808133818,-0.415830217303106,
18.9757204707956));
#272265=CARTESIAN_POINT('Ctrl Pts',(1.51434673854817,-0.360108444133716,
18.9798613228788));
#272266=CARTESIAN_POINT('Ctrl Pts',(1.52667525381189,-0.303591141822869,
18.984002174962));
#272267=CARTESIAN_POINT('Ctrl Pts',(1.53581857345245,-0.246660818612296,
18.9881430270452));
#272268=CARTESIAN_POINT('Ctrl Pts',(1.54458556497539,-0.192073679519882,
18.9921134466016));
#272269=CARTESIAN_POINT('Ctrl Pts',(1.55042449470638,-0.137107278980882,
18.996083866158));
#272270=CARTESIAN_POINT('Ctrl Pts',(1.5533318590112,-0.0820998525017198,
19.0000542857144));
#272271=CARTESIAN_POINT('Ctrl Pts',(1.55639086283974,-0.0242234013400301,
19.0042317906124));
#272272=CARTESIAN_POINT('Ctrl Pts',(1.55621714226099,0.0339443710004242,
19.0084092955105));
#272273=CARTESIAN_POINT('Ctrl Pts',(1.5527761988485,0.0920126420097034,
19.0125868004085));
#272274=CARTESIAN_POINT('Ctrl Pts',(1.5493589106132,0.149681715742147,19.0167355865494));
#272275=CARTESIAN_POINT('Ctrl Pts',(1.54271916565345,0.207252128343795,
19.0208843726902));
#272276=CARTESIAN_POINT('Ctrl Pts',(1.53287509576863,0.26433726708945,19.025033158831));
#272277=CARTESIAN_POINT('Ctrl Pts',(1.5229288118468,0.322015138571926,19.0292250231077));
#272278=CARTESIAN_POINT('Ctrl Pts',(1.50971124661987,0.379197060509291,
19.0334168873844));
#272279=CARTESIAN_POINT('Ctrl Pts',(1.49329504324451,0.43548841984761,19.0376087516611));
#272280=CARTESIAN_POINT('Ctrl Pts',(1.47687883986916,0.491779779185915,
19.0418006159377));
#272281=CARTESIAN_POINT('Ctrl Pts',(1.45726411221541,0.547180037965144,
19.0459924802144));
#272282=CARTESIAN_POINT('Ctrl Pts',(1.43457668357356,0.601306900797836,
19.0501843444911));
#272283=CARTESIAN_POINT('Origin',(0.,0.,0.));
#272284=CARTESIAN_POINT('',(-1.95399958593193,0.00127207619237379,0.22586969212423));
#272285=CARTESIAN_POINT('',(0.861527879758777,1.75382031930251,3.92573008738128E-5));
#272286=CARTESIAN_POINT('Ctrl Pts',(-1.95399958593193,0.00127207619237379,
0.22586969212423));
#272287=CARTESIAN_POINT('Ctrl Pts',(-1.95395602836775,0.0681795954810932,
0.222037005420703));
#272288=CARTESIAN_POINT('Ctrl Pts',(-1.95047621447863,0.134982233331218,
0.218204318717176));
#272289=CARTESIAN_POINT('Ctrl Pts',(-1.94359078332685,0.201422111415151,
0.214371632013649));
#272290=CARTESIAN_POINT('Ctrl Pts',(-1.93653822890983,0.269474618994986,
0.210445918293744));
#272291=CARTESIAN_POINT('Ctrl Pts',(-1.92589346976546,0.337288960092626,
0.206520204573839));
#272292=CARTESIAN_POINT('Ctrl Pts',(-1.9116826354016,0.40445704531381,0.202594490853934));
#272293=CARTESIAN_POINT('Ctrl Pts',(-1.89749324764944,0.471523762254662,
0.198674701716329));
#272294=CARTESIAN_POINT('Ctrl Pts',(-1.87974856750535,0.537945683733757,
0.194754912578725));
#272295=CARTESIAN_POINT('Ctrl Pts',(-1.85852642413187,0.603320421338104,
0.19083512344112));
#272296=CARTESIAN_POINT('Ctrl Pts',(-1.83732958192574,0.668617218785931,
0.18692000749977));
#272297=CARTESIAN_POINT('Ctrl Pts',(-1.81266366201142,0.732868848475346,
0.18300489155842));
#272298=CARTESIAN_POINT('Ctrl Pts',(-1.78465700711252,0.795685469871221,
0.17908977561707));
#272299=CARTESIAN_POINT('Ctrl Pts',(-1.75666822735431,0.858461998798042,
0.175177158483539));
#272300=CARTESIAN_POINT('Ctrl Pts',(-1.72534314184954,0.919804890152479,
0.171264541350008));
#272301=CARTESIAN_POINT('Ctrl Pts',(-1.69085862348574,0.979343206125368,
0.167351924216477));
#272302=CARTESIAN_POINT('Ctrl Pts',(-1.65638440769107,1.03886373447512,
0.16344047601354));
#272303=CARTESIAN_POINT('Ctrl Pts',(-1.61875287845868,1.09658033418713,
0.159529027810603));
#272304=CARTESIAN_POINT('Ctrl Pts',(-1.57818652774778,1.15214724911159,
0.155617579607666));
#272305=CARTESIAN_POINT('Ctrl Pts',(-1.53761852548644,1.20771642629433,
0.15170597216058));
#272306=CARTESIAN_POINT('Ctrl Pts',(-1.4941157553654,1.26113535078223,0.147794364713494));
#272307=CARTESIAN_POINT('Ctrl Pts',(-1.44794258902418,1.31208927245441,
0.143882757266408));
#272308=CARTESIAN_POINT('Ctrl Pts',(-1.40172219393538,1.36309531292405,
0.139967148787221));
#272309=CARTESIAN_POINT('Ctrl Pts',(-1.35282628071841,1.41163095476592,
0.136051540308034));
#272310=CARTESIAN_POINT('Ctrl Pts',(-1.30155719667164,1.45741718934293,
0.132135931828847));
#272311=CARTESIAN_POINT('Ctrl Pts',(-1.25025852714807,1.50322984544876,
0.128218063798002));
#272312=CARTESIAN_POINT('Ctrl Pts',(-1.19658434270726,1.54628962916973,
0.124300195767158));
#272313=CARTESIAN_POINT('Ctrl Pts',(-1.14086913813976,1.58635860058192,
0.120382327736313));
#272314=CARTESIAN_POINT('Ctrl Pts',(-1.08506069260544,1.6264946285483,0.116457903042778));
#272315=CARTESIAN_POINT('Ctrl Pts',(-1.02720482132577,1.66362958935378,
0.112533478349243));
#272316=CARTESIAN_POINT('Ctrl Pts',(-0.967663207261701,1.69757000365581,
0.108609053655708));
#272317=CARTESIAN_POINT('Ctrl Pts',(-0.940612178557402,1.71298985976741,
0.106826103584545));
#272318=CARTESIAN_POINT('Ctrl Pts',(-0.913213507191092,1.72775098046652,
0.105043153513382));
#272319=CARTESIAN_POINT('Ctrl Pts',(-0.885502465630419,1.74183850668265,
0.10326020344222));
#272320=CARTESIAN_POINT('Ctrl Pts',(-0.825166121774214,1.7725118331976,
0.0993781159235467));
#272321=CARTESIAN_POINT('Ctrl Pts',(-0.763105599279648,1.8001116002205,
0.0954960284048736));
#272322=CARTESIAN_POINT('Ctrl Pts',(-0.699669805911684,1.82443913647332,
0.0916139408862006));
#272323=CARTESIAN_POINT('Ctrl Pts',(-0.636340329488619,1.84872590032945,
0.0877383596577921));
#272324=CARTESIAN_POINT('Ctrl Pts',(-0.57164062294732,1.86975114375477,
0.0838627784293837));
#272325=CARTESIAN_POINT('Ctrl Pts',(-0.505943004118793,1.88736262455927,
0.0799871972009753));
#272326=CARTESIAN_POINT('Ctrl Pts',(-0.440306865741454,1.90495762437397,
0.0761152427780247));
#272327=CARTESIAN_POINT('Ctrl Pts',(-0.37367514811737,1.91914506387478,
0.0722432883550741));
#272328=CARTESIAN_POINT('Ctrl Pts',(-0.306437506041051,1.92982176764885,
0.0683713339321236));
#272329=CARTESIAN_POINT('Ctrl Pts',(-0.239238675526287,1.94049230851279,
0.0645016145161243));
#272330=CARTESIAN_POINT('Ctrl Pts',(-0.171435108718065,1.94765605344516,
0.0606318951001249));
#272331=CARTESIAN_POINT('Ctrl Pts',(-0.103426987508651,1.95126083808774,
0.0567621756841256));
#272332=CARTESIAN_POINT('Ctrl Pts',(-0.0354337387159423,1.95486483441478,
0.0528933025211718));
#272333=CARTESIAN_POINT('Ctrl Pts',(0.0327634747013058,1.95491138939906,
0.049024429358218));
#272334=CARTESIAN_POINT('Ctrl Pts',(0.100760960714834,1.95140032509883,
0.0451555561952642));
#272335=CARTESIAN_POINT('Ctrl Pts',(0.168813418867247,1.9478864223008,0.0412835552661926));
#272336=CARTESIAN_POINT('Ctrl Pts',(0.236665324606256,1.9408091779182,0.0374115543371211));
#272337=CARTESIAN_POINT('Ctrl Pts',(0.30391575984376,1.93022050836649,0.0335395534080496));
#272338=CARTESIAN_POINT('Ctrl Pts',(0.371191768943996,1.91962781217643,
0.0296660800421098));
#272339=CARTESIAN_POINT('Ctrl Pts',(0.437865359858098,1.90552113363803,
0.0257926066761699));
#272340=CARTESIAN_POINT('Ctrl Pts',(0.503546370093836,1.88800345687324,
0.0219191333102301));
#272341=CARTESIAN_POINT('Ctrl Pts',(0.569342432687873,1.87045509467874,
0.0180388748439399));
#272342=CARTESIAN_POINT('Ctrl Pts',(0.634141962373302,1.84948395228774,
0.0141586163776498));
#272343=CARTESIAN_POINT('Ctrl Pts',(0.697571235538963,1.82524255137465,
0.0102783579113597));
#272344=CARTESIAN_POINT('Ctrl Pts',(0.753362940759582,1.80392007633468,
0.00686532437453106));
#272345=CARTESIAN_POINT('Ctrl Pts',(0.808094597965651,1.78006831145149,
0.00345229083770244));
#272346=CARTESIAN_POINT('Ctrl Pts',(0.861527879758777,1.75382031930251,
3.92573008738128E-5));
#272347=CARTESIAN_POINT('',(-0.861525859670488,1.75382131162756,0.));
#272348=CARTESIAN_POINT('Origin',(0.,0.,0.));
#272349=CARTESIAN_POINT('',(-1.953998900791,0.00207260887720313,0.124130307921729));
#272350=CARTESIAN_POINT('Ctrl Pts',(-0.861525859670491,1.75382131162756,
-2.22044604925031E-15));
#272351=CARTESIAN_POINT('Ctrl Pts',(-0.92465034722954,1.72281280577237,
0.00400987370320275));
#272352=CARTESIAN_POINT('Ctrl Pts',(-0.986146025991561,1.68836919186938,
0.00801974740640772));
#272353=CARTESIAN_POINT('Ctrl Pts',(-1.04563219790624,1.65068752545773,
0.0120296211096127));
#272354=CARTESIAN_POINT('Ctrl Pts',(-1.10690424482723,1.61187459199569,
0.0161598779706933));
#272355=CARTESIAN_POINT('Ctrl Pts',(-1.16604372940432,1.56962626415352,
0.0202901348317739));
#272356=CARTESIAN_POINT('Ctrl Pts',(-1.22266333358954,1.52420811331514,
0.0244203916928544));
#272357=CARTESIAN_POINT('Ctrl Pts',(-1.27759315554719,1.48014544323648,
0.0284273832160793));
#272358=CARTESIAN_POINT('Ctrl Pts',(-1.33015104229541,1.4330998336613,0.0324343747393041));
#272359=CARTESIAN_POINT('Ctrl Pts',(-1.38001546857801,1.38335581340645,
0.0364413662625289));
#272360=CARTESIAN_POINT('Ctrl Pts',(-1.42988102198453,1.33361066874931,
0.0404484483588601));
#272361=CARTESIAN_POINT('Ctrl Pts',(-1.47705266894162,1.2811673162302,0.0444555304551913));
#272362=CARTESIAN_POINT('Ctrl Pts',(-1.52124575697518,1.22634715594117,
0.0484626125515224));
#272363=CARTESIAN_POINT('Ctrl Pts',(-1.56545178522649,1.17151094371184,
0.0524708679651565));
#272364=CARTESIAN_POINT('Ctrl Pts',(-1.60667723309791,1.11429689771893,
0.0564791233787905));
#272365=CARTESIAN_POINT('Ctrl Pts',(-1.64467863203096,1.0550583857497,0.0604873787924245));
#272366=CARTESIAN_POINT('Ctrl Pts',(-1.68270143072715,0.995786514742109,
0.0644978913786586));
#272367=CARTESIAN_POINT('Ctrl Pts',(-1.71749632401162,0.934488297596708,
0.0685084039648928));
#272368=CARTESIAN_POINT('Ctrl Pts',(-1.74886467593283,0.871543656551046,
0.072518916551127));
#272369=CARTESIAN_POINT('Ctrl Pts',(-1.7802817510142,0.808501246204819,
0.0765356585002418));
#272370=CARTESIAN_POINT('Ctrl Pts',(-1.80826145814717,0.74380771951913,
0.0805524004493565));
#272371=CARTESIAN_POINT('Ctrl Pts',(-1.83265261212681,0.677864590655674,
0.0845691423984713));
#272372=CARTESIAN_POINT('Ctrl Pts',(-1.85706588858064,0.611861652192088,
0.0885895274827229));
#272373=CARTESIAN_POINT('Ctrl Pts',(-1.87788399325823,0.544607291841708,
0.0926099125669745));
#272374=CARTESIAN_POINT('Ctrl Pts',(-1.89500585440512,0.476517378245858,
0.0966302976512262));
#272375=CARTESIAN_POINT('Ctrl Pts',(-1.91215919769098,0.408302267038415,
0.100658075058124));
#272376=CARTESIAN_POINT('Ctrl Pts',(-1.92560264274347,0.339248985282941,
0.104685852465021));
#272377=CARTESIAN_POINT('Ctrl Pts',(-1.93528643133502,0.269782187496798,
0.108713629871919));
#272378=CARTESIAN_POINT('Ctrl Pts',(-1.93724361674103,0.255742289625824,
0.109527681839795));
#272379=CARTESIAN_POINT('Ctrl Pts',(-1.93904739689901,0.241685508467463,
0.110341733807671));
#272380=CARTESIAN_POINT('Ctrl Pts',(-1.94069761933797,0.227615356019609,
0.111155785775547));
#272381=CARTESIAN_POINT('Ctrl Pts',(-1.94946481043858,0.152864393717388,
0.115480626475622));
#272382=CARTESIAN_POINT('Ctrl Pts',(-1.95391883477712,0.0775566253238957,
0.119805467175698));
#272383=CARTESIAN_POINT('Ctrl Pts',(-1.95399890079015,0.00207260967928642,
0.124130307875774));
#272384=CARTESIAN_POINT('',(-1.95388395640249,0.000897708686404772,0.824130264813444));
#272385=CARTESIAN_POINT('Ctrl Pts',(-1.953998900791,0.00207260887720443,
0.124130307921729));
#272386=CARTESIAN_POINT('Ctrl Pts',(-1.95406971485036,-0.0646889473779068,
0.12795539715713));
#272387=CARTESIAN_POINT('Ctrl Pts',(-1.95071486305986,-0.131609446464987,
0.13178048639253));
#272388=CARTESIAN_POINT('Ctrl Pts',(-1.94391209993599,-0.198297119803763,
0.135605575627931));
#272389=CARTESIAN_POINT('Ctrl Pts',(-1.93711993049559,-0.264880942973053,
0.139424708197796));
#272390=CARTESIAN_POINT('Ctrl Pts',(-1.92689055170305,-0.331232150947945,
0.143243840767662));
#272391=CARTESIAN_POINT('Ctrl Pts',(-1.91325372797823,-0.396958653234087,
0.147062973337527));
#272392=CARTESIAN_POINT('Ctrl Pts',(-1.89962855986798,-0.462628978011944,
0.150878841632798));
#272393=CARTESIAN_POINT('Ctrl Pts',(-1.88260181766083,-0.527675151600647,
0.154694709928069));
#272394=CARTESIAN_POINT('Ctrl Pts',(-1.86225490420209,-0.591711645799947,
0.15851057822334));
#272395=CARTESIAN_POINT('Ctrl Pts',(-1.84191771893619,-0.655717523101673,
0.162324622089429));
#272396=CARTESIAN_POINT('Ctrl Pts',(-1.81826366361196,-0.71871418653411,
0.166138665955518));
#272397=CARTESIAN_POINT('Ctrl Pts',(-1.79142439797722,-0.780329818943215,
0.169952709821607));
#272398=CARTESIAN_POINT('Ctrl Pts',(-1.76458786151898,-0.841939185907573,
0.173766365852982));
#272399=CARTESIAN_POINT('Ctrl Pts',(-1.73456696517133,-0.902167328318251,
0.177580021884358));
#272400=CARTESIAN_POINT('Ctrl Pts',(-1.70154123168827,-0.960663019411473,
0.181393677915734));
#272401=CARTESIAN_POINT('Ctrl Pts',(-1.66848411293453,-1.01921430058263,
0.185210958170229));
#272402=CARTESIAN_POINT('Ctrl Pts',(-1.63241671219014,-1.07602939448073,
0.189028238424724));
#272403=CARTESIAN_POINT('Ctrl Pts',(-1.59356352779417,-1.13078348187626,
0.192845518679218));
#272404=CARTESIAN_POINT('Ctrl Pts',(-1.5546904210311,-1.1855656449893,0.196664756283148));
#272405=CARTESIAN_POINT('Ctrl Pts',(-1.51302901232075,-1.23828429714149,
0.200483993887078));
#272406=CARTESIAN_POINT('Ctrl Pts',(-1.46884405400318,-1.28864779711894,
0.204303231491008));
#272407=CARTESIAN_POINT('Ctrl Pts',(-1.42458132810623,-1.33909993919613,
0.208129191130555));
#272408=CARTESIAN_POINT('Ctrl Pts',(-1.37778655272207,-1.38718829192004,
0.211955150770102));
#272409=CARTESIAN_POINT('Ctrl Pts',(-1.32876043561764,-1.43265896316507,
0.215781110409649));
#272410=CARTESIAN_POINT('Ctrl Pts',(-1.3008665054816,-1.45852998460954,
0.217957930790131));
#272411=CARTESIAN_POINT('Ctrl Pts',(-1.27225085348762,-1.48355436721595,
0.220134751170613));
#272412=CARTESIAN_POINT('Ctrl Pts',(-1.24297306706696,-1.50769159795568,
0.222311571551095));
#272413=CARTESIAN_POINT('Ctrl Pts',(-1.19019641227937,-1.55120179630116,
0.226235546407139));
#272414=CARTESIAN_POINT('Ctrl Pts',(-1.13502956194456,-1.59202229000584,
0.230159521263182));
#272415=CARTESIAN_POINT('Ctrl Pts',(-1.07777745471449,-1.6298809030445,
0.234083496119226));
#272416=CARTESIAN_POINT('Ctrl Pts',(-1.02061138076857,-1.66768262558654,
0.238001574381064));
#272417=CARTESIAN_POINT('Ctrl Pts',(-0.961366675148951,-1.70253103344955,
0.241919652642901));
#272418=CARTESIAN_POINT('Ctrl Pts',(-0.900381093305233,-1.73419430480511,
0.245837730904739));
#272419=CARTESIAN_POINT('Ctrl Pts',(-0.839467503967435,-1.76582019817423,
0.249751183937729));
#272420=CARTESIAN_POINT('Ctrl Pts',(-0.776817553295469,-1.79426819851077,
0.253664636970718));
#272421=CARTESIAN_POINT('Ctrl Pts',(-0.712796163719197,-1.81935088121758,
0.257578090003708));
#272422=CARTESIAN_POINT('Ctrl Pts',(-0.648815159425008,-1.84441774153717,
0.261489074394488));
#272423=CARTESIAN_POINT('Ctrl Pts',(-0.583464887912403,-1.86612331741961,
0.265400058785267));
#272424=CARTESIAN_POINT('Ctrl Pts',(-0.51713155549024,-1.88432771945759,
0.269311043176047));
#272425=CARTESIAN_POINT('Ctrl Pts',(-0.450817509770402,-1.90252682848721,
0.273220890431257));
#272426=CARTESIAN_POINT('Ctrl Pts',(-0.383521443077999,-1.91722665508607,
0.277130737686467));
#272427=CARTESIAN_POINT('Ctrl Pts',(-0.315644359726697,-1.92833727293042,
0.281040584941677));
#272428=CARTESIAN_POINT('Ctrl Pts',(-0.247763930970189,-1.93944843837518,
0.284950624898498));
#272429=CARTESIAN_POINT('Ctrl Pts',(-0.179302912831436,-1.94696996714431,
0.28886066485532));
#272430=CARTESIAN_POINT('Ctrl Pts',(-0.110670350904324,-1.95086341742079,
0.292770704812142));
#272431=CARTESIAN_POINT('Ctrl Pts',(-0.0419664489043466,-1.95476091474168,
0.296684809057511));
#272432=CARTESIAN_POINT('Ctrl Pts',(0.0269088624428499,-1.95502277925515,
0.30059891330288));
#272433=CARTESIAN_POINT('Ctrl Pts',(0.0955445968728496,-1.95166268345952,
0.30451301754825));
#272434=CARTESIAN_POINT('Ctrl Pts',(0.16422050178672,-1.94830062109829,
0.308429412604124));
#272435=CARTESIAN_POINT('Ctrl Pts',(0.232656062905091,-1.94131242848719,
0.312345807659998));
#272436=CARTESIAN_POINT('Ctrl Pts',(0.300446258658313,-1.93076359134365,
0.316262202715873));
#272437=CARTESIAN_POINT('Ctrl Pts',(0.368351200806611,-1.92019689850547,
0.320185226934111));
#272438=CARTESIAN_POINT('Ctrl Pts',(0.435608117702528,-1.90605763224043,
0.32410825115235));
#272439=CARTESIAN_POINT('Ctrl Pts',(0.501823857525544,-1.88846202398094,
0.328031275370588));
#272440=CARTESIAN_POINT('Ctrl Pts',(0.53240861122868,-1.88033469132088,
0.329843302689274));
#272441=CARTESIAN_POINT('Ctrl Pts',(0.56277147105196,-1.8714706486461,0.331655330007959));
#272442=CARTESIAN_POINT('Ctrl Pts',(0.592875114421119,-1.86188482423058,
0.333467357326644));
#272443=CARTESIAN_POINT('Ctrl Pts',(0.6580782666512,-1.84112235501877,0.337392127882037));
#272444=CARTESIAN_POINT('Ctrl Pts',(0.722313696634057,-1.81689109617585,
0.341316898437429));
#272445=CARTESIAN_POINT('Ctrl Pts',(0.785187368964933,-1.78930064427919,
0.345241668992821));
#272446=CARTESIAN_POINT('Ctrl Pts',(0.847968839732872,-1.76175065260527,
0.349160684039334));
#272447=CARTESIAN_POINT('Ctrl Pts',(0.909392071410045,-1.73085144117634,
0.353079699085847));
#272448=CARTESIAN_POINT('Ctrl Pts',(0.969079276154258,-1.6967620211828,
0.356998714132359));
#272449=CARTESIAN_POINT('Ctrl Pts',(1.02869916732254,-1.66271104629271,
0.360913309422276));
#272450=CARTESIAN_POINT('Ctrl Pts',(1.08658649656621,-1.6254772505299,0.364827904712192));
#272451=CARTESIAN_POINT('Ctrl Pts',(1.14238615553471,-1.58526649861865,
0.368742500002108));
#272452=CARTESIAN_POINT('Ctrl Pts',(1.19815243861168,-1.5450797982826,0.37265475382417));
#272453=CARTESIAN_POINT('Ctrl Pts',(1.25183313215595,-1.50191996032999,
0.376567007646231));
#272454=CARTESIAN_POINT('Ctrl Pts',(1.30310164381818,-1.4560364370023,0.380479261468293));
#272455=CARTESIAN_POINT('Ctrl Pts',(1.35435689983018,-1.41016477701757,
0.384390503763657));
#272456=CARTESIAN_POINT('Ctrl Pts',(1.40320084736407,-1.36157115648459,
0.388301746059021));
#272457=CARTESIAN_POINT('Ctrl Pts',(1.44934095252709,-1.31054446827563,
0.392212988354385));
#272458=CARTESIAN_POINT('Ctrl Pts',(1.49548479582514,-1.25951364603512,
0.396124547527046));
#272459=CARTESIAN_POINT('Ctrl Pts',(1.53892403512438,-1.20604972982545,
0.400036106699708));
#272460=CARTESIAN_POINT('Ctrl Pts',(1.57940512122791,-1.15047618968802,
0.40394766587237));
#272461=CARTESIAN_POINT('Ctrl Pts',(1.61993011734768,-1.09484236868154,
0.407863467930867));
#272462=CARTESIAN_POINT('Ctrl Pts',(1.65749026776217,-1.03709475378983,
0.411779269989364));
#272463=CARTESIAN_POINT('Ctrl Pts',(1.69187482098419,-0.977586615149637,
0.415695072047861));
#272464=CARTESIAN_POINT('Ctrl Pts',(1.72628040799284,-0.918042074073651,
0.419613269488507));
#272465=CARTESIAN_POINT('Ctrl Pts',(1.7575063090594,-0.856735302355073,
0.423531466929153));
#272466=CARTESIAN_POINT('Ctrl Pts',(1.78538859830257,-0.794042538565279,
0.427449664369799));
#272467=CARTESIAN_POINT('Ctrl Pts',(1.81331908096952,-0.731241412836216,
0.431374634258292));
#272468=CARTESIAN_POINT('Ctrl Pts',(1.83789424193406,-0.667049970909388,
0.435299604146784));
#272469=CARTESIAN_POINT('Ctrl Pts',(1.85899926528549,-0.601861887535665,
0.439224574035277));
#272470=CARTESIAN_POINT('Ctrl Pts',(1.86867551159723,-0.571974408104326,
0.441024097057582));
#272471=CARTESIAN_POINT('Ctrl Pts',(1.87762302268613,-0.541877600403308,
0.442823620079887));
#272472=CARTESIAN_POINT('Ctrl Pts',(1.88583433470006,-0.511610068378626,
0.444623143102192));
#272473=CARTESIAN_POINT('Ctrl Pts',(1.90368746628818,-0.445802042673616,
0.448535687316633));
#272474=CARTESIAN_POINT('Ctrl Pts',(1.91812816343621,-0.378924298650098,
0.452448231531075));
#272475=CARTESIAN_POINT('Ctrl Pts',(1.92903299696811,-0.311364250690772,
0.456360775745517));
#272476=CARTESIAN_POINT('Ctrl Pts',(1.93992115319753,-0.243907525661809,
0.460267336312143));
#272477=CARTESIAN_POINT('Ctrl Pts',(1.94728409878175,-0.175771050509559,
0.464173896878769));
#272478=CARTESIAN_POINT('Ctrl Pts',(1.95104862591321,-0.107355760544837,
0.468080457445395));
#272479=CARTESIAN_POINT('Ctrl Pts',(1.95480862761923,-0.0390227141883073,
0.47198232184488));
#272480=CARTESIAN_POINT('Ctrl Pts',(1.95497877423996,0.0295879910690269,
0.475884186244366));
#272481=CARTESIAN_POINT('Ctrl Pts',(1.95153747598598,0.0980687504879788,
0.479786050643852));
#272482=CARTESIAN_POINT('Ctrl Pts',(1.94809838760666,0.166505534092153,
0.483685409410112));
#272483=CARTESIAN_POINT('Ctrl Pts',(1.94105247895137,0.234812045663115,
0.487584768176372));
#272484=CARTESIAN_POINT('Ctrl Pts',(1.93043024173676,0.302580702934179,
0.491484126942632));
#272485=CARTESIAN_POINT('Ctrl Pts',(1.91981115370218,0.370329268797202,
0.495382329664029));
#272486=CARTESIAN_POINT('Ctrl Pts',(1.90561791803515,0.437539809572893,
0.499280532385427));
#272487=CARTESIAN_POINT('Ctrl Pts',(1.88793266539845,0.503811721699204,
0.503178735106825));
#272488=CARTESIAN_POINT('Ctrl Pts',(1.87024654240509,0.570086895311284,
0.507077129673188));
#272489=CARTESIAN_POINT('Ctrl Pts',(1.84906819099268,0.635422872417174,
0.510975524239551));
#272490=CARTESIAN_POINT('Ctrl Pts',(1.82452998782281,0.699432858489848,
0.514873918805914));
#272491=CARTESIAN_POINT('Ctrl Pts',(1.79996570268938,0.763510881578643,
0.518776457024702));
#272492=CARTESIAN_POINT('Ctrl Pts',(1.77203461565791,0.826259639158054,
0.522678995243489));
#272493=CARTESIAN_POINT('Ctrl Pts',(1.7409174097096,0.887311992801872,0.526581533462276));
#272494=CARTESIAN_POINT('Ctrl Pts',(1.70978171060432,0.948400630254737,
0.530486390984793));
#272495=CARTESIAN_POINT('Ctrl Pts',(1.67545637146238,1.00779043017206,0.53439124850731));
#272496=CARTESIAN_POINT('Ctrl Pts',(1.6381668245706,1.06514104928703,0.538296106029828));
#272497=CARTESIAN_POINT('Ctrl Pts',(1.60081238762202,1.12259146808428,0.542207758658415));
#272498=CARTESIAN_POINT('Ctrl Pts',(1.56048373837106,1.17799522513034,0.546119411287002));
#272499=CARTESIAN_POINT('Ctrl Pts',(1.51744764577593,1.23104372072201,0.550031063915589));
#272500=CARTESIAN_POINT('Ctrl Pts',(1.49636826473821,1.25702724721393,0.551947018902973));
#272501=CARTESIAN_POINT('Ctrl Pts',(1.47463991823078,1.28244626566927,0.553862973890357));
#272502=CARTESIAN_POINT('Ctrl Pts',(1.45229707936367,1.30726783532364,0.555778928877742));
#272503=CARTESIAN_POINT('Ctrl Pts',(1.40659466211201,1.35804051197105,0.559698026839719));
#272504=CARTESIAN_POINT('Ctrl Pts',(1.35813616589249,1.40651401080766,0.563617124801696));
#272505=CARTESIAN_POINT('Ctrl Pts',(1.30718194018394,1.45237439224773,0.567536222763673));
#272506=CARTESIAN_POINT('Ctrl Pts',(1.25630440716111,1.4981657478951,0.571449421977428));
#272507=CARTESIAN_POINT('Ctrl Pts',(1.2029389623525,1.54135146580705,0.575362621191183));
#272508=CARTESIAN_POINT('Ctrl Pts',(1.14738442864059,1.58165260816436,0.579275820404938));
#272509=CARTESIAN_POINT('Ctrl Pts',(1.09189524003699,1.62190634696454,0.583184416782355));
#272510=CARTESIAN_POINT('Ctrl Pts',(1.03422247241362,1.65928196144433,0.587093013159773));
#272511=CARTESIAN_POINT('Ctrl Pts',(0.974698429202499,1.69354036624764,
0.59100160953719));
#272512=CARTESIAN_POINT('Ctrl Pts',(0.915211719349837,1.72777728424935,
0.594907754450934));
#272513=CARTESIAN_POINT('Ctrl Pts',(0.853876462352962,1.75890062628619,
0.598813899364678));
#272514=CARTESIAN_POINT('Ctrl Pts',(0.791053073003582,1.78671515236525,
0.602720044278422));
#272515=CARTESIAN_POINT('Ctrl Pts',(0.728247568779264,1.81452175995596,
0.606625077155853));
#272516=CARTESIAN_POINT('Ctrl Pts',(0.663955222543311,1.83902122269039,
0.610530110033284));
#272517=CARTESIAN_POINT('Ctrl Pts',(0.59855848983272,1.8600655188055,0.614435142910714));
#272518=CARTESIAN_POINT('Ctrl Pts',(0.533157976618605,1.88111103146511,
0.618340401533223));
#272519=CARTESIAN_POINT('Ctrl Pts',(0.466653418924475,1.89870083278995,
0.622245660155732));
#272520=CARTESIAN_POINT('Ctrl Pts',(0.399442837896673,1.91273663091735,
0.626150918778241));
#272521=CARTESIAN_POINT('Ctrl Pts',(0.332160863866813,1.92678733827108,
0.630060325678188));
#272522=CARTESIAN_POINT('Ctrl Pts',(0.264171851944922,1.93727640759385,
0.633969732578135));
#272523=CARTESIAN_POINT('Ctrl Pts',(0.195883442020762,1.94415680364062,
0.637879139478082));
#272524=CARTESIAN_POINT('Ctrl Pts',(0.127554293985283,1.95104130425418,
0.641790878572521));
#272525=CARTESIAN_POINT('Ctrl Pts',(0.0589258835932126,1.95431282358562,
0.64570261766696));
#272526=CARTESIAN_POINT('Ctrl Pts',(-0.00959242815166069,1.95397645464887,
0.649614356761399));
#272527=CARTESIAN_POINT('Ctrl Pts',(-0.0782288447553711,1.95363950591374,
0.653532838511659));
#272528=CARTESIAN_POINT('Ctrl Pts',(-0.146754293397251,1.94968228507878,
0.657451320261919));
#272529=CARTESIAN_POINT('Ctrl Pts',(-0.214763690333836,1.94216182572776,
0.66136980201218));
#272530=CARTESIAN_POINT('Ctrl Pts',(-0.246958672714578,1.93860171393135,
0.66322477289255));
#272531=CARTESIAN_POINT('Ctrl Pts',(-0.279038147342052,1.9342438321239,
0.665079743772919));
#272532=CARTESIAN_POINT('Ctrl Pts',(-0.310960116170037,1.92909818468411,
0.666934714653289));
#272533=CARTESIAN_POINT('Ctrl Pts',(-0.378397140896669,1.91822770374662,
0.670853449045919));
#272534=CARTESIAN_POINT('Ctrl Pts',(-0.445396648823328,1.90379532395704,
0.674772183438549));
#272535=CARTESIAN_POINT('Ctrl Pts',(-0.511553747936856,1.88584961303169,
0.678690917831179));
#272536=CARTESIAN_POINT('Ctrl Pts',(-0.57761148609735,1.86793085466266,
0.682603766699971));
#272537=CARTESIAN_POINT('Ctrl Pts',(-0.642828855711058,1.84650936526824,
0.686516615568762));
#272538=CARTESIAN_POINT('Ctrl Pts',(-0.706809520717932,1.82168501707142,
0.690429464437553));
#272539=CARTESIAN_POINT('Ctrl Pts',(-0.770715273941606,1.79688973447105,
0.694337731945927));
#272540=CARTESIAN_POINT('Ctrl Pts',(-0.833386742062816,1.76869968288066,
0.6982459994543));
#272541=CARTESIAN_POINT('Ctrl Pts',(-0.894442926679376,1.73726447350806,
0.702154266962674));
#272542=CARTESIAN_POINT('Ctrl Pts',(-0.955461025584627,1.70584887283385,
0.706060096566535));
#272543=CARTESIAN_POINT('Ctrl Pts',(-1.0148654035447,1.67119235450491,0.709965926170395));
#272544=CARTESIAN_POINT('Ctrl Pts',(-1.07229666946121,1.63349191998687,
0.713871755774256));
#272545=CARTESIAN_POINT('Ctrl Pts',(-1.12971179117575,1.59580208324026,
0.717776487430839));
#272546=CARTESIAN_POINT('Ctrl Pts',(-1.1851544910801,1.55507029866374,0.721681219087423));
#272547=CARTESIAN_POINT('Ctrl Pts',(-1.2382931114427,1.51153768400049,0.725585950744007));
#272548=CARTESIAN_POINT('Ctrl Pts',(-1.29143500306418,1.46800238943228,
0.729490922779209));
#272549=CARTESIAN_POINT('Ctrl Pts',(-1.34227215480009,1.42166623603719,
0.733395894814411));
#272550=CARTESIAN_POINT('Ctrl Pts',(-1.39050626367589,1.37281037681033,
0.737300866849613));
#272551=CARTESIAN_POINT('Ctrl Pts',(-1.43879191173385,1.32390231404769,
0.741210011431374));
#272552=CARTESIAN_POINT('Ctrl Pts',(-1.48446861997378,1.27246952289924,
0.745119156013136));
#272553=CARTESIAN_POINT('Ctrl Pts',(-1.52727594550763,1.21882902257609,
0.749028300594897));
#272554=CARTESIAN_POINT('Ctrl Pts',(-1.57010895751071,1.16515633535399,
0.752939790852796));
#272555=CARTESIAN_POINT('Ctrl Pts',(-1.61006887410968,1.10927370250086,
0.756851281110694));
#272556=CARTESIAN_POINT('Ctrl Pts',(-1.64693812859499,1.0515278410865,0.760762771368593));
#272557=CARTESIAN_POINT('Ctrl Pts',(-1.68387116070946,0.993682089012924,
0.76468102784888));
#272558=CARTESIAN_POINT('Ctrl Pts',(-1.71770261794877,0.93396710317401,
0.768599284329167));
#272559=CARTESIAN_POINT('Ctrl Pts',(-1.74826090204655,0.872754156893794,
0.772517540809453));
#272560=CARTESIAN_POINT('Ctrl Pts',(-1.76274864544053,0.843732977063809,
0.774375194015915));
#272561=CARTESIAN_POINT('Ctrl Pts',(-1.77650137211546,0.814375384895663,
0.776232847222377));
#272562=CARTESIAN_POINT('Ctrl Pts',(-1.78950466680477,0.784722274109725,
0.778090500428838));
#272563=CARTESIAN_POINT('Ctrl Pts',(-1.81966708733528,0.715938968114354,
0.78239950968779));
#272564=CARTESIAN_POINT('Ctrl Pts',(-1.84589697902349,0.645330203163963,
0.786708518946742));
#272565=CARTESIAN_POINT('Ctrl Pts',(-1.86799266684287,0.573340559023402,
0.791017528205694));
#272566=CARTESIAN_POINT('Ctrl Pts',(-1.89002192877661,0.501567336109809,
0.795313583364345));
#272567=CARTESIAN_POINT('Ctrl Pts',(-1.90794163694281,0.428421806118558,
0.799609638522996));
#272568=CARTESIAN_POINT('Ctrl Pts',(-1.92159819855776,0.354367553959984,
0.803905693681647));
#272569=CARTESIAN_POINT('Ctrl Pts',(-1.93518759565743,0.280677508992798,
0.808180620354927));
#272570=CARTESIAN_POINT('Ctrl Pts',(-1.9445555435709,0.206087959977226,
0.812455547028207));
#272571=CARTESIAN_POINT('Ctrl Pts',(-1.94959882342639,0.131074130530993,
0.816730473701487));
#272572=CARTESIAN_POINT('Ctrl Pts',(-1.9525087531185,0.0877917873179581,
0.819197070125765));
#272573=CARTESIAN_POINT('Ctrl Pts',(-1.95397982047966,0.0443685117972613,
0.821663666550042));
#272574=CARTESIAN_POINT('Ctrl Pts',(-1.95399979374754,0.000897794274978164,
0.82413026297432));
#272575=CARTESIAN_POINT('',(-1.95294106986963,-0.00171292579279444,1.52413030787577));
#272576=CARTESIAN_POINT('Ctrl Pts',(-1.9511716724286,0.000895704665025933,
0.824130307875774));
#272577=CARTESIAN_POINT('Ctrl Pts',(-1.94962095971081,-0.381081020904075,
0.845835633985312));
#272578=CARTESIAN_POINT('Ctrl Pts',(-1.6566714212464,-1.41732346558056,
0.904592888686698));
#272579=CARTESIAN_POINT('Ctrl Pts',(0.0263707153274739,-2.30948448311516,
1.00040207197994));
#272580=CARTESIAN_POINT('Ctrl Pts',(1.95483546415058,-1.23008919255452,
1.11155785775549));
#272581=CARTESIAN_POINT('Ctrl Pts',(2.09350030880432,0.975583768053607,
1.22271364353102));
#272582=CARTESIAN_POINT('Ctrl Pts',(0.315389825019358,2.28801419101323,
1.33386942930658));
#272583=CARTESIAN_POINT('Ctrl Pts',(-1.55282847017919,1.58079173016818,
1.43434165075483));
#272584=CARTESIAN_POINT('Ctrl Pts',(-1.94904571141455,0.461263095178057,
1.49776194361122));
#272585=CARTESIAN_POINT('Ctrl Pts',(-1.95294106986963,-0.00171292579279444,
1.52413030787577));
#272586=CARTESIAN_POINT('',(-1.954314499219,0.000110167652081693,2.22413030787577));
#272587=CARTESIAN_POINT('Ctrl Pts',(-1.95294106986963,-0.00171292579279444,
1.52413030787577));
#272588=CARTESIAN_POINT('Ctrl Pts',(-1.95451933662198,-0.189295062189897,
1.53481387220307));
#272589=CARTESIAN_POINT('Ctrl Pts',(-1.84359709592533,-1.02560727269399,
1.58254936512225));
#272590=CARTESIAN_POINT('Ctrl Pts',(-0.650213426172095,-2.21623829060653,
1.66733678663321));
#272591=CARTESIAN_POINT('Ctrl Pts',(1.50962798548894,-1.74800320177882,
1.77849257240879));
#272592=CARTESIAN_POINT('Ctrl Pts',(2.28728253437157,0.320671512699175,
1.88964835818433));
#272593=CARTESIAN_POINT('Ctrl Pts',(0.970743942497957,2.09574505604618,
2.00080414395987));
#272594=CARTESIAN_POINT('Ctrl Pts',(-1.2345895468568,1.95199388459953,2.11195992973542));
#272595=CARTESIAN_POINT('Ctrl Pts',(-1.95450450452585,0.658811978361127,
2.18640198437405));
#272596=CARTESIAN_POINT('Ctrl Pts',(-1.9572031630521,0.00601498584378786,
2.22379211042084));
#272597=CARTESIAN_POINT('Ctrl Pts',(-1.95719833082201,0.000110330218013179,
2.22413030787577));
#272598=CARTESIAN_POINT('',(-1.95399930646857,0.00164630506337263,2.924130286497));
#272599=CARTESIAN_POINT('Ctrl Pts',(-1.95399999689534,0.000110149923111962,
2.22413030787577));
#272600=CARTESIAN_POINT('Ctrl Pts',(-1.9540038404061,-0.0680716498362349,
2.22804190863548));
#272601=CARTESIAN_POINT('Ctrl Pts',(-1.95043473464766,-0.136391042845262,
2.23195350939518));
#272602=CARTESIAN_POINT('Ctrl Pts',(-1.94327546182087,-0.204441873120198,
2.23586511015488));
#272603=CARTESIAN_POINT('Ctrl Pts',(-1.93577088073319,-0.275774952084673,
2.23996537645204));
#272604=CARTESIAN_POINT('Ctrl Pts',(-1.924320940806,-0.346812366580474,
2.24406564274919));
#272605=CARTESIAN_POINT('Ctrl Pts',(-1.9089674010183,-0.41708447807302,
2.24816590904634));
#272606=CARTESIAN_POINT('Ctrl Pts',(-1.89436009320224,-0.483941136384349,
2.25206688906518));
#272607=CARTESIAN_POINT('Ctrl Pts',(-1.87621991406215,-0.550104598981535,
2.25596786908402));
#272608=CARTESIAN_POINT('Ctrl Pts',(-1.85463575962332,-0.615176559311583,
2.25986884910286));
#272609=CARTESIAN_POINT('Ctrl Pts',(-1.83306463621632,-0.680209233655742,
2.26376747397756));
#272610=CARTESIAN_POINT('Ctrl Pts',(-1.80805381687011,-0.744151245189555,
2.26766609885226));
#272611=CARTESIAN_POINT('Ctrl Pts',(-1.7797423449315,-0.806618364319666,
2.27156472372696));
#272612=CARTESIAN_POINT('Ctrl Pts',(-1.75143816735893,-0.869069388983415,
2.27546234413263));
#272613=CARTESIAN_POINT('Ctrl Pts',(-1.71983522921158,-0.930045826120616,
2.27935996453829));
#272614=CARTESIAN_POINT('Ctrl Pts',(-1.68512041365749,-0.989184103933541,
2.28325758494396));
#272615=CARTESIAN_POINT('Ctrl Pts',(-1.65040252829768,-1.04832761130108,
2.28715555001334));
#272616=CARTESIAN_POINT('Ctrl Pts',(-1.61257247167267,-1.10563221234015,
2.29105351508273));
#272617=CARTESIAN_POINT('Ctrl Pts',(-1.57186177757689,-1.16076119516153,
2.29495148015211));
#272618=CARTESIAN_POINT('Ctrl Pts',(-1.53110703945126,-1.21594982085118,
2.29885366234659));
#272619=CARTESIAN_POINT('Ctrl Pts',(-1.48746573983048,-1.26895773441807,
2.30275584454108));
#272620=CARTESIAN_POINT('Ctrl Pts',(-1.44121059456054,-1.31948020906963,
2.30665802673556));
#272621=CARTESIAN_POINT('Ctrl Pts',(-1.3949262893077,-1.37003453389676,
2.31056266892807));
#272622=CARTESIAN_POINT('Ctrl Pts',(-1.34602521209539,-1.41809995660916,
2.31446731112058));
#272623=CARTESIAN_POINT('Ctrl Pts',(-1.29481591562462,-1.46340962981839,
2.31837195331309));
#272624=CARTESIAN_POINT('Ctrl Pts',(-1.2435199544286,-1.50879598344797,
2.32228320357808));
#272625=CARTESIAN_POINT('Ctrl Pts',(-1.18990836652197,-1.55141697652738,
2.32619445384307));
#272626=CARTESIAN_POINT('Ctrl Pts',(-1.13432082705043,-1.59104753584537,
2.33010570410807));
#272627=CARTESIAN_POINT('Ctrl Pts',(-1.11458575519372,-1.60511745049347,
2.33149430316755));
#272628=CARTESIAN_POINT('Ctrl Pts',(-1.09460186721579,-1.61881085322814,
2.33288290222703));
#272629=CARTESIAN_POINT('Ctrl Pts',(-1.07438510093941,-1.63211906884253,
2.33427150128652));
#272630=CARTESIAN_POINT('Ctrl Pts',(-1.01734369373402,-1.66966806830466,
2.33818941987519));
#272631=CARTESIAN_POINT('Ctrl Pts',(-0.958218234290233,-1.70429765930014,
2.34210733846386));
#272632=CARTESIAN_POINT('Ctrl Pts',(-0.897339749246061,-1.73576996587192,
2.34602525705253));
#272633=CARTESIAN_POINT('Ctrl Pts',(-0.836553011177559,-1.76719484207577,
2.34993727113846));
#272634=CARTESIAN_POINT('Ctrl Pts',(-0.774018924193188,-1.79547165303807,
2.3538492852244));
#272635=CARTESIAN_POINT('Ctrl Pts',(-0.710096901862582,-1.82040610578111,
2.35776129931034));
#272636=CARTESIAN_POINT('Ctrl Pts',(-0.64625013137306,-1.84531120457998,
2.3616687079997));
#272637=CARTESIAN_POINT('Ctrl Pts',(-0.581019126684705,-1.8668815817236,
2.36557611668907));
#272638=CARTESIAN_POINT('Ctrl Pts',(-0.51478562865045,-1.88496996170628,
2.36948352537844));
#272639=CARTESIAN_POINT('Ctrl Pts',(-0.448593699509874,-1.90304698921677,
2.37338848173385));
#272640=CARTESIAN_POINT('Ctrl Pts',(-0.381400998594416,-1.91764622525208,
2.37729343808926));
#272641=CARTESIAN_POINT('Ctrl Pts',(-0.313605385924358,-1.92866992041646,
2.38119839444467));
#272642=CARTESIAN_POINT('Ctrl Pts',(-0.245829062863987,-1.93969047905373,
2.38510223973874));
#272643=CARTESIAN_POINT('Ctrl Pts',(-0.177450653924596,-1.94713743746912,
2.38900608503281));
#272644=CARTESIAN_POINT('Ctrl Pts',(-0.108877407863952,-1.95096430260957,
2.39290993032689));
#272645=CARTESIAN_POINT('Ctrl Pts',(-0.0403001469218326,-1.95479139180838,
2.39681400418643));
#272646=CARTESIAN_POINT('Ctrl Pts',(0.0284714824719405,-1.95499794207696,
2.40071807804598));
#272647=CARTESIAN_POINT('Ctrl Pts',(0.0970277471845426,-1.95158951018812,
2.40462215190552));
#272648=CARTESIAN_POINT('Ctrl Pts',(0.165657075602355,-1.94817744576965,
2.40853038652415));
#272649=CARTESIAN_POINT('Ctrl Pts',(0.234070088995972,-1.94114273490312,
2.41243862114279));
#272650=CARTESIAN_POINT('Ctrl Pts',(0.301860711858535,-1.9305429574698,
2.41634685576142));
#272651=CARTESIAN_POINT('Ctrl Pts',(0.369691881963554,-1.91993684004834,
2.42025742799151));
#272652=CARTESIAN_POINT('Ctrl Pts',(0.436899439237921,-1.90576151382809,
2.4241680002216));
#272653=CARTESIAN_POINT('Ctrl Pts',(0.503088834207008,-1.88812542615586,
2.42807857245169));
#272654=CARTESIAN_POINT('Ctrl Pts',(0.569392704334207,-1.87045883671025,
2.43199590805187));
#272655=CARTESIAN_POINT('Ctrl Pts',(0.634674429834119,-1.84931969125412,
2.43591324365206));
#272656=CARTESIAN_POINT('Ctrl Pts',(0.698556743561265,-1.82486560492138,
2.43983057925224));
#272657=CARTESIAN_POINT('Ctrl Pts',(0.728979687507331,-1.81321973215399,
2.44169614852218));
#272658=CARTESIAN_POINT('Ctrl Pts',(0.759085571541915,-1.80082272628931,
2.44356171779213));
#272659=CARTESIAN_POINT('Ctrl Pts',(0.788835631960881,-1.78769526087331,
2.44542728706207));
#272660=CARTESIAN_POINT('Ctrl Pts',(0.851314316603462,-1.76012601360684,
2.44934520562944));
#272661=CARTESIAN_POINT('Ctrl Pts',(0.912469980201015,-1.72922272457703,
2.4532631241968));
#272662=CARTESIAN_POINT('Ctrl Pts',(0.97192326330304,-1.69513455815471,
2.45718104276417));
#272663=CARTESIAN_POINT('Ctrl Pts',(1.03128694726609,-1.66109776434298,
2.46109305682783));
#272664=CARTESIAN_POINT('Ctrl Pts',(1.0889529191399,-1.623885861664,2.46500507089149));
#272665=CARTESIAN_POINT('Ctrl Pts',(1.14456304812394,-1.5836954975213,2.46891708495516));
#272666=CARTESIAN_POINT('Ctrl Pts',(1.20010771037732,-1.54355244727253,
2.47282449362092));
#272667=CARTESIAN_POINT('Ctrl Pts',(1.25360093951805,-1.50043818604334,
2.47673190228669));
#272668=CARTESIAN_POINT('Ctrl Pts',(1.30471200480384,-1.45459361490444,
2.48063931095245));
#272669=CARTESIAN_POINT('Ctrl Pts',(1.35579099219528,-1.40877781634738,
2.48454426728345));
#272670=CARTESIAN_POINT('Ctrl Pts',(1.40449041608053,-1.36023543478269,
2.48844922361445));
#272671=CARTESIAN_POINT('Ctrl Pts',(1.45051241974066,-1.30924776882686,
2.49235417994545));
#272672=CARTESIAN_POINT('Ctrl Pts',(1.49652132893811,-1.25827461019438,
2.49625802521433));
#272673=CARTESIAN_POINT('Ctrl Pts',(1.5398540007316,-1.20485791334639,2.50016187048321));
#272674=CARTESIAN_POINT('Ctrl Pts',(1.58025055554452,-1.14931465739424,
2.50406571575209));
#272675=CARTESIAN_POINT('Ctrl Pts',(1.62064947551981,-1.09376814946134,
2.50796978958571));
#272676=CARTESIAN_POINT('Ctrl Pts',(1.65811164993965,-1.03609523458316,
2.51187386341933));
#272677=CARTESIAN_POINT('Ctrl Pts',(1.69241958669902,-0.976643201254944,
2.51577793725294));
#272678=CARTESIAN_POINT('Ctrl Pts',(1.7267640870668,-0.91712780705251,2.51968617184469));
#272679=CARTESIAN_POINT('Ctrl Pts',(1.75794739462104,-0.855829937270136,
2.52359440643644));
#272680=CARTESIAN_POINT('Ctrl Pts',(1.7857977125298,-0.793122014524463,
2.52750264102819));
#272681=CARTESIAN_POINT('Ctrl Pts',(1.81366468839611,-0.730376584633669,
2.53141321323081));
#272682=CARTESIAN_POINT('Ctrl Pts',(1.83819453139249,-0.666219882852152,
2.53532378543343));
#272683=CARTESIAN_POINT('Ctrl Pts',(1.85926443526242,-0.601042227941037,
2.53923435763605));
#272684=CARTESIAN_POINT('Ctrl Pts',(1.88037077971888,-0.535751847694842,
2.54315169320815));
#272685=CARTESIAN_POINT('Ctrl Pts',(1.89800511549755,-0.469437465318987,
2.54706902878025));
#272686=CARTESIAN_POINT('Ctrl Pts',(1.91209531989201,-0.40250153744684,
2.55098636435235));
#272687=CARTESIAN_POINT('Ctrl Pts',(1.91880555827064,-0.370624353870048,
2.55285193384744));
#272688=CARTESIAN_POINT('Ctrl Pts',(1.92471274895798,-0.338606306352277,
2.55471750334253));
#272689=CARTESIAN_POINT('Ctrl Pts',(1.92981324471967,-0.306491175247436,
2.55658307283762));
#272690=CARTESIAN_POINT('Ctrl Pts',(1.94052489466023,-0.239045566376628,
2.56050099146844));
#272691=CARTESIAN_POINT('Ctrl Pts',(1.94771778341508,-0.170903868566048,
2.56441891009927));
#272692=CARTESIAN_POINT('Ctrl Pts',(1.95131155312682,-0.102465714430763,
2.56833682873009));
#272693=CARTESIAN_POINT('Ctrl Pts',(1.95489990684488,-0.0341307000734099,
2.57224884285834));
#272694=CARTESIAN_POINT('Ctrl Pts',(1.95489988071068,0.0344993966206616,
2.57616085698659));
#272695=CARTESIAN_POINT('Ctrl Pts',(1.95128252454568,0.103017034526457,
2.58007287111484));
#272696=CARTESIAN_POINT('Ctrl Pts',(1.9476694268928,0.171454010429994,2.58398027984654));
#272697=CARTESIAN_POINT('Ctrl Pts',(1.94044748240011,0.239778301551508,
2.58788768857825));
#272698=CARTESIAN_POINT('Ctrl Pts',(1.92963978130998,0.307581394733121,
2.59179509730996));
#272699=CARTESIAN_POINT('Ctrl Pts',(1.91883886325545,0.375341933925608,
2.5957000537077));
#272700=CARTESIAN_POINT('Ctrl Pts',(1.90445673004048,0.442581439342766,
2.59960501010544));
#272701=CARTESIAN_POINT('Ctrl Pts',(1.88656824028271,0.50889711608203,2.60350996650318));
#272702=CARTESIAN_POINT('Ctrl Pts',(1.86868484026439,0.575193924290699,
2.6074138118395));
#272703=CARTESIAN_POINT('Ctrl Pts',(1.8472971922513,0.640566950886118,2.61131765717583));
#272704=CARTESIAN_POINT('Ctrl Pts',(1.82253072672411,0.70462596471211,2.61522150251216));
#272705=CARTESIAN_POINT('Ctrl Pts',(1.79776281115086,0.768688729114502,
2.61912557641383));
#272706=CARTESIAN_POINT('Ctrl Pts',(1.76961586509378,0.831436870089212,
2.6230296503155));
#272707=CARTESIAN_POINT('Ctrl Pts',(1.73826376917769,0.892499338242987,
2.62693372421716));
#272708=CARTESIAN_POINT('Ctrl Pts',(1.70687825983113,0.953626883594127,
2.6308419588774));
#272709=CARTESIAN_POINT('Ctrl Pts',(1.67228100866933,1.01306473236957,2.63475019353765));
#272710=CARTESIAN_POINT('Ctrl Pts',(1.63469179150203,1.07046660237295,2.63865842819789));
#272711=CARTESIAN_POINT('Ctrl Pts',(1.59708009129986,1.12790280584593,2.64256900046935));
#272712=CARTESIAN_POINT('Ctrl Pts',(1.55647315440075,1.18330021014323,2.64647957274082));
#272713=CARTESIAN_POINT('Ctrl Pts',(1.51313235688074,1.23634399362011,2.65039014501229));
#272714=CARTESIAN_POINT('Ctrl Pts',(1.4697166010684,1.2894795167893,2.65430748065307));
#272715=CARTESIAN_POINT('Ctrl Pts',(1.42355787850931,1.34025293097346,2.65822481629384));
#272716=CARTESIAN_POINT('Ctrl Pts',(1.37495524514224,1.38838541977934,2.66214215193461));
#272717=CARTESIAN_POINT('Ctrl Pts',(1.3518090127958,1.41130775324426,2.66400772082746));
#272718=CARTESIAN_POINT('Ctrl Pts',(1.32810900083288,1.4336317093052,2.66587328972032));
#272719=CARTESIAN_POINT('Ctrl Pts',(1.3038900178082,1.4553304853057,2.66773885861317));
#272720=CARTESIAN_POINT('Ctrl Pts',(1.25302724643474,1.50090051942615,2.67165677721371));
#272721=CARTESIAN_POINT('Ctrl Pts',(1.19967168565047,1.54389136363152,2.67557469581425));
#272722=CARTESIAN_POINT('Ctrl Pts',(1.1441155533377,1.58401881321239,2.67949261441479));
#272723=CARTESIAN_POINT('Ctrl Pts',(1.08864314694684,1.62408578868229,2.68340462851239));
#272724=CARTESIAN_POINT('Ctrl Pts',(1.03097714640215,1.66129764807336,2.68731664260999));
#272725=CARTESIAN_POINT('Ctrl Pts',(0.97144428838517,1.69540909357117,2.69122865670758));
#272726=CARTESIAN_POINT('Ctrl Pts',(0.911981515095867,1.72948038155852,
2.69513606540823));
#272727=CARTESIAN_POINT('Ctrl Pts',(0.850656673890062,1.76045826106261,
2.69904347410888));
#272728=CARTESIAN_POINT('Ctrl Pts',(0.787825534997934,1.78814063384433,
2.70295088280953));
#272729=CARTESIAN_POINT('Ctrl Pts',(0.725033829644162,1.81580563285362,
2.70685583917597));
#272730=CARTESIAN_POINT('Ctrl Pts',(0.660738151075758,1.84017903006499,
2.71076079554242));
#272731=CARTESIAN_POINT('Ctrl Pts',(0.595317534095197,1.86110532576714,
2.71466575190886));
#272732=CARTESIAN_POINT('Ctrl Pts',(0.529915530980779,1.88202566739419,
2.71856959721371));
#272733=CARTESIAN_POINT('Ctrl Pts',(0.463389693183081,1.89950070472482,
2.72247344251856));
#272734=CARTESIAN_POINT('Ctrl Pts',(0.396135919437877,1.91342424290357,
2.72637728782341));
#272735=CARTESIAN_POINT('Ctrl Pts',(0.328878208069503,1.92734859628783,
2.73028136169345));
#272736=CARTESIAN_POINT('Ctrl Pts',(0.260892958381072,1.93772094046943,
2.73418543556349));
#272737=CARTESIAN_POINT('Ctrl Pts',(0.192586221880882,1.94448619103907,
2.73808950943354));
#272738=CARTESIAN_POINT('Ctrl Pts',(0.124206687618644,1.95125865166041,
2.74199774406217));
#272739=CARTESIAN_POINT('Ctrl Pts',(0.0555054732576298,1.95441629810444,
2.7459059786908));
#272740=CARTESIAN_POINT('Ctrl Pts',(-0.0131072953684214,1.95395603809506,
2.74981421331943));
#272741=CARTESIAN_POINT('Ctrl Pts',(-0.0817611029776405,1.95349550279285,
2.75372478555924));
#272742=CARTESIAN_POINT('Ctrl Pts',(-0.150325868425877,1.94941278361112,
2.75763535779905));
#272743=CARTESIAN_POINT('Ctrl Pts',(-0.218395344346425,1.94175680082955,
2.76154593003887));
#272744=CARTESIAN_POINT('Ctrl Pts',(-0.286582547032858,1.93408757695746,
2.76546326564826));
#272745=CARTESIAN_POINT('Ctrl Pts',(-0.354272265493934,1.9228328357604,
2.76938060125765));
#272746=CARTESIAN_POINT('Ctrl Pts',(-0.421068075163712,1.90809268015941,
2.77329793686704));
#272747=CARTESIAN_POINT('Ctrl Pts',(-0.452878523869282,1.90107291400978,
2.77516350604093));
#272748=CARTESIAN_POINT('Ctrl Pts',(-0.484486454340456,1.89326339210832,
2.77702907521482));
#272749=CARTESIAN_POINT('Ctrl Pts',(-0.515850472278009,1.88467882946951,
2.77889464438871));
#272750=CARTESIAN_POINT('Ctrl Pts',(-0.581718664664873,1.86665022023404,
2.78281256298898));
#272751=CARTESIAN_POINT('Ctrl Pts',(-0.646771323487212,1.84512860016864,
2.78673048158925));
#272752=CARTESIAN_POINT('Ctrl Pts',(-0.710611204335022,1.82020540496767,
2.79064840018953));
#272753=CARTESIAN_POINT('Ctrl Pts',(-0.774354875228049,1.79531977029237,
2.79456041428675));
#272754=CARTESIAN_POINT('Ctrl Pts',(-0.836888940942152,1.76704291187986,
2.79847242838397));
#272755=CARTESIAN_POINT('Ctrl Pts',(-0.897830131913202,1.73551636530133,
2.80238444248119));
#272756=CARTESIAN_POINT('Ctrl Pts',(-0.958699580202227,1.70402693317642,
2.80629185118132));
#272757=CARTESIAN_POINT('Ctrl Pts',(-1.01797944305589,1.6692956356774,2.81019925988145));
#272758=CARTESIAN_POINT('Ctrl Pts',(-1.07530700680656,1.63151182683814,
2.81410666858158));
#272759=CARTESIAN_POINT('Ctrl Pts',(-1.13259859112415,1.59375173154839,
2.81801162494743));
#272760=CARTESIAN_POINT('Ctrl Pts',(-1.18793989707555,1.55294319532719,
2.82191658131328));
#272761=CARTESIAN_POINT('Ctrl Pts',(-1.24099475083012,1.50932038627062,
2.82582153767913));
#272762=CARTESIAN_POINT('Ctrl Pts',(-1.29403450909828,1.46570998903831,
2.82972538298329));
#272763=CARTESIAN_POINT('Ctrl Pts',(-1.34478872681381,1.4192872208373,2.83362922828745));
#272764=CARTESIAN_POINT('Ctrl Pts',(-1.39295351444384,1.37032715312752,
2.8375330735916));
#272765=CARTESIAN_POINT('Ctrl Pts',(-1.44112112206026,1.3213642188687,2.84143714746088));
#272766=CARTESIAN_POINT('Ctrl Pts',(-1.48669865542713,1.26986404265072,
2.84534122133016));
#272767=CARTESIAN_POINT('Ctrl Pts',(-1.52941966529898,1.21613793929668,
2.84924529519944));
#272768=CARTESIAN_POINT('Ctrl Pts',(-1.57218620499653,1.16235457746187,
2.85315352982717));
#272769=CARTESIAN_POINT('Ctrl Pts',(-1.61208983884711,1.10634093992012,
2.8570617644549));
#272770=CARTESIAN_POINT('Ctrl Pts',(-1.64890559451535,1.04843995554156,
2.86096999908264));
#272771=CARTESIAN_POINT('Ctrl Pts',(-1.68574337059115,0.990504339162355,
2.86488057132147));
#272772=CARTESIAN_POINT('Ctrl Pts',(-1.71948935101782,0.930679557828923,
2.86879114356031));
#272773=CARTESIAN_POINT('Ctrl Pts',(-1.74996436960873,0.869333483250198,
2.87270171579914));
#272774=CARTESIAN_POINT('Ctrl Pts',(-1.78049209501533,0.807881310089891,
2.87661905140745));
#272775=CARTESIAN_POINT('Ctrl Pts',(-1.80773737248884,0.744903043680049,
2.88053638701575));
#272776=CARTESIAN_POINT('Ctrl Pts',(-1.8315693677346,0.680786053893797,
2.88445372262406));
#272777=CARTESIAN_POINT('Ctrl Pts',(-1.84291897886717,0.65025135071175,
2.88631929180412));
#272778=CARTESIAN_POINT('Ctrl Pts',(-1.85349519563914,0.619458599171217,
2.88818486098419));
#272779=CARTESIAN_POINT('Ctrl Pts',(-1.86328793786741,0.588450559178767,
2.89005043016426));
#272780=CARTESIAN_POINT('Ctrl Pts',(-1.88814446964756,0.509744072931565,
2.89478573091368));
#272781=CARTESIAN_POINT('Ctrl Pts',(-1.90803027275293,0.429397174052618,
2.8995210316631));
#272782=CARTESIAN_POINT('Ctrl Pts',(-1.92276472469617,0.347982490168748,
2.90425633241252));
#272783=CARTESIAN_POINT('Ctrl Pts',(-1.93730951742571,0.267615761443961,
2.90893068122289));
#272784=CARTESIAN_POINT('Ctrl Pts',(-1.94683466612875,0.186208584307251,
2.91360503003325));
#272785=CARTESIAN_POINT('Ctrl Pts',(-1.95121262866794,0.104332534363677,
2.91827937884362));
#272786=CARTESIAN_POINT('Ctrl Pts',(-1.95303926845357,0.0701709697138529,
2.92022968139475));
#272787=CARTESIAN_POINT('Ctrl Pts',(-1.95397042305096,0.0359280303751402,
2.92217998394587));
#272788=CARTESIAN_POINT('Ctrl Pts',(-1.95399930646857,0.00164630506337263,
2.924130286497));
#272789=CARTESIAN_POINT('',(-1.95135389229221,-0.00104612722430151,3.62413030787577));
#272790=CARTESIAN_POINT('Ctrl Pts',(-1.95261817115182,0.00164476589090098,
2.92413030787577));
#272791=CARTESIAN_POINT('Ctrl Pts',(-1.94901781276173,-0.449643694625046,
2.94982227723045));
#272792=CARTESIAN_POINT('Ctrl Pts',(-1.56887368220728,-1.55723649878973,
3.01256617517698));
#272793=CARTESIAN_POINT('Ctrl Pts',(0.273666914822965,-2.29338130550848,
3.11236200171536));
#272794=CARTESIAN_POINT('Ctrl Pts',(2.07538330807382,-1.01354601124164,
3.22351778749091));
#272795=CARTESIAN_POINT('Ctrl Pts',(1.97691764050528,1.19427301524132,3.33467357326646));
#272796=CARTESIAN_POINT('Ctrl Pts',(0.0684232320151593,2.3086380516957,
3.44582935904201));
#272797=CARTESIAN_POINT('Ctrl Pts',(-1.6425693175686,1.44115442383729,3.54231493724512));
#272798=CARTESIAN_POINT('Ctrl Pts',(-1.94944131033335,0.392737674719044,
3.60174858685637));
#272799=CARTESIAN_POINT('Ctrl Pts',(-1.95135389229221,-0.00104612722430151,
3.62413030787577));
#272800=CARTESIAN_POINT('',(-1.95399969426645,-0.00109307210263392,4.32413030787578));
#272801=CARTESIAN_POINT('Ctrl Pts',(-1.95135389229221,-0.00104612722430151,
3.62413030787577));
#272802=CARTESIAN_POINT('Ctrl Pts',(-1.95260750341136,-0.259153629688766,
3.63880051544822));
#272803=CARTESIAN_POINT('Ctrl Pts',(-1.7848815556947,-1.16758857717685,
3.6905226516125));
#272804=CARTESIAN_POINT('Ctrl Pts',(-0.409009355221126,-2.27314820012038,
3.77929671636865));
#272805=CARTESIAN_POINT('Ctrl Pts',(1.6882291036661,-1.57618967319729,3.8904525021442));
#272806=CARTESIAN_POINT('Ctrl Pts',(2.2397566354332,0.563898578107994,4.00160828791975));
#272807=CARTESIAN_POINT('Ctrl Pts',(0.740604968531764,2.18769185968862,
4.1127640736953));
#272808=CARTESIAN_POINT('Ctrl Pts',(-1.36516131740615,1.82092354038783,
4.22027108665239));
#272809=CARTESIAN_POINT('Ctrl Pts',(-1.95250978895003,0.582719763414392,
4.29072617101763));
#272810=CARTESIAN_POINT('Ctrl Pts',(-1.95643501159432,-0.00107728777549013,
4.32412932679103));
#272811=CARTESIAN_POINT('',(-1.95399923813581,0.00172550418305494,5.02413030787578));
#272812=CARTESIAN_POINT('Ctrl Pts',(-1.95399969426645,-0.00109307210263392,
4.32413030787578));
#272813=CARTESIAN_POINT('Ctrl Pts',(-1.95396406853087,-0.0647784193523055,
4.32777875366598));
#272814=CARTESIAN_POINT('Ctrl Pts',(-1.95081522176893,-0.128375053248821,
4.33142719945619));
#272815=CARTESIAN_POINT('Ctrl Pts',(-1.9445774776562,-0.191662289958832,
4.3350756452464));
#272816=CARTESIAN_POINT('Ctrl Pts',(-1.93787901614206,-0.259623897837666,
4.33899356385134));
#272817=CARTESIAN_POINT('Ctrl Pts',(-1.92760015463464,-0.327368813282832,
4.34291148245628));
#272818=CARTESIAN_POINT('Ctrl Pts',(-1.91376424398393,-0.394490073954503,
4.34682940106122));
#272819=CARTESIAN_POINT('Ctrl Pts',(-1.89994918475547,-0.461510179466701,
4.35074141516321));
#272820=CARTESIAN_POINT('Ctrl Pts',(-1.8825878138515,-0.527908017599158,
4.3546534292652));
#272821=CARTESIAN_POINT('Ctrl Pts',(-1.86175521833767,-0.593281979325559,
4.35856544336719));
#272822=CARTESIAN_POINT('Ctrl Pts',(-1.84094714788169,-0.658578979917066,
4.36247285207222));
#272823=CARTESIAN_POINT('Ctrl Pts',(-1.81667611725424,-0.722854031451185,
4.36638026077724));
#272824=CARTESIAN_POINT('Ctrl Pts',(-1.78906780717862,-0.785717749142202,
4.37028766948227));
#272825=CARTESIAN_POINT('Ctrl Pts',(-1.76147682439289,-0.848542012847915,
4.37419262585308));
#272826=CARTESIAN_POINT('Ctrl Pts',(-1.73055291435365,-0.909956250382317,
4.37809758222389));
#272827=CARTESIAN_POINT('Ctrl Pts',(-1.69647039580353,-0.969589705061996,
4.3820025385947));
#272828=CARTESIAN_POINT('Ctrl Pts',(-1.66239757461609,-1.02920619247335,
4.38590638390389));
#272829=CARTESIAN_POINT('Ctrl Pts',(-1.62516817297791,-1.08704247596307,
4.38981022921309));
#272830=CARTESIAN_POINT('Ctrl Pts',(-1.58500225835342,-1.14275274710436,
4.39371407452228));
#272831=CARTESIAN_POINT('Ctrl Pts',(-1.54483399206581,-1.19846628001104,
4.39761814839664));
#272832=CARTESIAN_POINT('Ctrl Pts',(-1.50172916122758,-1.25205315589847,
4.401522222271));
#272833=CARTESIAN_POINT('Ctrl Pts',(-1.45594985515803,-1.30319838062565,
4.40542629614536));
#272834=CARTESIAN_POINT('Ctrl Pts',(-1.41012175988938,-1.35439811326845,
4.40933453077824));
#272835=CARTESIAN_POINT('Ctrl Pts',(-1.36161382973086,-1.40315063430612,
4.41324276541112));
#272836=CARTESIAN_POINT('Ctrl Pts',(-1.31072629105317,-1.44917652131892,
4.41715100004399));
#272837=CARTESIAN_POINT('Ctrl Pts',(-1.25980831528837,-1.49522993754553,
4.42106157228802));
#272838=CARTESIAN_POINT('Ctrl Pts',(-1.20650828017215,-1.53855316369342,
4.42497214453205));
#272839=CARTESIAN_POINT('Ctrl Pts',(-1.15115870068675,-1.57890773822703,
4.42888271677608));
#272840=CARTESIAN_POINT('Ctrl Pts',(-1.09571339361134,-1.61933210635621,
4.43280005238958));
#272841=CARTESIAN_POINT('Ctrl Pts',(-1.0382118794749,-1.65677730721562,
4.43671738800309));
#272842=CARTESIAN_POINT('Ctrl Pts',(-0.97901401930995,-1.69104924528962,
4.4406347236166));
#272843=CARTESIAN_POINT('Ctrl Pts',(-0.950821974592702,-1.70737071380278,
4.44250029275171));
#272844=CARTESIAN_POINT('Ctrl Pts',(-0.922245533750066,-1.72297317790248,
4.44436586188682));
#272845=CARTESIAN_POINT('Ctrl Pts',(-0.893325153439702,-1.73783951221968,
4.44623143102194));
#272846=CARTESIAN_POINT('Ctrl Pts',(-0.832588891273433,-1.76906059468301,
4.45014934962686));
#272847=CARTESIAN_POINT('Ctrl Pts',(-0.770093377070202,-1.7971557769571,
4.45406726823179));
#272848=CARTESIAN_POINT('Ctrl Pts',(-0.706193219306302,-1.8219240206457,
4.45798518683672));
#272849=CARTESIAN_POINT('Ctrl Pts',(-0.6423893623357,-1.84665493732919,
4.4618972009387));
#272850=CARTESIAN_POINT('Ctrl Pts',(-0.577185518011613,-1.86806868977168,
4.46580921504068));
#272851=CARTESIAN_POINT('Ctrl Pts',(-0.510959848584841,-1.88601061320825,
4.46972122914266));
#272852=CARTESIAN_POINT('Ctrl Pts',(-0.444812142961179,-1.90393141461467,
4.47362863784767));
#272853=CARTESIAN_POINT('Ctrl Pts',(-0.377645473848739,-1.91838837618161,
4.47753604655269));
#272854=CARTESIAN_POINT('Ctrl Pts',(-0.309855164515936,-1.92927597222969,
4.4814434552577));
#272855=CARTESIAN_POINT('Ctrl Pts',(-0.242107401153447,-1.94015673509847,
4.4853484116285));
#272856=CARTESIAN_POINT('Ctrl Pts',(-0.173737258608705,-1.94747249838319,
4.4892533679993));
#272857=CARTESIAN_POINT('Ctrl Pts',(-0.105150779999663,-1.9511687045116,
4.49315832437011));
#272858=CARTESIAN_POINT('Ctrl Pts',(-0.0365838160270698,-1.95486385897326,
4.49706216967929));
#272859=CARTESIAN_POINT('Ctrl Pts',(0.032198870821327,-1.95494147424573,
4.50096601498848));
#272860=CARTESIAN_POINT('Ctrl Pts',(0.100787394650277,-1.95139895999757,
4.50486986029766));
#272861=CARTESIAN_POINT('Ctrl Pts',(0.169379934249911,-1.94785623833972,
4.50877393417202));
#272862=CARTESIAN_POINT('Ctrl Pts',(0.237777797108343,-1.94069299428809,
4.51267800804637));
#272863=CARTESIAN_POINT('Ctrl Pts',(0.305574204187586,-1.92995865389265,
4.51658208192072));
#272864=CARTESIAN_POINT('Ctrl Pts',(0.373442865145013,-1.91921287339652,
4.52049031655359));
#272865=CARTESIAN_POINT('Ctrl Pts',(0.440708304253144,-1.90488847821343,
4.52439855118647));
#272866=CARTESIAN_POINT('Ctrl Pts',(0.50697295311195,-1.8870862261203,4.52830678581934));
#272867=CARTESIAN_POINT('Ctrl Pts',(0.573277236485244,-1.86927332606282,
4.53221735806336));
#272868=CARTESIAN_POINT('Ctrl Pts',(0.638579070522587,-1.8479785816739,
4.53612793030738));
#272869=CARTESIAN_POINT('Ctrl Pts',(0.702497796749431,-1.82335209039894,
4.5400385025514));
#272870=CARTESIAN_POINT('Ctrl Pts',(0.766527070981792,-1.79868300738829,
4.5439558381649));
#272871=CARTESIAN_POINT('Ctrl Pts',(0.829168014267321,-1.77067087752169,
4.5478731737784));
#272872=CARTESIAN_POINT('Ctrl Pts',(0.890062419102886,-1.73951283125498,
4.5517905093919));
#272873=CARTESIAN_POINT('Ctrl Pts',(0.919062416390822,-1.72467430446961,
4.5536560785271));
#272874=CARTESIAN_POINT('Ctrl Pts',(0.947666698135512,-1.70912294044003,
4.5555216476623));
#272875=CARTESIAN_POINT('Ctrl Pts',(0.97583893887946,-1.69288344707089,
4.55738721679749));
#272876=CARTESIAN_POINT('Ctrl Pts',(1.03500401835615,-1.65877856615003,
4.56130513540242));
#272877=CARTESIAN_POINT('Ctrl Pts',(1.09249646371974,-1.6215005929131,4.56522305400735));
#272878=CARTESIAN_POINT('Ctrl Pts',(1.14795508174258,-1.58123847989523,
4.56914097261228));
#272879=CARTESIAN_POINT('Ctrl Pts',(1.2033301208026,-1.54103704393293,4.57305298671426));
#272880=CARTESIAN_POINT('Ctrl Pts',(1.25667702071132,-1.49786068027829,
4.57696500081624));
#272881=CARTESIAN_POINT('Ctrl Pts',(1.30766078230223,-1.45194327658787,
4.58087701491822));
#272882=CARTESIAN_POINT('Ctrl Pts',(1.35858452354176,-1.40607992890701,
4.58478442362324));
#272883=CARTESIAN_POINT('Ctrl Pts',(1.40715028771411,-1.35748227744352,
4.58869183232825));
#272884=CARTESIAN_POINT('Ctrl Pts',(1.45305505958132,-1.30642527295867,
4.59259924103327));
#272885=CARTESIAN_POINT('Ctrl Pts',(1.49893102109081,-1.25540031243141,
4.59650419740407));
#272886=CARTESIAN_POINT('Ctrl Pts',(1.54214897499646,-1.20191942571252,
4.60040915377487));
#272887=CARTESIAN_POINT('Ctrl Pts',(1.58244291927386,-1.14629420623156,
4.60431411014568));
#272888=CARTESIAN_POINT('Ctrl Pts',(1.62272539887643,-1.09068481357184,
4.60821795545486));
#272889=CARTESIAN_POINT('Ctrl Pts',(1.66008523195781,-1.03293269753834,
4.61212180076404));
#272890=CARTESIAN_POINT('Ctrl Pts',(1.69429799803567,-0.973380857553883,
4.61602564607323));
#272891=CARTESIAN_POINT('Ctrl Pts',(1.72851276722741,-0.913825530885028,
4.61992971994758));
#272892=CARTESIAN_POINT('Ctrl Pts',(1.75957986076182,-0.852470698897036,
4.62383379382194));
#272893=CARTESIAN_POINT('Ctrl Pts',(1.78732024914569,-0.789684954265806,
4.62773786769629));
#272894=CARTESIAN_POINT('Ctrl Pts',(1.81509020179009,-0.726832295859382,
4.63164610232916));
#272895=CARTESIAN_POINT('Ctrl Pts',(1.83952617446589,-0.662546132222402,
4.63555433696203));
#272896=CARTESIAN_POINT('Ctrl Pts',(1.86049726291968,-0.597215149396232,
4.6394625715949));
#272897=CARTESIAN_POINT('Ctrl Pts',(1.88148089469671,-0.531845090504163,
4.64337314383893));
#272898=CARTESIAN_POINT('Ctrl Pts',(1.89899539227486,-0.465429444442277,
4.64728371608295));
#272899=CARTESIAN_POINT('Ctrl Pts',(1.91296047745239,-0.398369441229001,
4.65119428832697));
#272900=CARTESIAN_POINT('Ctrl Pts',(1.92694971536895,-0.33119345714373,
4.65511162394047));
#272901=CARTESIAN_POINT('Ctrl Pts',(1.93737721412613,-0.263371377663411,
4.65902895955397));
#272902=CARTESIAN_POINT('Ctrl Pts',(1.94421438782664,-0.195311070264557,
4.66294629516747));
#272903=CARTESIAN_POINT('Ctrl Pts',(1.94747048367496,-0.162898425206187,
4.66481186430266));
#272904=CARTESIAN_POINT('Ctrl Pts',(1.94991306204641,-0.130431770493967,
4.66667743343785));
#272905=CARTESIAN_POINT('Ctrl Pts',(1.95154318759175,-0.0979550252118336,
4.66854300257304));
#272906=CARTESIAN_POINT('Ctrl Pts',(1.95496664646119,-0.0297499706961675,
4.67246092117797));
#272907=CARTESIAN_POINT('Ctrl Pts',(1.95481701751349,0.038770144406793,
4.6763788397829));
#272908=CARTESIAN_POINT('Ctrl Pts',(1.95105722451954,0.107199378030411,
4.68029675838782));
#272909=CARTESIAN_POINT('Ctrl Pts',(1.94730309772518,0.175525485312703,
4.68420877248981));
#272910=CARTESIAN_POINT('Ctrl Pts',(1.93994963147098,0.243760495698615,
4.6881207865918));
#272911=CARTESIAN_POINT('Ctrl Pts',(1.92901170863315,0.311496112265012,
4.69203280069378));
#272912=CARTESIAN_POINT('Ctrl Pts',(1.91808666240449,0.37915198745137,4.6959402093988));
#272913=CARTESIAN_POINT('Ctrl Pts',(1.90358561816303,0.44630915306549,4.69984761810382));
#272914=CARTESIAN_POINT('Ctrl Pts',(1.88557530377411,0.51256392166944,4.70375502680883));
#272915=CARTESIAN_POINT('Ctrl Pts',(1.86757629286366,0.578777108025924,
4.70765998317964));
#272916=CARTESIAN_POINT('Ctrl Pts',(1.84607250950989,0.644088547188653,
4.71156493955044));
#272917=CARTESIAN_POINT('Ctrl Pts',(1.82118153925018,0.708105783830585,
4.71546989592125));
#272918=CARTESIAN_POINT('Ctrl Pts',(1.7962976511187,0.772104805904206,4.71937374123044));
#272919=CARTESIAN_POINT('Ctrl Pts',(1.7680286674486,0.834809898173339,4.72327758653962));
#272920=CARTESIAN_POINT('Ctrl Pts',(1.7365411083581,0.895846515304052,4.72718143184881));
#272921=CARTESIAN_POINT('Ctrl Pts',(1.70505170571113,0.956886706050949,
4.73108550572317));
#272922=CARTESIAN_POINT('Ctrl Pts',(1.67034358132991,1.01625779169783,4.73498957959752));
#272923=CARTESIAN_POINT('Ctrl Pts',(1.63262937131469,1.07360948948889,4.73889365347188));
#272924=CARTESIAN_POINT('Ctrl Pts',(1.59487496745953,1.13102230973116,4.74280188810475));
#272925=CARTESIAN_POINT('Ctrl Pts',(1.55410835509141,1.18641103522474,4.74671012273762));
#272926=CARTESIAN_POINT('Ctrl Pts',(1.51058514758464,1.23945492531866,4.7506183573705));
#272927=CARTESIAN_POINT('Ctrl Pts',(1.46703590777817,1.29253054226644,4.75452892961452));
#272928=CARTESIAN_POINT('Ctrl Pts',(1.42072712316509,1.34325816920577,4.75843950185855));
#272929=CARTESIAN_POINT('Ctrl Pts',(1.37195239703345,1.39135280223032,4.76235007410257));
#272930=CARTESIAN_POINT('Ctrl Pts',(1.32309331457916,1.43953061535045,4.76626740971607));
#272931=CARTESIAN_POINT('Ctrl Pts',(1.27176014637439,1.48506601956992,4.77018474532957));
#272932=CARTESIAN_POINT('Ctrl Pts',(1.21828010083953,1.52771384620891,4.77410208094308));
#272933=CARTESIAN_POINT('Ctrl Pts',(1.19281107491446,1.5480241991911,4.77596765007825));
#272934=CARTESIAN_POINT('Ctrl Pts',(1.16685557093406,1.56768028400996,4.77783321921342));
#272935=CARTESIAN_POINT('Ctrl Pts',(1.14045106888306,1.58665918189241,4.77969878834859));
#272936=CARTESIAN_POINT('Ctrl Pts',(1.08499845236565,1.6265171403635,4.78361670695352));
#272937=CARTESIAN_POINT('Ctrl Pts',(1.02734374656688,1.66354366412415,4.78753462555845));
#272938=CARTESIAN_POINT('Ctrl Pts',(0.967807938556677,1.69748749452439,
4.79145254416337));
#272939=CARTESIAN_POINT('Ctrl Pts',(0.908361854042292,1.73138016984289,
4.79536455826536));
#272940=CARTESIAN_POINT('Ctrl Pts',(0.847040717511409,1.76219913028732,
4.79927657236734));
#272941=CARTESIAN_POINT('Ctrl Pts',(0.78419566740042,1.78973549867862,4.80318858646933));
#272942=CARTESIAN_POINT('Ctrl Pts',(0.721424601277155,1.8172394500325,4.80709599517434));
#272943=CARTESIAN_POINT('Ctrl Pts',(0.657133632955883,1.84146828759698,
4.81100340387936));
#272944=CARTESIAN_POINT('Ctrl Pts',(0.591698138622352,1.86225919590986,
4.81491081258438));
#272945=CARTESIAN_POINT('Ctrl Pts',(0.526303712350415,1.88303705561187,
4.81881576895518));
#272946=CARTESIAN_POINT('Ctrl Pts',(0.459766652759582,1.9003811175651,4.82272072532598));
#272947=CARTESIAN_POINT('Ctrl Pts',(0.392480473834731,1.91417738928723,
4.82662568169679));
#272948=CARTESIAN_POINT('Ctrl Pts',(0.325213439577279,1.92796973561133,
4.83052952700597));
#272949=CARTESIAN_POINT('Ctrl Pts',(0.257198190796686,1.93821619683129,
4.83443337231516));
#272950=CARTESIAN_POINT('Ctrl Pts',(0.188839725512325,1.94485360839021,
4.83833721762434));
#272951=CARTESIAN_POINT('Ctrl Pts',(0.120477257926878,1.95149140856113,
4.8422412914987));
#272952=CARTESIAN_POINT('Ctrl Pts',(0.0517720238259972,1.95451969456067,
4.84614536537306));
#272953=CARTESIAN_POINT('Ctrl Pts',(-0.0168663607248519,1.95392720587946,
4.85004943924741));
#272954=CARTESIAN_POINT('Ctrl Pts',(-0.0855778964895568,1.95333408575467,
4.85395767388028));
#272955=CARTESIAN_POINT('Ctrl Pts',(-0.154221947650849,1.94911249411899,
4.85786590851315));
#272956=CARTESIAN_POINT('Ctrl Pts',(-0.222390418021636,1.94130329984064,
4.86177414314602));
#272957=CARTESIAN_POINT('Ctrl Pts',(-0.290599661629359,1.93348943469133,
4.86568471539005));
#272958=CARTESIAN_POINT('Ctrl Pts',(-0.358332273144911,1.92208377800183,
4.86959528763407));
#272959=CARTESIAN_POINT('Ctrl Pts',(-0.425189585458391,1.90717849621312,
4.8735058598781));
#272960=CARTESIAN_POINT('Ctrl Pts',(-0.492162528088149,1.89224743560698,
4.8774231954916));
#272961=CARTESIAN_POINT('Ctrl Pts',(-0.558256676514778,1.87380480187081,
4.8813405311051));
#272962=CARTESIAN_POINT('Ctrl Pts',(-0.623088613897518,1.85199259696989,
4.8852578667186));
#272963=CARTESIAN_POINT('Ctrl Pts',(-0.653963798790631,1.84160487933519,
4.88712343585378));
#272964=CARTESIAN_POINT('Ctrl Pts',(-0.684553012127485,1.83045365138825,
4.88898900498896));
#272965=CARTESIAN_POINT('Ctrl Pts',(-0.714816674560956,1.81855797866596,
4.89085457412414));
#272966=CARTESIAN_POINT('Ctrl Pts',(-0.77837399005539,1.79357564132026,
4.89477249272907));
#272967=CARTESIAN_POINT('Ctrl Pts',(-0.840746204620179,1.76520778252149,
4.898690411334));
#272968=CARTESIAN_POINT('Ctrl Pts',(-0.901548157631753,1.73358787474728,
4.90260832993892));
#272969=CARTESIAN_POINT('Ctrl Pts',(-0.962258479002415,1.70201561978505,
4.90652034404091));
#272970=CARTESIAN_POINT('Ctrl Pts',(-1.0214028024615,1.66720126770328,4.91043235814289));
#272971=CARTESIAN_POINT('Ctrl Pts',(-1.07861522978388,1.62932660509742,
4.91434437224487));
#272972=CARTESIAN_POINT('Ctrl Pts',(-1.1357603040926,1.59149653022865,4.91825178094988));
#272973=CARTESIAN_POINT('Ctrl Pts',(-1.1909775908175,1.55061357015786,4.9221591896549));
#272974=CARTESIAN_POINT('Ctrl Pts',(-1.24392675285296,1.50690485218434,
4.92606659835991));
#272975=CARTESIAN_POINT('Ctrl Pts',(-1.29684268339119,1.4632235663001,4.92997155473072));
#272976=CARTESIAN_POINT('Ctrl Pts',(-1.34749293447195,1.41672035297581,
4.93387651110152));
#272977=CARTESIAN_POINT('Ctrl Pts',(-1.39556835769231,1.36766405195427,
4.93778146747232));
#272978=CARTESIAN_POINT('Ctrl Pts',(-1.44363010220478,1.31862170872587,
4.94168531278151));
#272979=CARTESIAN_POINT('Ctrl Pts',(-1.48911812903031,1.26702807103927,
4.94558915809069));
#272980=CARTESIAN_POINT('Ctrl Pts',(-1.53175977084458,1.21318918739913,
4.94949300339987));
#272981=CARTESIAN_POINT('Ctrl Pts',(-1.5744039092727,1.15934715156088,4.95339707727423));
#272982=CARTESIAN_POINT('Ctrl Pts',(-1.61420102839992,1.10325999600695,
4.95730115114859));
#272983=CARTESIAN_POINT('Ctrl Pts',(-1.65091956898821,1.04526579238574,
4.96120522502295));
#272984=CARTESIAN_POINT('Ctrl Pts',(-1.68767724228383,0.987209781564125,
4.96511345965582));
#272985=CARTESIAN_POINT('Ctrl Pts',(-1.72134952549778,0.927243082981232,
4.96902169428869));
#272986=CARTESIAN_POINT('Ctrl Pts',(-1.75174948485069,0.865730756254706,
4.97292992892156));
#272987=CARTESIAN_POINT('Ctrl Pts',(-1.78216762716618,0.804181637494288,
4.97684050116558));
#272988=CARTESIAN_POINT('Ctrl Pts',(-1.80930935590143,0.741085502680043,
4.98075107340961));
#272989=CARTESIAN_POINT('Ctrl Pts',(-1.83303595225885,0.676827302734235,
4.98466164565363));
#272990=CARTESIAN_POINT('Ctrl Pts',(-1.85680358397568,0.612457967660123,
4.98857898126713));
#272991=CARTESIAN_POINT('Ctrl Pts',(-1.87714414903812,0.546923025771801,
4.99249631688063));
#272992=CARTESIAN_POINT('Ctrl Pts',(-1.89396907145856,0.480621635341562,
4.99641365249413));
#272993=CARTESIAN_POINT('Ctrl Pts',(-1.90198167468339,0.449046646673181,
4.99827922162931));
#272994=CARTESIAN_POINT('Ctrl Pts',(-1.90919768693769,0.417297961276106,
5.0001447907645));
#272995=CARTESIAN_POINT('Ctrl Pts',(-1.91561166762039,0.38541917294892,
5.00201035989968));
#272996=CARTESIAN_POINT('Ctrl Pts',(-1.93495299057814,0.289288864636548,
5.00763597321668));
#272997=CARTESIAN_POINT('Ctrl Pts',(-1.94706313315768,0.191658470633638,
5.01326158653369));
#272998=CARTESIAN_POINT('Ctrl Pts',(-1.95176526863315,0.0934255647955626,
5.01888719985069));
#272999=CARTESIAN_POINT('Ctrl Pts',(-1.9532260755329,0.0629076634335931,
5.02063490252572));
#273000=CARTESIAN_POINT('Ctrl Pts',(-1.95397221085221,0.0323318000566485,
5.02238260520075));
#273001=CARTESIAN_POINT('Ctrl Pts',(-1.95399923813581,0.00172550418305494,
5.02413030787578));
#273002=CARTESIAN_POINT('',(-1.95079228797786,3.78500716371835E-5,5.72413030787577));
#273003=CARTESIAN_POINT('Ctrl Pts',(-1.9546671565405,0.0017197843226782,
5.02413066805192));
#273004=CARTESIAN_POINT('Ctrl Pts',(-1.94988360819336,-0.518201249319763,
5.05380916059302));
#273005=CARTESIAN_POINT('Ctrl Pts',(-1.46932115474053,-1.69501948412908,
5.12053958172598));
#273006=CARTESIAN_POINT('Ctrl Pts',(0.517818131704895,-2.25085667576551,
5.22432193145079));
#273007=CARTESIAN_POINT('Ctrl Pts',(2.17203334564338,-0.785342306114842,
5.33547771722633));
#273008=CARTESIAN_POINT('Ctrl Pts',(1.83757553579813,1.39921676040448,5.44663350300188));
#273009=CARTESIAN_POINT('Ctrl Pts',(-0.179331995427646,2.30267918472736,
5.55778928877743));
#273010=CARTESIAN_POINT('Ctrl Pts',(-1.72107917867584,1.30007497440903,
5.65028822373539));
#273011=CARTESIAN_POINT('Ctrl Pts',(-1.95084822744177,0.32391356113618,
5.70573523010151));
#273012=CARTESIAN_POINT('Ctrl Pts',(-1.95079228797786,3.78500716371835E-5,
5.72413030787577));
#273013=CARTESIAN_POINT('',(-1.95399922102775,-0.00174477016505668,6.42413030787577));
#273014=CARTESIAN_POINT('Ctrl Pts',(-1.95079228797786,3.78500716371835E-5,
5.72413030787577));
#273015=CARTESIAN_POINT('Ctrl Pts',(-1.95073555246167,-0.328446807559118,
5.74278715869335));
#273016=CARTESIAN_POINT('Ctrl Pts',(-1.71625531119408,-1.30936792044859,
5.7984959381028));
#273017=CARTESIAN_POINT('Ctrl Pts',(-0.163096070439655,-2.30388607881722,
5.89125664610408));
#273018=CARTESIAN_POINT('Ctrl Pts',(1.84739289128347,-1.38622902061525,
6.00241243187962));
#273019=CARTESIAN_POINT('Ctrl Pts',(2.16644354493716,0.800633348643864,
6.11356821765517));
#273020=CARTESIAN_POINT('Ctrl Pts',(0.501939091571552,2.25445082907413,
6.22472400343072));
#273021=CARTESIAN_POINT('Ctrl Pts',(-1.47623102002116,1.68605736602827,
6.32824460474009));
#273022=CARTESIAN_POINT('Ctrl Pts',(-1.94977076795257,0.513689648483756,
6.3947132774576));
#273023=CARTESIAN_POINT('Ctrl Pts',(-1.95452816085295,-0.00174022619192097,
6.42413002158326));
#273024=CARTESIAN_POINT('',(-1.95399973054014,0.00102618178129684,7.12413030787578));
#273025=CARTESIAN_POINT('Ctrl Pts',(-1.95399922102775,-0.00174477016505668,
6.42413030787577));
#273026=CARTESIAN_POINT('Ctrl Pts',(-1.95391274289347,-0.0985931748455416,
6.42965921107939));
#273027=CARTESIAN_POINT('Ctrl Pts',(-1.94662244500826,-0.195131146519569,
6.43518811428301));
#273028=CARTESIAN_POINT('Ctrl Pts',(-1.9322863978956,-0.290491439646095,
6.44071701748663));
#273029=CARTESIAN_POINT('Ctrl Pts',(-1.92682520998912,-0.326818083628763,
6.44282320331836));
#273030=CARTESIAN_POINT('Ctrl Pts',(-1.92034203116191,-0.362974145946528,
6.44492938915009));
#273031=CARTESIAN_POINT('Ctrl Pts',(-1.91284727552396,-0.398912647731989,
6.44703557498182));
#273032=CARTESIAN_POINT('Ctrl Pts',(-1.89890556054757,-0.46576530748182,
6.45095349358675));
#273033=CARTESIAN_POINT('Ctrl Pts',(-1.88142727460356,-0.532018896690245,
6.45487141219167));
#273034=CARTESIAN_POINT('Ctrl Pts',(-1.86047923850533,-0.597271297728789,
6.4587893307966));
#273035=CARTESIAN_POINT('Ctrl Pts',(-1.83956277216473,-0.662425360074588,
6.46270134489859));
#273036=CARTESIAN_POINT('Ctrl Pts',(-1.8151870826716,-0.726580764134181,
6.46661335900057));
#273037=CARTESIAN_POINT('Ctrl Pts',(-1.78746985563884,-0.789346258103795,
6.47052537310256));
#273038=CARTESIAN_POINT('Ctrl Pts',(-1.75978525855835,-0.852037861742691,
6.47443278180757));
#273039=CARTESIAN_POINT('Ctrl Pts',(-1.72876713429301,-0.913342357046629,
6.47834019051259));
#273040=CARTESIAN_POINT('Ctrl Pts',(-1.69458216108227,-0.972886066989219,
6.4822475992176));
#273041=CARTESIAN_POINT('Ctrl Pts',(-1.66041864275012,-1.03239240662118,
6.4861525555884));
#273042=CARTESIAN_POINT('Ctrl Pts',(-1.62309246250114,-1.09013972735596,
6.49005751195921));
#273043=CARTESIAN_POINT('Ctrl Pts',(-1.58281666067281,-1.14577808440229,
6.49396246833001));
#273044=CARTESIAN_POINT('Ctrl Pts',(-1.54255231835727,-1.20140061088944,
6.49786631363919));
#273045=CARTESIAN_POINT('Ctrl Pts',(-1.49934030881723,-1.25491496658702,
6.50177015894838));
#273046=CARTESIAN_POINT('Ctrl Pts',(-1.45343648464424,-1.3060009131333,
6.50567400425756));
#273047=CARTESIAN_POINT('Ctrl Pts',(-1.40752997286077,-1.35708985069672,
6.50957807813192));
#273048=CARTESIAN_POINT('Ctrl Pts',(-1.35893166425077,-1.40574973262428,
6.51348215200628));
#273049=CARTESIAN_POINT('Ctrl Pts',(-1.30793588972586,-1.45169545992505,
6.51738622588064));
#273050=CARTESIAN_POINT('Ctrl Pts',(-1.25688576656164,-1.49769015378796,
6.5212944605135));
#273051=CARTESIAN_POINT('Ctrl Pts',(-1.20343344445735,-1.54096459032305,
6.52520269514637));
#273052=CARTESIAN_POINT('Ctrl Pts',(-1.14790736046466,-1.58127312371743,
6.52911092977924));
#273053=CARTESIAN_POINT('Ctrl Pts',(-1.09234806495694,-1.62160576663594,
6.53302150202327));
#273054=CARTESIAN_POINT('Ctrl Pts',(-1.03471295185424,-1.65896870823414,
6.53693207426729));
#273055=CARTESIAN_POINT('Ctrl Pts',(-0.975358172148888,-1.69316048737926,
6.54084264651131));
#273056=CARTESIAN_POINT('Ctrl Pts',(-0.915900737824142,-1.72741140151051,
6.54475998212481));
#273057=CARTESIAN_POINT('Ctrl Pts',(-0.854718139270463,-1.7584799841879,
6.54867731773831));
#273058=CARTESIAN_POINT('Ctrl Pts',(-0.79218896246577,-1.78621181491653,
6.55259465335181));
#273059=CARTESIAN_POINT('Ctrl Pts',(-0.76241043088079,-1.79941866073574,
6.55446022248699));
#273060=CARTESIAN_POINT('Ctrl Pts',(-0.732326754472248,-1.81186945472834,
6.55632579162218));
#273061=CARTESIAN_POINT('Ctrl Pts',(-0.701979991915673,-1.82355150487999,
6.55819136075737));
#273062=CARTESIAN_POINT('Ctrl Pts',(-0.638248156210868,-1.84808520924376,
6.5621092793623));
#273063=CARTESIAN_POINT('Ctrl Pts',(-0.573102123664993,-1.86932251147531,
6.56602719796722));
#273064=CARTESIAN_POINT('Ctrl Pts',(-0.506916001839037,-1.88710152537682,
6.56994511657215));
#273065=CARTESIAN_POINT('Ctrl Pts',(-0.44082962587064,-1.9048537453986,
6.57385713067414));
#273066=CARTESIAN_POINT('Ctrl Pts',(-0.373706742743016,-1.91915789406084,
6.57776914477612));
#273067=CARTESIAN_POINT('Ctrl Pts',(-0.305939909450436,-1.92990071553058,
6.58168115887811));
#273068=CARTESIAN_POINT('Ctrl Pts',(-0.238252854287599,-1.94063089007316,
6.58558856758312));
#273069=CARTESIAN_POINT('Ctrl Pts',(-0.169923838093017,-1.94780798720893,
6.58949597628814));
#273070=CARTESIAN_POINT('Ctrl Pts',(-0.101357215031177,-1.95136944604581,
6.59340338499316));
#273071=CARTESIAN_POINT('Ctrl Pts',(-0.0328336251630234,-1.95492866967055,
6.59730834136396));
#273072=CARTESIAN_POINT('Ctrl Pts',(0.0359267855861521,-1.95487673091302,
6.60121329773476));
#273073=CARTESIAN_POINT('Ctrl Pts',(0.104514465942167,-1.95120289216904,
6.60511825410557));
#273074=CARTESIAN_POINT('Ctrl Pts',(0.173082631319818,-1.9475300987277,
6.60902209941475));
#273075=CARTESIAN_POINT('Ctrl Pts',(0.241477672862865,-1.9402374773509,
6.61292594472394));
#273076=CARTESIAN_POINT('Ctrl Pts',(0.309291786723594,-1.92936637025354,
6.61682979003312));
#273077=CARTESIAN_POINT('Ctrl Pts',(0.377109871014345,-1.91849462666671,
6.62073386390748));
#273078=CARTESIAN_POINT('Ctrl Pts',(0.444346474763577,-1.90404406179105,
6.62463793778184));
#273079=CARTESIAN_POINT('Ctrl Pts',(0.510602456442851,-1.88610740189273,
6.6285420116562));
#273080=CARTESIAN_POINT('Ctrl Pts',(0.576929050295117,-1.86815162603687,
6.63245024628907));
#273081=CARTESIAN_POINT('Ctrl Pts',(0.642272460613658,-1.84670246932343,
6.63635848092194));
#273082=CARTESIAN_POINT('Ctrl Pts',(0.706248203474354,-1.82190270736097,
6.64026671555481));
#273083=CARTESIAN_POINT('Ctrl Pts',(0.770262211798635,-1.7970881120516,
6.64417728779884));
#273084=CARTESIAN_POINT('Ctrl Pts',(0.83290647589306,-1.76891912479073,
6.64808786004286));
#273085=CARTESIAN_POINT('Ctrl Pts',(0.893818610961755,-1.73758576499072,
6.65199843228689));
#273086=CARTESIAN_POINT('Ctrl Pts',(0.954836094109801,-1.70619821386627,
6.65591576790039));
#273087=CARTESIAN_POINT('Ctrl Pts',(1.01411504441724,-1.67163561492152,
6.65983310351389));
#273088=CARTESIAN_POINT('Ctrl Pts',(1.07132043821504,-1.63413234429245,
6.66375043912739));
#273089=CARTESIAN_POINT('Ctrl Pts',(1.0985636023358,-1.61627200475131,6.66561600826256));
#273090=CARTESIAN_POINT('Ctrl Pts',(1.12533695126987,-1.59774533089602,
6.66748157739774));
#273091=CARTESIAN_POINT('Ctrl Pts',(1.15160701602777,-1.57858078052269,
6.66934714653291));
#273092=CARTESIAN_POINT('Ctrl Pts',(1.20677729812938,-1.53833292958698,
6.67326506513784));
#273093=CARTESIAN_POINT('Ctrl Pts',(1.25994459082221,-1.49510946894049,
6.67718298374277));
#273094=CARTESIAN_POINT('Ctrl Pts',(1.31077002566914,-1.44913696378477,
6.6811009023477));
#273095=CARTESIAN_POINT('Ctrl Pts',(1.36151886399635,-1.40323374153646,
6.68501291644968));
#273096=CARTESIAN_POINT('Ctrl Pts',(1.40993248696035,-1.35459002436953,
6.68892493055167));
#273097=CARTESIAN_POINT('Ctrl Pts',(1.45570288401229,-1.30347424733989,
6.69283694465366));
#273098=CARTESIAN_POINT('Ctrl Pts',(1.50141939811739,-1.25241864607612,
6.69674435335867));
#273099=CARTESIAN_POINT('Ctrl Pts',(1.54449853961188,-1.19889712941683,
6.70065176206369));
#273100=CARTESIAN_POINT('Ctrl Pts',(1.58466849750097,-1.14321553218456,
6.70455917076871));
#273101=CARTESIAN_POINT('Ctrl Pts',(1.62481324426692,-1.08756888135697,
6.70846412713951));
#273102=CARTESIAN_POINT('Ctrl Pts',(1.66205214211782,-1.02976523726008,
6.71236908351031));
#273103=CARTESIAN_POINT('Ctrl Pts',(1.69615410631377,-0.970142900625954,
6.71627403988112));
#273104=CARTESIAN_POINT('Ctrl Pts',(1.73024636761423,-0.910537528096824,
6.7201778851903));
#273105=CARTESIAN_POINT('Ctrl Pts',(1.76120322295931,-0.849114917102498,
6.72408173049949));
#273106=CARTESIAN_POINT('Ctrl Pts',(1.78883829480519,-0.786240138277388,
6.72798557580867));
#273107=CARTESIAN_POINT('Ctrl Pts',(1.81647498464935,-0.723361678214043,
6.73188964968303));
#273108=CARTESIAN_POINT('Ctrl Pts',(1.84078930926984,-0.659031332907956,
6.73579372355738));
#273109=CARTESIAN_POINT('Ctrl Pts',(1.8616427630243,-0.593634755450892,
6.73969779743174));
#273110=CARTESIAN_POINT('Ctrl Pts',(1.88251844130321,-0.528168481729042,
6.74360603206461));
#273111=CARTESIAN_POINT('Ctrl Pts',(1.8999257379916,-0.461634177661315,
6.74751426669748));
#273112=CARTESIAN_POINT('Ctrl Pts',(1.91377614856796,-0.394432317606417,
6.75142250133035));
#273113=CARTESIAN_POINT('Ctrl Pts',(1.92763484341517,-0.32719026246799,
6.75533307357438));
#273114=CARTESIAN_POINT('Ctrl Pts',(1.93793234435327,-0.259280343150828,
6.7592436458184));
#273115=CARTESIAN_POINT('Ctrl Pts',(1.94463182551026,-0.191110081399764,
6.76315421806243));
#273116=CARTESIAN_POINT('Ctrl Pts',(1.9513428934795,-0.122821918574689,
6.76707155367593));
#273117=CARTESIAN_POINT('Ctrl Pts',(1.95444349962448,-0.0542730058415149,
6.77098888928943));
#273118=CARTESIAN_POINT('Ctrl Pts',(1.95394892397752,0.0141280744304211,
6.77490622490293));
#273119=CARTESIAN_POINT('Ctrl Pts',(1.95371339014712,0.0467030071802761,
6.77677179403811));
#273120=CARTESIAN_POINT('Ctrl Pts',(1.9526632350996,0.0792444735219877,
6.77863736317329));
#273121=CARTESIAN_POINT('Ctrl Pts',(1.95080422311103,0.111708921273798,
6.78050293230847));
#273122=CARTESIAN_POINT('Ctrl Pts',(1.94690007529929,0.179888149503358,
6.7844208509134));
#273123=CARTESIAN_POINT('Ctrl Pts',(1.93940965139226,0.247997782538903,
6.78833876951833));
#273124=CARTESIAN_POINT('Ctrl Pts',(1.92833958366678,0.315630242631857,
6.79225668812326));
#273125=CARTESIAN_POINT('Ctrl Pts',(1.91728619909734,0.383160777161784,
6.79616870222524));
#273126=CARTESIAN_POINT('Ctrl Pts',(1.90266395606301,0.450215084383322,
6.80008071632723));
#273127=CARTESIAN_POINT('Ctrl Pts',(1.88453139914629,0.516388812457961,
6.80399273042921));
#273128=CARTESIAN_POINT('Ctrl Pts',(1.86642018868192,0.582484637877146,
6.80790013913423));
#273129=CARTESIAN_POINT('Ctrl Pts',(1.84480700089815,0.64770147075974,6.81180754783924));
#273130=CARTESIAN_POINT('Ctrl Pts',(1.81980143302252,0.711645097200267,
6.81571495654426));
#273131=CARTESIAN_POINT('Ctrl Pts',(1.79481155892613,0.77554859189247,6.81961991291506));
#273132=CARTESIAN_POINT('Ctrl Pts',(1.76643370692484,0.838180008129233,
6.82352486928586));
#273133=CARTESIAN_POINT('Ctrl Pts',(1.73482683566997,0.899161748652228,
6.82742982565667));
#273134=CARTESIAN_POINT('Ctrl Pts',(1.70322895739177,0.960126138284474,
6.83133367096585));
#273135=CARTESIAN_POINT('Ctrl Pts',(1.66840410996748,1.01944134743096,6.83523751627504));
#273136=CARTESIAN_POINT('Ctrl Pts',(1.63055798594328,1.07675282886863,6.83914136158422));
#273137=CARTESIAN_POINT('Ctrl Pts',(1.59270964607673,1.13406766582053,6.84304543545857));
#273138=CARTESIAN_POINT('Ctrl Pts',(1.55183995163655,1.18937813305157,6.84694950933293));
#273139=CARTESIAN_POINT('Ctrl Pts',(1.50819784603678,1.24235874738741,6.85085358320728));
#273140=CARTESIAN_POINT('Ctrl Pts',(1.4645092289548,1.29539582570149,6.85476181784015));
#273141=CARTESIAN_POINT('Ctrl Pts',(1.4180426174066,1.3460977152817,6.85867005247303));
#273142=CARTESIAN_POINT('Ctrl Pts',(1.36908651935444,1.39417290983649,6.8625782871059));
#273143=CARTESIAN_POINT('Ctrl Pts',(1.32010113945727,1.44227685934627,6.86648885934992));
#273144=CARTESIAN_POINT('Ctrl Pts',(1.26862367837227,1.48775066133684,6.87039943159394));
#273145=CARTESIAN_POINT('Ctrl Pts',(1.21497658622953,1.53034241100286,6.87431000383797));
#273146=CARTESIAN_POINT('Ctrl Pts',(1.1612367109638,1.57300782347873,6.87822733945147));
#273147=CARTESIAN_POINT('Ctrl Pts',(1.10532011607045,1.61278095022153,6.88214467506497));
#273148=CARTESIAN_POINT('Ctrl Pts',(1.04757839517192,1.64945309298841,6.88606201067847));
#273149=CARTESIAN_POINT('Ctrl Pts',(1.0200798137511,1.66691762102912,6.88792757981365));
#273150=CARTESIAN_POINT('Ctrl Pts',(0.99216765700178,1.68367952315546,6.88979314894883));
#273151=CARTESIAN_POINT('Ctrl Pts',(0.963881644802451,1.69972002836141,
6.89165871808401));
#273152=CARTESIAN_POINT('Ctrl Pts',(0.904477631643619,1.73340701030902,
6.89557663668894));
#273153=CARTESIAN_POINT('Ctrl Pts',(0.843187582883122,1.76404291221313,
6.89949455529386));
#273154=CARTESIAN_POINT('Ctrl Pts',(0.780357559123363,1.79141231432605,
6.90341247389879));
#273155=CARTESIAN_POINT('Ctrl Pts',(0.717622223410446,1.81874046935559,
6.90732448800077));
#273156=CARTESIAN_POINT('Ctrl Pts',(0.653351966055132,1.84281169964799,
6.91123650210276));
#273157=CARTESIAN_POINT('Ctrl Pts',(0.587918284448726,1.8634559535473,6.91514851620474));
#273158=CARTESIAN_POINT('Ctrl Pts',(0.522561634282116,1.88407590411287,
6.91905592490975));
#273159=CARTESIAN_POINT('Ctrl Pts',(0.456044746888122,1.90127674330248,
6.92296333361477));
#273160=CARTESIAN_POINT('Ctrl Pts',(0.388758282549127,1.91493681299135,
6.92687074231978));
#273161=CARTESIAN_POINT('Ctrl Pts',(0.321514047961584,1.92858830946488,
6.93077569869059));
#273162=CARTESIAN_POINT('Ctrl Pts',(0.25350167555272,1.93870334695118,6.9346806550614));
#273163=CARTESIAN_POINT('Ctrl Pts',(0.18512462780308,1.94521075263859,6.9385856114322));
#273164=CARTESIAN_POINT('Ctrl Pts',(0.116767035101388,1.95171630679988,
6.94248945674139));
#273165=CARTESIAN_POINT('Ctrl Pts',(0.0480454625343314,1.95461622026885,
6.94639330205057));
#273166=CARTESIAN_POINT('Ctrl Pts',(-0.0206306555021805,1.95389108602643,
6.95029714735975));
#273167=CARTESIAN_POINT('Ctrl Pts',(-0.0893107944379186,1.95316590932833,
6.95420122123411));
#273168=CARTESIAN_POINT('Ctrl Pts',(-0.157944981674803,1.94881527129698,
6.95810529510846));
#273169=CARTESIAN_POINT('Ctrl Pts',(-0.22612475266668,1.94087186496982,
6.96200936898282));
#273170=CARTESIAN_POINT('Ctrl Pts',(-0.294377186106019,1.93291999297408,
6.96591760361569));
#273171=CARTESIAN_POINT('Ctrl Pts',(-0.362173747218213,1.92136776820417,
6.96982583824856));
#273172=CARTESIAN_POINT('Ctrl Pts',(-0.429113068040347,1.90629955013293,
6.97373407288143));
#273173=CARTESIAN_POINT('Ctrl Pts',(-0.496092426914868,1.89122231939025,
6.97764464512546));
#273174=CARTESIAN_POINT('Ctrl Pts',(-0.562213051426074,1.8726250432057,
6.98155521736948));
#273175=CARTESIAN_POINT('Ctrl Pts',(-0.627088444737639,1.85064207303209,
6.9854657896135));
#273176=CARTESIAN_POINT('Ctrl Pts',(-0.69207604061893,1.82862108311606,
6.989383125227));
#273177=CARTESIAN_POINT('Ctrl Pts',(-0.75581365023548,1.80320289443677,
6.99330046084051));
#273178=CARTESIAN_POINT('Ctrl Pts',(-0.817935278905976,1.77456977307769,
6.99721779645401));
#273179=CARTESIAN_POINT('Ctrl Pts',(-0.84751972213716,1.76093370184922,
6.99908336558919));
#273180=CARTESIAN_POINT('Ctrl Pts',(-0.87673803298852,1.74656915631899,
7.00094893472438));
#273181=CARTESIAN_POINT('Ctrl Pts',(-0.9055529027555,1.73149933303801,7.00281450385956));
#273182=CARTESIAN_POINT('Ctrl Pts',(-0.966067580142368,1.69985089938206,
7.00673242246449));
#273183=CARTESIAN_POINT('Ctrl Pts',(-1.02504123378782,1.66496341253867,
7.01065034106942));
#273184=CARTESIAN_POINT('Ctrl Pts',(-1.08210522136569,1.62701084504471,
7.01456825967435));
#273185=CARTESIAN_POINT('Ctrl Pts',(-1.13908321060705,1.58911547400353,
7.01848027377633));
#273186=CARTESIAN_POINT('Ctrl Pts',(-1.19415683917951,1.54816446004565,
7.02239228787832));
#273187=CARTESIAN_POINT('Ctrl Pts',(-1.24698179293194,1.5043777478068,7.02630430198031));
#273188=CARTESIAN_POINT('Ctrl Pts',(-1.29974455879966,1.4606425832328,7.03021171068532));
#273189=CARTESIAN_POINT('Ctrl Pts',(-1.35026353034211,1.41407866273953,
7.03411911939034));
#273190=CARTESIAN_POINT('Ctrl Pts',(-1.39822466545501,1.36494827188184,
7.03802652809535));
#273191=CARTESIAN_POINT('Ctrl Pts',(-1.4461556996132,1.31584871581709,7.04193148446616));
#273192=CARTESIAN_POINT('Ctrl Pts',(-1.49153173891609,1.26418623580297,
7.04583644083696));
#273193=CARTESIAN_POINT('Ctrl Pts',(-1.53407421973957,1.21026124796692,
7.04974139720776));
#273194=CARTESIAN_POINT('Ctrl Pts',(-1.57660459612112,1.15635160319199,
7.05364524251695));
#273195=CARTESIAN_POINT('Ctrl Pts',(-1.61630270994416,1.10018111456041,
7.05754908782613));
#273196=CARTESIAN_POINT('Ctrl Pts',(-1.65293025542248,1.04208328396005,
7.06145293313532));
#273197=CARTESIAN_POINT('Ctrl Pts',(-1.68955994539699,0.983982051805635,
7.06535700700968));
#273198=CARTESIAN_POINT('Ctrl Pts',(-1.72311844991441,0.923953671155186,
7.06926108088404));
#273199=CARTESIAN_POINT('Ctrl Pts',(-1.75341176577964,0.862359078125545,
7.0731651547584));
#273200=CARTESIAN_POINT('Ctrl Pts',(-1.78373736668246,0.800698840788064,
7.07707338939127));
#273201=CARTESIAN_POINT('Ctrl Pts',(-1.81079061662371,0.737469502159592,
7.08098162402414));
#273202=CARTESIAN_POINT('Ctrl Pts',(-1.83442477262436,0.673054049525057,
7.08488985865701));
#273203=CARTESIAN_POINT('Ctrl Pts',(-1.85807306479435,0.608600068425758,
7.08880043090104));
#273204=CARTESIAN_POINT('Ctrl Pts',(-1.87829804813884,0.542959031597052,
7.09271100314506));
#273205=CARTESIAN_POINT('Ctrl Pts',(-1.89500304837502,0.476528537077671,
7.09662157538908));
#273206=CARTESIAN_POINT('Ctrl Pts',(-1.91173694005769,0.409983150427166,
7.10053891100258));
#273207=CARTESIAN_POINT('Ctrl Pts',(-1.92493860358043,0.342646063501762,
7.10445624661608));
#273208=CARTESIAN_POINT('Ctrl Pts',(-1.93456274107396,0.274923627301158,
7.10837358222958));
#273209=CARTESIAN_POINT('Ctrl Pts',(-1.93914608435421,0.242671888057907,
7.11023915136476));
#273210=CARTESIAN_POINT('Ctrl Pts',(-1.94291881149136,0.21033280354338,
7.11210472049994));
#273211=CARTESIAN_POINT('Ctrl Pts',(-1.94588018410544,0.177950299538276,
7.11397028963512));
#273212=CARTESIAN_POINT('Ctrl Pts',(-1.95125613063908,0.119164515767483,
7.117356962382));
#273213=CARTESIAN_POINT('Ctrl Pts',(-1.95396869021499,0.0601314865954855,
7.12074363512889));
#273214=CARTESIAN_POINT('Ctrl Pts',(-1.95399973054014,0.00102618178129684,
7.12413030787578));
#273215=CARTESIAN_POINT('',(-1.95143063279042,0.00110697429861677,7.82413030787578));
#273216=CARTESIAN_POINT('Ctrl Pts',(-1.95653239756848,0.00101057639789689,
7.12413127700382));
#273217=CARTESIAN_POINT('Ctrl Pts',(-1.95277222847162,-0.587284438719568,
7.1577962098061));
#273218=CARTESIAN_POINT('Ctrl Pts',(-1.35742546160988,-1.82964434792259,
7.22851307120022));
#273219=CARTESIAN_POINT('Ctrl Pts',(0.756007498599133,-2.18241702119978,
7.33628186118621));
#273220=CARTESIAN_POINT('Ctrl Pts',(2.24367588325968,-0.548096636770858,
7.44743764696176));
#273221=CARTESIAN_POINT('Ctrl Pts',(1.67707667939426,1.58805075605049,7.55859343273731));
#273222=CARTESIAN_POINT('Ctrl Pts',(-0.425022500941536,2.27020863932239,
7.66974921851285));
#273223=CARTESIAN_POINT('Ctrl Pts',(-1.78903345425891,1.15826657200137,
7.75826151022568));
#273224=CARTESIAN_POINT('Ctrl Pts',(-1.95273655968318,0.25458387806612,
7.80972187334665));
#273225=CARTESIAN_POINT('Ctrl Pts',(-1.95143063279042,0.00110697429861677,
7.82413030787578));
#273226=CARTESIAN_POINT('',(-1.95399933299106,-0.00161451865900695,8.52413033064835));
#273227=CARTESIAN_POINT('Ctrl Pts',(-1.95143063279042,0.00110697429861677,
7.82413030787578));
#273228=CARTESIAN_POINT('Ctrl Pts',(-1.94937831074373,-0.397243224947184,
7.8467738019385));
#273229=CARTESIAN_POINT('Ctrl Pts',(-1.63702841788431,-1.45037623606872,
7.90646922459306));
#273230=CARTESIAN_POINT('Ctrl Pts',(0.0846950054830772,-2.30809838360649,
8.00321657583951));
#273231=CARTESIAN_POINT('Ctrl Pts',(1.98528689602104,-1.18030815164845,
8.11437236161505));
#273232=CARTESIAN_POINT('Ctrl Pts',(2.06818731211289,1.02815010303738,8.2255281473906));
#273233=CARTESIAN_POINT('Ctrl Pts',(0.257494186475546,2.29525339261092,
8.33668393316614));
#273234=CARTESIAN_POINT('Ctrl Pts',(-1.574992175394,1.54810389090286,8.4362179866612));
#273235=CARTESIAN_POINT('Ctrl Pts',(-1.94901851619721,0.44514694611732,
8.49870011156441));
#273236=CARTESIAN_POINT('Ctrl Pts',(-1.9524979245119,-0.00161287803163724,
8.52413030787577));
#273237=CARTESIAN_POINT('',(-1.95430622668274,-0.000195118721719283,9.22413030787577));
#273238=CARTESIAN_POINT('Ctrl Pts',(-1.95399933299106,-0.00161451865900695,
8.52413033064835));
#273239=CARTESIAN_POINT('Ctrl Pts',(-1.9539320163729,-0.0830856284773361,
8.52876425028391));
#273240=CARTESIAN_POINT('Ctrl Pts',(-1.94876546240929,-0.164338261234181,
8.53339816991947));
#273241=CARTESIAN_POINT('Ctrl Pts',(-1.93860446546909,-0.244803444549495,
8.53803208955503));
#273242=CARTESIAN_POINT('Ctrl Pts',(-1.92831626862875,-0.326275926985445,
8.54272401866726));
#273243=CARTESIAN_POINT('Ctrl Pts',(-1.91290789145434,-0.406941059896342,
8.54741594777949));
#273244=CARTESIAN_POINT('Ctrl Pts',(-1.89253714684451,-0.486229521742185,
8.55210787689172));
#273245=CARTESIAN_POINT('Ctrl Pts',(-1.88256924209821,-0.525027309957497,
8.55440375283356));
#273246=CARTESIAN_POINT('Ctrl Pts',(-1.87141388570986,-0.563495796774266,
8.5566996287754));
#273247=CARTESIAN_POINT('Ctrl Pts',(-1.85909368766508,-0.601570162561162,
8.55899550471724));
#273248=CARTESIAN_POINT('Ctrl Pts',(-1.8380692358398,-0.666544172423249,
8.56291342332217));
#273249=CARTESIAN_POINT('Ctrl Pts',(-1.81359276004705,-0.730543630978053,
8.5668313419271));
#273250=CARTESIAN_POINT('Ctrl Pts',(-1.78577378172853,-0.79317589505164,
8.57074926053202));
#273251=CARTESIAN_POINT('Ctrl Pts',(-1.75799672802768,-0.855713769112257,
8.574661274634));
#273252=CARTESIAN_POINT('Ctrl Pts',(-1.72688736713501,-0.916888091937685,
8.57857328873598));
#273253=CARTESIAN_POINT('Ctrl Pts',(-1.69260462824858,-0.976322473587231,
8.58248530283796));
#273254=CARTESIAN_POINT('Ctrl Pts',(-1.65836224852688,-1.03568688643971,
8.58639271154298));
#273255=CARTESIAN_POINT('Ctrl Pts',(-1.62095415485611,-1.09331500201994,
8.59030012024799));
#273256=CARTESIAN_POINT('Ctrl Pts',(-1.58058610395774,-1.14885315335586,
8.594207528953));
#273257=CARTESIAN_POINT('Ctrl Pts',(-1.54024338850793,-1.20435644831538,
8.59811248532381));
#273258=CARTESIAN_POINT('Ctrl Pts',(-1.49694468948603,-1.25777198394912,
8.60201744169461));
#273259=CARTESIAN_POINT('Ctrl Pts',(-1.45093931600466,-1.30877465641413,
8.60592239806541));
#273260=CARTESIAN_POINT('Ctrl Pts',(-1.40494703224824,-1.35976281729269,
8.6098262433746));
#273261=CARTESIAN_POINT('Ctrl Pts',(-1.35624993218061,-1.40833911273824,
8.61373008868378));
#273262=CARTESIAN_POINT('Ctrl Pts',(-1.30513670778591,-1.45421256148809,
8.61763393399296));
#273263=CARTESIAN_POINT('Ctrl Pts',(-1.25402049077697,-1.50008869606999,
8.62153800786732));
#273264=CARTESIAN_POINT('Ctrl Pts',(-1.2004882364131,-1.54326134310115,
8.62544208174167));
#273265=CARTESIAN_POINT('Ctrl Pts',(-1.14486312844721,-1.58347858120091,
8.62934615561603));
#273266=CARTESIAN_POINT('Ctrl Pts',(-1.08917873813962,-1.62373868073751,
8.6332543902489));
#273267=CARTESIAN_POINT('Ctrl Pts',(-1.03139744233148,-1.66103679664842,
8.63716262488177));
#273268=CARTESIAN_POINT('Ctrl Pts',(-0.971872107326577,-1.6951638879473,
8.64107085951464));
#273269=CARTESIAN_POINT('Ctrl Pts',(-0.912311168756344,-1.72931139149794,
8.64498143175866));
#273270=CARTESIAN_POINT('Ctrl Pts',(-0.851004554076599,-1.76028387386122,
8.64889200400269));
#273271=CARTESIAN_POINT('Ctrl Pts',(-0.788327949779091,-1.78791919381081,
8.65280257624671));
#273272=CARTESIAN_POINT('Ctrl Pts',(-0.725542945737033,-1.81560230929203,
8.65671991186021));
#273273=CARTESIAN_POINT('Ctrl Pts',(-0.661383682812903,-1.83993656860672,
8.66063724747371));
#273274=CARTESIAN_POINT('Ctrl Pts',(-0.596243113116256,-1.86080900418647,
8.66455458308721));
#273275=CARTESIAN_POINT('Ctrl Pts',(-0.565220946964255,-1.87074917154403,
8.6664201522224));
#273276=CARTESIAN_POINT('Ctrl Pts',(-0.533976400546536,-1.87990494439288,
8.6682857213576));
#273277=CARTESIAN_POINT('Ctrl Pts',(-0.502552650317926,-1.88826821020173,
8.67015129049279));
#273278=CARTESIAN_POINT('Ctrl Pts',(-0.436559011521794,-1.90583206998708,
8.67406920909772));
#273279=CARTESIAN_POINT('Ctrl Pts',(-0.369512513301717,-1.9199669785106,
8.67798712770265));
#273280=CARTESIAN_POINT('Ctrl Pts',(-0.301802455051448,-1.93055206563431,
8.68190504630758));
#273281=CARTESIAN_POINT('Ctrl Pts',(-0.234194439308534,-1.94112120049246,
8.68581706040956));
#273282=CARTESIAN_POINT('Ctrl Pts',(-0.165925330327548,-1.94815105591516,
8.68972907451155));
#273283=CARTESIAN_POINT('Ctrl Pts',(-0.0973975601784948,-1.95157108896173,
8.69364108861354));
#273284=CARTESIAN_POINT('Ctrl Pts',(-0.0289504639679613,-1.95498709579331,
8.69754849731855));
#273285=CARTESIAN_POINT('Ctrl Pts',(0.0397541996598223,-1.95480169567058,
8.70145590602357));
#273286=CARTESIAN_POINT('Ctrl Pts',(0.108307701137618,-1.95099601277765,
8.70536331472858));
#273287=CARTESIAN_POINT('Ctrl Pts',(0.176818177657025,-1.94719271837466,
8.70926827109939));
#273288=CARTESIAN_POINT('Ctrl Pts',(0.245177190141463,-1.93977367556684,
8.71317322747019));
#273289=CARTESIAN_POINT('Ctrl Pts',(0.312976394490285,-1.92877209034449,
8.717078183841));
#273290=CARTESIAN_POINT('Ctrl Pts',(0.38075630820264,-1.91777363535919,
8.72098202915019));
#273291=CARTESIAN_POINT('Ctrl Pts',(0.447976244614836,-1.90319474023785,
8.72488587445937));
#273292=CARTESIAN_POINT('Ctrl Pts',(0.514235177137632,-1.88512020375207,
8.72878971976855));
#273293=CARTESIAN_POINT('Ctrl Pts',(0.58049798903657,-1.86704460902518,
8.73269379364291));
#273294=CARTESIAN_POINT('Ctrl Pts',(0.645799211414756,-1.845473098534,8.73659786751727));
#273295=CARTESIAN_POINT('Ctrl Pts',(0.709751935731432,-1.82054063116578,
8.74050194139163));
#273296=CARTESIAN_POINT('Ctrl Pts',(0.773772817529424,-1.79558159207294,
8.7444101760245));
#273297=CARTESIAN_POINT('Ctrl Pts',(0.836441873899648,-1.76725462666114,
8.74831841065737));
#273298=CARTESIAN_POINT('Ctrl Pts',(0.897392132113103,-1.73574288453719,
8.75222664529025));
#273299=CARTESIAN_POINT('Ctrl Pts',(0.958378846173423,-1.7042122944661,
8.75613721753427));
#273300=CARTESIAN_POINT('Ctrl Pts',(1.01764429153029,-1.66949338529711,
8.76004778977829));
#273301=CARTESIAN_POINT('Ctrl Pts',(1.0748485293495,-1.63181391063908,8.76395836202231));
#273302=CARTESIAN_POINT('Ctrl Pts',(1.1321517024068,-1.59406926899451,8.76787569763581));
#273303=CARTESIAN_POINT('Ctrl Pts',(1.18738615716273,-1.55335413417732,
8.77179303324932));
#273304=CARTESIAN_POINT('Ctrl Pts',(1.24024391104561,-1.50993742953617,
8.77571036886282));
#273305=CARTESIAN_POINT('Ctrl Pts',(1.26541658041269,-1.48926091056487,
8.77757593799799));
#273306=CARTESIAN_POINT('Ctrl Pts',(1.29005074412221,-1.46797223198639,
8.77944150713316));
#273307=CARTESIAN_POINT('Ctrl Pts',(1.31411617499479,-1.44610327384218,
8.78130707626834));
#273308=CARTESIAN_POINT('Ctrl Pts',(1.36465646190966,-1.40017584270702,
8.78522499487327));
#273309=CARTESIAN_POINT('Ctrl Pts',(1.4128864653487,-1.35150454386662,8.78914291347819));
#273310=CARTESIAN_POINT('Ctrl Pts',(1.45849354319493,-1.30035094665197,
8.79306083208312));
#273311=CARTESIAN_POINT('Ctrl Pts',(1.50403188885132,-1.24927444051444,
8.79697284618511));
#273312=CARTESIAN_POINT('Ctrl Pts',(1.54695482921322,-1.19572342466037,
8.80088486028709));
#273313=CARTESIAN_POINT('Ctrl Pts',(1.58698488859974,-1.1399977909435,8.80479687438908));
#273314=CARTESIAN_POINT('Ctrl Pts',(1.62696782282021,-1.08433775992078,
8.80870428309409));
#273315=CARTESIAN_POINT('Ctrl Pts',(1.66406435402609,-1.02650859297274,
8.81261169179911));
#273316=CARTESIAN_POINT('Ctrl Pts',(1.69803700493591,-0.966843487782949,
8.81651910050412));
#273317=CARTESIAN_POINT('Ctrl Pts',(1.73198833422303,-0.90721582909281,
8.82042405687493));
#273318=CARTESIAN_POINT('Ctrl Pts',(1.76281942949986,-0.845754944393178,
8.82432901324573));
#273319=CARTESIAN_POINT('Ctrl Pts',(1.79033678388323,-0.78282194672521,
8.82823396961654));
#273320=CARTESIAN_POINT('Ctrl Pts',(1.81784630886381,-0.719906855131373,
8.83213781492572));
#273321=CARTESIAN_POINT('Ctrl Pts',(1.84204376765398,-0.655520932583686,
8.83604166023491));
#273322=CARTESIAN_POINT('Ctrl Pts',(1.86278297148862,-0.590047117722006,
8.8399455055441));
#273323=CARTESIAN_POINT('Ctrl Pts',(1.88352338957723,-0.524569469451849,
8.84384957941845));
#273324=CARTESIAN_POINT('Ctrl Pts',(1.90080500461284,-0.458004272158418,
8.84775365329281));
#273325=CARTESIAN_POINT('Ctrl Pts',(1.91453142947546,-0.39074979916904,
8.85165772716716));
#273326=CARTESIAN_POINT('Ctrl Pts',(1.92827248324649,-0.323423649866621,
8.85556596180004));
#273327=CARTESIAN_POINT('Ctrl Pts',(1.93845068668766,-0.25540724176912,
8.85947419643291));
#273328=CARTESIAN_POINT('Ctrl Pts',(1.94502095399775,-0.187108226729025,
8.86338243106578));
#273329=CARTESIAN_POINT('Ctrl Pts',(1.95159515114614,-0.118768360370054,
8.86729300330981));
#273330=CARTESIAN_POINT('Ctrl Pts',(1.95455709614358,-0.0501460422143237,
8.87120357555382));
#273331=CARTESIAN_POINT('Ctrl Pts',(1.95391383943899,0.0183496062298952,
8.87511414779785));
#273332=CARTESIAN_POINT('Ctrl Pts',(1.95326947021621,0.0869637185073052,
8.87903148341135));
#273333=CARTESIAN_POINT('Ctrl Pts',(1.94900748521415,0.155450233086523,
8.88294881902485));
#273334=CARTESIAN_POINT('Ctrl Pts',(1.94118685446954,0.223404556879756,
8.88686615463835));
#273335=CARTESIAN_POINT('Ctrl Pts',(1.93746240275688,0.25576672892183,8.88873172377353));
#273336=CARTESIAN_POINT('Ctrl Pts',(1.93293160515096,0.288008343806086,
8.89059729290871));
#273337=CARTESIAN_POINT('Ctrl Pts',(1.92760485918677,0.320086717686857,
8.89246286204389));
#273338=CARTESIAN_POINT('Ctrl Pts',(1.91641805472947,0.387455144550988,
8.89638078064882));
#273339=CARTESIAN_POINT('Ctrl Pts',(1.90167307614851,0.454370121717464,
8.90029869925375));
#273340=CARTESIAN_POINT('Ctrl Pts',(1.88342018786656,0.520427128363525,
8.90421661785868));
#273341=CARTESIAN_POINT('Ctrl Pts',(1.86519480761717,0.586384583735182,
8.90812863196066));
#273342=CARTESIAN_POINT('Ctrl Pts',(1.84347213961137,0.651486164384399,
8.91204064606265));
#273343=CARTESIAN_POINT('Ctrl Pts',(1.81835371609044,0.71533611902384,8.91595266016463));
#273344=CARTESIAN_POINT('Ctrl Pts',(1.7932648630947,0.779110906657251,8.91986006886965));
#273345=CARTESIAN_POINT('Ctrl Pts',(1.76478837315675,0.841636538986938,
8.92376747757466));
#273346=CARTESIAN_POINT('Ctrl Pts',(1.73307545102905,0.902532814384301,
8.92767488627968));
#273347=CARTESIAN_POINT('Ctrl Pts',(1.70138243229252,0.963390870585568,
8.93157984265049));
#273348=CARTESIAN_POINT('Ctrl Pts',(1.66645723735186,1.02262116302438,8.93548479902129));
#273349=CARTESIAN_POINT('Ctrl Pts',(1.62849836781698,1.07986529994136,8.93938975539209));
#273350=CARTESIAN_POINT('Ctrl Pts',(1.59055029856743,1.137093149413,8.94329360070128));
#273351=CARTESIAN_POINT('Ctrl Pts',(1.54957053996758,1.19233555540075,8.94719744601046));
#273352=CARTESIAN_POINT('Ctrl Pts',(1.50580158876996,1.24526205083824,8.95110129131965));
#273353=CARTESIAN_POINT('Ctrl Pts',(1.46203007495597,1.29819164505466,8.95500536519401));
#273354=CARTESIAN_POINT('Ctrl Pts',(1.41546935980839,1.34880468205008,8.95890943906836));
#273355=CARTESIAN_POINT('Ctrl Pts',(1.3664018278686,1.39680422565131,8.96281351294272));
#273356=CARTESIAN_POINT('Ctrl Pts',(1.31728200230992,1.4448549246651,8.96672174757559));
#273357=CARTESIAN_POINT('Ctrl Pts',(1.26565038050763,1.4902862269339,8.97062998220846));
#273358=CARTESIAN_POINT('Ctrl Pts',(1.21182504330288,1.53283921675562,8.97453821684133));
#273359=CARTESIAN_POINT('Ctrl Pts',(1.15796751184157,1.57541765856599,8.97844878908536));
#273360=CARTESIAN_POINT('Ctrl Pts',(1.10191405515166,1.61511407730049,8.98235936132938));
#273361=CARTESIAN_POINT('Ctrl Pts',(1.04401225770631,1.65171256753679,8.9862699335734));
#273362=CARTESIAN_POINT('Ctrl Pts',(0.986010318587284,1.68837435518747,
8.9901872691869));
#273363=CARTESIAN_POINT('Ctrl Pts',(0.926154087418501,1.72192728033022,
8.9941046048004));
#273364=CARTESIAN_POINT('Ctrl Pts',(0.864815494984659,1.75220151798657,
8.9980219404139));
#273365=CARTESIAN_POINT('Ctrl Pts',(0.835603960377922,1.76661914489812,
8.99988750954908));
#273366=CARTESIAN_POINT('Ctrl Pts',(0.806056514829847,1.78029387776113,
9.00175307868426));
#273367=CARTESIAN_POINT('Ctrl Pts',(0.77621466080163,1.7932113094548,9.00361864781944));
#273368=CARTESIAN_POINT('Ctrl Pts',(0.713543193474069,1.82033946300654,
9.00753656642437));
#273369=CARTESIAN_POINT('Ctrl Pts',(0.649323458916591,1.8442320195025,9.0114544850293));
#273370=CARTESIAN_POINT('Ctrl Pts',(0.583922606928159,1.8647118783121,9.01537240363423));
#273371=CARTESIAN_POINT('Ctrl Pts',(0.518620317355696,1.88516087293106,
9.01928441773621));
#273372=CARTESIAN_POINT('Ctrl Pts',(0.452140908689718,1.90220723124397,
9.02319643183819));
#273373=CARTESIAN_POINT('Ctrl Pts',(0.384871960076454,1.91572168499156,
9.02710844594018));
#273374=CARTESIAN_POINT('Ctrl Pts',(0.317682203460918,1.92922022892322,
9.03101585464519));
#273375=CARTESIAN_POINT('Ctrl Pts',(0.249705232869922,1.93919502950697,
9.03492326335021));
#273376=CARTESIAN_POINT('Ctrl Pts',(0.181342494852364,1.94556698665472,
9.03883067205523));
#273377=CARTESIAN_POINT('Ctrl Pts',(0.113022662067911,1.95193494468958,
9.04273562842603));
#273378=CARTESIAN_POINT('Ctrl Pts',(0.044318030841683,1.95470449918397,
9.04664058479684));
#273379=CARTESIAN_POINT('Ctrl Pts',(-0.0243626330771243,1.95384811643831,
9.05054554116764));
#273380=CARTESIAN_POINT('Ctrl Pts',(-0.0930237555613264,1.95299197735582,
9.05444938647683));
#273381=CARTESIAN_POINT('Ctrl Pts',(-0.161660432605449,1.94851195519506,
9.05835323178601));
#273382=CARTESIAN_POINT('Ctrl Pts',(-0.22986350742114,1.94043262391562,
9.0622570770952));
#273383=CARTESIAN_POINT('Ctrl Pts',(-0.298070575440003,1.93235281960162,
9.06616115096955));
#273384=CARTESIAN_POINT('Ctrl Pts',(-0.36584350260625,1.92067334819781,
9.07006522484391));
#273385=CARTESIAN_POINT('Ctrl Pts',(-0.43277967871086,1.90547047988021,
9.07396929871827));
#273386=CARTESIAN_POINT('Ctrl Pts',(-0.499787191904258,1.89025140913771,
9.07787753335114));
#273387=CARTESIAN_POINT('Ctrl Pts',(-0.565955693689586,1.87150155667804,
9.08178576798401));
#273388=CARTESIAN_POINT('Ctrl Pts',(-0.630895165440094,1.84934780131384,
9.08569400261688));
#273389=CARTESIAN_POINT('Ctrl Pts',(-0.695873479084083,1.82718079524428,
9.0896045748609));
#273390=CARTESIAN_POINT('Ctrl Pts',(-0.75962084305028,1.80160601754062,
9.09351514710492));
#273391=CARTESIAN_POINT('Ctrl Pts',(-0.821767380670605,1.77279845782474,
9.09742571934895));
#273392=CARTESIAN_POINT('Ctrl Pts',(-0.884021401280499,1.74394107517811,
9.10134305496245));
#273393=CARTESIAN_POINT('Ctrl Pts',(-0.94466863516237,1.71183998146086,
9.10526039057595));
#273394=CARTESIAN_POINT('Ctrl Pts',(-1.00336472363941,1.67671560837132,
9.10917772618945));
#273395=CARTESIAN_POINT('Ctrl Pts',(-1.03131780752665,1.65998818116222,
9.11104329532463));
#273396=CARTESIAN_POINT('Ctrl Pts',(-1.05882881364094,1.64257570288164,
9.11290886445981));
#273397=CARTESIAN_POINT('Ctrl Pts',(-1.08586313347053,1.62450523402344,
9.11477443359499));
#273398=CARTESIAN_POINT('Ctrl Pts',(-1.14248049445749,1.5866606621978,9.11868145259301));
#273399=CARTESIAN_POINT('Ctrl Pts',(-1.19723251652673,1.5457754581117,9.12258847159102));
#273400=CARTESIAN_POINT('Ctrl Pts',(-1.24977243038037,1.50206020926631,
9.12649549058904));
#273401=CARTESIAN_POINT('Ctrl Pts',(-1.30447872619442,1.45654244649299,
9.13056360797599));
#273402=CARTESIAN_POINT('Ctrl Pts',(-1.35678601891319,1.40795638949954,
9.13463172536294));
#273403=CARTESIAN_POINT('Ctrl Pts',(-1.40633472210552,1.3565908187071,9.13869984274989));
#273404=CARTESIAN_POINT('Ctrl Pts',(-1.45379225699105,1.3073930958457,9.14259626809244));
#273405=CARTESIAN_POINT('Ctrl Pts',(-1.4987189765413,1.25564614837589,9.146492693435));
#273406=CARTESIAN_POINT('Ctrl Pts',(-1.5408332642137,1.20164422850217,9.15038911877756));
#273407=CARTESIAN_POINT('Ctrl Pts',(-1.58292212734437,1.14767490977501,
9.15428319183461));
#273408=CARTESIAN_POINT('Ctrl Pts',(-1.62220162238339,1.09145370826315,
9.15817726489165));
#273409=CARTESIAN_POINT('Ctrl Pts',(-1.65842965663595,1.0333087989514,9.1620713379487));
#273410=CARTESIAN_POINT('Ctrl Pts',(-1.69464843478071,0.975178745415278,
9.16596441608673));
#273411=CARTESIAN_POINT('Ctrl Pts',(-1.7278170382089,0.915126379811159,
9.16985749422477));
#273412=CARTESIAN_POINT('Ctrl Pts',(-1.75773710396939,0.853508215150441,
9.17375057236281));
#273413=CARTESIAN_POINT('Ctrl Pts',(-1.7876599434774,0.791884338161662,
9.17764401140967));
#273414=CARTESIAN_POINT('Ctrl Pts',(-1.81433343401215,0.728694820586261,
9.18153745045653));
#273415=CARTESIAN_POINT('Ctrl Pts',(-1.83760633974216,0.664318402680099,
9.1854308895034));
#273416=CARTESIAN_POINT('Ctrl Pts',(-1.86090435888048,0.599872517244304,
9.18932852989605));
#273417=CARTESIAN_POINT('Ctrl Pts',(-1.88079430434863,0.534237642789977,
9.1932261702887));
#273418=CARTESIAN_POINT('Ctrl Pts',(-1.89717441254307,0.467808987078976,
9.19712381068135));
#273419=CARTESIAN_POINT('Ctrl Pts',(-1.91356497607487,0.401337930304608,
9.20102393891748));
#273420=CARTESIAN_POINT('Ctrl Pts',(-1.92644115296945,0.33407257033215,
9.2049240671536));
#273421=CARTESIAN_POINT('Ctrl Pts',(-1.935752581741,0.266416858105946,9.20882419538972));
#273422=CARTESIAN_POINT('Ctrl Pts',(-1.94507957848799,0.198648030858228,
9.21273084433303));
#273423=CARTESIAN_POINT('Ctrl Pts',(-1.95082989748065,0.130488041793009,
9.21663749327635));
#273424=CARTESIAN_POINT('Ctrl Pts',(-1.95300519580194,0.0623434452900937,
9.22054414221966));
#273425=CARTESIAN_POINT('Ctrl Pts',(-1.95367081146085,0.0414920015784572,
9.2217395307717));
#273426=CARTESIAN_POINT('Ctrl Pts',(-1.95400207064188,0.0206419743383481,
9.22293491932373));
#273427=CARTESIAN_POINT('Ctrl Pts',(-1.95399999026116,-0.000195088146951379,
9.22413030787577));
#273428=CARTESIAN_POINT('',(-1.95399923014638,0.00173452798668402,9.92413030787578));
#273429=CARTESIAN_POINT('Ctrl Pts',(-1.95718185414804,-0.000195405825525797,
9.22413030787577));
#273430=CARTESIAN_POINT('Ctrl Pts',(-1.95719676559863,-0.0106706459447958,
9.22473027837403));
#273431=CARTESIAN_POINT('Ctrl Pts',(-1.9571199413354,-0.0211456613651047,
9.22533024887228));
#273432=CARTESIAN_POINT('Ctrl Pts',(-1.94650003891758,-0.678424664968078,
9.26298214796238));
#273433=CARTESIAN_POINT('Ctrl Pts',(-1.2207993775171,-1.9606479215337,9.33708600514608));
#273434=CARTESIAN_POINT('Ctrl Pts',(0.98549264484445,-2.08885031520166,
9.44824179092163));
#273435=CARTESIAN_POINT('Ctrl Pts',(2.28948607134397,-0.304540508771072,
9.55939757669718));
#273436=CARTESIAN_POINT('Ctrl Pts',(1.49726895966604,1.7586008798989,9.67055336247273));
#273437=CARTESIAN_POINT('Ctrl Pts',(-0.665819550192416,2.21160026201443,
9.78170914824828));
#273438=CARTESIAN_POINT('Ctrl Pts',(-1.84711996695996,1.01628998128808,
9.86623464117473));
#273439=CARTESIAN_POINT('Ctrl Pts',(-1.95463561301669,0.184694303118807,
9.91370820550933));
#273440=CARTESIAN_POINT('Ctrl Pts',(-1.95307033066634,0.00174189496380082,
9.92412984125209));
#273441=CARTESIAN_POINT('',(-1.95399983006808,-0.000814919564481316,10.6241303079163));
#273442=CARTESIAN_POINT('Ctrl Pts',(-1.95399923014638,0.00173452798668402,
9.92413030787578));
#273443=CARTESIAN_POINT('Ctrl Pts',(-1.95405962454448,-0.0663016226432694,
9.92800408460677));
#273444=CARTESIAN_POINT('Ctrl Pts',(-1.95056232198822,-0.134411719177273,
9.93187786133777));
#273445=CARTESIAN_POINT('Ctrl Pts',(-1.94351084834083,-0.202191944403128,
9.93575163806877));
#273446=CARTESIAN_POINT('Ctrl Pts',(-1.93646276771955,-0.269939555159191,
9.93962355081696));
#273447=CARTESIAN_POINT('Ctrl Pts',(-1.92586395926989,-0.33735711184642,
9.94349546356515));
#273448=CARTESIAN_POINT('Ctrl Pts',(-1.91176993307524,-0.40404420920177,
9.94736737631334));
#273449=CARTESIAN_POINT('Ctrl Pts',(-1.89767765412431,-0.470723039323177,
9.95123880905851));
#273450=CARTESIAN_POINT('Ctrl Pts',(-1.88009112231765,-0.536671100075149,
9.95511024180368));
#273451=CARTESIAN_POINT('Ctrl Pts',(-1.85911690417107,-0.601498409495291,
9.95898167454884));
#273452=CARTESIAN_POINT('Ctrl Pts',(-1.83812279022283,-0.666387213045117,
9.96285677967205));
#273453=CARTESIAN_POINT('Ctrl Pts',(-1.81373472523136,-0.730152663798364,
9.96673188479526));
#273454=CARTESIAN_POINT('Ctrl Pts',(-1.78610878838271,-0.792421223884144,
9.97060698991846));
#273455=CARTESIAN_POINT('Ctrl Pts',(-1.75847015739071,-0.854718396430472,
9.97448387565603));
#273456=CARTESIAN_POINT('Ctrl Pts',(-1.7275909193593,-0.915516861522571,
9.97836076139359));
#273457=CARTESIAN_POINT('Ctrl Pts',(-1.69367353785893,-0.974467006704897,
9.98223764713116));
#273458=CARTESIAN_POINT('Ctrl Pts',(-1.65969279940653,-1.03352726951292,
9.98612177480938));
#273459=CARTESIAN_POINT('Ctrl Pts',(-1.62266285436743,-1.09073189453974,
9.99000590248759));
#273460=CARTESIAN_POINT('Ctrl Pts',(-1.58282959514847,-1.1457602160671,
9.9938900301658));
#273461=CARTESIAN_POINT('Ctrl Pts',(-1.54819819099351,-1.19360234799779,
9.99726692671033));
#273462=CARTESIAN_POINT('Ctrl Pts',(-1.51144864042195,-1.23979981747353,
10.0006438232549));
#273463=CARTESIAN_POINT('Ctrl Pts',(-1.47276553818141,-1.28416419103837,
10.0040207197994));
#273464=CARTESIAN_POINT('Ctrl Pts',(-1.42788490770719,-1.33563630523962,
10.0079386384043));
#273465=CARTESIAN_POINT('Ctrl Pts',(-1.38021357834289,-1.38485492894223,
10.0118565570092));
#273466=CARTESIAN_POINT('Ctrl Pts',(-1.33000664865851,-1.43150211823949,
10.0157744756142));
#273467=CARTESIAN_POINT('Ctrl Pts',(-1.27987538337502,-1.47807900784599,
10.0196864897162));
#273468=CARTESIAN_POINT('Ctrl Pts',(-1.22721645911195,-1.52209182193203,
10.0235985038181));
#273469=CARTESIAN_POINT('Ctrl Pts',(-1.17232401053735,-1.56325698921119,
10.0275105179201));
#273470=CARTESIAN_POINT('Ctrl Pts',(-1.11749618379432,-1.60437369502478,
10.0314179266251));
#273471=CARTESIAN_POINT('Ctrl Pts',(-1.06044044645612,-1.64264911813421,
10.0353253353302));
#273472=CARTESIAN_POINT('Ctrl Pts',(-1.00148505280831,-1.67783899376595,
10.0392327440352));
#273473=CARTESIAN_POINT('Ctrl Pts',(-0.942566660237059,-1.71300678383093,
10.043137700406));
#273474=CARTESIAN_POINT('Ctrl Pts',(-0.881751397842195,-1.74509261627888,
10.0470426567768));
#273475=CARTESIAN_POINT('Ctrl Pts',(-0.819396331698406,-1.77389561462877,
10.0509476131476));
#273476=CARTESIAN_POINT('Ctrl Pts',(-0.757059007192297,-1.8026904177767,
10.0548514584568));
#273477=CARTESIAN_POINT('Ctrl Pts',(-0.69318319504812,-1.82820403486895,
10.058755303766));
#273478=CARTESIAN_POINT('Ctrl Pts',(-0.628148753351215,-1.85028244969878,
10.0626591490751));
#273479=CARTESIAN_POINT('Ctrl Pts',(-0.563110503970661,-1.87236215719165,
10.0665632229495));
#273480=CARTESIAN_POINT('Ctrl Pts',(-0.496913957008386,-1.89100610739543,
10.0704672968238));
#273481=CARTESIAN_POINT('Ctrl Pts',(-0.429955323980053,-1.90610976058075,
10.0743713706982));
#273482=CARTESIAN_POINT('Ctrl Pts',(-0.362925329929332,-1.9212295104527,
10.0782796053311));
#273483=CARTESIAN_POINT('Ctrl Pts',(-0.295132109727523,-1.93280132493636,
10.0821878399639));
#273484=CARTESIAN_POINT('Ctrl Pts',(-0.226982304187082,-1.94077176236309,
10.0860960745968));
#273485=CARTESIAN_POINT('Ctrl Pts',(-0.158791736573707,-1.94874696710425,
10.0900066468408));
#273486=CARTESIAN_POINT('Ctrl Pts',(-0.0902446501664814,-1.95311647649373,
10.0939172190848));
#273487=CARTESIAN_POINT('Ctrl Pts',(-0.0217502250042049,-1.95387894397587,
10.0978277913289));
#273488=CARTESIAN_POINT('Ctrl Pts',(0.0468626618756505,-1.9546427301523,
10.1017451269424));
#273489=CARTESIAN_POINT('Ctrl Pts',(0.115422214466668,-1.95178704391515,
10.1056624625559));
#273490=CARTESIAN_POINT('Ctrl Pts',(0.183522714763041,-1.94536254029063,
10.1095797981693));
#273491=CARTESIAN_POINT('Ctrl Pts',(0.215954501053342,-1.94230297203981,
10.1114453673045));
#273492=CARTESIAN_POINT('Ctrl Pts',(0.248282302472955,-1.93843475375679,
10.1133109364397));
#273493=CARTESIAN_POINT('Ctrl Pts',(0.280463230798123,-1.93376740487844,
10.1151765055749));
#273494=CARTESIAN_POINT('Ctrl Pts',(0.348047034276776,-1.92396541327105,
10.1190944241799));
#273495=CARTESIAN_POINT('Ctrl Pts',(0.415250500290206,-1.91059669162971,
10.1230123427848));
#273496=CARTESIAN_POINT('Ctrl Pts',(0.481668161728989,-1.89370319268269,
10.1269302613897));
#273497=CARTESIAN_POINT('Ctrl Pts',(0.547985728368301,-1.87683515309923,
10.1308422754917));
#273498=CARTESIAN_POINT('Ctrl Pts',(0.613519367818316,-1.85645299892549,
10.1347542895937));
#273499=CARTESIAN_POINT('Ctrl Pts',(0.677871328599324,-1.83265011987094,
10.1386663036957));
#273500=CARTESIAN_POINT('Ctrl Pts',(0.742147531390295,-1.80887526262416,
10.1425737124007));
#273501=CARTESIAN_POINT('Ctrl Pts',(0.805244359098048,-1.78168784806091,
10.1464811211057));
#273502=CARTESIAN_POINT('Ctrl Pts',(0.866778587305234,-1.75123124703425,
10.1503885298107));
#273503=CARTESIAN_POINT('Ctrl Pts',(0.928274195929873,-1.72079376091732,
10.1542934861815));
#273504=CARTESIAN_POINT('Ctrl Pts',(0.988208710551904,-1.68709137611959,
10.1581984425523));
#273505=CARTESIAN_POINT('Ctrl Pts',(1.046219741459,-1.650315197949,10.1621033989231));
#273506=CARTESIAN_POINT('Ctrl Pts',(1.10421426671942,-1.61354948355735,
10.1660072442323));
#273507=CARTESIAN_POINT('Ctrl Pts',(1.16028597941404,-1.57371197523036,
10.1699110895415));
#273508=CARTESIAN_POINT('Ctrl Pts',(1.21409950582571,-1.53103833719269,
10.1738149348507));
#273509=CARTESIAN_POINT('Ctrl Pts',(1.26791618295084,-1.48836220066785,
10.177719008725));
#273510=CARTESIAN_POINT('Ctrl Pts',(1.31947402743773,-1.44284991242812,
10.1816230825994));
#273511=CARTESIAN_POINT('Ctrl Pts',(1.36847037087042,-1.39477770417001,
10.1855271564737));
#273512=CARTESIAN_POINT('Ctrl Pts',(1.417518932053,-1.34665426305713,10.1894353911066));
#273513=CARTESIAN_POINT('Ctrl Pts',(1.46400019225624,-1.29596580238125,
10.1933436257395));
#273514=CARTESIAN_POINT('Ctrl Pts',(1.50764876301083,-1.24302502283418,
10.1972518603724));
#273515=CARTESIAN_POINT('Ctrl Pts',(1.55132344104799,-1.19005257810617,
10.2011624326164));
#273516=CARTESIAN_POINT('Ctrl Pts',(1.59216176513657,-1.13482552900091,
10.2050730048604));
#273517=CARTESIAN_POINT('Ctrl Pts',(1.62994074259063,-1.07768695623688,
10.2089835771044));
#273518=CARTESIAN_POINT('Ctrl Pts',(1.66778505912221,-1.02044956180305,
10.2129009127179));
#273519=CARTESIAN_POINT('Ctrl Pts',(1.70255921943757,-0.961294469294182,
10.2168182483314));
#273520=CARTESIAN_POINT('Ctrl Pts',(1.73408580198429,-0.900590046223309,
10.2207355839449));
#273521=CARTESIAN_POINT('Ctrl Pts',(1.74909983834462,-0.871680524746696,
10.2226011530801));
#273522=CARTESIAN_POINT('Ctrl Pts',(1.76337803026822,-0.842419918247882,
10.2244667222153));
#273523=CARTESIAN_POINT('Ctrl Pts',(1.77690512200243,-0.812849424802369,
10.2263322913505));
#273524=CARTESIAN_POINT('Ctrl Pts',(1.80531363465236,-0.750747847196636,
10.2302502099554));
#273525=CARTESIAN_POINT('Ctrl Pts',(1.83051900333678,-0.68703193119432,
10.2341681285603));
#273526=CARTESIAN_POINT('Ctrl Pts',(1.8523366304931,-0.62206511502693,10.2380860471652));
#273527=CARTESIAN_POINT('Ctrl Pts',(1.87412137737377,-0.557196207161326,
10.2419980612672));
#273528=CARTESIAN_POINT('Ctrl Pts',(1.8925283599387,-0.491080603094183,
10.2459100753692));
#273529=CARTESIAN_POINT('Ctrl Pts',(1.90742038369684,-0.424103147663155,
10.2498220894712));
#273530=CARTESIAN_POINT('Ctrl Pts',(1.92229487590236,-0.357204541071136,
10.2537294981762));
#273531=CARTESIAN_POINT('Ctrl Pts',(1.93366252106905,-0.289446576072365,
10.2576369068812));
#273532=CARTESIAN_POINT('Ctrl Pts',(1.94143599774202,-0.221228991480406,
10.2615443155862));
#273533=CARTESIAN_POINT('Ctrl Pts',(1.94920459569248,-0.153054221021664,
10.265449271957));
#273534=CARTESIAN_POINT('Ctrl Pts',(1.95338344422542,-0.0844208908608971,
10.2693542283278));
#273535=CARTESIAN_POINT('Ctrl Pts',(1.95393662721973,-0.0157371156567165,
10.2732591846986));
#273536=CARTESIAN_POINT('Ctrl Pts',(1.95448965281909,0.0529271172276451,
10.2771630300078));
#273537=CARTESIAN_POINT('Ctrl Pts',(1.95141905679734,0.121641274970306,
10.281066875317));
#273538=CARTESIAN_POINT('Ctrl Pts',(1.9447410116955,0.189995782662541,10.2849707206262));
#273539=CARTESIAN_POINT('Ctrl Pts',(1.93806257560263,0.258354292424093,
10.2888747945005));
#273540=CARTESIAN_POINT('Ctrl Pts',(1.92777632148089,0.326352620970326,
10.2927788683749));
#273541=CARTESIAN_POINT('Ctrl Pts',(1.91395024154316,0.393586677743139,
10.2966829422492));
#273542=CARTESIAN_POINT('Ctrl Pts',(1.90010942648983,0.460892389070508,
10.3005911768821));
#273543=CARTESIAN_POINT('Ctrl Pts',(1.88272135598796,0.527431720296417,
10.304499411515));
#273544=CARTESIAN_POINT('Ctrl Pts',(1.86190487862007,0.59281213126147,10.3084076461479));
#273545=CARTESIAN_POINT('Ctrl Pts',(1.84107595040562,0.658231647856704,
10.3123182183919));
#273546=CARTESIAN_POINT('Ctrl Pts',(1.81681470801753,0.722490404341941,
10.3162287906359));
#273547=CARTESIAN_POINT('Ctrl Pts',(1.78928851404671,0.785215011000507,
10.3201393628799));
#273548=CARTESIAN_POINT('Ctrl Pts',(1.76171471327864,0.848048100424074,
10.3240566984934));
#273549=CARTESIAN_POINT('Ctrl Pts',(1.73086491185874,0.909341305167467,
10.3279740341069));
#273550=CARTESIAN_POINT('Ctrl Pts',(1.69695242853623,0.96874581562193,10.3318913697204));
#273551=CARTESIAN_POINT('Ctrl Pts',(1.68080214466305,0.99703627427289,10.3337569388556));
#273552=CARTESIAN_POINT('Ctrl Pts',(1.66395788216242,1.02489880606965,10.3356225079908));
#273553=CARTESIAN_POINT('Ctrl Pts',(1.64644598563396,1.05229825448387,10.337488077126));
#273554=CARTESIAN_POINT('Ctrl Pts',(1.60966890569531,1.10984037751821,10.341405995731));
#273555=CARTESIAN_POINT('Ctrl Pts',(1.56979861387346,1.16556638933122,10.3453239143359));
#273556=CARTESIAN_POINT('Ctrl Pts',(1.52704039622133,1.21912412342149,10.3492418329408));
#273557=CARTESIAN_POINT('Ctrl Pts',(1.48434661738156,1.27260114327792,10.3531538470428));
#273558=CARTESIAN_POINT('Ctrl Pts',(1.43877385480222,1.32391598927017,10.3570658611448));
#273559=CARTESIAN_POINT('Ctrl Pts',(1.39057108368565,1.37274471815313,10.3609778752468));
#273560=CARTESIAN_POINT('Ctrl Pts',(1.34242505901485,1.421515963685,10.3648852839518));
#273561=CARTESIAN_POINT('Ctrl Pts',(1.29165551877425,1.4678065562625,10.3687926926568));
#273562=CARTESIAN_POINT('Ctrl Pts',(1.23855099435898,1.51132638247745,10.3727001013618));
#273563=CARTESIAN_POINT('Ctrl Pts',(1.18547979894815,1.55481889515374,10.3766050577326));
#273564=CARTESIAN_POINT('Ctrl Pts',(1.13007690599375,1.59554377988425,10.3805100141034));
#273565=CARTESIAN_POINT('Ctrl Pts',(1.07266575709322,1.63324957479242,10.3844149704742));
#273566=CARTESIAN_POINT('Ctrl Pts',(1.01527094315726,1.67094464142158,10.3883188157834));
#273567=CARTESIAN_POINT('Ctrl Pts',(0.955869418588534,1.70562205356739,
10.3922226610926));
#273568=CARTESIAN_POINT('Ctrl Pts',(0.894814094910756,1.73707332474742,
10.3961265064018));
#273569=CARTESIAN_POINT('Ctrl Pts',(0.833755196521393,1.76852643735938,
10.4000305802762));
#273570=CARTESIAN_POINT('Ctrl Pts',(0.771042745283283,1.79675281099617,
10.4039346541505));
#273571=CARTESIAN_POINT('Ctrl Pts',(0.707053141642332,1.82159047397973,
10.4078387280249));
#273572=CARTESIAN_POINT('Ctrl Pts',(0.642995341216151,1.84645460765028,
10.4117469626578));
#273573=CARTESIAN_POINT('Ctrl Pts',(0.577658131479498,1.86792264481257,
10.4156551972906));
#273574=CARTESIAN_POINT('Ctrl Pts',(0.511435782531989,1.88588160825273,
10.4195634319235));
#273575=CARTESIAN_POINT('Ctrl Pts',(0.445173824370667,1.90385131339012,
10.4234740041675));
#273576=CARTESIAN_POINT('Ctrl Pts',(0.378026154340807,1.91830766413244,
10.4273845764115));
#273577=CARTESIAN_POINT('Ctrl Pts',(0.310397256258584,1.92918883039145,
10.4312951486555));
#273578=CARTESIAN_POINT('Ctrl Pts',(0.242651393395549,1.9400888157243,10.435212484269));
#273579=CARTESIAN_POINT('Ctrl Pts',(0.174423130244239,1.94740122317494,
10.4391298198825));
#273580=CARTESIAN_POINT('Ctrl Pts',(0.106121215206654,1.95111616457941,
10.443047155496));
#273581=CARTESIAN_POINT('Ctrl Pts',(0.0735935083316315,1.95288534667329,
10.4449127246312));
#273582=CARTESIAN_POINT('Ctrl Pts',(0.0410490824634399,1.95383939184425,
10.4467782937664));
#273583=CARTESIAN_POINT('Ctrl Pts',(0.00853176193233716,1.95398137376955,
10.4486438629016));
#273584=CARTESIAN_POINT('Ctrl Pts',(-0.0597585054663083,1.95427955281647,
10.4525617815065));
#273585=CARTESIAN_POINT('Ctrl Pts',(-0.128199965837453,1.95099396842147,
10.4564797001114));
#273586=CARTESIAN_POINT('Ctrl Pts',(-0.196385405575358,1.94410616286174,
10.4603976187163));
#273587=CARTESIAN_POINT('Ctrl Pts',(-0.264468086381559,1.93722873757592,
10.4643096328183));
#273588=CARTESIAN_POINT('Ctrl Pts',(-0.332295026796115,1.92675991422756,
10.4682216469203));
#273589=CARTESIAN_POINT('Ctrl Pts',(-0.399459038952325,1.91273324752807,
10.4721336610223));
#273590=CARTESIAN_POINT('Ctrl Pts',(-0.466543982646745,1.89872309364437,
10.4760410697273));
#273591=CARTESIAN_POINT('Ctrl Pts',(-0.532967068755224,1.88116351479865,
10.4799484784323));
#273592=CARTESIAN_POINT('Ctrl Pts',(-0.59832808697045,1.86013964538749,
10.4838558871373));
#273593=CARTESIAN_POINT('Ctrl Pts',(-0.663648083866068,1.83912897079626,
10.4877608435081));
#273594=CARTESIAN_POINT('Ctrl Pts',(-0.727906867860279,1.81465846888872,
10.4916657998789));
#273595=CARTESIAN_POINT('Ctrl Pts',(-0.79071777670186,1.7868635643517,10.4955707562498));
#273596=CARTESIAN_POINT('Ctrl Pts',(-0.853510814206847,1.75907656818766,
10.4994746015589));
#273597=CARTESIAN_POINT('Ctrl Pts',(-0.914856344709965,1.72796724608777,
10.5033784468681));
#273598=CARTESIAN_POINT('Ctrl Pts',(-0.974387836881763,1.6937190863118,
10.5072822921773));
#273599=CARTESIAN_POINT('Ctrl Pts',(-1.03392281454644,1.65946892134979,
10.5111863660517));
#273600=CARTESIAN_POINT('Ctrl Pts',(-1.09164311788173,1.62207980138402,
10.515090439926));
#273601=CARTESIAN_POINT('Ctrl Pts',(-1.14720856340261,1.58178017184934,
10.5189945138004));
#273602=CARTESIAN_POINT('Ctrl Pts',(-1.20283322768021,1.54143759306922,
10.5229027484332));
#273603=CARTESIAN_POINT('Ctrl Pts',(-1.25629805194379,1.49817860368856,
10.5268109830661));
#273604=CARTESIAN_POINT('Ctrl Pts',(-1.30729433089059,1.45227322925865,
10.530719217699));
#273605=CARTESIAN_POINT('Ctrl Pts',(-1.35832111196475,1.40634039769643,
10.534629789943));
#273606=CARTESIAN_POINT('Ctrl Pts',(-1.40687606141522,1.35775837889213,
10.538540362187));
#273607=CARTESIAN_POINT('Ctrl Pts',(-1.45268791200197,1.30683351285593,
10.5424509344311));
#273608=CARTESIAN_POINT('Ctrl Pts',(-1.49857899459168,1.25582057181108,
10.5463682700446));
#273609=CARTESIAN_POINT('Ctrl Pts',(-1.54171720044315,1.20245707875382,
10.5502856056581));
#273610=CARTESIAN_POINT('Ctrl Pts',(-1.58187259387785,1.14708112038258,
10.5542029412716));
#273611=CARTESIAN_POINT('Ctrl Pts',(-1.60099596496339,1.12070919595175,
10.5560685104068));
#273612=CARTESIAN_POINT('Ctrl Pts',(-1.61944348781101,1.09388124861885,
10.557934079542));
#273613=CARTESIAN_POINT('Ctrl Pts',(-1.63719398309528,1.06663576806547,
10.5597996486772));
#273614=CARTESIAN_POINT('Ctrl Pts',(-1.67525271209658,1.00821889888604,
10.5637996041157));
#273615=CARTESIAN_POINT('Ctrl Pts',(-1.71025039317968,0.947656606513882,
10.5677995595543));
#273616=CARTESIAN_POINT('Ctrl Pts',(-1.74194395780078,0.885295006131485,
10.5717995149929));
#273617=CARTESIAN_POINT('Ctrl Pts',(-1.77358357467427,0.823039555622688,
10.5757926618383));
#273618=CARTESIAN_POINT('Ctrl Pts',(-1.80193003757505,0.758991291439256,
10.5797858086838));
#273619=CARTESIAN_POINT('Ctrl Pts',(-1.82678404858984,0.693524361372909,
10.5837789555292));
#273620=CARTESIAN_POINT('Ctrl Pts',(-1.85159550625389,0.628169519340802,
10.5877652655796));
#273621=CARTESIAN_POINT('Ctrl Pts',(-1.87292624176117,0.561401274733641,
10.5917515756301));
#273622=CARTESIAN_POINT('Ctrl Pts',(-1.89062411321434,0.493615703288001,
10.5957378856805));
#273623=CARTESIAN_POINT('Ctrl Pts',(-1.90830416947359,0.425898366776875,
10.5997201829949));
#273624=CARTESIAN_POINT('Ctrl Pts',(-1.92235850832266,0.357166185273823,
10.6037024803093));
#273625=CARTESIAN_POINT('Ctrl Pts',(-1.93268440510735,0.287831531029609,
10.6076847776237));
#273626=CARTESIAN_POINT('Ctrl Pts',(-1.9430020556683,0.218552247188954,
10.6116638946899));
#273627=CARTESIAN_POINT('Ctrl Pts',(-1.94959711577114,0.148671905876252,
10.6156430117561));
#273628=CARTESIAN_POINT('Ctrl Pts',(-1.95241799906493,0.0786127020736065,
10.6196221288223));
#273629=CARTESIAN_POINT('Ctrl Pts',(-1.95348331470874,0.0521546185476659,
10.6211248551734));
#273630=CARTESIAN_POINT('Ctrl Pts',(-1.95401087610628,0.0256711001595666,
10.6226275815246));
#273631=CARTESIAN_POINT('Ctrl Pts',(-1.95399983006838,-0.000814918850473378,
10.6241303078758));
#273632=CARTESIAN_POINT('',(-1.95399956009588,-0.00131116173880527,11.3241303078758));
#273633=CARTESIAN_POINT('Ctrl Pts',(-1.95399983006808,-0.000814919564467043,
10.6241303079163));
#273634=CARTESIAN_POINT('Ctrl Pts',(-1.9539685147891,-0.0759021459440577,
10.6283905009516));
#273635=CARTESIAN_POINT('Ctrl Pts',(-1.94960488516428,-0.150851560010165,
10.6326506939869));
#273636=CARTESIAN_POINT('Ctrl Pts',(-1.94098145165923,-0.225182158073955,
10.6369108870221));
#273637=CARTESIAN_POINT('Ctrl Pts',(-1.93233214265287,-0.299735792760608,
10.6411838632058));
#273638=CARTESIAN_POINT('Ctrl Pts',(-1.91939756216364,-0.373666572052315,
10.6454568393895));
#273639=CARTESIAN_POINT('Ctrl Pts',(-1.90230107844747,-0.446504878962826,
10.6497298155732));
#273640=CARTESIAN_POINT('Ctrl Pts',(-1.88512890787792,-0.519665644125383,
10.6540217084024));
#273641=CARTESIAN_POINT('Ctrl Pts',(-1.86375805156586,-0.591723931865959,
10.6583136012317));
#273642=CARTESIAN_POINT('Ctrl Pts',(-1.83836197564382,-0.66222446836925,
10.6626054940609));
#273643=CARTESIAN_POINT('Ctrl Pts',(-1.82189249635873,-0.707944410658504,
10.6653888075248));
#273644=CARTESIAN_POINT('Ctrl Pts',(-1.80373115748422,-0.753009659755936,
10.6681721209887));
#273645=CARTESIAN_POINT('Ctrl Pts',(-1.78393560091633,-0.797301556365778,
10.6709554344526));
#273646=CARTESIAN_POINT('Ctrl Pts',(-1.75607047527468,-0.859648844238558,
10.6748733530575));
#273647=CARTESIAN_POINT('Ctrl Pts',(-1.7248776172163,-0.920657320442244,
10.6787912716625));
#273648=CARTESIAN_POINT('Ctrl Pts',(-1.6905079878465,-0.979948336917393,
10.6827091902674));
#273649=CARTESIAN_POINT('Ctrl Pts',(-1.65619015525919,-1.03914999881003,
10.6866212043694));
#273650=CARTESIAN_POINT('Ctrl Pts',(-1.61870529764365,-1.09663891563633,
10.6905332184714));
#273651=CARTESIAN_POINT('Ctrl Pts',(-1.5782517579668,-1.15205789284858,
10.6944452325734));
#273652=CARTESIAN_POINT('Ctrl Pts',(-1.53784584199584,-1.20741162837635,
10.6983526412784));
#273653=CARTESIAN_POINT('Ctrl Pts',(-1.49447847345894,-1.26069986838858,
10.7022600499834));
#273654=CARTESIAN_POINT('Ctrl Pts',(-1.44839211859912,-1.31159302787868,
10.7061674586884));
#273655=CARTESIAN_POINT('Ctrl Pts',(-1.40233468806056,-1.36245424624218,
10.7100724150592));
#273656=CARTESIAN_POINT('Ctrl Pts',(-1.35356198573122,-1.41092300207031,
10.71397737143));
#273657=CARTESIAN_POINT('Ctrl Pts',(-1.30235671910202,-1.45670277552074,
10.7178823278009));
#273658=CARTESIAN_POINT('Ctrl Pts',(-1.25116602170253,-1.50246952343533,
10.7217861731101));
#273659=CARTESIAN_POINT('Ctrl Pts',(-1.19754450055124,-1.54554848005739,
10.7256900184192));
#273660=CARTESIAN_POINT('Ctrl Pts',(-1.1418103631971,-1.58568127140851,
10.7295938637284));
#273661=CARTESIAN_POINT('Ctrl Pts',(-1.08607296268026,-1.6258164124834,
10.7334979376028));
#273662=CARTESIAN_POINT('Ctrl Pts',(-1.02822310109709,-1.66300476044023,
10.7374020114772));
#273663=CARTESIAN_POINT('Ctrl Pts',(-0.968609094096294,-1.69703047198156,
10.7413060853515));
#273664=CARTESIAN_POINT('Ctrl Pts',(-0.908931553592955,-1.73109244635338,
10.7452143199844));
#273665=CARTESIAN_POINT('Ctrl Pts',(-0.847486543551229,-1.76198481331922,
10.7491225546173));
#273666=CARTESIAN_POINT('Ctrl Pts',(-0.784647296834283,-1.78953754349291,
10.7530307892502));
#273667=CARTESIAN_POINT('Ctrl Pts',(-0.721770464420032,-1.81710675363144,
10.7569413614942));
#273668=CARTESIAN_POINT('Ctrl Pts',(-0.657498196058105,-1.84133217802094,
10.7608519337382));
#273669=CARTESIAN_POINT('Ctrl Pts',(-0.592221388308868,-1.86209286213914,
10.7647625059822));
#273670=CARTESIAN_POINT('Ctrl Pts',(-0.52683168374006,-1.88288945204516,
10.7686798415957));
#273671=CARTESIAN_POINT('Ctrl Pts',(-0.460434448035369,-1.90020921780993,
10.7725971772092));
#273672=CARTESIAN_POINT('Ctrl Pts',(-0.393432475219139,-1.91398194543286,
10.7765145128228));
#273673=CARTESIAN_POINT('Ctrl Pts',(-0.361523845269081,-1.92054098915428,
10.7783800819579));
#273674=CARTESIAN_POINT('Ctrl Pts',(-0.329478159965262,-1.9262963267367,
10.7802456510931));
#273675=CARTESIAN_POINT('Ctrl Pts',(-0.29733921643378,-1.93124451853476,
10.7821112202283));
#273676=CARTESIAN_POINT('Ctrl Pts',(-0.229843586048967,-1.94163631390749,
10.7860291388332));
#273677=CARTESIAN_POINT('Ctrl Pts',(-0.161668555654476,-1.948506087794,
10.7899470574381));
#273678=CARTESIAN_POINT('Ctrl Pts',(-0.0932141343151712,-1.95177537774301,
10.793864976043));
#273679=CARTESIAN_POINT('Ctrl Pts',(-0.0248628772764009,-1.95503974070551,
10.797776990145));
#273680=CARTESIAN_POINT('Ctrl Pts',(0.0437664476449764,-1.95471436531483,
10.801689004247));
#273681=CARTESIAN_POINT('Ctrl Pts',(0.112266166666696,-1.95077223371207,
10.805601018349));
#273682=CARTESIAN_POINT('Ctrl Pts',(0.180685244773023,-1.94683474296193,
10.809508427054));
#273683=CARTESIAN_POINT('Ctrl Pts',(0.248974531204067,-1.93928898016744,
10.813415835759));
#273684=CARTESIAN_POINT('Ctrl Pts',(0.316725626858963,-1.92815997191384,
10.817323244464));
#273685=CARTESIAN_POINT('Ctrl Pts',(0.384434201154495,-1.9170379483526,
10.8212282008348));
#273686=CARTESIAN_POINT('Ctrl Pts',(0.451604770365875,-1.90233721994039,
10.8251331572056));
#273687=CARTESIAN_POINT('Ctrl Pts',(0.517834898997069,-1.88413455394796,
10.8290381135764));
#273688=CARTESIAN_POINT('Ctrl Pts',(0.584046183434645,-1.8659370670873,
10.8329419588856));
#273689=CARTESIAN_POINT('Ctrl Pts',(0.649317084352055,-1.84423975094801,
10.8368458041948));
#273690=CARTESIAN_POINT('Ctrl Pts',(0.713257969600139,-1.81916988453577,
10.840749649504));
#273691=CARTESIAN_POINT('Ctrl Pts',(0.777202598505579,-1.7940985503148,
10.8446537233783));
#273692=CARTESIAN_POINT('Ctrl Pts',(0.839816600080803,-1.76565445574872,
10.8485577972527));
#273693=CARTESIAN_POINT('Ctrl Pts',(0.900729753407535,-1.73401323850956,
10.852461871127));
#273694=CARTESIAN_POINT('Ctrl Pts',(0.961707824799248,-1.7023382997097,
10.8563701057599));
#273695=CARTESIAN_POINT('Ctrl Pts',(1.02098099298303,-1.66745966542983,
10.8602783403928));
#273696=CARTESIAN_POINT('Ctrl Pts',(1.07820402153073,-1.62959875059935,
10.8641865750256));
#273697=CARTESIAN_POINT('Ctrl Pts',(1.13546127657767,-1.59171519022554,
10.8680971472696));
#273698=CARTESIAN_POINT('Ctrl Pts',(1.19066555611156,-1.55084609201704,
10.8720077195137));
#273699=CARTESIAN_POINT('Ctrl Pts',(1.2435032811134,-1.50725432155964,10.8759182917577));
#273700=CARTESIAN_POINT('Ctrl Pts',(1.29643238943057,-1.46358715874752,
10.8798356273712));
#273701=CARTESIAN_POINT('Ctrl Pts',(1.34698641197762,-1.41718825790193,
10.8837529629847));
#273702=CARTESIAN_POINT('Ctrl Pts',(1.39488795320832,-1.36835799336076,
10.8876702985982));
#273703=CARTESIAN_POINT('Ctrl Pts',(1.41770030468006,-1.34510335209972,
10.8895358677334));
#273704=CARTESIAN_POINT('Ctrl Pts',(1.4399116600572,-1.32129777398009,10.8914014368686));
#273705=CARTESIAN_POINT('Ctrl Pts',(1.46149538198817,-1.29697619424076,
10.8932670060037));
#273706=CARTESIAN_POINT('Ctrl Pts',(1.50682378291525,-1.24589796402959,
10.8971849246087));
#273707=CARTESIAN_POINT('Ctrl Pts',(1.54956120552918,-1.19233919937936,
10.9011028432136));
#273708=CARTESIAN_POINT('Ctrl Pts',(1.5894248336085,-1.13659346219684,10.9050207618185));
#273709=CARTESIAN_POINT('Ctrl Pts',(1.62922838516937,-1.08093173668033,
10.9089327759205));
#273710=CARTESIAN_POINT('Ctrl Pts',(1.66616645372537,-1.02308997668234,
10.9128447900225));
#273711=CARTESIAN_POINT('Ctrl Pts',(1.69999529315344,-0.963396078078033,
10.9167568041245));
#273712=CARTESIAN_POINT('Ctrl Pts',(1.73378430776737,-0.903772453785764,
10.9206642128295));
#273713=CARTESIAN_POINT('Ctrl Pts',(1.76447112129018,-0.842301447179175,
10.9245716215345));
#273714=CARTESIAN_POINT('Ctrl Pts',(1.79185532432582,-0.779339782562925,
10.9284790302395));
#273715=CARTESIAN_POINT('Ctrl Pts',(1.8192223407237,-0.716417633404564,
10.9323839866103));
#273716=CARTESIAN_POINT('Ctrl Pts',(1.84329066253446,-0.652007132170347,
10.9362889429811));
#273717=CARTESIAN_POINT('Ctrl Pts',(1.8639065886548,-0.586488046569769,
10.940193899352));
#273718=CARTESIAN_POINT('Ctrl Pts',(1.88451664900813,-0.520987602852581,
10.9440977446611));
#273719=CARTESIAN_POINT('Ctrl Pts',(1.90167611609606,-0.454379669965605,
10.9480015899703));
#273720=CARTESIAN_POINT('Ctrl Pts',(1.91528067306263,-0.387060645626431,
10.9519054352795));
#273721=CARTESIAN_POINT('Ctrl Pts',(1.92888602655869,-0.319737679844125,
10.9558095091539));
#273722=CARTESIAN_POINT('Ctrl Pts',(1.93893596177339,-0.251704022650568,
10.9597135830282));
#273723=CARTESIAN_POINT('Ctrl Pts',(1.94537731985309,-0.183365982126458,
10.9636176569026));
#273724=CARTESIAN_POINT('Ctrl Pts',(1.95182554279661,-0.114955110479479,
10.9675258915355));
#273725=CARTESIAN_POINT('Ctrl Pts',(1.95465746721037,-0.0462396988173985,
10.9714341261683));
#273726=CARTESIAN_POINT('Ctrl Pts',(1.95387194510453,0.0223701169744634,
10.9753423608012));
#273727=CARTESIAN_POINT('Ctrl Pts',(1.95308595315862,0.091020969982767,
10.9792529330452));
#273728=CARTESIAN_POINT('Ctrl Pts',(1.94867824014254,0.159565610423876,
10.9831635052893));
#273729=CARTESIAN_POINT('Ctrl Pts',(1.94069965165146,0.227598027407773,
10.9870740775333));
#273730=CARTESIAN_POINT('Ctrl Pts',(1.93270726412062,0.295748107061931,
10.9909914131468));
#273731=CARTESIAN_POINT('Ctrl Pts',(1.92113175793174,0.363383710495605,
10.9949087487603));
#273732=CARTESIAN_POINT('Ctrl Pts',(1.90607511418001,0.430108892146699,
10.9988260843738));
#273733=CARTESIAN_POINT('Ctrl Pts',(1.8989046257067,0.461885704681965,11.000691653509));
#273734=CARTESIAN_POINT('Ctrl Pts',(1.89094535045098,0.493456257333144,
11.0025572226442));
#273735=CARTESIAN_POINT('Ctrl Pts',(1.8822121994957,0.524779226027066,11.0044227917794));
#273736=CARTESIAN_POINT('Ctrl Pts',(1.86387153660521,0.590561211531077,
11.0083407103843));
#273737=CARTESIAN_POINT('Ctrl Pts',(1.84204176826305,0.655511113583888,
11.0122586289892));
#273738=CARTESIAN_POINT('Ctrl Pts',(1.8168162123231,0.719232125700695,11.0161765475941));
#273739=CARTESIAN_POINT('Ctrl Pts',(1.79162867258112,0.782857107005847,
11.0200885616961));
#273740=CARTESIAN_POINT('Ctrl Pts',(1.76305568148216,0.84525642020697,11.0240005757981));
#273741=CARTESIAN_POINT('Ctrl Pts',(1.73124058994447,0.906047471012826,
11.0279125899001));
#273742=CARTESIAN_POINT('Ctrl Pts',(1.69946295254735,0.966766955890282,
11.0318199986051));
#273743=CARTESIAN_POINT('Ctrl Pts',(1.66445102182194,1.02588150472803,11.0357274073101));
#273744=CARTESIAN_POINT('Ctrl Pts',(1.62639586916403,1.08302930558973,11.0396348160151));
#273745=CARTESIAN_POINT('Ctrl Pts',(1.5883646003534,1.14014123984066,11.0435397723859));
#273746=CARTESIAN_POINT('Ctrl Pts',(1.54729417039366,1.19528846612587,11.0474447287567));
#273747=CARTESIAN_POINT('Ctrl Pts',(1.50342033842383,1.24813592449444,11.0513496851275));
#273748=CARTESIAN_POINT('Ctrl Pts',(1.45955898969995,1.30096834638702,11.0552535304367));
#273749=CARTESIAN_POINT('Ctrl Pts',(1.41289613648942,1.35150192101288,11.0591573757459));
#273750=CARTESIAN_POINT('Ctrl Pts',(1.36370828778775,1.39943406626358,11.0630612210551));
#273751=CARTESIAN_POINT('Ctrl Pts',(1.31451755920018,1.44736901788033,11.0669652949294));
#273752=CARTESIAN_POINT('Ctrl Pts',(1.26280189572413,1.49270189623786,11.0708693688038));
#273753=CARTESIAN_POINT('Ctrl Pts',(1.2088738718207,1.53516773091061,11.0747734426781));
#273754=CARTESIAN_POINT('Ctrl Pts',(1.15488837423927,1.5776788234573,11.078681677311));
#273755=CARTESIAN_POINT('Ctrl Pts',(1.0986861979647,1.61731646942391,11.0825899119438));
#273756=CARTESIAN_POINT('Ctrl Pts',(1.04061133452346,1.65385732469923,11.0864981465767));
#273757=CARTESIAN_POINT('Ctrl Pts',(0.982501735079602,1.69042003595783,
11.0904087188207));
#273758=CARTESIAN_POINT('Ctrl Pts',(0.922517648943269,1.72388203048328,
11.0943192910648));
#273759=CARTESIAN_POINT('Ctrl Pts',(0.861027793049799,1.75406588804292,
11.0982298633088));
#273760=CARTESIAN_POINT('Ctrl Pts',(0.799431589903674,1.78430194885266,
11.1021471989223));
#273761=CARTESIAN_POINT('Ctrl Pts',(0.736324871501352,1.8112483639733,11.1060645345358));
#273762=CARTESIAN_POINT('Ctrl Pts',(0.672095623599954,1.83477613695453,
11.1099818701493));
#273763=CARTESIAN_POINT('Ctrl Pts',(0.641507460040964,1.84598086675665,
11.1118474392844));
#273764=CARTESIAN_POINT('Ctrl Pts',(0.610664917406567,1.85641098761622,
11.1137130084196));
#273765=CARTESIAN_POINT('Ctrl Pts',(0.579610802906014,1.86605662217272,
11.1155785775548));
#273766=CARTESIAN_POINT('Ctrl Pts',(0.514393443406147,1.88631360990501,
11.1194964961597));
#273767=CARTESIAN_POINT('Ctrl Pts',(0.447983410876055,1.90318773630915,
11.1234144147647));
#273768=CARTESIAN_POINT('Ctrl Pts',(0.380764717166862,1.91654225890295,
11.1273323333696));
#273769=CARTESIAN_POINT('Ctrl Pts',(0.313647325453663,1.92987665555084,
11.1312443474716));
#273770=CARTESIAN_POINT('Ctrl Pts',(0.245724169844897,1.9397018802542,11.1351563615736));
#273771=CARTESIAN_POINT('Ctrl Pts',(0.17739444888597,1.94593093646831,11.1390683756756));
#273772=CARTESIAN_POINT('Ctrl Pts',(0.109145168713203,1.95215265956044,
11.1429757843806));
#273773=CARTESIAN_POINT('Ctrl Pts',(0.0404907613303627,1.95478657761763,
11.1468831930856));
#273774=CARTESIAN_POINT('Ctrl Pts',(-0.0281611624639135,1.95379705929983,
11.1507906017906));
#273775=CARTESIAN_POINT('Ctrl Pts',(-0.096769999528806,1.95280816201501,
11.1546955581614));
#273776=CARTESIAN_POINT('Ctrl Pts',(-0.165375865315554,1.94820034651441,
11.1586005145322));
#273777=CARTESIAN_POINT('Ctrl Pts',(-0.233569397092006,1.93999003521721,
11.162505470903));
#273778=CARTESIAN_POINT('Ctrl Pts',(-0.301743526035585,1.93178205996705,
11.1664093162122));
#273779=CARTESIAN_POINT('Ctrl Pts',(-0.369505065683895,1.91997368248687,
11.1703131615214));
#273780=CARTESIAN_POINT('Ctrl Pts',(-0.43644984764403,1.90463317478498,
11.1742170068306));
#273781=CARTESIAN_POINT('Ctrl Pts',(-0.503398549135946,1.88929176891589,
11.178121080705));
#273782=CARTESIAN_POINT('Ctrl Pts',(-0.569529919061022,1.8704179346261,
11.1820251545793));
#273783=CARTESIAN_POINT('Ctrl Pts',(-0.634451836961836,1.84813064110083,
11.1859292284537));
#273784=CARTESIAN_POINT('Ctrl Pts',(-0.699442945259962,1.82581959493941,
11.1898374630866));
#273785=CARTESIAN_POINT('Ctrl Pts',(-0.763221562947385,1.80008798943833,
11.1937456977194));
#273786=CARTESIAN_POINT('Ctrl Pts',(-0.82541351117599,1.77110376194285,
11.1976539323523));
#273787=CARTESIAN_POINT('Ctrl Pts',(-0.887642657936773,1.74210219826882,
11.2015645045963));
#273788=CARTESIAN_POINT('Ctrl Pts',(-0.948282812127677,1.709844371824,11.2054750768404));
#273789=CARTESIAN_POINT('Ctrl Pts',(-1.00698497578881,1.67454389567297,
11.2093856490844));
#273790=CARTESIAN_POINT('Ctrl Pts',(-1.06578866536411,1.63918236703447,
11.2133029846979));
#273791=CARTESIAN_POINT('Ctrl Pts',(-1.12264726733472,1.6007679611778,11.2172203203114));
#273792=CARTESIAN_POINT('Ctrl Pts',(-1.17724202376935,1.55955673749673,
11.2211376559249));
#273793=CARTESIAN_POINT('Ctrl Pts',(-1.20324191313156,1.53993054395428,
11.2230032250601));
#273794=CARTESIAN_POINT('Ctrl Pts',(-1.22872886914824,1.51967060984118,
11.2248687941952));
#273795=CARTESIAN_POINT('Ctrl Pts',(-1.25367138196224,1.49880754803573,
11.2267343633304));
#273796=CARTESIAN_POINT('Ctrl Pts',(-1.3079287206718,1.45342422120985,11.2307925276864));
#273797=CARTESIAN_POINT('Ctrl Pts',(-1.35984680323557,1.40498323572559,
11.2348506920425));
#273798=CARTESIAN_POINT('Ctrl Pts',(-1.40905733704925,1.35376269002646,
11.2389088563985));
#273799=CARTESIAN_POINT('Ctrl Pts',(-1.45582513564135,1.30508465344787,
11.2427655797167));
#273800=CARTESIAN_POINT('Ctrl Pts',(-1.50014735042896,1.25389683588597,
11.2466223030348));
#273801=CARTESIAN_POINT('Ctrl Pts',(-1.54174049822195,1.20048000239168,
11.250479026353));
#273802=CARTESIAN_POINT('Ctrl Pts',(-1.58329453093444,1.14711340322331,
11.2543321227265));
#273803=CARTESIAN_POINT('Ctrl Pts',(-1.62212427238269,1.09152233964788,
11.2581852191001));
#273804=CARTESIAN_POINT('Ctrl Pts',(-1.65798463175839,1.03402270809348,
11.2620383154736));
#273805=CARTESIAN_POINT('Ctrl Pts',(-1.69382437880148,0.976556127003494,
11.2658891971091));
#273806=CARTESIAN_POINT('Ctrl Pts',(-1.72669786015049,0.917183582291981,
11.2697400787445));
#273807=CARTESIAN_POINT('Ctrl Pts',(-1.75640286533857,0.856250532630753,
11.2735909603799));
#273808=CARTESIAN_POINT('Ctrl Pts',(-1.78610165457326,0.795330233581561,
11.2774410361949));
#273809=CARTESIAN_POINT('Ctrl Pts',(-1.81263306292323,0.732850533811338,
11.2812911120099));
#273810=CARTESIAN_POINT('Ctrl Pts',(-1.83584141958589,0.669180306145414,
11.2851411878249));
#273811=CARTESIAN_POINT('Ctrl Pts',(-1.85906597067962,0.605465650382825,
11.2889939501631));
#273812=CARTESIAN_POINT('Ctrl Pts',(-1.87896266653266,0.540559285055208,
11.2928467125012));
#273813=CARTESIAN_POINT('Ctrl Pts',(-1.89542497282366,0.474847525418879,
11.2966994748393));
#273814=CARTESIAN_POINT('Ctrl Pts',(-1.91189397277362,0.409109047040911,
11.3005538037306));
#273815=CARTESIAN_POINT('Ctrl Pts',(-1.92492570561245,0.342565020072114,
11.3044081326218));
#273816=CARTESIAN_POINT('Ctrl Pts',(-1.93446485725264,0.275611531062305,
11.3082624615131));
#273817=CARTESIAN_POINT('Ctrl Pts',(-1.94401756415766,0.20856290022976,
11.3121222674584));
#273818=CARTESIAN_POINT('Ctrl Pts',(-1.95006774392593,0.141104150990945,
11.3159820734036));
#273819=CARTESIAN_POINT('Ctrl Pts',(-1.95261207530983,0.0736347971697302,
11.3198418793489));
#273820=CARTESIAN_POINT('Ctrl Pts',(-1.95355436648917,0.0486475736564669,
11.3212713555245));
#273821=CARTESIAN_POINT('Ctrl Pts',(-1.9540163153482,0.0236588741376556,
11.3227008317002));
#273822=CARTESIAN_POINT('Ctrl Pts',(-1.95399956009588,-0.00131116173880527,
11.3241303078758));
#273823=CARTESIAN_POINT('',(-1.95399932181806,0.00162798481247529,12.0241303078758));
#273824=CARTESIAN_POINT('Ctrl Pts',(-1.95604828032066,-0.00131253645946981,
11.3241303078758));
#273825=CARTESIAN_POINT('Ctrl Pts',(-1.95666788006178,-0.0815157866439698,
11.3287169216192));
#273826=CARTESIAN_POINT('Ctrl Pts',(-1.91576572910727,-0.80898595490767,
11.3703554639544));
#273827=CARTESIAN_POINT('Ctrl Pts',(-1.00369601420896,-2.08016482602406,
11.4490459348816));
#273828=CARTESIAN_POINT('Ctrl Pts',(1.20363141497037,-1.97123382916792,
11.560201720657));
#273829=CARTESIAN_POINT('Ctrl Pts',(2.3089364786395,-0.057478082500643,
11.6713575064327));
#273830=CARTESIAN_POINT('Ctrl Pts',(1.3002225757448,1.90890351927077,11.7825132922081));
#273831=CARTESIAN_POINT('Ctrl Pts',(-0.89895074918647,2.12752883479819,
11.8936690779838));
#273832=CARTESIAN_POINT('Ctrl Pts',(-1.89602525605444,0.874547554056413,
11.9742080832062));
#273833=CARTESIAN_POINT('Ctrl Pts',(-1.95616528042983,0.114289761396843,
12.0176951598369));
#273834=CARTESIAN_POINT('Ctrl Pts',(-1.95515771590482,0.00162894993460125,
12.0241303078758));
#273835=CARTESIAN_POINT('',(-1.95370249770292,0.000308414297733195,12.7241302921614));
#273836=CARTESIAN_POINT('Ctrl Pts',(-1.95399932181806,0.00162798481247529,
12.0241303078758));
#273837=CARTESIAN_POINT('Ctrl Pts',(-1.9540554909094,-0.0657893310810446,
12.0279834768089));
#273838=CARTESIAN_POINT('Ctrl Pts',(-1.95061836818367,-0.133329609715946,
12.031836645742));
#273839=CARTESIAN_POINT('Ctrl Pts',(-1.94367633872893,-0.200594841073482,
12.035689814675));
#273840=CARTESIAN_POINT('Ctrl Pts',(-1.9367409886327,-0.267795352366316,
12.0395392762345));
#273841=CARTESIAN_POINT('Ctrl Pts',(-1.92630746402906,-0.334720838234257,
12.043388737794));
#273842=CARTESIAN_POINT('Ctrl Pts',(-1.9124161765106,-0.400974273265233,
12.0472381993535));
#273843=CARTESIAN_POINT('Ctrl Pts',(-1.89853315627626,-0.467188278115878,
12.051085369938));
#273844=CARTESIAN_POINT('Ctrl Pts',(-1.88119655565532,-0.532730528746946,
12.0549325405225));
#273845=CARTESIAN_POINT('Ctrl Pts',(-1.86049823265094,-0.597212128395529,
12.0587797111069));
#273846=CARTESIAN_POINT('Ctrl Pts',(-1.83980463332279,-0.661679012349574,
12.0626260037078));
#273847=CARTESIAN_POINT('Ctrl Pts',(-1.81575098950706,-0.725085242231116,
12.0664722963087));
#273848=CARTESIAN_POINT('Ctrl Pts',(-1.78847902146685,-0.787057043531779,
12.0703185889096));
#273849=CARTESIAN_POINT('Ctrl Pts',(-1.76118407533488,-0.849081059389693,
12.0741681222177));
#273850=CARTESIAN_POINT('Ctrl Pts',(-1.73066559046174,-0.909667765005355,
12.0780176555258));
#273851=CARTESIAN_POINT('Ctrl Pts',(-1.69711300844451,-0.968464473570616,
12.081867188834));
#273852=CARTESIAN_POINT('Ctrl Pts',(-1.66354753547827,-1.02728377191368,
12.0857182011382));
#273853=CARTESIAN_POINT('Ctrl Pts',(-1.62694591854707,-1.08431127521329,
12.0895692134424));
#273854=CARTESIAN_POINT('Ctrl Pts',(-1.58754146245115,-1.13922258799519,
12.0934202257466));
#273855=CARTESIAN_POINT('Ctrl Pts',(-1.54806429116053,-1.19423523162126,
12.0972783445341));
#273856=CARTESIAN_POINT('Ctrl Pts',(-1.50577426642181,-1.24712348582285,
12.1011364633216));
#273857=CARTESIAN_POINT('Ctrl Pts',(-1.46094509962579,-1.29759601412743,
12.1049945821091));
#273858=CARTESIAN_POINT('Ctrl Pts',(-1.41839446150562,-1.34550317904688,
12.1086566045844));
#273859=CARTESIAN_POINT('Ctrl Pts',(-1.37355682168725,-1.39123398319979,
12.1123186270596));
#273860=CARTESIAN_POINT('Ctrl Pts',(-1.3266942071601,-1.43457257769965,
12.1159806495348));
#273861=CARTESIAN_POINT('Ctrl Pts',(-1.27655690992226,-1.48093960216542,
12.1198985681397));
#273862=CARTESIAN_POINT('Ctrl Pts',(-1.22388643151331,-1.52476709658075,
12.1238164867447));
#273863=CARTESIAN_POINT('Ctrl Pts',(-1.16897046839485,-1.56576628013913,
12.1277344053496));
#273864=CARTESIAN_POINT('Ctrl Pts',(-1.11413726643054,-1.60670367583915,
12.1316464194516));
#273865=CARTESIAN_POINT('Ctrl Pts',(-1.05706568690618,-1.64482092808708,
12.1355584335536));
#273866=CARTESIAN_POINT('Ctrl Pts',(-0.998078554773395,-1.67986761338549,
12.1394704476556));
#273867=CARTESIAN_POINT('Ctrl Pts',(-0.939160864915841,-1.71487304016737,
12.1433778563606));
#273868=CARTESIAN_POINT('Ctrl Pts',(-0.878332521961585,-1.74681482895347,
12.1472852650656));
#273869=CARTESIAN_POINT('Ctrl Pts',(-0.815946062527566,-1.77548529226399,
12.1511926737706));
#273870=CARTESIAN_POINT('Ctrl Pts',(-0.753598757546154,-1.80413776166515,
12.1550976301414));
#273871=CARTESIAN_POINT('Ctrl Pts',(-0.689695721890799,-1.82952277334644,
12.1590025865122));
#273872=CARTESIAN_POINT('Ctrl Pts',(-0.624613489224658,-1.85147886541505,
12.162907542883));
#273873=CARTESIAN_POINT('Ctrl Pts',(-0.559549774145845,-1.8734287104046,
12.1668113881922));
#273874=CARTESIAN_POINT('Ctrl Pts',(-0.493307994009486,-1.89195141535257,
12.1707152335014));
#273875=CARTESIAN_POINT('Ctrl Pts',(-0.426282322391558,-1.90693455095251,
12.1746190788106));
#273876=CARTESIAN_POINT('Ctrl Pts',(-0.359252726506088,-1.92191856379593,
12.1785231526849));
#273877=CARTESIAN_POINT('Ctrl Pts',(-0.291439628667888,-1.93336249102916,
12.1824272265593));
#273878=CARTESIAN_POINT('Ctrl Pts',(-0.22324816053472,-1.94120484720646,
12.1863313004336));
#273879=CARTESIAN_POINT('Ctrl Pts',(-0.154984017487743,-1.94905556135837,
12.1902395350665));
#273880=CARTESIAN_POINT('Ctrl Pts',(-0.0863411890446798,-1.9532969879008,
12.1941477696994));
#273881=CARTESIAN_POINT('Ctrl Pts',(-0.0177297011688613,-1.95391956274982,
12.1980560043323));
#273882=CARTESIAN_POINT('Ctrl Pts',(0.0509228249235043,-1.95454250997616,
12.2019665765763));
#273883=CARTESIAN_POINT('Ctrl Pts',(0.119543481598909,-1.95154231920351,
12.2058771488203));
#273884=CARTESIAN_POINT('Ctrl Pts',(0.18772530006829,-1.94496149363278,
12.2097877210643));
#273885=CARTESIAN_POINT('Ctrl Pts',(0.256025039599139,-1.93836928646571,
12.2137050566778));
#273886=CARTESIAN_POINT('Ctrl Pts',(0.323883939875557,-1.92818415766703,
12.2176223922913));
#273887=CARTESIAN_POINT('Ctrl Pts',(0.390904045973118,-1.91449994171895,
12.2215397279048));
#273888=CARTESIAN_POINT('Ctrl Pts',(0.42282131161165,-1.9079830502829,12.22340529704));
#273889=CARTESIAN_POINT('Ctrl Pts',(0.454548547372225,-1.90067330553549,
12.2252708661752));
#273890=CARTESIAN_POINT('Ctrl Pts',(0.486044131895434,-1.89258476741466,
12.2271364353103));
#273891=CARTESIAN_POINT('Ctrl Pts',(0.552188631314071,-1.87559786867538,
12.2310543539153));
#273892=CARTESIAN_POINT('Ctrl Pts',(0.617572821896984,-1.85510552414462,
12.2349722725202));
#273893=CARTESIAN_POINT('Ctrl Pts',(0.68179806575538,-1.83119288922064,
12.2388901911251));
#273894=CARTESIAN_POINT('Ctrl Pts',(0.745926518899189,-1.80731629185577,
12.2428022052271));
#273895=CARTESIAN_POINT('Ctrl Pts',(0.808899034363604,-1.78002980427668,
12.2467142193291));
#273896=CARTESIAN_POINT('Ctrl Pts',(0.870330156739797,-1.74946889605654,
12.2506262334311));
#273897=CARTESIAN_POINT('Ctrl Pts',(0.93168895966685,-1.71894396549662,
12.2545336421361));
#273898=CARTESIAN_POINT('Ctrl Pts',(0.991509534952271,-1.68515248802175,
12.2584410508411));
#273899=CARTESIAN_POINT('Ctrl Pts',(1.04942622590129,-1.64827807010546,
12.2623484595461));
#273900=CARTESIAN_POINT('Ctrl Pts',(1.10730656767539,-1.61142679499386,
12.2662534159169));
#273901=CARTESIAN_POINT('Ctrl Pts',(1.16328498136309,-1.57149668123188,
12.2701583722877));
#273902=CARTESIAN_POINT('Ctrl Pts',(1.21702163959142,-1.52871656259956,
12.2740633286585));
#273903=CARTESIAN_POINT('Ctrl Pts',(1.27074300834321,-1.48594861602337,
12.2779671739677));
#273904=CARTESIAN_POINT('Ctrl Pts',(1.32222350315288,-1.44033258059323,
12.2818710192769));
#273905=CARTESIAN_POINT('Ctrl Pts',(1.37115493142929,-1.39213869783766,
12.2857748645861));
#273906=CARTESIAN_POINT('Ctrl Pts',(1.42008922457854,-1.34394199339161,
12.2896789384604));
#273907=CARTESIAN_POINT('Ctrl Pts',(1.46647380620244,-1.29316748899696,
12.2935830123348));
#273908=CARTESIAN_POINT('Ctrl Pts',(1.51003734737879,-1.24012225587691,
12.2974870862091));
#273909=CARTESIAN_POINT('Ctrl Pts',(1.55364731630747,-1.18702048991128,
12.301395320842));
#273910=CARTESIAN_POINT('Ctrl Pts',(1.59442993185607,-1.13164354647098,
12.3053035554749));
#273911=CARTESIAN_POINT('Ctrl Pts',(1.63215483794644,-1.07433076143617,
12.3092117901078));
#273912=CARTESIAN_POINT('Ctrl Pts',(1.66990230822993,-1.01698369621663,
12.3131223623518));
#273913=CARTESIAN_POINT('Ctrl Pts',(1.70458818076787,-0.957698909690016,
12.3170329345958));
#273914=CARTESIAN_POINT('Ctrl Pts',(1.73602750630394,-0.896841400335714,
12.3209435068398));
#273915=CARTESIAN_POINT('Ctrl Pts',(1.7675212064332,-0.835878637377611,
12.3248608424533));
#273916=CARTESIAN_POINT('Ctrl Pts',(1.7957569506424,-0.773338170923284,
12.3287781780668));
#273917=CARTESIAN_POINT('Ctrl Pts',(1.8205978078482,-0.709605257913402,
12.3326955136803));
#273918=CARTESIAN_POINT('Ctrl Pts',(1.83242787324641,-0.679253465997395,
12.3345610828155));
#273919=CARTESIAN_POINT('Ctrl Pts',(1.8434887128893,-0.648631452940076,
12.3364266519507));
#273920=CARTESIAN_POINT('Ctrl Pts',(1.85376957305606,-0.617781814244768,
12.3382922210859));
#273921=CARTESIAN_POINT('Ctrl Pts',(1.8753606106448,-0.552993878423696,
12.3422101396908));
#273922=CARTESIAN_POINT('Ctrl Pts',(1.89359397391154,-0.486944101538939,
12.3461280582957));
#273923=CARTESIAN_POINT('Ctrl Pts',(1.90832506892014,-0.420013608506845,
12.3500459769006));
#273924=CARTESIAN_POINT('Ctrl Pts',(1.92303396341805,-0.353183983137696,
12.3539579910026));
#273925=CARTESIAN_POINT('Ctrl Pts',(1.93425095987221,-0.285476752365371,
12.3578700051046));
#273926=CARTESIAN_POINT('Ctrl Pts',(1.94188088816484,-0.217289245431345,
12.3617820192066));
#273927=CARTESIAN_POINT('Ctrl Pts',(1.94950183416659,-0.149182011862786,
12.3656894279116));
#273928=CARTESIAN_POINT('Ctrl Pts',(1.95354404418813,-0.0805961115949446,
12.3695968366166));
#273929=CARTESIAN_POINT('Ctrl Pts',(1.95396352987359,-0.011938338408627,
12.3735042453216));
#273930=CARTESIAN_POINT('Ctrl Pts',(1.95438275228505,0.0566763443772267,
12.3774092016925));
#273931=CARTESIAN_POINT('Ctrl Pts',(1.95118375756041,0.125362319778213,
12.3813141580633));
#273932=CARTESIAN_POINT('Ctrl Pts',(1.94437456419064,0.193709974261689,
12.3852191144341));
#273933=CARTESIAN_POINT('Ctrl Pts',(1.93756730821343,0.262038182060291,
12.3891229597433));
#273934=CARTESIAN_POINT('Ctrl Pts',(1.92715194147817,0.330027770748407,
12.3930268050524));
#273935=CARTESIAN_POINT('Ctrl Pts',(1.91318842773897,0.397273256041339,
12.3969306503616));
#273936=CARTESIAN_POINT('Ctrl Pts',(1.89922409645384,0.46452267847175,12.400834724236));
#273937=CARTESIAN_POINT('Ctrl Pts',(1.88171130825211,0.531027429868459,
12.4047387981103));
#273938=CARTESIAN_POINT('Ctrl Pts',(1.86076096062313,0.596393030996247,
12.4086428719847));
#273939=CARTESIAN_POINT('Ctrl Pts',(1.83978828520522,0.66182829537597,12.4125511066175));
#273940=CARTESIAN_POINT('Ctrl Pts',(1.81537088939659,0.72612151724033,12.4164593412504));
#273941=CARTESIAN_POINT('Ctrl Pts',(1.78766899671218,0.788895150317236,
12.4203675758833));
#273942=CARTESIAN_POINT('Ctrl Pts',(1.75995053484516,0.85170632984636,12.4242781481273));
#273943=CARTESIAN_POINT('Ctrl Pts',(1.72894388842041,0.91299567267797,12.4281887203713));
#273944=CARTESIAN_POINT('Ctrl Pts',(1.6948554637872,0.972409870821289,12.4320992926154));
#273945=CARTESIAN_POINT('Ctrl Pts',(1.66070808292043,1.03192682634868,12.4360166282289));
#273946=CARTESIAN_POINT('Ctrl Pts',(1.62346855284891,1.08956175148456,12.4399339638424));
#273947=CARTESIAN_POINT('Ctrl Pts',(1.58338633786399,1.14499070086428,12.4438512994559));
#273948=CARTESIAN_POINT('Ctrl Pts',(1.56429781685795,1.17138786142477,12.4457168685911));
#273949=CARTESIAN_POINT('Ctrl Pts',(1.54456516290423,1.19728520154391,12.4475824377263));
#273950=CARTESIAN_POINT('Ctrl Pts',(1.52421833582585,1.22265058979755,12.4494480068614));
#273951=CARTESIAN_POINT('Ctrl Pts',(1.48148756222014,1.27592094289543,12.4533659254664));
#273952=CARTESIAN_POINT('Ctrl Pts',(1.43587597248702,1.32705421430028,12.4572838440713));
#273953=CARTESIAN_POINT('Ctrl Pts',(1.387625404141,1.37572226040816,12.4612017626762));
#273954=CARTESIAN_POINT('Ctrl Pts',(1.33944755185965,1.42431696129111,12.4651137767782));
#273955=CARTESIAN_POINT('Ctrl Pts',(1.28863895757512,1.47045346370681,12.4690257908802));
#273956=CARTESIAN_POINT('Ctrl Pts',(1.23548187243687,1.51383636595238,12.4729378049822));
#273957=CARTESIAN_POINT('Ctrl Pts',(1.18238736618313,1.55716819591618,12.4768452136872));
#273958=CARTESIAN_POINT('Ctrl Pts',(1.12695023920267,1.59775255410474,12.4807526223922));
#273959=CARTESIAN_POINT('Ctrl Pts',(1.06948844639271,1.63533191219168,12.4846600310973));
#273960=CARTESIAN_POINT('Ctrl Pts',(1.01206271725846,1.67288768504543,12.4885649874681));
#273961=CARTESIAN_POINT('Ctrl Pts',(0.952615253736853,1.70744193029679,
12.4924699438389));
#273962=CARTESIAN_POINT('Ctrl Pts',(0.891494578602756,1.73877928913416,
12.4963749002097));
#273963=CARTESIAN_POINT('Ctrl Pts',(0.830391293889959,1.77010773167813,
12.5002787455189));
#273964=CARTESIAN_POINT('Ctrl Pts',(0.767616180191292,1.79822088045845,
12.504182590828));
#273965=CARTESIAN_POINT('Ctrl Pts',(0.70354245591668,1.82294926224586,12.5080864361372));
#273966=CARTESIAN_POINT('Ctrl Pts',(0.639464980207017,1.84767909184857,
12.5119905100116));
#273967=CARTESIAN_POINT('Ctrl Pts',(0.57408920283838,1.86902358627734,12.515894583886));
#273968=CARTESIAN_POINT('Ctrl Pts',(0.507806712048847,1.88686203607952,
12.5197986577603));
#273969=CARTESIAN_POINT('Ctrl Pts',(0.441453580834311,1.90471949717201,
12.5237068923932));
#273970=CARTESIAN_POINT('Ctrl Pts',(0.374192283648423,1.9190633284824,12.5276151270261));
#273971=CARTESIAN_POINT('Ctrl Pts',(0.306426925951779,1.92982344763757,
12.5315233616589));
#273972=CARTESIAN_POINT('Ctrl Pts',(0.238621036129936,1.94059000268433,
12.535433933903));
#273973=CARTESIAN_POINT('Ctrl Pts',(0.170310975093264,1.94776852818752,
12.539344506147));
#273974=CARTESIAN_POINT('Ctrl Pts',(0.101905523011608,1.95134088881972,
12.543255078391));
#273975=CARTESIAN_POINT('Ctrl Pts',(0.0333817630921084,1.95491942788141,
12.5471724140045));
#273976=CARTESIAN_POINT('Ctrl Pts',(-0.0352372254569389,1.95487935441795,
12.551089749618));
#273977=CARTESIAN_POINT('Ctrl Pts',(-0.103543987799294,1.95125463294533,
12.5550070852315));
#273978=CARTESIAN_POINT('Ctrl Pts',(-0.13607400312618,1.94952841666723,
12.5568726543667));
#273979=CARTESIAN_POINT('Ctrl Pts',(-0.168533302538319,1.94698996459378,
12.5587382235018));
#273980=CARTESIAN_POINT('Ctrl Pts',(-0.200878643321318,1.94364702830977,
12.560603792637));
#273981=CARTESIAN_POINT('Ctrl Pts',(-0.268807732653197,1.9366264617623,
12.5645217112419));
#273982=CARTESIAN_POINT('Ctrl Pts',(-0.336503158662888,1.9260265627108,
12.5684396298468));
#273983=CARTESIAN_POINT('Ctrl Pts',(-0.403558074281079,1.91187261099754,
12.5723575484517));
#273984=CARTESIAN_POINT('Ctrl Pts',(-0.47051193472534,1.89773999001058,
12.5762695625537));
#273985=CARTESIAN_POINT('Ctrl Pts',(-0.536826723058539,1.88006404713187,
12.5801815766557));
#273986=CARTESIAN_POINT('Ctrl Pts',(-0.602101190726571,1.85892177245995,
12.5840935907577));
#273987=CARTESIAN_POINT('Ctrl Pts',(-0.667298814388258,1.83780438741405,
12.5880009994627));
#273988=CARTESIAN_POINT('Ctrl Pts',(-0.731458083890375,1.81322892578366,
12.5919084081677));
#273989=CARTESIAN_POINT('Ctrl Pts',(-0.794190214627478,1.78532291280596,
12.5958158168727));
#273990=CARTESIAN_POINT('Ctrl Pts',(-0.856882973964803,1.75743441395986,
12.5997207732435));
#273991=CARTESIAN_POINT('Ctrl Pts',(-0.918149922826318,1.72621970971303,
12.6036257296144));
#273992=CARTESIAN_POINT('Ctrl Pts',(-0.977621135074021,1.69185487446666,
12.6075306859852));
#273993=CARTESIAN_POINT('Ctrl Pts',(-1.03707542621546,1.65749981690947,
12.6114345312943));
#273994=CARTESIAN_POINT('Ctrl Pts',(-1.09473456928394,1.61999665364559,
12.6153383766035));
#273995=CARTESIAN_POINT('Ctrl Pts',(-1.15025380299516,1.57956708901369,
12.6192422219127));
#273996=CARTESIAN_POINT('Ctrl Pts',(-1.20577628728657,1.53913515728244,
12.623146295787));
#273997=CARTESIAN_POINT('Ctrl Pts',(-1.2591582173127,1.49577677567557,12.6270503696613));
#273998=CARTESIAN_POINT('Ctrl Pts',(-1.31008584493853,1.44975552383555,
12.6309544435357));
#273999=CARTESIAN_POINT('Ctrl Pts',(-1.36106774857662,1.40368522494297,
12.6348626781685));
#274000=CARTESIAN_POINT('Ctrl Pts',(-1.40958976402385,1.35494672257884,
12.6387709128014));
#274001=CARTESIAN_POINT('Ctrl Pts',(-1.45537389526011,1.30384156437637,
12.6426791474343));
#274002=CARTESIAN_POINT('Ctrl Pts',(-1.50118541111011,1.25270583892319,
12.6465897196783));
#274003=CARTESIAN_POINT('Ctrl Pts',(-1.54425547511677,1.19920102368488,
12.6505002919223));
#274004=CARTESIAN_POINT('Ctrl Pts',(-1.58434720475194,1.14366076036329,
12.6544108641663));
#274005=CARTESIAN_POINT('Ctrl Pts',(-1.62450827339006,1.08802443966234,
12.6583281997798));
#274006=CARTESIAN_POINT('Ctrl Pts',(-1.66168046053407,1.03034605811188,
12.6622455353933));
#274007=CARTESIAN_POINT('Ctrl Pts',(-1.69567137881452,0.970986392834244,
12.6661628710068));
#274008=CARTESIAN_POINT('Ctrl Pts',(-1.71185901609634,0.942717290988959,
12.6680284401421));
#274009=CARTESIAN_POINT('Ctrl Pts',(-1.72732583476716,0.914067205865857,
12.6698940092773));
#274010=CARTESIAN_POINT('Ctrl Pts',(-1.74205490144005,0.88507667485291,
12.6717595784125));
#274011=CARTESIAN_POINT('Ctrl Pts',(-1.77651139766982,0.817257569628513,
12.6761238044224));
#274012=CARTESIAN_POINT('Ctrl Pts',(-1.80705483983964,0.747321895345659,
12.6804880304322));
#274013=CARTESIAN_POINT('Ctrl Pts',(-1.83343982526576,0.67573249672445,
12.6848522564421));
#274014=CARTESIAN_POINT('Ctrl Pts',(-1.8586008869996,0.60746392468978,12.689014038542));
#274015=CARTESIAN_POINT('Ctrl Pts',(-1.8799804781929,0.537692051207313,
12.693175820642));
#274016=CARTESIAN_POINT('Ctrl Pts',(-1.89741215384907,0.466843783749794,
12.697337602742));
#274017=CARTESIAN_POINT('Ctrl Pts',(-1.9148071043119,0.396144779987412,
12.7014906167662));
#274018=CARTESIAN_POINT('Ctrl Pts',(-1.92827058971641,0.324374272716027,
12.7056436307904));
#274019=CARTESIAN_POINT('Ctrl Pts',(-1.93768523310141,0.251976065174288,
12.7097966448147));
#274020=CARTESIAN_POINT('Ctrl Pts',(-1.94707437508419,0.179773962331943,
12.7139384095885));
#274021=CARTESIAN_POINT('Ctrl Pts',(-1.95243646025069,0.106947933259381,
12.7180801743623));
#274022=CARTESIAN_POINT('Ctrl Pts',(-1.95370500604768,0.033952162585741,
12.7222219391361));
#274023=CARTESIAN_POINT('Ctrl Pts',(-1.95389983693685,0.0227410333228769,
12.7228580562676));
#274024=CARTESIAN_POINT('Ctrl Pts',(-1.95399820468377,0.0115259205146458,
12.7234941733992));
#274025=CARTESIAN_POINT('Ctrl Pts',(-1.9539999756484,0.000308489971946228,
12.7241302905307));
#274026=CARTESIAN_POINT('',(-1.95402820026386,-0.00178509135925994,13.4241303078758));
#274027=CARTESIAN_POINT('Ctrl Pts',(-1.95083582512995,0.000307685056475884,
12.7241303078758));
#274028=CARTESIAN_POINT('Ctrl Pts',(-1.95035082451635,-0.344675762667878,
12.7437253266466));
#274029=CARTESIAN_POINT('Ctrl Pts',(-1.69859020752685,-1.34264473489564,
12.800372274009));
#274030=CARTESIAN_POINT('Ctrl Pts',(-0.104847311655371,-2.30727077595995,
12.8940711499638));
#274031=CARTESIAN_POINT('Ctrl Pts',(1.88181988362473,-1.33912109906285,
13.0052269357391));
#274032=CARTESIAN_POINT('Ctrl Pts',(2.1455280618664,0.85510275879836,13.1163827215148));
#274033=CARTESIAN_POINT('Ctrl Pts',(0.44483095739769,2.26641055673969,13.2275385072902));
#274034=CARTESIAN_POINT('Ctrl Pts',(-1.50056042635302,1.65383118156618,
13.3301210360774));
#274035=CARTESIAN_POINT('Ctrl Pts',(-1.94943588392903,0.497535626713033,
13.3956516362725));
#274036=CARTESIAN_POINT('Ctrl Pts',(-1.95402820026386,-0.00178509135925994,
13.4241303078758));
#274037=CARTESIAN_POINT('',(-1.95413348876404,0.000767679038905043,14.1241303078758));
#274038=CARTESIAN_POINT('Ctrl Pts',(-1.95402820026386,-0.00178509135925994,
13.4241303078758));
#274039=CARTESIAN_POINT('Ctrl Pts',(-1.95541067725083,-0.152101261135744,
13.4327035648643));
#274040=CARTESIAN_POINT('Ctrl Pts',(-1.87089950475814,-0.950516301187075,
13.4783287504445));
#274041=CARTESIAN_POINT('Ctrl Pts',(-0.775036692012782,-2.17573195003328,
13.5610058646171));
#274042=CARTESIAN_POINT('Ctrl Pts',(1.40791228892896,-1.83092172935965,
13.6721616503923));
#274043=CARTESIAN_POINT('Ctrl Pts',(2.30180316472699,0.190246112222753,
13.7833174361682));
#274044=CARTESIAN_POINT('Ctrl Pts',(1.08820620248698,2.03722817897972,13.8944732219435));
#274045=CARTESIAN_POINT('Ctrl Pts',(-1.12173196396984,2.01896230607907,
14.0056290077192));
#274046=CARTESIAN_POINT('Ctrl Pts',(-1.93638948072713,0.733314628616374,
14.0821813696965));
#274047=CARTESIAN_POINT('Ctrl Pts',(-1.95705073983529,0.0435387888036669,
14.1216818030821));
#274048=CARTESIAN_POINT('Ctrl Pts',(-1.95683651916685,0.000768740921214415,
14.1241303078758));
#274049=CARTESIAN_POINT('',(-1.95399956106643,0.00130971454563185,14.8241303078238));
#274050=CARTESIAN_POINT('Ctrl Pts',(-1.95399984921942,0.000767626538767374,
14.1241303078758));
#274051=CARTESIAN_POINT('Ctrl Pts',(-1.95402643386531,-0.0669038145125677,
14.1280100028959));
#274052=CARTESIAN_POINT('Ctrl Pts',(-1.95053334135365,-0.134718102982957,
14.1318896979161));
#274053=CARTESIAN_POINT('Ctrl Pts',(-1.94350227311917,-0.20227435423359,
14.1357693929362));
#274054=CARTESIAN_POINT('Ctrl Pts',(-1.93648251703331,-0.269721915548593,
14.1396428459907));
#274055=CARTESIAN_POINT('Ctrl Pts',(-1.92593613721697,-0.336911768377198,
14.1435162990451));
#274056=CARTESIAN_POINT('Ctrl Pts',(-1.91189683763907,-0.403443282538866,
14.1473897520996));
#274057=CARTESIAN_POINT('Ctrl Pts',(-1.89787010835416,-0.469915226732554,
14.151259737001));
#274058=CARTESIAN_POINT('Ctrl Pts',(-1.88035676061684,-0.535729511362023,
14.1551297219024));
#274059=CARTESIAN_POINT('Ctrl Pts',(-1.85944208487721,-0.600492408767574,
14.1589997068038));
#274060=CARTESIAN_POINT('Ctrl Pts',(-1.83853862212686,-0.665220584828008,
14.1628676168894));
#274061=CARTESIAN_POINT('Ctrl Pts',(-1.81423760121725,-0.728898014171866,
14.166735526975));
#274062=CARTESIAN_POINT('Ctrl Pts',(-1.78667452646286,-0.791144826494302,
14.1706034370606));
#274063=CARTESIAN_POINT('Ctrl Pts',(-1.75911632835618,-0.85338062568496,
14.1744706628091));
#274064=CARTESIAN_POINT('Ctrl Pts',(-1.72829742601706,-0.914185851384229,
14.1783378885577));
#274065=CARTESIAN_POINT('Ctrl Pts',(-1.69440120631608,-0.973201187851012,
14.1822051143062));
#274066=CARTESIAN_POINT('Ctrl Pts',(-1.66047473866568,-1.03226918779851,
14.1860757910486));
#274067=CARTESIAN_POINT('Ctrl Pts',(-1.62346571708041,-1.08954367020213,
14.1899464677911));
#274068=CARTESIAN_POINT('Ctrl Pts',(-1.58360266826016,-1.14469148205065,
14.1938171445336));
#274069=CARTESIAN_POINT('Ctrl Pts',(-1.54372302155348,-1.19986225594409,
14.1976894329202));
#274070=CARTESIAN_POINT('Ctrl Pts',(-1.50098729627419,-1.25290420366035,
14.2015617213069));
#274071=CARTESIAN_POINT('Ctrl Pts',(-1.45566457516665,-1.30351702888949,
14.2054340096936));
#274072=CARTESIAN_POINT('Ctrl Pts',(-1.41025760552753,-1.35422393620596,
14.209313496117));
#274073=CARTESIAN_POINT('Ctrl Pts',(-1.36225438800566,-1.40249234297613,
14.2131929825405));
#274074=CARTESIAN_POINT('Ctrl Pts',(-1.31196066470999,-1.44805911973707,
14.2170724689639));
#274075=CARTESIAN_POINT('Ctrl Pts',(-1.26499588012766,-1.4906098341097,
14.2206951723993));
#274076=CARTESIAN_POINT('Ctrl Pts',(-1.21603438180848,-1.53080491841486,
14.2243178758348));
#274077=CARTESIAN_POINT('Ctrl Pts',(-1.16534810818424,-1.56846414901693,
14.2279405792703));
#274078=CARTESIAN_POINT('Ctrl Pts',(-1.1105313952005,-1.60919224140752,
14.2318584978752));
#274079=CARTESIAN_POINT('Ctrl Pts',(-1.05346818430586,-1.64712400283433,
14.2357764164801));
#274080=CARTESIAN_POINT('Ctrl Pts',(-0.994475457487556,-1.68200314044146,
14.239694335085));
#274081=CARTESIAN_POINT('Ctrl Pts',(-0.935571635714056,-1.71682971341122,
14.243606349187));
#274082=CARTESIAN_POINT('Ctrl Pts',(-0.874744489147849,-1.74861254445149,
14.247518363289));
#274083=CARTESIAN_POINT('Ctrl Pts',(-0.812341816209655,-1.77713724108106,
14.251430377391));
#274084=CARTESIAN_POINT('Ctrl Pts',(-0.750012606473188,-1.80562835716922,
14.255337786096));
#274085=CARTESIAN_POINT('Ctrl Pts',(-0.686111999261733,-1.83086875287559,
14.259245194801));
#274086=CARTESIAN_POINT('Ctrl Pts',(-0.621012754626721,-1.85268970920414,
14.263152603506));
#274087=CARTESIAN_POINT('Ctrl Pts',(-0.555954367019157,-1.87449697045195,
14.2670575598768));
#274088=CARTESIAN_POINT('Ctrl Pts',(-0.48969929964492,-1.89288889344172,
14.2709625162476));
#274089=CARTESIAN_POINT('Ctrl Pts',(-0.422639218570995,-1.90774528984498,
14.2748674726184));
#274090=CARTESIAN_POINT('Ctrl Pts',(-0.355598217833756,-1.92259745921718,
14.2787713179276));
#274091=CARTESIAN_POINT('Ctrl Pts',(-0.287753138159825,-1.9339159926138,
14.2826751632368));
#274092=CARTESIAN_POINT('Ctrl Pts',(-0.21950793033573,-1.94163134207288,
14.286579008546));
#274093=CARTESIAN_POINT('Ctrl Pts',(-0.151258726841537,-1.94934714325586,
14.2904830824203));
#274094=CARTESIAN_POINT('Ctrl Pts',(-0.0826098377990403,-1.95345928894754,
14.2943871562947));
#274095=CARTESIAN_POINT('Ctrl Pts',(-0.0139706505631757,-1.95395005589264,
14.298291230169));
#274096=CARTESIAN_POINT('Ctrl Pts',(0.0547416887419765,-1.95444134587158,
14.3021994648019));
#274097=CARTESIAN_POINT('Ctrl Pts',(0.123443812729814,-1.9513035512105,
14.3061076994348));
#274098=CARTESIAN_POINT('Ctrl Pts',(0.191727031081185,-1.94457109552538,
14.3100159340677));
#274099=CARTESIAN_POINT('Ctrl Pts',(0.260051091303008,-1.93783461299313,
14.3139265063117));
#274100=CARTESIAN_POINT('Ctrl Pts',(0.327955260822571,-1.92749926447036,
14.3178370785557));
#274101=CARTESIAN_POINT('Ctrl Pts',(0.395039467697114,-1.91365091355806,
14.3217476507997));
#274102=CARTESIAN_POINT('Ctrl Pts',(0.462239697304064,-1.89977861179969,
14.3256649864132));
#274103=CARTESIAN_POINT('Ctrl Pts',(0.528616658251948,-1.88238130595424,
14.3295823220267));
#274104=CARTESIAN_POINT('Ctrl Pts',(0.593784740514013,-1.86159492960545,
14.3334996576402));
#274105=CARTESIAN_POINT('Ctrl Pts',(0.624820009090008,-1.8516957465957,
14.3353652267754));
#274106=CARTESIAN_POINT('Ctrl Pts',(0.655581390671758,-1.8410286354368,
14.3372307959106));
#274107=CARTESIAN_POINT('Ctrl Pts',(0.686029009967765,-1.82961203469005,
14.3390963650457));
#274108=CARTESIAN_POINT('Ctrl Pts',(0.749972656904149,-1.8056358058668,
14.3430142836507));
#274109=CARTESIAN_POINT('Ctrl Pts',(0.812784777378005,-1.7782557751123,
14.3469322022556));
#274110=CARTESIAN_POINT('Ctrl Pts',(0.874078152400699,-1.74759932006618,
14.3508501208605));
#274111=CARTESIAN_POINT('Ctrl Pts',(0.935279155184495,-1.71698906585968,
14.3547621349625));
#274112=CARTESIAN_POINT('Ctrl Pts',(0.994965518577663,-1.68311240526268,
14.3586741490645));
#274113=CARTESIAN_POINT('Ctrl Pts',(1.05276852114657,-1.64614532799594,
14.3625861631665));
#274114=CARTESIAN_POINT('Ctrl Pts',(1.11050347545034,-1.6092217700165,14.3664935718715));
#274115=CARTESIAN_POINT('Ctrl Pts',(1.16635905979217,-1.56921528460179,
14.3704009805765));
#274116=CARTESIAN_POINT('Ctrl Pts',(1.21999139515354,-1.5263475999101,14.3743083892815));
#274117=CARTESIAN_POINT('Ctrl Pts',(1.27359007025038,-1.48350681946557,
14.3782133456523));
#274118=CARTESIAN_POINT('Ctrl Pts',(1.32496788084573,-1.43780870831795,
14.3821183020231));
#274119=CARTESIAN_POINT('Ctrl Pts',(1.37381147447616,-1.38951719406333,
14.3860232583939));
#274120=CARTESIAN_POINT('Ctrl Pts',(1.42264117083421,-1.34123942000016,
14.3899271037031));
#274121=CARTESIAN_POINT('Ctrl Pts',(1.46893773196347,-1.29037005336541,
14.3938309490123));
#274122=CARTESIAN_POINT('Ctrl Pts',(1.512423694745,-1.23721080159117,14.3977347943215));
#274123=CARTESIAN_POINT('Ctrl Pts',(1.55591220357432,-1.18404843741039,
14.4016388681959));
#274124=CARTESIAN_POINT('Ctrl Pts',(1.59658947785309,-1.12859630430256,
14.4055429420702));
#274125=CARTESIAN_POINT('Ctrl Pts',(1.63421865207261,-1.07118877758217,
14.4094470159446));
#274126=CARTESIAN_POINT('Ctrl Pts',(1.67188792950531,-1.01372006891107,
14.4133552505775));
#274127=CARTESIAN_POINT('Ctrl Pts',(1.70650235362224,-0.954292219893747,
14.4172634852103));
#274128=CARTESIAN_POINT('Ctrl Pts',(1.73786925291926,-0.893267294687242,
14.4211717198432));
#274129=CARTESIAN_POINT('Ctrl Pts',(1.76925491352942,-0.832205868973619,
14.4250822920872));
#274130=CARTESIAN_POINT('Ctrl Pts',(1.79738898201236,-0.769545914793622,
14.4289928643313));
#274131=CARTESIAN_POINT('Ctrl Pts',(1.82212668193712,-0.705670146012158,
14.4329034365753));
#274132=CARTESIAN_POINT('Ctrl Pts',(1.8469071659339,-0.641683903520521,
14.4368207721888));
#274133=CARTESIAN_POINT('Ctrl Pts',(1.86827940447334,-0.576478116851078,
14.4407381078023));
#274134=CARTESIAN_POINT('Ctrl Pts',(1.88614853348424,-0.510450496752881,
14.4446554434158));
#274135=CARTESIAN_POINT('Ctrl Pts',(1.89465842358414,-0.479005886875614,
14.446521012551));
#274136=CARTESIAN_POINT('Ctrl Pts',(1.90237456301791,-0.447375030903409,
14.4483865816862));
#274137=CARTESIAN_POINT('Ctrl Pts',(1.90929082390855,-0.415601431348128,
14.4502521508214));
#274138=CARTESIAN_POINT('Ctrl Pts',(1.92381580007209,-0.348873067067548,
14.4541700694263));
#274139=CARTESIAN_POINT('Ctrl Pts',(1.93486722982208,-0.281249887143623,
14.4580879880312));
#274140=CARTESIAN_POINT('Ctrl Pts',(1.94234218761738,-0.213126315131955,
14.4620059066361));
#274141=CARTESIAN_POINT('Ctrl Pts',(1.94980588027048,-0.145105408813827,
14.4659179207381));
#274142=CARTESIAN_POINT('Ctrl Pts',(1.95370374478881,-0.0765860921174858,
14.4698299348401));
#274143=CARTESIAN_POINT('Ctrl Pts',(1.95398373116002,-0.00797360407566831,
14.4737419489421));
#274144=CARTESIAN_POINT('Ctrl Pts',(1.95426338791883,0.0605581102938482,
14.4776493576471));
#274145=CARTESIAN_POINT('Ctrl Pts',(1.95093362319341,0.129182288571518,
14.4815567663521));
#274146=CARTESIAN_POINT('Ctrl Pts',(1.94399428818267,0.197489765590924,
14.4854641750572));
#274147=CARTESIAN_POINT('Ctrl Pts',(1.93705930837763,0.265754372059655,
14.489369131428));
#274148=CARTESIAN_POINT('Ctrl Pts',(1.92651930171783,0.333702183235872,
14.4932740877988));
#274149=CARTESIAN_POINT('Ctrl Pts',(1.91242612898619,0.400926802759444,
14.4971790441696));
#274150=CARTESIAN_POINT('Ctrl Pts',(1.89833696612862,0.46813229513088,14.5010828894787));
#274151=CARTESIAN_POINT('Ctrl Pts',(1.88069674501712,0.534614523082058,
14.5049867347879));
#274152=CARTESIAN_POINT('Ctrl Pts',(1.85960853023193,0.599976761457181,
14.5088905800971));
#274153=CARTESIAN_POINT('Ctrl Pts',(1.83851908075864,0.665342826708067,
14.5127946539714));
#274154=CARTESIAN_POINT('Ctrl Pts',(1.81398139030327,0.729588304806202,
14.5166987278458));
#274155=CARTESIAN_POINT('Ctrl Pts',(1.78614798482388,0.792332869638516,
14.5206028017201));
#274156=CARTESIAN_POINT('Ctrl Pts',(1.75828491595114,0.855144304358821,
14.524511036353));
#274157=CARTESIAN_POINT('Ctrl Pts',(1.72711932220709,0.916451182948067,
14.5284192709859));
#274158=CARTESIAN_POINT('Ctrl Pts',(1.69285095732083,0.975895299864676,
14.5323275056188));
#274159=CARTESIAN_POINT('Ctrl Pts',(1.65856209568363,1.03537497176801,14.5362380778628));
#274160=CARTESIAN_POINT('Ctrl Pts',(1.62116703730577,1.09298925190883,14.5401486501068));
#274161=CARTESIAN_POINT('Ctrl Pts',(1.58090885585488,1.14840898180031,14.5440592223508));
#274162=CARTESIAN_POINT('Ctrl Pts',(1.54058104752112,1.20392456060753,14.5479765579643));
#274163=CARTESIAN_POINT('Ctrl Pts',(1.49738054259637,1.25723763189034,14.5518938935778));
#274164=CARTESIAN_POINT('Ctrl Pts',(1.45159007873062,1.30805284424247,14.5558112291913));
#274165=CARTESIAN_POINT('Ctrl Pts',(1.42978309446835,1.33225278550745,14.5576767983265));
#274166=CARTESIAN_POINT('Ctrl Pts',(1.40738923910176,1.35588676737919,14.5595423674617));
#274167=CARTESIAN_POINT('Ctrl Pts',(1.38444174273771,1.3789260534798,14.5614079365968));
#274168=CARTESIAN_POINT('Ctrl Pts',(1.3362492521751,1.42731131348196,14.5653258552018));
#274169=CARTESIAN_POINT('Ctrl Pts',(1.2854215092442,1.47326312640682,14.5692437738067));
#274170=CARTESIAN_POINT('Ctrl Pts',(1.23223411854782,1.5164811495982,14.5731616924116));
#274171=CARTESIAN_POINT('Ctrl Pts',(1.17912688395893,1.55963404102681,14.5770737065136));
#274172=CARTESIAN_POINT('Ctrl Pts',(1.12366743790186,1.60006101162009,14.5809857206156));
#274173=CARTESIAN_POINT('Ctrl Pts',(1.06616805780133,1.63749860229685,14.5848977347176));
#274174=CARTESIAN_POINT('Ctrl Pts',(1.00873636852802,1.67489211977704,14.5888051434226));
#274175=CARTESIAN_POINT('Ctrl Pts',(0.949269924912657,1.70930297941689,
14.5927125521276));
#274176=CARTESIAN_POINT('Ctrl Pts',(0.888112444611049,1.7405092029998,14.5966199608326));
#274177=CARTESIAN_POINT('Ctrl Pts',(0.826993347440678,1.77169584120133,
14.6005249172034));
#274178=CARTESIAN_POINT('Ctrl Pts',(0.764185756086352,1.79968160994729,
14.6044298735742));
#274179=CARTESIAN_POINT('Ctrl Pts',(0.700059261816433,1.82428973300434,
14.608334829945));
#274180=CARTESIAN_POINT('Ctrl Pts',(0.635951013201532,1.84889085441052,
14.6122386752542));
#274181=CARTESIAN_POINT('Ctrl Pts',(0.570525065692171,1.87011606175263,
14.6161425205634));
#274182=CARTESIAN_POINT('Ctrl Pts',(0.504170647569705,1.88783684626854,
14.6200463658726));
#274183=CARTESIAN_POINT('Ctrl Pts',(0.437812344480365,1.90555866831387,
14.623950439747));
#274184=CARTESIAN_POINT('Ctrl Pts',(0.370525938794869,1.91977553572203,
14.6278545136213));
#274185=CARTESIAN_POINT('Ctrl Pts',(0.302713698029415,1.93040939104257,
14.6317585874957));
#274186=CARTESIAN_POINT('Ctrl Pts',(0.234829186511242,1.94105457937202,
14.6356668221286));
#274187=CARTESIAN_POINT('Ctrl Pts',(0.166418208443643,1.94810905848887,
14.6395750567615));
#274188=CARTESIAN_POINT('Ctrl Pts',(0.0978900520182863,1.95154644774749,
14.6434832913943));
#274189=CARTESIAN_POINT('Ctrl Pts',(0.0293209072190169,1.95498589299308,
14.6473938636384));
#274190=CARTESIAN_POINT('Ctrl Pts',(-0.0393650634138969,1.95480394398451,
14.6513044358824));
#274191=CARTESIAN_POINT('Ctrl Pts',(-0.107759489808657,1.9510263689546,
14.6552150081264));
#274192=CARTESIAN_POINT('Ctrl Pts',(-0.176272204972246,1.94724226057508,
14.6591323437399));
#274193=CARTESIAN_POINT('Ctrl Pts',(-0.244491880700859,1.93985016757965,
14.6630496793534));
#274194=CARTESIAN_POINT('Ctrl Pts',(-0.312017046916634,1.92892751611703,
14.6669670149669));
#274195=CARTESIAN_POINT('Ctrl Pts',(-0.344174839449375,1.92372577609436,
14.6688325841021));
#274196=CARTESIAN_POINT('Ctrl Pts',(-0.376175295340427,1.9177240530037,
14.6706981532373));
#274197=CARTESIAN_POINT('Ctrl Pts',(-0.407976251362151,1.91093468709019,
14.6725637223725));
#274198=CARTESIAN_POINT('Ctrl Pts',(-0.47476206749868,1.89667620557556,
14.6764816409774));
#274199=CARTESIAN_POINT('Ctrl Pts',(-0.540932054278828,1.87888403280015,
14.6803995595823));
#274200=CARTESIAN_POINT('Ctrl Pts',(-0.606084415364867,1.85762689511426,
14.6843174781872));
#274201=CARTESIAN_POINT('Ctrl Pts',(-0.671138588523441,1.83640179301783,
14.6882294922892));
#274202=CARTESIAN_POINT('Ctrl Pts',(-0.735177715747694,1.81172224090109,
14.6921415063912));
#274203=CARTESIAN_POINT('Ctrl Pts',(-0.797811107533291,1.78370777783148,
14.6960535204932));
#274204=CARTESIAN_POINT('Ctrl Pts',(-0.860370764504758,1.7557262946336,
14.6999609291982));
#274205=CARTESIAN_POINT('Ctrl Pts',(-0.921527525735173,1.72441789746557,
14.7038683379033));
#274206=CARTESIAN_POINT('Ctrl Pts',(-0.980908508555638,1.68995103415547,
14.7077757466083));
#274207=CARTESIAN_POINT('Ctrl Pts',(-1.04025222319486,1.65550580264142,
14.7116807029791));
#274208=CARTESIAN_POINT('Ctrl Pts',(-1.09782194571756,1.61790628359267,
14.7155856593499));
#274209=CARTESIAN_POINT('Ctrl Pts',(-1.1532687452085,1.57736717390886,14.7194906157207));
#274210=CARTESIAN_POINT('Ctrl Pts',(-1.20869976864335,1.53683959865577,
14.7233944610299));
#274211=CARTESIAN_POINT('Ctrl Pts',(-1.26200867120127,1.49337438334165,
14.7272983063391));
#274212=CARTESIAN_POINT('Ctrl Pts',(-1.31287643101941,1.44722889581218,
14.7312021516482));
#274213=CARTESIAN_POINT('Ctrl Pts',(-1.36374716908006,1.40108070652322,
14.7351062255226));
#274214=CARTESIAN_POINT('Ctrl Pts',(-1.41217611800806,1.35225226588987,
14.739010299397));
#274215=CARTESIAN_POINT('Ctrl Pts',(-1.45787957732774,1.30103925306298,
14.7429143732713));
#274216=CARTESIAN_POINT('Ctrl Pts',(-1.50363174501301,1.24977166007546,
14.7468226079042));
#274217=CARTESIAN_POINT('Ctrl Pts',(-1.54665229802001,1.19611479085303,
14.7507308425371));
#274218=CARTESIAN_POINT('Ctrl Pts',(-1.58669715029207,1.14039824327075,
14.7546390771699));
#274219=CARTESIAN_POINT('Ctrl Pts',(-1.62676595437416,1.08464837025244,
14.758549649414));
#274220=CARTESIAN_POINT('Ctrl Pts',(-1.66385524983905,1.02683678119652,
14.762460221658));
#274221=CARTESIAN_POINT('Ctrl Pts',(-1.69776526619505,0.967320578144422,
14.766370793902));
#274222=CARTESIAN_POINT('Ctrl Pts',(-1.73173393022585,0.907701441289936,
14.7702881295155));
#274223=CARTESIAN_POINT('Ctrl Pts',(-1.76251212021033,0.846372245822791,
14.774205465129));
#274224=CARTESIAN_POINT('Ctrl Pts',(-1.78994721212184,0.783712305516029,
14.7781228007425));
#274225=CARTESIAN_POINT('Ctrl Pts',(-1.80301274077191,0.75387149988175,
14.7799883698777));
#274226=CARTESIAN_POINT('Ctrl Pts',(-1.8153207795147,0.7237291370088,14.7818539390128));
#274227=CARTESIAN_POINT('Ctrl Pts',(-1.8268588358628,0.693327335268145,
14.783719508148));
#274228=CARTESIAN_POINT('Ctrl Pts',(-1.85454088667258,0.620387474766188,
14.788195372889));
#274229=CARTESIAN_POINT('Ctrl Pts',(-1.87787906227524,0.545713210096145,
14.79267123763));
#274230=CARTESIAN_POINT('Ctrl Pts',(-1.8966828185995,0.469798132850119,
14.797147102371));
#274231=CARTESIAN_POINT('Ctrl Pts',(-1.91557621125608,0.393521173170883,
14.8016443032798));
#274232=CARTESIAN_POINT('Ctrl Pts',(-1.92989163872075,0.315991707952488,
14.8061415041886));
#274233=CARTESIAN_POINT('Ctrl Pts',(-1.93948425663725,0.237732661315694,
14.8106387050974));
#274234=CARTESIAN_POINT('Ctrl Pts',(-1.94907687455376,0.1594736146789,14.8151359060062));
#274235=CARTESIAN_POINT('Ctrl Pts',(-1.95394649182682,0.0804851892759246,
14.819633106915));
#274236=CARTESIAN_POINT('Ctrl Pts',(-1.95399956106643,0.00130971454563252,
14.8241303078238));
#274237=CARTESIAN_POINT('',(-1.95399944231052,-0.00147629610118066,15.5241303078758));
#274238=CARTESIAN_POINT('Ctrl Pts',(-1.95399956106705,0.00130971363016174,
14.8241303078758));
#274239=CARTESIAN_POINT('Ctrl Pts',(-1.95404586063319,-0.0677659452257072,
14.8280538349129));
#274240=CARTESIAN_POINT('Ctrl Pts',(-1.95042499795379,-0.136864374352902,
14.8319773619499));
#274241=CARTESIAN_POINT('Ctrl Pts',(-1.94315626763052,-0.205571689607818,
14.835900888987));
#274242=CARTESIAN_POINT('Ctrl Pts',(-1.93588716306388,-0.274282542379846,
14.8398246180337));
#274243=CARTESIAN_POINT('Ctrl Pts',(-1.92496987030036,-0.342601759347549,
14.8437483470805));
#274244=CARTESIAN_POINT('Ctrl Pts',(-1.91047548303559,-0.410121236611718,
14.8476720761272));
#274245=CARTESIAN_POINT('Ctrl Pts',(-1.8959446266587,-0.477810598627981,
14.8516056776102));
#274246=CARTESIAN_POINT('Ctrl Pts',(-1.87781875978922,-0.544695714643512,
14.8555392790933));
#274247=CARTESIAN_POINT('Ctrl Pts',(-1.85622038180967,-0.610378484347524,
14.8594728805763));
#274248=CARTESIAN_POINT('Ctrl Pts',(-1.83463860778333,-0.676010759813655,
14.8634034580667));
#274249=CARTESIAN_POINT('Ctrl Pts',(-1.80958986356056,-0.740442093694928,
14.8673340355571));
#274250=CARTESIAN_POINT('Ctrl Pts',(-1.78124471143847,-0.803295262012971,
14.8712646130476));
#274251=CARTESIAN_POINT('Ctrl Pts',(-1.75284094456976,-0.866278403968806,
14.8752033185524));
#274252=CARTESIAN_POINT('Ctrl Pts',(-1.72112737001053,-0.927676426106799,
14.8791420240572));
#274253=CARTESIAN_POINT('Ctrl Pts',(-1.68632081344798,-0.987136319933643,
14.883080729562));
#274254=CARTESIAN_POINT('Ctrl Pts',(-1.65157774273774,-1.04648776114666,
14.8870122510158));
#274255=CARTESIAN_POINT('Ctrl Pts',(-1.61375329407324,-1.10390778401485,
14.8909437724697));
#274256=CARTESIAN_POINT('Ctrl Pts',(-1.573103708595,-1.15907753062711,14.8948752939235));
#274257=CARTESIAN_POINT('Ctrl Pts',(-1.53259476845624,-1.21405639293761,
14.8987932125284));
#274258=CARTESIAN_POINT('Ctrl Pts',(-1.48911974745898,-1.26701818210528,
14.9027111311334));
#274259=CARTESIAN_POINT('Ctrl Pts',(-1.44290681470613,-1.3176251075608,
14.9066290497383));
#274260=CARTESIAN_POINT('Ctrl Pts',(-1.3967635271974,-1.36815576580132,
14.9105410638403));
#274261=CARTESIAN_POINT('Ctrl Pts',(-1.34789084593812,-1.41633824326813,
14.9144530779423));
#274262=CARTESIAN_POINT('Ctrl Pts',(-1.29655866312948,-1.46186580542261,
14.9183650920442));
#274263=CARTESIAN_POINT('Ctrl Pts',(-1.24528691084912,-1.50733977050637,
14.9222725007493));
#274264=CARTESIAN_POINT('Ctrl Pts',(-1.19156177366926,-1.55016470264205,
14.9261799094543));
#274265=CARTESIAN_POINT('Ctrl Pts',(-1.13569037152903,-1.5900702437365,
14.9300873181593));
#274266=CARTESIAN_POINT('Ctrl Pts',(-1.07985403491722,-1.62995073965879,
14.9339922745301));
#274267=CARTESIAN_POINT('Ctrl Pts',(-1.02187450480552,-1.66691519382847,
14.9378972309009));
#274268=CARTESIAN_POINT('Ctrl Pts',(-0.962091173610014,-1.70073412785823,
14.9418021872717));
#274269=CARTESIAN_POINT('Ctrl Pts',(-0.902324852326635,-1.73454343952195,
14.9457060325809));
#274270=CARTESIAN_POINT('Ctrl Pts',(-0.840756176772905,-1.76520876562135,
14.9496098778901));
#274271=CARTESIAN_POINT('Ctrl Pts',(-0.777751097026513,-1.79254546136885,
14.9535137231993));
#274272=CARTESIAN_POINT('Ctrl Pts',(-0.714742328412924,-1.81988375764508,
14.9574177970736));
#274273=CARTESIAN_POINT('Ctrl Pts',(-0.650297440949275,-1.84389284319112,
14.961321870948));
#274274=CARTESIAN_POINT('Ctrl Pts',(-0.584802739996737,-1.86443604215653,
14.9652259448224));
#274275=CARTESIAN_POINT('Ctrl Pts',(-0.519238238204495,-1.88500113499301,
14.9691341794552));
#274276=CARTESIAN_POINT('Ctrl Pts',(-0.452622160354177,-1.90209282208422,
14.9730424140881));
#274277=CARTESIAN_POINT('Ctrl Pts',(-0.385355395870925,-1.91562449840076,
14.976950648721));
#274278=CARTESIAN_POINT('Ctrl Pts',(-0.318048397483143,-1.92916426834537,
14.980861220965));
#274279=CARTESIAN_POINT('Ctrl Pts',(-0.250090424695966,-1.93913971830562,
14.9847717932091));
#274280=CARTESIAN_POINT('Ctrl Pts',(-0.181889169252525,-1.94551595472991,
14.9886823654531));
#274281=CARTESIAN_POINT('Ctrl Pts',(-0.113569959131261,-1.9519032189118,
14.9925997010666));
#274282=CARTESIAN_POINT('Ctrl Pts',(-0.0450071178671433,-1.95467882572272,
14.9965170366801));
#274283=CARTESIAN_POINT('Ctrl Pts',(0.0233908491985165,-1.95385999195791,
15.0004343722936));
#274284=CARTESIAN_POINT('Ctrl Pts',(0.0559642993326093,-1.95347003532689,
15.0022999414288));
#274285=CARTESIAN_POINT('Ctrl Pts',(0.0885004216232417,-1.95226562528409,
15.0041655105639));
#274286=CARTESIAN_POINT('Ctrl Pts',(0.120955691704299,-1.95025273250529,
15.0060310796991));
#274287=CARTESIAN_POINT('Ctrl Pts',(0.189115645727107,-1.94602541660517,
15.009948998304));
#274288=CARTESIAN_POINT('Ctrl Pts',(0.257189004158087,-1.93821219483261,
15.0138669169089));
#274289=CARTESIAN_POINT('Ctrl Pts',(0.324768225269652,-1.92682163156199,
15.0177848355139));
#274290=CARTESIAN_POINT('Ctrl Pts',(0.392245601052069,-1.91544823445053,
15.0216968496158));
#274291=CARTESIAN_POINT('Ctrl Pts',(0.459229836267934,-1.90050827659049,
15.0256088637178));
#274292=CARTESIAN_POINT('Ctrl Pts',(0.52531686116011,-1.88206221878579,
15.0295208778198));
#274293=CARTESIAN_POINT('Ctrl Pts',(0.591326085467733,-1.86363787650062,
15.0334282865248));
#274294=CARTESIAN_POINT('Ctrl Pts',(0.656439725564638,-1.84171576321858,
15.0373356952299));
#274295=CARTESIAN_POINT('Ctrl Pts',(0.720264091534097,-1.81640734375485,
15.0412431039349));
#274296=CARTESIAN_POINT('Ctrl Pts',(0.784048400604479,-1.79111480814346,
15.0451480603057));
#274297=CARTESIAN_POINT('Ctrl Pts',(0.846544584390473,-1.76244036314053,
15.0490530166765));
#274298=CARTESIAN_POINT('Ctrl Pts',(0.907375803439642,-1.73054475565709,
15.0529579730473));
#274299=CARTESIAN_POINT('Ctrl Pts',(0.968189714425392,-1.69865822330327,
15.0568618183565));
#274300=CARTESIAN_POINT('Ctrl Pts',(1.02733916561554,-1.6635525762057,15.0607656636657));
#274301=CARTESIAN_POINT('Ctrl Pts',(1.08447058888164,-1.62543518537366,
15.0646695089749));
#274302=CARTESIAN_POINT('Ctrl Pts',(1.14160535711974,-1.58731556281698,
15.0685735828492));
#274303=CARTESIAN_POINT('Ctrl Pts',(1.19672145505932,-1.54618412159655,
15.0724776567236));
#274304=CARTESIAN_POINT('Ctrl Pts',(1.24949458333011,-1.50229134532178,
15.076381730598));
#274305=CARTESIAN_POINT('Ctrl Pts',(1.3023239544513,-1.45835179041306,15.0802899652308));
#274306=CARTESIAN_POINT('Ctrl Pts',(1.35280499365664,-1.41164534250131,
15.0841981998637));
#274307=CARTESIAN_POINT('Ctrl Pts',(1.40064756563739,-1.36246188822809,
15.0881064344966));
#274308=CARTESIAN_POINT('Ctrl Pts',(1.44851875343587,-1.3132490161225,15.0920170067406));
#274309=CARTESIAN_POINT('Ctrl Pts',(1.49374800925436,-1.26155655936768,
15.0959275789846));
#274310=CARTESIAN_POINT('Ctrl Pts',(1.53608495973236,-1.20770815865591,
15.0998381512287));
#274311=CARTESIAN_POINT('Ctrl Pts',(1.57849513234272,-1.15376662665621,
15.1037554868422));
#274312=CARTESIAN_POINT('Ctrl Pts',(1.61800273271483,-1.09766211072205,
15.1076728224557));
#274313=CARTESIAN_POINT('Ctrl Pts',(1.65440073172345,-1.03974718988459,
15.1115901580692));
#274314=CARTESIAN_POINT('Ctrl Pts',(1.67173470313451,-1.01216612473229,
15.1134557272043));
#274315=CARTESIAN_POINT('Ctrl Pts',(1.68836409592214,-0.984174819782734,
15.1153212963395));
#274316=CARTESIAN_POINT('Ctrl Pts',(1.70427032758818,-0.95581308345433,
15.1171868654746));
#274317=CARTESIAN_POINT('Ctrl Pts',(1.73767531902174,-0.89625004055497,
15.1211047840796));
#274318=CARTESIAN_POINT('Ctrl Pts',(1.7680203237141,-0.834815447264566,
15.1250227026845));
#274319=CARTESIAN_POINT('Ctrl Pts',(1.79509156488076,-0.771856381520527,
15.1289406212894));
#274320=CARTESIAN_POINT('Ctrl Pts',(1.82212200830776,-0.708992198296166,
15.1328526353914));
#274321=CARTESIAN_POINT('Ctrl Pts',(1.84588828711157,-0.644608550526538,
15.1367646494934));
#274322=CARTESIAN_POINT('Ctrl Pts',(1.86622211267582,-0.579077737579145,
15.1406766635954));
#274323=CARTESIAN_POINT('Ctrl Pts',(1.88653200035639,-0.51362407041887,
15.1445840723004));
#274324=CARTESIAN_POINT('Ctrl Pts',(1.90341731483462,-0.447026387783651,
15.1484914810054));
#274325=CARTESIAN_POINT('Ctrl Pts',(1.91675825132557,-0.379675922301295,
15.1523988897104));
#274326=CARTESIAN_POINT('Ctrl Pts',(1.93009081489281,-0.312367726738288,
15.1563038460812));
#274327=CARTESIAN_POINT('Ctrl Pts',(1.93988331776019,-0.244308167001138,
15.160208802452));
#274328=CARTESIAN_POINT('Ctrl Pts',(1.94606650057897,-0.175901038440164,
15.1641137588228));
#274329=CARTESIAN_POINT('Ctrl Pts',(1.95224792412148,-0.107513373485817,
15.168017604132));
#274330=CARTESIAN_POINT('Ctrl Pts',(1.95482202199657,-0.038778825736158,
15.1719214494412));
#274331=CARTESIAN_POINT('Ctrl Pts',(1.953771328377,0.0298930830122975,15.1758252947503));
#274332=CARTESIAN_POINT('Ctrl Pts',(1.95272057324065,0.0985690124136654,
15.1797293686247));
#274333=CARTESIAN_POINT('Ctrl Pts',(1.94804461534932,0.167181803690281,
15.1836334424991));
#274334=CARTESIAN_POINT('Ctrl Pts',(1.93977808374912,0.235323151871166,
15.1875375163734));
#274335=CARTESIAN_POINT('Ctrl Pts',(1.9315027421103,0.303537121550285,15.1914457510063));
#274336=CARTESIAN_POINT('Ctrl Pts',(1.91962924927223,0.37127815611275,15.1953539856392));
#274337=CARTESIAN_POINT('Ctrl Pts',(1.90424386649369,0.438145292022133,
15.199262220272));
#274338=CARTESIAN_POINT('Ctrl Pts',(1.88884928133971,0.505052422808323,
15.2031727925161));
#274339=CARTESIAN_POINT('Ctrl Pts',(1.8699387612331,0.571084141675299,15.2070833647601));
#274340=CARTESIAN_POINT('Ctrl Pts',(1.84764848835242,0.635854593039192,
15.2109939370041));
#274341=CARTESIAN_POINT('Ctrl Pts',(1.82531966424652,0.700737065474845,
15.2149112726176));
#274342=CARTESIAN_POINT('Ctrl Pts',(1.79959960526362,0.764353460855958,
15.2188286082311));
#274343=CARTESIAN_POINT('Ctrl Pts',(1.77067231048155,0.826338652668465,
15.2227459438446));
#274344=CARTESIAN_POINT('Ctrl Pts',(1.75689614381259,0.855858120003723,
15.2246115129798));
#274345=CARTESIAN_POINT('Ctrl Pts',(1.74239324672286,0.885008005651919,
15.226477082115));
#274346=CARTESIAN_POINT('Ctrl Pts',(1.72718699236919,0.913751111293806,
15.2283426512502));
#274347=CARTESIAN_POINT('Ctrl Pts',(1.69525203712161,0.974115075423408,
15.2322605698551));
#274348=CARTESIAN_POINT('Ctrl Pts',(1.66008537049449,1.03292267800056,15.23617848846));
#274349=CARTESIAN_POINT('Ctrl Pts',(1.62186271066378,1.0898061055795,15.2400964070649));
#274350=CARTESIAN_POINT('Ctrl Pts',(1.58369765432871,1.1466038069351,15.2440084211669));
#274351=CARTESIAN_POINT('Ctrl Pts',(1.54248601726698,1.20148268337229,15.2479204352689));
#274352=CARTESIAN_POINT('Ctrl Pts',(1.49844937390611,1.25409946728336,15.2518324493709));
#274353=CARTESIAN_POINT('Ctrl Pts',(1.45446457244015,1.30665430837648,15.2557398580759));
#274354=CARTESIAN_POINT('Ctrl Pts',(1.40766168382216,1.3569519702945,15.2596472667809));
#274355=CARTESIAN_POINT('Ctrl Pts',(1.3583044794147,1.40467965785867,15.2635546754859));
#274356=CARTESIAN_POINT('Ctrl Pts',(1.30897825215094,1.45237739098249,15.2674596318567));
#274357=CARTESIAN_POINT('Ctrl Pts',(1.25710124200206,1.49750800810701,15.2713645882275));
#274358=CARTESIAN_POINT('Ctrl Pts',(1.20297518228468,1.53979437289761,15.2752695445984));
#274359=CARTESIAN_POINT('Ctrl Pts',(1.14886452283863,1.58206870611793,15.2791733899075));
#274360=CARTESIAN_POINT('Ctrl Pts',(1.0925064716272,1.62150009079892,15.2830772352167));
#274361=CARTESIAN_POINT('Ctrl Pts',(1.03423565650843,1.65785180483859,15.2869810805259));
#274362=CARTESIAN_POINT('Ctrl Pts',(0.975961429707744,1.69420564722476,
15.2908851544003));
#274363=CARTESIAN_POINT('Ctrl Pts',(0.915774635395799,1.7274792027814,15.2947892282746));
#274364=CARTESIAN_POINT('Ctrl Pts',(0.85403712532951,1.75748018155509,15.298693302149));
#274365=CARTESIAN_POINT('Ctrl Pts',(0.792233818641646,1.78751313380884,
15.3026015367818));
#274366=CARTESIAN_POINT('Ctrl Pts',(0.72887694127389,1.8142663333555,15.3065097714147));
#274367=CARTESIAN_POINT('Ctrl Pts',(0.66435017186063,1.83759485446296,15.3104180060476));
#274368=CARTESIAN_POINT('Ctrl Pts',(0.59978480740128,1.86093732893204,15.3143285782916));
#274369=CARTESIAN_POINT('Ctrl Pts',(0.534048629164836,1.88085090566003,
15.3182391505356));
#274370=CARTESIAN_POINT('Ctrl Pts',(0.467539689018546,1.89724079631249,
15.3221497227796));
#274371=CARTESIAN_POINT('Ctrl Pts',(0.4009157210687,1.91365903342661,15.3260670583932));
#274372=CARTESIAN_POINT('Ctrl Pts',(0.333516806699145,1.92654132891995,
15.3299843940067));
#274373=CARTESIAN_POINT('Ctrl Pts',(0.265749507083569,1.93584431178875,
15.3339017296202));
#274374=CARTESIAN_POINT('Ctrl Pts',(0.233476402348129,1.94027471025791,
15.3357672987554));
#274375=CARTESIAN_POINT('Ctrl Pts',(0.201119796147725,1.94389408762178,
15.3376328678906));
#274376=CARTESIAN_POINT('Ctrl Pts',(0.168723617269851,1.94670191374421,
15.3394984370257));
#274377=CARTESIAN_POINT('Ctrl Pts',(0.100687761852009,1.95259868486726,
15.3434163556307));
#274378=CARTESIAN_POINT('Ctrl Pts',(0.0322073647878031,1.95493615796299,
15.3473342742356));
#274379=CARTESIAN_POINT('Ctrl Pts',(-0.0363132450550216,1.95366254717481,
15.3512521928405));
#274380=CARTESIAN_POINT('Ctrl Pts',(-0.104730590847791,1.95239085578298,
15.3551642069425));
#274381=CARTESIAN_POINT('Ctrl Pts',(-0.173187541255314,1.94751889014242,
15.3590762210445));
#274382=CARTESIAN_POINT('Ctrl Pts',(-0.241275528199328,1.93904670379342,
15.3629882351465));
#274383=CARTESIAN_POINT('Ctrl Pts',(-0.309283358937298,1.93058449127895,
15.3668956438515));
#274384=CARTESIAN_POINT('Ctrl Pts',(-0.376922602996216,1.91853053588878,
15.3708030525565));
#274385=CARTESIAN_POINT('Ctrl Pts',(-0.443787416982026,1.90293686929662,
15.3747104612615));
#274386=CARTESIAN_POINT('Ctrl Pts',(-0.510610265849078,1.8873529894672,
15.3786154176323));
#274387=CARTESIAN_POINT('Ctrl Pts',(-0.576659170782764,1.868233916762,15.3825203740031));
#274388=CARTESIAN_POINT('Ctrl Pts',(-0.641537667170822,1.84568291469608,
15.3864253303739));
#274389=CARTESIAN_POINT('Ctrl Pts',(-0.70639770393955,1.82313832897667,
15.3903291756831));
#274390=CARTESIAN_POINT('Ctrl Pts',(-0.770087528791084,1.79716391378434,
15.3942330209923));
#274391=CARTESIAN_POINT('Ctrl Pts',(-0.832226799177427,1.76791248503168,
15.3981368663015));
#274392=CARTESIAN_POINT('Ctrl Pts',(-0.89436970773915,1.73865934364501,
15.4020409401758));
#274393=CARTESIAN_POINT('Ctrl Pts',(-0.954961437599773,1.70612901961545,
15.4059450140502));
#274394=CARTESIAN_POINT('Ctrl Pts',(-1.01364421897853,1.67052129508468,
15.4098490879245));
#274395=CARTESIAN_POINT('Ctrl Pts',(-1.07238954140798,1.63487562169647,
15.4137573225574));
#274396=CARTESIAN_POINT('Ctrl Pts',(-1.12922143379994,1.59614625812135,
15.4176655571903));
#274397=CARTESIAN_POINT('Ctrl Pts',(-1.18381008911126,1.55457700771573,
15.4215737918232));
#274398=CARTESIAN_POINT('Ctrl Pts',(-1.2384313952384,1.51298289372021,15.4254843640672));
#274399=CARTESIAN_POINT('Ctrl Pts',(-1.29080641881575,1.46854583067027,
15.4293949363112));
#274400=CARTESIAN_POINT('Ctrl Pts',(-1.34063968711691,1.42154888390342,
15.4333055085552));
#274401=CARTESIAN_POINT('Ctrl Pts',(-1.39055914249879,1.37447065549917,
15.4372228441687));
#274402=CARTESIAN_POINT('Ctrl Pts',(-1.43792772942498,1.32482406278651,
15.4411401797822));
#274403=CARTESIAN_POINT('Ctrl Pts',(-1.48248856441694,1.27292719995018,
15.4450575153957));
#274404=CARTESIAN_POINT('Ctrl Pts',(-1.50370995737396,1.24821213974798,
15.4469230845309));
#274405=CARTESIAN_POINT('Ctrl Pts',(-1.52429517046379,1.2229871747464,15.4487886536661));
#274406=CARTESIAN_POINT('Ctrl Pts',(-1.54421993964279,1.19728892837511,
15.4506542228012));
#274407=CARTESIAN_POINT('Ctrl Pts',(-1.58608153931649,1.14329735174773,
15.454573751685));
#274408=CARTESIAN_POINT('Ctrl Pts',(-1.62519387850404,1.08699708252043,
15.4584932805689));
#274409=CARTESIAN_POINT('Ctrl Pts',(-1.66129293659796,1.02869907106488,
15.4624128094527));
#274410=CARTESIAN_POINT('Ctrl Pts',(-1.69733844138664,0.970487545278667,
15.4663265236771));
#274411=CARTESIAN_POINT('Ctrl Pts',(-1.73037927662693,0.910284569449585,
15.4702402379015));
#274412=CARTESIAN_POINT('Ctrl Pts',(-1.76019243483317,0.848433021726573,
15.4741539521259));
#274413=CARTESIAN_POINT('Ctrl Pts',(-1.78997153867594,0.786652124522111,
15.4780631958731));
#274414=CARTESIAN_POINT('Ctrl Pts',(-1.81653007025389,0.723226832147985,
15.4819724396202));
#274415=CARTESIAN_POINT('Ctrl Pts',(-1.83968996959911,0.658526245305715,
15.4858816833674));
#274416=CARTESIAN_POINT('Ctrl Pts',(-1.86283217533394,0.5938750881677,15.4897879405456));
#274417=CARTESIAN_POINT('Ctrl Pts',(-1.88258073813993,0.527951031449829,
15.4936941977238));
#274418=CARTESIAN_POINT('Ctrl Pts',(-1.89880565127024,0.461143251825488,
15.497600454902));
#274419=CARTESIAN_POINT('Ctrl Pts',(-1.91502356470393,0.394364294185336,
15.5015050268561));
#274420=CARTESIAN_POINT('Ctrl Pts',(-1.92772073426583,0.326702847837579,
15.5054095988102));
#274421=CARTESIAN_POINT('Ctrl Pts',(-1.93681746653096,0.258561600669126,
15.5093141707643));
#274422=CARTESIAN_POINT('Ctrl Pts',(-1.94591515674891,0.19041317772614,
15.5132191538985));
#274423=CARTESIAN_POINT('Ctrl Pts',(-1.95141158638116,0.121785339361323,
15.5171241370327));
#274424=CARTESIAN_POINT('Ctrl Pts',(-1.95327870347652,0.0530877249942702,
15.5210291201669));
#274425=CARTESIAN_POINT('Ctrl Pts',(-1.95377296771858,0.0349020555576315,
15.5220628494032));
#274426=CARTESIAN_POINT('Ctrl Pts',(-1.95401318365985,0.0167115111454544,
15.5230965786395));
#274427=CARTESIAN_POINT('Ctrl Pts',(-1.95399944231052,-0.00147629610118066,
15.5241303078758));
#274428=CARTESIAN_POINT('',(-1.9542420472437,-0.000492779743085885,16.2241302604684));
#274429=CARTESIAN_POINT('Ctrl Pts',(-1.95209224254652,-0.00148915573612675,
15.5241311214624));
#274430=CARTESIAN_POINT('Ctrl Pts',(-1.95364004303147,-0.222253404836076,
15.5366907505006));
#274431=CARTESIAN_POINT('Ctrl Pts',(-1.81714905168899,-1.09243017089523,
15.5863023081303));
#274432=CARTESIAN_POINT('Ctrl Pts',(-0.537454058353606,-2.24624899054346,
15.6729657943525));
#274433=CARTESIAN_POINT('Ctrl Pts',(1.5959832982511,-1.66952948583204,15.7841215801279));
#274434=CARTESIAN_POINT('Ctrl Pts',(2.2681682583395,0.43577992637193,15.8952773659034));
#274435=CARTESIAN_POINT('Ctrl Pts',(0.863660870300283,2.14209740522327,
16.0064331516791));
#274436=CARTESIAN_POINT('Ctrl Pts',(-1.30121699004713,1.89067897567588,
16.1160505996986));
#274437=CARTESIAN_POINT('Ctrl Pts',(-1.9549464319646,0.619678012551105,
16.1886161191264));
#274438=CARTESIAN_POINT('Ctrl Pts',(-1.95705348401711,-0.000483876568800027,
16.2241297099623));
#274439=CARTESIAN_POINT('',(-1.953999187747,0.0017816520611407,16.9241302923036));
#274440=CARTESIAN_POINT('Ctrl Pts',(-1.95399993766937,-0.000493546448478972,
16.2241303078758));
#274441=CARTESIAN_POINT('Ctrl Pts',(-1.95399316389338,-0.027311605637371,
16.2256684463272));
#274442=CARTESIAN_POINT('Ctrl Pts',(-1.95343431063418,-0.0541219966759405,
16.2272065847787));
#274443=CARTESIAN_POINT('Ctrl Pts',(-1.95232417177688,-0.0809093832366167,
16.2287447232302));
#274444=CARTESIAN_POINT('Ctrl Pts',(-1.94949644604203,-0.149141732594158,
16.2326626418351));
#274445=CARTESIAN_POINT('Ctrl Pts',(-1.9430817925214,-0.217361090421165,
16.23658056044));
#274446=CARTESIAN_POINT('Ctrl Pts',(-1.93308041068442,-0.285159825059866,
16.2404984790448));
#274447=CARTESIAN_POINT('Ctrl Pts',(-1.92309410143939,-0.352856383551347,
16.2444104931467));
#274448=CARTESIAN_POINT('Ctrl Pts',(-1.90953186281156,-0.420133094167381,
16.2483225072486));
#274449=CARTESIAN_POINT('Ctrl Pts',(-1.89244585101954,-0.486584731530828,
16.2522345213504));
#274450=CARTESIAN_POINT('Ctrl Pts',(-1.87537995364044,-0.552958139071596,
16.2561419300553));
#274451=CARTESIAN_POINT('Ctrl Pts',(-1.8547986436603,-0.61850792821327,
16.2600493387601));
#274452=CARTESIAN_POINT('Ctrl Pts',(-1.83080528357202,-0.682838204587869,
16.263956747465));
#274453=CARTESIAN_POINT('Ctrl Pts',(-1.80682698198983,-0.747128106548239,
16.2678617038356));
#274454=CARTESIAN_POINT('Ctrl Pts',(-1.77944104973901,-0.810199554116817,
16.2717666602062));
#274455=CARTESIAN_POINT('Ctrl Pts',(-1.74880046681653,-0.871672488531269,
16.2756716165768));
#274456=CARTESIAN_POINT('Ctrl Pts',(-1.71816860193657,-0.933127932297529,
16.2795754618858));
#274457=CARTESIAN_POINT('Ctrl Pts',(-1.68428414405233,-0.992985325723271,
16.2834793071948));
#274458=CARTESIAN_POINT('Ctrl Pts',(-1.64734716498844,-1.0508869197038,
16.2873831525037));
#274459=CARTESIAN_POINT('Ctrl Pts',(-1.61040802331153,-1.10879190374881,
16.2912872263779));
#274460=CARTESIAN_POINT('Ctrl Pts',(-1.57041627235939,-1.16474044764703,
16.295191300252));
#274461=CARTESIAN_POINT('Ctrl Pts',(-1.52761568809808,-1.21840318018159,
16.2990953741261));
#274462=CARTESIAN_POINT('Ctrl Pts',(-1.48476948920408,-1.27212310366054,
16.3030036087587));
#274463=CARTESIAN_POINT('Ctrl Pts',(-1.43910879018471,-1.32355196871172,
16.3069118433913));
#274464=CARTESIAN_POINT('Ctrl Pts',(-1.39091746281637,-1.37239375240215,
16.310820078024));
#274465=CARTESIAN_POINT('Ctrl Pts',(-1.34269731103114,-1.42126474956339,
16.3147306502678));
#274466=CARTESIAN_POINT('Ctrl Pts',(-1.29194388205237,-1.46754525424671,
16.3186412225115));
#274467=CARTESIAN_POINT('Ctrl Pts',(-1.23897561054832,-1.51097830443273,
16.3225517947553));
#274468=CARTESIAN_POINT('Ctrl Pts',(-1.18591572994759,-1.55448647246536,
16.3264691303686));
#274469=CARTESIAN_POINT('Ctrl Pts',(-1.13063375764106,-1.59513706573119,
16.3303864659819));
#274470=CARTESIAN_POINT('Ctrl Pts',(-1.07347795000258,-1.6327158634797,
16.3343038015952));
#274471=CARTESIAN_POINT('Ctrl Pts',(-1.04625840048215,-1.65061217163273,
16.3361693707319));
#274472=CARTESIAN_POINT('Ctrl Pts',(-1.01861423899964,-1.66781246799583,
16.3380349398686));
#274473=CARTESIAN_POINT('Ctrl Pts',(-0.9905848842623,-1.6842973570813,16.3399005090053));
#274474=CARTESIAN_POINT('Ctrl Pts',(-0.931719882550855,-1.71891759837199,
16.3438184276108));
#274475=CARTESIAN_POINT('Ctrl Pts',(-0.870920931029039,-1.75051690307593,
16.3477363462163));
#274476=CARTESIAN_POINT('Ctrl Pts',(-0.808530647667815,-1.77887441709129,
16.3516542648218));
#274477=CARTESIAN_POINT('Ctrl Pts',(-0.746234389642191,-1.8071891948883,
16.3555662789244));
#274478=CARTESIAN_POINT('Ctrl Pts',(-0.682352003608599,-1.83227167611146,
16.3594782930269));
#274479=CARTESIAN_POINT('Ctrl Pts',(-0.617252257112829,-1.85394596768329,
16.3633903071295));
#274480=CARTESIAN_POINT('Ctrl Pts',(-0.552229148933675,-1.8755947433152,
16.3672977158351));
#274481=CARTESIAN_POINT('Ctrl Pts',(-0.485991991036962,-1.89384314303914,
16.3712051245408));
#274482=CARTESIAN_POINT('Ctrl Pts',(-0.418929475171209,-1.90856335887305,
16.3751125332464));
#274483=CARTESIAN_POINT('Ctrl Pts',(-0.351909048504303,-1.92327433613183,
16.3790174896178));
#274484=CARTESIAN_POINT('Ctrl Pts',(-0.284064770837009,-1.93446141676652,
16.3829224459892));
#274485=CARTESIAN_POINT('Ctrl Pts',(-0.215798931230133,-1.94204706979,16.3868274023607));
#274486=CARTESIAN_POINT('Ctrl Pts',(-0.147552515029612,-1.94963056449796,
16.3907312476705));
#274487=CARTESIAN_POINT('Ctrl Pts',(-0.0788852636999524,-1.95361461147805,
16.3946350929803));
#274488=CARTESIAN_POINT('Ctrl Pts',(-0.0102062543892486,-1.95397334484669,
16.3985389382901));
#274489=CARTESIAN_POINT('Ctrl Pts',(0.0584767759899475,-1.95433209921871,
16.4024430121651));
#274490=CARTESIAN_POINT('Ctrl Pts',(0.127171073771154,-1.95106511856314,
16.40634708604));
#274491=CARTESIAN_POINT('Ctrl Pts',(0.195467709344648,-1.94419864587021,
16.410251159915));
#274492=CARTESIAN_POINT('Ctrl Pts',(0.263837131913595,-1.93732485524848,
16.4141593945485));
#274493=CARTESIAN_POINT('Ctrl Pts',(0.331807556064612,-1.9268439660771,
16.418067629182));
#274494=CARTESIAN_POINT('Ctrl Pts',(0.398976332539859,-1.91283399333895,
16.4219758638155));
#274495=CARTESIAN_POINT('Ctrl Pts',(0.466185284310451,-1.89881564089193,
16.4258864360601));
#274496=CARTESIAN_POINT('Ctrl Pts',(0.532591158464872,-1.88126412966425,
16.4297970083048));
#274497=CARTESIAN_POINT('Ctrl Pts',(0.597805386096926,-1.86030769507453,
16.4337075805494));
#274498=CARTESIAN_POINT('Ctrl Pts',(0.663132402315464,-1.83931501614486,
16.4376249161635));
#274499=CARTESIAN_POINT('Ctrl Pts',(0.727263199095435,-1.814905835472,16.4415422517776));
#274500=CARTESIAN_POINT('Ctrl Pts',(0.789828950992136,-1.78725662068285,
16.4454595873917));
#274501=CARTESIAN_POINT('Ctrl Pts',(0.819624900796952,-1.77408911943775,
16.4473251565216));
#274502=CARTESIAN_POINT('Ctrl Pts',(0.849066259865159,-1.76018745667784,
16.4491907256515));
#274503=CARTESIAN_POINT('Ctrl Pts',(0.878115358073886,-1.74557423729693,
16.4510562947813));
#274504=CARTESIAN_POINT('Ctrl Pts',(0.93912194340399,-1.71488472643146,
16.4549742133857));
#274505=CARTESIAN_POINT('Ctrl Pts',(0.998638812367975,-1.68093224684657,
16.45889213199));
#274506=CARTESIAN_POINT('Ctrl Pts',(1.05629462308656,-1.6438849318728,16.4628100505943));
#274507=CARTESIAN_POINT('Ctrl Pts',(1.11386354356105,-1.6068934490901,16.4667220646957));
#274508=CARTESIAN_POINT('Ctrl Pts',(1.16957656159134,-1.56681665120158,
16.4706340787971));
#274509=CARTESIAN_POINT('Ctrl Pts',(1.22308593495831,-1.52386902183461,
16.4745460928984));
#274510=CARTESIAN_POINT('Ctrl Pts',(1.27653231471146,-1.48097195232674,
16.4784535016028));
#274511=CARTESIAN_POINT('Ctrl Pts',(1.32777982013092,-1.43521106985662,
16.4823609103072));
#274512=CARTESIAN_POINT('Ctrl Pts',(1.37651030909296,-1.38684367142112,
16.4862683190116));
#274513=CARTESIAN_POINT('Ctrl Pts',(1.42521021424511,-1.33850662891575,
16.4901732753818));
#274514=CARTESIAN_POINT('Ctrl Pts',(1.47139588819428,-1.28756666126125,
16.494078231752));
#274515=CARTESIAN_POINT('Ctrl Pts',(1.51478406114057,-1.23431975116437,
16.4979831881222));
#274516=CARTESIAN_POINT('Ctrl Pts',(1.5581598890236,-1.1810879911978,16.5018870334308));
#274517=CARTESIAN_POINT('Ctrl Pts',(1.59873948540423,-1.12555097299784,
16.5057908787394));
#274518=CARTESIAN_POINT('Ctrl Pts',(1.63627931118113,-1.0680383962202,16.509694724048));
#274519=CARTESIAN_POINT('Ctrl Pts',(1.67382133486708,-1.01052245215434,
16.5135987979217));
#274520=CARTESIAN_POINT('Ctrl Pts',(1.70832296786059,-0.951031133220822,
16.5175028717955));
#274521=CARTESIAN_POINT('Ctrl Pts',(1.73958453519513,-0.889922269026882,
16.5214069456692));
#274522=CARTESIAN_POINT('Ctrl Pts',(1.77087941947939,-0.828748278189293,
16.5253151803015));
#274523=CARTESIAN_POINT('Ctrl Pts',(1.79892712227707,-0.765953740510865,
16.5292234149338));
#274524=CARTESIAN_POINT('Ctrl Pts',(1.82357487496324,-0.701919279834076,
16.5331316495661));
#274525=CARTESIAN_POINT('Ctrl Pts',(1.8482373700759,-0.637846518573021,
16.5370422218095));
#274526=CARTESIAN_POINT('Ctrl Pts',(1.86949571557832,-0.572532826192455,
16.5409527940529));
#274527=CARTESIAN_POINT('Ctrl Pts',(1.88724697473463,-0.506374225602937,
16.5448633662964));
#274528=CARTESIAN_POINT('Ctrl Pts',(1.90502893485162,-0.440101203124977,
16.5487807019093));
#274529=CARTESIAN_POINT('Ctrl Pts',(1.91929160048593,-0.372980836894027,
16.5526980375223));
#274530=CARTESIAN_POINT('Ctrl Pts',(1.92998326678699,-0.305418712462424,
16.5566153731352));
#274531=CARTESIAN_POINT('Ctrl Pts',(1.93507500379461,-0.273243319067745,
16.5584809422757));
#274532=CARTESIAN_POINT('Ctrl Pts',(1.93935760399372,-0.24096779895067,
16.5603465114162));
#274533=CARTESIAN_POINT('Ctrl Pts',(1.94282963590388,-0.208636060769936,
16.5622120805567));
#274534=CARTESIAN_POINT('Ctrl Pts',(1.95012131870425,-0.140735538741785,
16.5661299991607));
#274535=CARTESIAN_POINT('Ctrl Pts',(1.95386357534866,-0.0723175288653932,
16.5700479177647));
#274536=CARTESIAN_POINT('Ctrl Pts',(1.95399633371426,-0.00378521217720786,
16.5739658363687));
#274537=CARTESIAN_POINT('Ctrl Pts',(1.95412889200624,0.0646438228180311,
16.5778778504698));
#274538=CARTESIAN_POINT('Ctrl Pts',(1.95066274689834,0.133186334766387,
16.5817898645709));
#274539=CARTESIAN_POINT('Ctrl Pts',(1.94358956775634,0.201433840525196,
16.585701878672));
#274540=CARTESIAN_POINT('Ctrl Pts',(1.93652471547539,0.269601002285023,
16.5896092873761));
#274541=CARTESIAN_POINT('Ctrl Pts',(1.92586131293985,0.337473360588105,
16.5935166960802));
#274542=CARTESIAN_POINT('Ctrl Pts',(1.91164305261644,0.404644089766898,
16.5974241047843));
#274543=CARTESIAN_POINT('Ctrl Pts',(1.8974337158352,0.471772661830811,16.6013290611542));
#274544=CARTESIAN_POINT('Ctrl Pts',(1.87967404861689,0.53819999808793,16.605234017524));
#274545=CARTESIAN_POINT('Ctrl Pts',(1.85845915694204,0.60352759835675,16.6091389738939));
#274546=CARTESIAN_POINT('Ctrl Pts',(1.83725030145551,0.668836611224643,
16.6130428192022));
#274547=CARTESIAN_POINT('Ctrl Pts',(1.81258832499304,0.733046041599784,
16.6169466645105));
#274548=CARTESIAN_POINT('Ctrl Pts',(1.78461820633659,0.795772491112862,
16.6208505098187));
#274549=CARTESIAN_POINT('Ctrl Pts',(1.75664645006534,0.858502613179624,
16.6247545836921));
#274550=CARTESIAN_POINT('Ctrl Pts',(1.72536636974336,0.919749133749592,
16.6286586575656));
#274551=CARTESIAN_POINT('Ctrl Pts',(1.69097036370414,0.979150258680603,
16.632562731439));
#274552=CARTESIAN_POINT('Ctrl Pts',(1.65653770019385,1.03861469023553,16.636470966071));
#274553=CARTESIAN_POINT('Ctrl Pts',(1.61898273063974,1.09622937460925,16.6403792007029));
#274554=CARTESIAN_POINT('Ctrl Pts',(1.57854243913934,1.15165957115635,16.6442874353349));
#274555=CARTESIAN_POINT('Ctrl Pts',(1.53807795930705,1.20712292186583,16.648198007578));
#274556=CARTESIAN_POINT('Ctrl Pts',(1.49472503345375,1.26039880276027,16.6521085798211));
#274557=CARTESIAN_POINT('Ctrl Pts',(1.44876060395979,1.31118599459194,16.6560191520642));
#274558=CARTESIAN_POINT('Ctrl Pts',(1.40271667857609,1.36206102332372,16.6599364876767));
#274559=CARTESIAN_POINT('Ctrl Pts',(1.35405258373583,1.41043842576115,16.6638538232893));
#274560=CARTESIAN_POINT('Ctrl Pts',(1.30308107517443,1.45605484495683,16.6677711589019));
#274561=CARTESIAN_POINT('Ctrl Pts',(1.27880670019815,1.47777894329889,16.6696367280454));
#274562=CARTESIAN_POINT('Ctrl Pts',(1.25400947284102,1.49887745941012,16.6715022971888));
#274563=CARTESIAN_POINT('Ctrl Pts',(1.22872551090253,1.51932538281216,16.6733678663323));
#274564=CARTESIAN_POINT('Ctrl Pts',(1.17562616299812,1.56226847065926,16.6772857849413));
#274565=CARTESIAN_POINT('Ctrl Pts',(1.12016746720938,1.60250976330026,16.6812037035503));
#274566=CARTESIAN_POINT('Ctrl Pts',(1.0626556220808,1.63978017699326,16.6851216221593));
#274567=CARTESIAN_POINT('Ctrl Pts',(1.00523045023266,1.67699442227417,16.6890336362654));
#274568=CARTESIAN_POINT('Ctrl Pts',(0.945758679412449,1.71124640897584,
16.6929456503715));
#274569=CARTESIAN_POINT('Ctrl Pts',(0.884579017944451,1.74230765394991,
16.6968576644776));
#274570=CARTESIAN_POINT('Ctrl Pts',(0.823471379894613,1.77333233224509,
16.7007650731867));
#274571=CARTESIAN_POINT('Ctrl Pts',(0.760660280836818,1.80117350717616,
16.7046724818958));
#274572=CARTESIAN_POINT('Ctrl Pts',(0.696511243825545,1.82564730636139,
16.7085798906049));
#274573=CARTESIAN_POINT('Ctrl Pts',(0.632402467480672,1.85010574551144,
16.7124848469797));
#274574=CARTESIAN_POINT('Ctrl Pts',(0.566957877471911,1.87120082625279,
16.7163898033546));
#274575=CARTESIAN_POINT('Ctrl Pts',(0.50056387830783,1.8887963902267,16.7202947597295));
#274576=CARTESIAN_POINT('Ctrl Pts',(0.434188769962954,1.90638694780513,
16.7241986050427));
#274577=CARTESIAN_POINT('Ctrl Pts',(0.366865264016026,1.9204798392786,16.728102450356));
#274578=CARTESIAN_POINT('Ctrl Pts',(0.298994117277603,1.93098899992553,
16.7320062956692));
#274579=CARTESIAN_POINT('Ctrl Pts',(0.231118996770347,1.94149877587037,
16.7359103695476));
#274580=CARTESIAN_POINT('Ctrl Pts',(0.162696658351408,1.94842433167081,
16.739814443426));
#274581=CARTESIAN_POINT('Ctrl Pts',(0.0941354173468984,1.95173116058563,
16.7437185173044));
#274582=CARTESIAN_POINT('Ctrl Pts',(0.0255011073450798,1.95504151374636,
16.7476267519413));
#274583=CARTESIAN_POINT('Ctrl Pts',(-0.0432719083604364,1.95472541954719,
16.7515349865782));
#274584=CARTESIAN_POINT('Ctrl Pts',(-0.111773871146991,1.95080050280105,
16.755443221215));
#274585=CARTESIAN_POINT('Ctrl Pts',(-0.180316806639969,1.9468732384658,
16.759353793463));
#274586=CARTESIAN_POINT('Ctrl Pts',(-0.248587877520439,1.93933290973836,
16.763264365711));
#274587=CARTESIAN_POINT('Ctrl Pts',(-0.316183825544045,1.92824889173165,
16.767174937959));
#274588=CARTESIAN_POINT('Ctrl Pts',(-0.383896681359458,1.91714570381746,
16.7710922735764));
#274589=CARTESIAN_POINT('Ctrl Pts',(-0.450931603554621,1.90248669937868,
16.7750096091938));
#274590=CARTESIAN_POINT('Ctrl Pts',(-0.516897729096984,1.88439187475811,
16.7789269448112));
#274591=CARTESIAN_POINT('Ctrl Pts',(-0.548313052522219,1.87577450086955,
16.78079251391));
#274592=CARTESIAN_POINT('Ctrl Pts',(-0.579486230068499,1.86637860719992,
16.7826580830089));
#274593=CARTESIAN_POINT('Ctrl Pts',(-0.610376663439658,1.85622098057539,
16.7845236521078));
#274594=CARTESIAN_POINT('Ctrl Pts',(-0.675250274141671,1.8348887477971,
16.7884415707076));
#274595=CARTESIAN_POINT('Ctrl Pts',(-0.739132979750126,1.81010914982836,
16.7923594893073));
#274596=CARTESIAN_POINT('Ctrl Pts',(-0.801632660703622,1.78199356825249,
16.7962774079071));
#274597=CARTESIAN_POINT('Ctrl Pts',(-0.86403815145392,1.75392035829038,
16.8001894220039));
#274598=CARTESIAN_POINT('Ctrl Pts',(-0.925064309086546,1.72252134266924,
16.8041014361007));
#274599=CARTESIAN_POINT('Ctrl Pts',(-0.984335501314149,1.68795723312311,
16.8080134501975));
#274600=CARTESIAN_POINT('Ctrl Pts',(-1.04353691685918,1.65343381398339,
16.8119208588974));
#274601=CARTESIAN_POINT('Ctrl Pts',(-1.10098704719417,1.6157529476028,16.8158282675974));
#274602=CARTESIAN_POINT('Ctrl Pts',(-1.15633320473661,1.57512206499165,
16.8197356762973));
#274603=CARTESIAN_POINT('Ctrl Pts',(-1.21164462640057,1.53451668278493,
16.823640632663));
#274604=CARTESIAN_POINT('Ctrl Pts',(-1.26485429900329,1.49096524750577,
16.8275455890287));
#274605=CARTESIAN_POINT('Ctrl Pts',(-1.31563830423586,1.44471860665923,
16.8314505453945));
#274606=CARTESIAN_POINT('Ctrl Pts',(-1.36640786009908,1.39848512418395,
16.8353543906986));
#274607=CARTESIAN_POINT('Ctrl Pts',(-1.41475275512536,1.34955828953871,
16.8392582360028));
#274608=CARTESIAN_POINT('Ctrl Pts',(-1.46038337990191,1.29822817089534,
16.8431620813069));
#274609=CARTESIAN_POINT('Ctrl Pts',(-1.506016676294,1.24689504693826,16.8470661551763));
#274610=CARTESIAN_POINT('Ctrl Pts',(-1.54893506200075,1.1931587289922,16.8509702290457));
#274611=CARTESIAN_POINT('Ctrl Pts',(-1.58888815056499,1.13734359144199,
16.8548743029151));
#274612=CARTESIAN_POINT('Ctrl Pts',(-1.62888381905042,1.08146896902481,
16.8587825375431));
#274613=CARTESIAN_POINT('Ctrl Pts',(-1.66590759656421,1.02351150631851,
16.8626907721711));
#274614=CARTESIAN_POINT('Ctrl Pts',(-1.69975211727543,0.963825056645488,
16.8665990067991));
#274615=CARTESIAN_POINT('Ctrl Pts',(-1.7336168812265,0.90410290703963,16.8705095790383));
#274616=CARTESIAN_POINT('Ctrl Pts',(-1.76429838408449,0.84265015251891,
16.8744201512775));
#274617=CARTESIAN_POINT('Ctrl Pts',(-1.79163626743338,0.779843244003176,
16.8783307235167));
#274618=CARTESIAN_POINT('Ctrl Pts',(-1.81902143189563,0.716927710378318,
16.8822480591255));
#274619=CARTESIAN_POINT('Ctrl Pts',(-1.84305126298817,0.652653808977684,
16.8861653947343));
#274620=CARTESIAN_POINT('Ctrl Pts',(-1.86361465725008,0.587415023031145,
16.8900827303431));
#274621=CARTESIAN_POINT('Ctrl Pts',(-1.87340764881474,0.556346082158551,
16.8919482995232));
#274622=CARTESIAN_POINT('Ctrl Pts',(-1.88241520042632,0.525058482026375,
16.8938138687033));
#274623=CARTESIAN_POINT('Ctrl Pts',(-1.89062940432749,0.493595437065913,
16.8956794378834));
#274624=CARTESIAN_POINT('Ctrl Pts',(-1.91275769521846,0.408836960215565,
16.9007051053724));
#274625=CARTESIAN_POINT('Ctrl Pts',(-1.92919629943473,0.322535927961186,
16.9057307728614));
#274626=CARTESIAN_POINT('Ctrl Pts',(-1.93977379464525,0.235358504430079,
16.9107564403505));
#274627=CARTESIAN_POINT('Ctrl Pts',(-1.94915641929425,0.158028945155436,
16.9152143910015));
#274628=CARTESIAN_POINT('Ctrl Pts',(-1.95392785941723,0.080009888355393,
16.9196723416526));
#274629=CARTESIAN_POINT('Ctrl Pts',(-1.953999187747,0.0017816520611407,
16.9241302923036));
#274630=CARTESIAN_POINT('',(-1.95094246698047,-0.000563023513259459,17.6241303078758));
#274631=CARTESIAN_POINT('Ctrl Pts',(-1.95354848948922,0.00178096791722124,
16.9241303078758));
#274632=CARTESIAN_POINT('Ctrl Pts',(-1.94920835895243,-0.481881162347818,
16.9516986131368));
#274633=CARTESIAN_POINT('Ctrl Pts',(-1.52352210899758,-1.62241065435048,
17.0163188469899));
#274634=CARTESIAN_POINT('Ctrl Pts',(0.389143425895551,-2.27663321337086,
17.1179910094344));
#274635=CARTESIAN_POINT('Ctrl Pts',(2.12392328477785,-0.907436657176078,
17.2291467952101));
#274636=CARTESIAN_POINT('Ctrl Pts',(1.91407877620591,1.29259189050651,17.3403025809855));
#274637=CARTESIAN_POINT('Ctrl Pts',(-0.0482603607290702,2.30914753798913,
17.4514583667612));
#274638=CARTESIAN_POINT('Ctrl Pts',(-1.68087886701888,1.37488706274673,
17.5460676090578));
#274639=CARTESIAN_POINT('Ctrl Pts',(-1.9500108862808,0.36039877990176,17.6036249227627));
#274640=CARTESIAN_POINT('Ctrl Pts',(-1.95094246698047,-0.000563023513259459,
17.6241303078758));
#274641=CARTESIAN_POINT('',(-1.95561232558833,-0.0014928043343815,18.3241303078758));
#274642=CARTESIAN_POINT('Ctrl Pts',(-1.95094246698047,-0.000563023513259459,
17.6241303078758));
#274643=CARTESIAN_POINT('Ctrl Pts',(-1.95169419343994,-0.291836274002239,
17.6406768513546));
#274644=CARTESIAN_POINT('Ctrl Pts',(-1.75385900573772,-1.23437415643904,
17.6942753234252));
#274645=CARTESIAN_POINT('Ctrl Pts',(-0.293683595883821,-2.29090409153417,
17.7849257240878));
#274646=CARTESIAN_POINT('Ctrl Pts',(1.76567929076945,-1.48891520582879,
17.8960815098634));
#274647=CARTESIAN_POINT('Ctrl Pts',(2.20841865870259,0.676296302087549,
18.0072372956388));
#274648=CARTESIAN_POINT('Ctrl Pts',(0.629172532386841,2.22230403884525,
18.1183930814145));
#274649=CARTESIAN_POINT('Ctrl Pts',(-1.41900919557561,1.75790052996025,
18.2240240854933));
#274650=CARTESIAN_POINT('Ctrl Pts',(-1.9509415634449,0.550122899281012,
18.2926031609805));
#274651=CARTESIAN_POINT('Ctrl Pts',(-1.95561232558833,-0.0014928043343815,
18.3241303078758));
#274652=CARTESIAN_POINT('',(-1.95561294514167,0.00149323284471017,19.0241303078758));
#274653=CARTESIAN_POINT('Ctrl Pts',(-1.95561232558833,-0.0014928043343815,
18.3241303078758));
#274654=CARTESIAN_POINT('Ctrl Pts',(-1.95643082468325,-0.0981573186656843,
18.3296550895723));
#274655=CARTESIAN_POINT('Ctrl Pts',(-1.90597210246247,-0.842244556469267,
18.372231799861));
#274656=CARTESIAN_POINT('Ctrl Pts',(-0.950834908026892,-2.10485633930825,
18.4518604387409));
#274657=CARTESIAN_POINT('Ctrl Pts',(1.25304999289457,-1.9401976262354,18.5630162245168));
#274658=CARTESIAN_POINT('Ctrl Pts',(2.30963487490165,0.000858495533198333,
18.6741720102921));
#274659=CARTESIAN_POINT('Ctrl Pts',(1.25162020209078,1.94114985842893,18.7853277960678));
#274660=CARTESIAN_POINT('Ctrl Pts',(-0.952466446087789,2.10412033278024,
18.8964835818432));
#274661=CARTESIAN_POINT('Ctrl Pts',(-1.90620395697742,0.841282306943821,
18.9760844191126));
#274662=CARTESIAN_POINT('Ctrl Pts',(-1.9564186700096,0.0976720719330024,
19.0186333277901));
#274663=CARTESIAN_POINT('Ctrl Pts',(-1.95561294514167,0.00149323284471017,
19.0241303078758));
#274664=CARTESIAN_POINT('Origin',(0.00633869323629521,0.000406037882227006,
19.0313468175703));
#274665=CARTESIAN_POINT('',(-1.47320923595053,1.28365515116407,19.0459999669866));
#274666=CARTESIAN_POINT('Origin',(0.,0.,19.046));
#274667=CARTESIAN_POINT('',(-1.95399969215015,-0.00109684872514523,18.4258696921242));
#274668=CARTESIAN_POINT('Ctrl Pts',(-1.47320923595053,1.28365515116407,
19.0459999669866));
#274669=CARTESIAN_POINT('Ctrl Pts',(-1.42581084117245,1.33805274610456,
19.0419127014303));
#274670=CARTESIAN_POINT('Ctrl Pts',(-1.37545460949829,1.38975536399569,
19.0378254358741));
#274671=CARTESIAN_POINT('Ctrl Pts',(-1.32247459452319,1.43846339781057,
19.0337381703178));
#274672=CARTESIAN_POINT('Ctrl Pts',(-1.26932992720409,1.48732280742145,
19.0296382022763));
#274673=CARTESIAN_POINT('Ctrl Pts',(-1.21354549144269,1.53316875258888,
19.0255382342349));
#274674=CARTESIAN_POINT('Ctrl Pts',(-1.15548848752197,1.57574184281696,
19.0214382661934));
#274675=CARTESIAN_POINT('Ctrl Pts',(-1.0973329601268,1.61838718012091,19.017331340454));
#274676=CARTESIAN_POINT('Ctrl Pts',(-1.03689752655318,1.65774836347391,
19.0132244147147));
#274677=CARTESIAN_POINT('Ctrl Pts',(-0.974575828299399,1.69361092193412,
19.0091174889753));
#274678=CARTESIAN_POINT('Ctrl Pts',(-0.912074034894885,1.72957711481143,
19.0049986951798));
#274679=CARTESIAN_POINT('Ctrl Pts',(-0.847675457691548,1.76202429151714,
19.0008799013843));
#274680=CARTESIAN_POINT('Ctrl Pts',(-0.781795983461404,1.79078503462689,
18.9967611075888));
#274681=CARTESIAN_POINT('Ctrl Pts',(-0.757494229514739,1.80139435582357,
18.9952417585876));
#274682=CARTESIAN_POINT('Ctrl Pts',(-0.732991117784341,1.81150253783091,
18.9937224095863));
#274683=CARTESIAN_POINT('Ctrl Pts',(-0.708307999362921,1.82110290155128,
18.9922030605851));
#274684=CARTESIAN_POINT('Ctrl Pts',(-0.644556172088405,1.84589882560043,
18.9882788694256));
#274685=CARTESIAN_POINT('Ctrl Pts',(-0.579376664124773,1.86739131888459,
18.9843546782661));
#274686=CARTESIAN_POINT('Ctrl Pts',(-0.51314437284014,1.88541742132147,
18.9804304871067));
#274687=CARTESIAN_POINT('Ctrl Pts',(-0.447011520927206,1.90341645985544,
18.9765121876217));
#274688=CARTESIAN_POINT('Ctrl Pts',(-0.379829492183832,1.91795930969979,
18.9725938881367));
#274689=CARTESIAN_POINT('Ctrl Pts',(-0.311991705435798,1.92893161510181,
18.9686755886518));
#274690=CARTESIAN_POINT('Ctrl Pts',(-0.24423390183834,1.93989098376757,
18.9647619089806));
#274691=CARTESIAN_POINT('Ctrl Pts',(-0.175822357499235,1.94728809182404,
18.9608482293093));
#274692=CARTESIAN_POINT('Ctrl Pts',(-0.107162381747267,1.95105925690079,
18.9569345496381));
#274693=CARTESIAN_POINT('Ctrl Pts',(-0.0385456533880884,1.95482804660447,
18.9530233351067));
#274694=CARTESIAN_POINT('Ctrl Pts',(0.0303187076642368,1.95497539760276,
18.9491121205753));
#274695=CARTESIAN_POINT('Ctrl Pts',(0.0990200711887029,1.95148943771207,
18.9452009060439));
#274696=CARTESIAN_POINT('Ctrl Pts',(0.167701515547227,1.94800448853515,
18.9412908255239));
#274697=CARTESIAN_POINT('Ctrl Pts',(0.236219566972794,1.94088834477837,
18.937380745004));
#274698=CARTESIAN_POINT('Ctrl Pts',(0.304165193452798,1.93018121819994,
18.933470664484));
#274699=CARTESIAN_POINT('Ctrl Pts',(0.372114216289481,1.9194735564109,18.9295603885132));
#274700=CARTESIAN_POINT('Ctrl Pts',(0.43949027364022,1.90517463419125,18.9256501125424));
#274701=CARTESIAN_POINT('Ctrl Pts',(0.505892824047464,1.88737607555497,
18.9217398365716));
#274702=CARTESIAN_POINT('Ctrl Pts',(0.572364360708856,1.86955902582336,
18.9178254981772));
#274703=CARTESIAN_POINT('Ctrl Pts',(0.637859897647259,1.84823521057338,
18.9139111597827));
#274704=CARTESIAN_POINT('Ctrl Pts',(0.701993375156466,1.82354635291687,
18.9099968213883));
#274705=CARTESIAN_POINT('Ctrl Pts',(0.766164417825701,1.79884303415636,
18.9060801902327));
#274706=CARTESIAN_POINT('Ctrl Pts',(0.828971365391464,1.77077094949238,
18.902163559077));
#274707=CARTESIAN_POINT('Ctrl Pts',(0.890050050998562,1.73951915962931,
18.8982469279214));
#274708=CARTESIAN_POINT('Ctrl Pts',(0.951231951283219,1.70821455848875,
18.8943236781914));
#274709=CARTESIAN_POINT('Ctrl Pts',(1.01067933662763,1.67371977322852,18.8904004284614));
#274710=CARTESIAN_POINT('Ctrl Pts',(1.06805520883447,1.63626833706503,18.8864771787315));
#274711=CARTESIAN_POINT('Ctrl Pts',(1.09430899175348,1.61913148428662,18.8846819964922));
#274712=CARTESIAN_POINT('Ctrl Pts',(1.12012948878298,1.60137615623275,18.8828868142529));
#274713=CARTESIAN_POINT('Ctrl Pts',(1.14548677551538,1.58302749411353,18.8810916320137));
#274714=CARTESIAN_POINT('Ctrl Pts',(1.20092748359473,1.54291031474283,18.8771666783888));
#274715=CARTESIAN_POINT('Ctrl Pts',(1.25436369953291,1.49980083127761,18.873241724764));
#274716=CARTESIAN_POINT('Ctrl Pts',(1.30545543201943,1.45392644759319,18.8693167711392));
#274717=CARTESIAN_POINT('Ctrl Pts',(1.35647230034779,1.40811928314266,18.8653975687061));
#274718=CARTESIAN_POINT('Ctrl Pts',(1.40515114237818,1.35955558495761,18.861478366273));
#274719=CARTESIAN_POINT('Ctrl Pts',(1.45118286073189,1.3085046063037,18.8575591638399));
#274720=CARTESIAN_POINT('Ctrl Pts',(1.49716272292246,1.25751113816586,18.8536443765102));
#274721=CARTESIAN_POINT('Ctrl Pts',(1.54050105766794,1.20403631694402,18.8497295891806));
#274722=CARTESIAN_POINT('Ctrl Pts',(1.58092496836611,1.14838680086311,18.845814801851));
#274723=CARTESIAN_POINT('Ctrl Pts',(1.6213247329099,1.09277052554944,18.8419023529161));
#274724=CARTESIAN_POINT('Ctrl Pts',(1.65881323989536,1.03498252806685,18.8379899039812));
#274725=CARTESIAN_POINT('Ctrl Pts',(1.69315831477619,0.975361943641562,
18.8340774550464));
#274726=CARTESIAN_POINT('Ctrl Pts',(1.72749453418746,0.915756731675726,
18.83016601489));
#274727=CARTESIAN_POINT('Ctrl Pts',(1.75868868634086,0.854320295252809,
18.8262545747335));
#274728=CARTESIAN_POINT('Ctrl Pts',(1.78655328498693,0.791418574398155,
18.8223431345771));
#274729=CARTESIAN_POINT('Ctrl Pts',(1.81442015830947,0.728511718674476,
18.8184313751173));
#274730=CARTESIAN_POINT('Ctrl Pts',(1.83895674239513,0.664139789928554,
18.8145196156575));
#274731=CARTESIAN_POINT('Ctrl Pts',(1.86002339623353,0.598689373100854,
18.8106078561977));
#274732=CARTESIAN_POINT('Ctrl Pts',(1.88111288826538,0.533168001991905,
18.8066918560303));
#274733=CARTESIAN_POINT('Ctrl Pts',(1.89872479260933,0.466566276707873,
18.8027758558629));
#274734=CARTESIAN_POINT('Ctrl Pts',(1.91276944054903,0.39928569634003,18.7988598556955));
#274735=CARTESIAN_POINT('Ctrl Pts',(1.9268226857782,0.331963930844073,18.7949414583881));
#274736=CARTESIAN_POINT('Ctrl Pts',(1.93730425376752,0.263962967355806,
18.7910230610807));
#274737=CARTESIAN_POINT('Ctrl Pts',(1.94417613596757,0.195691472308317,
18.7871046637733));
#274738=CARTESIAN_POINT('Ctrl Pts',(1.95105987668993,0.127302163971462,
18.7831795046501));
#274739=CARTESIAN_POINT('Ctrl Pts',(1.95432147595897,0.0586418813374403,
18.7792543455269));
#274740=CARTESIAN_POINT('Ctrl Pts',(1.95397502420171,-0.00987951395203889,
18.7753291864037));
#274741=CARTESIAN_POINT('Ctrl Pts',(1.953817649304,-0.0410051969617995,
18.7735461920832));
#274742=CARTESIAN_POINT('Ctrl Pts',(1.95291649744364,-0.0721022797467864,
18.7717631977627));
#274743=CARTESIAN_POINT('Ctrl Pts',(1.95127640791245,-0.103132826608546,
18.7699802034423));
#274744=CARTESIAN_POINT('Ctrl Pts',(1.9476772661379,-0.171228705140731,
18.7660674601313));
#274745=CARTESIAN_POINT('Ctrl Pts',(1.94050187012511,-0.239274528996423,
18.7621547168202));
#274746=CARTESIAN_POINT('Ctrl Pts',(1.92975404797098,-0.306863673867736,
18.7582419735092));
#274747=CARTESIAN_POINT('Ctrl Pts',(1.91902265009754,-0.374349532410877,
18.7543352094555));
#274748=CARTESIAN_POINT('Ctrl Pts',(1.90472973637868,-0.441379613629611,
18.7504284454018));
#274749=CARTESIAN_POINT('Ctrl Pts',(1.88693106645239,-0.507550145755895,
18.7465216813482));
#274750=CARTESIAN_POINT('Ctrl Pts',(1.86915376980208,-0.573641217953406,
18.7426196086757));
#274751=CARTESIAN_POINT('Ctrl Pts',(1.8478792046855,-0.638874316687479,
18.7387175360033));
#274752=CARTESIAN_POINT('Ctrl Pts',(1.82321424775281,-0.702855466501586,
18.7348154633308));
#274753=CARTESIAN_POINT('Ctrl Pts',(1.79856510893852,-0.766795583955237,
18.7309158931338));
#274754=CARTESIAN_POINT('Ctrl Pts',(1.77053006806591,-0.829484885686202,
18.7270163229367));
#274755=CARTESIAN_POINT('Ctrl Pts',(1.73926546778139,-0.89054569370874,
18.7231167527396));
#274756=CARTESIAN_POINT('Ctrl Pts',(1.70801011323798,-0.951588444490264,
18.7192183357451));
#274757=CARTESIAN_POINT('Ctrl Pts',(1.67352731978124,-1.01100321848788,
18.7153199187506));
#274758=CARTESIAN_POINT('Ctrl Pts',(1.63602030203372,-1.06843510394105,
18.7114215017561));
#274759=CARTESIAN_POINT('Ctrl Pts',(1.59851141418806,-1.12586985294531,
18.7075228903867));
#274760=CARTESIAN_POINT('Ctrl Pts',(1.55797827466797,-1.1813211053985,18.7036242790173));
#274761=CARTESIAN_POINT('Ctrl Pts',(1.51466751281931,-1.23446276801277,
18.6997256676478));
#274762=CARTESIAN_POINT('Ctrl Pts',(1.47131074123148,-1.28766088389482,
18.695822914719));
#274763=CARTESIAN_POINT('Ctrl Pts',(1.42517077092788,-1.33854413022793,
18.6919201617903));
#274764=CARTESIAN_POINT('Ctrl Pts',(1.37653397585288,-1.38682018060117,
18.6880174088615));
#274765=CARTESIAN_POINT('Ctrl Pts',(1.32786825384278,-1.43512494335511,
18.6841123347542));
#274766=CARTESIAN_POINT('Ctrl Pts',(1.27670312001706,-1.48081909566736,
18.680207260647));
#274767=CARTESIAN_POINT('Ctrl Pts',(1.22335908468114,-1.52364974647329,
18.6763021865397));
#274768=CARTESIAN_POINT('Ctrl Pts',(1.16992237404742,-1.56655480753509,
18.6723903280956));
#274769=CARTESIAN_POINT('Ctrl Pts',(1.11429960723626,-1.60658615033506,
18.6684784696515));
#274770=CARTESIAN_POINT('Ctrl Pts',(1.05684064036482,-1.64353395488906,
18.6645666112073));
#274771=CARTESIAN_POINT('Ctrl Pts',(1.02894326166577,-1.66147278936285,
18.6626673324285));
#274772=CARTESIAN_POINT('Ctrl Pts',(1.00061341462232,-1.67868543812271,
18.6607680536497));
#274773=CARTESIAN_POINT('Ctrl Pts',(0.971893015866229,-1.6951519004828,
18.6588687748708));
#274774=CARTESIAN_POINT('Ctrl Pts',(0.912626357980133,-1.72913165820057,
18.6549494732423));
#274775=CARTESIAN_POINT('Ctrl Pts',(0.851458535485548,-1.76006659392973,
18.6510301716139));
#274776=CARTESIAN_POINT('Ctrl Pts',(0.788734919209241,-1.78773969783635,
18.6471108699854));
#274777=CARTESIAN_POINT('Ctrl Pts',(0.72610563165396,-1.81537118474679,
18.6431974625118));
#274778=CARTESIAN_POINT('Ctrl Pts',(0.661925640058772,-1.8397503786959,
18.6392840550382));
#274779=CARTESIAN_POINT('Ctrl Pts',(0.596565939931027,-1.86070553267147,
18.6353706475646));
#274780=CARTESIAN_POINT('Ctrl Pts',(0.531283030199932,-1.88163606666588,
18.6314618379106));
#274781=CARTESIAN_POINT('Ctrl Pts',(0.46482363052957,-1.89915040096931,
18.6275530282567));
#274782=CARTESIAN_POINT('Ctrl Pts',(0.397578104515613,-1.913125100669,18.6236442186027));
#274783=CARTESIAN_POINT('Ctrl Pts',(0.330374695937586,-1.92709104768945,
18.6197378571271));
#274784=CARTESIAN_POINT('Ctrl Pts',(0.262386617923052,-1.93752165815829,
18.6158314956514));
#274785=CARTESIAN_POINT('Ctrl Pts',(0.194017255254432,-1.94434392653757,
18.6119251341758));
#274786=CARTESIAN_POINT('Ctrl Pts',(0.125667303993895,-1.95116425794054,
18.6080198817931));
#274787=CARTESIAN_POINT('Ctrl Pts',(0.0569367718664548,-1.9543782322859,
18.6041146294104));
#274788=CARTESIAN_POINT('Ctrl Pts',(-0.0117647544452431,-1.95396458272734,
18.6002093770277));
#274789=CARTESIAN_POINT('Ctrl Pts',(-0.0804702979021206,-1.9535509089817,
18.5963038962954));
#274790=CARTESIAN_POINT('Ctrl Pts',(-0.149146340665118,-1.94950919572022,
18.5923984155631));
#274791=CARTESIAN_POINT('Ctrl Pts',(-0.217384028907364,-1.9418702799044,
18.5884929348308));
#274792=CARTESIAN_POINT('Ctrl Pts',(-0.28569416176618,-1.93422325422523,
18.5845833078406));
#274793=CARTESIAN_POINT('Ctrl Pts',(-0.353564521924234,-1.92297145924986,
18.5806736808504));
#274794=CARTESIAN_POINT('Ctrl Pts',(-0.420593115150671,-1.90819742990285,
18.5767640538602));
#274795=CARTESIAN_POINT('Ctrl Pts',(-0.487661725079951,-1.89341458032087,
18.5728520927858));
#274796=CARTESIAN_POINT('Ctrl Pts',(-0.553887094051403,-1.87510544224461,
18.5689401317114));
#274797=CARTESIAN_POINT('Ctrl Pts',(-0.61888186044793,-1.85340261217268,
18.565028170637));
#274798=CARTESIAN_POINT('Ctrl Pts',(-0.683988474229122,-1.83166243440465,
18.5611094775957));
#274799=CARTESIAN_POINT('Ctrl Pts',(-0.747859801662094,-1.80651708861102,
18.5571907845544));
#274800=CARTESIAN_POINT('Ctrl Pts',(-0.81012875650471,-1.77814718116475,
18.5532720915131));
#274801=CARTESIAN_POINT('Ctrl Pts',(-0.839338956356765,-1.76483893360568,
18.5514338431085));
#274802=CARTESIAN_POINT('Ctrl Pts',(-0.868196910416859,-1.75082177012659,
18.5495955947039));
#274803=CARTESIAN_POINT('Ctrl Pts',(-0.896666821613518,-1.73611768351616,
18.5477573462993));
#274804=CARTESIAN_POINT('Ctrl Pts',(-0.957361315609888,-1.70477030451191,
18.5438384174349));
#274805=CARTESIAN_POINT('Ctrl Pts',(-1.01652969689966,-1.67017445412417,
18.5399194885705));
#274806=CARTESIAN_POINT('Ctrl Pts',(-1.0738023578566,-1.63250252565245,
18.536000559706));
#274807=CARTESIAN_POINT('Ctrl Pts',(-1.13098907038735,-1.59488713101221,
18.5320875119333));
#274808=CARTESIAN_POINT('Ctrl Pts',(-1.18628530129918,-1.55420508805625,
18.5281744641605));
#274809=CARTESIAN_POINT('Ctrl Pts',(-1.23934556821764,-1.51067486989732,
18.5242614163877));
#274810=CARTESIAN_POINT('Ctrl Pts',(-1.2923437780468,-1.46719556287761,
18.5203529451534));
#274811=CARTESIAN_POINT('Ctrl Pts',(-1.34311083921788,-1.42087500670096,
18.5164444739192));
#274812=CARTESIAN_POINT('Ctrl Pts',(-1.39133134932632,-1.3719741529569,
18.5125360026849));
#274813=CARTESIAN_POINT('Ctrl Pts',(-1.43952182110403,-1.32310376135466,
18.5086299661812));
#274814=CARTESIAN_POINT('Ctrl Pts',(-1.48516854423479,-1.27165661002935,
18.5047239296776));
#274815=CARTESIAN_POINT('Ctrl Pts',(-1.52799142088666,-1.21793194296593,
18.5008178931739));
#274816=CARTESIAN_POINT('Ctrl Pts',(-1.57080229168217,-1.16422233819366,
18.4969129517698));
#274817=CARTESIAN_POINT('Ctrl Pts',(-1.61079058138535,-1.10823686957285,
18.4930080103657));
#274818=CARTESIAN_POINT('Ctrl Pts',(-1.64771629625348,-1.05030805341134,
18.4891030689616));
#274819=CARTESIAN_POINT('Ctrl Pts',(-1.68464430805058,-0.992375633842908,
18.4851978846543));
#274820=CARTESIAN_POINT('Ctrl Pts',(-1.71850910468994,-0.932500042688802,
18.481292700347));
#274821=CARTESIAN_POINT('Ctrl Pts',(-1.74911486508527,-0.871041439162183,
18.4773875160397));
#274822=CARTESIAN_POINT('Ctrl Pts',(-1.77975331029039,-0.809517202148931,
18.473478161269));
#274823=CARTESIAN_POINT('Ctrl Pts',(-1.80712555385027,-0.746407019901457,
18.4695688064982));
#274824=CARTESIAN_POINT('Ctrl Pts',(-1.8310829286302,-0.682093328276309,
18.4656594517275));
#274825=CARTESIAN_POINT('Ctrl Pts',(-1.85505468953874,-0.617741017017433,
18.461747749434));
#274826=CARTESIAN_POINT('Ctrl Pts',(-1.87560735349436,-0.552184227264455,
18.4578360471406));
#274827=CARTESIAN_POINT('Ctrl Pts',(-1.89264224981713,-0.485820248864909,
18.4539243448471));
#274828=CARTESIAN_POINT('Ctrl Pts',(-1.90970656556094,-0.419341659270481,
18.4500058870082));
#274829=CARTESIAN_POINT('Ctrl Pts',(-1.92324089160671,-0.352053580509883,
18.4460874291693));
#274830=CARTESIAN_POINT('Ctrl Pts',(-1.93319788949831,-0.284362304181293,
18.4421689713304));
#274831=CARTESIAN_POINT('Ctrl Pts',(-1.93787600823236,-0.252558759440938,
18.4403279534629));
#274832=CARTESIAN_POINT('Ctrl Pts',(-1.9417652074676,-0.22066626547931,
18.4384869355955));
#274833=CARTESIAN_POINT('Ctrl Pts',(-1.94486454898216,-0.188727014792367,
18.436645917728));
#274834=CARTESIAN_POINT('Ctrl Pts',(-1.95091178404236,-0.126409210948082,
18.4330538425267));
#274835=CARTESIAN_POINT('Ctrl Pts',(-1.95396449707421,-0.0637957113532713,
18.4294617673255));
#274836=CARTESIAN_POINT('Ctrl Pts',(-1.95399969215015,-0.00109684872514523,
18.4258696921242));
#274837=CARTESIAN_POINT('',(-1.95134777043173,-0.00103525977712474,17.7258696921242));
#274838=CARTESIAN_POINT('Ctrl Pts',(-1.95645114732722,-0.00108114071341489,
18.4258687145873));
#274839=CARTESIAN_POINT('Ctrl Pts',(-1.952565755839,0.583424133764486,18.392423972777));
#274840=CARTESIAN_POINT('Ctrl Pts',(-1.3640428686297,1.82206153794779,18.3219420881096));
#274841=CARTESIAN_POINT('Ctrl Pts',(0.742083973805834,2.18684491535976,
18.2144230605852));
#274842=CARTESIAN_POINT('Ctrl Pts',(2.23963755709721,0.563107605485782,
18.1033116320136));
#274843=CARTESIAN_POINT('Ctrl Pts',(1.68811978691671,-1.57585659307529,
17.9922002034423));
#274844=CARTESIAN_POINT('Ctrl Pts',(-0.407879737212788,-2.27303301670108,
17.8810887748708));
#274845=CARTESIAN_POINT('Ctrl Pts',(-1.78439856374539,-1.16847809341345,
17.7923119377648));
#274846=CARTESIAN_POINT('Ctrl Pts',(-1.95259122315044,-0.259714155535947,
17.7405722435159));
#274847=CARTESIAN_POINT('Ctrl Pts',(-1.95134777043173,-0.00103525977712474,
17.7258696921242));
#274848=CARTESIAN_POINT('',(-1.95399929689543,0.00165762847613276,17.0258696715309));
#274849=CARTESIAN_POINT('Ctrl Pts',(-1.95134777043173,-0.00103525977712474,
17.7258696921242));
#274850=CARTESIAN_POINT('Ctrl Pts',(-1.94945884600364,0.391922894462037,
17.7035351006588));
#274851=CARTESIAN_POINT('Ctrl Pts',(-1.64362033274317,1.43922352125159,
17.6441633663363));
#274852=CARTESIAN_POINT('Ctrl Pts',(0.0645653811787344,2.30843805668281,
17.5477544891566));
#274853=CARTESIAN_POINT('Ctrl Pts',(1.97418123894165,1.19819262885406,17.4366430605851));
#274854=CARTESIAN_POINT('Ctrl Pts',(2.07759448914051,-1.00829461665569,
17.3255316320136));
#274855=CARTESIAN_POINT('Ctrl Pts',(0.280191065138641,-2.29228039229647,
17.2144202034423));
#274856=CARTESIAN_POINT('Ctrl Pts',(-1.56609907861032,-1.56118274288362,
17.1145328901458));
#274857=CARTESIAN_POINT('Ctrl Pts',(-1.94902844534429,-0.451721645161182,
17.0516827197064));
#274858=CARTESIAN_POINT('Ctrl Pts',(-1.95268185958658,0.00165614916274905,
17.0258696921242));
#274859=CARTESIAN_POINT('',(-1.95399999965015,3.69758055297757E-5,16.3258696921745));
#274860=CARTESIAN_POINT('Ctrl Pts',(-1.95399929689543,0.00165762847613276,
17.0258696715309));
#274861=CARTESIAN_POINT('Ctrl Pts',(-1.95392944244911,0.0840014956052798,
17.0211845557084));
#274862=CARTESIAN_POINT('Ctrl Pts',(-1.9486506380379,0.166119521674429,
17.0164994398858));
#274863=CARTESIAN_POINT('Ctrl Pts',(-1.93827107857988,0.24742923420808,
17.0118143240633));
#274864=CARTESIAN_POINT('Ctrl Pts',(-1.92774884814808,0.329856579519055,
17.0070648095503));
#274865=CARTESIAN_POINT('Ctrl Pts',(-1.91198475580092,0.411453222331514,
17.0023152950372));
#274866=CARTESIAN_POINT('Ctrl Pts',(-1.89114037462833,0.491634095085596,
16.9975657805242));
#274867=CARTESIAN_POINT('Ctrl Pts',(-1.88328682180889,0.521843901463097,
16.9957763024493));
#274868=CARTESIAN_POINT('Ctrl Pts',(-1.87471257563528,0.55185295002992,
16.9939868243743));
#274869=CARTESIAN_POINT('Ctrl Pts',(-1.86542801643474,0.581630738097954,
16.9921973462993));
#274870=CARTESIAN_POINT('Ctrl Pts',(-1.84509919017844,0.646830115565059,
16.9882792293387));
#274871=CARTESIAN_POINT('Ctrl Pts',(-1.82130773338751,0.711091673200386,
16.9843611123781));
#274872=CARTESIAN_POINT('Ctrl Pts',(-1.79415901651518,0.774021591079526,
16.9804429954175));
#274873=CARTESIAN_POINT('Ctrl Pts',(-1.76705118104201,0.836856747091851,
16.9765307784817));
#274874=CARTESIAN_POINT('Ctrl Pts',(-1.73659631207985,0.898363795000412,
16.972618561546));
#274875=CARTESIAN_POINT('Ctrl Pts',(-1.70294935694726,0.958164645388731,
16.9687063446102));
#274876=CARTESIAN_POINT('Ctrl Pts',(-1.66934196849415,1.01789517378,16.9647987281927));
#274877=CARTESIAN_POINT('Ctrl Pts',(-1.63255018881405,1.07592306269883,
16.9608911117753));
#274878=CARTESIAN_POINT('Ctrl Pts',(-1.59277603073726,1.13189244891414,
16.9569834953578));
#274879=CARTESIAN_POINT('Ctrl Pts',(-1.5530268014057,1.18782675590623,16.9530783280676));
#274880=CARTESIAN_POINT('Ctrl Pts',(-1.51029918592256,1.24170471945634,
16.9491731607774));
#274881=CARTESIAN_POINT('Ctrl Pts',(-1.46483904964484,1.29319857664459,
16.9452679934872));
#274882=CARTESIAN_POINT('Ctrl Pts',(-1.41939181376794,1.34467782121942,
16.9413639343816));
#274883=CARTESIAN_POINT('Ctrl Pts',(-1.37121392181844,1.39377393392444,
16.9374598752761));
#274884=CARTESIAN_POINT('Ctrl Pts',(-1.3205909817362,1.44019285477918,16.9335558161705));
#274885=CARTESIAN_POINT('Ctrl Pts',(-1.26996504484116,1.48661452357422,
16.9296515259496));
#274886=CARTESIAN_POINT('Ctrl Pts',(-1.21689413671791,1.53035835532792,
16.9257472357288));
#274887=CARTESIAN_POINT('Ctrl Pts',(-1.16169876999093,1.57116898130072,
16.9218429455079));
#274888=CARTESIAN_POINT('Ctrl Pts',(-1.10644461140303,1.61202307709334,
16.9179344965958));
#274889=CARTESIAN_POINT('Ctrl Pts',(-1.04906187445869,1.64993743891098,
16.9140260476837));
#274890=CARTESIAN_POINT('Ctrl Pts',(-0.989901207589153,1.68469926076245,
16.9101175987716));
#274891=CARTESIAN_POINT('Ctrl Pts',(-0.930705129006683,1.71948188994625,
16.9062068103851));
#274892=CARTESIAN_POINT('Ctrl Pts',(-0.869729439220855,1.75110799716119,
16.9022960219985));
#274893=CARTESIAN_POINT('Ctrl Pts',(-0.807348105016895,1.77941143003119,
16.8983852336119));
#274894=CARTESIAN_POINT('Ctrl Pts',(-0.74485905837139,1.80776373379978,
16.8944676925553));
#274895=CARTESIAN_POINT('Ctrl Pts',(-0.680959980998942,1.83278173348723,
16.8905501514987));
#274896=CARTESIAN_POINT('Ctrl Pts',(-0.616042625149195,1.85434826394593,
16.8866326104421));
#274897=CARTESIAN_POINT('Ctrl Pts',(-0.585404645907629,1.86452666545131,
16.8847837128707));
#274898=CARTESIAN_POINT('Ctrl Pts',(-0.554540039311765,1.87393701832972,
16.8829348152994));
#274899=CARTESIAN_POINT('Ctrl Pts',(-0.523490742810242,1.88257096604404,
16.881085917728));
#274900=CARTESIAN_POINT('Ctrl Pts',(-0.457692198149527,1.90086771535206,
16.8771678009547));
#274901=CARTESIAN_POINT('Ctrl Pts',(-0.390802818928335,1.9157469518832,
16.8732496841813));
#274902=CARTESIAN_POINT('Ctrl Pts',(-0.32321059275063,1.92708352510569,
16.869331567408));
#274903=CARTESIAN_POINT('Ctrl Pts',(-0.255720149132896,1.93840302734963,
16.8654193506616));
#274904=CARTESIAN_POINT('Ctrl Pts',(-0.187529440249675,1.946190372983,16.8615071339152));
#274905=CARTESIAN_POINT('Ctrl Pts',(-0.119040137275175,1.95037059189209,
16.8575949171688));
#274906=CARTESIAN_POINT('Ctrl Pts',(-0.050631373407831,1.954545895127,16.853687300943));
#274907=CARTESIAN_POINT('Ctrl Pts',(0.0180747985636558,1.9551224660021,
16.8497796847171));
#274908=CARTESIAN_POINT('Ctrl Pts',(0.0866698429625813,1.95207692940643,
16.8458720684912));
#274909=CARTESIAN_POINT('Ctrl Pts',(0.155221894890366,1.94903330162423,
16.8419669013938));
#274910=CARTESIAN_POINT('Ctrl Pts',(0.223662467116329,1.94237209146302,
16.8380617342965));
#274911=CARTESIAN_POINT('Ctrl Pts',(0.291582837074114,1.93212200679041,
16.8341565671991));
#274912=CARTESIAN_POINT('Ctrl Pts',(0.359483932985028,1.92187483082711,
16.8302525082873));
#274913=CARTESIAN_POINT('Ctrl Pts',(0.42686463353449,1.90804087547645,16.8263484493754));
#274914=CARTESIAN_POINT('Ctrl Pts',(0.49332296545365,1.89070051879086,16.8224443904636));
#274915=CARTESIAN_POINT('Ctrl Pts',(0.559785231609485,1.87335913558135,
16.8185401004372));
#274916=CARTESIAN_POINT('Ctrl Pts',(0.625324545432984,1.85251106559555,
16.8146358104108));
#274917=CARTESIAN_POINT('Ctrl Pts',(0.689552498035929,1.82828699947585,
16.8107315203843));
#274918=CARTESIAN_POINT('Ctrl Pts',(0.753848863651919,1.80403713086231,
16.8068230716663));
#274919=CARTESIAN_POINT('Ctrl Pts',(0.816830619331629,1.77640426357738,
16.8029146229483));
#274920=CARTESIAN_POINT('Ctrl Pts',(0.878128760066116,1.74556749532774,
16.7990061742303));
#274921=CARTESIAN_POINT('Ctrl Pts',(0.939463591938396,1.71471226915915,
16.7950953860379));
#274922=CARTESIAN_POINT('Ctrl Pts',(0.999112376041192,1.68064956929513,
16.7911845978456));
#274923=CARTESIAN_POINT('Ctrl Pts',(1.05673264645341,1.64360339313339,16.7872738096532));
#274924=CARTESIAN_POINT('Ctrl Pts',(1.11445240851875,1.60649325015438,16.7833562687889));
#274925=CARTESIAN_POINT('Ctrl Pts',(1.17013626735915,1.56638963661305,16.7794387279245));
#274926=CARTESIAN_POINT('Ctrl Pts',(1.22347325827623,1.52355806790649,16.7755211870602));
#274927=CARTESIAN_POINT('Ctrl Pts',(1.24864586748505,1.50334353532201,16.773672287759));
#274928=CARTESIAN_POINT('Ctrl Pts',(1.27329624906766,1.48252192830883,16.7718233884578));
#274929=CARTESIAN_POINT('Ctrl Pts',(1.2973946303134,1.461123941777,16.7699744891565));
#274930=CARTESIAN_POINT('Ctrl Pts',(1.34846299905584,1.41577814633084,16.7660563724033));
#274931=CARTESIAN_POINT('Ctrl Pts',(1.39725238884547,1.36766186930103,16.7621382556502));
#274932=CARTESIAN_POINT('Ctrl Pts',(1.44344716950006,1.31703313126978,16.758220138897));
#274933=CARTESIAN_POINT('Ctrl Pts',(1.48957238854848,1.26648063164221,16.7543079221717));
#274934=CARTESIAN_POINT('Ctrl Pts',(1.53311042369732,1.21342354005044,16.7503957054464));
#274935=CARTESIAN_POINT('Ctrl Pts',(1.57378037375586,1.15815859673054,16.7464834887212));
#274936=CARTESIAN_POINT('Ctrl Pts',(1.6144024985005,1.10295864152247,16.7425758725177));
#274937=CARTESIAN_POINT('Ctrl Pts',(1.65216294620333,1.04555638516053,16.7386682563143));
#274938=CARTESIAN_POINT('Ctrl Pts',(1.6868204325988,0.986282326804649,16.7347606401108));
#274939=CARTESIAN_POINT('Ctrl Pts',(1.72145619714115,0.927045418932637,
16.7308554730367));
#274940=CARTESIAN_POINT('Ctrl Pts',(1.75299261053317,0.86593945992652,16.7269503059625));
#274941=CARTESIAN_POINT('Ctrl Pts',(1.78123203824553,0.803323363240291,
16.7230451388883));
#274942=CARTESIAN_POINT('Ctrl Pts',(1.80946345233201,0.740725035397593,
16.7191410800005));
#274943=CARTESIAN_POINT('Ctrl Pts',(1.83439953594026,0.676617868775745,
16.7152370211127));
#274944=CARTESIAN_POINT('Ctrl Pts',(1.85588972070514,0.611383140576348,
16.7113329622249));
#274945=CARTESIAN_POINT('Ctrl Pts',(1.87738117765369,0.54614455058809,16.7074286722232));
#274946=CARTESIAN_POINT('Ctrl Pts',(1.8954261792976,0.479778734483987,16.7035243822215));
#274947=CARTESIAN_POINT('Ctrl Pts',(1.90992378050061,0.412682871801403,
16.6996200922198));
#274948=CARTESIAN_POINT('Ctrl Pts',(1.92443682395765,0.345515541340018,
16.6957116435275));
#274949=CARTESIAN_POINT('Ctrl Pts',(1.9353948220809,0.277617094127129,16.6918031948352));
#274950=CARTESIAN_POINT('Ctrl Pts',(1.94274802045342,0.2093946728652,16.6878947461429));
#274951=CARTESIAN_POINT('Ctrl Pts',(1.950105620218,0.141131415818891,16.6839839579767));
#274952=CARTESIAN_POINT('Ctrl Pts',(1.95385409912709,0.0725442899996735,
16.6800731698106));
#274953=CARTESIAN_POINT('Ctrl Pts',(1.95399581835698,0.00404250460009209,
16.6761623816445));
#274954=CARTESIAN_POINT('Ctrl Pts',(1.95413778229033,-0.0645775613149842,
16.6722448408071));
#274955=CARTESIAN_POINT('Ctrl Pts',(1.9506605819423,-0.133111501725674,
16.6683272999696));
#274956=CARTESIAN_POINT('Ctrl Pts',(1.94361854554447,-0.201154043995133,
16.6644097591322));
#274957=CARTESIAN_POINT('Ctrl Pts',(1.94029502749426,-0.233267001758994,
16.6625608596165));
#274958=CARTESIAN_POINT('Ctrl Pts',(1.93617821866225,-0.26527063846103,
16.6607119601008));
#274959=CARTESIAN_POINT('Ctrl Pts',(1.93127775061767,-0.297123290856094,
16.658863060585));
#274960=CARTESIAN_POINT('Ctrl Pts',(1.92089286702049,-0.364624207987812,
16.6549449437687));
#274961=CARTESIAN_POINT('Ctrl Pts',(1.90694425660678,-0.431713827933215,
16.6510268269523));
#274962=CARTESIAN_POINT('Ctrl Pts',(1.88947742054759,-0.497987025173156,
16.6471087101359));
#274963=CARTESIAN_POINT('Ctrl Pts',(1.87203688661393,-0.564160426093595,
16.6431964933463));
#274964=CARTESIAN_POINT('Ctrl Pts',(1.85108876575637,-0.629519372412166,
16.6392842765567));
#274965=CARTESIAN_POINT('Ctrl Pts',(1.82672992672002,-0.693666904807687,
16.635372059767));
#274966=CARTESIAN_POINT('Ctrl Pts',(1.80239973214376,-0.757739003746423,
16.6314644434979));
#274967=CARTESIAN_POINT('Ctrl Pts',(1.77466695866875,-0.820602060268188,
16.6275568272288));
#274968=CARTESIAN_POINT('Ctrl Pts',(1.74367832738289,-0.881874078661569,
16.6236492109596));
#274969=CARTESIAN_POINT('Ctrl Pts',(1.71270911845958,-0.943107694347085,
16.619744043819));
#274970=CARTESIAN_POINT('Ctrl Pts',(1.67848832119053,-1.00275181207261,
16.6158388766783));
#274971=CARTESIAN_POINT('Ctrl Pts',(1.64121020734743,-1.06044568710453,
16.6119337095376));
#274972=CARTESIAN_POINT('Ctrl Pts',(1.60394267207081,-1.11812319010393,
16.6080296505826));
#274973=CARTESIAN_POINT('Ctrl Pts',(1.56361980935094,-1.17385113611301,
16.6041255916276));
#274974=CARTESIAN_POINT('Ctrl Pts',(1.52048021258001,-1.22729618395587,
16.6002215326726));
#274975=CARTESIAN_POINT('Ctrl Pts',(1.47733806200913,-1.28074439566605,
16.5963172426031));
#274976=CARTESIAN_POINT('Ctrl Pts',(1.43137915727873,-1.33190905976387,
16.5924129525336));
#274977=CARTESIAN_POINT('Ctrl Pts',(1.38288237295785,-1.3804898922348,16.5885086624641));
#274978=CARTESIAN_POINT('Ctrl Pts',(1.33433393183387,-1.42912247103352,
16.5846002137035));
#274979=CARTESIAN_POINT('Ctrl Pts',(1.28324256445431,-1.47516537690042,
16.580691764943));
#274980=CARTESIAN_POINT('Ctrl Pts',(1.22992328793101,-1.51835592197777,
16.5767833161824));
#274981=CARTESIAN_POINT('Ctrl Pts',(1.17657209617025,-1.56157231955335,
16.5728725279477));
#274982=CARTESIAN_POINT('Ctrl Pts',(1.12099073931128,-1.60193266937518,
16.5689617397129));
#274983=CARTESIAN_POINT('Ctrl Pts',(1.06352424536954,-1.63921694095417,
16.5650509514782));
#274984=CARTESIAN_POINT('Ctrl Pts',(1.00595852530987,-1.67656559045628,
16.5611334105723));
#274985=CARTESIAN_POINT('Ctrl Pts',(0.946501597619499,-1.71082731556612,
16.5572158696665));
#274986=CARTESIAN_POINT('Ctrl Pts',(0.885523377905878,-1.74182787530289,
16.5532983287606));
#274987=CARTESIAN_POINT('Ctrl Pts',(0.856744466079466,-1.75645871200858,
16.551449429845));
#274988=CARTESIAN_POINT('Ctrl Pts',(0.827626992125715,-1.77036385166465,
16.5496005309293));
#274989=CARTESIAN_POINT('Ctrl Pts',(0.798211179823588,-1.78352878092972,
16.5477516320137));
#274990=CARTESIAN_POINT('Ctrl Pts',(0.735874300842777,-1.81142740205085,
16.5438335152278));
#274991=CARTESIAN_POINT('Ctrl Pts',(0.671949444664659,-1.83610924804977,
16.5399153984419));
#274992=CARTESIAN_POINT('Ctrl Pts',(0.606801614227519,-1.85739274279052,
16.535997281656));
#274993=CARTESIAN_POINT('Ctrl Pts',(0.541751885503323,-1.87864418815559,
16.5320850648972));
#274994=CARTESIAN_POINT('Ctrl Pts',(0.475483301232471,-1.89650728686393,
16.5281728481384));
#274995=CARTESIAN_POINT('Ctrl Pts',(0.408381873685793,-1.91084804347308,
16.5242606313797));
#274996=CARTESIAN_POINT('Ctrl Pts',(0.341359353198165,-1.92517193625428,
16.5203530151418));
#274997=CARTESIAN_POINT('Ctrl Pts',(0.273506413221159,-1.93598161080183,
16.5164453989039));
#274998=CARTESIAN_POINT('Ctrl Pts',(0.205223543266017,-1.9431930674252,
16.5125377826661));
#274999=CARTESIAN_POINT('Ctrl Pts',(0.136983470128228,-1.9504000042123,
16.5086326155569));
#275000=CARTESIAN_POINT('Ctrl Pts',(0.068314489600747,-1.95401314515249,
16.5047274484478));
#275001=CARTESIAN_POINT('Ctrl Pts',(-0.000374961877715423,-1.95399996402344,
16.5008222813386));
#275002=CARTESIAN_POINT('Ctrl Pts',(-0.0690449210593987,-1.95398678663484,
16.4969182224153));
#275003=CARTESIAN_POINT('Ctrl Pts',(-0.137734848010914,-1.95034933012595,
16.493014163492));
#275004=CARTESIAN_POINT('Ctrl Pts',(-0.206035279610768,-1.94310716728535,
16.4891101045687));
#275005=CARTESIAN_POINT('Ctrl Pts',(-0.274339754492164,-1.93586457571975,
16.485205814531));
#275006=CARTESIAN_POINT('Ctrl Pts',(-0.342254199379061,-1.925016908578,
16.4813015244933));
#275007=CARTESIAN_POINT('Ctrl Pts',(-0.409375065767647,-1.91063551090409,
16.4773972344557));
#275008=CARTESIAN_POINT('Ctrl Pts',(-0.476567426575125,-1.89623879474988,
16.4734887857269));
#275009=CARTESIAN_POINT('Ctrl Pts',(-0.542964040064954,-1.87830093956203,
16.4695803369982));
#275010=CARTESIAN_POINT('Ctrl Pts',(-0.608173330622478,-1.85694404867771,
16.4656718882695));
#275011=CARTESIAN_POINT('Ctrl Pts',(-0.673421653404437,-1.83557437423216,
16.4617611000666));
#275012=CARTESIAN_POINT('Ctrl Pts',(-0.737480780057206,-1.8107817686867,
16.4578503118638));
#275013=CARTESIAN_POINT('Ctrl Pts',(-0.799978686095661,-1.78273668885583,
16.4539395236609));
#275014=CARTESIAN_POINT('Ctrl Pts',(-0.862584505884696,-1.75464318420658,
16.4500219827866));
#275015=CARTESIAN_POINT('Ctrl Pts',(-0.923623287534398,-1.72328622133261,
16.4461044419124));
#275016=CARTESIAN_POINT('Ctrl Pts',(-0.982747968393865,-1.68888200612646,
16.4421869010381));
#275017=CARTESIAN_POINT('Ctrl Pts',(-1.01065209972749,-1.67264479815193,
16.4403380018395));
#275018=CARTESIAN_POINT('Ctrl Pts',(-1.03813031028421,-1.65572946599459,
16.4384891026409));
#275019=CARTESIAN_POINT('Ctrl Pts',(-1.06514858527807,-1.63816192462166,
16.4366402034423));
#275020=CARTESIAN_POINT('Ctrl Pts',(-1.12237316433513,-1.60095395481743,
16.4327242436563));
#275021=CARTESIAN_POINT('Ctrl Pts',(-1.17775982360252,-1.56066973669982,
16.4288082838704));
#275022=CARTESIAN_POINT('Ctrl Pts',(-1.23095822858698,-1.51751699808404,
16.4248923240845));
#275023=CARTESIAN_POINT('Ctrl Pts',(-1.28407650419064,-1.47442925769944,
16.4209822626603));
#275024=CARTESIAN_POINT('Ctrl Pts',(-1.33501268735557,-1.4284818792864,
16.4170722012361));
#275025=CARTESIAN_POINT('Ctrl Pts',(-1.3834449916962,-1.37992606865394,
16.4131621398119));
#275026=CARTESIAN_POINT('Ctrl Pts',(-1.43182040739025,-1.33142729173871,
16.4092566711508));
#275027=CARTESIAN_POINT('Ctrl Pts',(-1.47769743890976,-1.28032651433722,
16.4053512024897));
#275028=CARTESIAN_POINT('Ctrl Pts',(-1.52078842845766,-1.22691424144856,
16.4014457338286));
#275029=CARTESIAN_POINT('Ctrl Pts',(-1.56385248865943,-1.17353534810395,
16.3975427058568));
#275030=CARTESIAN_POINT('Ctrl Pts',(-1.60413365205027,-1.11784820716031,
16.393639677885));
#275031=CARTESIAN_POINT('Ctrl Pts',(-1.6413831816081,-1.06017793371399,
16.3897366499133));
#275032=CARTESIAN_POINT('Ctrl Pts',(-1.6786222472096,-1.00252386071987,
16.3858347183611));
#275033=CARTESIAN_POINT('Ctrl Pts',(-1.71283110250474,-0.942888174647101,
16.3819327868089));
#275034=CARTESIAN_POINT('Ctrl Pts',(-1.74380421683398,-0.881625120644844,
16.3780308552567));
#275035=CARTESIAN_POINT('Ctrl Pts',(-1.77477928560832,-0.820358200861631,
16.3741286774874));
#275036=CARTESIAN_POINT('Ctrl Pts',(-1.80251798820246,-0.757464149983337,
16.3702264997181));
#275037=CARTESIAN_POINT('Ctrl Pts',(-1.8268614954187,-0.693320327522964,
16.3663243219488));
#275038=CARTESIAN_POINT('Ctrl Pts',(-1.85123096816227,-0.629108087305018,
16.3624179819977));
#275039=CARTESIAN_POINT('Ctrl Pts',(-1.87219784364341,-0.563643876634213,
16.3585116420465));
#275040=CARTESIAN_POINT('Ctrl Pts',(-1.88965243210149,-0.49732251693738,
16.3546053020954));
#275041=CARTESIAN_POINT('Ctrl Pts',(-1.90711756295254,-0.430961099817349,
16.3506966027549));
#275042=CARTESIAN_POINT('Ctrl Pts',(-1.92106608512885,-0.3637419856602,
16.3467879034144));
#275043=CARTESIAN_POINT('Ctrl Pts',(-1.93143953667531,-0.296069782597726,
16.3428792040738));
#275044=CARTESIAN_POINT('Ctrl Pts',(-1.94183081966495,-0.228281254410631,
16.3389637858751));
#275045=CARTESIAN_POINT('Ctrl Pts',(-1.94863471911459,-0.160038572711775,
16.3350483676763));
#275046=CARTESIAN_POINT('Ctrl Pts',(-1.95184474547632,-0.0917501474466611,
16.3311329494776));
#275047=CARTESIAN_POINT('Ctrl Pts',(-1.95328309287062,-0.0611514957619569,
16.3293785303766));
#275048=CARTESIAN_POINT('Ctrl Pts',(-1.95400057833122,-0.0305436375502851,
16.3276241112755));
#275049=CARTESIAN_POINT('Ctrl Pts',(-1.95399999965015,3.69758055581722E-5,
16.3258696921745));
#275050=CARTESIAN_POINT('',(-1.95399927660164,-0.00168138046293059,15.625869711382));
#275051=CARTESIAN_POINT('Ctrl Pts',(-1.95399999965013,3.69766827344706E-5,
16.3258696921242));
#275052=CARTESIAN_POINT('Ctrl Pts',(-1.9539999621663,0.00201777642562759,
16.3257560530398));
#275053=CARTESIAN_POINT('Ctrl Pts',(-1.953996912733,0.00399857278929908,
16.3256424139553));
#275054=CARTESIAN_POINT('Ctrl Pts',(-1.95399085137439,0.00597935993164894,
16.3255287748708));
#275055=CARTESIAN_POINT('Ctrl Pts',(-1.95378186420173,0.0742741319649818,
16.3216106580765));
#275056=CARTESIAN_POINT('Ctrl Pts',(-1.94998765241292,0.142693315948708,
16.3176925412822));
#275057=CARTESIAN_POINT('Ctrl Pts',(-1.94259283162147,0.210829529556217,
16.3137744244879));
#275058=CARTESIAN_POINT('Ctrl Pts',(-1.9352091461905,0.278863141447944,
16.3098622077207));
#275059=CARTESIAN_POINT('Ctrl Pts',(-1.92423566498077,0.346614143558209,
16.3059499909535));
#275060=CARTESIAN_POINT('Ctrl Pts',(-1.9097090145515,0.413675573053036,
16.3020377741863));
#275061=CARTESIAN_POINT('Ctrl Pts',(-1.89519944654936,0.480658142525099,
16.2981301579399));
#275062=CARTESIAN_POINT('Ctrl Pts',(-1.87714511114424,0.546952271375196,
16.2942225416935));
#275063=CARTESIAN_POINT('Ctrl Pts',(-1.85563416057608,0.612158363581769,
16.2903149254472));
#275064=CARTESIAN_POINT('Ctrl Pts',(-1.83413669216254,0.677323587365809,
16.2864097583295));
#275065=CARTESIAN_POINT('Ctrl Pts',(-1.80918705990762,0.741401661179688,
16.2825045912118));
#275066=CARTESIAN_POINT('Ctrl Pts',(-1.78092360280814,0.804006915990707,
16.2785994240941));
#275067=CARTESIAN_POINT('Ctrl Pts',(-1.75266816614954,0.866594405043498,
16.2746953651623));
#275068=CARTESIAN_POINT('Ctrl Pts',(-1.72110097375604,0.927709456691211,
16.2707913062304));
#275069=CARTESIAN_POINT('Ctrl Pts',(-1.68640827532238,0.986986893998192,
16.2668872472985));
#275070=CARTESIAN_POINT('Ctrl Pts',(-1.65171352313379,1.04626784043922,
16.2629829572523));
#275071=CARTESIAN_POINT('Ctrl Pts',(-1.61389314823192,1.1037105333433,16.2590786672061));
#275072=CARTESIAN_POINT('Ctrl Pts',(-1.57317815826722,1.15897648049948,
16.2551743771598));
#275073=CARTESIAN_POINT('Ctrl Pts',(-1.53241980035068,1.21430129469546,
16.2512659284226));
#275074=CARTESIAN_POINT('Ctrl Pts',(-1.48876096651499,1.26744433919756,
16.2473574796854));
#275075=CARTESIAN_POINT('Ctrl Pts',(-1.44247400641579,1.31809891162036,
16.2434490309482));
#275076=CARTESIAN_POINT('Ctrl Pts',(-1.39615934040257,1.36878380427214,
16.2395382427368));
#275077=CARTESIAN_POINT('Ctrl Pts',(-1.3472137678834,1.41697691526967,16.2356274545255));
#275078=CARTESIAN_POINT('Ctrl Pts',(-1.2959456716492,1.4624092505635,16.2317166663141));
#275079=CARTESIAN_POINT('Ctrl Pts',(-1.24458905193016,1.50792003286317,
16.2277991254315));
#275080=CARTESIAN_POINT('Ctrl Pts',(-1.19090228930025,1.55066021915519,
16.2238815845489));
#275081=CARTESIAN_POINT('Ctrl Pts',(-1.13522520038532,1.59040238443298,
16.2199640436663));
#275082=CARTESIAN_POINT('Ctrl Pts',(-1.10894817510018,1.60915885863526,
16.218115144544));
#275083=CARTESIAN_POINT('Ctrl Pts',(-1.08222821521553,1.62724819735638,
16.2162662454217));
#275084=CARTESIAN_POINT('Ctrl Pts',(-1.05510293232958,1.6446500546285,16.2144173462994));
#275085=CARTESIAN_POINT('Ctrl Pts',(-0.997620063192867,1.68152740954919,
16.2104992295099));
#275086=CARTESIAN_POINT('Ctrl Pts',(-0.938087542964199,1.71546057626014,
16.2065811127204));
#275087=CARTESIAN_POINT('Ctrl Pts',(-0.876839237282497,1.74621560866975,
16.2026629959309));
#275088=CARTESIAN_POINT('Ctrl Pts',(-0.815683161283005,1.77692432915555,
16.1987507791685));
#275089=CARTESIAN_POINT('Ctrl Pts',(-0.75281686356938,1.80446419438366,
16.1948385624062));
#275090=CARTESIAN_POINT('Ctrl Pts',(-0.688602075615101,1.82864517647863,
16.1909263456438));
#275091=CARTESIAN_POINT('Ctrl Pts',(-0.624462800213449,1.85279772325924,
16.1870187294024));
#275092=CARTESIAN_POINT('Ctrl Pts',(-0.558978642019656,1.87359905881964,
16.183111113161));
#275093=CARTESIAN_POINT('Ctrl Pts',(-0.492533099124756,1.89090643509047,
16.1792034969195));
#275094=CARTESIAN_POINT('Ctrl Pts',(-0.426129201488483,1.90820296382919,
16.1752983298068));
#275095=CARTESIAN_POINT('Ctrl Pts',(-0.358765589358424,1.92200975357006,
16.1713931626941));
#275096=CARTESIAN_POINT('Ctrl Pts',(-0.290841290289802,1.9322337705005,
16.1674879955814));
#275097=CARTESIAN_POINT('Ctrl Pts',(-0.222936266387693,1.94245488611827,
16.1635839366546));
#275098=CARTESIAN_POINT('Ctrl Pts',(-0.15447135757717,1.94909517406813,
16.1596798777277));
#275099=CARTESIAN_POINT('Ctrl Pts',(-0.0858543711445922,1.95211296470142,
16.1557758188009));
#275100=CARTESIAN_POINT('Ctrl Pts',(-0.0172333226914123,1.9551309339833,
16.1518715287597));
#275101=CARTESIAN_POINT('Ctrl Pts',(0.0515393297417269,1.95452596114806,
16.1479672387185));
#275102=CARTESIAN_POINT('Ctrl Pts',(0.120053911615658,1.9503084520931,16.1440629486773));
#275103=CARTESIAN_POINT('Ctrl Pts',(0.188641472436451,1.94608645071897,
16.1401544999452));
#275104=CARTESIAN_POINT('Ctrl Pts',(0.256969922217087,1.93824426413374,
16.136246051213));
#275105=CARTESIAN_POINT('Ctrl Pts',(0.324633860893539,1.92684427402978,
16.1323376024808));
#275106=CARTESIAN_POINT('Ctrl Pts',(0.392338301068817,1.91543746025143,
16.1284268142745));
#275107=CARTESIAN_POINT('Ctrl Pts',(0.459376958409542,1.90046871188476,
16.1245160260683));
#275108=CARTESIAN_POINT('Ctrl Pts',(0.525356559333032,1.88205113787212,
16.120605237862));
#275109=CARTESIAN_POINT('Ctrl Pts',(0.591450085771083,1.86360176264264,
16.1166876969844));
#275110=CARTESIAN_POINT('Ctrl Pts',(0.656480440214814,1.84169183348761,
16.1127701561068));
#275111=CARTESIAN_POINT('Ctrl Pts',(0.720072213984936,1.8164834176636,16.1088526152292));
#275112=CARTESIAN_POINT('Ctrl Pts',(0.750084607277191,1.8045862044687,16.1070037160621));
#275113=CARTESIAN_POINT('Ctrl Pts',(0.779776899876457,1.79195496374141,
16.105154816895));
#275114=CARTESIAN_POINT('Ctrl Pts',(0.809111594666034,1.77861025167882,
16.103305917728));
#275115=CARTESIAN_POINT('Ctrl Pts',(0.871276564085345,1.75033064545719,
16.0993878009381));
#275116=CARTESIAN_POINT('Ctrl Pts',(0.93208036016985,1.71873192474972,16.0954696841482));
#275117=CARTESIAN_POINT('Ctrl Pts',(0.991145325020365,1.68396761984614,
16.0915515673583));
#275118=CARTESIAN_POINT('Ctrl Pts',(1.05012134793391,1.64925566415877,16.0876393505956));
#275119=CARTESIAN_POINT('Ctrl Pts',(1.10736331569261,1.61138783225709,16.0837271338329));
#275120=CARTESIAN_POINT('Ctrl Pts',(1.16251534446752,1.5705648900563,16.0798149170701));
#275121=CARTESIAN_POINT('Ctrl Pts',(1.21760251792454,1.5297899530686,16.0759073008283));
#275122=CARTESIAN_POINT('Ctrl Pts',(1.27060423981632,1.486067098487,16.0719996845865));
#275123=CARTESIAN_POINT('Ctrl Pts',(1.32119253330485,1.43964102815234,16.0680920683447));
#275124=CARTESIAN_POINT('Ctrl Pts',(1.37174912018855,1.39324405571689,16.0641869012316));
#275125=CARTESIAN_POINT('Ctrl Pts',(1.41989491766924,1.34414756024183,16.0602817341186));
#275126=CARTESIAN_POINT('Ctrl Pts',(1.46533528483458,1.29263626090975,16.0563765670055));
#275127=CARTESIAN_POINT('Ctrl Pts',(1.51076275719404,1.24113957915776,16.0524725080783));
#275128=CARTESIAN_POINT('Ctrl Pts',(1.55348599807477,1.18722982260129,16.0485684491511));
#275129=CARTESIAN_POINT('Ctrl Pts',(1.5932487504838,1.13122695295057,16.0446643902239));
#275130=CARTESIAN_POINT('Ctrl Pts',(1.63301385678685,1.07522076801575,16.0407601001824));
#275131=CARTESIAN_POINT('Ctrl Pts',(1.66981784400191,1.01712162653524,16.0368558101408));
#275132=CARTESIAN_POINT('Ctrl Pts',(1.70344718695854,0.957279312031251,
16.0329515200993));
#275133=CARTESIAN_POINT('Ctrl Pts',(1.73711235052379,0.897373255927272,
16.0290430713668));
#275134=CARTESIAN_POINT('Ctrl Pts',(1.76759587996122,0.83572075091901,16.0251346226343));
#275135=CARTESIAN_POINT('Ctrl Pts',(1.79473023028621,0.772696189001096,
16.0212261739018));
#275136=CARTESIAN_POINT('Ctrl Pts',(1.82188082237713,0.709633902569045,
16.0173153856952));
#275137=CARTESIAN_POINT('Ctrl Pts',(1.84567807517417,0.645198386229305,
16.0134045974886));
#275138=CARTESIAN_POINT('Ctrl Pts',(1.86600363512424,0.5797813671576,16.009493809282));
#275139=CARTESIAN_POINT('Ctrl Pts',(1.88636429076809,0.514251393969258,
16.0055762684041));
#275140=CARTESIAN_POINT('Ctrl Pts',(1.90324116860687,0.447737012140573,
16.0016587275262));
#275141=CARTESIAN_POINT('Ctrl Pts',(1.9165667339101,0.380641503870971,15.9977411866483));
#275142=CARTESIAN_POINT('Ctrl Pts',(1.92285578801716,0.34897550905233,15.9958922874844));
#275143=CARTESIAN_POINT('Ctrl Pts',(1.92835457016774,0.317180165470872,
15.9940433883205));
#275144=CARTESIAN_POINT('Ctrl Pts',(1.93306000430126,0.285298124373133,
15.9921944891566));
#275145=CARTESIAN_POINT('Ctrl Pts',(1.94303158136038,0.217734915413521,
15.9882763723656));
#275146=CARTESIAN_POINT('Ctrl Pts',(1.94947651482669,0.149514364227127,
15.9843582555746));
#275147=CARTESIAN_POINT('Ctrl Pts',(1.95231887838287,0.0810370107410566,
15.9804401387836));
#275148=CARTESIAN_POINT('Ctrl Pts',(1.95515696181598,0.0126627726711564,
15.9765279220198));
#275149=CARTESIAN_POINT('Ctrl Pts',(1.95440322154275,-0.0559670127300859,
15.9726157052559));
#275150=CARTESIAN_POINT('Ctrl Pts',(1.95003322385718,-0.124444468953685,
15.9687034884921));
#275151=CARTESIAN_POINT('Ctrl Pts',(1.94566836501407,-0.192841399995072,
15.9647958722491));
#275152=CARTESIAN_POINT('Ctrl Pts',(1.93769572544993,-0.261085869055538,
15.9608882560061));
#275153=CARTESIAN_POINT('Ctrl Pts',(1.92614291961,-0.328769605097942,15.9569806397632));
#275154=CARTESIAN_POINT('Ctrl Pts',(1.91459735458058,-0.396410919834754,
15.9530754726489));
#275155=CARTESIAN_POINT('Ctrl Pts',(1.89947615702947,-0.463491714927154,
15.9491703055347));
#275156=CARTESIAN_POINT('Ctrl Pts',(1.88085864327038,-0.529610011267826,
15.9452651384205));
#275157=CARTESIAN_POINT('Ctrl Pts',(1.86224641268212,-0.595709544939138,
15.9413610794921));
#275158=CARTESIAN_POINT('Ctrl Pts',(1.84013996875894,-0.660846648827569,
15.9374570205637));
#275159=CARTESIAN_POINT('Ctrl Pts',(1.81466905746596,-0.724632466755111,
15.9335529616353));
#275160=CARTESIAN_POINT('Ctrl Pts',(1.78919663833397,-0.788422060705574,
15.9296486715926));
#275161=CARTESIAN_POINT('Ctrl Pts',(1.76035954120025,-0.85085975402567,
15.9257443815498));
#275162=CARTESIAN_POINT('Ctrl Pts',(1.72833574705956,-0.911576406800913,
15.9218400915071));
#275163=CARTESIAN_POINT('Ctrl Pts',(1.6962778424755,-0.972357732485841,
15.9179316427734));
#275164=CARTESIAN_POINT('Ctrl Pts',(1.66102669674379,-1.03141392325265,
15.9140231940397));
#275165=CARTESIAN_POINT('Ctrl Pts',(1.62280590891998,-1.08840111263009,
15.910114745306));
#275166=CARTESIAN_POINT('Ctrl Pts',(1.58456224333848,-1.14542241274107,
15.9062039570982));
#275167=CARTESIAN_POINT('Ctrl Pts',(1.54334569323334,-1.20037185319889,
15.9022931688904));
#275168=CARTESIAN_POINT('Ctrl Pts',(1.49942110819802,-1.2529374845898,15.8983823806825));
#275169=CARTESIAN_POINT('Ctrl Pts',(1.45542067955548,-1.30559387989111,
15.8944648398034));
#275170=CARTESIAN_POINT('Ctrl Pts',(1.40870321831996,-1.35585789101151,
15.8905472989243));
#275171=CARTESIAN_POINT('Ctrl Pts',(1.35957085206292,-1.40345398863693,
15.8866297580452));
#275172=CARTESIAN_POINT('Ctrl Pts',(1.33638263445959,-1.42591715808889,
15.8847808588918));
#275173=CARTESIAN_POINT('Ctrl Pts',(1.31265700314292,-1.44778665477442,
15.8829319597385));
#275174=CARTESIAN_POINT('Ctrl Pts',(1.28842811743316,-1.46903675454621,
15.8810830605851));
#275175=CARTESIAN_POINT('Ctrl Pts',(1.23708318402424,-1.51406915804942,
15.8771649437949));
#275176=CARTESIAN_POINT('Ctrl Pts',(1.18327270622517,-1.55649572105797,
15.8732468270046));
#275177=CARTESIAN_POINT('Ctrl Pts',(1.12729195521896,-1.59603535289749,
15.8693287102144));
#275178=CARTESIAN_POINT('Ctrl Pts',(1.07139550184042,-1.63551544467898,
15.8654164934513));
#275179=CARTESIAN_POINT('Ctrl Pts',(1.01333565974962,-1.67211695152243,
15.8615042766881));
#275180=CARTESIAN_POINT('Ctrl Pts',(0.95344180006052,-1.70559805754385,
15.857592059925));
#275181=CARTESIAN_POINT('Ctrl Pts',(0.893618371784101,-1.73903979188998,
15.8536844436828));
#275182=CARTESIAN_POINT('Ctrl Pts',(0.831965636444704,-1.76936817401605,
15.8497768274406));
#275183=CARTESIAN_POINT('Ctrl Pts',(0.768841534976206,-1.79638489586598,
15.8458692111984));
#275184=CARTESIAN_POINT('Ctrl Pts',(0.705756997027155,-1.82338468477627,
15.8419640440849));
#275185=CARTESIAN_POINT('Ctrl Pts',(0.641203373469786,-1.847076737653,15.8380588769714));
#275186=CARTESIAN_POINT('Ctrl Pts',(0.575561370375906,-1.86730959107776,
15.8341537098579));
#275187=CARTESIAN_POINT('Ctrl Pts',(0.509937994791741,-1.88753670293987,
15.8302496509303));
#275188=CARTESIAN_POINT('Ctrl Pts',(0.443227322636232,-1.90430641923978,
15.8263455920027));
#275189=CARTESIAN_POINT('Ctrl Pts',(0.375826396658372,-1.91751675861641,
15.822441533075));
#275190=CARTESIAN_POINT('Ctrl Pts',(0.308421480648792,-1.93072788002492,
15.8185372430331));
#275191=CARTESIAN_POINT('Ctrl Pts',(0.240326712879047,-1.9403791140884,
15.8146329529911));
#275192=CARTESIAN_POINT('Ctrl Pts',(0.171948743514836,-1.94641969513352,
15.8107286629492));
#275193=CARTESIAN_POINT('Ctrl Pts',(0.103497940718056,-1.95246671035995,
15.8068202142162));
#275194=CARTESIAN_POINT('Ctrl Pts',(0.034763825229422,-1.95489535393298,
15.8029117654833));
#275195=CARTESIAN_POINT('Ctrl Pts',(-0.0338434333726768,-1.95370689255516,
15.7990033167503));
#275196=CARTESIAN_POINT('Ctrl Pts',(-0.102491758115139,-1.95251771980186,
15.7950925285433));
#275197=CARTESIAN_POINT('Ctrl Pts',(-0.171012584112308,-1.94770716763265,
15.7911817403363));
#275198=CARTESIAN_POINT('Ctrl Pts',(-0.239000172764327,-1.93932847073894,
15.7872709521292));
#275199=CARTESIAN_POINT('Ctrl Pts',(-0.307105154078534,-1.93093530653504,
15.7833534112509));
#275200=CARTESIAN_POINT('Ctrl Pts',(-0.374674576343085,-1.9189617869472,
15.7794358703725));
#275201=CARTESIAN_POINT('Ctrl Pts',(-0.441313069903809,-1.90351222069418,
15.7755183294942));
#275202=CARTESIAN_POINT('Ctrl Pts',(-0.472763374726625,-1.89622073581697,
15.773669430334));
#275203=CARTESIAN_POINT('Ctrl Pts',(-0.504006548632445,-1.88815571513218,
15.7718205311738));
#275204=CARTESIAN_POINT('Ctrl Pts',(-0.53500244970063,-1.87933189692889,
15.7699716320137));
#275205=CARTESIAN_POINT('Ctrl Pts',(-0.600687784533275,-1.86063279694431,
15.7660535152233));
#275206=CARTESIAN_POINT('Ctrl Pts',(-0.665521807765686,-1.83844878915834,
15.7621353984329));
#275207=CARTESIAN_POINT('Ctrl Pts',(-0.729108197939647,-1.81287540545323,
15.7582172816425));
#275208=CARTESIAN_POINT('Ctrl Pts',(-0.792598837668159,-1.78734053097744,
15.7543050648793));
#275209=CARTESIAN_POINT('Ctrl Pts',(-0.854845120261035,-1.75842659194378,
15.7503928481161));
#275210=CARTESIAN_POINT('Ctrl Pts',(-0.915465215454334,-1.72627907340996,
15.7464806313529));
#275211=CARTESIAN_POINT('Ctrl Pts',(-0.976014025227648,-1.69416935833641,
15.7425730151105));
#275212=CARTESIAN_POINT('Ctrl Pts',(-1.03494001294859,-1.65883384491755,
15.7386653988682));
#275213=CARTESIAN_POINT('Ctrl Pts',(-1.09188239574313,-1.62046562254996,
15.7347577826259));
#275214=CARTESIAN_POINT('Ctrl Pts',(-1.1487890894583,-1.58212144776287,
15.7308526155123));
#275215=CARTESIAN_POINT('Ctrl Pts',(-1.20371423743605,-1.54074860880089,
15.7269474483987));
#275216=CARTESIAN_POINT('Ctrl Pts',(-1.25632405649873,-1.49658473367283,
15.7230422812852));
#275217=CARTESIAN_POINT('Ctrl Pts',(-1.30891894624984,-1.45243339111499,
15.7191382223574));
#275218=CARTESIAN_POINT('Ctrl Pts',(-1.35919943484673,-1.40549290080089,
15.7152341634297));
#275219=CARTESIAN_POINT('Ctrl Pts',(-1.40686444203506,-1.35604146018378,
15.7113301045019));
#275220=CARTESIAN_POINT('Ctrl Pts',(-1.4545322709189,-1.30658709211705,
15.7074258144599));
#275221=CARTESIAN_POINT('Ctrl Pts',(-1.49958397148951,-1.2546218345644,
15.7035215244178));
#275222=CARTESIAN_POINT('Ctrl Pts',(-1.54175627363209,-1.20045974223049,
15.6996172343758));
#275223=CARTESIAN_POINT('Ctrl Pts',(-1.58397349599608,-1.14623995863819,
15.6957087856427));
#275224=CARTESIAN_POINT('Ctrl Pts',(-1.6233048963418,-1.08981905924165,
15.6918003369097));
#275225=CARTESIAN_POINT('Ctrl Pts',(-1.65952900374366,-1.03154228499543,
15.6878918881766));
#275226=CARTESIAN_POINT('Ctrl Pts',(-1.69577479375325,-0.973230628110908,
15.6839810999695));
#275227=CARTESIAN_POINT('Ctrl Pts',(-1.7289093519144,-0.91306131647089,
15.6800703117623));
#275228=CARTESIAN_POINT('Ctrl Pts',(-1.75875726583993,-0.851404063800066,
15.6761595235552));
#275229=CARTESIAN_POINT('Ctrl Pts',(-1.78865671749675,-0.7896403489179,
15.6722419826767));
#275230=CARTESIAN_POINT('Ctrl Pts',(-1.81525800800206,-0.726384018482055,
15.6683244417983));
#275231=CARTESIAN_POINT('Ctrl Pts',(-1.83843425416253,-0.662023785918493,
15.6644069009198));
#275232=CARTESIAN_POINT('Ctrl Pts',(-1.84937237666568,-0.631648715545271,
15.6625580017606));
#275233=CARTESIAN_POINT('Ctrl Pts',(-1.85954833023355,-0.601027963721518,
15.6607091026014));
#275234=CARTESIAN_POINT('Ctrl Pts',(-1.86895271668084,-0.570203246931559,
15.6588602034422));
#275235=CARTESIAN_POINT('Ctrl Pts',(-1.8933156493855,-0.490348967760566,
15.6540704592047));
#275236=CARTESIAN_POINT('Ctrl Pts',(-1.91257560688055,-0.408869779193623,
15.6492807149672));
#275237=CARTESIAN_POINT('Ctrl Pts',(-1.92655338481555,-0.32635571920184,
15.6444909707297));
#275238=CARTESIAN_POINT('Ctrl Pts',(-1.94033383030346,-0.245006558341653,
15.6397688461063));
#275239=CARTESIAN_POINT('Ctrl Pts',(-1.94898014136491,-0.162651520851779,
15.635046721483));
#275240=CARTESIAN_POINT('Ctrl Pts',(-1.95236668761014,-0.079876887208999,
15.6303245968597));
#275241=CARTESIAN_POINT('Ctrl Pts',(-1.95343165143404,-0.0538468306315289,
15.6288396350338));
#275242=CARTESIAN_POINT('Ctrl Pts',(-1.95397682314485,-0.0277754378755728,
15.6273546732079));
#275243=CARTESIAN_POINT('Ctrl Pts',(-1.95399927660164,-0.00168138046293059,
15.625869711382));
#275244=CARTESIAN_POINT('',(-1.95392498394666,0.000982598694633225,14.9258696453069));
#275245=CARTESIAN_POINT('Ctrl Pts',(-1.9527894730371,-0.0016800012556531,
15.6258696921242));
#275246=CARTESIAN_POINT('Ctrl Pts',(-1.94903578034424,0.455625916679805,
15.5998293863731));
#275247=CARTESIAN_POINT('Ctrl Pts',(-1.56072621450247,1.56910039980144,
15.5367519377649));
#275248=CARTESIAN_POINT('Ctrl Pts',(0.294214790414482,2.29052272133908,
15.4366373462993));
#275249=CARTESIAN_POINT('Ctrl Pts',(2.08372643567803,0.995560556227894,
15.325525917728));
#275250=CARTESIAN_POINT('Ctrl Pts',(1.96681121926772,-1.21025216695624,
15.2144144891566));
#275251=CARTESIAN_POINT('Ctrl Pts',(0.0504363060114985,-2.30879034537602,
15.1033030605851));
#275252=CARTESIAN_POINT('Ctrl Pts',(-1.64838339262918,-1.4312106179003,
15.0071214615743));
#275253=CARTESIAN_POINT('Ctrl Pts',(-1.94951755043896,-0.388009868955187,
14.9479770054207));
#275254=CARTESIAN_POINT('Ctrl Pts',(-1.9512855068604,0.000980447537236029,
14.9258696921242));
#275255=CARTESIAN_POINT('',(-1.95399967130156,0.00113338140505696,14.2258696921744));
#275256=CARTESIAN_POINT('Ctrl Pts',(-1.95399975291197,0.000982659630874597,
14.9258696439807));
#275257=CARTESIAN_POINT('Ctrl Pts',(-1.95396157458776,0.0768995221230205,
14.9215610769975));
#275258=CARTESIAN_POINT('Ctrl Pts',(-1.94949495136225,0.15266488028038,
14.9172525100143));
#275259=CARTESIAN_POINT('Ctrl Pts',(-1.94067744149054,0.22778733083678,
14.9129439430311));
#275260=CARTESIAN_POINT('Ctrl Pts',(-1.93182839971281,0.303178423457082,
14.9086199683726));
#275261=CARTESIAN_POINT('Ctrl Pts',(-1.91859743506083,0.377921711246782,
14.9042959937141));
#275262=CARTESIAN_POINT('Ctrl Pts',(-1.90111289227954,0.45153712007822,
14.8999720190555));
#275263=CARTESIAN_POINT('Ctrl Pts',(-1.88354470861175,0.525504683274326,
14.8956273597798));
#275264=CARTESIAN_POINT('Ctrl Pts',(-1.86168229836676,0.598333268948949,
14.8912827005041));
#275265=CARTESIAN_POINT('Ctrl Pts',(-1.8357040846616,0.669556953183755,
14.8869380412285));
#275266=CARTESIAN_POINT('Ctrl Pts',(-1.82402874165582,0.70156688862484,
14.884985428633));
#275267=CARTESIAN_POINT('Ctrl Pts',(-1.81152269757046,0.733252964852512,
14.8830328160376));
#275268=CARTESIAN_POINT('Ctrl Pts',(-1.79820517487775,0.76457448887789,
14.8810802034422));
#275269=CARTESIAN_POINT('Ctrl Pts',(-1.77148220412985,0.827424328868625,
14.8771620866518));
#275270=CARTESIAN_POINT('Ctrl Pts',(-1.74140725560317,0.888996061353628,
14.8732439698614));
#275271=CARTESIAN_POINT('Ctrl Pts',(-1.70812440854876,0.948908322716141,
14.869325853071));
#275272=CARTESIAN_POINT('Ctrl Pts',(-1.67489167988323,1.00873036625537,
14.8654136363077));
#275273=CARTESIAN_POINT('Ctrl Pts',(-1.63846087658321,1.06689747154796,
14.8615014195444));
#275274=CARTESIAN_POINT('Ctrl Pts',(-1.59902384104076,1.12304886616,14.8575892027811));
#275275=CARTESIAN_POINT('Ctrl Pts',(-1.55963318097214,1.179134230263,14.8536815865387));
#275276=CARTESIAN_POINT('Ctrl Pts',(-1.5172435908701,1.23320819061896,14.8497739702964));
#275277=CARTESIAN_POINT('Ctrl Pts',(-1.47209153029668,1.28493677915638,
14.845866354054));
#275278=CARTESIAN_POINT('Ctrl Pts',(-1.42696776912689,1.33663294640034,
14.8419611869404));
#275279=CARTESIAN_POINT('Ctrl Pts',(-1.37908529476368,1.38598628806162,
14.8380560198267));
#275280=CARTESIAN_POINT('Ctrl Pts',(-1.32872140174712,1.43269516525295,
14.8341508527131));
#275281=CARTESIAN_POINT('Ctrl Pts',(-1.27837180070615,1.47939078766803,
14.8302467937853));
#275282=CARTESIAN_POINT('Ctrl Pts',(-1.22554253937853,1.5234431010258,14.8263427348575));
#275283=CARTESIAN_POINT('Ctrl Pts',(-1.17054709964035,1.56458796094166,
14.8224386759297));
#275284=CARTESIAN_POINT('Ctrl Pts',(-1.11554840425626,1.60573525657028,
14.8185343858876));
#275285=CARTESIAN_POINT('Ctrl Pts',(-1.05838367125969,1.64397446443823,
14.8146300958455));
#275286=CARTESIAN_POINT('Ctrl Pts',(-0.999397259087691,1.67908341619111,
14.8107258058034));
#275287=CARTESIAN_POINT('Ctrl Pts',(-0.940348016987983,1.71422976457178,
14.8068173570702));
#275288=CARTESIAN_POINT('Ctrl Pts',(-0.879473646804447,1.7462389507024,
14.8029089083371));
#275289=CARTESIAN_POINT('Ctrl Pts',(-0.817144252694092,1.77493415942367,
14.799000459604));
#275290=CARTESIAN_POINT('Ctrl Pts',(-0.75477755017502,1.8036465441915,14.7950896713968));
#275291=CARTESIAN_POINT('Ctrl Pts',(-0.690954547508917,1.82904082186524,
14.7911788831896));
#275292=CARTESIAN_POINT('Ctrl Pts',(-0.626063903494332,1.8509889218311,
14.7872680949824));
#275293=CARTESIAN_POINT('Ctrl Pts',(-0.561061214243252,1.8729749190946,
14.7833505541039));
#275294=CARTESIAN_POINT('Ctrl Pts',(-0.494987677728567,1.89150272979415,
14.7794330132254));
#275295=CARTESIAN_POINT('Ctrl Pts',(-0.428244769546033,1.90649479867018,
14.7755154723469));
#275296=CARTESIAN_POINT('Ctrl Pts',(-0.396745185849562,1.91357036581587,
14.7736665731882));
#275297=CARTESIAN_POINT('Ctrl Pts',(-0.365096616230716,1.91985912672413,
14.7718176740295));
#275298=CARTESIAN_POINT('Ctrl Pts',(-0.333341622120266,1.92535694429948,
14.7699687748708));
#275299=CARTESIAN_POINT('Ctrl Pts',(-0.266047646124195,1.93700771024388,
14.7660506580804));
#275300=CARTESIAN_POINT('Ctrl Pts',(-0.198008720544545,1.94514929338545,
14.76213254129));
#275301=CARTESIAN_POINT('Ctrl Pts',(-0.129623370609614,1.94969581776025,
14.7582144244996));
#275302=CARTESIAN_POINT('Ctrl Pts',(-0.0613409975491255,1.95423549583141,
14.7543022077363));
#275303=CARTESIAN_POINT('Ctrl Pts',(0.0072862777138335,1.95519082675997,
14.750389990973));
#275304=CARTESIAN_POINT('Ctrl Pts',(0.075851313510783,1.95252722855244,
14.7464777742098));
#275305=CARTESIAN_POINT('Ctrl Pts',(0.144335721137273,1.94986676256892,
14.7425701579674));
#275306=CARTESIAN_POINT('Ctrl Pts',(0.212757545471486,1.94359583820583,
14.738662541725));
#275307=CARTESIAN_POINT('Ctrl Pts',(0.280707954473607,1.93373189566063,
14.7347549254826));
#275308=CARTESIAN_POINT('Ctrl Pts',(0.348615775030661,1.9238741354178,14.730849758369));
#275309=CARTESIAN_POINT('Ctrl Pts',(0.416052280675558,1.91042789465421,
14.7269445912553));
#275310=CARTESIAN_POINT('Ctrl Pts',(0.482613642004295,1.89346245607124,
14.7230394241417));
#275311=CARTESIAN_POINT('Ctrl Pts',(0.549156114933165,1.87650183184276,
14.7191353652139));
#275312=CARTESIAN_POINT('Ctrl Pts',(0.614823460133153,1.85602411373327,
14.7152313062861));
#275313=CARTESIAN_POINT('Ctrl Pts',(0.679223711395073,1.83214932521307,
14.7113272473583));
#275314=CARTESIAN_POINT('Ctrl Pts',(0.743627775053325,1.80827312334192,
14.7074229573162));
#275315=CARTESIAN_POINT('Ctrl Pts',(0.806764135539207,1.78099962518855,
14.7035186672741));
#275316=CARTESIAN_POINT('Ctrl Pts',(0.868259335773061,1.75049756522051,
14.6996143772319));
#275317=CARTESIAN_POINT('Ctrl Pts',(0.92982003819369,1.71996301569845,14.6957059284988));
#275318=CARTESIAN_POINT('Ctrl Pts',(0.989735650203325,1.68619326030272,
14.6917974797657));
#275319=CARTESIAN_POINT('Ctrl Pts',(1.04765684446948,1.6494032667108,14.6878890310326));
#275320=CARTESIAN_POINT('Ctrl Pts',(1.10561270853501,1.6125912517895,14.6839782428254));
#275321=CARTESIAN_POINT('Ctrl Pts',(1.16157137821388,1.57275568607684,14.6800674546182));
#275322=CARTESIAN_POINT('Ctrl Pts',(1.21521440622377,1.53015356971325,14.676156666411));
#275323=CARTESIAN_POINT('Ctrl Pts',(1.26895005846096,1.48747789321975,14.6722391255325));
#275324=CARTESIAN_POINT('Ctrl Pts',(1.32036172060979,1.44202645768731,14.668321584654));
#275325=CARTESIAN_POINT('Ctrl Pts',(1.36916642599834,1.39409443651387,14.6644040437755));
#275326=CARTESIAN_POINT('Ctrl Pts',(1.39220000280892,1.37147272652516,14.6625551446168));
#275327=CARTESIAN_POINT('Ctrl Pts',(1.41465347216608,1.34829898736798,14.6607062454581));
#275328=CARTESIAN_POINT('Ctrl Pts',(1.43650026735261,1.32460672725752,14.6588573462994));
#275329=CARTESIAN_POINT('Ctrl Pts',(1.48279716496029,1.27439899055916,14.6549392295089));
#275330=CARTESIAN_POINT('Ctrl Pts',(1.52655042044952,1.22166159012838,14.6510211127185));
#275331=CARTESIAN_POINT('Ctrl Pts',(1.56747167823192,1.16668270662628,14.6471029959281));
#275332=CARTESIAN_POINT('Ctrl Pts',(1.60833131545921,1.1117866121073,14.6431907791648));
#275333=CARTESIAN_POINT('Ctrl Pts',(1.64636712720353,1.05465612469319,14.6392785624015));
#275334=CARTESIAN_POINT('Ctrl Pts',(1.68132917142388,0.995614492320737,
14.6353663456382));
#275335=CARTESIAN_POINT('Ctrl Pts',(1.71625010247877,0.936642289195202,
14.6314587293958));
#275336=CARTESIAN_POINT('Ctrl Pts',(1.74810419513703,0.875763825691861,
14.6275511131535));
#275337=CARTESIAN_POINT('Ctrl Pts',(1.77668429032641,0.813331994026637,
14.6236434969111));
#275338=CARTESIAN_POINT('Ctrl Pts',(1.80524647271982,0.750939291995364,
14.6197383297974));
#275339=CARTESIAN_POINT('Ctrl Pts',(1.83053852388676,0.68699559932706,14.6158331626838));
#275340=CARTESIAN_POINT('Ctrl Pts',(1.8523995480318,0.621877732718885,14.6119279955702));
#275341=CARTESIAN_POINT('Ctrl Pts',(1.87425436858127,0.556778344883991,
14.6080239366424));
#275342=CARTESIAN_POINT('Ctrl Pts',(1.89267993847419,0.490505910654328,
14.6041198777146));
#275343=CARTESIAN_POINT('Ctrl Pts',(1.90756442185842,0.423454810410668,
14.6002158187868));
#275344=CARTESIAN_POINT('Ctrl Pts',(1.92244978638131,0.356399740844437,
14.5963115287446));
#275345=CARTESIAN_POINT('Ctrl Pts',(1.9337935441209,0.288566394492564,14.5924072387025));
#275346=CARTESIAN_POINT('Ctrl Pts',(1.94153481981558,0.220360031411555,
14.5885029486604));
#275347=CARTESIAN_POINT('Ctrl Pts',(1.94928434120234,0.152081017686014,
14.5845944999273));
#275348=CARTESIAN_POINT('Ctrl Pts',(1.95342366706846,0.0834286839793453,
14.5806860511942));
#275349=CARTESIAN_POINT('Ctrl Pts',(1.95394385076509,0.0148131042422796,
14.5767776024611));
#275350=CARTESIAN_POINT('Ctrl Pts',(1.95446434582726,-0.0538435466158792,
14.5728668142538));
#275351=CARTESIAN_POINT('Ctrl Pts',(1.95136140959826,-0.122462908276107,
14.5689560260466));
#275352=CARTESIAN_POINT('Ctrl Pts',(1.94467815763461,-0.190638042422939,
14.5650452378394));
#275353=CARTESIAN_POINT('Ctrl Pts',(1.93798336584796,-0.258930893062583,
14.5611276969609));
#275354=CARTESIAN_POINT('Ctrl Pts',(1.92769599364402,-0.326777499241707,
14.5572101560824));
#275355=CARTESIAN_POINT('Ctrl Pts',(1.91391047295192,-0.393780016665343,
14.5532926152039));
#275356=CARTESIAN_POINT('Ctrl Pts',(1.90740434106983,-0.425402123985535,
14.5514437160453));
#275357=CARTESIAN_POINT('Ctrl Pts',(1.90011975577961,-0.456836425151338,
14.5495948168866));
#275358=CARTESIAN_POINT('Ctrl Pts',(1.89207045129286,-0.488042423713781,
14.547745917728));
#275359=CARTESIAN_POINT('Ctrl Pts',(1.87501267130884,-0.55417298922247,
14.5438278009376));
#275360=CARTESIAN_POINT('Ctrl Pts',(1.85444986686256,-0.61953927903166,
14.5399096841471));
#275361=CARTESIAN_POINT('Ctrl Pts',(1.83046767206848,-0.683742715875045,
14.5359915673567));
#275362=CARTESIAN_POINT('Ctrl Pts',(1.80652159043993,-0.74784947310416,
14.5320793505934));
#275363=CARTESIAN_POINT('Ctrl Pts',(1.77916650819632,-0.81079639552836,
14.5281671338301));
#275364=CARTESIAN_POINT('Ctrl Pts',(1.74853835796165,-0.872198148780866,
14.5242549170668));
#275365=CARTESIAN_POINT('Ctrl Pts',(1.71794622450565,-0.933527697432714,
14.5203473008244));
#275366=CARTESIAN_POINT('Ctrl Pts',(1.68408888559597,-0.993315247470937,
14.5164396845821));
#275367=CARTESIAN_POINT('Ctrl Pts',(1.64715038750284,-1.05119532007579,
14.5125320683397));
#275368=CARTESIAN_POINT('Ctrl Pts',(1.61023504089945,-1.10903911589691,
14.508626901226));
#275369=CARTESIAN_POINT('Ctrl Pts',(1.57024262990491,-1.16497739212295,
14.5047217341124));
#275370=CARTESIAN_POINT('Ctrl Pts',(1.52740239786812,-1.21867055227683,
14.5008165669987));
#275371=CARTESIAN_POINT('Ctrl Pts',(1.48457432278571,-1.27234847569489,
14.4969125080709));
#275372=CARTESIAN_POINT('Ctrl Pts',(1.43890033758603,-1.3237821634938,14.4930084491431));
#275373=CARTESIAN_POINT('Ctrl Pts',(1.39065105676619,-1.37266370182761,
14.4891043902153));
#275374=CARTESIAN_POINT('Ctrl Pts',(1.34239891966273,-1.42154813387372,
14.4852001001732));
#275375=CARTESIAN_POINT('Ctrl Pts',(1.29157153162983,-1.46787976823632,
14.481295810131));
#275376=CARTESIAN_POINT('Ctrl Pts',(1.23847629474704,-1.51138759666396,
14.4773915200889));
#275377=CARTESIAN_POINT('Ctrl Pts',(1.18532450297689,-1.55494176786131,
14.4734830713558));
#275378=CARTESIAN_POINT('Ctrl Pts',(1.12990042271788,-1.59566581811973,
14.4695746226227));
#275379=CARTESIAN_POINT('Ctrl Pts',(1.07254367340351,-1.63332974890011,
14.4656661738895));
#275380=CARTESIAN_POINT('Ctrl Pts',(1.01515259214869,-1.67101622412111,
14.4617553856823));
#275381=CARTESIAN_POINT('Ctrl Pts',(0.955826964408324,-1.7056386864992,
14.4578445974751));
#275382=CARTESIAN_POINT('Ctrl Pts',(0.894932021626566,-1.73701257239762,
14.4539338092679));
#275383=CARTESIAN_POINT('Ctrl Pts',(0.833931932897054,-1.7684406308893,
14.4500162683894));
#275384=CARTESIAN_POINT('Ctrl Pts',(0.771357569288752,-1.79660871594869,
14.4460987275109));
#275385=CARTESIAN_POINT('Ctrl Pts',(0.707594364402169,-1.8213803050067,
14.4421811866323));
#275386=CARTESIAN_POINT('Ctrl Pts',(0.677501063650518,-1.83307135599676,
14.4403322874737));
#275387=CARTESIAN_POINT('Ctrl Pts',(0.647143180102627,-1.84400659166273,
14.4384833883152));
#275388=CARTESIAN_POINT('Ctrl Pts',(0.616562183300354,-1.85417557801949,
14.4366344891566));
#275389=CARTESIAN_POINT('Ctrl Pts',(0.551756097753758,-1.87572530721959,
14.4327163723661));
#275390=CARTESIAN_POINT('Ctrl Pts',(0.485690395251855,-1.89391606649548,
14.4287982555757));
#275391=CARTESIAN_POINT('Ctrl Pts',(0.418746351910798,-1.90860354520298,
14.4248801387853));
#275392=CARTESIAN_POINT('Ctrl Pts',(0.351903115078058,-1.92326890702942,
14.420967922022));
#275393=CARTESIAN_POINT('Ctrl Pts',(0.284184638953922,-1.93444135343305,
14.4170557052587));
#275394=CARTESIAN_POINT('Ctrl Pts',(0.215988364403192,-1.94202601075331,
14.4131434884954));
#275395=CARTESIAN_POINT('Ctrl Pts',(0.147872284382886,-1.94960174899352,
14.4092358722531));
#275396=CARTESIAN_POINT('Ctrl Pts',(0.0792800083515805,-1.95359802306459,
14.4053282560107));
#275397=CARTESIAN_POINT('Ctrl Pts',(0.0106184017329989,-1.95397114859576,
14.4014206397683));
#275398=CARTESIAN_POINT('Ctrl Pts',(-0.0580001706919385,-1.95434404026761,
14.3975154726547));
#275399=CARTESIAN_POINT('Ctrl Pts',(-0.126687496737633,-1.95109828535075,
14.393610305541));
#275400=CARTESIAN_POINT('Ctrl Pts',(-0.195033931461197,-1.94424220856836,
14.3897051384274));
#275401=CARTESIAN_POINT('Ctrl Pts',(-0.263360971226991,-1.93738807736398,
14.3858010794996));
#275402=CARTESIAN_POINT('Ctrl Pts',(-0.331346822514729,-1.92692570720796,
14.3818970205718));
#275403=CARTESIAN_POINT('Ctrl Pts',(-0.398586008999103,-1.91291536494173,
14.377992961644));
#275404=CARTESIAN_POINT('Ctrl Pts',(-0.465829175940538,-1.89890419328466,
14.3740886716018));
#275405=CARTESIAN_POINT('Ctrl Pts',(-0.53232510931066,-1.88134473537189,
14.3701843815597));
#275406=CARTESIAN_POINT('Ctrl Pts',(-0.597679375619929,-1.86034818352871,
14.3662800915176));
#275407=CARTESIAN_POINT('Ctrl Pts',(-0.663103254636134,-1.8393292670123,
14.3623716427845));
#275408=CARTESIAN_POINT('Ctrl Pts',(-0.727382570513591,-1.81486610098012,
14.3584631940514));
#275409=CARTESIAN_POINT('Ctrl Pts',(-0.790139859719754,-1.7871191907878,
14.3545547453182));
#275410=CARTESIAN_POINT('Ctrl Pts',(-0.852934713459206,-1.75935567217048,
14.350643957111));
#275411=CARTESIAN_POINT('Ctrl Pts',(-0.914205288582151,-1.72830471997885,
14.3467331689038));
#275412=CARTESIAN_POINT('Ctrl Pts',(-0.97359839248268,-1.69417300478881,
14.3428223806966));
#275413=CARTESIAN_POINT('Ctrl Pts',(-1.03309404913903,-1.65998235512281,
14.3389048398181));
#275414=CARTESIAN_POINT('Ctrl Pts',(-1.09070535174908,-1.62270059271197,
14.3349872989396));
#275415=CARTESIAN_POINT('Ctrl Pts',(-1.1461085029673,-1.58257742288523,
14.3310697580611));
#275416=CARTESIAN_POINT('Ctrl Pts',(-1.17225624279953,-1.56364113166703,
14.3292208589024));
#275417=CARTESIAN_POINT('Ctrl Pts',(-1.19791262477217,-1.54407252066101,
14.3273719597438));
#275418=CARTESIAN_POINT('Ctrl Pts',(-1.22304638500535,-1.5239007645268,
14.3255230605851));
#275419=CARTESIAN_POINT('Ctrl Pts',(-1.27563331533746,-1.48169574925391,
14.3216546409637));
#275420=CARTESIAN_POINT('Ctrl Pts',(-1.3261501296571,-1.43667130044735,
14.3177862213423));
#275421=CARTESIAN_POINT('Ctrl Pts',(-1.37427307974457,-1.38906065464737,
14.3139178017208));
#275422=CARTESIAN_POINT('Ctrl Pts',(-1.42231339471332,-1.34153176425434,
14.31005602482));
#275423=CARTESIAN_POINT('Ctrl Pts',(-1.46796764949847,-1.29142584504702,
14.3061942479193));
#275424=CARTESIAN_POINT('Ctrl Pts',(-1.51094458999001,-1.23901672546416,
14.3023324710185));
#275425=CARTESIAN_POINT('Ctrl Pts',(-1.55388041591974,-1.18665774388466,
14.2984743885469));
#275426=CARTESIAN_POINT('Ctrl Pts',(-1.59414368403146,-1.13200031688669,
14.2946163060754));
#275427=CARTESIAN_POINT('Ctrl Pts',(-1.6314805829482,-1.07535441016579,
14.2907582236038));
#275428=CARTESIAN_POINT('Ctrl Pts',(-1.66879534981622,-1.01874208121924,
14.2869024280728));
#275429=CARTESIAN_POINT('Ctrl Pts',(-1.70318690899608,-0.960144030741889,
14.2830466325418));
#275430=CARTESIAN_POINT('Ctrl Pts',(-1.73444351762022,-0.899900930205772,
14.2791908370109));
#275431=CARTESIAN_POINT('Ctrl Pts',(-1.76569297032403,-0.839671621787436,
14.2753359242297));
#275432=CARTESIAN_POINT('Ctrl Pts',(-1.79380866506376,-0.777798459862591,
14.2714810114485));
#275433=CARTESIAN_POINT('Ctrl Pts',(-1.81862474501653,-0.71464679164854,
14.2676260986674));
#275434=CARTESIAN_POINT('Ctrl Pts',(-1.84345890682138,-0.651449108950134,
14.2637683770638));
#275435=CARTESIAN_POINT('Ctrl Pts',(-1.8649884655503,-0.586971530388544,
14.2599106554601));
#275436=CARTESIAN_POINT('Ctrl Pts',(-1.88309618852626,-0.521598259926026,
14.2560529338565));
#275437=CARTESIAN_POINT('Ctrl Pts',(-1.90121085946659,-0.45619990562752,
14.2521937320385));
#275438=CARTESIAN_POINT('Ctrl Pts',(-1.91590096983881,-0.389905669032521,
14.2483345302205));
#275439=CARTESIAN_POINT('Ctrl Pts',(-1.9271002332678,-0.323110957627873,
14.2444753284025));
#275440=CARTESIAN_POINT('Ctrl Pts',(-1.9383168977339,-0.256212462857527,
14.2406101302871));
#275441=CARTESIAN_POINT('Ctrl Pts',(-1.94603182977727,-0.18881244354424,
14.2367449321717));
#275442=CARTESIAN_POINT('Ctrl Pts',(-1.9502306389416,-0.121311396552158,
14.2328797340563));
#275443=CARTESIAN_POINT('Ctrl Pts',(-1.95276900197994,-0.080504073325935,
14.230543053429));
#275444=CARTESIAN_POINT('Ctrl Pts',(-1.95402333266491,-0.0396598555490369,
14.2282063728017));
#275445=CARTESIAN_POINT('Ctrl Pts',(-1.95399967130156,0.00113338140508406,
14.2258696921744));
#275446=CARTESIAN_POINT('',(-1.95399924704828,-0.00171538181413171,13.5258696921242));
#275447=CARTESIAN_POINT('Ctrl Pts',(-1.95399967130105,0.00113338228141676,
14.2258696921242));
#275448=CARTESIAN_POINT('Ctrl Pts',(-1.95396099627773,0.0678107815027306,
14.2220503387541));
#275449=CARTESIAN_POINT('Ctrl Pts',(-1.95050967149899,0.134387737031145,
14.2182309853839));
#275450=CARTESIAN_POINT('Ctrl Pts',(-1.94367482159854,0.200609540859539,
14.2144116320137));
#275451=CARTESIAN_POINT('Ctrl Pts',(-1.93666323153074,0.268543752840517,
14.2104935152232));
#275452=CARTESIAN_POINT('Ctrl Pts',(-1.92607185784042,0.336244591636888,
14.2065753984326));
#275453=CARTESIAN_POINT('Ctrl Pts',(-1.91192597679905,0.403305168874657,
14.2026572816421));
#275454=CARTESIAN_POINT('Ctrl Pts',(-1.89780139708343,0.470264764123595,
14.1987450648787));
#275455=CARTESIAN_POINT('Ctrl Pts',(-1.88013303352604,0.536585533846818,
14.1948328481153));
#275456=CARTESIAN_POINT('Ctrl Pts',(-1.85899787281899,0.601866188495818,
14.1909206313519));
#275457=CARTESIAN_POINT('Ctrl Pts',(-1.83788756573183,0.667070077200144,
14.1870130151094));
#275458=CARTESIAN_POINT('Ctrl Pts',(-1.81331870874471,0.731235814195912,
14.1831053988669));
#275459=CARTESIAN_POINT('Ctrl Pts',(-1.78541882401548,0.793974573176728,
14.1791977826244));
#275460=CARTESIAN_POINT('Ctrl Pts',(-1.75753642575506,0.856674010154522,
14.1752926155107));
#275461=CARTESIAN_POINT('Ctrl Pts',(-1.72632734059869,0.917947794828203,
14.1713874483969));
#275462=CARTESIAN_POINT('Ctrl Pts',(-1.69196764037068,0.977425958289674,
14.1674822812832));
#275463=CARTESIAN_POINT('Ctrl Pts',(-1.65761769054058,1.03688724338034,
14.1635782223553));
#275464=CARTESIAN_POINT('Ctrl Pts',(-1.62011914644008,1.09455349308656,
14.1596741634274));
#275465=CARTESIAN_POINT('Ctrl Pts',(-1.57969371079616,1.15007990160295,
14.1557701044995));
#275466=CARTESIAN_POINT('Ctrl Pts',(-1.53926588202827,1.20560959719782,
14.1518658144572));
#275467=CARTESIAN_POINT('Ctrl Pts',(-1.4959111093021,1.25899880396326,14.147961524415));
#275468=CARTESIAN_POINT('Ctrl Pts',(-1.44989297226855,1.3099337269367,14.1440572343728));
#275469=CARTESIAN_POINT('Ctrl Pts',(-1.40382581858658,1.36092290371902,
14.1401487856396));
#275470=CARTESIAN_POINT('Ctrl Pts',(-1.35508996939058,1.40945221388702,
14.1362403369064));
#275471=CARTESIAN_POINT('Ctrl Pts',(-1.30398697371899,1.45524361272304,
14.1323318881732));
#275472=CARTESIAN_POINT('Ctrl Pts',(-1.25285338940657,1.50106242084561,
14.1284210999659));
#275473=CARTESIAN_POINT('Ctrl Pts',(-1.19935022191233,1.54413974755261,
14.1245103117586));
#275474=CARTESIAN_POINT('Ctrl Pts',(-1.14381111758975,1.58423865856067,
14.1205995235513));
#275475=CARTESIAN_POINT('Ctrl Pts',(-1.08817611512694,1.62440680746943,
14.1166819826727));
#275476=CARTESIAN_POINT('Ctrl Pts',(-1.03049857285806,1.66158601019015,
14.1127644417941));
#275477=CARTESIAN_POINT('Ctrl Pts',(-0.971139273420767,1.69558382618489,
14.1088469009154));
#275478=CARTESIAN_POINT('Ctrl Pts',(-0.943124413555305,1.71162923204131,
14.1069980017577));
#275479=CARTESIAN_POINT('Ctrl Pts',(-0.914735283688362,1.72696669522707,
14.1051491026));
#275480=CARTESIAN_POINT('Ctrl Pts',(-0.886011335217463,1.74157971791881,
14.1033002034423));
#275481=CARTESIAN_POINT('Ctrl Pts',(-0.825140635849454,1.77254707994524,
14.0993820866519));
#275482=CARTESIAN_POINT('Ctrl Pts',(-0.762523786706094,1.80038071020465,
14.0954639698615));
#275483=CARTESIAN_POINT('Ctrl Pts',(-0.698516298684525,1.82488108666622,
14.0915458530711));
#275484=CARTESIAN_POINT('Ctrl Pts',(-0.634605195211164,1.84934456966752,
14.0876336363079));
#275485=CARTESIAN_POINT('Ctrl Pts',(-0.569308064526748,1.87048458602418,
14.0837214195446));
#275486=CARTESIAN_POINT('Ctrl Pts',(-0.503003769532962,1.88814808948759,
14.0798092027813));
#275487=CARTESIAN_POINT('Ctrl Pts',(-0.436777444220597,1.90579082178168,
14.075901586539));
#275488=CARTESIAN_POINT('Ctrl Pts',(-0.369546779812551,1.91996503431085,
14.0719939702966));
#275489=CARTESIAN_POINT('Ctrl Pts',(-0.301707587451943,1.93056689386147,
14.0680863540542));
#275490=CARTESIAN_POINT('Ctrl Pts',(-0.233910913830512,1.94116210861452,
14.0641811869406));
#275491=CARTESIAN_POINT('Ctrl Pts',(-0.165506953722486,1.94818933607535,
14.060276019827));
#275492=CARTESIAN_POINT('Ctrl Pts',(-0.0969020178623522,1.95159575704965,
14.0563708527133));
#275493=CARTESIAN_POINT('Ctrl Pts',(-0.0283165503158982,1.95500121136942,
14.0524667937856));
#275494=CARTESIAN_POINT('Ctrl Pts',(0.0404692887207486,1.95478787456847,
14.0485627348578));
#275495=CARTESIAN_POINT('Ctrl Pts',(0.10904556944404,1.9509549107513,14.04465867593));
#275496=CARTESIAN_POINT('Ctrl Pts',(0.177625909778235,1.94712172002855,
14.0407543858879));
#275497=CARTESIAN_POINT('Ctrl Pts',(0.245996176201372,1.93966850688678,
14.0368500958457));
#275498=CARTESIAN_POINT('Ctrl Pts',(0.31374976880134,1.9286464379396,14.0329458058036));
#275499=CARTESIAN_POINT('Ctrl Pts',(0.381575529773145,1.91761262873276,
14.0290373570705));
#275500=CARTESIAN_POINT('Ctrl Pts',(0.448782819611164,1.90300245643445,
14.0251289083374));
#275501=CARTESIAN_POINT('Ctrl Pts',(0.514974469532562,1.88491837906305,
14.0212204596043));
#275502=CARTESIAN_POINT('Ctrl Pts',(0.581205739687136,1.86682347713351,
14.0173096713971));
#275503=CARTESIAN_POINT('Ctrl Pts',(0.646419692976838,1.84525068630374,
14.0133988831899));
#275504=CARTESIAN_POINT('Ctrl Pts',(0.710236280311381,1.82035173143254,
14.0094880949827));
#275505=CARTESIAN_POINT('Ctrl Pts',(0.774163058332594,1.79540978408792,
14.0055705541042));
#275506=CARTESIAN_POINT('Ctrl Pts',(0.836687206903627,1.76713041276687,
14.0016530132257));
#275507=CARTESIAN_POINT('Ctrl Pts',(0.897451330277916,1.7357122773612,13.9977354723472));
#275508=CARTESIAN_POINT('Ctrl Pts',(0.926129202462533,1.72088436211435,
13.9958865731884));
#275509=CARTESIAN_POINT('Ctrl Pts',(0.954415441251867,1.70535795982813,
13.9940376740296));
#275510=CARTESIAN_POINT('Ctrl Pts',(0.982274783907155,1.68915725996727,
13.9921887748708));
#275511=CARTESIAN_POINT('Ctrl Pts',(1.04131324347289,1.65482535287576,13.9882706580804));
#275512=CARTESIAN_POINT('Ctrl Pts',(1.09866664513048,1.61732644504668,13.98435254129));
#275513=CARTESIAN_POINT('Ctrl Pts',(1.15397450463527,1.57685092594442,13.9804344244996));
#275514=CARTESIAN_POINT('Ctrl Pts',(1.2091990797742,1.53643635618954,13.9765222077363));
#275515=CARTESIAN_POINT('Ctrl Pts',(1.26238383220613,1.49305435904853,13.972609990973));
#275516=CARTESIAN_POINT('Ctrl Pts',(1.31319464913323,1.44694015546182,13.9686977742097));
#275517=CARTESIAN_POINT('Ctrl Pts',(1.3639457157348,1.40088017927868,13.9647901579674));
#275518=CARTESIAN_POINT('Ctrl Pts',(1.41232802847653,1.35209470652972,13.960882541725));
#275519=CARTESIAN_POINT('Ctrl Pts',(1.45803961969731,1.30085989537418,13.9569749254826));
#275520=CARTESIAN_POINT('Ctrl Pts',(1.5037225608243,1.2496571960333,13.953069758369));
#275521=CARTESIAN_POINT('Ctrl Pts',(1.54673777417703,1.19600856972771,13.9491645912554));
#275522=CARTESIAN_POINT('Ctrl Pts',(1.58682044878298,1.14022667190528,13.9452594241417));
#275523=CARTESIAN_POINT('Ctrl Pts',(1.62689174895831,1.08446060354863,13.9413553652139));
#275524=CARTESIAN_POINT('Ctrl Pts',(1.66403187551092,1.02656286469612,13.9374513062861));
#275525=CARTESIAN_POINT('Ctrl Pts',(1.69801772136349,0.966877354133167,
13.9335472473583));
#275526=CARTESIAN_POINT('Ctrl Pts',(1.73200557912613,0.907188310279321,
13.9296429573162));
#275527=CARTESIAN_POINT('Ctrl Pts',(1.76283854430515,0.845711713307905,
13.9257386672741));
#275528=CARTESIAN_POINT('Ctrl Pts',(1.79033899997154,0.78281687844661,13.921834377232));
#275529=CARTESIAN_POINT('Ctrl Pts',(1.81786874800509,0.719855050564654,
13.9179259284989));
#275530=CARTESIAN_POINT('Ctrl Pts',(1.84205870507964,0.655472421551075,
13.9140174797658));
#275531=CARTESIAN_POINT('Ctrl Pts',(1.8627794572565,0.590058212063163,13.9101090310327));
#275532=CARTESIAN_POINT('Ctrl Pts',(1.88351261222184,0.52460484769339,13.9061982428255));
#275533=CARTESIAN_POINT('Ctrl Pts',(1.90077230594726,0.458119150130883,
13.9022874546183));
#275534=CARTESIAN_POINT('Ctrl Pts',(1.91447979817761,0.391002688443205,
13.8983766664111));
#275535=CARTESIAN_POINT('Ctrl Pts',(1.92821095883092,0.323770338248981,
13.8944591255326));
#275536=CARTESIAN_POINT('Ctrl Pts',(1.9383776036575,0.255905536401278,13.8905415846541));
#275537=CARTESIAN_POINT('Ctrl Pts',(1.94495270955195,0.187816286851116,
13.8866240437756));
#275538=CARTESIAN_POINT('Ctrl Pts',(1.9480558571984,0.155681291935121,13.8847751446169));
#275539=CARTESIAN_POINT('Ctrl Pts',(1.95035977824699,0.123496319967377,
13.8829262454581));
#275540=CARTESIAN_POINT('Ctrl Pts',(1.9518656609298,0.0913041164628929,
13.8810773462994));
#275541=CARTESIAN_POINT('Ctrl Pts',(1.95505687024807,0.0230836229466753,
13.8771592295089));
#275542=CARTESIAN_POINT('Ctrl Pts',(1.95467349411293,-0.0454396124766511,
13.8732411127185));
#275543=CARTESIAN_POINT('Ctrl Pts',(1.95067988638708,-0.113859478502549,
13.8693229959281));
#275544=CARTESIAN_POINT('Ctrl Pts',(1.94669229236508,-0.182176315678574,
13.8654107791648));
#275545=CARTESIAN_POINT('Ctrl Pts',(1.93910528452002,-0.250389605287109,
13.8614985624015));
#275546=CARTESIAN_POINT('Ctrl Pts',(1.92793518405277,-0.318091065720813,
13.8575863456382));
#275547=CARTESIAN_POINT('Ctrl Pts',(1.91677821892126,-0.385712913494362,
13.8536787293958));
#275548=CARTESIAN_POINT('Ctrl Pts',(1.90204660892068,-0.452823644413003,
13.8497711131534));
#275549=CARTESIAN_POINT('Ctrl Pts',(1.88380850378713,-0.519019769430116,
13.845863496911));
#275550=CARTESIAN_POINT('Ctrl Pts',(1.86558182952721,-0.585174405513252,
13.8419583297973));
#275551=CARTESIAN_POINT('Ctrl Pts',(1.84385315007809,-0.650415099667435,
13.8380531626836));
#275552=CARTESIAN_POINT('Ctrl Pts',(1.81874143303448,-0.714349774104889,
13.83414799557));
#275553=CARTESIAN_POINT('Ctrl Pts',(1.79363684204934,-0.778266305528533,
13.8302439366422));
#275554=CARTESIAN_POINT('Ctrl Pts',(1.76515129901099,-0.840877095353031,
13.8263398777144));
#275555=CARTESIAN_POINT('Ctrl Pts',(1.73345264296861,-0.901808147326888,
13.8224358187865));
#275556=CARTESIAN_POINT('Ctrl Pts',(1.70175211041427,-0.962742806325828,
13.8185315287444));
#275557=CARTESIAN_POINT('Ctrl Pts',(1.66683831650622,-1.02199709487888,
13.8146272387023));
#275558=CARTESIAN_POINT('Ctrl Pts',(1.62892513120441,-1.07922144017374,
13.8107229486601));
#275559=CARTESIAN_POINT('Ctrl Pts',(1.59097156231926,-1.13650673851434,
13.806814499927));
#275560=CARTESIAN_POINT('Ctrl Pts',(1.55001249834279,-1.19175736765287,
13.8029060511939));
#275561=CARTESIAN_POINT('Ctrl Pts',(1.50630468257954,-1.24465344704418,
13.7989976024607));
#275562=CARTESIAN_POINT('Ctrl Pts',(1.46257070469682,-1.29758118835966,
13.7950868142535));
#275563=CARTESIAN_POINT('Ctrl Pts',(1.41608503347078,-1.34815121286628,
13.7911760260463));
#275564=CARTESIAN_POINT('Ctrl Pts',(1.36714227790619,-1.39607950775072,
13.787265237839));
#275565=CARTESIAN_POINT('Ctrl Pts',(1.31811501397054,-1.44409055935943,
13.7833476969605));
#275566=CARTESIAN_POINT('Ctrl Pts',(1.26662256706105,-1.48945045252723,
13.779430156082));
#275567=CARTESIAN_POINT('Ctrl Pts',(1.21299301048388,-1.53191512706065,
13.7755126152035));
#275568=CARTESIAN_POINT('Ctrl Pts',(1.18768232577094,-1.55195650083197,
13.773663716045));
#275569=CARTESIAN_POINT('Ctrl Pts',(1.16189604347026,-1.57135361705028,
13.7718148168865));
#275570=CARTESIAN_POINT('Ctrl Pts',(1.13567071565667,-1.59008428254601,
13.7699659177279));
#275571=CARTESIAN_POINT('Ctrl Pts',(1.08009499819913,-1.62977759661178,
13.7660478009375));
#275572=CARTESIAN_POINT('Ctrl Pts',(1.02232559979735,-1.66663241147189,
13.7621296841471));
#275573=CARTESIAN_POINT('Ctrl Pts',(0.96268432550937,-1.70039845019294,
13.7582115673567));
#275574=CARTESIAN_POINT('Ctrl Pts',(0.903132860983582,-1.73411364291945,
13.7542993505934));
#275575=CARTESIAN_POINT('Ctrl Pts',(0.841715539352873,-1.76474905006382,
13.7503871338302));
#275576=CARTESIAN_POINT('Ctrl Pts',(0.778784183350029,-1.79209687119972,
13.7464749170669));
#275577=CARTESIAN_POINT('Ctrl Pts',(0.715926830664457,-1.81941253301772,
13.7425673008245));
#275578=CARTESIAN_POINT('Ctrl Pts',(0.651559428515125,-1.84344809163674,
13.7386596845822));
#275579=CARTESIAN_POINT('Ctrl Pts',(0.586057893006253,-1.86404188419817,
13.7347520683398));
#275580=CARTESIAN_POINT('Ctrl Pts',(0.520597411091987,-1.88462276944065,
13.7308469012261));
#275581=CARTESIAN_POINT('Ctrl Pts',(0.454004674054457,-1.9017660205359,
13.7269417341125));
#275582=CARTESIAN_POINT('Ctrl Pts',(0.386673583144682,-1.91535885413101,
13.7230365669989));
#275583=CARTESIAN_POINT('Ctrl Pts',(0.319361599064237,-1.92894783043006,
13.7191325080711));
#275584=CARTESIAN_POINT('Ctrl Pts',(0.251312158982779,-1.93898829203193,
13.7152284491433));
#275585=CARTESIAN_POINT('Ctrl Pts',(0.182930490072227,-1.94541831897459,
13.7113243902155));
#275586=CARTESIAN_POINT('Ctrl Pts',(0.114544773071485,-1.95184872656502,
13.7074201001734));
#275587=CARTESIAN_POINT('Ctrl Pts',(0.0458272781528218,-1.95466823166777,
13.7035158101313));
#275588=CARTESIAN_POINT('Ctrl Pts',(-0.0228123100831663,-1.95386683233752,
13.6996115200892));
#275589=CARTESIAN_POINT('Ctrl Pts',(-0.0915250104175157,-1.9530645793893,
13.6957030713561));
#275590=CARTESIAN_POINT('Ctrl Pts',(-0.160159145670226,-1.94863373070259,
13.691794622623));
#275591=CARTESIAN_POINT('Ctrl Pts',(-0.228306712890433,-1.94061640847674,
13.6878861738899));
#275592=CARTESIAN_POINT('Ctrl Pts',(-0.296495071094226,-1.93259428733477,
13.6839753856827));
#275593=CARTESIAN_POINT('Ctrl Pts',(-0.364195796770205,-1.9209815033955,
13.6800645974755));
#275594=CARTESIAN_POINT('Ctrl Pts',(-0.431010473043962,-1.90587144690465,
13.6761538092683));
#275595=CARTESIAN_POINT('Ctrl Pts',(-0.497940516738045,-1.89073530021423,
13.6722362683898));
#275596=CARTESIAN_POINT('Ctrl Pts',(-0.563980984428117,-1.87208996234832,
13.6683187275113));
#275597=CARTESIAN_POINT('Ctrl Pts',(-0.628748864686283,-1.85007861053408,
13.6644011866328));
#275598=CARTESIAN_POINT('Ctrl Pts',(-0.659316326018667,-1.83969026460129,
13.662552287474));
#275599=CARTESIAN_POINT('Ctrl Pts',(-0.689600625865148,-1.82855286564416,
13.6607033883153));
#275600=CARTESIAN_POINT('Ctrl Pts',(-0.719563290249536,-1.81668507764149,
13.6588544891566));
#275601=CARTESIAN_POINT('Ctrl Pts',(-0.783059029244552,-1.79153531259394,
13.6549363723662));
#275602=CARTESIAN_POINT('Ctrl Pts',(-0.845360519085135,-1.76300278495008,
13.6510182555757));
#275603=CARTESIAN_POINT('Ctrl Pts',(-0.906082926910697,-1.73122203358233,
13.6471001387853));
#275604=CARTESIAN_POINT('Ctrl Pts',(-0.966713896968201,-1.69948913869914,
13.643187922022));
#275605=CARTESIAN_POINT('Ctrl Pts',(-1.02577007187256,-1.66451795380519,
13.6392757052587));
#275606=CARTESIAN_POINT('Ctrl Pts',(-1.0828860142905,-1.62649127881278,
13.6353634884955));
#275607=CARTESIAN_POINT('Ctrl Pts',(-1.13993479195181,-1.5885093207989,
13.6314558722531));
#275608=CARTESIAN_POINT('Ctrl Pts',(-1.19504746090461,-1.54747927987148,
13.6275482560107));
#275609=CARTESIAN_POINT('Ctrl Pts',(-1.24788426892885,-1.50362922669118,
13.6236406397683));
#275610=CARTESIAN_POINT('Ctrl Pts',(-1.30068796107453,-1.45980665687125,
13.6197354726547));
#275611=CARTESIAN_POINT('Ctrl Pts',(-1.35121824418428,-1.41316789431115,
13.615830305541));
#275612=CARTESIAN_POINT('Ctrl Pts',(-1.3991666684344,-1.36398263696507,
13.6119251384274));
#275613=CARTESIAN_POINT('Ctrl Pts',(-1.44710148615675,-1.31481133712812,
13.6080210794996));
#275614=CARTESIAN_POINT('Ctrl Pts',(-1.49245555629169,-1.26309532909577,
13.6041170205718));
#275615=CARTESIAN_POINT('Ctrl Pts',(-1.53495701085206,-1.20914142052785,
13.600212961644));
#275616=CARTESIAN_POINT('Ctrl Pts',(-1.5774609814335,-1.1551843179711,13.5963086716018));
#275617=CARTESIAN_POINT('Ctrl Pts',(-1.61711169881252,-1.09898943983908,
13.5924043815597));
#275618=CARTESIAN_POINT('Ctrl Pts',(-1.65367848921153,-1.04089550595584,
13.5885000915176));
#275619=CARTESIAN_POINT('Ctrl Pts',(-1.69028422906881,-0.982739692776438,
13.5845916427845));
#275620=CARTESIAN_POINT('Ctrl Pts',(-1.72379922382787,-0.92268120404838,
13.5806831940514));
#275621=CARTESIAN_POINT('Ctrl Pts',(-1.75403749779322,-0.86108562659895,
13.5767747453182));
#275622=CARTESIAN_POINT('Ctrl Pts',(-1.78429387143533,-0.799453179980236,
13.572863957111));
#275623=CARTESIAN_POINT('Ctrl Pts',(-1.81126942765639,-0.736282265989115,
13.5689531689038));
#275624=CARTESIAN_POINT('Ctrl Pts',(-1.83482645819514,-0.671958234049603,
13.5650423806966));
#275625=CARTESIAN_POINT('Ctrl Pts',(-1.85842416413629,-0.607523135230167,
13.5611248398181));
#275626=CARTESIAN_POINT('Ctrl Pts',(-1.87859141908748,-0.541931414528383,
13.5572072989395));
#275627=CARTESIAN_POINT('Ctrl Pts',(-1.89524069535008,-0.475582491991621,
13.553289758061));
#275628=CARTESIAN_POINT('Ctrl Pts',(-1.9030983881805,-0.444268851404427,
13.5514408589024));
#275629=CARTESIAN_POINT('Ctrl Pts',(-1.91017322836625,-0.412786680116798,
13.5495919597437));
#275630=CARTESIAN_POINT('Ctrl Pts',(-1.91646002034225,-0.381178423352868,
13.5477430605851));
#275631=CARTESIAN_POINT('Ctrl Pts',(-1.935685974682,-0.284515625598044,
13.5420888491942));
#275632=CARTESIAN_POINT('Ctrl Pts',(-1.94760342518579,-0.186354486565157,
13.5364346378032));
#275633=CARTESIAN_POINT('Ctrl Pts',(-1.95203518396287,-0.087605025946325,
13.5307804264123));
#275634=CARTESIAN_POINT('Ctrl Pts',(-1.953318191635,-0.0590167561496238,
13.5291435149829));
#275635=CARTESIAN_POINT('Ctrl Pts',(-1.95397408345252,-0.0303793484914462,
13.5275066035536));
#275636=CARTESIAN_POINT('Ctrl Pts',(-1.95399924704828,-0.00171538181413171,
13.5258696921242));
#275637=CARTESIAN_POINT('',(-1.95079785653176,-3.37693124380367E-5,12.8258696921242));
#275638=CARTESIAN_POINT('Ctrl Pts',(-1.95470780459474,-0.00170932991778109,
13.5258693111351));
#275639=CARTESIAN_POINT('Ctrl Pts',(-1.94992637237433,0.51936472124033,
13.4961234180947));
#275640=CARTESIAN_POINT('Ctrl Pts',(-1.46762209028228,1.69704725867551,
13.429340382197));
#275641=CARTESIAN_POINT('Ctrl Pts',(0.520936993743039,2.24981806562466,
13.3255202034423));
#275642=CARTESIAN_POINT('Ctrl Pts',(2.17254014841156,0.783023616121871,
13.2144087748708));
#275643=CARTESIAN_POINT('Ctrl Pts',(1.83645968680275,-1.40016873933449,
13.1032973462993));
#275644=CARTESIAN_POINT('Ctrl Pts',(-0.179820256539059,-2.3023295496518,
12.992185917728));
#275645=CARTESIAN_POINT('Ctrl Pts',(-1.72100430673717,-1.30004007511163,
12.899710033003));
#275646=CARTESIAN_POINT('Ctrl Pts',(-1.95084782093774,-0.324022277657586,
12.844271291135));
#275647=CARTESIAN_POINT('Ctrl Pts',(-1.95079785653176,-3.37693124380367E-5,
12.8258696921242));
#275648=CARTESIAN_POINT('',(-1.95399923090066,0.0017336780615255,12.1258696921242));
#275649=CARTESIAN_POINT('Ctrl Pts',(-1.95079785653176,-3.37693124380367E-5,
12.8258696921242));
#275650=CARTESIAN_POINT('Ctrl Pts',(-1.95074725691387,0.32807369838409,
12.8072341482779));
#275651=CARTESIAN_POINT('Ctrl Pts',(-1.71669518394517,1.30834496185473,
12.7515614615743));
#275652=CARTESIAN_POINT('Ctrl Pts',(-0.165312909848787,2.30341666263357,
12.6588516320137));
#275653=CARTESIAN_POINT('Ctrl Pts',(1.84524376358971,1.38857197609474,12.5477402034423));
#275654=CARTESIAN_POINT('Ctrl Pts',(2.1675642957523,-0.796694234723817,
12.4366287748709));
#275655=CARTESIAN_POINT('Ctrl Pts',(0.506753680239931,-2.25305512303262,
12.3255173462994));
#275656=CARTESIAN_POINT('Ctrl Pts',(-1.47381110597352,-1.68904181734237,
12.221931090597));
#275657=CARTESIAN_POINT('Ctrl Pts',(-1.94982291098112,-0.515331947862959,
12.1553819777518));
#275658=CARTESIAN_POINT('Ctrl Pts',(-1.95458395099462,0.00172866677834459,
12.1258700077636));
#275659=CARTESIAN_POINT('',(-1.95399970412604,-0.00107530244352288,11.4258696921242));
#275660=CARTESIAN_POINT('Ctrl Pts',(-1.95399923090066,0.0017336780615255,
12.1258696921242));
#275661=CARTESIAN_POINT('Ctrl Pts',(-1.95391274729375,0.0992078891813078,
12.1203044978164));
#275662=CARTESIAN_POINT('Ctrl Pts',(-1.94652911131939,0.19636936180308,
12.1147393035087));
#275663=CARTESIAN_POINT('Ctrl Pts',(-1.93200815213827,0.292336279088428,
12.1091741092009));
#275664=CARTESIAN_POINT('Ctrl Pts',(-1.92689436108002,0.32613258395921,
12.1072142358528));
#275665=CARTESIAN_POINT('Ctrl Pts',(-1.9208957923614,0.359781016894373,
12.1052543625046));
#275666=CARTESIAN_POINT('Ctrl Pts',(-1.91402071706402,0.39324381069478,
12.1032944891565));
#275667=CARTESIAN_POINT('Ctrl Pts',(-1.90027628404543,0.460141569353427,
12.099376372366));
#275668=CARTESIAN_POINT('Ctrl Pts',(-1.88299312449379,0.526450491574315,
12.0954582555756));
#275669=CARTESIAN_POINT('Ctrl Pts',(-1.86223692385971,0.591768231162787,
12.0915401387851));
#275670=CARTESIAN_POINT('Ctrl Pts',(-1.84151197858469,0.656987613183806,
12.0876279220218));
#275671=CARTESIAN_POINT('Ctrl Pts',(-1.81732451933111,0.721218309756002,
12.0837157052585));
#275672=CARTESIAN_POINT('Ctrl Pts',(-1.78979112696608,0.784068697139146,
12.0798034884952));
#275673=CARTESIAN_POINT('Ctrl Pts',(-1.76229011213906,0.846845176419049,
12.0758958722528));
#275674=CARTESIAN_POINT('Ctrl Pts',(-1.73145117482954,0.908244121713762,
12.0719882560104));
#275675=CARTESIAN_POINT('Ctrl Pts',(-1.69743993836622,0.967891344955244,
12.068080639768));
#275676=CARTESIAN_POINT('Ctrl Pts',(-1.66345001870875,1.02750118383764,
12.0641754726543));
#275677=CARTESIAN_POINT('Ctrl Pts',(-1.62629198708003,1.0853610522253,12.0602703055406));
#275678=CARTESIAN_POINT('Ctrl Pts',(-1.5861778963528,1.14112036224134,12.056365138427));
#275679=CARTESIAN_POINT('Ctrl Pts',(-1.54607518897126,1.19686384920143,
12.0524610794991));
#275680=CARTESIAN_POINT('Ctrl Pts',(-1.50301837487858,1.25050756201909,
12.0485570205713));
#275681=CARTESIAN_POINT('Ctrl Pts',(-1.45726240406239,1.30173049657227,
12.0446529616435));
#275682=CARTESIAN_POINT('Ctrl Pts',(-1.41150372456271,1.35295646344485,
12.0407486716013));
#275683=CARTESIAN_POINT('Ctrl Pts',(-1.36304590070439,1.40176100241345,
12.0368443815592));
#275684=CARTESIAN_POINT('Ctrl Pts',(-1.31218246172391,1.44785813778291,
12.032940091517));
#275685=CARTESIAN_POINT('Ctrl Pts',(-1.26126484507645,1.49400437394654,
12.0290316427839));
#275686=CARTESIAN_POINT('Ctrl Pts',(-1.20793686479125,1.53743712035715,
12.0251231940507));
#275687=CARTESIAN_POINT('Ctrl Pts',(-1.15252626910834,1.57790975629635,
12.0212147453176));
#275688=CARTESIAN_POINT('Ctrl Pts',(-1.09708250639116,1.61840661787844,
12.0173039571104));
#275689=CARTESIAN_POINT('Ctrl Pts',(-1.03955405934958,1.65593957391646,
12.0133931689031));
#275690=CARTESIAN_POINT('Ctrl Pts',(-0.980296518374739,1.69030610720732,
12.0094823806959));
#275691=CARTESIAN_POINT('Ctrl Pts',(-0.920936658717528,1.72473198042937,
12.0055648398173));
#275692=CARTESIAN_POINT('Ctrl Pts',(-0.859842184062017,1.75598029500031,
12.0016472989388));
#275693=CARTESIAN_POINT('Ctrl Pts',(-0.797391253547561,1.78389550948643,
11.9977297580603));
#275694=CARTESIAN_POINT('Ctrl Pts',(-0.767917285962512,1.79707020712689,
11.9958808589019));
#275695=CARTESIAN_POINT('Ctrl Pts',(-0.738141436690851,1.80950319841902,
11.9940319597435));
#275696=CARTESIAN_POINT('Ctrl Pts',(-0.708104604416077,1.82118199782579,
11.9921830605852));
#275697=CARTESIAN_POINT('Ctrl Pts',(-0.644451691635783,1.84593126543223,
11.9882649437947));
#275698=CARTESIAN_POINT('Ctrl Pts',(-0.57937350324923,1.86738843594533,
11.9843468270043));
#275699=CARTESIAN_POINT('Ctrl Pts',(-0.513243658350625,1.88539039648633,
11.9804287102139));
#275700=CARTESIAN_POINT('Ctrl Pts',(-0.447213393913931,1.90336524909219,
11.9765164934506));
#275701=CARTESIAN_POINT('Ctrl Pts',(-0.380135086678046,1.91789508961401,
11.9726042766873));
#275702=CARTESIAN_POINT('Ctrl Pts',(-0.312400961577164,1.92886537612288,
11.968692059924));
#275703=CARTESIAN_POINT('Ctrl Pts',(-0.244746487548015,1.93982276226467,
11.9647844436816));
#275704=CARTESIAN_POINT('Ctrl Pts',(-0.176438210524025,1.94722882921171,
11.9608768274393));
#275705=CARTESIAN_POINT('Ctrl Pts',(-0.107880316682717,1.95101969166701,
11.9569692111969));
#275706=CARTESIAN_POINT('Ctrl Pts',(-0.0393653920322853,1.95480817816992,
11.9530640440832));
#275707=CARTESIAN_POINT('Ctrl Pts',(0.0293983490624891,1.95498592782676,
11.9491588769696));
#275708=CARTESIAN_POINT('Ctrl Pts',(0.0980013551684196,1.95154086157199,
11.9452537098559));
#275709=CARTESIAN_POINT('Ctrl Pts',(0.166584893508266,1.94809677293829,
11.9413496509281));
#275710=CARTESIAN_POINT('Ctrl Pts',(0.235007296377531,1.94103193393072,
11.9374455920003));
#275711=CARTESIAN_POINT('Ctrl Pts',(0.302860589942995,1.93038635072345,
11.9335415330725));
#275712=CARTESIAN_POINT('Ctrl Pts',(0.370717900319621,1.91974013731393,
11.9296372430304));
#275713=CARTESIAN_POINT('Ctrl Pts',(0.438005548968938,1.90551283763362,
11.9257329529882));
#275714=CARTESIAN_POINT('Ctrl Pts',(0.504324055963543,1.8877958699437,11.9218286629461));
#275715=CARTESIAN_POINT('Ctrl Pts',(0.57071320273515,1.8700600308602,11.917920214213));
#275716=CARTESIAN_POINT('Ctrl Pts',(0.636130671593625,1.84882723287807,
11.9140117654799));
#275717=CARTESIAN_POINT('Ctrl Pts',(0.700191476562453,1.82423899096289,
11.9101033167467));
#275718=CARTESIAN_POINT('Ctrl Pts',(0.764290626307935,1.79963603130189,
11.9061925285395));
#275719=CARTESIAN_POINT('Ctrl Pts',(0.827031046681989,1.77167383075916,
11.9022817403323));
#275720=CARTESIAN_POINT('Ctrl Pts',(0.88804969428404,1.74054122056389,11.8983709521251));
#275721=CARTESIAN_POINT('Ctrl Pts',(0.949173701432201,1.70935485438076,
11.8944534112466));
#275722=CARTESIAN_POINT('Ctrl Pts',(1.00856957676314,1.67498739898236,11.8905358703681));
#275723=CARTESIAN_POINT('Ctrl Pts',(1.06590149327693,1.63767213038203,11.8866183294895));
#275724=CARTESIAN_POINT('Ctrl Pts',(1.09295952164025,1.6200610394301,11.8847694303309));
#275725=CARTESIAN_POINT('Ctrl Pts',(1.11955828035541,1.60179395133601,11.8829205311723));
#275726=CARTESIAN_POINT('Ctrl Pts',(1.14566509189828,1.5828984481658,11.8810716320136));
#275727=CARTESIAN_POINT('Ctrl Pts',(1.20098965417766,1.54285581637127,11.8771535152232));
#275728=CARTESIAN_POINT('Ctrl Pts',(1.25432203901108,1.49982980681833,11.8732353984328));
#275729=CARTESIAN_POINT('Ctrl Pts',(1.30532252235046,1.45404577391657,11.8693172816424));
#275730=CARTESIAN_POINT('Ctrl Pts',(1.3562462075105,1.40833068409416,11.8654050648791));
#275731=CARTESIAN_POINT('Ctrl Pts',(1.40484459708485,1.35986613934267,11.8614928481158));
#275732=CARTESIAN_POINT('Ctrl Pts',(1.45080867347306,1.30891947535949,11.8575806313526));
#275733=CARTESIAN_POINT('Ctrl Pts',(1.49671869899783,1.25803272144942,11.8536730151102));
#275734=CARTESIAN_POINT('Ctrl Pts',(1.54000023565451,1.20467000860407,11.8497653988678));
#275735=CARTESIAN_POINT('Ctrl Pts',(1.58038032930572,1.14913620373894,11.8458577826255));
#275736=CARTESIAN_POINT('Ctrl Pts',(1.62073511442054,1.09363720511605,11.8419526155118));
#275737=CARTESIAN_POINT('Ctrl Pts',(1.65819177523754,1.03597021070243,11.8380474483982));
#275738=CARTESIAN_POINT('Ctrl Pts',(1.69251796539022,0.976472701529003,
11.8341422812846));
#275739=CARTESIAN_POINT('Ctrl Pts',(1.7268344146543,0.916992076216168,11.8302382223568));
#275740=CARTESIAN_POINT('Ctrl Pts',(1.75802191108362,0.855682393204036,
11.826334163429));
#275741=CARTESIAN_POINT('Ctrl Pts',(1.78589271726098,0.792908066823759,
11.8224301045012));
#275742=CARTESIAN_POINT('Ctrl Pts',(1.81376517334743,0.730130024299399,
11.8185258144591));
#275743=CARTESIAN_POINT('Ctrl Pts',(1.83832035211883,0.665887616869239,
11.814621524417));
#275744=CARTESIAN_POINT('Ctrl Pts',(1.85941831203987,0.600566017062898,
11.8107172343749));
#275745=CARTESIAN_POINT('Ctrl Pts',(1.88053874464993,0.535174839344564,
11.8068087856418));
#275746=CARTESIAN_POINT('Ctrl Pts',(1.89819445783113,0.468702644149648,
11.8029003369087));
#275747=CARTESIAN_POINT('Ctrl Pts',(1.91229545626018,0.401549608350767,
11.7989918881756));
#275748=CARTESIAN_POINT('Ctrl Pts',(1.92640489510198,0.334356376863449,
11.7950810999684));
#275749=CARTESIAN_POINT('Ctrl Pts',(1.93695530903598,0.266481979822375,
11.7911703117612));
#275750=CARTESIAN_POINT('Ctrl Pts',(1.9439083545101,0.198333832882401,11.787259523554));
#275751=CARTESIAN_POINT('Ctrl Pts',(1.95087340565371,0.130068016047827,
11.7833419826755));
#275752=CARTESIAN_POINT('Ctrl Pts',(1.9542286671504,0.0615279969557309,
11.779424441797));
#275753=CARTESIAN_POINT('Ctrl Pts',(1.95398789637902,-0.00687755801797681,
11.7755069009185));
#275754=CARTESIAN_POINT('Ctrl Pts',(1.95387426364602,-0.0391618345492261,
11.7736580017598));
#275755=CARTESIAN_POINT('Ctrl Pts',(1.95296040136146,-0.0714162191886032,
11.771809102601));
#275756=CARTESIAN_POINT('Ctrl Pts',(1.95125175022806,-0.10359829743738,
11.7699602034423));
#275757=CARTESIAN_POINT('Ctrl Pts',(1.94763084171983,-0.171797333897219,
11.7660420866519));
#275758=CARTESIAN_POINT('Ctrl Pts',(1.94042297028202,-0.239941499894348,
11.7621239698614));
#275759=CARTESIAN_POINT('Ctrl Pts',(1.92963312460916,-0.307623153242896,
11.758205853071));
#275760=CARTESIAN_POINT('Ctrl Pts',(1.91885952663531,-0.375202889366135,
11.7542936363077));
#275761=CARTESIAN_POINT('Ctrl Pts',(1.90451473612943,-0.442321013241658,
11.7503814195445));
#275762=CARTESIAN_POINT('Ctrl Pts',(1.88665566681589,-0.508572900252736,
11.7464692027812));
#275763=CARTESIAN_POINT('Ctrl Pts',(1.86881759864483,-0.57474687921085,
11.7425615865388));
#275764=CARTESIAN_POINT('Ctrl Pts',(1.84747358643237,-0.640056171660605,
11.7386539702964));
#275765=CARTESIAN_POINT('Ctrl Pts',(1.8227316371679,-0.704106084952569,
11.734746354054));
#275766=CARTESIAN_POINT('Ctrl Pts',(1.79800519511173,-0.768115854465375,
11.7308411869404));
#275767=CARTESIAN_POINT('Ctrl Pts',(1.76988521746549,-0.830867352785871,
11.7269360198267));
#275768=CARTESIAN_POINT('Ctrl Pts',(1.73852913946858,-0.891982304319223,
11.7230308527131));
#275769=CARTESIAN_POINT('Ctrl Pts',(1.70718195951896,-0.953079913003496,
11.7191267937853));
#275770=CARTESIAN_POINT('Ctrl Pts',(1.67260072667862,-1.01254145939989,
11.7152227348575));
#275771=CARTESIAN_POINT('Ctrl Pts',(1.634989703211,-1.07001152815939,11.7113186759296));
#275772=CARTESIAN_POINT('Ctrl Pts',(1.59737645322832,-1.12748499905906,
11.7074143858875));
#275773=CARTESIAN_POINT('Ctrl Pts',(1.55673332802689,-1.18296634809468,
11.7035100958454));
#275774=CARTESIAN_POINT('Ctrl Pts',(1.51330795868977,-1.23612904753759,
11.6996058058033));
#275775=CARTESIAN_POINT('Ctrl Pts',(1.46983633441501,-1.28934837372624,
11.6956973570702));
#275776=CARTESIAN_POINT('Ctrl Pts',(1.42357686347721,-1.34024373982725,
11.691788908337));
#275777=CARTESIAN_POINT('Ctrl Pts',(1.37481687903088,-1.38852243378773,
11.6878804596039));
#275778=CARTESIAN_POINT('Ctrl Pts',(1.32602770839632,-1.43683002585114,
11.6839696713967));
#275779=CARTESIAN_POINT('Ctrl Pts',(1.27473541283795,-1.48251750142439,
11.6800588831895));
#275780=CARTESIAN_POINT('Ctrl Pts',(1.22126142963808,-1.52533161000431,
11.6761480949823));
#275781=CARTESIAN_POINT('Ctrl Pts',(1.16769511409685,-1.5682196447564,11.6722305541038));
#275782=CARTESIAN_POINT('Ctrl Pts',(1.11193999188157,-1.60822412380125,
11.6683130132252));
#275783=CARTESIAN_POINT('Ctrl Pts',(1.05434681795526,-1.64513488427777,
11.6643954723467));
#275784=CARTESIAN_POINT('Ctrl Pts',(1.02716548810646,-1.66255506599524,
11.6625465731881));
#275785=CARTESIAN_POINT('Ctrl Pts',(0.999575108630041,-1.67928681524516,
11.6606976740295));
#275786=CARTESIAN_POINT('Ctrl Pts',(0.971614260689926,-1.69531169064098,
11.6588487748708));
#275787=CARTESIAN_POINT('Ctrl Pts',(0.91236069497888,-1.72927099721534,
11.6549306580804));
#275788=CARTESIAN_POINT('Ctrl Pts',(0.851207137213693,-1.76018738676486,
11.65101254129));
#275789=CARTESIAN_POINT('Ctrl Pts',(0.788498724613717,-1.7878438861608,
11.6470944244995));
#275790=CARTESIAN_POINT('Ctrl Pts',(0.725884740372109,-1.81545873950435,
11.6431822077362));
#275791=CARTESIAN_POINT('Ctrl Pts',(0.661720994481132,-1.83982324812798,
11.639269990973));
#275792=CARTESIAN_POINT('Ctrl Pts',(0.596378260925824,-1.86076569451801,
11.6353577742097));
#275793=CARTESIAN_POINT('Ctrl Pts',(0.531112366316169,-1.88168351390803,
11.6314501579673));
#275794=CARTESIAN_POINT('Ctrl Pts',(0.46467070367683,-1.89918711363325,
11.6275425417249));
#275795=CARTESIAN_POINT('Ctrl Pts',(0.397443424205221,-1.91315308445405,
11.6236349254825));
#275796=CARTESIAN_POINT('Ctrl Pts',(0.330258279951637,-1.92711030199447,
11.6197297583688));
#275797=CARTESIAN_POINT('Ctrl Pts',(0.262288976130544,-1.9375341890993,
11.6158245912552));
#275798=CARTESIAN_POINT('Ctrl Pts',(0.193938690156597,-1.944351764589,11.6119194241415));
#275799=CARTESIAN_POINT('Ctrl Pts',(0.12560780023328,-1.95116740542638,
11.6080153652137));
#275800=CARTESIAN_POINT('Ctrl Pts',(0.0568966320012735,-1.95437871743335,
11.6041113062859));
#275801=CARTESIAN_POINT('Ctrl Pts',(-0.011785434644376,-1.95396445810313,
11.6002072473581));
#275802=CARTESIAN_POINT('Ctrl Pts',(-0.0804715671632938,-1.95355017424939,
11.596302957316));
#275803=CARTESIAN_POINT('Ctrl Pts',(-0.149128102821917,-1.94950989847778,
11.5923986672738));
#275804=CARTESIAN_POINT('Ctrl Pts',(-0.217346398632557,-1.9418744920827,
11.5884943772317));
#275805=CARTESIAN_POINT('Ctrl Pts',(-0.285637357798015,-1.9342309527632,
11.5845859284986));
#275806=CARTESIAN_POINT('Ctrl Pts',(-0.353488655770739,-1.92298469536685,
11.5806774797655));
#275807=CARTESIAN_POINT('Ctrl Pts',(-0.420498515544062,-1.90821827850622,
11.5767690310323));
#275808=CARTESIAN_POINT('Ctrl Pts',(-0.487548485305181,-1.89344302293436,
11.5728582428251));
#275809=CARTESIAN_POINT('Ctrl Pts',(-0.553755540325949,-1.87514354552687,
11.5689474546179));
#275810=CARTESIAN_POINT('Ctrl Pts',(-0.618732549399968,-1.85345246292237,
11.5650366664107));
#275811=CARTESIAN_POINT('Ctrl Pts',(-0.683821752835107,-1.83172392680641,
11.5611191255322));
#275812=CARTESIAN_POINT('Ctrl Pts',(-0.747676213911406,-1.80659227748625,
11.5572015846537));
#275813=CARTESIAN_POINT('Ctrl Pts',(-0.80992909009743,-1.77823813619379,
11.5532840437751));
#275814=CARTESIAN_POINT('Ctrl Pts',(-0.839309585150223,-1.76485628528171,
11.5514351446165));
#275815=CARTESIAN_POINT('Ctrl Pts',(-0.868333705387705,-1.75075731663089,
11.549586245458));
#275816=CARTESIAN_POINT('Ctrl Pts',(-0.896965027564618,-1.73596363421761,
11.5477373462994));
#275817=CARTESIAN_POINT('Ctrl Pts',(-0.957639436783788,-1.70461342499374,
11.5438192295089));
#275818=CARTESIAN_POINT('Ctrl Pts',(-1.01678854115817,-1.67001625427391,
11.5399011127185));
#275819=CARTESIAN_POINT('Ctrl Pts',(-1.07404282521682,-1.632344329362,11.5359829959281));
#275820=CARTESIAN_POINT('Ctrl Pts',(-1.13121089392045,-1.59472913205456,
11.5320707791648));
#275821=CARTESIAN_POINT('Ctrl Pts',(-1.18648939745831,-1.55404863778721,
11.5281585624015));
#275822=CARTESIAN_POINT('Ctrl Pts',(-1.23953292724915,-1.51052114260779,
11.5242463456382));
#275823=CARTESIAN_POINT('Ctrl Pts',(-1.2925140811846,-1.46704483302548,
11.5203387293958));
#275824=CARTESIAN_POINT('Ctrl Pts',(-1.34326510255321,-1.42072848205026,
11.5164311131535));
#275825=CARTESIAN_POINT('Ctrl Pts',(-1.39147065006314,-1.37183287247859,
11.5125234969111));
#275826=CARTESIAN_POINT('Ctrl Pts',(-1.43964598437286,-1.32296790860887,
11.5086183297974));
#275827=CARTESIAN_POINT('Ctrl Pts',(-1.48527866502574,-1.27152724239304,
11.5047131626838));
#275828=CARTESIAN_POINT('Ctrl Pts',(-1.52808864439131,-1.21780995844275,
11.5008079955701));
#275829=CARTESIAN_POINT('Ctrl Pts',(-1.57088647538741,-1.16410791807403,
11.4969039366423));
#275830=CARTESIAN_POINT('Ctrl Pts',(-1.61086288882351,-1.10813092696698,
11.4929998777145));
#275831=CARTESIAN_POINT('Ctrl Pts',(-1.64777793385773,-1.05021135048691,
11.4890958187867));
#275832=CARTESIAN_POINT('Ctrl Pts',(-1.68469516420617,-0.9922883452565,
11.4851915287446));
#275833=CARTESIAN_POINT('Ctrl Pts',(-1.71855040414558,-0.932422942513319,
11.4812872387025));
#275834=CARTESIAN_POINT('Ctrl Pts',(-1.74914787126292,-0.870975157198189,
11.4773829486603));
#275835=CARTESIAN_POINT('Ctrl Pts',(-1.77977792955806,-0.809461920200752,
11.4734744999272));
#275836=CARTESIAN_POINT('Ctrl Pts',(-1.80714307022,-0.746363378073689,11.4695660511941));
#275837=CARTESIAN_POINT('Ctrl Pts',(-1.83109466309896,-0.682061826208244,
11.465657602461));
#275838=CARTESIAN_POINT('Ctrl Pts',(-1.85506059264569,-0.617721785462693,
11.4617468142538));
#275839=CARTESIAN_POINT('Ctrl Pts',(-1.87560876081767,-0.552177771299046,
11.4578360260465));
#275840=CARTESIAN_POINT('Ctrl Pts',(-1.89264053357121,-0.485826934909212,
11.4539252378393));
#275841=CARTESIAN_POINT('Ctrl Pts',(-1.90970171470921,-0.419361532001062,
11.4500076969608));
#275842=CARTESIAN_POINT('Ctrl Pts',(-1.92323428537703,-0.352087008383132,
11.4460901560823));
#275843=CARTESIAN_POINT('Ctrl Pts',(-1.93319094420419,-0.284409516800858,
11.4421726152038));
#275844=CARTESIAN_POINT('Ctrl Pts',(-1.93789002934436,-0.252468852714836,
11.4403237160452));
#275845=CARTESIAN_POINT('Ctrl Pts',(-1.94179336691381,-0.220438485429623,
11.4384748168865));
#275846=CARTESIAN_POINT('Ctrl Pts',(-1.94490001565959,-0.188361166611744,
11.4366259177279));
#275847=CARTESIAN_POINT('Ctrl Pts',(-1.95092446803442,-0.126156425958906,
11.4330405091934));
#275848=CARTESIAN_POINT('Ctrl Pts',(-1.95396526428295,-0.0636581075121945,
11.4294551006588));
#275849=CARTESIAN_POINT('Ctrl Pts',(-1.95399970412604,-0.00107530244352288,
11.4258696921242));
#275850=CARTESIAN_POINT('',(-1.95134965453372,-0.00103648843533824,10.7258696921242));
#275851=CARTESIAN_POINT('Ctrl Pts',(-1.95645396550645,-0.00105959575216067,
11.4258687161274));
#275852=CARTESIAN_POINT('Ctrl Pts',(-1.95257275277448,0.583565857793029,
11.3924173071372));
#275853=CARTESIAN_POINT('Ctrl Pts',(-1.36384586590087,1.82225161540351,
11.3219287552896));
#275854=CARTESIAN_POINT('Ctrl Pts',(0.742476273254284,2.18672944451667,
11.214403060585));
#275855=CARTESIAN_POINT('Ctrl Pts',(2.2397387517957,0.562696191178322,11.1032916320137));
#275856=CARTESIAN_POINT('Ctrl Pts',(1.68783678799721,-1.57615470590446,
10.9921802034423));
#275857=CARTESIAN_POINT('Ctrl Pts',(-0.408287745359925,-2.2729623395146,
10.8810687748709));
#275858=CARTESIAN_POINT('Ctrl Pts',(-1.7845049539434,-1.16824013984896,
10.7922986044314));
#275859=CARTESIAN_POINT('Ctrl Pts',(-1.95259451044093,-0.259597370141399,
10.7405655768493));
#275860=CARTESIAN_POINT('Ctrl Pts',(-1.95134965453372,-0.00103648843533824,
10.7258696921242));
#275861=CARTESIAN_POINT('',(-1.95399929751496,0.00165689801507491,10.0258696714934));
#275862=CARTESIAN_POINT('Ctrl Pts',(-1.95134965453372,-0.00103648843533824,
10.7258696921242));
#275863=CARTESIAN_POINT('Ctrl Pts',(-1.94945717594664,0.392037865993335,
10.7035284339921));
#275864=CARTESIAN_POINT('Ctrl Pts',(-1.64348006051442,1.43945790588366,
10.6441500330031));
#275865=CARTESIAN_POINT('Ctrl Pts',(0.0649797842751265,2.30842680358238,
10.5477344891565));
#275866=CARTESIAN_POINT('Ctrl Pts',(1.97439630915861,1.19783800834803,10.4366230605851));
#275867=CARTESIAN_POINT('Ctrl Pts',(2.07741344546512,-1.0086674657501,10.3255116320137));
#275868=CARTESIAN_POINT('Ctrl Pts',(0.279779552238291,-2.29233070956424,
10.2144002034423));
#275869=CARTESIAN_POINT('Ctrl Pts',(-1.56625610044506,-1.56095036901687,
10.1145195568125));
#275870=CARTESIAN_POINT('Ctrl Pts',(-1.94902830395309,-0.451607116338367,
10.0516760530398));
#275871=CARTESIAN_POINT('Ctrl Pts',(-1.95267873247834,0.00165541588313972,
10.0258696921242));
#275872=CARTESIAN_POINT('',(-1.95399999960791,3.91444967126425E-5,9.32586969217706));
#275873=CARTESIAN_POINT('Ctrl Pts',(-1.95399929751496,0.00165689801507491,
10.0258696714934));
#275874=CARTESIAN_POINT('Ctrl Pts',(-1.95392948695817,0.0839853079092353,
10.0211854615976));
#275875=CARTESIAN_POINT('Ctrl Pts',(-1.94865267969109,0.166088006905242,
10.0165012517017));
#275876=CARTESIAN_POINT('Ctrl Pts',(-1.93827701010705,0.247382764335887,
10.0118170418058));
#275877=CARTESIAN_POINT('Ctrl Pts',(-1.92775896101606,0.329793084226128,
10.007068553119));
#275878=CARTESIAN_POINT('Ctrl Pts',(-1.91200123245361,0.411373120614258,
10.0023200644323));
#275879=CARTESIAN_POINT('Ctrl Pts',(-1.8911653299869,0.491538090747332,
9.99757157574553));
#275880=CARTESIAN_POINT('Ctrl Pts',(-1.88327554679925,0.521893590568139,
9.99577349926348));
#275881=CARTESIAN_POINT('Ctrl Pts',(-1.87465811584151,0.552046411622639,
9.99397542278144));
#275882=CARTESIAN_POINT('Ctrl Pts',(-1.86532357338296,0.581965606012771,
9.99217734629939));
#275883=CARTESIAN_POINT('Ctrl Pts',(-1.84498304398784,0.647161329924655,
9.98825922950897));
#275884=CARTESIAN_POINT('Ctrl Pts',(-1.82118005276578,0.711418612616846,
9.98434111271855));
#275885=CARTESIAN_POINT('Ctrl Pts',(-1.7940200408267,0.774343653110278,
9.98042299592813));
#275886=CARTESIAN_POINT('Ctrl Pts',(-1.76690092731312,0.837173939040036,
9.97651077916485));
#275887=CARTESIAN_POINT('Ctrl Pts',(-1.73643501904436,0.898675516260269,
9.97259856240157));
#275888=CARTESIAN_POINT('Ctrl Pts',(-1.70277733117232,0.95847032319508,
9.96868634563829));
#275889=CARTESIAN_POINT('Ctrl Pts',(-1.66915922262466,1.0181948151971,9.9647787293959));
#275890=CARTESIAN_POINT('Ctrl Pts',(-1.63235702878227,1.0762160963446,9.96087111315351));
#275891=CARTESIAN_POINT('Ctrl Pts',(-1.59257282631954,1.13217833969238,
9.95696349691113));
#275892=CARTESIAN_POINT('Ctrl Pts',(-1.55281355891379,1.18810550827076,
9.95305832979748));
#275893=CARTESIAN_POINT('Ctrl Pts',(-1.51007627474735,1.24197579902889,
9.94915316268384));
#275894=CARTESIAN_POINT('Ctrl Pts',(-1.46460689797784,1.29346149320176,
9.94524799557019));
#275895=CARTESIAN_POINT('Ctrl Pts',(-1.41915042424628,1.34493257706077,
9.94134393664239));
#275896=CARTESIAN_POINT('Ctrl Pts',(-1.37096372246039,1.39402003916266,
9.93743987771458));
#275897=CARTESIAN_POINT('Ctrl Pts',(-1.32033245331152,1.4404298708137,9.93353581878677));
#275898=CARTESIAN_POINT('Ctrl Pts',(-1.26969818686899,1.48684244985577,
9.92963152874465));
#275899=CARTESIAN_POINT('Ctrl Pts',(-1.21661943008506,1.53057675327101,
9.92572723870252));
#275900=CARTESIAN_POINT('Ctrl Pts',(-1.16141674139082,1.57137746987066,
9.9218229486604));
#275901=CARTESIAN_POINT('Ctrl Pts',(-1.10615525303724,1.6122216457346,9.91791449992728));
#275902=CARTESIAN_POINT('Ctrl Pts',(-1.04876571419292,1.65012570585005,
9.91400605119417));
#275903=CARTESIAN_POINT('Ctrl Pts',(-0.98959881145575,1.68487690718502,
9.91009760246104));
#275904=CARTESIAN_POINT('Ctrl Pts',(-0.930396493277447,1.71964890949263,
9.90618681425383));
#275905=CARTESIAN_POINT('Ctrl Pts',(-0.869415130643365,1.7512640707161,
9.90227602604662));
#275906=CARTESIAN_POINT('Ctrl Pts',(-0.807028720130453,1.77955630562357,
9.89836523783941));
#275907=CARTESIAN_POINT('Ctrl Pts',(-0.74453458838551,1.80789739210586,
9.8944476969609));
#275908=CARTESIAN_POINT('Ctrl Pts',(-0.68063102453977,1.83290392174707,
9.89053015608238));
#275909=CARTESIAN_POINT('Ctrl Pts',(-0.615709801840668,1.85445879973574,
9.88661261520387));
#275910=CARTESIAN_POINT('Ctrl Pts',(-0.585069969928584,1.86463171101191,
9.88476371604523));
#275911=CARTESIAN_POINT('Ctrl Pts',(-0.554203648136369,1.87403653167203,
9.88291481688659));
#275912=CARTESIAN_POINT('Ctrl Pts',(-0.523152775522914,1.88266491268698,
9.88106591772794));
#275913=CARTESIAN_POINT('Ctrl Pts',(-0.457350947026457,1.90094984962951,
9.87714780093752));
#275914=CARTESIAN_POINT('Ctrl Pts',(-0.390458897492729,1.91581707799529,
9.87322968414709));
#275915=CARTESIAN_POINT('Ctrl Pts',(-0.322864636989375,1.92714151690573,
9.86931156735667));
#275916=CARTESIAN_POINT('Ctrl Pts',(-0.255372162112371,1.93844890310935,
9.86539935059339));
#275917=CARTESIAN_POINT('Ctrl Pts',(-0.187180056070632,1.9462240070194,
9.8614871338301));
#275918=CARTESIAN_POINT('Ctrl Pts',(-0.118690003493383,1.95039193063106,
9.85757491706682));
#275919=CARTESIAN_POINT('Ctrl Pts',(-0.0502804909110705,1.95455495302664,
9.85366730082444));
#275920=CARTESIAN_POINT('Ctrl Pts',(0.0184257837265425,1.95511918970179,
9.84975968458205));
#275921=CARTESIAN_POINT('Ctrl Pts',(0.0870202805502169,1.95206133888589,
9.84585206833967));
#275922=CARTESIAN_POINT('Ctrl Pts',(0.155571785241821,1.94900540460167,
9.84194690122602));
#275923=CARTESIAN_POINT('Ctrl Pts',(0.2240111608026,1.94233190798178,9.83804173411238));
#275924=CARTESIAN_POINT('Ctrl Pts',(0.291929689823532,1.93206963026686,
9.83413656699874));
#275925=CARTESIAN_POINT('Ctrl Pts',(0.359828945315338,1.92181026472203,
9.83023250807094));
#275926=CARTESIAN_POINT('Ctrl Pts',(0.427207161550223,1.90796421324135,
9.82632844914314));
#275927=CARTESIAN_POINT('Ctrl Pts',(0.493662379692254,1.89061192603786,
9.82242439021533));
#275928=CARTESIAN_POINT('Ctrl Pts',(0.560121531881548,1.8732586116055,9.81852010017321));
#275929=CARTESIAN_POINT('Ctrl Pts',(0.625657102224863,1.85239877611429,
9.81461581013109));
#275930=CARTESIAN_POINT('Ctrl Pts',(0.689880705298606,1.82816317993135,
9.81071152008897));
#275931=CARTESIAN_POINT('Ctrl Pts',(0.754172716742869,1.80390176897683,
9.80680307135586));
#275932=CARTESIAN_POINT('Ctrl Pts',(0.817149510945161,1.77625759537737,
9.80289462262275));
#275933=CARTESIAN_POINT('Ctrl Pts',(0.878442115050694,1.74540982308032,
9.79898617388963));
#275934=CARTESIAN_POINT('Ctrl Pts',(0.93977140697515,1.71454358628007,9.79507538568242));
#275935=CARTESIAN_POINT('Ctrl Pts',(0.999414075337499,1.68047017848876,
9.79116459747521));
#275936=CARTESIAN_POINT('Ctrl Pts',(1.05702769443046,1.64341365857991,9.78725380926801));
#275937=CARTESIAN_POINT('Ctrl Pts',(1.11474079368233,1.60629315399962,9.7833362683895));
#275938=CARTESIAN_POINT('Ctrl Pts',(1.17041745233701,1.56617954436482,9.77941872751099));
#275939=CARTESIAN_POINT('Ctrl Pts',(1.22374675336249,1.52333840089285,9.77550118663248));
#275940=CARTESIAN_POINT('Ctrl Pts',(1.24891573126341,1.50311935109166,9.77365228747383));
#275941=CARTESIAN_POINT('Ctrl Pts',(1.27356237264419,1.48229332071419,9.77180338831518));
#275942=CARTESIAN_POINT('Ctrl Pts',(1.29765691031169,1.46089101000736,9.76995448915654));
#275943=CARTESIAN_POINT('Ctrl Pts',(1.34871713831335,1.41553604700562,9.76603637236611));
#275944=CARTESIAN_POINT('Ctrl Pts',(1.39749788996994,1.36741101154671,9.76211825557569));
#275945=CARTESIAN_POINT('Ctrl Pts',(1.44368358142382,1.3167739808818,9.75820013878526));
#275946=CARTESIAN_POINT('Ctrl Pts',(1.48979972496789,1.26621320109742,9.75428792202198));
#275947=CARTESIAN_POINT('Ctrl Pts',(1.53332823495643,1.21314829381023,9.7503757052587));
#275948=CARTESIAN_POINT('Ctrl Pts',(1.57398826347465,1.15787604968928,9.74646348849542));
#275949=CARTESIAN_POINT('Ctrl Pts',(1.61460047835618,1.10266880225171,9.74255587225303));
#275950=CARTESIAN_POINT('Ctrl Pts',(1.652350620811,1.04525976740311,9.73864825601065));
#275951=CARTESIAN_POINT('Ctrl Pts',(1.68699746590993,0.985979487623083,
9.73474063976826));
#275952=CARTESIAN_POINT('Ctrl Pts',(1.72162259583039,0.926736362217474,
9.73083547265462));
#275953=CARTESIAN_POINT('Ctrl Pts',(1.75314803904495,0.865624742091583,
9.72693030554098));
#275954=CARTESIAN_POINT('Ctrl Pts',(1.78137622546144,0.803003576181791,
9.72302513842733));
#275955=CARTESIAN_POINT('Ctrl Pts',(1.80959640144573,0.740400180545905,
9.71912107949953));
#275956=CARTESIAN_POINT('Ctrl Pts',(1.83452097606573,0.676288537729521,
9.71521702057172));
#275957=CARTESIAN_POINT('Ctrl Pts',(1.8559994494078,0.611049951966226,9.71131296164392));
#275958=CARTESIAN_POINT('Ctrl Pts',(1.87747919424264,0.545807504178463,
9.7074086716018));
#275959=CARTESIAN_POINT('Ctrl Pts',(1.89551228139774,0.479438449005124,
9.70350438155968));
#275960=CARTESIAN_POINT('Ctrl Pts',(1.90999783704255,0.412339984106304,
9.69960009151755));
#275961=CARTESIAN_POINT('Ctrl Pts',(1.92449882211221,0.345170048651036,
9.69569164278444));
#275962=CARTESIAN_POINT('Ctrl Pts',(1.93544463058594,0.277269634669579,
9.69178319405132));
#275963=CARTESIAN_POINT('Ctrl Pts',(1.94278558114032,0.209045893796705,
9.6878747453182));
#275964=CARTESIAN_POINT('Ctrl Pts',(1.95013092575609,0.14078131634512,9.68396395711099));
#275965=CARTESIAN_POINT('Ctrl Pts',(1.95386709136618,0.072193518053941,
9.68005316890378));
#275966=CARTESIAN_POINT('Ctrl Pts',(1.95399651261058,0.00369170769181413,
9.67614238069657));
#275967=CARTESIAN_POINT('Ctrl Pts',(1.95412615732378,-0.0649283832276949,
9.67222483981805));
#275968=CARTESIAN_POINT('Ctrl Pts',(1.95063665321014,-0.133461698906467,
9.66830729893954));
#275969=CARTESIAN_POINT('Ctrl Pts',(1.94358240125738,-0.201502976460919,
9.66438975806103));
#275970=CARTESIAN_POINT('Ctrl Pts',(1.94025311870366,-0.233615330798652,
9.66254085890239));
#275971=CARTESIAN_POINT('Ctrl Pts',(1.93613056531544,-0.265618221702319,
9.66069195974374));
#275972=CARTESIAN_POINT('Ctrl Pts',(1.93122438013529,-0.297469987681229,
9.6588430605851));
#275973=CARTESIAN_POINT('Ctrl Pts',(1.92082737906498,-0.364969038942825,
9.65492494379468));
#275974=CARTESIAN_POINT('Ctrl Pts',(1.90686672512084,-0.432056153290937,
9.65100682700425));
#275975=CARTESIAN_POINT('Ctrl Pts',(1.88938799219554,-0.498326213385671,
9.64708871021382));
#275976=CARTESIAN_POINT('Ctrl Pts',(1.87193557931229,-0.564496481877911,
9.64317649345054));
#275977=CARTESIAN_POINT('Ctrl Pts',(1.85097572581657,-0.629851666130271,
9.63926427668725));
#275978=CARTESIAN_POINT('Ctrl Pts',(1.82660537170836,-0.693994824221443,
9.63535205992397));
#275979=CARTESIAN_POINT('Ctrl Pts',(1.80226367560408,-0.758062553992272,
9.63144444368158));
#275980=CARTESIAN_POINT('Ctrl Pts',(1.77451961774217,-0.820920630569309,
9.6275368274392));
#275981=CARTESIAN_POINT('Ctrl Pts',(1.74351998777852,-0.88218708458966,
9.62362921119681));
#275982=CARTESIAN_POINT('Ctrl Pts',(1.71253978707301,-0.943415139385506,
9.61972404408316));
#275983=CARTESIAN_POINT('Ctrl Pts',(1.6783082834547,-1.00305311255965,9.61581887696952));
#275984=CARTESIAN_POINT('Ctrl Pts',(1.64101981344774,-1.06074029426243,
9.61191370985587));
#275985=CARTESIAN_POINT('Ctrl Pts',(1.60374192494811,-1.11841110582891,
9.60800965092807));
#275986=CARTESIAN_POINT('Ctrl Pts',(1.56340905906781,-1.17413181198458,
9.60410559200026));
#275987=CARTESIAN_POINT('Ctrl Pts',(1.52025986903153,-1.22756911439325,
9.60020153307246));
#275988=CARTESIAN_POINT('Ctrl Pts',(1.47710812462923,-1.28100958020845,
9.59629724303034));
#275989=CARTESIAN_POINT('Ctrl Pts',(1.4311400360793,-1.33216599282712,9.59239295298821));
#275990=CARTESIAN_POINT('Ctrl Pts',(1.38263453184847,-1.3807381183049,9.58848866294609));
#275991=CARTESIAN_POINT('Ctrl Pts',(1.33407736152685,-1.42936198083572,
9.58458021421297));
#275992=CARTESIAN_POINT('Ctrl Pts',(1.28297772990803,-1.47539571401498,
9.58067176547986));
#275993=CARTESIAN_POINT('Ctrl Pts',(1.22965070125184,-1.51857668654265,
9.57676331674674));
#275994=CARTESIAN_POINT('Ctrl Pts',(1.17629175271886,-1.56178350583804,
9.57285252853952));
#275995=CARTESIAN_POINT('Ctrl Pts',(1.12070315185605,-1.60213387711285,
9.56894174033231));
#275996=CARTESIAN_POINT('Ctrl Pts',(1.06322996616869,-1.63940783182249,
9.5650309521251));
#275997=CARTESIAN_POINT('Ctrl Pts',(1.00565754280569,-1.67674614664343,
9.56111341124659));
#275998=CARTESIAN_POINT('Ctrl Pts',(0.946194466017227,-1.71099719765996,
9.55719587036807));
#275999=CARTESIAN_POINT('Ctrl Pts',(0.885210682680147,-1.74198681030281,
9.55327832948956));
#276000=CARTESIAN_POINT('Ctrl Pts',(0.856429141096074,-1.75661248250855,
9.55142943033093));
#276001=CARTESIAN_POINT('Ctrl Pts',(0.827309167574824,-1.7705123967077,
9.5495805311723));
#276002=CARTESIAN_POINT('Ctrl Pts',(0.797890988516439,-1.78367204677437,
9.54773163201366));
#276003=CARTESIAN_POINT('Ctrl Pts',(0.73554910211656,-1.81155947678457,
9.54381351522324));
#276004=CARTESIAN_POINT('Ctrl Pts',(0.671619816017365,-1.83622984664296,
9.53989539843281));
#276005=CARTESIAN_POINT('Ctrl Pts',(0.606468165748695,-1.85750164574178,
9.53597728164239));
#276006=CARTESIAN_POINT('Ctrl Pts',(0.541414622944768,-1.87874141307668,
9.5320650648791));
#276007=CARTESIAN_POINT('Ctrl Pts',(0.475142832887637,-1.89659261499268,
9.52815284811582));
#276008=CARTESIAN_POINT('Ctrl Pts',(0.408038831897616,-1.9109213253464,
9.52424063135254));
#276009=CARTESIAN_POINT('Ctrl Pts',(0.341013740993034,-1.92523318603777,
9.52033301511015));
#276010=CARTESIAN_POINT('Ctrl Pts',(0.273158861483582,-1.93603067946743,
9.51642539886777));
#276011=CARTESIAN_POINT('Ctrl Pts',(0.204874697954479,-1.94322987784206,
9.51251778262539));
#276012=CARTESIAN_POINT('Ctrl Pts',(0.136633332053651,-1.95042456406336,
9.50861261551174));
#276013=CARTESIAN_POINT('Ctrl Pts',(0.0679637039277501,-1.95402537749045,
9.5047074483981));
#276014=CARTESIAN_POINT('Ctrl Pts',(-0.000725744151200082,-1.953999865224,
9.50080228128446));
#276015=CARTESIAN_POINT('Ctrl Pts',(-0.0693956999340427,-1.95397436019728,
9.49689822235665));
#276016=CARTESIAN_POINT('Ctrl Pts',(-0.138084972855544,-1.95032457251632,
9.49299416342885));
#276017=CARTESIAN_POINT('Ctrl Pts',(-0.206384103313727,-1.94307014847622,
9.48909010450105));
#276018=CARTESIAN_POINT('Ctrl Pts',(-0.27468727697597,-1.9358152949853,
9.48518581445893));
#276019=CARTESIAN_POINT('Ctrl Pts',(-0.342599773465787,-1.92495543598685,
9.48128152441681));
#276020=CARTESIAN_POINT('Ctrl Pts',(-0.409718057092925,-1.91056198896869,
9.47737723437469));
#276021=CARTESIAN_POINT('Ctrl Pts',(-0.476907832386587,-1.89615321063604,
9.47346878564157));
#276022=CARTESIAN_POINT('Ctrl Pts',(-0.543301224668324,-1.87820343617182,
9.46956033690846));
#276023=CARTESIAN_POINT('Ctrl Pts',(-0.60850668024895,-1.85683483920687,
9.46565188817534));
#276024=CARTESIAN_POINT('Ctrl Pts',(-0.673751165757901,-1.83545345167401,
9.46174109996814));
#276025=CARTESIAN_POINT('Ctrl Pts',(-0.737805840669606,-1.81064934657337,
9.45783031176093));
#276026=CARTESIAN_POINT('Ctrl Pts',(-0.800298711104466,-1.78259304750258,
9.45391952355373));
#276027=CARTESIAN_POINT('Ctrl Pts',(-0.862899486593402,-1.75448830424212,
9.45000198267521));
#276028=CARTESIAN_POINT('Ctrl Pts',(-0.923932638108802,-1.7231203841169,
9.4460844417967));
#276029=CARTESIAN_POINT('Ctrl Pts',(-0.983051141817712,-1.68870555532067,
9.44216690091819));
#276030=CARTESIAN_POINT('Ctrl Pts',(-1.01095235718662,-1.6724633385884,
9.44031800175954));
#276031=CARTESIAN_POINT('Ctrl Pts',(-1.03842753006701,-1.65554307417473,
9.4384691026009));
#276032=CARTESIAN_POINT('Ctrl Pts',(-1.06544265032794,-1.63797068315101,
9.43662020344225));
#276033=CARTESIAN_POINT('Ctrl Pts',(-1.1226587199488,-1.60075363068159,
9.43270436882958));
#276034=CARTESIAN_POINT('Ctrl Pts',(-1.1780364749103,-1.56046083031989,
9.42878853421692));
#276035=CARTESIAN_POINT('Ctrl Pts',(-1.23122563104289,-1.51730005123016,
9.42487269960425));
#276036=CARTESIAN_POINT('Ctrl Pts',(-1.28433467052284,-1.47420428345847,
9.42096276325326));
#276037=CARTESIAN_POINT('Ctrl Pts',(-1.33526127416141,-1.42824941800991,
9.41705282690228));
#276038=CARTESIAN_POINT('Ctrl Pts',(-1.38368371239994,-1.37968669778291,
9.41314289055129));
#276039=CARTESIAN_POINT('Ctrl Pts',(-1.43204927728936,-1.33118101566968,
9.40923754651707));
#276040=CARTESIAN_POINT('Ctrl Pts',(-1.47791617174053,-1.28007390884125,
9.40533220248285));
#276041=CARTESIAN_POINT('Ctrl Pts',(-1.52099680099037,-1.22665591401056,
9.40142685844863));
#276042=CARTESIAN_POINT('Ctrl Pts',(-1.56405051188734,-1.17327129669684,
9.39752395461621));
#276043=CARTESIAN_POINT('Ctrl Pts',(-1.60432110247687,-1.1175790381103,
9.39362105078379));
#276044=CARTESIAN_POINT('Ctrl Pts',(-1.64155990459192,-1.05990427852527,
9.38971814695136));
#276045=CARTESIAN_POINT('Ctrl Pts',(-1.67878825190776,-1.00224571113753,
9.38581633885976));
#276046=CARTESIAN_POINT('Ctrl Pts',(-1.71298623341745,-0.942606161247988,
9.38191453076817));
#276047=CARTESIAN_POINT('Ctrl Pts',(-1.74394839247643,-0.881339891516826,
9.37801272267657));
#276048=CARTESIAN_POINT('Ctrl Pts',(-1.77491251225945,-0.820069742009442,
9.37411066749727));
#276049=CARTESIAN_POINT('Ctrl Pts',(-1.80264018298136,-0.757173108918886,
9.37020861231796));
#276050=CARTESIAN_POINT('Ctrl Pts',(-1.82697265374871,-0.693027360538097,
9.36630655713865));
#276051=CARTESIAN_POINT('Ctrl Pts',(-1.8513310801166,-0.628813187481577,
9.36240033961239));
#276052=CARTESIAN_POINT('Ctrl Pts',(-1.87228690420847,-0.563347701541565,
9.35849412208613));
#276053=CARTESIAN_POINT('Ctrl Pts',(-1.88973051800933,-0.497025722980409,
9.35458790455987));
#276054=CARTESIAN_POINT('Ctrl Pts',(-1.90718467303244,-0.430663665871048,
9.35067932649597));
#276055=CARTESIAN_POINT('Ctrl Pts',(-1.92112229410764,-0.363444568437687,
9.34677074843206));
#276056=CARTESIAN_POINT('Ctrl Pts',(-1.93148500290727,-0.295773027073632,
9.34286217036815));
#276057=CARTESIAN_POINT('Ctrl Pts',(-1.94186551985346,-0.227985193266197,
9.3389468754764));
#276058=CARTESIAN_POINT('Ctrl Pts',(-1.9486588156178,-0.159743853599226,
9.33503158058464));
#276059=CARTESIAN_POINT('Ctrl Pts',(-1.95185848490155,-0.0914573940029764,
9.33111628569289));
#276060=CARTESIAN_POINT('Ctrl Pts',(-1.95328769730922,-0.060955536880899,
9.32936742118761));
#276061=CARTESIAN_POINT('Ctrl Pts',(-1.95400061029009,-0.0304446549697955,
9.32761855668234));
#276062=CARTESIAN_POINT('Ctrl Pts',(-1.95399999960791,3.91444967267211E-5,
9.32586969217706));
#276063=CARTESIAN_POINT('',(-1.9539992760325,-0.00168204175487709,8.62586971134118));
#276064=CARTESIAN_POINT('Ctrl Pts',(-1.95399999960789,3.91454175048696E-5,
9.32586969212423));
#276065=CARTESIAN_POINT('Ctrl Pts',(-1.9539999575976,0.00213614972020012,
9.32574938637309));
#276066=CARTESIAN_POINT('Ctrl Pts',(-1.95399653987704,0.00423315001500904,
9.32562908062195));
#276067=CARTESIAN_POINT('Ctrl Pts',(-1.95398974647657,0.00633013936807953,
9.32550877487081));
#276068=CARTESIAN_POINT('Ctrl Pts',(-1.95376849906167,0.0746248727085479,
9.32159065808039));
#276069=CARTESIAN_POINT('Ctrl Pts',(-1.9499620047619,0.143043374382022,
9.31767254128996));
#276070=CARTESIAN_POINT('Ctrl Pts',(-1.94255495232333,0.211178259307431,
9.31375442449954));
#276071=CARTESIAN_POINT('Ctrl Pts',(-1.93515905366417,0.279210544516802,
9.30984220773625));
#276072=CARTESIAN_POINT('Ctrl Pts',(-1.9241734100253,0.346959575514039,
9.30592999097297));
#276073=CARTESIAN_POINT('Ctrl Pts',(-1.90963472102237,0.414018396047568,
9.30201777420969));
#276074=CARTESIAN_POINT('Ctrl Pts',(-1.89511312860348,0.480998359625015,
9.2981101579673));
#276075=CARTESIAN_POINT('Ctrl Pts',(-1.87704689243386,0.547289246240515,
9.29420254172492));
#276076=CARTESIAN_POINT('Ctrl Pts',(-1.85552423648662,0.612491475704569,
9.29029492548253));
#276077=CARTESIAN_POINT('Ctrl Pts',(-1.83401507003066,0.677652839166399,
9.28638975836889));
#276078=CARTESIAN_POINT('Ctrl Pts',(-1.80905393495955,0.74172643294925,
9.28248459125525));
#276079=CARTESIAN_POINT('Ctrl Pts',(-1.78077923950232,0.804326612861677,
9.2785794241416));
#276080=CARTESIAN_POINT('Ctrl Pts',(-1.75251256767537,0.866909028455468,
9.2746753652138));
#276081=CARTESIAN_POINT('Ctrl Pts',(-1.72093440450345,0.928018412148079,
9.27077130628599));
#276082=CARTESIAN_POINT('Ctrl Pts',(-1.68623106523404,0.987289620445632,
9.26686724735819));
#276083=CARTESIAN_POINT('Ctrl Pts',(-1.65152567158002,1.04656433750806,
9.26296295731607));
#276084=CARTESIAN_POINT('Ctrl Pts',(-1.61369498527018,1.10400023995831,
9.25905866727395));
#276085=CARTESIAN_POINT('Ctrl Pts',(-1.57297007471654,1.15925887706165,
9.25515437723183));
#276086=CARTESIAN_POINT('Ctrl Pts',(-1.53220178564418,1.21457637341826,
9.25124592849871));
#276087=CARTESIAN_POINT('Ctrl Pts',(-1.48853341237372,1.26771157942995,
9.2473374797656));
#276088=CARTESIAN_POINT('Ctrl Pts',(-1.44223735961487,1.31835784160869,
9.24342903103248));
#276089=CARTESIAN_POINT('Ctrl Pts',(-1.39591359549956,1.369034419042,9.23951824282527));
#276090=CARTESIAN_POINT('Ctrl Pts',(-1.34695937224762,1.41721874256836,
9.23560745461806));
#276091=CARTESIAN_POINT('Ctrl Pts',(-1.29568312093407,1.46264187350375,
9.23169666641085));
#276092=CARTESIAN_POINT('Ctrl Pts',(-1.24431833205406,1.50814343555239,
9.22777912553234));
#276093=CARTESIAN_POINT('Ctrl Pts',(-1.19062389767963,1.55087398333843,
9.22386158465383));
#276094=CARTESIAN_POINT('Ctrl Pts',(-1.1349396752578,1.59060615286303,9.21994404377531));
#276095=CARTESIAN_POINT('Ctrl Pts',(-1.10865928274165,1.60935790991755,
9.21809514461667));
#276096=CARTESIAN_POINT('Ctrl Pts',(-1.08193607537915,1.62744245196018,
9.21624624545803));
#276097=CARTESIAN_POINT('Ctrl Pts',(-1.05480766842268,1.6448394397742,9.21439734629939));
#276098=CARTESIAN_POINT('Ctrl Pts',(-0.997318179990151,1.68170647480873,
9.21047922950896));
#276099=CARTESIAN_POINT('Ctrl Pts',(-0.937779569037563,1.7156289537267,
9.20656111271854));
#276100=CARTESIAN_POINT('Ctrl Pts',(-0.876525743196571,1.74637299037568,
9.20264299592811));
#276101=CARTESIAN_POINT('Ctrl Pts',(-0.815364155350078,1.77707073165871,
9.19873077916483));
#276102=CARTESIAN_POINT('Ctrl Pts',(-0.752492914688218,1.80459931071507,
9.19481856240154));
#276103=CARTESIAN_POINT('Ctrl Pts',(-0.68827378679257,1.82876876461028,
9.19090634563826));
#276104=CARTESIAN_POINT('Ctrl Pts',(-0.624130176553013,1.85290979674757,
9.18699872939587));
#276105=CARTESIAN_POINT('Ctrl Pts',(-0.558642285150861,1.87369937628413,
9.18309111315349));
#276106=CARTESIAN_POINT('Ctrl Pts',(-0.492193636297234,1.89099482399834,
9.1791834969111));
#276107=CARTESIAN_POINT('Ctrl Pts',(-0.425786634648827,1.90827943165676,
9.17527832979746));
#276108=CARTESIAN_POINT('Ctrl Pts',(-0.358420544998612,1.92207412808434,
9.17137316268381));
#276109=CARTESIAN_POINT('Ctrl Pts',(-0.290494411596948,1.93228595110324,
9.16746799557017));
#276110=CARTESIAN_POINT('Ctrl Pts',(-0.222587553882365,1.94249487626979,
9.16356393664236));
#276111=CARTESIAN_POINT('Ctrl Pts',(-0.15412145409728,1.94912287331416,
9.15965987771456));
#276112=CARTESIAN_POINT('Ctrl Pts',(-0.085503927002166,1.95212834579779,
9.15575581878675));
#276113=CARTESIAN_POINT('Ctrl Pts',(-0.0168823378544266,1.95513399620079,
9.15185152874463));
#276114=CARTESIAN_POINT('Ctrl Pts',(0.0518902048814037,1.95451667732754,
9.14794723870251));
#276115=CARTESIAN_POINT('Ctrl Pts',(0.120404028540657,1.95028686861989,
9.14404294866039));
#276116=CARTESIAN_POINT('Ctrl Pts',(0.188990830338985,1.946052554492,9.14013449992727));
#276117=CARTESIAN_POINT('Ctrl Pts',(0.257317871206661,1.93819810172526,
9.13622605119416));
#276118=CARTESIAN_POINT('Ctrl Pts',(0.324979762284765,1.92678596478834,
9.13231760246104));
#276119=CARTESIAN_POINT('Ctrl Pts',(0.392682153635994,1.91536699690633,
9.12840681425383));
#276120=CARTESIAN_POINT('Ctrl Pts',(0.459718122725694,1.90038621401291,
9.12449602604662));
#276121=CARTESIAN_POINT('Ctrl Pts',(0.52569441628263,1.88195679564895,9.12058523783941));
#276122=CARTESIAN_POINT('Ctrl Pts',(0.591784629643076,1.86349555561685,
9.1166676969609));
#276123=CARTESIAN_POINT('Ctrl Pts',(0.656811049788291,1.84157395257368,
9.11275015608239));
#276124=CARTESIAN_POINT('Ctrl Pts',(0.720398297139112,1.81635412116665,
9.10883261520387));
#276125=CARTESIAN_POINT('Ctrl Pts',(0.750408554025555,1.80445152039857,
9.10698371604523));
#276126=CARTESIAN_POINT('Ctrl Pts',(0.780098578454699,1.791814949581,9.10513481688659));
#276127=CARTESIAN_POINT('Ctrl Pts',(0.809430877001208,1.77846497164185,
9.10328591772795));
#276128=CARTESIAN_POINT('Ctrl Pts',(0.871590768685767,1.75017420604185,
9.09936780093752));
#276129=CARTESIAN_POINT('Ctrl Pts',(0.932388891210524,1.71856457036587,
9.0954496841471));
#276130=CARTESIAN_POINT('Ctrl Pts',(0.991447614244024,1.68378966269835,
9.09153156735667));
#276131=CARTESIAN_POINT('Ctrl Pts',(1.05041740473991,1.6490671202129,9.08761935059339));
#276132=CARTESIAN_POINT('Ctrl Pts',(1.10765257356635,1.6111890128601,9.0837071338301));
#276133=CARTESIAN_POINT('Ctrl Pts',(1.16279727294156,1.57035617044022,9.07979491706682));
#276134=CARTESIAN_POINT('Ctrl Pts',(1.217877125618,1.52957134487531,9.07588730082444));
#276135=CARTESIAN_POINT('Ctrl Pts',(1.27087099755288,1.48583897614279,9.07197968458206));
#276136=CARTESIAN_POINT('Ctrl Pts',(1.32145095584223,1.43940382495798,9.06807206833967));
#276137=CARTESIAN_POINT('Ctrl Pts',(1.37199921275103,1.39299777736377,9.06416690122603));
#276138=CARTESIAN_POINT('Ctrl Pts',(1.42013619567741,1.34389263955688,9.06026173411238));
#276139=CARTESIAN_POINT('Ctrl Pts',(1.46556731482643,1.29237318360931,9.05635656699874));
#276140=CARTESIAN_POINT('Ctrl Pts',(1.51098554179404,1.24086834755629,9.05245250807093));
#276141=CARTESIAN_POINT('Ctrl Pts',(1.5536991041313,1.18695092219986,9.04854844914313));
#276142=CARTESIAN_POINT('Ctrl Pts',(1.59345180228874,1.13094091524835,9.04464439021532));
#276143=CARTESIAN_POINT('Ctrl Pts',(1.63320685374508,1.07492759259013,9.0407401001732));
#276144=CARTESIAN_POINT('Ctrl Pts',(1.67000041043341,1.0168218449986,9.03683581013108));
#276145=CARTESIAN_POINT('Ctrl Pts',(1.70361900997975,0.956973494322396,
9.03293152008896));
#276146=CARTESIAN_POINT('Ctrl Pts',(1.73727341869132,0.897061395616624,
9.02902307135584));
#276147=CARTESIAN_POINT('Ctrl Pts',(1.76774587980351,0.835403419200247,
9.02511462262273));
#276148=CARTESIAN_POINT('Ctrl Pts',(1.79486891554512,0.772373987139582,
9.02120617388961));
#276149=CARTESIAN_POINT('Ctrl Pts',(1.82200818628015,0.709306827649563,
9.0172953856824));
#276150=CARTESIAN_POINT('Ctrl Pts',(1.84579387125264,0.644867040264066,
9.01338459747519));
#276151=CARTESIAN_POINT('Ctrl Pts',(1.86610768723412,0.579446373399391,
9.00947380926798));
#276152=CARTESIAN_POINT('Ctrl Pts',(1.88645657863134,0.513912746119507,
9.00555626838946));
#276153=CARTESIAN_POINT('Ctrl Pts',(1.90332151555797,0.447395335621599,
9.00163872751095));
#276154=CARTESIAN_POINT('Ctrl Pts',(1.9166350356817,0.380297436222503,8.99772118663244));
#276155=CARTESIAN_POINT('Ctrl Pts',(1.92291840499899,0.348630312995853,
8.9958722874738));
#276156=CARTESIAN_POINT('Ctrl Pts',(1.92841147915643,0.316833982878587,
8.99402338831516));
#276157=CARTESIAN_POINT('Ctrl Pts',(1.93311118975024,0.284951097668394,
8.99217448915653));
#276158=CARTESIAN_POINT('Ctrl Pts',(1.94307063772863,0.217386099715046,
8.9882563723661));
#276159=CARTESIAN_POINT('Ctrl Pts',(1.94950332416642,0.149164392646867,
8.98433825557568));
#276160=CARTESIAN_POINT('Ctrl Pts',(1.9523333946522,0.080686530014642,8.98042013878525));
#276161=CARTESIAN_POINT('Ctrl Pts',(1.9551592035262,0.0123117835654661,
8.97650792202197));
#276162=CARTESIAN_POINT('Ctrl Pts',(1.95439314287712,-0.0563178654085932,
8.97259570525868));
#276163=CARTESIAN_POINT('Ctrl Pts',(1.95001085222104,-0.124794536018906,
8.9686834884954));
#276164=CARTESIAN_POINT('Ctrl Pts',(1.9456337148632,-0.193190682370652,
8.96477587225301));
#276165=CARTESIAN_POINT('Ctrl Pts',(1.93764882421341,-0.261433719077107,
8.96086825601063));
#276166=CARTESIAN_POINT('Ctrl Pts',(1.92608386800902,-0.32911538006514,
8.95696063976824));
#276167=CARTESIAN_POINT('Ctrl Pts',(1.91452616023048,-0.396754621048032,
8.9530554726546));
#276168=CARTESIAN_POINT('Ctrl Pts',(1.89939292061308,-0.463832700500047,
8.94915030554095));
#276169=CARTESIAN_POINT('Ctrl Pts',(1.88076353763226,-0.529947653559265,
8.94524513842731));
#276170=CARTESIAN_POINT('Ctrl Pts',(1.86213944119049,-0.596043844897758,
8.9413410794995));
#276171=CARTESIAN_POINT('Ctrl Pts',(1.84002130424594,-0.661176979189807,
8.93743702057169));
#276172=CARTESIAN_POINT('Ctrl Pts',(1.81453894256888,-0.724958223555688,
8.93353296164389));
#276173=CARTESIAN_POINT('Ctrl Pts',(1.78905507237499,-0.788743243673656,
8.92962867160177));
#276174=CARTESIAN_POINT('Ctrl Pts',(1.760206766927,-0.851175759158179,8.92572438155965));
#276175=CARTESIAN_POINT('Ctrl Pts',(1.72817207348456,-0.911886662051858,
8.92182009151753));
#276176=CARTESIAN_POINT('Ctrl Pts',(1.69610325798926,-0.972662231730667,
8.91791164278441));
#276177=CARTESIAN_POINT('Ctrl Pts',(1.66084151109396,-1.03171209327063,
8.91400319405129));
#276178=CARTESIAN_POINT('Ctrl Pts',(1.62261049358127,-1.08869242034652,
8.91009474531818));
#276179=CARTESIAN_POINT('Ctrl Pts',(1.58435659218775,-1.14570685404836,
8.90618395711097));
#276180=CARTESIAN_POINT('Ctrl Pts',(1.54313017825848,-1.20064889444029,
8.90227316890376));
#276181=CARTESIAN_POINT('Ctrl Pts',(1.49919615738359,-1.25320663965935,
8.89836238069655));
#276182=CARTESIAN_POINT('Ctrl Pts',(1.45518627660879,-1.30585513517196,
8.89444483981803));
#276183=CARTESIAN_POINT('Ctrl Pts',(1.40845979276512,-1.35611075878259,
8.89052729893952));
#276184=CARTESIAN_POINT('Ctrl Pts',(1.359318882882,-1.40369803541946,8.88660975806101));
#276185=CARTESIAN_POINT('Ctrl Pts',(1.33612663301012,-1.42615704183813,
8.88476085890236));
#276186=CARTESIAN_POINT('Ctrl Pts',(1.3123970760063,-1.44802227902029,8.88291195974372));
#276187=CARTESIAN_POINT('Ctrl Pts',(1.28816437580854,-1.46926802895108,
8.88106306058508));
#276188=CARTESIAN_POINT('Ctrl Pts',(1.2368113590264,-1.51429121430976,8.87714494379466));
#276189=CARTESIAN_POINT('Ctrl Pts',(1.18299326569307,-1.55670811660198,
8.87322682700423));
#276190=CARTESIAN_POINT('Ctrl Pts',(1.12700541744814,-1.59623769816483,
8.86930871021381));
#276191=CARTESIAN_POINT('Ctrl Pts',(1.07110187751812,-1.6357077548037,8.86539649345053));
#276192=CARTESIAN_POINT('Ctrl Pts',(1.01303546567295,-1.67229883817997,
8.86148427668724));
#276193=CARTESIAN_POINT('Ctrl Pts',(0.953135596431997,-1.70576919154211,
8.85757205992396));
#276194=CARTESIAN_POINT('Ctrl Pts',(0.893306165670571,-1.73920018587343,
8.85366444368157));
#276195=CARTESIAN_POINT('Ctrl Pts',(0.831647986783256,-1.7695174996381,
8.84975682743919));
#276196=CARTESIAN_POINT('Ctrl Pts',(0.768519036298377,-1.79652288904066,
8.84584921119681));
#276197=CARTESIAN_POINT('Ctrl Pts',(0.705429652372076,-1.8235113526063,
8.84194404408317));
#276198=CARTESIAN_POINT('Ctrl Pts',(0.640871776664479,-1.84719181646173,
8.83803887696952));
#276199=CARTESIAN_POINT('Ctrl Pts',(0.575226142431937,-1.86741288553519,
8.83413370985588));
#276200=CARTESIAN_POINT('Ctrl Pts',(0.509599136739551,-1.88762821639009,
8.83022965092808));
#276201=CARTESIAN_POINT('Ctrl Pts',(0.442885455163538,-1.90438595654717,
8.82632559200028));
#276202=CARTESIAN_POINT('Ctrl Pts',(0.375482158754177,-1.91758419592395,
8.82242153307247));
#276203=CARTESIAN_POINT('Ctrl Pts',(0.308074872172716,-1.93078321661632,
8.81851724303035));
#276204=CARTESIAN_POINT('Ctrl Pts',(0.239978372911714,-1.94042222617882,
8.81461295298823));
#276205=CARTESIAN_POINT('Ctrl Pts',(0.171599320243784,-1.94645053194061,
8.8107086629461));
#276206=CARTESIAN_POINT('Ctrl Pts',(0.103147432989423,-1.95248525880856,
8.80680021421299));
#276207=CARTESIAN_POINT('Ctrl Pts',(0.0344128826163948,-1.95490156322096,
8.80289176547987));
#276208=CARTESIAN_POINT('Ctrl Pts',(-0.034194161530893,-1.95370078551379,
8.79898331674676));
#276209=CARTESIAN_POINT('Ctrl Pts',(-0.102842271690139,-1.95249928905897,
8.79507252853955));
#276210=CARTESIAN_POINT('Ctrl Pts',(-0.171362232997545,-1.94767643613482,
8.79116174033234));
#276211=CARTESIAN_POINT('Ctrl Pts',(-0.239348316416433,-1.93928553426993,
8.78725095212513));
#276212=CARTESIAN_POINT('Ctrl Pts',(-0.307451789898405,-1.93088014402081,
8.78333341124662));
#276213=CARTESIAN_POINT('Ctrl Pts',(-0.375019061595339,-1.91889449458849,
8.77941587036811));
#276214=CARTESIAN_POINT('Ctrl Pts',(-0.441654780584861,-1.90343296566665,
8.7754983294896));
#276215=CARTESIAN_POINT('Ctrl Pts',(-0.473103775910238,-1.89613583496618,
8.77364943033096));
#276216=CARTESIAN_POINT('Ctrl Pts',(-0.504345501457461,-1.88806520565594,
8.77180053117231));
#276217=CARTESIAN_POINT('Ctrl Pts',(-0.535339817952452,-1.87923582323098,
8.76995163201367));
#276218=CARTESIAN_POINT('Ctrl Pts',(-0.601021794873224,-1.86052493174368,
8.76603351522324));
#276219=CARTESIAN_POINT('Ctrl Pts',(-0.665851834598212,-1.83832928533814,
8.76211539843282));
#276220=CARTESIAN_POINT('Ctrl Pts',(-0.729433632825423,-1.81274448704254,
8.75819728164239));
#276221=CARTESIAN_POINT('Ctrl Pts',(-0.792919687521939,-1.7871982151647,
8.75428506487911));
#276222=CARTESIAN_POINT('Ctrl Pts',(-0.85516077849453,-1.75827310216983,
8.75037284811583));
#276223=CARTESIAN_POINT('Ctrl Pts',(-0.915775101602816,-1.72611470165929,
8.74646063135254));
#276224=CARTESIAN_POINT('Ctrl Pts',(-0.976318146078768,-1.69399411740553,
8.74255301511016));
#276225=CARTESIAN_POINT('Ctrl Pts',(-1.03523778943443,-1.6586480261867,
8.73864539886777));
#276226=CARTESIAN_POINT('Ctrl Pts',(-1.09217328346492,-1.62026958216386,
8.73473778262538));
#276227=CARTESIAN_POINT('Ctrl Pts',(-1.14907309273361,-1.58191519212802,
8.73083261551174));
#276228=CARTESIAN_POINT('Ctrl Pts',(-1.2039908125922,-1.54053249369231,
8.7269274483981));
#276229=CARTESIAN_POINT('Ctrl Pts',(-1.25659270252728,-1.49635917478231,
8.72302228128445));
#276230=CARTESIAN_POINT('Ctrl Pts',(-1.3091796654009,-1.45219839112241,
8.71911822235665));
#276231=CARTESIAN_POINT('Ctrl Pts',(-1.35945172645085,-1.40524887523147,
8.71521416342884));
#276232=CARTESIAN_POINT('Ctrl Pts',(-1.40710785536954,-1.35578887860807,
8.71131010450104));
#276233=CARTESIAN_POINT('Ctrl Pts',(-1.45476680545818,-1.30632595402851,
8.70740581445891));
#276234=CARTESIAN_POINT('Ctrl Pts',(-1.49980917652182,-1.25435260964972,
8.70350152441679));
#276235=CARTESIAN_POINT('Ctrl Pts',(-1.54197175482886,-1.20018294743343,
8.69959723437466));
#276236=CARTESIAN_POINT('Ctrl Pts',(-1.58417924299986,-1.14595558589565,
8.69568878564155));
#276237=CARTESIAN_POINT('Ctrl Pts',(-1.62350051405559,-1.08952762665063,
8.69178033690843));
#276238=CARTESIAN_POINT('Ctrl Pts',(-1.65971415905155,-1.03124435040576,
8.68787188817532));
#276239=CARTESIAN_POINT('Ctrl Pts',(-1.69594948039281,-0.972926187630654,
8.6839610999681));
#276240=CARTESIAN_POINT('Ctrl Pts',(-1.72907323645024,-0.912750928657007,
8.6800503117609));
#276241=CARTESIAN_POINT('Ctrl Pts',(-1.75891008121036,-0.851088318693526,
8.67613952355368));
#276242=CARTESIAN_POINT('Ctrl Pts',(-1.78879844458889,-0.789319237268361,
8.67222198267517));
#276243=CARTESIAN_POINT('Ctrl Pts',(-1.81538837891523,-0.726058132398077,
8.66830444179666));
#276244=CARTESIAN_POINT('Ctrl Pts',(-1.83855307077977,-0.661693740280396,
8.66438690091814));
#276245=CARTESIAN_POINT('Ctrl Pts',(-1.849485740183,-0.631316706798713,
8.66253800175951));
#276246=CARTESIAN_POINT('Ctrl Pts',(-1.85965619655906,-0.600694128694863,
8.66068910260087));
#276247=CARTESIAN_POINT('Ctrl Pts',(-1.86905504921175,-0.569867724139624,
8.65884020344224));
#276248=CARTESIAN_POINT('Ctrl Pts',(-1.89340905280269,-0.489991339757814,
8.65404939562637));
#276249=CARTESIAN_POINT('Ctrl Pts',(-1.91265750479486,-0.408490306856713,
8.6492585878105));
#276250=CARTESIAN_POINT('Ctrl Pts',(-1.92662122241073,-0.32595500511049,
8.64446777999463));
#276251=CARTESIAN_POINT('Ctrl Pts',(-1.94038744774897,-0.24458702034784,
8.63974472974686));
#276252=CARTESIAN_POINT('Ctrl Pts',(-1.94901732302756,-0.162213796102582,
8.63502167949909));
#276253=CARTESIAN_POINT('Ctrl Pts',(-1.9523852493591,-0.0794218992784852,
8.63029862925131));
#276254=CARTESIAN_POINT('Ctrl Pts',(-1.95343797789026,-0.0535432477417661,
8.62882232328127));
#276255=CARTESIAN_POINT('Ctrl Pts',(-1.95397694480636,-0.0276238470575762,
8.62734601731123));
#276256=CARTESIAN_POINT('Ctrl Pts',(-1.9539992760325,-0.00168204175487709,
8.62586971134118));
#276257=CARTESIAN_POINT('',(-1.95392409726504,0.000980978241176287,7.92586964537097));
#276258=CARTESIAN_POINT('Ctrl Pts',(-1.95279265841963,-0.00168066560016861,
8.62586969212423));
#276259=CARTESIAN_POINT('Ctrl Pts',(-1.94903606971378,0.455740440167666,
8.59982271970643));
#276260=CARTESIAN_POINT('Ctrl Pts',(-1.56056803492106,1.56933253783666,
8.53673860443147));
#276261=CARTESIAN_POINT('Ctrl Pts',(0.294625979349027,2.29046986711343,
8.43661734629939));
#276262=CARTESIAN_POINT('Ctrl Pts',(2.08390512471393,0.995186470493358,
8.32550591772794));
#276263=CARTESIAN_POINT('Ctrl Pts',(1.96659392361522,-1.21060522857867,
8.21439448915653));
#276264=CARTESIAN_POINT('Ctrl Pts',(0.050021832127414,-2.30879936247667,
8.10328306058509));
#276265=CARTESIAN_POINT('Ctrl Pts',(-1.64852255647152,-1.43097552685388,
8.007108128241));
#276266=CARTESIAN_POINT('Ctrl Pts',(-1.94951932046294,-0.387895067694587,
7.94797033875404));
#276267=CARTESIAN_POINT('Ctrl Pts',(-1.95128373292697,0.000978829950653015,
7.92586969212423));
#276268=CARTESIAN_POINT('',(-1.95399967035838,0.00113500632438228,7.22586969217443));
#276269=CARTESIAN_POINT('Ctrl Pts',(-1.95399975372591,0.000981039797854494,
7.92586964403131));
#276270=CARTESIAN_POINT('Ctrl Pts',(-1.95396164266519,0.0768892786098886,
7.92156158023155));
#276271=CARTESIAN_POINT('Ctrl Pts',(-1.94949609136418,0.152646150253345,
7.9172535164318));
#276272=CARTESIAN_POINT('Ctrl Pts',(-1.9406806068828,0.227760361057462,
7.91294545263205));
#276273=CARTESIAN_POINT('Ctrl Pts',(-1.93183365313758,0.303142712418422,
7.90862201002962));
#276274=CARTESIAN_POINT('Ctrl Pts',(-1.91860579166216,0.377877515271295,
7.90429856742719));
#276275=CARTESIAN_POINT('Ctrl Pts',(-1.90112531659489,0.451484806612561,
7.89997512482476));
#276276=CARTESIAN_POINT('Ctrl Pts',(-1.88356128832724,0.525443926193005,
7.89563101702503));
#276277=CARTESIAN_POINT('Ctrl Pts',(-1.86170404067933,0.598264447757228,
7.89128690922531));
#276278=CARTESIAN_POINT('Ctrl Pts',(-1.83573194611037,0.669480561353234,
7.88694280142558));
#276279=CARTESIAN_POINT('Ctrl Pts',(-1.82400852685083,0.701626461465531,
7.88498193543113));
#276280=CARTESIAN_POINT('Ctrl Pts',(-1.81144735004282,0.733445775577763,
7.88302106943669));
#276281=CARTESIAN_POINT('Ctrl Pts',(-1.79806788981147,0.764897289594456,
7.88106020344224));
#276282=CARTESIAN_POINT('Ctrl Pts',(-1.77133363671727,0.827742331276123,
7.87714208665181));
#276283=CARTESIAN_POINT('Ctrl Pts',(-1.74124763534362,0.889308663726999,
7.87322396986138));
#276284=CARTESIAN_POINT('Ctrl Pts',(-1.70795403340147,0.949214949201517,
7.86930585307096));
#276285=CARTESIAN_POINT('Ctrl Pts',(-1.67471056604327,1.00903102585144,
7.86539363630767));
#276286=CARTESIAN_POINT('Ctrl Pts',(-1.63826932119591,1.06719159016438,
7.86148141954439));
#276287=CARTESIAN_POINT('Ctrl Pts',(-1.59882220601409,1.12333590415167,
7.8575692027811));
#276288=CARTESIAN_POINT('Ctrl Pts',(-1.55942147815914,1.17941419595628,
7.85366158653872));
#276289=CARTESIAN_POINT('Ctrl Pts',(-1.51702218140544,1.23348054567958,
7.84975397029633));
#276290=CARTESIAN_POINT('Ctrl Pts',(-1.47186083526503,1.28520102770459,
7.84584635405395));
#276291=CARTESIAN_POINT('Ctrl Pts',(-1.42672779434805,1.33688909351695,
7.8419411869403));
#276292=CARTESIAN_POINT('Ctrl Pts',(-1.37883646086518,1.38623383854134,
7.83803601982666));
#276293=CARTESIAN_POINT('Ctrl Pts',(-1.32846418350209,1.43293367367514,
7.83413085271301));
#276294=CARTESIAN_POINT('Ctrl Pts',(-1.27810620049383,1.47962025659862,
7.83022679378521));
#276295=CARTESIAN_POINT('Ctrl Pts',(-1.2252690317646,1.5236630853598,7.8263227348574));
#276296=CARTESIAN_POINT('Ctrl Pts',(-1.17026620660454,1.56479807185446,
7.82241867592959));
#276297=CARTESIAN_POINT('Ctrl Pts',(-1.11526012536134,1.60593549347741,
7.81851438588747));
#276298=CARTESIAN_POINT('Ctrl Pts',(-1.05808852859925,1.64416443854038,
7.81461009584535));
#276299=CARTESIAN_POINT('Ctrl Pts',(-0.999095814633345,1.67926280051162,
7.81070580580322));
#276300=CARTESIAN_POINT('Ctrl Pts',(-0.940040264027335,1.71439854783084,
7.8067973570701));
#276301=CARTESIAN_POINT('Ctrl Pts',(-0.879160148548953,1.74639680530431,
7.80288890833698));
#276302=CARTESIAN_POINT('Ctrl Pts',(-0.816825604091032,1.77508082421655,
7.79898045960386));
#276303=CARTESIAN_POINT('Ctrl Pts',(-0.754453748141543,1.80378201247749,
7.79506967139665));
#276304=CARTESIAN_POINT('Ctrl Pts',(-0.690626187733681,1.8291648322634,
7.79115888318944));
#276305=CARTESIAN_POINT('Ctrl Pts',(-0.625731604650915,1.85110128273441,
7.78724809498223));
#276306=CARTESIAN_POINT('Ctrl Pts',(-0.56072496953018,1.87307561038815,
7.78333055410371));
#276307=CARTESIAN_POINT('Ctrl Pts',(-0.494648107975295,1.89159155929559,
7.7794130132252));
#276308=CARTESIAN_POINT('Ctrl Pts',(-0.42790250949824,1.90657164627116,
7.77549547234669));
#276309=CARTESIAN_POINT('Ctrl Pts',(-0.396401656107539,1.91364155851053,
7.77364657318806));
#276310=CARTESIAN_POINT('Ctrl Pts',(-0.364751958044,1.91992463777932,7.77179767402944));
#276311=CARTESIAN_POINT('Ctrl Pts',(-0.332995977480395,1.92541675462272,
7.76994877487081));
#276312=CARTESIAN_POINT('Ctrl Pts',(-0.265699911027953,1.93705543979314,
7.76603065808039));
#276313=CARTESIAN_POINT('Ctrl Pts',(-0.197659524970958,1.94518480848424,
7.76211254128997));
#276314=CARTESIAN_POINT('Ctrl Pts',(-0.129273359947703,1.94971905627653,
7.75819442449954));
#276315=CARTESIAN_POINT('Ctrl Pts',(-0.0609901730262491,1.95424647625166,
7.75428220773626));
#276316=CARTESIAN_POINT('Ctrl Pts',(0.00763727263162475,1.95518948722522,
7.75036999097297));
#276317=CARTESIAN_POINT('Ctrl Pts',(0.0762018291558524,1.95251358029421,
7.74645777420969));
#276318=CARTESIAN_POINT('Ctrl Pts',(0.144685758073215,1.94984082006147,
7.74255015796731));
#276319=CARTESIAN_POINT('Ctrl Pts',(0.213106455551338,1.94355761274228,
7.73864254172492));
#276320=CARTESIAN_POINT('Ctrl Pts',(0.281055092687847,1.93368147192712,
7.73473492548254));
#276321=CARTESIAN_POINT('Ctrl Pts',(0.348961142489828,1.9238115210597,7.73082975836889));
#276322=CARTESIAN_POINT('Ctrl Pts',(0.416395233184727,1.91035317433958,
7.72692459125525));
#276323=CARTESIAN_POINT('Ctrl Pts',(0.482953547812651,1.89337578696232,
7.7230194241416));
#276324=CARTESIAN_POINT('Ctrl Pts',(0.549492974905274,1.87640321733029,
7.7191153652138));
#276325=CARTESIAN_POINT('Ctrl Pts',(0.615156642895896,1.8559137109765,7.71521130628599));
#276326=CARTESIAN_POINT('Ctrl Pts',(0.67955260712821,1.83202736173488,7.71130724735818));
#276327=CARTESIAN_POINT('Ctrl Pts',(0.74395238350307,1.80813959845793,7.70740295731606));
#276328=CARTESIAN_POINT('Ctrl Pts',(0.807083846844779,1.78085476653105,
7.70349866727394));
#276329=CARTESIAN_POINT('Ctrl Pts',(0.868573570370838,1.75034166746189,
7.69959437723182));
#276330=CARTESIAN_POINT('Ctrl Pts',(0.930128790250098,1.71979606708032,
7.69568592849871));
#276331=CARTESIAN_POINT('Ctrl Pts',(0.990038338962065,1.68601555620313,
7.69177747976559));
#276332=CARTESIAN_POINT('Ctrl Pts',(1.04795292777079,1.64921516521545,7.68786903103247));
#276333=CARTESIAN_POINT('Ctrl Pts',(1.10590218242506,1.61239274667485,7.68395824282526));
#276334=CARTESIAN_POINT('Ctrl Pts',(1.16185369993829,1.57254713592708,7.68004745461805));
#276335=CARTESIAN_POINT('Ctrl Pts',(1.21548907916982,1.52993539027598,7.67613666641084));
#276336=CARTESIAN_POINT('Ctrl Pts',(1.26921706942169,1.48725006786827,7.67221912553233));
#276337=CARTESIAN_POINT('Ctrl Pts',(1.32062057131954,1.44178940366806,7.66830158465381));
#276338=CARTESIAN_POINT('Ctrl Pts',(1.36941667118543,1.3938486218666,7.6643840437753));
#276339=CARTESIAN_POINT('Ctrl Pts',(1.39244618658421,1.37122277726507,7.66253514461666));
#276340=CARTESIAN_POINT('Ctrl Pts',(1.41489549543891,1.34804500764465,7.66068624545802));
#276341=CARTESIAN_POINT('Ctrl Pts',(1.43673803704815,1.32434882598923,7.65883734629937));
#276342=CARTESIAN_POINT('Ctrl Pts',(1.48302592063803,1.2741327789003,7.65491922950895));
#276343=CARTESIAN_POINT('Ctrl Pts',(1.52676970802628,1.22138752475329,7.65100111271853));
#276344=CARTESIAN_POINT('Ctrl Pts',(1.56768109536323,1.16640129597011,7.6470829959281));
#276345=CARTESIAN_POINT('Ctrl Pts',(1.6085308770083,1.11149786723083,7.64317077916482));
#276346=CARTESIAN_POINT('Ctrl Pts',(1.64655643209863,1.05436055256439,7.63925856240154));
#276347=CARTESIAN_POINT('Ctrl Pts',(1.68150787662658,0.995312644771864,
7.63534634563826));
#276348=CARTESIAN_POINT('Ctrl Pts',(1.71641822045364,0.936334173605751,
7.63143872939587));
#276349=CARTESIAN_POINT('Ctrl Pts',(1.74826138372243,0.875449992650089,
7.62753111315349));
#276350=CARTESIAN_POINT('Ctrl Pts',(1.77683027071511,0.813013031304224,
7.62362349691111));
#276351=CARTESIAN_POINT('Ctrl Pts',(1.80538125193662,0.750615202807394,
7.61971832979746));
#276352=CARTESIAN_POINT('Ctrl Pts',(1.83066182355119,0.686666970751107,
7.61581316268382));
#276353=CARTESIAN_POINT('Ctrl Pts',(1.85251115741193,0.621545180710399,
7.61190799557018));
#276354=CARTESIAN_POINT('Ctrl Pts',(1.87435429099451,0.556441870556314,
7.60800393664238));
#276355=CARTESIAN_POINT('Ctrl Pts',(1.892767963391,0.490166129643999,7.60409987771457));
#276356=CARTESIAN_POINT('Ctrl Pts',(1.90764040955008,0.423112358424593,
7.60019581878677));
#276357=CARTESIAN_POINT('Ctrl Pts',(1.92251373613521,0.356054617724526,
7.59629152874465));
#276358=CARTESIAN_POINT('Ctrl Pts',(1.9338453162782,0.288219236039119,7.59238723870253));
#276359=CARTESIAN_POINT('Ctrl Pts',(1.94157434747052,0.220011484346647,
7.58848294866041));
#276360=CARTESIAN_POINT('Ctrl Pts',(1.94931161131259,0.151731080530541,
7.5845744999273));
#276361=CARTESIAN_POINT('Ctrl Pts',(1.95343861267395,0.0830780048401049,
7.58066605119418));
#276362=CARTESIAN_POINT('Ctrl Pts',(1.95394647852218,0.0144623328255586,
7.57675760246107));
#276363=CARTESIAN_POINT('Ctrl Pts',(1.95445464836289,-0.0541944103653153,
7.57284681425386));
#276364=CARTESIAN_POINT('Ctrl Pts',(1.95133939366496,-0.122813213881998,
7.56893602604665));
#276365=CARTESIAN_POINT('Ctrl Pts',(1.94464390303761,-0.19098714715567,
7.56502523783944));
#276366=CARTESIAN_POINT('Ctrl Pts',(1.93793685145502,-0.259278794848623,
7.56110769696093));
#276367=CARTESIAN_POINT('Ctrl Pts',(1.92763729962266,-0.327123553149722,
7.55719015608242));
#276368=CARTESIAN_POINT('Ctrl Pts',(1.91383975088898,-0.394123594722792,
7.55327261520391));
#276369=CARTESIAN_POINT('Ctrl Pts',(1.90732794232431,-0.425744533555481,
7.55142371604526));
#276370=CARTESIAN_POINT('Ctrl Pts',(1.90003771407892,-0.457177526489178,
7.54957481688661));
#276371=CARTESIAN_POINT('Ctrl Pts',(1.89198280763412,-0.488382079541124,
7.54772591772796));
#276372=CARTESIAN_POINT('Ctrl Pts',(1.87491315619368,-0.554509581778629,
7.54380780093753));
#276373=CARTESIAN_POINT('Ctrl Pts',(1.85433861754993,-0.61987217910844,
7.53988968414711));
#276374=CARTESIAN_POINT('Ctrl Pts',(1.83034489736836,-0.684071309643672,
7.53597156735668));
#276375=CARTESIAN_POINT('Ctrl Pts',(1.80638730770762,-0.748173767049212,
7.5320593505934));
#276376=CARTESIAN_POINT('Ctrl Pts',(1.77902092569981,-0.811115777686176,
7.52814713383011));
#276377=CARTESIAN_POINT('Ctrl Pts',(1.74838175314181,-0.872512031596563,
7.52423491706683));
#276378=CARTESIAN_POINT('Ctrl Pts',(1.71777861032403,-0.933836087373181,
7.52032730082445));
#276379=CARTESIAN_POINT('Ctrl Pts',(1.68391053892414,-0.993617558392718,
7.51641968458206));
#276380=CARTESIAN_POINT('Ctrl Pts',(1.64696165082001,-1.05149099888122,
7.51251206833968));
#276381=CARTESIAN_POINT('Ctrl Pts',(1.61003592071762,-1.10932816674273,
7.50860690122603));
#276382=CARTESIAN_POINT('Ctrl Pts',(1.57003346835176,-1.16525926264657,
7.50470173411239));
#276383=CARTESIAN_POINT('Ctrl Pts',(1.52718359803182,-1.21894473127479,
7.50079656699874));
#276384=CARTESIAN_POINT('Ctrl Pts',(1.48434588740137,-1.27261496534984,
7.49689250807094));
#276385=CARTESIAN_POINT('Ctrl Pts',(1.43866266958375,-1.32404045294532,
7.49298844914313));
#276386=CARTESIAN_POINT('Ctrl Pts',(1.39040461434827,-1.37291332880086,
7.48908439021533));
#276387=CARTESIAN_POINT('Ctrl Pts',(1.34214370230976,-1.42178909785585,
7.4851801001732));
#276388=CARTESIAN_POINT('Ctrl Pts',(1.29130799766047,-1.46811160696053,
7.48127581013109));
#276389=CARTESIAN_POINT('Ctrl Pts',(1.23820495112629,-1.51160990305249,
7.47737152008897));
#276390=CARTESIAN_POINT('Ctrl Pts',(1.18504534138621,-1.55515453176072,
7.47346307135585));
#276391=CARTESIAN_POINT('Ctrl Pts',(1.12961395125601,-1.59586863165535,
7.46955462262273));
#276392=CARTESIAN_POINT('Ctrl Pts',(1.07225044145295,-1.63352226516933,
7.46564617388961));
#276393=CARTESIAN_POINT('Ctrl Pts',(1.01485259566282,-1.67119843696031,
7.4617353856824));
#276394=CARTESIAN_POINT('Ctrl Pts',(0.955520753468631,-1.70581024866879,
7.45782459747519));
#276395=CARTESIAN_POINT('Ctrl Pts',(0.894620179441413,-1.73717320222717,
7.45391380926798));
#276396=CARTESIAN_POINT('Ctrl Pts',(0.833614449743095,-1.7685903095022,
7.44999626838946));
#276397=CARTESIAN_POINT('Ctrl Pts',(0.771035030420414,-1.7967471607843,
7.44607872751095));
#276398=CARTESIAN_POINT('Ctrl Pts',(0.707267379576142,-1.82150730269947,
7.44216118663244));
#276399=CARTESIAN_POINT('Ctrl Pts',(0.677171980536121,-1.83319295116478,
7.4403122874738));
#276400=CARTESIAN_POINT('Ctrl Pts',(0.646812134387758,-1.84412273682034,
7.43846338831516));
#276401=CARTESIAN_POINT('Ctrl Pts',(0.616229312545353,-1.8542862331258,
7.43661448915652));
#276402=CARTESIAN_POINT('Ctrl Pts',(0.551419359444688,-1.87582432801744,
7.43269637236609));
#276403=CARTESIAN_POINT('Ctrl Pts',(0.485350392409882,-1.89400322691309,
7.42877825557567));
#276404=CARTESIAN_POINT('Ctrl Pts',(0.41840371345753,-1.90867868761742,
7.42486013878524));
#276405=CARTESIAN_POINT('Ctrl Pts',(0.351557844982249,-1.92333204953779,
7.42094792202196));
#276406=CARTESIAN_POINT('Ctrl Pts',(0.283837364276381,-1.93449233896904,
7.41703570525867));
#276407=CARTESIAN_POINT('Ctrl Pts',(0.215639729230009,-1.94206475360056,
7.41312348849539));
#276408=CARTESIAN_POINT('Ctrl Pts',(0.147522290313935,-1.94962826354866,
7.409215872253));
#276409=CARTESIAN_POINT('Ctrl Pts',(0.0789292979784414,-1.95361222389878,
7.40530825601062));
#276410=CARTESIAN_POINT('Ctrl Pts',(0.0102676254828897,-1.95397302332119,
7.40140063976823));
#276411=CARTESIAN_POINT('Ctrl Pts',(-0.0583510127776918,-1.95433359660976,
7.39749547265459));
#276412=CARTESIAN_POINT('Ctrl Pts',(-0.127037755040009,-1.95107551102531,
7.39359030554095));
#276413=CARTESIAN_POINT('Ctrl Pts',(-0.195382957862223,-1.94420716483018,
7.3896851384273));
#276414=CARTESIAN_POINT('Ctrl Pts',(-0.263708766076322,-1.93734076769479,
7.3857810794995));
#276415=CARTESIAN_POINT('Ctrl Pts',(-0.331692738068321,-1.92686619291591,
7.38187702057169));
#276416=CARTESIAN_POINT('Ctrl Pts',(-0.398929408338525,-1.91284378012494,
7.37797296164389));
#276417=CARTESIAN_POINT('Ctrl Pts',(-0.466170058916744,-1.89882053722859,
7.37406867160176));
#276418=CARTESIAN_POINT('Ctrl Pts',(-0.532662838948834,-1.88124914227677,
7.37016438155964));
#276419=CARTESIAN_POINT('Ctrl Pts',(-0.598013334912811,-1.86024085840153,
7.36626009151752));
#276420=CARTESIAN_POINT('Ctrl Pts',(-0.663433439567792,-1.83921019735655,
7.3623516427844));
#276421=CARTESIAN_POINT('Ctrl Pts',(-0.727708362792241,-1.81473549232277,
7.35844319405129));
#276422=CARTESIAN_POINT('Ctrl Pts',(-0.790460669873548,-1.78697731641537,
7.35453474531817));
#276423=CARTESIAN_POINT('Ctrl Pts',(-0.853250538505934,-1.75920252533968,
7.35062395711096));
#276424=CARTESIAN_POINT('Ctrl Pts',(-0.914515538387683,-1.72814057438052,
7.34671316890375));
#276425=CARTESIAN_POINT('Ctrl Pts',(-0.973902514019989,-1.69399819751544,
7.34280238069653));
#276426=CARTESIAN_POINT('Ctrl Pts',(-1.03339203182661,-1.6597968677651,
7.33888483981802));
#276427=CARTESIAN_POINT('Ctrl Pts',(-1.09099664070203,-1.62250476359817,
7.33496729893951));
#276428=CARTESIAN_POINT('Ctrl Pts',(-1.14639258813295,-1.58237164846753,
7.33104975806099));
#276429=CARTESIAN_POINT('Ctrl Pts',(-1.17253692810868,-1.56343066352329,
7.32920085890236));
#276430=CARTESIAN_POINT('Ctrl Pts',(-1.19818979671896,-1.54385744700979,
7.32735195974373));
#276431=CARTESIAN_POINT('Ctrl Pts',(-1.22331993532184,-1.52368117919864,
7.3255030605851));
#276432=CARTESIAN_POINT('Ctrl Pts',(-1.27589864383253,-1.48146724155033,
7.32163468837022));
#276433=CARTESIAN_POINT('Ctrl Pts',(-1.32640679421288,-1.43643430037098,
7.31776631615534));
#276434=CARTESIAN_POINT('Ctrl Pts',(-1.37452068432708,-1.38881564232155,
7.31389794394046));
#276435=CARTESIAN_POINT('Ctrl Pts',(-1.42255195296738,-1.34127875533041,
7.31003621451862));
#276436=CARTESIAN_POINT('Ctrl Pts',(-1.46819676697969,-1.29116531828427,
7.30617448509677));
#276437=CARTESIAN_POINT('Ctrl Pts',(-1.51116392529286,-1.2387492041949,
7.30231275567492));
#276438=CARTESIAN_POINT('Ctrl Pts',(-1.55408997821229,-1.1863832350323,
7.29845472065398));
#276439=CARTESIAN_POINT('Ctrl Pts',(-1.59434313263755,-1.13171934287596,
7.29459668563303));
#276440=CARTESIAN_POINT('Ctrl Pts',(-1.63166963652991,-1.0750675314725,
7.29073865061208));
#276441=CARTESIAN_POINT('Ctrl Pts',(-1.66897401501377,-1.01844930061738,
7.28688290245414));
#276442=CARTESIAN_POINT('Ctrl Pts',(-1.70335490479476,-0.959845908057318,
7.2830271542962));
#276443=CARTESIAN_POINT('Ctrl Pts',(-1.73460062779139,-0.899598055837012,
7.27917140613825));
#276444=CARTESIAN_POINT('Ctrl Pts',(-1.76583919829406,-0.839363995021011,
7.275316540604));
#276445=CARTESIAN_POINT('Ctrl Pts',(-1.79394379459118,-0.777486670783983,
7.27146167506975));
#276446=CARTESIAN_POINT('Ctrl Pts',(-1.81874862909382,-0.714331452596999,
7.2676068095355));
#276447=CARTESIAN_POINT('Ctrl Pts',(-1.84357152823297,-0.651130240309164,
7.26374913661526));
#276448=CARTESIAN_POINT('Ctrl Pts',(-1.86508967956487,-0.586649746365874,
7.25989146369503));
#276449=CARTESIAN_POINT('Ctrl Pts',(-1.88318592322611,-0.521274187508859,
7.2560337907748));
#276450=CARTESIAN_POINT('Ctrl Pts',(-1.90128911181104,-0.455873539010295,
7.25217463736809));
#276451=CARTESIAN_POINT('Ctrl Pts',(-1.91596766743185,-0.389577635578429,
7.24831548396138));
#276452=CARTESIAN_POINT('Ctrl Pts',(-1.92715537849078,-0.322781887896566,
7.24445633055467));
#276453=CARTESIAN_POINT('Ctrl Pts',(-1.93836046069429,-0.255882426543101,
7.24059118504543));
#276454=CARTESIAN_POINT('Ctrl Pts',(-1.9460638204368,-0.188482074251308,
7.23672603953618));
#276455=CARTESIAN_POINT('Ctrl Pts',(-1.95025114287136,-0.120981319752049,
7.23286089402694));
#276456=CARTESIAN_POINT('Ctrl Pts',(-1.9527757926585,-0.0802832918018328,
7.23053049340943));
#276457=CARTESIAN_POINT('Ctrl Pts',(-1.95402330207662,-0.0395487931071784,
7.22820009279193));
#276458=CARTESIAN_POINT('Ctrl Pts',(-1.95399967035838,0.00113500632439505,
7.22586969217443));
#276459=CARTESIAN_POINT('',(-1.95399924754167,-0.00171481969227626,6.52586969212423));
#276460=CARTESIAN_POINT('Ctrl Pts',(-1.95399967035787,0.00113500720075899,
7.22586969212423));
#276461=CARTESIAN_POINT('Ctrl Pts',(-1.95396087209433,0.0679291157453965,
7.22204367208738));
#276462=CARTESIAN_POINT('Ctrl Pts',(-1.95049746579392,0.134622301780259,
7.21821765205052));
#276463=CARTESIAN_POINT('Ctrl Pts',(-1.94363877693846,0.200958465313502,
7.21439163201366));
#276464=CARTESIAN_POINT('Ctrl Pts',(-1.93661499146268,0.26889141748018,
7.21047351522322));
#276465=CARTESIAN_POINT('Ctrl Pts',(-1.92601146431731,0.33659035382485,
7.20655539843279));
#276466=CARTESIAN_POINT('Ctrl Pts',(-1.91185354481783,0.40364839051768,
7.20263728164236));
#276467=CARTESIAN_POINT('Ctrl Pts',(-1.89771694477201,0.470605449047257,
7.19872506487907));
#276468=CARTESIAN_POINT('Ctrl Pts',(-1.88003667562339,0.536923045882934,
7.19481284811578));
#276469=CARTESIAN_POINT('Ctrl Pts',(-1.85888979610215,0.602199905303309,
7.19090063135249));
#276470=CARTESIAN_POINT('Ctrl Pts',(-1.83776778398139,0.667400003241948,
7.1869930151101));
#276471=CARTESIAN_POINT('Ctrl Pts',(-1.81318740838512,0.731561328611459,
7.18308539886771));
#276472=CARTESIAN_POINT('Ctrl Pts',(-1.78527626127104,0.794295078004447,
7.17917778262532));
#276473=CARTESIAN_POINT('Ctrl Pts',(-1.75738260768456,0.856989508534178,
7.17527261551167));
#276474=CARTESIAN_POINT('Ctrl Pts',(-1.7261625231884,0.918257689577472,
7.17136744839802));
#276475=CARTESIAN_POINT('Ctrl Pts',(-1.69179214602062,0.977729683840544,
7.16746228128437));
#276476=CARTESIAN_POINT('Ctrl Pts',(-1.65743152228059,1.03718480148352,
7.16355822235656));
#276477=CARTESIAN_POINT('Ctrl Pts',(-1.61992262656499,1.09484431853679,
7.15965416342875));
#276478=CARTESIAN_POINT('Ctrl Pts',(-1.57948722349662,1.15036346900054,
7.15575010450094));
#276479=CARTESIAN_POINT('Ctrl Pts',(-1.53904942671422,1.20588590611308,
7.15184581445881));
#276480=CARTESIAN_POINT('Ctrl Pts',(-1.49568507028046,1.25926732898709,
7.14794152441668));
#276481=CARTESIAN_POINT('Ctrl Pts',(-1.4496577901743,1.31019398998277,7.14403723437455));
#276482=CARTESIAN_POINT('Ctrl Pts',(-1.40358148368096,1.36117489598693,
7.14012878564143));
#276483=CARTESIAN_POINT('Ctrl Pts',(-1.35483692331089,1.40969545633347,
7.13622033690831));
#276484=CARTESIAN_POINT('Ctrl Pts',(-1.30372570801213,1.45547768044318,
7.13231188817518));
#276485=CARTESIAN_POINT('Ctrl Pts',(-1.25258389915257,1.50128730834772,
7.12840109996797));
#276486=CARTESIAN_POINT('Ctrl Pts',(-1.19907299929902,1.54435502949446,
7.12449031176075));
#276487=CARTESIAN_POINT('Ctrl Pts',(-1.14352669733391,1.5844439694999,7.12057952355354));
#276488=CARTESIAN_POINT('Ctrl Pts',(-1.08788448480055,1.62460213018936,
7.11666198267502));
#276489=CARTESIAN_POINT('Ctrl Pts',(-1.03020026906842,1.66177097806323,
7.1127444417965));
#276490=CARTESIAN_POINT('Ctrl Pts',(-0.970834867316236,1.69575813735422,
7.10882690091799));
#276491=CARTESIAN_POINT('Ctrl Pts',(-0.942817127424808,1.71179851374448,
7.10697800175941));
#276492=CARTESIAN_POINT('Ctrl Pts',(-0.914425244627133,1.72713088028601,
7.10512910260083));
#276493=CARTESIAN_POINT('Ctrl Pts',(-0.885698673281844,1.74173874623802,
7.10328020344225));
#276494=CARTESIAN_POINT('Ctrl Pts',(-0.824822415646611,1.77269518028322,
7.09936208665183));
#276495=CARTESIAN_POINT('Ctrl Pts',(-0.762200570830366,1.8005175691438,
7.0954439698614));
#276496=CARTESIAN_POINT('Ctrl Pts',(-0.698188685542636,1.82500645461331,
7.09152585307098));
#276497=CARTESIAN_POINT('Ctrl Pts',(-0.634273191424624,1.84945846392608,
7.0876136363077));
#276498=CARTESIAN_POINT('Ctrl Pts',(-0.568972266745221,1.8705867578287,
7.08370141954441));
#276499=CARTESIAN_POINT('Ctrl Pts',(-0.502664801874807,1.88823835808834,
7.07978920278113));
#276500=CARTESIAN_POINT('Ctrl Pts',(-0.436435310413426,1.90586920117608,
7.07588158653875));
#276501=CARTESIAN_POINT('Ctrl Pts',(-0.369202102539755,1.92003134425622,
7.07197397029636));
#276502=CARTESIAN_POINT('Ctrl Pts',(-0.301361008030636,1.93062102517267,
7.06806635405398));
#276503=CARTESIAN_POINT('Ctrl Pts',(-0.233562433452862,1.9412040689246,
7.06416118694033));
#276504=CARTESIAN_POINT('Ctrl Pts',(-0.165157212921858,1.94821901642196,
7.06025601982669));
#276505=CARTESIAN_POINT('Ctrl Pts',(-0.0965516666476493,1.95161312141202,
7.05635085271304));
#276506=CARTESIAN_POINT('Ctrl Pts',(-0.0279655888603678,1.9550062632425,
7.05244679378524));
#276507=CARTESIAN_POINT('Ctrl Pts',(0.0408202107700112,1.95478057803995,
7.04854273485744));
#276508=CARTESIAN_POINT('Ctrl Pts',(0.109395802296484,1.9509353034993,7.04463867592963));
#276509=CARTESIAN_POINT('Ctrl Pts',(0.177975453393033,1.94708980132429,
7.04073438588751));
#276510=CARTESIAN_POINT('Ctrl Pts',(0.246344380716998,1.93962431450095,
7.03683009584539));
#276511=CARTESIAN_POINT('Ctrl Pts',(0.314095993548228,1.92859008263471,
7.03292580580327));
#276512=CARTESIAN_POINT('Ctrl Pts',(0.381919772642543,1.91754409755336,
7.02901735707015));
#276513=CARTESIAN_POINT('Ctrl Pts',(0.44912443858583,1.90292186046582,7.02510890833704));
#276514=CARTESIAN_POINT('Ctrl Pts',(0.51531284099487,1.88482590068839,7.02120045960392));
#276515=CARTESIAN_POINT('Ctrl Pts',(0.581540861693244,1.86671910924039,
7.01728967139671));
#276516=CARTESIAN_POINT('Ctrl Pts',(0.646750941193973,1.84513461157647,
7.0133788831895));
#276517=CARTESIAN_POINT('Ctrl Pts',(0.710563057650473,1.82022420077924,
7.00946809498229));
#276518=CARTESIAN_POINT('Ctrl Pts',(0.774485357073851,1.7952707777279,7.00555055410378));
#276519=CARTESIAN_POINT('Ctrl Pts',(0.837004427936686,1.76698018255334,
7.00163301322526));
#276520=CARTESIAN_POINT('Ctrl Pts',(0.89776291016151,1.73555113930369,6.99771547234675));
#276521=CARTESIAN_POINT('Ctrl Pts',(0.926438119980652,1.72071807605725,
6.9958665731881));
#276522=CARTESIAN_POINT('Ctrl Pts',(0.95472157101878,1.70518659608866,6.99401767402945));
#276523=CARTESIAN_POINT('Ctrl Pts',(0.982578004880193,1.68898089519262,
6.9921687748708));
#276524=CARTESIAN_POINT('Ctrl Pts',(1.04161030024528,1.65463839009477,6.98825065808037));
#276525=CARTESIAN_POINT('Ctrl Pts',(1.0989569691907,1.61712918681125,6.98433254128995));
#276526=CARTESIAN_POINT('Ctrl Pts',(1.15425756165627,1.57664373951737,6.98041442449952));
#276527=CARTESIAN_POINT('Ctrl Pts',(1.20947488069895,1.53621925652104,6.97650220773624));
#276528=CARTESIAN_POINT('Ctrl Pts',(1.26265184435615,1.4928277123745,6.97258999097296));
#276529=CARTESIAN_POINT('Ctrl Pts',(1.31345438206221,1.44670438799417,6.96867777420967));
#276530=CARTESIAN_POINT('Ctrl Pts',(1.36419717917855,1.40063530174292,6.96477015796729));
#276531=CARTESIAN_POINT('Ctrl Pts',(1.4125707331932,1.35184114420746,6.96086254172491));
#276532=CARTESIAN_POINT('Ctrl Pts',(1.45827312602572,1.30059812775168,6.95695492548252));
#276533=CARTESIAN_POINT('Ctrl Pts',(1.50394687452962,1.24938722825329,6.95304975836888));
#276534=CARTESIAN_POINT('Ctrl Pts',(1.54695245621044,1.19573088073896,6.94914459125524));
#276535=CARTESIAN_POINT('Ctrl Pts',(1.5870251162277,1.13994178819028,6.9452394241416));
#276536=CARTESIAN_POINT('Ctrl Pts',(1.62708640465622,1.08416852714908,6.9413353652138));
#276537=CARTESIAN_POINT('Ctrl Pts',(1.66421613683263,1.02626412184942,6.93743130628599));
#276538=CARTESIAN_POINT('Ctrl Pts',(1.69819126741979,0.966572511123276,
6.93352724735819));
#276539=CARTESIAN_POINT('Ctrl Pts',(1.7321684092827,0.906877366745105,6.92962295731607));
#276540=CARTESIAN_POINT('Ctrl Pts',(1.76299033771203,0.845395235643157,
6.92571866727396));
#276541=CARTESIAN_POINT('Ctrl Pts',(1.79047950208093,0.78249546492489,6.92181437723184));
#276542=CARTESIAN_POINT('Ctrl Pts',(1.81799794678996,0.71952869592848,6.91790592849873));
#276543=CARTESIAN_POINT('Ctrl Pts',(1.84217634553217,0.65514172538121,6.91399747976561));
#276544=CARTESIAN_POINT('Ctrl Pts',(1.86288535424368,0.589723797166438,
6.91008903103249));
#276545=CARTESIAN_POINT('Ctrl Pts',(1.8836067587144,0.524266711843878,6.90617824282529));
#276546=CARTESIAN_POINT('Ctrl Pts',(1.90085451667714,0.457777916899523,
6.90226745461808));
#276547=CARTESIAN_POINT('Ctrl Pts',(1.91454995996751,0.390658995529884,
6.89835666641087));
#276548=CARTESIAN_POINT('Ctrl Pts',(1.9282690508762,0.323424181406629,6.89443912553236));
#276549=CARTESIAN_POINT('Ctrl Pts',(1.93842351247812,0.255557555540475,
6.89052158465385));
#276550=CARTESIAN_POINT('Ctrl Pts',(1.94498639491301,0.187467126727044,
6.88660404377534));
#276551=CARTESIAN_POINT('Ctrl Pts',(1.94808377364842,0.155331575254947,
6.88475514461669));
#276552=CARTESIAN_POINT('Ctrl Pts',(1.95038191682708,0.123146190208738,
6.88290624545804));
#276553=CARTESIAN_POINT('Ctrl Pts',(1.95188202035471,0.0909537168894154,
6.88105734629938));
#276554=CARTESIAN_POINT('Ctrl Pts',(1.95506098270725,0.022732651588192,
6.87713922950896));
#276555=CARTESIAN_POINT('Ctrl Pts',(1.95466530531591,-0.0457905139071906,
6.87322111271853));
#276556=CARTESIAN_POINT('Ctrl Pts',(1.9506594149489,-0.114209661899562,
6.86930299592811));
#276557=CARTESIAN_POINT('Ctrl Pts',(1.94665955678132,-0.182525782123295,
6.86539077916482));
#276558=CARTESIAN_POINT('Ctrl Pts',(1.93906030343754,-0.250737708615958,
6.86147856240154));
#276559=CARTESIAN_POINT('Ctrl Pts',(1.92787804941269,-0.31843716270677,
6.85756634563826));
#276560=CARTESIAN_POINT('Ctrl Pts',(1.91670894501538,-0.386057006496763,
6.85365872939587));
#276561=CARTESIAN_POINT('Ctrl Pts',(1.90196528756213,-0.453165091721353,
6.84975111315348));
#276562=CARTESIAN_POINT('Ctrl Pts',(1.88371529922209,-0.519357941574634,
6.8458434969111));
#276563=CARTESIAN_POINT('Ctrl Pts',(1.86547674920357,-0.585509304546669,
6.84193832979745));
#276564=CARTESIAN_POINT('Ctrl Pts',(1.84373635812278,-0.650746096925991,
6.83803316268381));
#276565=CARTESIAN_POINT('Ctrl Pts',(1.81861316395814,-0.71467626228816,
6.83412799557017));
#276566=CARTESIAN_POINT('Ctrl Pts',(1.79349709910888,-0.778588285916091,
6.83022393664236));
#276567=CARTESIAN_POINT('Ctrl Pts',(1.76500031666709,-0.84119396101884,
6.82631987771455));
#276568=CARTESIAN_POINT('Ctrl Pts',(1.7332907228189,-0.902119321481338,
6.82241581878675));
#276569=CARTESIAN_POINT('Ctrl Pts',(1.70157925181126,-0.963048288631953,
6.81851152874463));
#276570=CARTESIAN_POINT('Ctrl Pts',(1.66665482116111,-1.02229630852045,
6.81460723870251));
#276571=CARTESIAN_POINT('Ctrl Pts',(1.62873136358012,-1.07951384673401,
6.81070294866039));
#276572=CARTESIAN_POINT('Ctrl Pts',(1.59076751147415,-1.13679233074269,
6.80679449992727));
#276573=CARTESIAN_POINT('Ctrl Pts',(1.54979852958826,-1.19203560603691,
6.80288605119415));
#276574=CARTESIAN_POINT('Ctrl Pts',(1.50608121864768,-1.24492383816711,
6.79897760246103));
#276575=CARTESIAN_POINT('Ctrl Pts',(1.46233773990412,-1.29784372752434,
6.79506681425382));
#276576=CARTESIAN_POINT('Ctrl Pts',(1.41584299111794,-1.34840540612791,
6.79115602604661));
#276577=CARTESIAN_POINT('Ctrl Pts',(1.36689163227498,-1.39632491405712,
6.7872452378394));
#276578=CARTESIAN_POINT('Ctrl Pts',(1.31785575020588,-1.44432716353839,
6.78332769696088));
#276579=CARTESIAN_POINT('Ctrl Pts',(1.26635516113751,-1.48967781207289,
6.77941015608237));
#276580=CARTESIAN_POINT('Ctrl Pts',(1.21271798218434,-1.53213285836664,
6.77549261520385));
#276581=CARTESIAN_POINT('Ctrl Pts',(1.18740370005856,-1.55216968805304,
6.77364371604522));
#276582=CARTESIAN_POINT('Ctrl Pts',(1.16161393600949,-1.57156217481763,
6.77179481688659));
#276583=CARTESIAN_POINT('Ctrl Pts',(1.13538524609547,-1.59028813205304,
6.76994591772795));
#276584=CARTESIAN_POINT('Ctrl Pts',(1.07980240380627,-1.62997146854989,
6.76602780093753));
#276585=CARTESIAN_POINT('Ctrl Pts',(1.02202639017435,-1.66681591207812,
6.7621096841471));
#276586=CARTESIAN_POINT('Ctrl Pts',(0.962379055182175,-1.70057124347869,
6.75819156735668));
#276587=CARTESIAN_POINT('Ctrl Pts',(0.902821539078585,-1.73427574500814,
6.7542793505934));
#276588=CARTESIAN_POINT('Ctrl Pts',(0.841398718781946,-1.76490012604718,
6.75036713383011));
#276589=CARTESIAN_POINT('Ctrl Pts',(0.77846245432362,-1.7922366493319,6.74645491706683));
#276590=CARTESIAN_POINT('Ctrl Pts',(0.715600198954619,-1.81954102658427,
6.74254730082445));
#276591=CARTESIAN_POINT('Ctrl Pts',(0.651228482988933,-1.84356502960705,
6.73863968458206));
#276592=CARTESIAN_POINT('Ctrl Pts',(0.585723251546375,-1.86414706302854,
6.73473206833968));
#276593=CARTESIAN_POINT('Ctrl Pts',(0.520259076014899,-1.8847161965012,
6.73082690122604));
#276594=CARTESIAN_POINT('Ctrl Pts',(0.45366326250104,-1.90184749262005,
6.72692173411239));
#276595=CARTESIAN_POINT('Ctrl Pts',(0.38632973249629,-1.91542823874698,
6.72301656699875));
#276596=CARTESIAN_POINT('Ctrl Pts',(0.319015310012996,-1.92900513100796,
6.71911250807095));
#276597=CARTESIAN_POINT('Ctrl Pts',(0.250964068568436,-1.93903337624113,
6.71520844914314));
#276598=CARTESIAN_POINT('Ctrl Pts',(0.182581246443851,-1.94545112723168,
6.71130439021534));
#276599=CARTESIAN_POINT('Ctrl Pts',(0.114194376160842,-1.95186925814327,
6.70740010017322));
#276600=CARTESIAN_POINT('Ctrl Pts',(0.0454763761929554,-1.95467642706471,
6.7034958101311));
#276601=CARTESIAN_POINT('Ctrl Pts',(-0.0231630670702663,-1.95386270559727,
6.69959152008898));
#276602=CARTESIAN_POINT('Ctrl Pts',(-0.0918756222774577,-1.95304811738682,
6.69568307135586));
#276603=CARTESIAN_POINT('Ctrl Pts',(-0.160508961000291,-1.94860494760029,
6.69177462262275));
#276604=CARTESIAN_POINT('Ctrl Pts',(-0.228655087856236,-1.94057539168089,
6.68786617388963));
#276605=CARTESIAN_POINT('Ctrl Pts',(-0.296842004833592,-1.93254102952267,
6.68395538568242));
#276606=CARTESIAN_POINT('Ctrl Pts',(-0.364540644696712,-1.92091609216458,
6.68004459747521));
#276607=CARTESIAN_POINT('Ctrl Pts',(-0.431352607342982,-1.90579404137446,
6.676133809268));
#276608=CARTESIAN_POINT('Ctrl Pts',(-0.498279932724058,-1.89064587967447,
6.67221626838949));
#276609=CARTESIAN_POINT('Ctrl Pts',(-0.564317052146925,-1.87198868655183,
6.66829872751097));
#276610=CARTESIAN_POINT('Ctrl Pts',(-0.629080979892976,-1.84996570798945,
6.66438118663246));
#276611=CARTESIAN_POINT('Ctrl Pts',(-0.65964657582003,-1.83957187476661,
6.66253228747381));
#276612=CARTESIAN_POINT('Ctrl Pts',(-0.689928875796084,-1.8284290393646,
6.66068338831517));
#276613=CARTESIAN_POINT('Ctrl Pts',(-0.71988940919612,-1.81655587266873,
6.65883448915652));
#276614=CARTESIAN_POINT('Ctrl Pts',(-0.783380632292711,-1.79139470929808,
6.6549163723661));
#276615=CARTESIAN_POINT('Ctrl Pts',(-0.845676998981992,-1.76285099777674,
6.65099825557567));
#276616=CARTESIAN_POINT('Ctrl Pts',(-0.906393700561943,-1.73105934605999,
6.64708013878525));
#276617=CARTESIAN_POINT('Ctrl Pts',(-0.967018972966463,-1.6993155672419,
6.64316792202197));
#276618=CARTESIAN_POINT('Ctrl Pts',(-1.02606886890676,-1.66433378117181,
6.63925570525869));
#276619=CARTESIAN_POINT('Ctrl Pts',(-1.0831779838716,-1.62629685336222,
6.63534348849541));
#276620=CARTESIAN_POINT('Ctrl Pts',(-1.14021994210852,-1.5883046545878,
6.63143587225302));
#276621=CARTESIAN_POINT('Ctrl Pts',(-1.19532524447755,-1.54726472051837,
6.62752825601064));
#276622=CARTESIAN_POINT('Ctrl Pts',(-1.2481541797073,-1.50340518280309,
6.62362063976826));
#276623=CARTESIAN_POINT('Ctrl Pts',(-1.30095000399279,-1.45957313439273,
6.61971547265461));
#276624=CARTESIAN_POINT('Ctrl Pts',(-1.35147191371725,-1.412925301409,6.61581030554097));
#276625=CARTESIAN_POINT('Ctrl Pts',(-1.39941150747801,-1.36373143717454,
6.61190513842733));
#276626=CARTESIAN_POINT('Ctrl Pts',(-1.44733749721686,-1.31455153289164,
6.60800107949952));
#276627=CARTESIAN_POINT('Ctrl Pts',(-1.49268228258494,-1.26282738374907,
6.60409702057172));
#276628=CARTESIAN_POINT('Ctrl Pts',(-1.53517405067746,-1.20886584620733,
6.60019296164392));
#276629=CARTESIAN_POINT('Ctrl Pts',(-1.57766833421764,-1.15490111422513,
6.5962886716018));
#276630=CARTESIAN_POINT('Ctrl Pts',(-1.61730896287684,-1.09869911891853,
6.59238438155968));
#276631=CARTESIAN_POINT('Ctrl Pts',(-1.65386532368805,-1.04059862151659,
6.58848009151756));
#276632=CARTESIAN_POINT('Ctrl Pts',(-1.69046062284836,-0.982436237827272,
6.58457164278445));
#276633=CARTESIAN_POINT('Ctrl Pts',(-1.72396483539274,-0.922371733469224,
6.58066319405133));
#276634=CARTESIAN_POINT('Ctrl Pts',(-1.75419205125869,-0.860770728650109,
6.57675474531821));
#276635=CARTESIAN_POINT('Ctrl Pts',(-1.78443736018233,-0.799132851413129,
6.572843957111));
#276636=CARTESIAN_POINT('Ctrl Pts',(-1.81140157555279,-0.7359570957995,
6.56893316890379));
#276637=CARTESIAN_POINT('Ctrl Pts',(-1.83494705828878,-0.671628835948359,
6.56502238069658));
#276638=CARTESIAN_POINT('Ctrl Pts',(-1.85853319648786,-0.607189501916973,
6.56110483981807));
#276639=CARTESIAN_POINT('Ctrl Pts',(-1.87868867611599,-0.541594161854998,
6.55718729893955));
#276640=CARTESIAN_POINT('Ctrl Pts',(-1.89532604117965,-0.475242251516302,
6.55326975806104));
#276641=CARTESIAN_POINT('Ctrl Pts',(-1.90317811247189,-0.443927200823934,
6.55142085890239));
#276642=CARTESIAN_POINT('Ctrl Pts',(-1.91024730087751,-0.412443759971224,
6.54957195974374));
#276643=CARTESIAN_POINT('Ctrl Pts',(-1.91652841845126,-0.380834375114328,
6.54772306058509));
#276644=CARTESIAN_POINT('Ctrl Pts',(-1.93574599944975,-0.284122936955839,
6.54206620590562));
#276645=CARTESIAN_POINT('Ctrl Pts',(-1.94764796351427,-0.185913139877314,
6.53640935122614));
#276646=CARTESIAN_POINT('Ctrl Pts',(-1.95205706279423,-0.0871161500250206,
6.53075249654666));
#276647=CARTESIAN_POINT('Ctrl Pts',(-1.9533256576043,-0.0586900836973724,
6.52912489507252));
#276648=CARTESIAN_POINT('Ctrl Pts',(-1.95397423542428,-0.0302155762360542,
6.52749729359838));
#276649=CARTESIAN_POINT('Ctrl Pts',(-1.95399924754167,-0.00171481969227626,
6.52586969212423));
#276650=CARTESIAN_POINT('',(-1.95079791861852,-3.56937016110504E-5,5.82586969212423));
#276651=CARTESIAN_POINT('Ctrl Pts',(-1.95471132575424,-0.00170873845395426,
6.52586930929363));
#276652=CARTESIAN_POINT('Ctrl Pts',(-1.94992942299147,0.519479667493671,
6.49611675020031));
#276653=CARTESIAN_POINT('Ctrl Pts',(-1.4674451005583,1.69727522902121,6.42932704824985));
#276654=CARTESIAN_POINT('Ctrl Pts',(0.521340871742519,2.24972451098197,
6.32550020344223));
#276655=CARTESIAN_POINT('Ctrl Pts',(2.17268068147358,0.782633590011064,
6.21438877487081));
#276656=CARTESIAN_POINT('Ctrl Pts',(1.83620829950793,-1.40049839724295,
6.10327734629938));
#276657=CARTESIAN_POINT('Ctrl Pts',(-0.180233566874121,-2.3022972312962,
5.99216591772794));
#276658=CARTESIAN_POINT('Ctrl Pts',(-1.72112656933261,-1.29980337605498,
5.89969669966956));
#276659=CARTESIAN_POINT('Ctrl Pts',(-1.95085071127348,-0.323906799394953,
5.84426462446833));
#276660=CARTESIAN_POINT('Ctrl Pts',(-1.95079791861852,-3.56937016110504E-5,
5.82586969212423));
#276661=CARTESIAN_POINT('',(-1.9539992304742,0.00173415865262049,5.12586969212423));
#276662=CARTESIAN_POINT('Ctrl Pts',(-1.95079791861852,-3.56937016110504E-5,
5.82586969212423));
#276663=CARTESIAN_POINT('Ctrl Pts',(-1.95074441628598,0.328189124878196,
5.80722748161118));
#276664=CARTESIAN_POINT('Ctrl Pts',(-1.71657185386281,1.30858158663414,
5.75154812824101));
#276665=CARTESIAN_POINT('Ctrl Pts',(-0.164899398794644,2.30344630242157,
5.65883163201366));
#276666=CARTESIAN_POINT('Ctrl Pts',(1.84549300971326,1.3882406963353,5.54772020344223));
#276667=CARTESIAN_POINT('Ctrl Pts',(2.167421238611,-0.797083342116639,5.43660877487082));
#276668=CARTESIAN_POINT('Ctrl Pts',(0.506349204565716,-2.25314605893584,
5.32549734629937));
#276669=CARTESIAN_POINT('Ctrl Pts',(-1.47398685042411,-1.68881353075032,
5.22191775663669));
#276670=CARTESIAN_POINT('Ctrl Pts',(-1.94982006439799,-0.51521705165863,
5.15537530983116));
#276671=CARTESIAN_POINT('Ctrl Pts',(-1.95458041427723,0.00172917730281742,
5.12587000588275));
#276672=CARTESIAN_POINT('',(-1.95399970505248,-0.00107361763076356,4.42586969212423));
#276673=CARTESIAN_POINT('Ctrl Pts',(-1.9539992304742,0.00173415865262049,
5.12586969212423));
#276674=CARTESIAN_POINT('Ctrl Pts',(-1.9539127601795,0.0991663567078893,
5.12030693244776));
#276675=CARTESIAN_POINT('Ctrl Pts',(-1.94653542196257,0.196286002198207,
5.11474417277129));
#276676=CARTESIAN_POINT('Ctrl Pts',(-1.93202691376388,0.292212259311616,
5.10918141309482));
#276677=CARTESIAN_POINT('Ctrl Pts',(-1.92689153376234,0.326165976375911,
5.10721243844872));
#276678=CARTESIAN_POINT('Ctrl Pts',(-1.92086312817625,0.359970460063155,
5.10524346380262));
#276679=CARTESIAN_POINT('Ctrl Pts',(-1.91395009125867,0.393587408552323,
5.10327448915652));
#276680=CARTESIAN_POINT('Ctrl Pts',(-1.9001936490042,0.460482698737512,
5.0993563723661));
#276681=CARTESIAN_POINT('Ctrl Pts',(-1.88289858598141,0.52678851722377,
5.09543825557568));
#276682=CARTESIAN_POINT('Ctrl Pts',(-1.86213065986891,0.592102529614751,
5.09152013878526));
#276683=CARTESIAN_POINT('Ctrl Pts',(-1.84139400677205,0.657318190050875,
5.08760792202197));
#276684=CARTESIAN_POINT('Ctrl Pts',(-1.81719501724086,0.721544543465094,
5.08369570525869));
#276685=CARTESIAN_POINT('Ctrl Pts',(-1.78965034244472,0.784389987052042,
5.07978348849541));
#276686=CARTESIAN_POINT('Ctrl Pts',(-1.76213805845403,0.847161528349269,
5.07587587225303));
#276687=CARTESIAN_POINT('Ctrl Pts',(-1.73128809932901,0.908554936461109,
5.07196825601064));
#276688=CARTESIAN_POINT('Ctrl Pts',(-1.69726615556976,0.968196053058186,
5.06806063976826));
#276689=CARTESIAN_POINT('Ctrl Pts',(-1.66326553532723,1.02779978912358,
5.06415547265462));
#276690=CARTESIAN_POINT('Ctrl Pts',(-1.6260971173185,1.08565298598435,5.06025030554098));
#276691=CARTESIAN_POINT('Ctrl Pts',(-1.58597301735029,1.1414050938369,5.05634513842733));
#276692=CARTESIAN_POINT('Ctrl Pts',(-1.54586030356815,1.19714138067728,
5.05244107949953));
#276693=CARTESIAN_POINT('Ctrl Pts',(-1.50279386007308,1.25077736308912,
5.04853702057173));
#276694=CARTESIAN_POINT('Ctrl Pts',(-1.45702869447512,1.30199208272406,
5.04463296164393));
#276695=CARTESIAN_POINT('Ctrl Pts',(-1.41126081964942,1.353209834192,5.04072867160181));
#276696=CARTESIAN_POINT('Ctrl Pts',(-1.36279423520233,1.40200567324579,
5.0368243815597));
#276697=CARTESIAN_POINT('Ctrl Pts',(-1.31192252170383,1.44809367688913,
5.03292009151758));
#276698=CARTESIAN_POINT('Ctrl Pts',(-1.2609966217246,1.49423077159996,5.02901164278447));
#276699=CARTESIAN_POINT('Ctrl Pts',(-1.20766084527101,1.53765394389409,
5.02510319405135));
#276700=CARTESIAN_POINT('Ctrl Pts',(-1.15224298485108,1.57811663189432,
5.02119474531824));
#276701=CARTESIAN_POINT('Ctrl Pts',(-1.09679195304843,1.61860353958292,
5.01728395711103));
#276702=CARTESIAN_POINT('Ctrl Pts',(-1.03925676903407,1.65612616753363,
5.01337316890382));
#276703=CARTESIAN_POINT('Ctrl Pts',(-0.979993059549189,1.69048206238204,
5.00946238069661));
#276704=CARTESIAN_POINT('Ctrl Pts',(-0.920627020730927,1.72489727879246,
5.0055448398181));
#276705=CARTESIAN_POINT('Ctrl Pts',(-0.859526937376322,1.75613462520569,
5.00162729893959));
#276706=CARTESIAN_POINT('Ctrl Pts',(-0.797070996541357,1.78403862807748,
4.99770975806108));
#276707=CARTESIAN_POINT('Ctrl Pts',(-0.767594664310405,1.79720803435375,
4.99586085890241));
#276708=CARTESIAN_POINT('Ctrl Pts',(-0.737816583548416,1.80963568009972,
4.99401195974375));
#276709=CARTESIAN_POINT('Ctrl Pts',(-0.707777655179647,1.82130908712069,
4.99216306058509));
#276710=CARTESIAN_POINT('Ctrl Pts',(-0.644120300446923,1.8460469273842,
4.98824494379466));
#276711=CARTESIAN_POINT('Ctrl Pts',(-0.57903826112679,1.86749241474253,
4.98432682700424));
#276712=CARTESIAN_POINT('Ctrl Pts',(-0.512905185589397,1.88548250339151,
4.98040871021381));
#276713=CARTESIAN_POINT('Ctrl Pts',(-0.446871695378696,1.90344550198243,
4.97649649345053));
#276714=CARTESIAN_POINT('Ctrl Pts',(-0.379790780832813,1.91796330040063,
4.97258427668724));
#276715=CARTESIAN_POINT('Ctrl Pts',(-0.312054687442142,1.92892142713108,
4.96867205992396));
#276716=CARTESIAN_POINT('Ctrl Pts',(-0.244398247437811,1.93986666779357,
4.96476444368157));
#276717=CARTESIAN_POINT('Ctrl Pts',(-0.176088641980505,1.94726047194811,
4.96085682743919));
#276718=CARTESIAN_POINT('Ctrl Pts',(-0.107530068709893,1.95103902685806,
4.9569492111968));
#276719=CARTESIAN_POINT('Ctrl Pts',(-0.0390144650559959,1.95481521352946,
4.95304404408316));
#276720=CARTESIAN_POINT('Ctrl Pts',(0.029749306840273,1.95498061874556,
4.94913887696951));
#276721=CARTESIAN_POINT('Ctrl Pts',(0.0983516933838985,1.95152323696351,
4.94523370985587));
#276722=CARTESIAN_POINT('Ctrl Pts',(0.166934612337252,1.94806683629734,
4.94132965092806));
#276723=CARTESIAN_POINT('Ctrl Pts',(0.235355745827034,1.94098971424263,
4.93742559200026));
#276724=CARTESIAN_POINT('Ctrl Pts',(0.303207127208492,1.93033195021218,
4.93352153307245));
#276725=CARTESIAN_POINT('Ctrl Pts',(0.371062525287945,1.91967355525841,
4.92961724303033));
#276726=CARTESIAN_POINT('Ctrl Pts',(0.438347618774167,1.90543417635696,
4.92571295298821));
#276727=CARTESIAN_POINT('Ctrl Pts',(0.504662944157557,1.88770530348204,
4.92180866294609));
#276728=CARTESIAN_POINT('Ctrl Pts',(0.571048905929022,1.86995754653263,
4.91790021421297));
#276729=CARTESIAN_POINT('Ctrl Pts',(0.636462562030419,1.84871300517614,
4.91399176547985));
#276730=CARTESIAN_POINT('Ctrl Pts',(0.700518951896146,1.82411326348841,
4.91008331674673));
#276731=CARTESIAN_POINT('Ctrl Pts',(0.764613683895754,1.79949879717146,
4.90617252853952));
#276732=CARTESIAN_POINT('Ctrl Pts',(0.827349083496318,1.77152533394545,
4.90226174033231));
#276733=CARTESIAN_POINT('Ctrl Pts',(0.888362141202018,1.74038177020991,
4.8983509521251));
#276734=CARTESIAN_POINT('Ctrl Pts',(0.949480548801892,1.70918443157326,
4.89443341124659));
#276735=CARTESIAN_POINT('Ctrl Pts',(1.00887025354459,1.67480631400611,4.89051587036808));
#276736=CARTESIAN_POINT('Ctrl Pts',(1.06619547031322,1.63748075380555,4.88659832948956));
#276737=CARTESIAN_POINT('Ctrl Pts',(1.0932503367049,1.61986480569153,4.88474943033093));
#276738=CARTESIAN_POINT('Ctrl Pts',(1.11984581569148,1.60159294289382,4.88290053117229));
#276739=CARTESIAN_POINT('Ctrl Pts',(1.1459492347009,1.58269275334426,4.88105163201366));
#276740=CARTESIAN_POINT('Ctrl Pts',(1.20126660765259,1.54264019035267,4.87713351522323));
#276741=CARTESIAN_POINT('Ctrl Pts',(1.25459126761568,1.49960460728557,4.87321539843281));
#276742=CARTESIAN_POINT('Ctrl Pts',(1.3055835310031,1.45381141953607,4.86929728164238));
#276743=CARTESIAN_POINT('Ctrl Pts',(1.35649900858906,1.40808718865157,4.86538506487909));
#276744=CARTESIAN_POINT('Ctrl Pts',(1.40508869704579,1.35961392031835,4.86147284811581));
#276745=CARTESIAN_POINT('Ctrl Pts',(1.45104362676979,1.30865900570422,4.85756063135253));
#276746=CARTESIAN_POINT('Ctrl Pts',(1.49694451638626,1.25776401086545,4.85365301511014));
#276747=CARTESIAN_POINT('Ctrl Pts',(1.54021647269384,1.2043935289965,4.84974539886775));
#276748=CARTESIAN_POINT('Ctrl Pts',(1.58058659628917,1.14885247600856,4.84583778262537));
#276749=CARTESIAN_POINT('Ctrl Pts',(1.62093141759691,1.0933462338057,4.84193261551172));
#276750=CARTESIAN_POINT('Ctrl Pts',(1.6583777254558,1.0356725161171,4.83802744839808));
#276751=CARTESIAN_POINT('Ctrl Pts',(1.69269323408757,0.976168845678951,
4.83412228128443));
#276752=CARTESIAN_POINT('Ctrl Pts',(1.72699900486188,0.916682060849792,
4.83021822235663));
#276753=CARTESIAN_POINT('Ctrl Pts',(1.75817549450015,0.8553667800591,4.82631416342882));
#276754=CARTESIAN_POINT('Ctrl Pts',(1.78603503100773,0.792587451334697,
4.82241010450102));
#276755=CARTESIAN_POINT('Ctrl Pts',(1.81389621675724,0.729804406170085,
4.81850581445889));
#276756=CARTESIAN_POINT('Ctrl Pts',(1.83843986236296,0.665557591639494,
4.81460152441677));
#276757=CARTESIAN_POINT('Ctrl Pts',(1.85952609543786,0.600232205388584,
4.81069723437465));
#276758=CARTESIAN_POINT('Ctrl Pts',(1.88063478871081,0.534837237192506,
4.80678878564153));
#276759=CARTESIAN_POINT('Ctrl Pts',(1.8982785685469,0.468361873522238,4.80288033690841));
#276760=CARTESIAN_POINT('Ctrl Pts',(1.91236751146388,0.401206307399874,
4.79897188817529));
#276761=CARTESIAN_POINT('Ctrl Pts',(1.92646488757756,0.334010544074505,
4.79506109996808));
#276762=CARTESIAN_POINT('Ctrl Pts',(1.93700311655821,0.266134254121011,
4.79115031176087));
#276763=CARTESIAN_POINT('Ctrl Pts',(1.94394392799346,0.197984860071106,
4.78723952355366));
#276764=CARTESIAN_POINT('Ctrl Pts',(1.95089672397394,0.129717793973247,
4.78332198267515));
#276765=CARTESIAN_POINT('Ctrl Pts',(1.95423968114099,0.0611771736502074,
4.77940444179663));
#276766=CARTESIAN_POINT('Ctrl Pts',(1.95398663023682,-0.00722833699840476,
4.77548690091812));
#276767=CARTESIAN_POINT('Ctrl Pts',(1.95386720184582,-0.0395125926082593,
4.77363800175949));
#276768=CARTESIAN_POINT('Ctrl Pts',(1.95294754928242,-0.0717668126698533,
4.77178910260086));
#276769=CARTESIAN_POINT('Ctrl Pts',(1.95123312086349,-0.103948583661862,
4.76994020344222));
#276770=CARTESIAN_POINT('Ctrl Pts',(1.94759996935126,-0.172146968998725,
4.7660220866518));
#276771=CARTESIAN_POINT('Ctrl Pts',(1.94037986481757,-0.240289839943688,
4.76210396986138));
#276772=CARTESIAN_POINT('Ctrl Pts',(1.92957786913664,-0.307969555213016,
4.75818585307095));
#276773=CARTESIAN_POINT('Ctrl Pts',(1.9187921394506,-0.375547356175459,
4.75427363630767));
#276774=CARTESIAN_POINT('Ctrl Pts',(1.90443530015851,-0.442662903798645,
4.75036141954439));
#276775=CARTESIAN_POINT('Ctrl Pts',(1.88656433762187,-0.508911583689494,
4.7464492027811));
#276776=CARTESIAN_POINT('Ctrl Pts',(1.86871439021339,-0.575082359298746,
4.74254158653872));
#276777=CARTESIAN_POINT('Ctrl Pts',(1.84735865404818,-0.640387819027977,
4.73863397029634));
#276778=CARTESIAN_POINT('Ctrl Pts',(1.82260520696893,-0.704433289623483,
4.73472635405396));
#276779=CARTESIAN_POINT('Ctrl Pts',(1.79786727430432,-0.768438619224335,
4.73082118694031));
#276780=CARTESIAN_POINT('Ctrl Pts',(1.76973603198864,-0.831185068447074,
4.72691601982667));
#276781=CARTESIAN_POINT('Ctrl Pts',(1.73836898316663,-0.892294389965669,
4.72301085271303));
#276782=CARTESIAN_POINT('Ctrl Pts',(1.70701083550515,-0.953386370232826,
4.71910679378522));
#276783=CARTESIAN_POINT('Ctrl Pts',(1.6724189287103,-1.01284170766265,4.71520273485742));
#276784=CARTESIAN_POINT('Ctrl Pts',(1.63479758884621,-1.07030502358095,
4.71129867592962));
#276785=CARTESIAN_POINT('Ctrl Pts',(1.59717402185634,-1.12777174123966,
4.7073943858875));
#276786=CARTESIAN_POINT('Ctrl Pts',(1.55652093732143,-1.18324579314449,
4.70349009584538));
#276787=CARTESIAN_POINT('Ctrl Pts',(1.51308602493867,-1.2364006960267,4.69958580580326));
#276788=CARTESIAN_POINT('Ctrl Pts',(1.46960484745339,-1.28961221735006,
4.69567735707014));
#276789=CARTESIAN_POINT('Ctrl Pts',(1.42333624054634,-1.34049927815017,
4.69176890833703));
#276790=CARTESIAN_POINT('Ctrl Pts',(1.37456758991495,-1.38876921796079,
4.68786045960391));
#276791=CARTESIAN_POINT('Ctrl Pts',(1.32576974790802,-1.43706805063437,
4.6839496713967));
#276792=CARTESIAN_POINT('Ctrl Pts',(1.27446925137984,-1.48274631750008,
4.68003888318949));
#276793=CARTESIAN_POINT('Ctrl Pts',(1.22098758307095,-1.52555082576313,
4.67612809498229));
#276794=CARTESIAN_POINT('Ctrl Pts',(1.16741356915097,-1.5684292436217,4.67221055410378));
#276795=CARTESIAN_POINT('Ctrl Pts',(1.11165126624692,-1.60842371288584,
4.66829301322526));
#276796=CARTESIAN_POINT('Ctrl Pts',(1.05405146704452,-1.64532413366524,
4.66437547234675));
#276797=CARTESIAN_POINT('Ctrl Pts',(1.02686701036971,-1.66273943552134,
4.6625265731881));
#276798=CARTESIAN_POINT('Ctrl Pts',(0.999273627660957,-1.67946623148854,
4.66067767402945));
#276799=CARTESIAN_POINT('Ctrl Pts',(0.971309903392171,-1.69548608710667,
4.6588287748708));
#276800=CARTESIAN_POINT('Ctrl Pts',(0.912050242275597,-1.72943475595857,
4.65491065808038));
#276801=CARTESIAN_POINT('Ctrl Pts',(0.850891135398688,-1.7603401667489,
4.65099254128995));
#276802=CARTESIAN_POINT('Ctrl Pts',(0.788177758926153,-1.78798540831131,
4.64707442449953));
#276803=CARTESIAN_POINT('Ctrl Pts',(0.725558818286718,-1.81558902077374,
4.64316220773625));
#276804=CARTESIAN_POINT('Ctrl Pts',(0.661390699523402,-1.83994201035609,
4.63924999097297));
#276805=CARTESIAN_POINT('Ctrl Pts',(0.596044207441925,-1.86087272610862,
4.63533777420968));
#276806=CARTESIAN_POINT('Ctrl Pts',(0.530774558725907,-1.88177882865563,
4.6314301579673));
#276807=CARTESIAN_POINT('Ctrl Pts',(0.464329754918427,-1.89927050051948,
4.62752254172491));
#276808=CARTESIAN_POINT('Ctrl Pts',(0.397099969364987,-1.91322440250231,
4.62361492548253));
#276809=CARTESIAN_POINT('Ctrl Pts',(0.329912320600278,-1.92716955876902,
4.61970975836889));
#276810=CARTESIAN_POINT('Ctrl Pts',(0.261941146582688,-1.93758124388507,
4.61580459125524));
#276811=CARTESIAN_POINT('Ctrl Pts',(0.193589637821925,-1.94438654905036,
4.6118994241416));
#276812=CARTESIAN_POINT('Ctrl Pts',(0.125257525458772,-1.95118992304534,
4.6079953652138));
#276813=CARTESIAN_POINT('Ctrl Pts',(0.0565457818406509,-1.95438890000059,
4.60409130628599));
#276814=CARTESIAN_POINT('Ctrl Pts',(-0.0121362093305447,-1.95396231090139,
4.60018724735819));
#276815=CARTESIAN_POINT('Ctrl Pts',(-0.0808222663705408,-1.95353569654876,
4.59628295731607));
#276816=CARTESIAN_POINT('Ctrl Pts',(-0.149478075614179,-1.94948309564992,
4.59237866727395));
#276817=CARTESIAN_POINT('Ctrl Pts',(-0.217694999620562,-1.94183544285817,
4.58847437723183));
#276818=CARTESIAN_POINT('Ctrl Pts',(-0.285984585520565,-1.93417964409764,
4.58456592849871));
#276819=CARTESIAN_POINT('Ctrl Pts',(-0.353833863476488,-1.92292120624612,
4.58065747976559));
#276820=CARTESIAN_POINT('Ctrl Pts',(-0.420841071309029,-1.90814276004168,
4.57674903103248));
#276821=CARTESIAN_POINT('Ctrl Pts',(-0.487888387541988,-1.89335546792562,
4.57283824282527));
#276822=CARTESIAN_POINT('Ctrl Pts',(-0.554092156381364,-1.87504410535043,
4.56892745461806));
#276823=CARTESIAN_POINT('Ctrl Pts',(-0.619065270434279,-1.85334135845023,
4.56501666641085));
#276824=CARTESIAN_POINT('Ctrl Pts',(-0.684150572122884,-1.83160113789806,
4.56109912553233));
#276825=CARTESIAN_POINT('Ctrl Pts',(-0.748000520547101,-1.80645802585699,
4.55718158465382));
#276826=CARTESIAN_POINT('Ctrl Pts',(-0.810248305606452,-1.77809270941137,
4.55326404377531));
#276827=CARTESIAN_POINT('Ctrl Pts',(-0.839626397882392,-1.76470558434048,
4.55141514461666));
#276828=CARTESIAN_POINT('Ctrl Pts',(-0.868647986612071,-1.75060140551863,
4.54956624545802));
#276829=CARTESIAN_POINT('Ctrl Pts',(-0.897276652572764,-1.73580258346041,
4.54771734629938));
#276830=CARTESIAN_POINT('Ctrl Pts',(-0.957945432837846,-1.7044414824973,
4.54379922950895));
#276831=CARTESIAN_POINT('Ctrl Pts',(-1.01708832538956,-1.66983369391263,
4.53988111271852));
#276832=CARTESIAN_POINT('Ctrl Pts',(-1.07433584567749,-1.63215149134277,
4.5359629959281));
#276833=CARTESIAN_POINT('Ctrl Pts',(-1.13149716079555,-1.59452603185379,
4.53205077916481));
#276834=CARTESIAN_POINT('Ctrl Pts',(-1.18676836049747,-1.55383561466824,
4.52813856240153));
#276835=CARTESIAN_POINT('Ctrl Pts',(-1.23980407539598,-1.51029859783803,
4.52422634563824));
#276836=CARTESIAN_POINT('Ctrl Pts',(-1.29277742362883,-1.46681277780186,
4.52031872939586));
#276837=CARTESIAN_POINT('Ctrl Pts',(-1.34352012948776,-1.42048731677101,
4.51641111315347));
#276838=CARTESIAN_POINT('Ctrl Pts',(-1.39171689850161,-1.37158305414767,
4.51250349691109));
#276839=CARTESIAN_POINT('Ctrl Pts',(-1.43988345981725,-1.32270944264964,
4.50859832979745));
#276840=CARTESIAN_POINT('Ctrl Pts',(-1.48550690512802,-1.27126058530313,
4.5046931626838));
#276841=CARTESIAN_POINT('Ctrl Pts',(-1.52830724049951,-1.217535616989,4.50078799557016));
#276842=CARTESIAN_POINT('Ctrl Pts',(-1.57109543023826,-1.16382589443704,
4.49688393664235));
#276843=CARTESIAN_POINT('Ctrl Pts',(-1.61106179406427,-1.10784172768312,
4.49297987771455));
#276844=CARTESIAN_POINT('Ctrl Pts',(-1.64796644080564,-1.04991552516305,
4.48907581878674));
#276845=CARTESIAN_POINT('Ctrl Pts',(-1.68487327224562,-0.991985893500431,
4.48517152874462));
#276846=CARTESIAN_POINT('Ctrl Pts',(-1.71871776462754,-0.932114414043584,
4.4812672387025));
#276847=CARTESIAN_POINT('Ctrl Pts',(-1.74930420017124,-0.870661136874301,
4.47736294866038));
#276848=CARTESIAN_POINT('Ctrl Pts',(-1.77992321514238,-0.809142402172982,
4.47345449992727));
#276849=CARTESIAN_POINT('Ctrl Pts',(-1.80727702793962,-0.746038948484227,
4.46954605119415));
#276850=CARTESIAN_POINT('Ctrl Pts',(-1.83121707704509,-0.681733097875147,
4.46563760246103));
#276851=CARTESIAN_POINT('Ctrl Pts',(-1.85517145590862,-0.617388755812789,
4.46172681425382));
#276852=CARTESIAN_POINT('Ctrl Pts',(-1.87570785731568,-0.551841053906824,
4.4578160260466));
#276853=CARTESIAN_POINT('Ctrl Pts',(-1.89272771852057,-0.485487161049503,
4.45390523783939));
#276854=CARTESIAN_POINT('Ctrl Pts',(-1.9097769675425,-0.419018696396381,
4.44998769696088));
#276855=CARTESIAN_POINT('Ctrl Pts',(-1.92329746089811,-0.351741744501189,
4.44607015608236));
#276856=CARTESIAN_POINT('Ctrl Pts',(-1.93324197013006,-0.28406246659434,
4.44215261520385));
#276857=CARTESIAN_POINT('Ctrl Pts',(-1.93793532121998,-0.252120959444919,
4.44030371604521));
#276858=CARTESIAN_POINT('Ctrl Pts',(-1.94183290864853,-0.22008989195002,
4.43845481688658));
#276859=CARTESIAN_POINT('Ctrl Pts',(-1.94493379883751,-0.188012015944455,
4.43660591772794));
#276860=CARTESIAN_POINT('Ctrl Pts',(-1.95093590311411,-0.125921859562347,
4.43302717586003));
#276861=CARTESIAN_POINT('Ctrl Pts',(-1.95396538326698,-0.0635397665011596,
4.42944843399213));
#276862=CARTESIAN_POINT('Ctrl Pts',(-1.95399970505248,-0.00107361763076356,
4.42586969212423));
#276863=CARTESIAN_POINT('',(-1.95135153623783,-0.00103806439304008,3.72586969212423));
#276864=CARTESIAN_POINT('Ctrl Pts',(-1.9564564746551,-0.00105791454139017,
4.42586871637248));
#276865=CARTESIAN_POINT('Ctrl Pts',(-1.95257935738576,0.583682076751817,
4.39241064063383));
#276866=CARTESIAN_POINT('Ctrl Pts',(-1.36364931315002,1.82247384836932,
4.32191542203802));
#276867=CARTESIAN_POINT('Ctrl Pts',(0.742868822040285,2.18659612025236,
4.21438306058509));
#276868=CARTESIAN_POINT('Ctrl Pts',(2.2398397306889,0.562294105152547,4.10327163201366));
#276869=CARTESIAN_POINT('Ctrl Pts',(1.68755381017009,-1.57645768025738,
3.99216020344222));
#276870=CARTESIAN_POINT('Ctrl Pts',(-0.408695780024086,-2.27288900724468,
3.8810487748708));
#276871=CARTESIAN_POINT('Ctrl Pts',(-1.78461130773358,-1.16800275096967,
3.79228527109813));
#276872=CARTESIAN_POINT('Ctrl Pts',(-1.95259779099517,-0.2594810280554,
3.74055891018261));
#276873=CARTESIAN_POINT('Ctrl Pts',(-1.95135153623783,-0.00103806439304008,
3.72586969212423));
#276874=CARTESIAN_POINT('',(-1.95399929813707,0.00165616419005204,3.02586967145614));
#276875=CARTESIAN_POINT('Ctrl Pts',(-1.95135153623783,-0.00103806439304008,
3.72586969212423));
#276876=CARTESIAN_POINT('Ctrl Pts',(-1.94945550559233,0.392152634644927,
3.70352176732547));
#276877=CARTESIAN_POINT('Ctrl Pts',(-1.64333976564086,1.43969285576572,
3.64413669966957));
#276878=CARTESIAN_POINT('Ctrl Pts',(0.0653941910371889,2.30841510124345,
3.54771448915652));
#276879=CARTESIAN_POINT('Ctrl Pts',(1.97461131271872,1.19748354624812,3.43660306058508));
#276880=CARTESIAN_POINT('Ctrl Pts',(2.0772323364324,-1.00904038587818,3.32549163201366));
#276881=CARTESIAN_POINT('Ctrl Pts',(0.279368029483037,-2.2923808985465,
3.21438020344223));
#276882=CARTESIAN_POINT('Ctrl Pts',(-1.56641308901667,-1.56071800928074,
3.11450622347908));
#276883=CARTESIAN_POINT('Ctrl Pts',(-1.94902816663213,-0.451492593907781,
3.05166938637309));
#276884=CARTESIAN_POINT('Ctrl Pts',(-1.9526756070676,0.00165467924746206,
3.02586969212423));
#276885=CARTESIAN_POINT('',(-1.95399999956327,4.13126301758459E-5,2.32586969217956));
#276886=CARTESIAN_POINT('Ctrl Pts',(-1.95399929813707,0.00165616419005204,
3.02586967145614));
#276887=CARTESIAN_POINT('Ctrl Pts',(-1.95392953159649,0.0839691209373926,
3.02118636728134));
#276888=CARTESIAN_POINT('Ctrl Pts',(-1.94865472071711,0.166056497020639,
3.01650306310655));
#276889=CARTESIAN_POINT('Ctrl Pts',(-1.93828293935986,0.247336303413968,
3.01181975893175));
#276890=CARTESIAN_POINT('Ctrl Pts',(-1.92776906934288,0.329729605971204,
3.00707229563226));
#276891=CARTESIAN_POINT('Ctrl Pts',(-1.912017700784,0.411293043825035,3.00232483233277));
#276892=CARTESIAN_POINT('Ctrl Pts',(-1.89119027174125,0.491442118739601,
2.99757736903329));
#276893=CARTESIAN_POINT('Ctrl Pts',(-1.88326427479092,0.521943306478164,
2.99577069478865));
#276894=CARTESIAN_POINT('Ctrl Pts',(-1.87460364264371,0.552239885614248,
2.99396402054401));
#276895=CARTESIAN_POINT('Ctrl Pts',(-1.86521906910856,0.582300458727094,
2.99215734629938));
#276896=CARTESIAN_POINT('Ctrl Pts',(-1.84486683613545,0.647492530056354,
2.98823922950956));
#276897=CARTESIAN_POINT('Ctrl Pts',(-1.82105230986066,0.711745538601787,
2.98432111271974));
#276898=CARTESIAN_POINT('Ctrl Pts',(-1.79388100208733,0.774665702319497,
2.98040299592992));
#276899=CARTESIAN_POINT('Ctrl Pts',(-1.76675060974911,0.837491118817201,
2.97649077916723));
#276900=CARTESIAN_POINT('Ctrl Pts',(-1.73627366123969,0.898987225812118,
2.97257856240455));
#276901=CARTESIAN_POINT('Ctrl Pts',(-1.70260523957784,0.958775989562772,
2.96866634564187));
#276902=CARTESIAN_POINT('Ctrl Pts',(-1.66897640986261,1.01849444548712,
2.96475872940008));
#276903=CARTESIAN_POINT('Ctrl Pts',(-1.63216380066439,1.07650911897933,
2.96085111315828));
#276904=CARTESIAN_POINT('Ctrl Pts',(-1.59236955253217,1.13246421937671,
2.95694349691649));
#276905=CARTESIAN_POINT('Ctrl Pts',(-1.55260024575307,1.18838424948169,
2.95303832980343));
#276906=CARTESIAN_POINT('Ctrl Pts',(-1.50985329151177,1.24224686718789,
2.94913316269037));
#276907=CARTESIAN_POINT('Ctrl Pts',(-1.46437467279383,1.29372439788386,
2.94522799557731));
#276908=CARTESIAN_POINT('Ctrl Pts',(-1.41890895973643,1.34518732058261,
2.94132393665009));
#276909=CARTESIAN_POINT('Ctrl Pts',(-1.37071344657607,1.39426613143396,
2.93741987772286));
#276910=CARTESIAN_POINT('Ctrl Pts',(-1.32007384677977,1.4406668730307,2.93351581879564));
#276911=CARTESIAN_POINT('Ctrl Pts',(-1.26943124919653,1.48707036148046,
2.92961152875409));
#276912=CARTESIAN_POINT('Ctrl Pts',(-1.21634464211473,1.53079513551345,
2.92570723871255));
#276913=CARTESIAN_POINT('Ctrl Pts',(-1.16113462979361,1.57158594149161,
2.921802948671));
#276914=CARTESIAN_POINT('Ctrl Pts',(-1.1058658100121,1.61242019617782,2.91789449993844));
#276915=CARTESIAN_POINT('Ctrl Pts',(-1.04846946758296,1.65031395313702,
2.91398605120588));
#276916=CARTESIAN_POINT('Ctrl Pts',(-0.989296327289874,1.68505453229584,
2.91007760247332));
#276917=CARTESIAN_POINT('Ctrl Pts',(-0.930087767821911,1.71981590606929,
2.90616681426667));
#276918=CARTESIAN_POINT('Ctrl Pts',(-0.869100730642009,1.75142011943706,
2.90225602606001));
#276919=CARTESIAN_POINT('Ctrl Pts',(-0.806709242136566,1.77970115430975,
2.89834523785335));
#276920=CARTESIAN_POINT('Ctrl Pts',(-0.74421002363075,1.80803102141854,
2.89442769697537));
#276921=CARTESIAN_POINT('Ctrl Pts',(-0.680301971665396,1.83302607872028,
2.8905101560974));
#276922=CARTESIAN_POINT('Ctrl Pts',(-0.615376880502353,1.85456930173644,
2.88659261521942));
#276923=CARTESIAN_POINT('Ctrl Pts',(-0.584735222763013,1.86473671243142,
2.88474371605559));
#276924=CARTESIAN_POINT('Ctrl Pts',(-0.553867213033213,1.87413599185907,
2.88289481689176));
#276925=CARTESIAN_POINT('Ctrl Pts',(-0.522814791870344,1.88275879851923,
2.88104591772793));
#276926=CARTESIAN_POINT('Ctrl Pts',(-0.457009681946909,1.9010319224455,
2.87712780093843));
#276927=CARTESIAN_POINT('Ctrl Pts',(-0.390114964549388,1.91588714213598,
2.87320968414892));
#276928=CARTESIAN_POINT('Ctrl Pts',(-0.322518672193423,1.92719944636942,
2.86929156735941));
#276929=CARTESIAN_POINT('Ctrl Pts',(-0.255024168523623,1.93849471616879,
2.86537935059706));
#276930=CARTESIAN_POINT('Ctrl Pts',(-0.186830667813991,1.94625757813585,
2.8614671338347));
#276931=CARTESIAN_POINT('Ctrl Pts',(-0.118339868132747,1.95041320637713,
2.85755491707235));
#276932=CARTESIAN_POINT('Ctrl Pts',(-0.0499296093251734,1.95456394786091,
2.8536473008309));
#276933=CARTESIAN_POINT('Ctrl Pts',(0.0187767654808092,1.95511585040939,
2.84973968458946));
#276934=CARTESIAN_POINT('Ctrl Pts',(0.0873707122396018,1.95204568559313,
2.84583206834801));
#276935=CARTESIAN_POINT('Ctrl Pts',(0.155921667210954,1.94897744502645,
2.84192690123531));
#276936=CARTESIAN_POINT('Ctrl Pts',(0.224359843630586,1.94229166231341,
2.83802173412261));
#276937=CARTESIAN_POINT('Ctrl Pts',(0.292276529263017,1.93201719206687,
2.83411656700991));
#276938=CARTESIAN_POINT('Ctrl Pts',(0.360173941889366,1.92174563745035,
2.83021250808306));
#276939=CARTESIAN_POINT('Ctrl Pts',(0.427549671387565,1.90788749049407,
2.8263084491562));
#276940=CARTESIAN_POINT('Ctrl Pts',(0.494001773370695,1.89052327356915,
2.82240439022935));
#276941=CARTESIAN_POINT('Ctrl Pts',(0.560457809216534,1.87315802870916,
2.81850010018818));
#276942=CARTESIAN_POINT('Ctrl Pts',(0.625989633742968,1.85228642864929,
2.81459581014701));
#276943=CARTESIAN_POINT('Ctrl Pts',(0.690208885006844,1.82803930347726,
2.81069152010585));
#276944=CARTESIAN_POINT('Ctrl Pts',(0.754496540005923,1.80376635125341,
2.80678307137368));
#276945=CARTESIAN_POINT('Ctrl Pts',(0.817468370513111,1.77611087254772,
2.80287462264151));
#276946=CARTESIAN_POINT('Ctrl Pts',(0.878755435843135,1.7452520975424,2.79896617390935));
#276947=CARTESIAN_POINT('Ctrl Pts',(0.940079185676753,1.714374851448,2.79505538570309));
#276948=CARTESIAN_POINT('Ctrl Pts',(0.999715736226602,1.68029073719743,
2.79114459749683));
#276949=CARTESIAN_POINT('Ctrl Pts',(1.05732270201401,1.6432238751326,2.78723380929057));
#276950=CARTESIAN_POINT('Ctrl Pts',(1.11502913647236,1.60609301053865,2.783316268413));
#276951=CARTESIAN_POINT('Ctrl Pts',(1.17069859304666,1.56596940652051,2.77939872753543));
#276952=CARTESIAN_POINT('Ctrl Pts',(1.22402020238525,1.52311869010684,2.77548118665786));
#276953=CARTESIAN_POINT('Ctrl Pts',(1.24918555028494,1.50289512221988,2.77363228749075));
#276954=CARTESIAN_POINT('Ctrl Pts',(1.27382845270328,1.48206466753042,2.77178338832364));
#276955=CARTESIAN_POINT('Ctrl Pts',(1.2979191479585,1.46065803162913,2.76993448915652));
#276956=CARTESIAN_POINT('Ctrl Pts',(1.3489712330856,1.41529390300022,2.76601637236201));
#276957=CARTESIAN_POINT('Ctrl Pts',(1.39774334461602,1.36716011116494,2.7620982555675));
#276958=CARTESIAN_POINT('Ctrl Pts',(1.44391994502689,1.31651479002461,2.75818013877299));
#276959=CARTESIAN_POINT('Ctrl Pts',(1.49002701121773,1.26594573224868,2.75426792200561));
#276960=CARTESIAN_POINT('Ctrl Pts',(1.53354599434848,1.21287301153751,2.75035570523823));
#276961=CARTESIAN_POINT('Ctrl Pts',(1.57419609978841,1.15759346897387,2.74644348847085));
#276962=CARTESIAN_POINT('Ctrl Pts',(1.61479840326056,1.10237893167612,2.74253587222438));
#276963=CARTESIAN_POINT('Ctrl Pts',(1.65253823908165,1.04496312079801,2.73862825597791));
#276964=CARTESIAN_POINT('Ctrl Pts',(1.68717444166508,0.985676622119112,
2.73472063973143));
#276965=CARTESIAN_POINT('Ctrl Pts',(1.72178893574027,0.926427281712436,
2.73081547261371));
#276966=CARTESIAN_POINT('Ctrl Pts',(1.75330340772147,0.865310003067912,
2.72691030549598));
#276967=CARTESIAN_POINT('Ctrl Pts',(1.78152035195789,0.802683770584543,
2.72300513837825));
#276968=CARTESIAN_POINT('Ctrl Pts',(1.80972928895227,0.740075309813019,
2.71910107944638));
#276969=CARTESIAN_POINT('Ctrl Pts',(1.83464235386879,0.675959193508858,
2.7151970205145));
#276970=CARTESIAN_POINT('Ctrl Pts',(1.85610911524766,0.610716752917867,
2.71129296158262));
#276971=CARTESIAN_POINT('Ctrl Pts',(1.87757714742586,0.545470450074506,
2.70738867153645));
#276972=CARTESIAN_POINT('Ctrl Pts',(1.8955983197249,0.479098158605541,2.70348438149028));
#276973=CARTESIAN_POINT('Ctrl Pts',(1.91007182962046,0.411997094274172,
2.6995800914441));
#276974=CARTESIAN_POINT('Ctrl Pts',(1.92456075611001,0.344824556618577,
2.69567164270699));
#276975=CARTESIAN_POINT('Ctrl Pts',(1.93549437491877,0.27692217867235,2.69176319396987));
#276976=CARTESIAN_POINT('Ctrl Pts',(1.94282307781572,0.208697120983155,
2.68785474523276));
#276977=CARTESIAN_POINT('Ctrl Pts',(1.95015616744294,0.140431225927526,
2.68394395702157));
#276978=CARTESIAN_POINT('Ctrl Pts',(1.95388002009114,0.0718427579564729,
2.68003316881039));
#276979=CARTESIAN_POINT('Ctrl Pts',(1.95399714386114,0.00334092539568565,
2.67612238059921));
#276980=CARTESIAN_POINT('Ctrl Pts',(1.95411446986615,-0.0652791877592747,
2.6722048397168));
#276981=CARTESIAN_POINT('Ctrl Pts',(1.95061266267349,-0.133811875965454,
2.6682872988344));
#276982=CARTESIAN_POINT('Ctrl Pts',(1.94354619602246,-0.20185188611111,
2.664369757952));
#276983=CARTESIAN_POINT('Ctrl Pts',(1.94021114876168,-0.233963641627143,
2.66252085882969));
#276984=CARTESIAN_POINT('Ctrl Pts',(1.93608285036119,-0.265965791307287,
2.66067195970739));
#276985=CARTESIAN_POINT('Ctrl Pts',(1.9311709473418,-0.297816675394412,
2.65882306058509));
#276986=CARTESIAN_POINT('Ctrl Pts',(1.92076182905302,-0.365313859022907,
2.65490494379978));
#276987=CARTESIAN_POINT('Ctrl Pts',(1.90678913190683,-0.432398466001827,
2.65098682701447));
#276988=CARTESIAN_POINT('Ctrl Pts',(1.88929850252114,-0.498665387179999,
2.64706871022916));
#276989=CARTESIAN_POINT('Ctrl Pts',(1.87183421109152,-0.564832521482559,
2.64315649347098));
#276990=CARTESIAN_POINT('Ctrl Pts',(1.85086262543722,-0.630183941907614,
2.63924427671279));
#276991=CARTESIAN_POINT('Ctrl Pts',(1.82648075681501,-0.694322723943613,
2.63533205995461));
#276992=CARTESIAN_POINT('Ctrl Pts',(1.80212755973679,-0.75838608280596,
2.63142444371727));
#276993=CARTESIAN_POINT('Ctrl Pts',(1.77437221811931,-0.821239177707652,
2.62751682747993));
#276994=CARTESIAN_POINT('Ctrl Pts',(1.74336159018658,-0.882500065644257,
2.62360921124259));
#276995=CARTESIAN_POINT('Ctrl Pts',(1.71237039840481,-0.943722557845439,
2.61970404413396));
#276996=CARTESIAN_POINT('Ctrl Pts',(1.67812818921998,-1.00335438478286,
2.61579887702533));
#276997=CARTESIAN_POINT('Ctrl Pts',(1.64082936390711,-1.06103487150056,
2.6118937099167));
#276998=CARTESIAN_POINT('Ctrl Pts',(1.60354112303974,-1.11869898998244,
2.60798965099386));
#276999=CARTESIAN_POINT('Ctrl Pts',(1.56319825492906,-1.17441245466215,
2.60408559207103));
#277000=CARTESIAN_POINT('Ctrl Pts',(1.52003947262901,-1.22784201005248,
2.6001815331482));
#277001=CARTESIAN_POINT('Ctrl Pts',(1.47687813539453,-1.28127472839143,
2.596277243111));
#277002=CARTESIAN_POINT('Ctrl Pts',(1.43090086409557,-1.33242288798782,
2.5923729530738));
#277003=CARTESIAN_POINT('Ctrl Pts',(1.38238664109173,-1.38098630497595,
2.5884686630366));
#277004=CARTESIAN_POINT('Ctrl Pts',(1.33382074270884,-1.42960144974257,
2.58456021430829));
#277005=CARTESIAN_POINT('Ctrl Pts',(1.28271284805352,-1.47562600878443,
2.58065176557999));
#277006=CARTESIAN_POINT('Ctrl Pts',(1.22937806852749,-1.51879740736664,
2.57674331685169));
#277007=CARTESIAN_POINT('Ctrl Pts',(1.17601136448446,-1.56199464698654,
2.57283252864924));
#277008=CARTESIAN_POINT('Ctrl Pts',(1.12041552094019,-1.60233503837291,
2.56892174044679));
#277009=CARTESIAN_POINT('Ctrl Pts',(1.06293564488252,-1.63959867493182,
2.56501095224434));
#277010=CARTESIAN_POINT('Ctrl Pts',(1.00535651959502,-1.67692665378725,
2.56109341137045));
#277011=CARTESIAN_POINT('Ctrl Pts',(0.945887295140474,-1.71116702948653,
2.55717587049657));
#277012=CARTESIAN_POINT('Ctrl Pts',(0.88489794965692,-1.74214569387666,
2.55325832962268));
#277013=CARTESIAN_POINT('Ctrl Pts',(0.856113782270623,-1.75676619937872,
2.55140943041967));
#277014=CARTESIAN_POINT('Ctrl Pts',(0.826991313224014,-1.77066088609606,
2.54956053121666));
#277015=CARTESIAN_POINT('Ctrl Pts',(0.797570771523595,-1.78381525512348,
2.54771163201366));
#277016=CARTESIAN_POINT('Ctrl Pts',(0.735223879866186,-1.81169149305702,
2.54379351522746));
#277017=CARTESIAN_POINT('Ctrl Pts',(0.671290166061522,-1.83635038593064,
2.53987539844126));
#277018=CARTESIAN_POINT('Ctrl Pts',(0.606134698217115,-1.85761048867012,
2.53595728165506));
#277019=CARTESIAN_POINT('Ctrl Pts',(0.541077343587392,-1.87883857725802,
2.53204506489608));
#277020=CARTESIAN_POINT('Ctrl Pts',(0.474802350038025,-1.89667788179146,
2.52813284813709));
#277021=CARTESIAN_POINT('Ctrl Pts',(0.40769577792443,-1.91099454542984,
2.52422063137811));
#277022=CARTESIAN_POINT('Ctrl Pts',(0.340668118921272,-1.92529437357173,
2.5203130151401));
#277023=CARTESIAN_POINT('Ctrl Pts',(0.272811302223436,-1.93607968555399,
2.5164053989021));
#277024=CARTESIAN_POINT('Ctrl Pts',(0.204525847475429,-1.94326662548258,
2.5124977826641));
#277025=CARTESIAN_POINT('Ctrl Pts',(0.1362831911659,-1.95044906094082,2.50859261555489));
#277026=CARTESIAN_POINT('Ctrl Pts',(0.0676129178068932,-1.95403754678965,
2.50468744844568));
#277027=CARTESIAN_POINT('Ctrl Pts',(-0.00107652451106434,-1.95399970345314,
2.50078228133647));
#277028=CARTESIAN_POINT('Ctrl Pts',(-0.0697464745338006,-1.95396187085561,
2.49687822241314));
#277029=CARTESIAN_POINT('Ctrl Pts',(-0.138435091067868,-1.95029975220233,
2.49297416348981));
#277030=CARTESIAN_POINT('Ctrl Pts',(-0.206732918045551,-1.9430330672936,
2.48907010456648));
#277031=CARTESIAN_POINT('Ctrl Pts',(-0.275034788149518,-1.9357659522083,
2.48516581452887));
#277032=CARTESIAN_POINT('Ctrl Pts',(-0.342945333921737,-1.92489390181521,
2.48126152449125));
#277033=CARTESIAN_POINT('Ctrl Pts',(-0.410061032500004,-1.91048840604308,
2.47735723445364));
#277034=CARTESIAN_POINT('Ctrl Pts',(-0.477248219990985,-1.89606756612268,
2.47344878572506));
#277035=CARTESIAN_POINT('Ctrl Pts',(-0.543638388808918,-1.87810587310111,
2.46954033699648));
#277036=CARTESIAN_POINT('Ctrl Pts',(-0.608840007204148,-1.85672557089831,
2.46563188826789));
#277037=CARTESIAN_POINT('Ctrl Pts',(-0.674080653230671,-1.83533247112128,
2.46172110006523));
#277038=CARTESIAN_POINT('Ctrl Pts',(-0.738130874239155,-1.81051686743246,
2.45781031186258));
#277039=CARTESIAN_POINT('Ctrl Pts',(-0.800618706968965,-1.78244935020644,
2.45389952365992));
#277040=CARTESIAN_POINT('Ctrl Pts',(-0.863214436054704,-1.75433336942045,
2.44998198278594));
#277041=CARTESIAN_POINT('Ctrl Pts',(-0.924241955393526,-1.72295449324751,
2.44606444191196));
#277042=CARTESIAN_POINT('Ctrl Pts',(-0.983354279983066,-1.68852905217499,
2.44214690103798));
#277043=CARTESIAN_POINT('Ctrl Pts',(-1.01125257972668,-1.67228182656653,
2.4402980018394));
#277044=CARTESIAN_POINT('Ctrl Pts',(-1.03872471524778,-1.65535662974093,
2.43844910264081));
#277045=CARTESIAN_POINT('Ctrl Pts',(-1.06573668106705,-1.63777938887635,
2.43660020344223));
#277046=CARTESIAN_POINT('Ctrl Pts',(-1.12294424235479,-1.60055325395682,
2.43268449382947));
#277047=CARTESIAN_POINT('Ctrl Pts',(-1.17831309400748,-1.56025187137137,
2.42876878421671));
#277048=CARTESIAN_POINT('Ctrl Pts',(-1.23149300216491,-1.517083051655,2.42485307460396));
#277049=CARTESIAN_POINT('Ctrl Pts',(-1.28459280640327,-1.47397925633903,
2.42094326315269));
#277050=CARTESIAN_POINT('Ctrl Pts',(-1.33550983127716,-1.42801690352454,
2.41703345170141));
#277051=CARTESIAN_POINT('Ctrl Pts',(-1.38392240404207,-1.37944727321867,
2.41312364025014));
#277052=CARTESIAN_POINT('Ctrl Pts',(-1.43227811874202,-1.33093468543372,
2.40921842067037));
#277053=CARTESIAN_POINT('Ctrl Pts',(-1.47813487660824,-1.27982124855245,
2.40531320109061));
#277054=CARTESIAN_POINT('Ctrl Pts',(-1.52120514589974,-1.22639753101845,
2.40140798151084));
#277055=CARTESIAN_POINT('Ctrl Pts',(-1.56424850782029,-1.17300718898474,
2.3975052016463));
#277056=CARTESIAN_POINT('Ctrl Pts',(-1.60450852579453,-1.11730981187041,
2.39360242178176));
#277057=CARTESIAN_POINT('Ctrl Pts',(-1.64173660049825,-1.05963056514261,
2.38969964191722));
#277058=CARTESIAN_POINT('Ctrl Pts',(-1.67895422954386,-1.00196750237533,
2.38579795711614));
#277059=CARTESIAN_POINT('Ctrl Pts',(-1.71314133713107,-0.942324087565681,
2.38189627231505));
#277060=CARTESIAN_POINT('Ctrl Pts',(-1.74409254061705,-0.881054600898244,
2.37799458751397));
#277061=CARTESIAN_POINT('Ctrl Pts',(-1.77504571108668,-0.819781220486312,
2.37409265475645));
#277062=CARTESIAN_POINT('Ctrl Pts',(-1.80276234945153,-0.7568820039011,
2.37019072199893));
#277063=CARTESIAN_POINT('Ctrl Pts',(-1.82708378310748,-0.692734328228109,
2.3662887892414));
#277064=CARTESIAN_POINT('Ctrl Pts',(-1.85143116240428,-0.628518221040039,
2.36238269397655));
#277065=CARTESIAN_POINT('Ctrl Pts',(-1.87237593424198,-0.563051458451526,
2.35847659871169));
#277066=CARTESIAN_POINT('Ctrl Pts',(-1.88980857233421,-0.496728859572438,
2.35457050344684));
#277067=CARTESIAN_POINT('Ctrl Pts',(-1.9072517504597,-0.430366161059865,
2.35066204649847));
#277068=CARTESIAN_POINT('Ctrl Pts',(-1.92117846918179,-0.363147078863803,
2.3467535895501));
#277069=CARTESIAN_POINT('Ctrl Pts',(-1.93153043378067,-0.2954761976523,
2.34284513260173));
#277070=CARTESIAN_POINT('Ctrl Pts',(-1.94190018322113,-0.227689056779093,
2.3389299608615));
#277071=CARTESIAN_POINT('Ctrl Pts',(-1.94868287364594,-0.159449057639085,
2.33501478912126));
#277072=CARTESIAN_POINT('Ctrl Pts',(-1.9518721839828,-0.0911645621620376,
2.33109961738103));
#277073=CARTESIAN_POINT('Ctrl Pts',(-1.95329228809852,-0.0607595269588351,
2.32935630898054));
#277074=CARTESIAN_POINT('Ctrl Pts',(-1.95400064202245,-0.0303456469757893,
2.32761300058005));
#277075=CARTESIAN_POINT('Ctrl Pts',(-1.95399999956327,4.13126301756066E-5,
2.32586969217956));
#277076=CARTESIAN_POINT('',(-1.95399927547201,-0.00168269273987639,1.62586971130023));
#277077=CARTESIAN_POINT('Ctrl Pts',(-1.95399999956325,4.13135945347792E-5,
2.32586969212423));
#277078=CARTESIAN_POINT('Ctrl Pts',(-1.95399995276918,0.00225452253103485,
2.32574271970642));
#277079=CARTESIAN_POINT('Ctrl Pts',(-1.95399614577176,0.0044677267577048,
2.32561574728861));
#277080=CARTESIAN_POINT('Ctrl Pts',(-1.95398857860865,0.00668091812061876,
2.3254887748708));
#277081=CARTESIAN_POINT('Ctrl Pts',(-1.95375507097746,0.0749756099772388,
2.32157065812134));
#277082=CARTESIAN_POINT('Ctrl Pts',(-1.94993629437008,0.143393426555683,
2.31765254137188));
#277083=CARTESIAN_POINT('Ctrl Pts',(-1.94251701066304,0.211526980039711,
2.31373442462242));
#277084=CARTESIAN_POINT('Ctrl Pts',(-1.93510889915362,0.279557935813039,
2.30982220790001));
#277085=CARTESIAN_POINT('Ctrl Pts',(-1.92411109363811,0.347304992968974,
2.30590999117761));
#277086=CARTESIAN_POINT('Ctrl Pts',(-1.90956036678483,0.414361201857249,
2.3019977744552));
#277087=CARTESIAN_POINT('Ctrl Pts',(-1.89502675067027,0.481338556865477,
2.29809015825336));
#277088=CARTESIAN_POINT('Ctrl Pts',(-1.87694861462697,0.547626198615865,
2.29418254205152));
#277089=CARTESIAN_POINT('Ctrl Pts',(-1.85541425435577,0.612824562769333,
2.29027492584969));
#277090=CARTESIAN_POINT('Ctrl Pts',(-1.83389339091051,0.67798206334657,
2.28636975877636));
#277091=CARTESIAN_POINT('Ctrl Pts',(-1.80892075423999,0.742051174598245,
2.28246459170303));
#277092=CARTESIAN_POINT('Ctrl Pts',(-1.78063482179842,0.804646277191972,
2.2785594246297));
#277093=CARTESIAN_POINT('Ctrl Pts',(-1.75235691617392,0.867223616912274,
2.27465536574193));
#277094=CARTESIAN_POINT('Ctrl Pts',(-1.72076778375044,0.928327330315059,
2.27075130685415));
#277095=CARTESIAN_POINT('Ctrl Pts',(-1.68605380531961,0.987592307365376,
2.26684724796638));
#277096=CARTESIAN_POINT('Ctrl Pts',(-1.65133777187124,1.046860792817,2.26294295796394));
#277097=CARTESIAN_POINT('Ctrl Pts',(-1.61349677597143,1.10428990267778,
2.25903866796151));
#277098=CARTESIAN_POINT('Ctrl Pts',(-1.57276194678371,1.15954122770565,
2.25513437795907));
#277099=CARTESIAN_POINT('Ctrl Pts',(-1.53198372850369,1.21485140420998,
2.25122592926485));
#277100=CARTESIAN_POINT('Ctrl Pts',(-1.48830581788254,1.26797876983067,
2.24731748057063));
#277101=CARTESIAN_POINT('Ctrl Pts',(-1.44200067467252,1.31861671999259,
2.24340903187641));
#277102=CARTESIAN_POINT('Ctrl Pts',(-1.39566781465987,1.36928498043913,
2.23949824370771));
#277103=CARTESIAN_POINT('Ctrl Pts',(-1.34670494300387,1.41746051485351,
2.23558745553901));
#277104=CARTESIAN_POINT('Ctrl Pts',(-1.29542053905071,1.46287443993173,
2.2316766673703));
#277105=CARTESIAN_POINT('Ctrl Pts',(-1.24404758344009,1.50836678024006,
2.2277591265293));
#277106=CARTESIAN_POINT('Ctrl Pts',(-1.19034547986167,1.55108768817199,
2.22384158568829));
#277107=CARTESIAN_POINT('Ctrl Pts',(-1.13465412656932,1.59080986074993,
2.21992404484728));
#277108=CARTESIAN_POINT('Ctrl Pts',(-1.1083703632788,1.60955690350795,2.21807514533131));
#277109=CARTESIAN_POINT('Ctrl Pts',(-1.0816439047551,1.6276366515146,2.21622624581534));
#277110=CARTESIAN_POINT('Ctrl Pts',(-1.05451236992383,1.64502877229476,
2.21437734629937));
#277111=CARTESIAN_POINT('Ctrl Pts',(-0.997016264336595,1.68188548604064,
2.21045922952302));
#277112=CARTESIAN_POINT('Ctrl Pts',(-0.937471564875764,1.71579727589714,
2.20654111274667));
#277113=CARTESIAN_POINT('Ctrl Pts',(-0.876212221149488,1.74653031565681,
2.20262299597032));
#277114=CARTESIAN_POINT('Ctrl Pts',(-0.815045123734695,1.77721707660601,
2.1987107792216));
#277115=CARTESIAN_POINT('Ctrl Pts',(-0.752168942461889,1.80473436849974,
2.19479856247288));
#277116=CARTESIAN_POINT('Ctrl Pts',(-0.687945477004168,1.82889229334849,
2.19088634572416));
#277117=CARTESIAN_POINT('Ctrl Pts',(-0.623797534314021,1.8530218099927,
2.18697872949698));
#277118=CARTESIAN_POINT('Ctrl Pts',(-0.558305912133177,1.8737996328006,
2.18307111326981));
#277119=CARTESIAN_POINT('Ctrl Pts',(-0.49185415977605,1.89108315140054,
2.17916349704263));
#277120=CARTESIAN_POINT('Ctrl Pts',(-0.425444056576054,1.9083558374196,
2.17525832994458));
#277121=CARTESIAN_POINT('Ctrl Pts',(-0.358075491891942,1.92213844012248,
2.17135316284652));
#277122=CARTESIAN_POINT('Ctrl Pts',(-0.290147526652456,1.93233806896657,
2.16744799574847));
#277123=CARTESIAN_POINT('Ctrl Pts',(-0.222238837626192,1.94253480341776,
2.16354393683662));
#277124=CARTESIAN_POINT('Ctrl Pts',(-0.153771549376384,1.94915050944118,
2.15963987792477));
#277125=CARTESIAN_POINT('Ctrl Pts',(-0.0851534841210611,1.95214366380706,
2.15573581901292));
#277126=CARTESIAN_POINT('Ctrl Pts',(-0.0165313567871024,1.95513699536284,
2.15183152898708));
#277127=CARTESIAN_POINT('Ctrl Pts',(0.0522410737505755,1.95450733063121,
2.14792723896125));
#277128=CARTESIAN_POINT('Ctrl Pts',(0.120754136718002,1.9502652225955,2.14402294893542));
#277129=CARTESIAN_POINT('Ctrl Pts',(0.189340177007754,1.94601859603921,
2.14011450021897));
#277130=CARTESIAN_POINT('Ctrl Pts',(0.257665806500161,1.93815187756227,
2.13620605150253));
#277131=CARTESIAN_POINT('Ctrl Pts',(0.325325647557145,1.92672759440496,
2.13229760278608));
#277132=CARTESIAN_POINT('Ctrl Pts',(0.393025987656144,1.9152964730329,2.12838681459579));
#277133=CARTESIAN_POINT('Ctrl Pts',(0.460059266106312,1.9003036563682,2.1244760264055));
#277134=CARTESIAN_POINT('Ctrl Pts',(0.526032249962911,1.88186239454402,
2.1205652382152));
#277135=CARTESIAN_POINT('Ctrl Pts',(0.592119147905457,1.86338929060264,
2.1166476973538));
#277136=CARTESIAN_POINT('Ctrl Pts',(0.657141631466861,1.84145601470102,
2.1127301564924));
#277137=CARTESIAN_POINT('Ctrl Pts',(0.72072435018235,1.81622476886927,2.108812615631));
#277138=CARTESIAN_POINT('Ctrl Pts',(0.750732472203038,1.80431678004858,
2.10696371632998));
#277139=CARTESIAN_POINT('Ctrl Pts',(0.780420229962298,1.79167487856341,
2.10511481702896));
#277140=CARTESIAN_POINT('Ctrl Pts',(0.809750133717947,1.778319634077,2.10326591772794));
#277141=CARTESIAN_POINT('Ctrl Pts',(0.871904948480085,1.75001770870858,
2.09934780076015));
#277142=CARTESIAN_POINT('Ctrl Pts',(0.932697398100167,1.71839715751514,
2.09542968379236));
#277143=CARTESIAN_POINT('Ctrl Pts',(0.991749879805991,1.68361164640329,
2.09151156682456));
#277144=CARTESIAN_POINT('Ctrl Pts',(1.05071343838672,1.6488785164322,2.08759934988324));
#277145=CARTESIAN_POINT('Ctrl Pts',(1.10794180861744,1.61099013280824,2.08368713294192));
#277146=CARTESIAN_POINT('Ctrl Pts',(1.16307917875715,1.57014738924141,2.0797749160006));
#277147=CARTESIAN_POINT('Ctrl Pts',(1.21815171082154,1.52935267416916,2.07586729958006));
#277148=CARTESIAN_POINT('Ctrl Pts',(1.27113773279588,1.48561079024756,2.07195968315951));
#277149=CARTESIAN_POINT('Ctrl Pts',(1.32170935570517,1.43916655708832,2.06805206673896));
#277150=CARTESIAN_POINT('Ctrl Pts',(1.37224928245928,1.39275143321084,2.06414689944718));
#277151=CARTESIAN_POINT('Ctrl Pts',(1.42037745047451,1.3436376518615,2.0602417321554));
#277152=CARTESIAN_POINT('Ctrl Pts',(1.4657993210686,1.29211003802108,2.05633656486362));
#277153=CARTESIAN_POINT('Ctrl Pts',(1.51120830210297,1.24059704639342,2.05243250575797));
#277154=CARTESIAN_POINT('Ctrl Pts',(1.55391218517407,1.18667195089701,2.04852844665232));
#277155=CARTESIAN_POINT('Ctrl Pts',(1.59365482817077,1.13065480525578,2.04462438754667));
#277156=CARTESIAN_POINT('Ctrl Pts',(1.63339982386536,1.07463434349338,2.04072009732726));
#277157=CARTESIAN_POINT('Ctrl Pts',(1.67018294892636,1.01652198836168,2.03681580710785));
#277158=CARTESIAN_POINT('Ctrl Pts',(1.70379080376997,0.956667600051811,
2.03291151688845));
#277159=CARTESIAN_POINT('Ctrl Pts',(1.73743445631471,0.896749457315643,
2.02900306798009));
#277160=CARTESIAN_POINT('Ctrl Pts',(1.76789584759997,0.835086008032117,
2.02509461907174));
#277161=CARTESIAN_POINT('Ctrl Pts',(1.79500756706025,0.772051704354332,
2.02118617016338));
#277162=CARTESIAN_POINT('Ctrl Pts',(1.82213551473332,0.70897967034763,2.01727538178185));
#277163=CARTESIAN_POINT('Ctrl Pts',(1.84590962998046,0.644535610442962,
2.01336459340032));
#277164=CARTESIAN_POINT('Ctrl Pts',(1.86621169988821,0.579111294312565,
2.00945380501878));
#277165=CARTESIAN_POINT('Ctrl Pts',(1.88654882491167,0.513574011524938,
2.00553626396918));
#277166=CARTESIAN_POINT('Ctrl Pts',(1.90340181860026,0.447053570943978,
2.00161872291957));
#277167=CARTESIAN_POINT('Ctrl Pts',(1.9167032910083,0.379953279019851,1.99770118186997));
#277168=CARTESIAN_POINT('Ctrl Pts',(1.92298096869351,0.348285055205146,
1.99585228429881));
#277169=CARTESIAN_POINT('Ctrl Pts',(1.92846832939046,0.31648776660826,1.99400338672766));
#277170=CARTESIAN_POINT('Ctrl Pts',(1.93316231235789,0.284604065464821,
1.99215448915651));
#277171=CARTESIAN_POINT('Ctrl Pts',(1.94310963030885,0.217037285839111,
1.9882363726813));
#277172=CARTESIAN_POINT('Ctrl Pts',(1.94953006943767,0.148814430209601,
1.9843182562061));
#277173=CARTESIAN_POINT('Ctrl Pts',(1.95234784722165,0.0803360656803328,
1.98040013973089));
#277174=CARTESIAN_POINT('Ctrl Pts',(1.95516138190453,0.0119608180915343,
1.97648792328245));
#277175=CARTESIAN_POINT('Ctrl Pts',(1.95438300189478,-0.0566686872867476,
1.97257570683401));
#277176=CARTESIAN_POINT('Ctrl Pts',(1.94998841991117,-0.125144565252865,
1.96866349038556));
#277177=CARTESIAN_POINT('Ctrl Pts',(1.94559900567774,-0.193539919922068,
1.96475587445596));
#277178=CARTESIAN_POINT('Ctrl Pts',(1.93760186620457,-0.261781517418771,
1.96084825852636));
#277179=CARTESIAN_POINT('Ctrl Pts',(1.92602476249998,-0.329461096697164,
1.95694064259676));
#277180=CARTESIAN_POINT('Ctrl Pts',(1.91445491483107,-0.39709825729692,
1.95303547579444));
#277181=CARTESIAN_POINT('Ctrl Pts',(1.89930963660505,-0.464173614679122,
1.94913030899212));
#277182=CARTESIAN_POINT('Ctrl Pts',(1.88066838843659,-0.530285218288522,
1.94522514218981));
#277183=CARTESIAN_POINT('Ctrl Pts',(1.86203243016553,-0.596378061158479,
1.94132108357142));
#277184=CARTESIAN_POINT('Ctrl Pts',(1.83990260479671,-0.661507219978381,
1.93741702495304));
#277185=CARTESIAN_POINT('Ctrl Pts',(1.81440879788158,-0.725283885226974,
1.93351296633465));
#277186=CARTESIAN_POINT('Ctrl Pts',(1.78891348175653,-0.789064325995465,
1.92960867659959));
#277187=CARTESIAN_POINT('Ctrl Pts',(1.76005397366994,-0.851491658445897,
1.92570438686453));
#277188=CARTESIAN_POINT('Ctrl Pts',(1.72800838712072,-0.91219680663794,
1.92180009712947));
#277189=CARTESIAN_POINT('Ctrl Pts',(1.69592866686687,-0.972966615578026,
1.91789164869778));
#277190=CARTESIAN_POINT('Ctrl Pts',(1.6606563254714,-1.03201014353248,1.9139832002661));
#277191=CARTESIAN_POINT('Ctrl Pts',(1.62241508541658,-1.08898360438196,
1.91007475183441));
#277192=CARTESIAN_POINT('Ctrl Pts',(1.58415095533317,-1.14599116779049,
1.90616396392586));
#277193=CARTESIAN_POINT('Ctrl Pts',(1.5429146851814,-1.20092580466354,1.90225317601731));
#277194=CARTESIAN_POINT('Ctrl Pts',(1.49897123651761,-1.25347566075009,
1.89834238810876));
#277195=CARTESIAN_POINT('Ctrl Pts',(1.45495191158654,-1.30611625361418,
1.89442484752154));
#277196=CARTESIAN_POINT('Ctrl Pts',(1.40821641355045,-1.3563634873396,1.89050730693432));
#277197=CARTESIAN_POINT('Ctrl Pts',(1.35906696886309,-1.403941941159,1.8865897663471));
#277198=CARTESIAN_POINT('Ctrl Pts',(1.33587065457882,-1.42639681882801,
1.88474086442643));
#277199=CARTESIAN_POINT('Ctrl Pts',(1.31213713815235,-1.44825782905257,
1.88289196250575));
#277200=CARTESIAN_POINT('Ctrl Pts',(1.28790058829699,-1.46949925983794,
1.88104306058508));
#277201=CARTESIAN_POINT('Ctrl Pts',(1.23653949008005,-1.51451322508245,
1.87712494378595));
#277202=CARTESIAN_POINT('Ctrl Pts',(1.18271378322824,-1.55692046485142,
1.87320682698681));
#277203=CARTESIAN_POINT('Ctrl Pts',(1.12671883981177,-1.59643999449188,
1.86928871018768));
#277204=CARTESIAN_POINT('Ctrl Pts',(1.07080821544005,-1.6359000143126,1.8653764934189));
#277205=CARTESIAN_POINT('Ctrl Pts',(1.01273523600505,-1.67248067271155,
1.86146427665012));
#277206=CARTESIAN_POINT('Ctrl Pts',(0.952829359406696,-1.70594027206483,
1.85755205988134));
#277207=CARTESIAN_POINT('Ctrl Pts',(0.892993928424069,-1.73936052499314,
1.85364444363817));
#277208=CARTESIAN_POINT('Ctrl Pts',(0.831330308286831,-1.76966676917587,
1.84973682739499));
#277209=CARTESIAN_POINT('Ctrl Pts',(0.768196511093922,-1.79666082507053,
1.84582921115182));
#277210=CARTESIAN_POINT('Ctrl Pts',(0.705102283544324,-1.82363796221152,
1.84192404404029));
#277211=CARTESIAN_POINT('Ctrl Pts',(0.640540158052951,-1.84730683613038,
1.83801887692877));
#277212=CARTESIAN_POINT('Ctrl Pts',(0.574890895038697,-1.8675161200915,
1.83411370981725));
#277213=CARTESIAN_POINT('Ctrl Pts',(0.509260261642748,-1.88771966916346,
1.83020965089444));
#277214=CARTESIAN_POINT('Ctrl Pts',(0.442543573042965,-1.9044654325612,
1.82630559197164));
#277215=CARTESIAN_POINT('Ctrl Pts',(0.375137908571045,-1.91765157146781,
1.82240153304883));
#277216=CARTESIAN_POINT('Ctrl Pts',(0.307728253836181,-1.93083849096402,
1.81849724301456));
#277217=CARTESIAN_POINT('Ctrl Pts',(0.239630025475597,-1.9404652756969,
1.8145929529803));
#277218=CARTESIAN_POINT('Ctrl Pts',(0.171249891851364,-1.9464813059829,
1.81068866294603));
#277219=CARTESIAN_POINT('Ctrl Pts',(0.102796922562699,-1.95250374429328,
1.80678021422497));
#277220=CARTESIAN_POINT('Ctrl Pts',(0.0340619396847903,-1.95490770949013,
1.80287176550391));
#277221=CARTESIAN_POINT('Ctrl Pts',(-0.0345448876872097,-1.95369461552585,
1.79896331678284));
#277222=CARTESIAN_POINT('Ctrl Pts',(-0.103192780899194,-1.95248079544254,
1.7950525285901));
#277223=CARTESIAN_POINT('Ctrl Pts',(-0.171711875212067,-1.94764564196821,
1.79114174039736));
#277224=CARTESIAN_POINT('Ctrl Pts',(-0.239696451164668,-1.93924253545013,
1.78723095220461));
#277225=CARTESIAN_POINT('Ctrl Pts',(-0.307798414516753,-1.93082491948182,
1.78331341134409));
#277226=CARTESIAN_POINT('Ctrl Pts',(-0.375363533421236,-1.91882714065102,
1.77939587048356));
#277227=CARTESIAN_POINT('Ctrl Pts',(-0.441996475697194,-1.90335364960673,
1.77547832962303));
#277228=CARTESIAN_POINT('Ctrl Pts',(-0.473444161442377,-1.89605087312529,
1.77362943041991));
#277229=CARTESIAN_POINT('Ctrl Pts',(-0.504684438554311,-1.88797463520856,
1.77178053121678));
#277230=CARTESIAN_POINT('Ctrl Pts',(-0.53567717040266,-1.87913968855681,
1.76993163201366));
#277231=CARTESIAN_POINT('Ctrl Pts',(-0.601355806447537,-1.86041700065518,
1.76601351410009));
#277232=CARTESIAN_POINT('Ctrl Pts',(-0.666181878691961,-1.8382097089528,
1.76209539618651));
#277233=CARTESIAN_POINT('Ctrl Pts',(-0.729759099842181,-1.81261348781187,
1.75817727827294));
#277234=CARTESIAN_POINT('Ctrl Pts',(-0.793240584466634,-1.78705581024427,
1.75426506038126));
#277235=CARTESIAN_POINT('Ctrl Pts',(-0.855476497621202,-1.75811951341578,
1.75035284248957));
#277236=CARTESIAN_POINT('Ctrl Pts',(-0.916085061160763,-1.72595021965238,
1.74644062459789));
#277237=CARTESIAN_POINT('Ctrl Pts',(-0.976622352896508,-1.693818754926,
1.74253300722484));
#277238=CARTESIAN_POINT('Ctrl Pts',(-1.03553566315849,-1.65846207320843,
1.7386253898518));
#277239=CARTESIAN_POINT('Ctrl Pts',(-1.09246427829761,-1.62007339359786,
1.73471777247875));
#277240=CARTESIAN_POINT('Ctrl Pts',(-1.1493572130075,-1.58170877437524,
1.7308126042337));
#277241=CARTESIAN_POINT('Ctrl Pts',(-1.20426751323631,-1.54031620129325,
1.72690743598865));
#277242=CARTESIAN_POINT('Ctrl Pts',(-1.25686148103153,-1.49613342235886,
1.7230022677436));
#277243=CARTESIAN_POINT('Ctrl Pts',(-1.30944052400483,-1.45196318136628,
1.71909820768534));
#277244=CARTESIAN_POINT('Ctrl Pts',(-1.35970416298529,-1.40500462259933,
1.71519414762709));
#277245=CARTESIAN_POINT('Ctrl Pts',(-1.40735141751415,-1.35553605175993,
1.71129008756883));
#277246=CARTESIAN_POINT('Ctrl Pts',(-1.45500149265431,-1.30606455249137,
1.70738579639892));
#277247=CARTESIAN_POINT('Ctrl Pts',(-1.50003453646376,-1.25408310220287,
1.70348150522901));
#277248=CARTESIAN_POINT('Ctrl Pts',(-1.54218739149781,-1.19990585026708,
1.6995772140591));
#277249=CARTESIAN_POINT('Ctrl Pts',(-1.58438514589974,-1.14567089110451,
1.69566876420989));
#277250=CARTESIAN_POINT('Ctrl Pts',(-1.6236962864148,-1.08923585159076,
1.69176031436068));
#277251=CARTESIAN_POINT('Ctrl Pts',(-1.65989946598296,-1.03094605233712,
1.68785186451148));
#277252=CARTESIAN_POINT('Ctrl Pts',(-1.69612431557922,-0.97262136273397,
1.68394107519322));
#277253=CARTESIAN_POINT('Ctrl Pts',(-1.72923726469211,-0.912440134903767,
1.68003028587496));
#277254=CARTESIAN_POINT('Ctrl Pts',(-1.7590630335812,-0.850772145693606,
1.6761194965567));
#277255=CARTESIAN_POINT('Ctrl Pts',(-1.78894030180151,-0.788997676070033,
1.67220195458656));
#277256=CARTESIAN_POINT('Ctrl Pts',(-1.81551887123367,-0.725731774693214,
1.66828441261642));
#277257=CARTESIAN_POINT('Ctrl Pts',(-1.83867199814743,-0.661363200691231,
1.66436687064629));
#277258=CARTESIAN_POINT('Ctrl Pts',(-1.84959914674408,-0.63098436781505,
1.66251798157827));
#277259=CARTESIAN_POINT('Ctrl Pts',(-1.85976404653653,-0.600360129903417,
1.66066909251025));
#277260=CARTESIAN_POINT('Ctrl Pts',(-1.86915731446041,-0.569532206112297,
1.65882020344223));
#277261=CARTESIAN_POINT('Ctrl Pts',(-1.8935023589502,-0.489633795643859,
1.65402833686476));
#277262=CARTESIAN_POINT('Ctrl Pts',(-1.9127392853033,-0.408111000000661,
1.6492364702873));
#277263=CARTESIAN_POINT('Ctrl Pts',(-1.92668893233299,-0.325554539248911,
1.64444460370984));
#277264=CARTESIAN_POINT('Ctrl Pts',(-1.94044092837958,-0.244167811723697,
1.63972063255209));
#277265=CARTESIAN_POINT('Ctrl Pts',(-1.9490543683818,-0.161776482890145,
1.63499666139434));
#277266=CARTESIAN_POINT('Ctrl Pts',(-1.95240368494034,-0.0789674048668311,
1.63027269023658));
#277267=CARTESIAN_POINT('Ctrl Pts',(-1.9534442621557,-0.0532399950175315,
1.62880503059113));
#277268=CARTESIAN_POINT('Ctrl Pts',(-1.95397706656825,-0.0274724170513964,
1.62733737094568));
#277269=CARTESIAN_POINT('Ctrl Pts',(-1.95399927547201,-0.00168269273987639,
1.62586971130023));
#277270=CARTESIAN_POINT('',(-1.95128155810217,0.000979544143981243,0.92586969212423));
#277271=CARTESIAN_POINT('Ctrl Pts',(-1.95279584397335,-0.00168131964740442,
1.62586969212423));
#277272=CARTESIAN_POINT('Ctrl Pts',(-1.94903635596163,0.455855006369031,
1.59981605303975));
#277273=CARTESIAN_POINT('Ctrl Pts',(-1.5604097983178,1.56956480808681,1.53672527109813));
#277274=CARTESIAN_POINT('Ctrl Pts',(0.295037094833478,2.29041656967945,
1.43659734629937));
#277275=CARTESIAN_POINT('Ctrl Pts',(2.08408386827561,0.994813055513272,
1.32548591772794));
#277276=CARTESIAN_POINT('Ctrl Pts',(1.96637633306231,-1.2109595884189,1.21437448915651));
#277277=CARTESIAN_POINT('Ctrl Pts',(0.0496077971367581,-2.30880576088663,
1.10326306058507));
#277278=CARTESIAN_POINT('Ctrl Pts',(-1.64866235520027,-1.43074427962715,
1.00709479490765));
#277279=CARTESIAN_POINT('Ctrl Pts',(-1.94952086313801,-0.387778936703525,
0.94796367208737));
#277280=CARTESIAN_POINT('Ctrl Pts',(-1.95128155810217,0.000979544143981243,
0.92586969212423));
#277281=CARTESIAN_POINT('Ctrl Pts',(-1.95128155810217,0.000979544143981243,
0.92586969212423));
#277282=CARTESIAN_POINT('Ctrl Pts',(-1.95247239613589,0.26391457510812,
0.910926529230228));
#277283=CARTESIAN_POINT('Ctrl Pts',(-1.78053982253993,1.17704879552172,
0.858946223479081));
#277284=CARTESIAN_POINT('Ctrl Pts',(-0.393146886163405,2.27561306770598,
0.769928774870794));
#277285=CARTESIAN_POINT('Ctrl Pts',(1.69830019267039,1.56491440632532,0.658817346299364));
#277286=CARTESIAN_POINT('Ctrl Pts',(2.23593132308835,-0.577660774765208,
0.547705917727936));
#277287=CARTESIAN_POINT('Ctrl Pts',(0.727920063175579,-2.19150414145949,
0.436594489156507));
#277288=CARTESIAN_POINT('Ctrl Pts',(-1.37114873684965,-1.8142179137927,
0.329316074498916));
#277289=CARTESIAN_POINT('Ctrl Pts',(-1.95230321089235,-0.579086516543689,
0.259074802698467));
#277290=CARTESIAN_POINT('Ctrl Pts',(-1.95633516444562,0.00125643977877596,
0.225870673755162));
#277291=CARTESIAN_POINT('Origin',(0.,0.,-1.29405622560371));
#277292=CARTESIAN_POINT('',(-1.5554991203045,0.00165430708296759,19.3559437744328));
#277293=CARTESIAN_POINT('Ctrl Pts',(1.43457668357356,0.601306900797836,
19.0501843444911));
#277294=CARTESIAN_POINT('Ctrl Pts',(1.41216525140568,0.65477530102884,19.0543252140175));
#277295=CARTESIAN_POINT('Ctrl Pts',(1.38675571510824,0.707000646875421,
19.0584660835438));
#277296=CARTESIAN_POINT('Ctrl Pts',(1.35851806141379,0.757633768263079,
19.0626069530701));
#277297=CARTESIAN_POINT('Ctrl Pts',(1.33025588857326,0.808310855091825,
19.0667514181709));
#277298=CARTESIAN_POINT('Ctrl Pts',(1.29916094303211,0.857392499965521,
19.0708958832716));
#277299=CARTESIAN_POINT('Ctrl Pts',(1.26544878283799,0.904554933662872,
19.0750403483724));
#277300=CARTESIAN_POINT('Ctrl Pts',(1.23172305766809,0.951736344407892,
19.0791864811078));
#277301=CARTESIAN_POINT('Ctrl Pts',(1.19537834213245,0.996996597851846,
19.0833326138433));
#277302=CARTESIAN_POINT('Ctrl Pts',(1.15667116469418,1.04004426192591,19.0874787465787));
#277303=CARTESIAN_POINT('Ctrl Pts',(1.11789124042643,1.08317283040286,19.0916326716161));
#277304=CARTESIAN_POINT('Ctrl Pts',(1.07674034965028,1.12408013174388,19.0957865966534));
#277305=CARTESIAN_POINT('Ctrl Pts',(1.03351196134665,1.16251162392185,19.0999405216907));
#277306=CARTESIAN_POINT('Ctrl Pts',(0.994573128000671,1.19712955736511,
19.1036822525557));
#277307=CARTESIAN_POINT('Ctrl Pts',(0.953949324318807,1.229739010674,19.1074239834207));
#277308=CARTESIAN_POINT('Ctrl Pts',(0.911875475596432,1.26018386238111,
19.1111657142858));
#277309=CARTESIAN_POINT('Ctrl Pts',(0.865165552439733,1.29398340121437,
19.1153197426546));
#277310=CARTESIAN_POINT('Ctrl Pts',(0.816478836708566,1.32525119701336,
19.1194737710234));
#277311=CARTESIAN_POINT('Ctrl Pts',(0.766120348130251,1.3537502953576,19.1236277993922));
#277312=CARTESIAN_POINT('Ctrl Pts',(0.715849438396,1.38219983069547,19.1277746034575));
#277313=CARTESIAN_POINT('Ctrl Pts',(0.663912975180353,1.40788997309079,
19.1319214075229));
#277314=CARTESIAN_POINT('Ctrl Pts',(0.610645586257866,1.4306265124007,19.1360682115882));
#277315=CARTESIAN_POINT('Ctrl Pts',(0.557429987971653,1.45334094550527,
19.140210983813));
#277316=CARTESIAN_POINT('Ctrl Pts',(0.502886503168866,1.47310726328047,
19.1443537560377));
#277317=CARTESIAN_POINT('Ctrl Pts',(0.447373486568487,1.48977757182593,
19.1484965282625));
#277318=CARTESIAN_POINT('Ctrl Pts',(0.391893291858678,1.50643802410566,
19.1526368510866));
#277319=CARTESIAN_POINT('Ctrl Pts',(0.335445197875963,1.52000594727083,
19.1567771739108));
#277320=CARTESIAN_POINT('Ctrl Pts',(0.278404563902768,1.53038268050776,
19.1609174967349));
#277321=CARTESIAN_POINT('Ctrl Pts',(0.22137592216974,1.54075723213715,19.1650569490964));
#277322=CARTESIAN_POINT('Ctrl Pts',(0.163755498144067,1.54794183323517,
19.1691964014578));
#277323=CARTESIAN_POINT('Ctrl Pts',(0.10592858108544,1.55188897338348,19.1733358538192));
#277324=CARTESIAN_POINT('Ctrl Pts',(0.0480488391534791,1.55583971924327,
19.1774790875693));
#277325=CARTESIAN_POINT('Ctrl Pts',(-0.0100372538376572,1.55654705787194,
19.1816223213193));
#277326=CARTESIAN_POINT('Ctrl Pts',(-0.0679408912885707,1.55401553573023,
19.1857655550694));
#277327=CARTESIAN_POINT('Ctrl Pts',(-0.12586890829889,1.55148294772466,
19.1899105332731));
#277328=CARTESIAN_POINT('Ctrl Pts',(-0.183613799011935,1.54570883074677,
19.1940555114768));
#277329=CARTESIAN_POINT('Ctrl Pts',(-0.240791598067284,1.53674970515703,
19.1982004896806));
#277330=CARTESIAN_POINT('Ctrl Pts',(-0.298080326888325,1.52777319810596,
19.2023535094926));
#277331=CARTESIAN_POINT('Ctrl Pts',(-0.354799255932419,1.51559944214355,
19.2065065293045));
#277332=CARTESIAN_POINT('Ctrl Pts',(-0.410575232362685,1.50033603854947,
19.2106595491165));
#277333=CARTESIAN_POINT('Ctrl Pts',(-0.462584185204256,1.48610350173825,
19.2145320803634));
#277334=CARTESIAN_POINT('Ctrl Pts',(-0.513773077525469,1.46918519379234,
19.2184046116103));
#277335=CARTESIAN_POINT('Ctrl Pts',(-0.563855216483735,1.4497060201448,
19.2222771428572));
#277336=CARTESIAN_POINT('Ctrl Pts',(-0.616912826678665,1.42906955325644,
19.2263797482498));
#277337=CARTESIAN_POINT('Ctrl Pts',(-0.668961426240364,1.40546750481788,
19.2304823536425));
#277338=CARTESIAN_POINT('Ctrl Pts',(-0.719642355782659,1.37901962631559,
19.2345849590351));
#277339=CARTESIAN_POINT('Ctrl Pts',(-0.77049884857814,1.35248013000692,
19.2387017762182));
#277340=CARTESIAN_POINT('Ctrl Pts',(-0.819977650252828,1.32307518099454,
19.2428185934012));
#277341=CARTESIAN_POINT('Ctrl Pts',(-0.867733843715434,1.29097568779231,
19.2469354105843));
#277342=CARTESIAN_POINT('Ctrl Pts',(-0.915193225731834,1.25907569744635,
19.2510266411707));
#277343=CARTESIAN_POINT('Ctrl Pts',(-0.960950890138361,1.22451483889158,
19.255117871757));
#277344=CARTESIAN_POINT('Ctrl Pts',(-1.00469287591273,1.18750683159728,
19.2592091023434));
#277345=CARTESIAN_POINT('Ctrl Pts',(-1.04840932105716,1.15052043301146,
19.2632979440897));
#277346=CARTESIAN_POINT('Ctrl Pts',(-1.09011201223326,1.11109005909351,
19.2673867858361));
#277347=CARTESIAN_POINT('Ctrl Pts',(-1.1295188048071,1.06947067261666,19.2714756275824));
#277348=CARTESIAN_POINT('Ctrl Pts',(-1.16891852586963,1.02785875469899,
19.27556373559));
#277349=CARTESIAN_POINT('Ctrl Pts',(-1.20602279940129,0.984058990653992,
19.2796518435976));
#277350=CARTESIAN_POINT('Ctrl Pts',(-1.24058691992718,0.938362586693218,
19.2837399516052));
#277351=CARTESIAN_POINT('Ctrl Pts',(-1.27556766726258,0.892115370309084,
19.2878773365905));
#277352=CARTESIAN_POINT('Ctrl Pts',(-1.30794624959268,0.843925907830145,
19.2920147215758));
#277353=CARTESIAN_POINT('Ctrl Pts',(-1.33751322872518,0.794127579791279,
19.2961521065611));
#277354=CARTESIAN_POINT('Ctrl Pts',(-1.36677378652093,0.744845343375333,
19.3002466132045));
#277355=CARTESIAN_POINT('Ctrl Pts',(-1.39328056462831,0.693987948459924,
19.304341119848));
#277356=CARTESIAN_POINT('Ctrl Pts',(-1.41687753982944,0.641902085311207,
19.3084356264915));
#277357=CARTESIAN_POINT('Ctrl Pts',(-1.44084518209379,0.588998044673036,
19.3125944506477));
#277358=CARTESIAN_POINT('Ctrl Pts',(-1.46181059972095,0.53482713688006,
19.3167532748039));
#277359=CARTESIAN_POINT('Ctrl Pts',(-1.47966264316261,0.479769436739197,
19.32091209896));
#277360=CARTESIAN_POINT('Ctrl Pts',(-1.49751468660427,0.424711736598334,
19.3250709231162));
#277361=CARTESIAN_POINT('Ctrl Pts',(-1.51225329463471,0.36876781285147,
19.3292297472724));
#277362=CARTESIAN_POINT('Ctrl Pts',(-1.52382169500351,0.312326258640937,
19.3333885714286));
#277363=CARTESIAN_POINT('Ctrl Pts',(-1.54270018455889,0.220219203414235,
19.3401753626783));
#277364=CARTESIAN_POINT('Ctrl Pts',(-1.55321832214834,0.126427694770151,
19.346962153928));
#277365=CARTESIAN_POINT('Ctrl Pts',(-1.55516758360058,0.0321564444232205,
19.3537489451776));
#277366=CARTESIAN_POINT('Ctrl Pts',(-1.55537771215927,0.021994091939033,
19.3544805549172));
#277367=CARTESIAN_POINT('Ctrl Pts',(-1.55548830227265,0.0118261996198327,
19.3552121646567));
#277368=CARTESIAN_POINT('Ctrl Pts',(-1.55549912030396,0.00165430758992738,
19.3559437743963));
#277369=CARTESIAN_POINT('Ctrl Pts',(-1.5554991203045,0.00165430708298941,
19.3559437744328));
#277370=CARTESIAN_POINT('Ctrl Pts',(-1.55556084030585,-0.056379300333557,
19.3601178211375));
#277371=CARTESIAN_POINT('Ctrl Pts',(-1.55237061563408,-0.114519110625628,
19.3642918678422));
#277372=CARTESIAN_POINT('Ctrl Pts',(-1.54591951792332,-0.172374865057931,
19.3684659145469));
#277373=CARTESIAN_POINT('Ctrl Pts',(-1.53947673878304,-0.230156015571265,
19.372634578896));
#277374=CARTESIAN_POINT('Ctrl Pts',(-1.52978148020292,-0.287653331891395,
19.3768032432451));
#277375=CARTESIAN_POINT('Ctrl Pts',(-1.51687679201396,-0.344477935214204,
19.3809719075943));
#277376=CARTESIAN_POINT('Ctrl Pts',(-1.5039840172698,-0.401250078782456,
19.3851367234852));
#277377=CARTESIAN_POINT('Ctrl Pts',(-1.48788780344455,-0.457350244605693,
19.3893015393762));
#277378=CARTESIAN_POINT('Ctrl Pts',(-1.46868254079216,-0.512398130726777,
19.3934663552672));
#277379=CARTESIAN_POINT('Ctrl Pts',(-1.44907153883229,-0.568608984082246,
19.3977191589949));
#277380=CARTESIAN_POINT('Ctrl Pts',(-1.4262186995935,-0.62372204056427,
19.4019719627227));
#277381=CARTESIAN_POINT('Ctrl Pts',(-1.40027824131161,-0.67734857858363,
19.4062247664504));
#277382=CARTESIAN_POINT('Ctrl Pts',(-1.37488544150799,-0.729842945849225,
19.4103877844082));
#277383=CARTESIAN_POINT('Ctrl Pts',(-1.34653441421956,-0.7809125017701,
19.4145508023661));
#277384=CARTESIAN_POINT('Ctrl Pts',(-1.31541745783214,-0.830215129728687,
19.418713820324));
#277385=CARTESIAN_POINT('Ctrl Pts',(-1.28329383035402,-0.881112757199572,
19.4230115169366));
#277386=CARTESIAN_POINT('Ctrl Pts',(-1.2482224869797,-0.9301266417569,19.4273092135493));
#277387=CARTESIAN_POINT('Ctrl Pts',(-1.21046337906679,-0.976912820029617,
19.431606910162));
#277388=CARTESIAN_POINT('Ctrl Pts',(-1.17270427115388,-1.02369899830233,
19.4359046067747));
#277389=CARTESIAN_POINT('Ctrl Pts',(-1.1322578120547,-1.06825703820874,
19.4402023033873));
#277390=CARTESIAN_POINT('Ctrl Pts',(-1.08942750315405,-1.11028283125136,
19.4445));
#277391=CARTESIAN_POINT('Ctrl Pts',(1.43457668357355,0.601306900797844,
19.188224604057));
#277392=CARTESIAN_POINT('Ctrl Pts',(1.41216743227266,0.654770097993729,
19.1923698776825));
#277393=CARTESIAN_POINT('Ctrl Pts',(1.38678365308771,0.706935688811212,
19.196515151308));
#277394=CARTESIAN_POINT('Ctrl Pts',(1.35861269545265,0.757464054430887,
19.2006604249335));
#277395=CARTESIAN_POINT('Ctrl Pts',(1.33038896676601,0.808087071962046,
19.2048134636641));
#277396=CARTESIAN_POINT('Ctrl Pts',(1.29936790941001,0.857066299073572,
19.2089665023947));
#277397=CARTESIAN_POINT('Ctrl Pts',(1.26578076354097,0.904090321068441,
19.2131195411254));
#277398=CARTESIAN_POINT('Ctrl Pts',(1.24133295867943,0.938318716598623,
19.2161425035666));
#277399=CARTESIAN_POINT('Ctrl Pts',(1.21552649144371,0.971511806329961,
19.2191654660078));
#277400=CARTESIAN_POINT('Ctrl Pts',(1.18846325072905,1.00356133428233,19.222188428449));
#277401=CARTESIAN_POINT('Ctrl Pts',(1.1517364653547,1.04705487398317,19.2262908082764));
#277402=CARTESIAN_POINT('Ctrl Pts',(1.11253187745988,1.08863250047883,19.2303931881038));
#277403=CARTESIAN_POINT('Ctrl Pts',(1.07107902497437,1.12799378201298,19.2344955679313));
#277404=CARTESIAN_POINT('Ctrl Pts',(1.0294613286051,1.16751158996519,19.2386142615268));
#277405=CARTESIAN_POINT('Ctrl Pts',(0.985577740531738,1.20479492777059,
19.2427329551224));
#277406=CARTESIAN_POINT('Ctrl Pts',(0.939702167676443,1.2395725416708,19.2468516487179));
#277407=CARTESIAN_POINT('Ctrl Pts',(0.894135131767176,1.27411625813681,
19.2509426419696));
#277408=CARTESIAN_POINT('Ctrl Pts',(0.846603236937218,1.30618750689656,
19.2550336352213));
#277409=CARTESIAN_POINT('Ctrl Pts',(0.797410439026016,1.33555862534459,
19.2591246284729));
#277410=CARTESIAN_POINT('Ctrl Pts',(0.748246399707,1.36491257314868,19.2632132300898));
#277411=CARTESIAN_POINT('Ctrl Pts',(0.697423837101224,1.39156924397987,
19.2673018317067));
#277412=CARTESIAN_POINT('Ctrl Pts',(0.645275403958348,1.41534444678544,
19.2713904333236));
#277413=CARTESIAN_POINT('Ctrl Pts',(0.593136361375232,1.43911536830298,
19.275478298691));
#277414=CARTESIAN_POINT('Ctrl Pts',(0.539672406972039,1.4600056302342,19.2795661640584));
#277415=CARTESIAN_POINT('Ctrl Pts',(0.485238336597361,1.47787821104996,
19.2836540294258));
#277416=CARTESIAN_POINT('Ctrl Pts',(0.430098739008545,1.49598244075887,
19.287794878159));
#277417=CARTESIAN_POINT('Ctrl Pts',(0.373964217362291,1.51098999177411,
19.2919357268923));
#277418=CARTESIAN_POINT('Ctrl Pts',(0.317219060538567,1.5228106637501,19.2960765756255));
#277419=CARTESIAN_POINT('Ctrl Pts',(0.261112250559756,1.53449836070086,
19.3001708424498));
#277420=CARTESIAN_POINT('Ctrl Pts',(0.2044090212878,1.54307051340458,19.3042651092742));
#277421=CARTESIAN_POINT('Ctrl Pts',(0.147487896314991,1.54849203111949,
19.3083593760985));
#277422=CARTESIAN_POINT('Ctrl Pts',(0.0895953539540989,1.55400607259568,
19.3125235157862));
#277423=CARTESIAN_POINT('Ctrl Pts',(0.0314779830049255,1.55626090059159,
19.3166876554739));
#277424=CARTESIAN_POINT('Ctrl Pts',(-0.0264670923239539,1.55527481270157,
19.3208517951615));
#277425=CARTESIAN_POINT('Ctrl Pts',(-0.0844121676528332,1.55428872481156,
19.3250159348492));
#277426=CARTESIAN_POINT('Ctrl Pts',(-0.142184385757248,1.55006184865992,
19.3291800745368));
#277427=CARTESIAN_POINT('Ctrl Pts',(-0.199396272421212,1.54266696877341,
19.3333442142245));
#277428=CARTESIAN_POINT('Ctrl Pts',(-0.257983830795176,1.53509427746251,
19.3376084815167));
#277429=CARTESIAN_POINT('Ctrl Pts',(-0.316239637736243,1.52416678472547,
19.341872748809));
#277430=CARTESIAN_POINT('Ctrl Pts',(-0.373762636432102,1.50992772727946,
19.3461370161012));
#277431=CARTESIAN_POINT('Ctrl Pts',(-0.431161723190074,1.49571934259465,
19.3503920976132));
#277432=CARTESIAN_POINT('Ctrl Pts',(-0.487830672928362,1.47821369472334,
19.3546471791252));
#277433=CARTESIAN_POINT('Ctrl Pts',(-0.543377082667122,1.45750526449552,
19.3589022606373));
#277434=CARTESIAN_POINT('Ctrl Pts',(-0.59885268524449,1.43682323210635,
19.3631519180319));
#277435=CARTESIAN_POINT('Ctrl Pts',(-0.653208136621592,1.41294669183088,
19.3674015754266));
#277436=CARTESIAN_POINT('Ctrl Pts',(-0.706065742672148,1.38601999156752,
19.3716512328213));
#277437=CARTESIAN_POINT('Ctrl Pts',(-0.75887202062975,1.35911943884049,
19.3758967635287));
#277438=CARTESIAN_POINT('Ctrl Pts',(-0.810182910949864,1.32917482829704,
19.3801422942362));
#277439=CARTESIAN_POINT('Ctrl Pts',(-0.859641922762942,1.29637803692767,
19.3843878249436));
#277440=CARTESIAN_POINT('Ctrl Pts',(-0.909067905774261,1.26360314730443,
19.3886305204793));
#277441=CARTESIAN_POINT('Ctrl Pts',(-0.956644063784778,1.22798012937832,
19.392873216015));
#277442=CARTESIAN_POINT('Ctrl Pts',(-1.00204122892994,1.18974519352867,
19.3971159115506));
#277443=CARTESIAN_POINT('Ctrl Pts',(-1.04743549440577,1.15151269987273,
19.4013583360911));
#277444=CARTESIAN_POINT('Ctrl Pts',(-1.0906506639901,1.11066892264387,19.4056007606316));
#277445=CARTESIAN_POINT('Ctrl Pts',(-1.13139026211381,1.06749066731005,
19.4098431851721));
#277446=CARTESIAN_POINT('Ctrl Pts',(-1.17212552180437,1.02431701010636,
19.4140851579292));
#277447=CARTESIAN_POINT('Ctrl Pts',(-1.21038540545579,0.978809726755231,
19.4183271306862));
#277448=CARTESIAN_POINT('Ctrl Pts',(-1.24591151176093,0.931281243696875,
19.4225691034433));
#277449=CARTESIAN_POINT('Ctrl Pts',(-1.28146386078651,0.883717651902334,
19.4268142096961));
#277450=CARTESIAN_POINT('Ctrl Pts',(-1.31427811083376,0.834130270116786,
19.431059315949));
#277451=CARTESIAN_POINT('Ctrl Pts',(-1.34413794171349,0.782862340163462,
19.4353044222019));
#277452=CARTESIAN_POINT('Ctrl Pts',(-1.36569832846932,0.745844166737887,
19.4383696148012));
#277453=CARTESIAN_POINT('Ctrl Pts',(-1.38571928238916,0.707950473050287,
19.4414348074006));
#277454=CARTESIAN_POINT('Ctrl Pts',(-1.40413430885519,0.669318379170746,
19.4445));
#277455=CARTESIAN_POINT('Origin',(0.,0.,19.5));
#277456=CARTESIAN_POINT('Ctrl Pts',(-1.47185199869187,1.28247177392349,
19.0478006871829));
#277457=CARTESIAN_POINT('Ctrl Pts',(-1.51144177862091,1.22242094713282,
19.057401752771));
#277458=CARTESIAN_POINT('Ctrl Pts',(-1.54765772157622,1.16040792388231,
19.0669290794631));
#277459=CARTESIAN_POINT('Ctrl Pts',(-1.58029338748837,1.09674732240684,
19.0764143170251));
#277460=CARTESIAN_POINT('Ctrl Pts',(-1.61209525197559,1.03471317158705,
19.0856572183462));
#277461=CARTESIAN_POINT('Ctrl Pts',(-1.64049721800471,0.971114777397238,
19.0948602908743));
#277462=CARTESIAN_POINT('Ctrl Pts',(-1.66529723976271,0.906247628640641,
19.1040834245205));
#277463=CARTESIAN_POINT('Ctrl Pts',(-1.68190479772454,0.862808758170836,
19.110259779046));
#277464=CARTESIAN_POINT('Ctrl Pts',(-1.69689691388732,0.818801033375964,
19.1164457635402));
#277465=CARTESIAN_POINT('Ctrl Pts',(-1.71021021312761,0.774313234575083,
19.1226667961376));
#277466=CARTESIAN_POINT('Ctrl Pts',(-1.7216141158004,0.736205886539485,
19.1279956067491));
#277467=CARTESIAN_POINT('Ctrl Pts',(-1.73178621748778,0.697746318117437,
19.133350240274));
#277468=CARTESIAN_POINT('Ctrl Pts',(-1.74068496568679,0.658989750956657,
19.1387499787417));
#277469=CARTESIAN_POINT('Ctrl Pts',(-1.7432210526171,0.647944374546164,
19.1402888700384));
#277470=CARTESIAN_POINT('Ctrl Pts',(-1.74565316923663,0.636876891220236,
19.1418311622824));
#277471=CARTESIAN_POINT('Ctrl Pts',(-1.74797838874301,0.625799357894018,
19.1433758366721));
#277472=CARTESIAN_POINT('Ctrl Pts',(-1.76164806252324,0.560675929141002,
19.1524567836303));
#277473=CARTESIAN_POINT('Ctrl Pts',(-1.77165033127344,0.495102739838834,
19.1616335477411));
#277474=CARTESIAN_POINT('Ctrl Pts',(-1.77788723803438,0.429303598977395,
19.171015415248));
#277475=CARTESIAN_POINT('Ctrl Pts',(-1.77990435472474,0.40802309081357,
19.174049663195));
#277476=CARTESIAN_POINT('Ctrl Pts',(-1.78152735810959,0.386718695885184,
19.1771054696483));
#277477=CARTESIAN_POINT('Ctrl Pts',(-1.782752068437,0.365397267570637,19.1801867951176));
#277478=CARTESIAN_POINT('Ctrl Pts',(-1.78664149044997,0.297684902631543,
19.1899724357224));
#277479=CARTESIAN_POINT('Ctrl Pts',(-1.78651848057804,0.229795248329717,
19.2000151467373));
#277480=CARTESIAN_POINT('Ctrl Pts',(-1.78241468021328,0.161998904792477,
19.2102386367469));
#277481=CARTESIAN_POINT('Ctrl Pts',(-1.77917700700339,0.108511311418388,
19.2183044091465));
#277482=CARTESIAN_POINT('Ctrl Pts',(-1.77345979502346,0.0550827527395637,
19.2264826262492));
#277483=CARTESIAN_POINT('Ctrl Pts',(-1.76525906565932,0.00187739191350949,
19.2347399360171));
#277484=CARTESIAN_POINT('Ctrl Pts',(1.13606316703866,-1.59291762710367,
-0.2315727930662));
#277485=CARTESIAN_POINT('Ctrl Pts',(1.66580206489195,-1.21512977859719,
-0.19452378898432));
#277486=CARTESIAN_POINT('Ctrl Pts',(2.30945033465884,0.103704944516998,
-0.120437642045298));
#277487=CARTESIAN_POINT('Ctrl Pts',(1.16340190037011,2.00012615618488,-0.00931435224913369));
#277488=CARTESIAN_POINT('Ctrl Pts',(-1.04789748215315,2.06050089268765,
0.101797076322295));
#277489=CARTESIAN_POINT('Ctrl Pts',(-2.29995644073094,0.238662326668711,
0.212908504893725));
#277490=CARTESIAN_POINT('Ctrl Pts',(-1.4480231663316,-1.80307307028203,
0.324019933465153));
#277491=CARTESIAN_POINT('Ctrl Pts',(0.72886412800377,-2.19434637934446,
0.435131362036582));
#277492=CARTESIAN_POINT('Ctrl Pts',(2.23883118012918,-0.578409963100118,
0.546242790608011));
#277493=CARTESIAN_POINT('Ctrl Pts',(1.70050277721327,1.56694399820618,0.657354219179439));
#277494=CARTESIAN_POINT('Ctrl Pts',(-0.393656772023556,2.27856438938052,
0.768465647750868));
#277495=CARTESIAN_POINT('Ctrl Pts',(-2.12764424093886,0.905559934895846,
0.879577076322298));
#277496=CARTESIAN_POINT('Ctrl Pts',(-1.91502951955452,-1.29598480721124,
0.990688504893724));
#277497=CARTESIAN_POINT('Ctrl Pts',(0.0496721352129712,-2.31180013131849,
1.10179993346515));
#277498=CARTESIAN_POINT('Ctrl Pts',(1.96892659486843,-1.2125301239951,1.21291136203658));
#277499=CARTESIAN_POINT('Ctrl Pts',(2.08678678907498,0.996103263138911,
1.32402279060801));
#277500=CARTESIAN_POINT('Ctrl Pts',(0.295419738695494,2.29338709053012,
1.43513421917944));
#277501=CARTESIAN_POINT('Ctrl Pts',(-1.76623022736053,1.49242425224886,
1.54624564775086));
#277502=CARTESIAN_POINT('Ctrl Pts',(-2.21193462336081,-0.673976513940082,
1.6573570763223));
#277503=CARTESIAN_POINT('Ctrl Pts',(-0.633912852843943,-2.22374754587002,
1.76846850489372));
#277504=CARTESIAN_POINT('Ctrl Pts',(1.52408352559897,-1.73898487447381,
1.87957993346515));
#277505=CARTESIAN_POINT('Ctrl Pts',(2.28767721897072,0.336796477013934,
1.99069136203658));
#277506=CARTESIAN_POINT('Ctrl Pts',(0.95824696965368,2.1044385505715,2.10180279060801));
#277507=CARTESIAN_POINT('Ctrl Pts',(-1.24789517519063,1.94670402200824,
2.21291421917944));
#277508=CARTESIAN_POINT('Ctrl Pts',(-2.31232272803813,0.00790610348200404,
2.32402564775087));
#277509=CARTESIAN_POINT('Ctrl Pts',(-1.26117786751997,-1.93812519847901,
2.4351370763223));
#277510=CARTESIAN_POINT('Ctrl Pts',(0.943834084851752,-2.11094199967052,
2.54624850489373));
#277511=CARTESIAN_POINT('Ctrl Pts',(2.28532066231724,-0.352432083948816,
2.65735993346515));
#277512=CARTESIAN_POINT('Ctrl Pts',(1.53593934849974,1.72852226495878,2.76847136203658));
#277513=CARTESIAN_POINT('Ctrl Pts',(-0.618691705176725,2.22803040322512,
2.87958279060801));
#277514=CARTESIAN_POINT('Ctrl Pts',(-2.20727413292089,0.689086210494794,
2.99069421917944));
#277515=CARTESIAN_POINT('Ctrl Pts',(-1.77639439610933,-1.48031140398554,
3.10180564775087));
#277516=CARTESIAN_POINT('Ctrl Pts',(0.279730351589628,-2.29535396700367,
3.21291707632229));
#277517=CARTESIAN_POINT('Ctrl Pts',(2.07992637124202,-1.01034904542294,
3.32402850489373));
#277518=CARTESIAN_POINT('Ctrl Pts',(1.97717225475611,1.19903660427677,3.43513993346515));
#277519=CARTESIAN_POINT('Ctrl Pts',(0.0654790030363215,2.31140896501537,
3.54625136203659));
#277520=CARTESIAN_POINT('Ctrl Pts',(-1.90612179130951,1.30904492668386,
3.65736279060801));
#277521=CARTESIAN_POINT('Ctrl Pts',(-2.13378839047699,-0.890980363446882,
3.76847421917944));
#277522=CARTESIAN_POINT('Ctrl Pts',(-0.409225831785102,-2.27583679599057,
3.87958564775087));
#277523=CARTESIAN_POINT('Ctrl Pts',(1.68974245735601,-1.57850224301131,
3.9906970763223));
#277524=CARTESIAN_POINT('Ctrl Pts',(2.24274465667945,0.563023363919505,
4.10180850489373));
#277525=CARTESIAN_POINT('Ctrl Pts',(0.743832274433361,2.18943199275407,
4.21291993346515));
#277526=CARTESIAN_POINT('Ctrl Pts',(-1.43562137478499,1.8127024498367,4.32403136203659));
#277527=CARTESIAN_POINT('Ctrl Pts',(-2.30160742805521,-0.222490787460244,
4.43514279060801));
#277528=CARTESIAN_POINT('Ctrl Pts',(-1.06182462858958,-2.0541244756597,
4.54625421917945));
#277529=CARTESIAN_POINT('Ctrl Pts',(1.14943454112788,-2.00641449831427,
4.65736564775087));
#277530=CARTESIAN_POINT('Ctrl Pts',(2.30906195754891,-0.123011298603022,
4.7684770763223));
#277531=CARTESIAN_POINT('Ctrl Pts',(1.35610028081068,1.87293644627061,4.87958850489373));
#277532=CARTESIAN_POINT('Ctrl Pts',(-0.837574168101038,2.15531167498194,
4.99069993346516));
#277533=CARTESIAN_POINT('Ctrl Pts',(-2.26494174228494,0.465765828972943,
5.10181136203659));
#277534=CARTESIAN_POINT('Ctrl Pts',(-1.6200863491512,-1.64991488407055,
5.21292279060802));
#277535=CARTESIAN_POINT('Ctrl Pts',(0.507005906446861,-2.25606824236582,
5.32403421917943));
#277536=CARTESIAN_POINT('Ctrl Pts',(2.17023224254229,-0.798117107205096,
5.43514564775089));
#277537=CARTESIAN_POINT('Ctrl Pts',(1.84788649373611,1.39004115394159,5.54625707632229));
#277538=CARTESIAN_POINT('Ctrl Pts',(-0.16511326255594,2.30643372198547,
5.65736850489374));
#277539=CARTESIAN_POINT('Ctrl Pts',(-2.02704887071144,1.11264180180822,
5.76847993346515));
#277540=CARTESIAN_POINT('Ctrl Pts',(-2.0344126162256,-1.09911974339729,
5.87959136203659));
#277541=CARTESIAN_POINT('Ctrl Pts',(-0.180467318050853,-2.30528316058985,
5.99070279060801));
#277542=CARTESIAN_POINT('Ctrl Pts',(1.83858974186744,-1.40231475228758,
6.10181421917945));
#277543=CARTESIAN_POINT('Ctrl Pts',(2.17549850655909,0.783648614713761,
6.21292564775089));
#277544=CARTESIAN_POINT('Ctrl Pts',(0.522017016837799,2.25264225688753,
6.3240370763223));
#277545=CARTESIAN_POINT('Ctrl Pts',(-1.60906424131313,1.66066588172064,
6.43514850489373));
#277546=CARTESIAN_POINT('Ctrl Pts',(-2.26799289858753,-0.450674067747575,
6.54625993346516));
#277547=CARTESIAN_POINT('Ctrl Pts',(-0.851907048237055,-2.14968678754548,
6.65737136203658));
#277548=CARTESIAN_POINT('Ctrl Pts',(1.34359900459318,-1.88192471109761,
6.76848279060803));
#277549=CARTESIAN_POINT('Ctrl Pts',(2.30982985612209,0.107633355195401,
6.87959421917944));
#277550=CARTESIAN_POINT('Ctrl Pts',(1.16276905467301,1.99871634527724,6.99070564775088));
#277551=CARTESIAN_POINT('Ctrl Pts',(-1.04812340999086,2.06114924758318,
7.10181707632231));
#277552=CARTESIAN_POINT('Ctrl Pts',(-2.30007491727047,0.237811434390506,
7.21292850489373));
#277553=CARTESIAN_POINT('Ctrl Pts',(-1.44765968471916,-1.80310297560135,
7.32403993346517));
#277554=CARTESIAN_POINT('Ctrl Pts',(0.729237141124034,-2.19433636787728,
7.43515136203658));
#277555=CARTESIAN_POINT('Ctrl Pts',(2.23894596639031,-0.577944515475454,
7.54626279060803));
#277556=CARTESIAN_POINT('Ctrl Pts',(1.700215678403,1.5672158595089,7.65737421917944));
#277557=CARTESIAN_POINT('Ctrl Pts',(-0.39406277773538,2.27851123117423,
7.76848564775089));
#277558=CARTESIAN_POINT('Ctrl Pts',(-2.12780836746792,0.905168743780466,
7.8795970763223));
#277559=CARTESIAN_POINT('Ctrl Pts',(-1.91479599570453,-1.2963237243133,
7.99070850489374));
#277560=CARTESIAN_POINT('Ctrl Pts',(0.0500867071799966,-2.31179372461027,
8.10181993346516));
#277561=CARTESIAN_POINT('Ctrl Pts',(1.96914446762206,-1.21217530457315,
8.2129313620366));
#277562=CARTESIAN_POINT('Ctrl Pts',(2.08660781369462,0.996477162413753,
8.32404279060801));
#277563=CARTESIAN_POINT('Ctrl Pts',(0.295008090021127,2.29344045708749,
8.43515421917946));
#277564=CARTESIAN_POINT('Ctrl Pts',(-1.76649815189665,1.49210696088762,
8.54626564775088));
#277565=CARTESIAN_POINT('Ctrl Pts',(-2.21181357806678,-0.674373486476905,
8.65737707632231));
#277566=CARTESIAN_POINT('Ctrl Pts',(-0.633513645693009,-2.22386136350815,
8.76848850489374));
#277567=CARTESIAN_POINT('Ctrl Pts',(1.52439568775516,-1.73871121539405,
8.87959993346515));
#277568=CARTESIAN_POINT('Ctrl Pts',(2.28761671798039,0.337207139604478,
8.99071136203661));
#277569=CARTESIAN_POINT('Ctrl Pts',(0.957869167637863,2.10461054855105,
9.10182279060801));
#277570=CARTESIAN_POINT('Ctrl Pts',(-1.24824462727842,1.94647996492492,
9.21293421917946));
#277571=CARTESIAN_POINT('Ctrl Pts',(-2.31232410970608,0.0074909983048494,
9.32404564775087));
#277572=CARTESIAN_POINT('Ctrl Pts',(-1.26082991597317,-1.93835157450104,
9.43515707632232));
#277573=CARTESIAN_POINT('Ctrl Pts',(0.944213025165924,-2.11077252836269,
9.54626850489372));
#277574=CARTESIAN_POINT('Ctrl Pts',(2.2853838938978,-0.352021818778507,
9.65737993346518));
#277575=CARTESIAN_POINT('Ctrl Pts',(1.53562902018864,1.72879796845614,9.7684913620366));
#277576=CARTESIAN_POINT('Ctrl Pts',(-0.619091670303133,2.22791929996239,
9.87960279060802));
#277577=CARTESIAN_POINT('Ctrl Pts',(-2.20739780181248,0.688689950512571,
9.99071421917945));
#277578=CARTESIAN_POINT('Ctrl Pts',(-1.77612862260868,-1.480630277731,10.1018256477509));
#277579=CARTESIAN_POINT('Ctrl Pts',(0.280142408063027,-2.29530371292957,
10.2129370763223));
#277580=CARTESIAN_POINT('Ctrl Pts',(2.08010771516136,-1.00997564164182,
10.3240485048938));
#277581=CARTESIAN_POINT('Ctrl Pts',(1.9769569723504,1.19939152609093,10.4351599334652));
#277582=CARTESIAN_POINT('Ctrl Pts',(0.0650640588157258,2.31142068253143,
10.5462713620366));
#277583=CARTESIAN_POINT('Ctrl Pts',(-1.9063567597894,1.30870271940912,10.6573827906081));
#277584=CARTESIAN_POINT('Ctrl Pts',(-2.13362840767391,-0.891363405884791,
10.7684942191795));
#277585=CARTESIAN_POINT('Ctrl Pts',(-0.408817267926587,-2.27591022336749,
10.8796056477509));
#277586=CARTESIAN_POINT('Ctrl Pts',(1.6900258021868,-1.57819887572082,10.9907170763223));
#277587=CARTESIAN_POINT('Ctrl Pts',(2.24264354682321,0.563425971424641,
11.1018285048938));
#277588=CARTESIAN_POINT('Ctrl Pts',(0.743439216537086,2.18956548993136,
11.2129399334652));
#277589=CARTESIAN_POINT('Ctrl Pts',(-1.43594676723325,1.81244469848213,
11.3240513620366));
#277590=CARTESIAN_POINT('Ctrl Pts',(-2.30156744951535,-0.222903967472517,
11.435162790608));
#277591=CARTESIAN_POINT('Ctrl Pts',(-1.06145585591785,-2.05431506087097,
11.5462742191795));
#277592=CARTESIAN_POINT('Ctrl Pts',(1.14979471329312,-2.00620811997828,
11.6573856477509));
#277593=CARTESIAN_POINT('Ctrl Pts',(2.3090840032781,-0.122596774789466,
11.7684970763223));
#277594=CARTESIAN_POINT('Ctrl Pts',(1.35576403019591,1.87317986264281,11.8796085048938));
#277595=CARTESIAN_POINT('Ctrl Pts',(-0.837961075250009,2.15516127928966,
11.9907199334652));
#277596=CARTESIAN_POINT('Ctrl Pts',(-2.26502531987419,0.465359220078858,
12.1018313620366));
#277597=CARTESIAN_POINT('Ctrl Pts',(-1.61979013101972,-1.65020569470438,
12.212942790608));
#277598=CARTESIAN_POINT('Ctrl Pts',(0.507410906699071,-2.25597718852529,
12.3240542191795));
#277599=CARTESIAN_POINT('Ctrl Pts',(2.17037548521933,-0.797727495165182,
12.4351656477509));
#277600=CARTESIAN_POINT('Ctrl Pts',(1.84763692435666,1.39037286334906,12.5462770763223));
#277601=CARTESIAN_POINT('Ctrl Pts',(-0.165527309906998,2.30640404375699,
12.6573885048938));
#277602=CARTESIAN_POINT('Ctrl Pts',(-2.02724857903657,1.11227788891887,
12.7684999334652));
#277603=CARTESIAN_POINT('Ctrl Pts',(-2.03421526992979,-1.09948494258363,
12.8796113620366));
#277604=CARTESIAN_POINT('Ctrl Pts',(-0.180053471679505,-2.30531552086038,
12.9907227906081));
#277605=CARTESIAN_POINT('Ctrl Pts',(1.83884145519558,-1.40198466683405,
13.1018342191795));
#277606=CARTESIAN_POINT('Ctrl Pts',(2.17535779123418,0.784039146663179,
13.2129456477509));
#277607=CARTESIAN_POINT('Ctrl Pts',(0.521612615035739,2.25273593286457,
13.3240570763224));
#277608=CARTESIAN_POINT('Ctrl Pts',(-1.60936233742585,1.66037699642546,
13.4351685048938));
#277609=CARTESIAN_POINT('Ctrl Pts',(-2.26791195722282,-0.451081209616796,
13.5462799334652));
#277610=CARTESIAN_POINT('Ctrl Pts',(-0.851521123641821,-2.14983968690118,
13.6573913620366));
#277611=CARTESIAN_POINT('Ctrl Pts',(1.34393682527549,-1.88168347844478,
13.7685027906081));
#277612=CARTESIAN_POINT('Ctrl Pts',(2.30981049660767,0.108048013145282,
13.8796142191795));
#277613=CARTESIAN_POINT('Ctrl Pts',(1.16241022721892,1.99892505288228,13.9907256477509));
#277614=CARTESIAN_POINT('Ctrl Pts',(-1.04849340974778,2.06096105569685,
14.1018370763224));
#277615=CARTESIAN_POINT('Ctrl Pts',(-2.30011757201657,0.237398522076775,
14.2129485048938));
#277616=CARTESIAN_POINT('Ctrl Pts',(-1.4473359691043,-1.80336282980451,
14.3240599334652));
#277617=CARTESIAN_POINT('Ctrl Pts',(0.729631055715192,-2.19420542017367,
14.4351713620366));
#277618=CARTESIAN_POINT('Ctrl Pts',(2.23904968266907,-0.577542571524482,
14.5462827906081));
#277619=CARTESIAN_POINT('Ctrl Pts',(1.69993430507442,1.5675210562588,14.6573942191795));
#277620=CARTESIAN_POINT('Ctrl Pts',(-0.394471808763476,2.27844045247504,
14.7685056477509));
#277621=CARTESIAN_POINT('Ctrl Pts',(-2.12797082869335,0.904786745931656,
14.8796170763224));
#277622=CARTESIAN_POINT('Ctrl Pts',(-1.91456324936044,-1.29666744679644,
14.9907285048938));
#277623=CARTESIAN_POINT('Ctrl Pts',(0.0505017186100073,-2.31178469581453,
15.1018399334652));
#277624=CARTESIAN_POINT('Ctrl Pts',(1.96936204509281,-1.21182178505348,
15.2129513620366));
#277625=CARTESIAN_POINT('Ctrl Pts',(2.0864288929107,0.996851733312993,15.3240627906081));
#277626=CARTESIAN_POINT('Ctrl Pts',(0.294596367801226,2.2934933798619,15.4351742191795));
#277627=CARTESIAN_POINT('Ctrl Pts',(-1.76676598584593,1.49178981583561,
15.5462856477509));
#277628=CARTESIAN_POINT('Ctrl Pts',(-2.21169247918187,-0.674770539446852,
15.6573970763223));
#277629=CARTESIAN_POINT('Ctrl Pts',(-0.633114408827972,-2.22397505578959,
15.7685085048938));
#277630=CARTESIAN_POINT('Ctrl Pts',(1.5247077958973,-1.73843752848017,15.8796199334652));
#277631=CARTESIAN_POINT('Ctrl Pts',(2.28755614583539,0.337617806115804,
15.9907313620366));
#277632=CARTESIAN_POINT('Ctrl Pts',(0.957491333401296,2.10478247099586,
16.1018427906081));
#277633=CARTESIAN_POINT('Ctrl Pts',(-1.24859403842671,1.94625584904281,
16.2129542191795));
#277634=CARTESIAN_POINT('Ctrl Pts',(-2.31232541723185,0.00707589104983105,
16.3240656477509));
#277635=CARTESIAN_POINT('Ctrl Pts',(-1.26048192358796,-1.93857788752706,
16.4351770763223));
#277636=CARTESIAN_POINT('Ctrl Pts',(0.944591934930056,-2.11060298847667,
16.5462885048938));
#277637=CARTESIAN_POINT('Ctrl Pts',(2.28544705191438,-0.351611544136238,
16.6573999334652));
#277638=CARTESIAN_POINT('Ctrl Pts',(1.535318642296,1.72907362023293,16.7685113620367));
#277639=CARTESIAN_POINT('Ctrl Pts',(-0.619491615341388,2.22780811707463,
16.879622790608));
#277640=CARTESIAN_POINT('Ctrl Pts',(-2.20752139980484,0.688293683343328,
16.9907342191795));
#277641=CARTESIAN_POINT('Ctrl Pts',(-1.77586279142397,-1.4809491323765,
17.1018456477509));
#277642=CARTESIAN_POINT('Ctrl Pts',(0.28055445466867,-2.2952533304037,17.2129570763224));
#277643=CARTESIAN_POINT('Ctrl Pts',(2.08028899363887,-1.00960230898613,
17.3240685048938));
#277644=CARTESIAN_POINT('Ctrl Pts',(1.97674162320076,1.19974660651667,17.4351799334652));
#277645=CARTESIAN_POINT('Ctrl Pts',(0.0646491182662103,2.31143195022664,
17.5462913620366));
#277646=CARTESIAN_POINT('Ctrl Pts',(-1.90659167780665,1.30836118408193,
17.6574027906081));
#277647=CARTESIAN_POINT('Ctrl Pts',(-2.13346833523032,-0.891747778323729,
17.7685142191795));
#277648=CARTESIAN_POINT('Ctrl Pts',(-0.408408730619048,-2.2759809922174,
17.8796256477509));
#277649=CARTESIAN_POINT('Ctrl Pts',(1.69030916813735,-1.57790037625904,
17.9907370763224));
#277650=CARTESIAN_POINT('Ctrl Pts',(2.24254222088181,0.56383791930961,18.1018485048938));
#277651=CARTESIAN_POINT('Ctrl Pts',(0.743046408301969,2.18968111053243,
18.2129599334652));
#277652=CARTESIAN_POINT('Ctrl Pts',(-1.43627263399722,1.81222076736117,
18.3240713620366));
#277653=CARTESIAN_POINT('Ctrl Pts',(-2.3015264063899,-0.223381600007984,
18.4351827906081));
#277654=CARTESIAN_POINT('Ctrl Pts',(-1.06108893265441,-2.05438293086541,
18.5462942191795));
#277655=CARTESIAN_POINT('Ctrl Pts',(1.15015842546083,-2.00623507679203,
18.6574056477509));
#277656=CARTESIAN_POINT('Ctrl Pts',(2.30909922726198,-0.121737808789031,
18.7685170763224));
#277657=CARTESIAN_POINT('Ctrl Pts',(1.3554400697113,1.87257450567142,18.8796285048938));
#277658=CARTESIAN_POINT('Ctrl Pts',(-0.838367091757206,2.15665232290657,
18.9907399334652));
#277659=CARTESIAN_POINT('Ctrl Pts',(-2.26513615382795,0.461567928622731,
19.101853497924));
#277660=CARTESIAN_POINT('Ctrl Pts',(-1.83454523104888,-0.941064438844653,
19.1759299195257));
#277661=CARTESIAN_POINT('Ctrl Pts',(-1.37022001648085,-1.39661133546032,
19.2129691982704));
#277662=CARTESIAN_POINT('Ctrl Pts',(1.05790751410524,-1.48333259624667,
-0.153861392747535));
#277663=CARTESIAN_POINT('Ctrl Pts',(1.55120293711735,-1.13153472508212,
-0.116812388665656));
#277664=CARTESIAN_POINT('Ctrl Pts',(2.15057131801661,0.0965705457561521,
-0.0427262417266339));
#277665=CARTESIAN_POINT('Ctrl Pts',(1.08336547476853,1.8625271474138,0.0683970480695312));
#277666=CARTESIAN_POINT('Ctrl Pts',(-0.975807202051508,1.91874839396202,
0.17950847664096));
#277667=CARTESIAN_POINT('Ctrl Pts',(-2.14173055808719,0.222243512545894,
0.290619905212389));
#277668=CARTESIAN_POINT('Ctrl Pts',(-1.3484061737991,-1.67903036105319,
0.401731333783817));
#277669=CARTESIAN_POINT('Ctrl Pts',(0.678721800115099,-2.04338595829077,
0.512842762355246));
#277670=CARTESIAN_POINT('Ctrl Pts',(2.08481041986917,-0.538618154298584,
0.623954190926675));
#277671=CARTESIAN_POINT('Ctrl Pts',(1.58351640821179,1.45914582743268,0.735065619498103));
#277672=CARTESIAN_POINT('Ctrl Pts',(-0.36657508947119,2.12181017643735,
0.846177048069534));
#277673=CARTESIAN_POINT('Ctrl Pts',(-1.98127260449714,0.843261789831782,
0.957288476640961));
#277674=CARTESIAN_POINT('Ctrl Pts',(-1.7832847479344,-1.20682731866822,
1.06839990521239));
#277675=CARTESIAN_POINT('Ctrl Pts',(0.0462549324791658,-2.15275946002753,
1.17951133378381));
#277676=CARTESIAN_POINT('Ctrl Pts',(1.83347396506348,-1.12911391414712,
1.29062276235524));
#277677=CARTESIAN_POINT('Ctrl Pts',(1.94322594777237,0.927576174876139,
1.40173419092667));
#277678=CARTESIAN_POINT('Ctrl Pts',(0.275096289051986,2.13561314741684,
1.5128456194981));
#277679=CARTESIAN_POINT('Ctrl Pts',(-1.64472212758652,1.38975267968814,
1.62395704806953));
#277680=CARTESIAN_POINT('Ctrl Pts',(-2.05976421615942,-0.627610188512866,
1.73506847664096));
#277681=CARTESIAN_POINT('Ctrl Pts',(-0.590302713589067,-2.07076446671643,
1.84617990521239));
#277682=CARTESIAN_POINT('Ctrl Pts',(1.41923394810694,-1.6193511232449,1.95729133378382));
#277683=CARTESIAN_POINT('Ctrl Pts',(2.13029608741303,0.313626507834027,
2.06840276235524));
#277684=CARTESIAN_POINT('Ctrl Pts',(0.892324211344424,1.95966335342563,
2.17951419092667));
#277685=CARTESIAN_POINT('Ctrl Pts',(-1.1620460208133,1.81278019776812,2.2906256194981));
#277686=CARTESIAN_POINT('Ctrl Pts',(-2.15324610461966,0.0073622017891174,
2.40173704806953));
#277687=CARTESIAN_POINT('Ctrl Pts',(-1.17441492813331,-1.80479155581837,
2.51284847664096));
#277688=CARTESIAN_POINT('Ctrl Pts',(0.87890286332936,-1.96571939667137,
2.62395990521239));
#277689=CARTESIAN_POINT('Ctrl Pts',(2.12810165046316,-0.32818646061126,
2.73507133378382));
#277690=CARTESIAN_POINT('Ctrl Pts',(1.43027414771603,1.60960829067691,2.84618276235524));
#277691=CARTESIAN_POINT('Ctrl Pts',(-0.57612870728583,2.07475268419347,
2.95729419092668));
#277692=CARTESIAN_POINT('Ctrl Pts',(-2.05542434492789,0.641680411001263,
3.0684056194981));
#277693=CARTESIAN_POINT('Ctrl Pts',(-1.65418705067002,-1.3784731368187,
3.17951704806954));
#277694=CARTESIAN_POINT('Ctrl Pts',(0.260486255919504,-2.13744471229902,
3.29062847664096));
#277695=CARTESIAN_POINT('Ctrl Pts',(1.93683749351561,-0.940841916218584,
3.4017399052124));
#277696=CARTESIAN_POINT('Ctrl Pts',(1.84115236341935,1.11654868334311,3.51285133378381));
#277697=CARTESIAN_POINT('Ctrl Pts',(0.0609743642238004,2.15239520407475,
3.62396276235526));
#277698=CARTESIAN_POINT('Ctrl Pts',(-1.77498982832302,1.21898896506789,
3.73507419092667));
#277699=CARTESIAN_POINT('Ctrl Pts',(-1.98699406625453,-0.829685222405054,
3.84618561949811));
#277700=CARTESIAN_POINT('Ctrl Pts',(-0.381073073198851,-2.11927022828449,
3.95729704806953));
#277701=CARTESIAN_POINT('Ctrl Pts',(1.57349634633365,-1.4699089208803,4.06840847664097));
#277702=CARTESIAN_POINT('Ctrl Pts',(2.08845466815477,0.524290078746098,
4.17951990521239));
#277703=CARTESIAN_POINT('Ctrl Pts',(0.692660210442579,2.03880965773632,
4.29063133378382));
#277704=CARTESIAN_POINT('Ctrl Pts',(-1.33685756554719,1.68799728585336,
4.40174276235526));
#277705=CARTESIAN_POINT('Ctrl Pts',(-2.1432679654662,-0.207184497044221,
4.51285419092667));
#277706=CARTESIAN_POINT('Ctrl Pts',(-0.988776228152036,-1.91281064359507,
4.62396561949811));
#277707=CARTESIAN_POINT('Ctrl Pts',(1.07035900230882,-1.86838288200936,
4.73507704806953));
#277708=CARTESIAN_POINT('Ctrl Pts',(2.150209659374,-0.114548716028891,4.84618847664097));
#277709=CARTESIAN_POINT('Ctrl Pts',(1.26280713834729,1.74408747456893,4.9572999052124));
#277710=CARTESIAN_POINT('Ctrl Pts',(-0.779953115075661,2.00703665285239,
5.06841133378382));
#277711=CARTESIAN_POINT('Ctrl Pts',(-2.10912470159532,0.433723391955705,
5.17952276235525));
#277712=CARTESIAN_POINT('Ctrl Pts',(-1.50863224158034,-1.53640871752064,
5.29063419092668));
#277713=CARTESIAN_POINT('Ctrl Pts',(0.472126351498558,-2.10086165556654,
5.40174561949812));
#277714=CARTESIAN_POINT('Ctrl Pts',(2.02093075750676,-0.743210509191247,
5.51285704806953));
#277715=CARTESIAN_POINT('Ctrl Pts',(1.72076083765024,1.29441304351369,5.62396847664098));
#277716=CARTESIAN_POINT('Ctrl Pts',(-0.153754268428281,2.1477622337096,
5.73507990521239));
#277717=CARTESIAN_POINT('Ctrl Pts',(-1.88759770935448,1.03609742555844,
5.84619133378383));
#277718=CARTESIAN_POINT('Ctrl Pts',(-1.89445486478159,-1.02350561938589,
5.95730276235525));
#277719=CARTESIAN_POINT('Ctrl Pts',(-0.168052039143294,-2.14669082537494,
6.0684141909267));
#277720=CARTESIAN_POINT('Ctrl Pts',(1.71210365735957,-1.30584227763736,
6.17952561949811));
#277721=CARTESIAN_POINT('Ctrl Pts',(2.02583472802201,0.72973737902694,6.29063704806955));
#277722=CARTESIAN_POINT('Ctrl Pts',(0.48610477007458,2.09767136132423,6.40174847664096));
#277723=CARTESIAN_POINT('Ctrl Pts',(-1.49836840146871,1.54642009851438,
6.51285990521241));
#277724=CARTESIAN_POINT('Ctrl Pts',(-2.11196595309689,-0.419669870932711,
6.62397133378382));
#277725=CARTESIAN_POINT('Ctrl Pts',(-0.793299962358999,-2.00179873047476,
6.73508276235527));
#277726=CARTESIAN_POINT('Ctrl Pts',(1.25116588948884,-1.75245739023484,
6.84619419092668));
#277727=CARTESIAN_POINT('Ctrl Pts',(2.1509247302382,0.10022870077407,6.95730561949813));
#277728=CARTESIAN_POINT('Ctrl Pts',(1.08277616579552,1.86121432468007,7.06841704806953));
#277729=CARTESIAN_POINT('Ctrl Pts',(-0.976017587146367,1.91935214517559,
7.17952847664098));
#277730=CARTESIAN_POINT('Ctrl Pts',(-2.14184088401364,0.221451157542293,
7.29063990521239));
#277731=CARTESIAN_POINT('Ctrl Pts',(-1.34806769796412,-1.67905820903114,
7.40175133378384));
#277732=CARTESIAN_POINT('Ctrl Pts',(0.679069151736237,-2.04337663556412,
7.51286276235525));
#277733=CARTESIAN_POINT('Ctrl Pts',(2.08491730939053,-0.538184727220017,
7.6239741909267));
#277734=CARTESIAN_POINT('Ctrl Pts',(1.58324906041151,1.45939898599225,7.7350856194981));
#277735=CARTESIAN_POINT('Ctrl Pts',(-0.366953163953109,2.12176067525863,
7.84619704806955));
#277736=CARTESIAN_POINT('Ctrl Pts',(-1.98142543991457,0.8428975107737,7.95730847664098));
#277737=CARTESIAN_POINT('Ctrl Pts',(-1.78306728939617,-1.20714291991236,
8.06841990521241));
#277738=CARTESIAN_POINT('Ctrl Pts',(0.046640983899346,-2.15275349406987,
8.17953133378384));
#277739=CARTESIAN_POINT('Ctrl Pts',(1.83367684922511,-1.12878350458582,
8.29064276235526));
#277740=CARTESIAN_POINT('Ctrl Pts',(1.94305928503282,0.927924351688705,
8.4017541909267));
#277741=CARTESIAN_POINT('Ctrl Pts',(0.274712959816065,2.13566284261309,
8.51286561949811));
#277742=CARTESIAN_POINT('Ctrl Pts',(-1.64497162021,1.38945721643843,8.62397704806956));
#277743=CARTESIAN_POINT('Ctrl Pts',(-2.05965149819634,-0.627979851258548,
8.73508847664097));
#277744=CARTESIAN_POINT('Ctrl Pts',(-0.58993096995992,-2.07087045425137,
8.84619990521242));
#277745=CARTESIAN_POINT('Ctrl Pts',(1.41952463501611,-1.61909629058667,
8.95731133378382));
#277746=CARTESIAN_POINT('Ctrl Pts',(2.13023974859831,0.314008918823931,
9.06842276235528));
#277747=CARTESIAN_POINT('Ctrl Pts',(0.891972400280589,1.95982351877582,
9.17953419092668));
#277748=CARTESIAN_POINT('Ctrl Pts',(-1.16237143228708,1.81257155472881,
9.29064561949813));
#277749=CARTESIAN_POINT('Ctrl Pts',(-2.15324739123553,0.00697565384108067,
9.40175704806954));
#277750=CARTESIAN_POINT('Ctrl Pts',(-1.17409091397056,-1.80500235826464,
9.51286847664099));
#277751=CARTESIAN_POINT('Ctrl Pts',(0.879255734382123,-1.9655615841701,
9.62397990521238));
#277752=CARTESIAN_POINT('Ctrl Pts',(2.12816053201671,-0.327804419701003,
9.73509133378385));
#277753=CARTESIAN_POINT('Ctrl Pts',(1.42998516849226,1.6098650271067,9.84620276235524));
#277754=CARTESIAN_POINT('Ctrl Pts',(-0.576501156745404,2.07464922429802,
9.95731419092671));
#277755=CARTESIAN_POINT('Ctrl Pts',(-2.05553950599769,0.641311411789866,
10.0684256194981));
#277756=CARTESIAN_POINT('Ctrl Pts',(-1.65393956110117,-1.37877007359226,
10.1795370480696));
#277757=CARTESIAN_POINT('Ctrl Pts',(0.26086996489986,-2.13739791546223,
10.290648476641));
#277758=CARTESIAN_POINT('Ctrl Pts',(1.93700636185011,-0.940494200812156,
10.4017599052124));
#277759=CARTESIAN_POINT('Ctrl Pts',(1.84095189140225,1.11687918825252,10.5128713337839));
#277760=CARTESIAN_POINT('Ctrl Pts',(0.0605879661592919,2.15240611548235,
10.6239827623553));
#277761=CARTESIAN_POINT('Ctrl Pts',(-1.7752086321076,1.21867029999906,10.7350941909267));
#277762=CARTESIAN_POINT('Ctrl Pts',(-1.98684508949477,-0.830041913375277,
10.8462056194981));
#277763=CARTESIAN_POINT('Ctrl Pts',(-0.380692616558361,-2.1193386042129,
10.9573170480696));
#277764=CARTESIAN_POINT('Ctrl Pts',(1.57376019841008,-1.46962642379259,
11.068428476641));
#277765=CARTESIAN_POINT('Ctrl Pts',(2.08836051416776,0.524664988801521,
11.1795399052124));
#277766=CARTESIAN_POINT('Ctrl Pts',(0.6922941930291,2.03893397095329,11.2906513337839));
#277767=CARTESIAN_POINT('Ctrl Pts',(-1.3371605725683,1.68775726654574,11.4017627623553));
#277768=CARTESIAN_POINT('Ctrl Pts',(-2.1432307372566,-0.207569252269409,
11.5128741909267));
#277769=CARTESIAN_POINT('Ctrl Pts',(-0.988432825257067,-1.91298811746531,
11.6239856194981));
#277770=CARTESIAN_POINT('Ctrl Pts',(1.07069439637054,-1.86819070150503,
11.7350970480696));
#277771=CARTESIAN_POINT('Ctrl Pts',(2.15023018846362,-0.11416270944945,
11.846208476641));
#277772=CARTESIAN_POINT('Ctrl Pts',(1.26249402014902,1.74431414507166,11.9573199052124));
#277773=CARTESIAN_POINT('Ctrl Pts',(-0.780313404883507,2.00689660365656,
12.0684313337839));
#277774=CARTESIAN_POINT('Ctrl Pts',(-2.10920252945054,0.433344755787544,
12.1795427623553));
#277775=CARTESIAN_POINT('Ctrl Pts',(-1.50835640182406,-1.53667952178895,
12.2906541909267));
#277776=CARTESIAN_POINT('Ctrl Pts',(0.472503489691624,-2.10077686578998,
12.4017656194981));
#277777=CARTESIAN_POINT('Ctrl Pts',(2.02106414578021,-0.742847700575875,
12.5128770480696));
#277778=CARTESIAN_POINT('Ctrl Pts',(1.72052843743741,1.29472193291777,12.623988476641));
#277779=CARTESIAN_POINT('Ctrl Pts',(-0.154139831323539,2.14773459719973,
12.7350999052125));
#277780=CARTESIAN_POINT('Ctrl Pts',(-1.88778367871244,1.03575854811633,
12.8462113337838));
#277781=CARTESIAN_POINT('Ctrl Pts',(-1.89427109495674,-1.02384569463398,
12.9573227623553));
#277782=CARTESIAN_POINT('Ctrl Pts',(-0.167666663401311,-2.14672095941532,
13.0684341909267));
#277783=CARTESIAN_POINT('Ctrl Pts',(1.71233805402778,-1.30553490046703,
13.1795456194982));
#277784=CARTESIAN_POINT('Ctrl Pts',(2.02570369323109,0.730101044266491,
13.2906570480696));
#277785=CARTESIAN_POINT('Ctrl Pts',(0.485728189161183,2.09775859284699,
13.401768476641));
#277786=CARTESIAN_POINT('Ctrl Pts',(-1.4986459900102,1.54615108713072,13.5128799052124));
#277787=CARTESIAN_POINT('Ctrl Pts',(-2.11189058010671,-0.420049003409895,
13.6239913337839));
#277788=CARTESIAN_POINT('Ctrl Pts',(-0.792940587509937,-2.00194111109406,
13.7351027623553));
#277789=CARTESIAN_POINT('Ctrl Pts',(1.25148046974159,-1.75223275322215,
13.8462141909267));
#277790=CARTESIAN_POINT('Ctrl Pts',(2.15090670256477,0.100614832261903,
13.9573256194981));
#277791=CARTESIAN_POINT('Ctrl Pts',(1.08244202393532,1.86140867421099,14.0684370480696));
#277792=CARTESIAN_POINT('Ctrl Pts',(-0.97636213270898,1.91917689998111,
14.179548476641));
#277793=CARTESIAN_POINT('Ctrl Pts',(-2.14188060431944,0.221066651599284,
14.2906599052124));
#277794=CARTESIAN_POINT('Ctrl Pts',(-1.34776625241837,-1.67930018652154,
14.4017713337838));
#277795=CARTESIAN_POINT('Ctrl Pts',(0.679435966908132,-2.04325469642938,
14.5128827623553));
#277796=CARTESIAN_POINT('Ctrl Pts',(2.08501389049079,-0.53781043506944,
14.6239941909267));
#277797=CARTESIAN_POINT('Ctrl Pts',(1.58298704420748,1.4596831866814,14.7351056194982));
#277798=CARTESIAN_POINT('Ctrl Pts',(-0.36733405562417,2.12169476579173,
14.8462170480696));
#277799=CARTESIAN_POINT('Ctrl Pts',(-1.9815767245932,0.842541792529895,
14.957328476641));
#277800=CARTESIAN_POINT('Ctrl Pts',(-1.78285055487521,-1.20746299595058,
15.0684399052124));
#277801=CARTESIAN_POINT('Ctrl Pts',(0.0470274445495869,-2.15274508641162,
15.1795513337839));
#277802=CARTESIAN_POINT('Ctrl Pts',(1.83387945841787,-1.1284543054998,15.2906627623553));
#277803=CARTESIAN_POINT('Ctrl Pts',(1.94289267313373,0.928273153921158,
15.4017741909267));
#277804=CARTESIAN_POINT('Ctrl Pts',(0.274329562094182,2.13571212455651,
15.5128856194982));
#277805=CARTESIAN_POINT('Ctrl Pts',(-1.64522102847855,1.38916188943257,
15.6239970480696));
#277806=CARTESIAN_POINT('Ctrl Pts',(-2.05953873032919,-0.628349588903945,
15.735108476641));
#277807=CARTESIAN_POINT('Ctrl Pts',(-0.589559198660854,-2.07097632505356,
15.8462199052124));
#277808=CARTESIAN_POINT('Ctrl Pts',(1.41981527162715,-1.61884143200916,
15.9573313337839));
#277809=CARTESIAN_POINT('Ctrl Pts',(2.13018334352401,0.314391333464881,
16.0684427623553));
#277810=CARTESIAN_POINT('Ctrl Pts',(0.891620559212638,1.95998361378768,
16.1795541909267));
#277811=CARTESIAN_POINT('Ctrl Pts',(-1.16269680563781,1.81236285693576,
16.2906656194981));
#277812=CARTESIAN_POINT('Ctrl Pts',(-2.15324860880986,0.00658910395812926,
16.4017770480696));
#277813=CARTESIAN_POINT('Ctrl Pts',(-1.17376686177888,-1.8052131020487,
16.512888476641));
#277814=CARTESIAN_POINT('Ctrl Pts',(0.87960857698654,-1.96540370780851,
16.6239999052125));
#277815=CARTESIAN_POINT('Ctrl Pts',(2.12821934506713,-0.327422369970407,
16.7351113337838));
#277816=CARTESIAN_POINT('Ctrl Pts',(1.42969614309794,1.61012171537405,16.8462227623553));
#277817=CARTESIAN_POINT('Ctrl Pts',(-0.576873587498792,2.07454569025536,
16.9573341909267));
#277818=CARTESIAN_POINT('Ctrl Pts',(-2.05565460104578,0.640942405885882,
17.0684456194982));
#277819=CARTESIAN_POINT('Ctrl Pts',(-1.65369201781665,-1.37906699257984,
17.1795570480696));
#277820=CARTESIAN_POINT('Ctrl Pts',(0.261253664691311,-2.13735099901054,
17.290668476641));
#277821=CARTESIAN_POINT('Ctrl Pts',(1.93717516924488,-0.940146551638089,
17.4017799052124));
#277822=CARTESIAN_POINT('Ctrl Pts',(1.84075135723286,1.11720984086182,17.5128913337839));
#277823=CARTESIAN_POINT('Ctrl Pts',(0.0602015715133129,2.15241660801462,
17.6240027623553));
#277824=CARTESIAN_POINT('Ctrl Pts',(-1.7754273889011,1.21835226065102,17.7351141909267));
#277825=CARTESIAN_POINT('Ctrl Pts',(-1.98669602926134,-0.830399842848887,
17.8462256194982));
#277826=CARTESIAN_POINT('Ctrl Pts',(-0.380312184642269,-2.11940450450811,
17.9573370480696));
#277827=CARTESIAN_POINT('Ctrl Pts',(1.57402407015333,-1.4693484596505,18.068448476641));
#277828=CARTESIAN_POINT('Ctrl Pts',(2.0882661589612,0.525048596663805,18.1795599052125));
#277829=CARTESIAN_POINT('Ctrl Pts',(0.691928408101298,2.03904163741605,
18.2906713337839));
#277830=CARTESIAN_POINT('Ctrl Pts',(-1.33746402127451,1.68754874080316,
18.4017827623553));
#277831=CARTESIAN_POINT('Ctrl Pts',(-2.14319251769972,-0.208014025995827,
18.5128941909267));
#277832=CARTESIAN_POINT('Ctrl Pts',(-0.988091144540052,-1.91305131833229,
18.6240056194981));
#277833=CARTESIAN_POINT('Ctrl Pts',(1.07103308689969,-1.86821580382033,
18.7351170480696));
#277834=CARTESIAN_POINT('Ctrl Pts',(2.15024436511102,-0.113362836156677,
18.846228476641));
#277835=CARTESIAN_POINT('Ctrl Pts',(1.26219234657939,1.74375043373295,18.9573399052124));
#277836=CARTESIAN_POINT('Ctrl Pts',(-0.780691489418133,2.00828507068194,
19.0684513337839));
#277837=CARTESIAN_POINT('Ctrl Pts',(-2.10930573856417,0.429814286852394,
19.1795648982427));
#277838=CARTESIAN_POINT('Ctrl Pts',(-1.70833738932978,-0.876323755576083,
19.2536413198444));
#277839=CARTESIAN_POINT('Ctrl Pts',(-1.27595550447344,-1.3005312283113,
19.290680598589));
#277840=CARTESIAN_POINT('Ctrl Pts',(0.979751861171807,-1.37374756538967,
-0.0761499924288698));
#277841=CARTESIAN_POINT('Ctrl Pts',(1.43660380934276,-1.04793967156705,
-0.0391009883469908));
#277842=CARTESIAN_POINT('Ctrl Pts',(1.99169230137438,0.0894361469953051,
0.0349851585920312));
#277843=CARTESIAN_POINT('Ctrl Pts',(1.00332904916694,1.72492813864273,0.146108448388196));
#277844=CARTESIAN_POINT('Ctrl Pts',(-0.903716921949864,1.77699589523638,
0.257219876959625));
#277845=CARTESIAN_POINT('Ctrl Pts',(-1.98350467544344,0.205824698423077,
0.368331305531054));
#277846=CARTESIAN_POINT('Ctrl Pts',(-1.24878918126658,-1.55498765182436,
0.479442734102483));
#277847=CARTESIAN_POINT('Ctrl Pts',(0.628579472226426,-1.89242553723708,
0.590554162673911));
#277848=CARTESIAN_POINT('Ctrl Pts',(1.93078965960915,-0.498826345497046,
0.701665591245341));
#277849=CARTESIAN_POINT('Ctrl Pts',(1.4665300392103,1.35134765665918,0.812777019816767));
#277850=CARTESIAN_POINT('Ctrl Pts',(-0.339493406918823,1.96505596349419,
0.923888448388199));
#277851=CARTESIAN_POINT('Ctrl Pts',(-1.83490096805542,0.780963644767716,
1.03499987695962));
#277852=CARTESIAN_POINT('Ctrl Pts',(-1.65153997631426,-1.11766983012519,
1.14611130553105));
#277853=CARTESIAN_POINT('Ctrl Pts',(0.0428377297453559,-1.99371878873657,
1.25722273410248));
#277854=CARTESIAN_POINT('Ctrl Pts',(1.69802133525854,-1.04569770429913,
1.36833416267391));
#277855=CARTESIAN_POINT('Ctrl Pts',(1.79966510646976,0.859049086613364,
1.47944559124534));
#277856=CARTESIAN_POINT('Ctrl Pts',(0.254772839408482,1.97783920430355,
1.59055701981676));
#277857=CARTESIAN_POINT('Ctrl Pts',(-1.5232140278125,1.28708110712742,1.7016684483882));
#277858=CARTESIAN_POINT('Ctrl Pts',(-1.907593808958,-0.581243863085647,
1.81277987695962));
#277859=CARTESIAN_POINT('Ctrl Pts',(-0.546692574334192,-1.91778138756283,
1.92389130553106));
#277860=CARTESIAN_POINT('Ctrl Pts',(1.31438437061491,-1.49971737201599,
2.03500273410248));
#277861=CARTESIAN_POINT('Ctrl Pts',(1.97291495585534,0.290456538654119,
2.14611416267391));
#277862=CARTESIAN_POINT('Ctrl Pts',(0.826401453035167,1.81488815627977,
2.25722559124534));
#277863=CARTESIAN_POINT('Ctrl Pts',(-1.07619686643597,1.67885637352799,
2.36833701981677));
#277864=CARTESIAN_POINT('Ctrl Pts',(-1.9941694812012,0.00681830009622902,
2.4794484483882));
#277865=CARTESIAN_POINT('Ctrl Pts',(-1.08765198874667,-1.67145791315773,
2.59055987695962));
#277866=CARTESIAN_POINT('Ctrl Pts',(0.813971641806969,-1.82049679367221,
2.70167130553106));
#277867=CARTESIAN_POINT('Ctrl Pts',(1.97088263860907,-0.303940837273705,
2.81278273410248));
#277868=CARTESIAN_POINT('Ctrl Pts',(1.32460894693233,1.49069431639504,2.92389416267391));
#277869=CARTESIAN_POINT('Ctrl Pts',(-0.533565709394934,1.92147496516182,
3.03500559124534));
#277870=CARTESIAN_POINT('Ctrl Pts',(-1.90357455693488,0.594274611507729,
3.14611701981677));
#277871=CARTESIAN_POINT('Ctrl Pts',(-1.5319797052307,-1.27663486965186,
3.2572284483882));
#277872=CARTESIAN_POINT('Ctrl Pts',(0.241242160249381,-1.97953545759437,
3.36833987695962));
#277873=CARTESIAN_POINT('Ctrl Pts',(1.79374861578921,-0.871334787014221,
3.47945130553106));
#277874=CARTESIAN_POINT('Ctrl Pts',(1.70513247208259,1.03406076240944,3.59056273410248));
#277875=CARTESIAN_POINT('Ctrl Pts',(0.0564697254112784,1.99338144313412,
3.70167416267392));
#277876=CARTESIAN_POINT('Ctrl Pts',(-1.64385786533654,1.12893300345194,
3.81278559124534));
#277877=CARTESIAN_POINT('Ctrl Pts',(-1.84019974203207,-0.76839008136323,
3.92389701981677));
#277878=CARTESIAN_POINT('Ctrl Pts',(-0.3529203146126,-1.9627036605784,4.0350084483882));
#277879=CARTESIAN_POINT('Ctrl Pts',(1.45725023531129,-1.36131559874929,
4.14611987695963));
#277880=CARTESIAN_POINT('Ctrl Pts',(1.93416467963008,0.485556793572691,
4.25723130553106));
#277881=CARTESIAN_POINT('Ctrl Pts',(0.641488146451795,1.88818732271859,
4.36834273410248));
#277882=CARTESIAN_POINT('Ctrl Pts',(-1.23809375630938,1.56329212187003,
4.47945416267392));
#277883=CARTESIAN_POINT('Ctrl Pts',(-1.98492850287721,-0.1918782066282,
4.59056559124534));
#277884=CARTESIAN_POINT('Ctrl Pts',(-0.915727827714486,-1.77149681153045,
4.70167701981678));
#277885=CARTESIAN_POINT('Ctrl Pts',(0.991283463489736,-1.73035126570446,
4.8127884483882));
#277886=CARTESIAN_POINT('Ctrl Pts',(1.9913573611991,-0.106086133454761,
4.92389987695964));
#277887=CARTESIAN_POINT('Ctrl Pts',(1.16951399588391,1.61523850286725,5.03501130553107));
#277888=CARTESIAN_POINT('Ctrl Pts',(-0.72233206205028,1.85876163072283,
5.14612273410249));
#277889=CARTESIAN_POINT('Ctrl Pts',(-1.95330766090571,0.401680954938468,
5.25723416267391));
#277890=CARTESIAN_POINT('Ctrl Pts',(-1.39717813400948,-1.42290255097073,
5.36834559124535));
#277891=CARTESIAN_POINT('Ctrl Pts',(0.437246796550256,-1.94565506876726,
5.47945701981677));
#277892=CARTESIAN_POINT('Ctrl Pts',(1.87162927247121,-0.688303911177398,
5.59056844838821));
#277893=CARTESIAN_POINT('Ctrl Pts',(1.59363518156437,1.1987849330858,5.70167987695963));
#277894=CARTESIAN_POINT('Ctrl Pts',(-0.142395274300623,1.98909074543372,
5.81279130553107));
#277895=CARTESIAN_POINT('Ctrl Pts',(-1.74814654799753,0.959553049308661,
5.92390273410249));
#277896=CARTESIAN_POINT('Ctrl Pts',(-1.75449711333758,-0.947891495374496,
6.03501416267391));
#277897=CARTESIAN_POINT('Ctrl Pts',(-0.155636760235733,-1.98809849016002,
6.14612559124535));
#277898=CARTESIAN_POINT('Ctrl Pts',(1.58561757285168,-1.20936980298714,
6.25723701981678));
#277899=CARTESIAN_POINT('Ctrl Pts',(1.87617094948495,0.675826143340122,
6.36834844838821));
#277900=CARTESIAN_POINT('Ctrl Pts',(0.45019252331136,1.94270046576094,6.47945987695964));
#277901=CARTESIAN_POINT('Ctrl Pts',(-1.3876725616243,1.43217431530812,6.59057130553106));
#277902=CARTESIAN_POINT('Ctrl Pts',(-1.95593900760625,-0.388665674117844,
6.7016827341025));
#277903=CARTESIAN_POINT('Ctrl Pts',(-0.734692876480939,-1.85391067340403,
6.81279416267391));
#277904=CARTESIAN_POINT('Ctrl Pts',(1.15873277438451,-1.62299006937209,
6.92390559124537));
#277905=CARTESIAN_POINT('Ctrl Pts',(1.99201960435431,0.0928240463527359,
7.03501701981677));
#277906=CARTESIAN_POINT('Ctrl Pts',(1.00278327691804,1.72371230408288,7.14612844838821));
#277907=CARTESIAN_POINT('Ctrl Pts',(-0.903911764301868,1.77755504276799,
7.25723987695964));
#277908=CARTESIAN_POINT('Ctrl Pts',(-1.98360685075681,0.205090880694083,
7.36835130553106));
#277909=CARTESIAN_POINT('Ctrl Pts',(-1.24847571120909,-1.55501344246093,
7.4794627341025));
#277910=CARTESIAN_POINT('Ctrl Pts',(0.62890116234844,-1.89241690325098,
7.59057416267391));
#277911=CARTESIAN_POINT('Ctrl Pts',(1.93088865239076,-0.49842493896458,
7.70168559124536));
#277912=CARTESIAN_POINT('Ctrl Pts',(1.46628244242002,1.35158211247559,7.81279701981678));
#277913=CARTESIAN_POINT('Ctrl Pts',(-0.33984355017084,1.96501011934303,
7.92390844838821));
#277914=CARTESIAN_POINT('Ctrl Pts',(-1.83504251236122,0.780626277766932,
8.03501987695964));
#277915=CARTESIAN_POINT('Ctrl Pts',(-1.65133858308781,-1.1179621155114,
8.14613130553108));
#277916=CARTESIAN_POINT('Ctrl Pts',(0.0431952606186986,-1.99371326352946,
8.25724273410249));
#277917=CARTESIAN_POINT('Ctrl Pts',(1.69820923082814,-1.04539170459849,
8.36835416267393));
#277918=CARTESIAN_POINT('Ctrl Pts',(1.79951075637102,0.859371540963658,
8.47946559124535));
#277919=CARTESIAN_POINT('Ctrl Pts',(0.254417829611001,1.97788522813869,
8.59057701981678));
#277920=CARTESIAN_POINT('Ctrl Pts',(-1.52344508852334,1.28680747198924,
8.70168844838821));
#277921=CARTESIAN_POINT('Ctrl Pts',(-1.90748941832589,-0.58158621604019,
8.81279987695964));
#277922=CARTESIAN_POINT('Ctrl Pts',(-0.54634829422683,-1.91787954499458,
8.92391130553106));
#277923=CARTESIAN_POINT('Ctrl Pts',(1.31465358227707,-1.49948136577929,
9.03502273410249));
#277924=CARTESIAN_POINT('Ctrl Pts',(1.97286277921622,0.290810698043381,
9.14613416267393));
#277925=CARTESIAN_POINT('Ctrl Pts',(0.826075632923317,1.81503648900058,
9.25724559124534));
#277926=CARTESIAN_POINT('Ctrl Pts',(-1.07649823729575,1.67866314453268,
9.36835701981679));
#277927=CARTESIAN_POINT('Ctrl Pts',(-1.99417067276499,0.00646030937731316,
9.47946844838821));
#277928=CARTESIAN_POINT('Ctrl Pts',(-1.08735191196796,-1.67165314202824,
9.59057987695965));
#277929=CARTESIAN_POINT('Ctrl Pts',(0.814298443598325,-1.82035063997751,
9.70169130553106));
#277930=CARTESIAN_POINT('Ctrl Pts',(1.97093717013561,-0.303587020623497,
9.81280273410251));
#277931=CARTESIAN_POINT('Ctrl Pts',(1.3243413167959,1.49093208575727,9.92391416267391));
#277932=CARTESIAN_POINT('Ctrl Pts',(-0.533910643187675,1.92137914863364,
10.0350255912454));
#277933=CARTESIAN_POINT('Ctrl Pts',(-1.9036812101829,0.59393287306716,10.1461370198168));
#277934=CARTESIAN_POINT('Ctrl Pts',(-1.53175049959366,-1.27690986945351,
10.2572484483882));
#277935=CARTESIAN_POINT('Ctrl Pts',(0.24159752173669,-1.9794921179949,10.3683598769596));
#277936=CARTESIAN_POINT('Ctrl Pts',(1.79390500853888,-0.8710127599825,10.4794713055311));
#277937=CARTESIAN_POINT('Ctrl Pts',(1.70494681045408,1.03436685041413,10.5905827341025));
#277938=CARTESIAN_POINT('Ctrl Pts',(0.0561118735028585,1.99339154843327,
10.7016941626739));
#277939=CARTESIAN_POINT('Ctrl Pts',(-1.64406050442579,1.128637880589,10.8128055912454));
#277940=CARTESIAN_POINT('Ctrl Pts',(-1.84006177131562,-0.768720420865766,
10.9239170198168));
#277941=CARTESIAN_POINT('Ctrl Pts',(-0.352567965190137,-1.96276698505831,
11.0350284483882));
#277942=CARTESIAN_POINT('Ctrl Pts',(1.45749459463335,-1.36105397186436,
11.1461398769597));
#277943=CARTESIAN_POINT('Ctrl Pts',(1.93407748151231,0.485904006178401,
11.2572513055311));
#277944=CARTESIAN_POINT('Ctrl Pts',(0.641149169521112,1.88830245197522,
11.3683627341025));
#277945=CARTESIAN_POINT('Ctrl Pts',(-1.23837437790336,1.56306983460935,
11.4794741626739));
#277946=CARTESIAN_POINT('Ctrl Pts',(-1.98489402499784,-0.192234537066302,
11.5905855912454));
#277947=CARTESIAN_POINT('Ctrl Pts',(-0.915409794596289,-1.77166117405965,
11.7016970198168));
#277948=CARTESIAN_POINT('Ctrl Pts',(0.991594079447964,-1.73017328303178,
11.8128084483882));
#277949=CARTESIAN_POINT('Ctrl Pts',(1.99137637364914,-0.105728644109437,
11.9239198769596));
#277950=CARTESIAN_POINT('Ctrl Pts',(1.16922401010214,1.61544842750052,12.0350313055311));
#277951=CARTESIAN_POINT('Ctrl Pts',(-0.722665734517006,1.85863192802346,
12.1461427341025));
#277952=CARTESIAN_POINT('Ctrl Pts',(-1.95337973902688,0.401330291496232,
12.2572541626739));
#277953=CARTESIAN_POINT('Ctrl Pts',(-1.39692267262841,-1.42315334887352,
12.3683655912453));
#277954=CARTESIAN_POINT('Ctrl Pts',(0.437596072684178,-1.94557654305468,
12.4794770198168));
#277955=CARTESIAN_POINT('Ctrl Pts',(1.87175280634107,-0.687967905986568,
12.5905884483882));
#277956=CARTESIAN_POINT('Ctrl Pts',(1.59341995051815,1.19907100248648,12.7016998769597));
#277957=CARTESIAN_POINT('Ctrl Pts',(-0.142752352740081,1.98906515064247,
12.8128113055311));
#277958=CARTESIAN_POINT('Ctrl Pts',(-1.74831877838833,0.959239207313788,
12.9239227341025));
#277959=CARTESIAN_POINT('Ctrl Pts',(-1.7543269199837,-0.948206446684336,
13.0350341626739));
#277960=CARTESIAN_POINT('Ctrl Pts',(-0.155279855123116,-1.98812639797025,
13.1461455912454));
#277961=CARTESIAN_POINT('Ctrl Pts',(1.58583465285997,-1.20908513410002,
13.2572570198168));
#277962=CARTESIAN_POINT('Ctrl Pts',(1.87604959522801,0.676162941869805,
13.3683684483882));
#277963=CARTESIAN_POINT('Ctrl Pts',(0.449843763286628,1.9427812528294,13.4794798769597));
#277964=CARTESIAN_POINT('Ctrl Pts',(-1.38792964259454,1.43192517783599,
13.5905913055311));
#277965=CARTESIAN_POINT('Ctrl Pts',(-1.95586920299061,-0.389016797202991,
13.7017027341025));
#277966=CARTESIAN_POINT('Ctrl Pts',(-0.734360051378052,-1.85404253528694,
13.8128141626739));
#277967=CARTESIAN_POINT('Ctrl Pts',(1.15902411420771,-1.62278202799953,
13.9239255912454));
#277968=CARTESIAN_POINT('Ctrl Pts',(1.99200290852187,0.0931816513785255,
14.0350370198168));
#277969=CARTESIAN_POINT('Ctrl Pts',(1.00247382065172,1.7238922955397,14.1461484483882));
#277970=CARTESIAN_POINT('Ctrl Pts',(-0.904230855670186,1.77739274426537,
14.2572598769597));
#277971=CARTESIAN_POINT('Ctrl Pts',(-1.98364363662232,0.204734781121791,
14.3683713055311));
#277972=CARTESIAN_POINT('Ctrl Pts',(-1.24819653573245,-1.55523754323857,
14.4794827341025));
#277973=CARTESIAN_POINT('Ctrl Pts',(0.629240878101075,-1.8923039726851,
14.590594162674));
#277974=CARTESIAN_POINT('Ctrl Pts',(1.9309780983125,-0.498078298614397,
14.7017055912454));
#277975=CARTESIAN_POINT('Ctrl Pts',(1.46603978334054,1.351845317104,14.8128170198168));
#277976=CARTESIAN_POINT('Ctrl Pts',(-0.340196302484868,1.96494907910841,
14.9239284483882));
#277977=CARTESIAN_POINT('Ctrl Pts',(-1.83518262049305,0.780296839128134,
15.0350398769597));
#277978=CARTESIAN_POINT('Ctrl Pts',(-1.65113786038999,-1.11825854510472,
15.1461513055311));
#277979=CARTESIAN_POINT('Ctrl Pts',(0.0435531704891701,-1.99370547700871,
15.2572627341025));
#277980=CARTESIAN_POINT('Ctrl Pts',(1.69839687174293,-1.04508682594613,
15.3683741626739));
#277981=CARTESIAN_POINT('Ctrl Pts',(1.79935645335677,0.859694574529323,
15.4794855912454));
#277982=CARTESIAN_POINT('Ctrl Pts',(0.254062756387133,1.97793086925111,
15.5905970198168));
#277983=CARTESIAN_POINT('Ctrl Pts',(-1.52367607111119,1.28653396302953,
15.7017084483882));
#277984=CARTESIAN_POINT('Ctrl Pts',(-1.90738498147651,-0.58192863836104,
15.8128198769597));
#277985=CARTESIAN_POINT('Ctrl Pts',(-0.546003988493735,-1.91797759431753,
15.9239313055311));
#277986=CARTESIAN_POINT('Ctrl Pts',(1.31492274735698,-1.49924533553815,
16.0350427341025));
#277987=CARTESIAN_POINT('Ctrl Pts',(1.97281054121263,0.291164860813958,
16.146154162674));
#277988=CARTESIAN_POINT('Ctrl Pts',(0.82574978502398,1.8151847565795,16.2572655912454));
#277989=CARTESIAN_POINT('Ctrl Pts',(-1.07679957284889,1.67846986482871,
16.3683770198168));
#277990=CARTESIAN_POINT('Ctrl Pts',(-1.99417180038787,0.00610231686643078,
16.4794884483882));
#277991=CARTESIAN_POINT('Ctrl Pts',(-1.0870517999698,-1.67184831657035,
16.5905998769597));
#277992=CARTESIAN_POINT('Ctrl Pts',(0.814625219043029,-1.82020442714035,
16.7017113055311));
#277993=CARTESIAN_POINT('Ctrl Pts',(1.97099163821986,-0.303233195804582,
16.8128227341025));
#277994=CARTESIAN_POINT('Ctrl Pts',(1.32407364389988,1.49116981051517,16.923934162674));
#277995=CARTESIAN_POINT('Ctrl Pts',(-0.5342555596562,1.92128326343608,17.0350455912454));
#277996=CARTESIAN_POINT('Ctrl Pts',(-1.90378780228672,0.593591128428439,
17.1461570198168));
#277997=CARTESIAN_POINT('Ctrl Pts',(-1.53152124420933,-1.27718485278317,
17.2572684483882));
#277998=CARTESIAN_POINT('Ctrl Pts',(0.241952874713956,-1.97944866761738,
17.3683798769597));
#277999=CARTESIAN_POINT('Ctrl Pts',(1.79406134485088,-0.870690794290049,
17.4794913055311));
#278000=CARTESIAN_POINT('Ctrl Pts',(1.70476109126497,1.03467307520697,17.5906027341025));
#278001=CARTESIAN_POINT('Ctrl Pts',(0.0557540247604131,1.9934012658026,
17.7017141626739));
#278002=CARTESIAN_POINT('Ctrl Pts',(-1.64426309999555,1.12834333722013,
17.8128255912454));
#278003=CARTESIAN_POINT('Ctrl Pts',(-1.83992372329235,-0.769051907374047,
17.9239370198168));
#278004=CARTESIAN_POINT('Ctrl Pts',(-0.35221563866549,-1.96282801679883,
18.0350484483882));
#278005=CARTESIAN_POINT('Ctrl Pts',(1.45773897216931,-1.36079654304198,
18.1461598769597));
#278006=CARTESIAN_POINT('Ctrl Pts',(1.9339900970406,0.486259274017999,18.2572713055311));
#278007=CARTESIAN_POINT('Ctrl Pts',(0.640810407900626,1.88840216429967,
18.3683827341025));
#278008=CARTESIAN_POINT('Ctrl Pts',(-1.23865540855179,1.56287671424517,
18.479494162674));
#278009=CARTESIAN_POINT('Ctrl Pts',(-1.98485862900955,-0.192646451983672,
18.5906055912454));
#278010=CARTESIAN_POINT('Ctrl Pts',(-0.915093356425693,-1.77171970579917,
18.7017170198168));
#278011=CARTESIAN_POINT('Ctrl Pts',(0.991907748338541,-1.73019653084864,
18.8128284483882));
#278012=CARTESIAN_POINT('Ctrl Pts',(1.99138950296005,-0.10498786352432,
18.9239398769597));
#278013=CARTESIAN_POINT('Ctrl Pts',(1.16894462344746,1.61492636179448,19.0350513055311));
#278014=CARTESIAN_POINT('Ctrl Pts',(-0.723015887079062,1.85991781845732,
19.1461627341025));
#278015=CARTESIAN_POINT('Ctrl Pts',(-1.95347532330039,0.398060645082057,
19.2572762985614));
#278016=CARTESIAN_POINT('Ctrl Pts',(-1.58212954761068,-0.811583072307517,
19.331352720163));
#278017=CARTESIAN_POINT('Ctrl Pts',(-1.18169099246603,-1.20445112116229,
19.3683919989077));
#278018=CARTESIAN_POINT('Ctrl Pts',(0.90159620823838,-1.26416253453268,
0.00156140788979508));
#278019=CARTESIAN_POINT('Ctrl Pts',(1.32200468156816,-0.964344618051984,
0.0386104119716742));
#278020=CARTESIAN_POINT('Ctrl Pts',(1.83281328473215,0.0823017482344568,
0.112696558910696));
#278021=CARTESIAN_POINT('Ctrl Pts',(0.923292623565352,1.58732912987166,
0.223819848706861));
#278022=CARTESIAN_POINT('Ctrl Pts',(-0.831626641848217,1.63524339651075,
0.334931277278289));
#278023=CARTESIAN_POINT('Ctrl Pts',(-1.82527879279968,0.189405884300259,
0.446042705849719));
#278024=CARTESIAN_POINT('Ctrl Pts',(-1.14917218873408,-1.43094494259553,
0.557154134421147));
#278025=CARTESIAN_POINT('Ctrl Pts',(0.578437144337754,-1.74146511618339,
0.668265562992576));
#278026=CARTESIAN_POINT('Ctrl Pts',(1.77676889934914,-0.459034536695509,
0.779376991564005));
#278027=CARTESIAN_POINT('Ctrl Pts',(1.34954367020881,1.24354948588568,0.890488420135434));
#278028=CARTESIAN_POINT('Ctrl Pts',(-0.312411724366456,1.80830175055102,
1.00159984870686));
#278029=CARTESIAN_POINT('Ctrl Pts',(-1.68852933161371,0.71866549970365,
1.11271127727829));
#278030=CARTESIAN_POINT('Ctrl Pts',(-1.51979520469414,-1.02851234158217,
1.22382270584972));
#278031=CARTESIAN_POINT('Ctrl Pts',(0.0394205270115515,-1.83467811744561,
1.33493413442115));
#278032=CARTESIAN_POINT('Ctrl Pts',(1.56256870545359,-0.962281494451149,
1.44604556299257));
#278033=CARTESIAN_POINT('Ctrl Pts',(1.65610426516714,0.790521998350591,
1.557156991564));
#278034=CARTESIAN_POINT('Ctrl Pts',(0.234449389764976,1.82006526119027,
1.66826842013543));
#278035=CARTESIAN_POINT('Ctrl Pts',(-1.40170592803849,1.1844095345667,1.77937984870686));
#278036=CARTESIAN_POINT('Ctrl Pts',(-1.75542340175659,-0.53487753765843,
1.89049127727829));
#278037=CARTESIAN_POINT('Ctrl Pts',(-0.503082435079318,-1.76479830840923,
2.00160270584972));
#278038=CARTESIAN_POINT('Ctrl Pts',(1.20953479312287,-1.38008362078707,
2.11271413442115));
#278039=CARTESIAN_POINT('Ctrl Pts',(1.81553382429765,0.267286569474214,
2.22382556299257));
#278040=CARTESIAN_POINT('Ctrl Pts',(0.760478694725908,1.6701129591339,2.33493699156401));
#278041=CARTESIAN_POINT('Ctrl Pts',(-0.990347712058639,1.54493254928788,
2.44604842013543));
#278042=CARTESIAN_POINT('Ctrl Pts',(-1.83509285778272,0.00627439840333995,
2.55715984870686));
#278043=CARTESIAN_POINT('Ctrl Pts',(-1.00088904936001,-1.53812427049709,
2.66827127727829));
#278044=CARTESIAN_POINT('Ctrl Pts',(0.749040420284577,-1.67527419067305,
2.77938270584972));
#278045=CARTESIAN_POINT('Ctrl Pts',(1.813663626755,-0.279695213936149,2.89049413442115));
#278046=CARTESIAN_POINT('Ctrl Pts',(1.21894374614861,1.37178034211317,3.00160556299258));
#278047=CARTESIAN_POINT('Ctrl Pts',(-0.491002711504038,1.76819724613016,
3.11271699156401));
#278048=CARTESIAN_POINT('Ctrl Pts',(-1.75172476894188,0.546868812014197,
3.22382842013543));
#278049=CARTESIAN_POINT('Ctrl Pts',(-1.40977235979138,-1.17479660248503,
3.33493984870686));
#278050=CARTESIAN_POINT('Ctrl Pts',(0.221998064579255,-1.82162620288972,
3.4460512772783));
#278051=CARTESIAN_POINT('Ctrl Pts',(1.65065973806281,-0.801827657809858,
3.55716270584972));
#278052=CARTESIAN_POINT('Ctrl Pts',(1.56911258074583,0.951572841475777,
3.66827413442115));
#278053=CARTESIAN_POINT('Ctrl Pts',(0.0519650865987583,1.8343676821935,
3.77938556299258));
#278054=CARTESIAN_POINT('Ctrl Pts',(-1.51272590235006,1.03887704183597,
3.89049699156401));
#278055=CARTESIAN_POINT('Ctrl Pts',(-1.69340541780961,-0.707094940321402,
4.00160842013543));
#278056=CARTESIAN_POINT('Ctrl Pts',(-0.324767556026349,-1.80613709287233,
4.11271984870687));
#278057=CARTESIAN_POINT('Ctrl Pts',(1.34100412428894,-1.25272227661828,
4.2238312772783));
#278058=CARTESIAN_POINT('Ctrl Pts',(1.77987469110539,0.446823508399282,
4.33494270584973));
#278059=CARTESIAN_POINT('Ctrl Pts',(0.59031608246101,1.73756498770084,4.44605413442115));
#278060=CARTESIAN_POINT('Ctrl Pts',(-1.13932994707157,1.43858695788669,
4.55716556299259));
#278061=CARTESIAN_POINT('Ctrl Pts',(-1.8265890402882,-0.176571916212174,
4.66827699156401));
#278062=CARTESIAN_POINT('Ctrl Pts',(-0.842679427276936,-1.63018297946582,
4.77938842013544));
#278063=CARTESIAN_POINT('Ctrl Pts',(0.912207924670662,-1.59231964939954,
4.89049984870687));
#278064=CARTESIAN_POINT('Ctrl Pts',(1.83250506302419,-0.0976235508806328,
5.0016112772783));
#278065=CARTESIAN_POINT('Ctrl Pts',(1.07622085342053,1.48638953116558,5.11272270584973));
#278066=CARTESIAN_POINT('Ctrl Pts',(-0.6647110090249,1.71048660859329,5.22383413442115));
#278067=CARTESIAN_POINT('Ctrl Pts',(-1.79749062021609,0.369638517921229,
5.33494556299259));
#278068=CARTESIAN_POINT('Ctrl Pts',(-1.28572402643862,-1.30939638442082,
5.44605699156401));
#278069=CARTESIAN_POINT('Ctrl Pts',(0.402367241601951,-1.79044848196799,
5.55716842013545));
#278070=CARTESIAN_POINT('Ctrl Pts',(1.72232778743567,-0.633397313163549,
5.66827984870687));
#278071=CARTESIAN_POINT('Ctrl Pts',(1.4665095254785,1.1031568226579,5.7793912772783));
#278072=CARTESIAN_POINT('Ctrl Pts',(-0.131036280172964,1.83041925715784,
5.89050270584972));
#278073=CARTESIAN_POINT('Ctrl Pts',(-1.60869538664057,0.883008673058882,
6.00161413442115));
#278074=CARTESIAN_POINT('Ctrl Pts',(-1.61453936189358,-0.872277371363101,
6.11272556299259));
#278075=CARTESIAN_POINT('Ctrl Pts',(-0.143221481328173,-1.8295061549451,
6.22383699156401));
#278076=CARTESIAN_POINT('Ctrl Pts',(1.4591314883438,-1.11289732833692,6.33494842013545));
#278077=CARTESIAN_POINT('Ctrl Pts',(1.72650717094787,0.621914907653302,
6.44605984870686));
#278078=CARTESIAN_POINT('Ctrl Pts',(0.414280276548138,1.78772957019764,
6.55717127727831));
#278079=CARTESIAN_POINT('Ctrl Pts',(-1.27697672177988,1.31792853210186,
6.66828270584972));
#278080=CARTESIAN_POINT('Ctrl Pts',(-1.79991206211562,-0.357661477302979,
6.77939413442117));
#278081=CARTESIAN_POINT('Ctrl Pts',(-0.67608579060288,-1.7060226163333,
6.89050556299257));
#278082=CARTESIAN_POINT('Ctrl Pts',(1.06629965928017,-1.49352274850932,
7.00161699156402));
#278083=CARTESIAN_POINT('Ctrl Pts',(1.83311447847042,0.0854193919314032,
7.11272842013543));
#278084=CARTESIAN_POINT('Ctrl Pts',(0.922790388040553,1.58621028348571,
7.22383984870687));
#278085=CARTESIAN_POINT('Ctrl Pts',(-0.83180594145737,1.63575794036039,
7.33495127727829));
#278086=CARTESIAN_POINT('Ctrl Pts',(-1.82537281749998,0.188730603845873,
7.44606270584973));
#278087=CARTESIAN_POINT('Ctrl Pts',(-1.14888372445405,-1.43096867589072,
7.55717413442116));
#278088=CARTESIAN_POINT('Ctrl Pts',(0.578733172960644,-1.74145717093782,
7.66828556299258));
#278089=CARTESIAN_POINT('Ctrl Pts',(1.77685999539097,-0.458665150709145,
7.77939699156402));
#278090=CARTESIAN_POINT('Ctrl Pts',(1.34931582442854,1.24376523895894,7.89050842013544));
#278091=CARTESIAN_POINT('Ctrl Pts',(-0.312733936388572,1.80825956342743,
8.00161984870688));
#278092=CARTESIAN_POINT('Ctrl Pts',(-1.68865958480786,0.718355044760163,
8.1127312772783));
#278093=CARTESIAN_POINT('Ctrl Pts',(-1.51960987677947,-1.02878131111046,
8.22384270584974));
#278094=CARTESIAN_POINT('Ctrl Pts',(0.0397495373380485,-1.83467303298905,
8.33495413442116));
#278095=CARTESIAN_POINT('Ctrl Pts',(1.56274161243117,-0.961999904611144,
8.44606556299259));
#278096=CARTESIAN_POINT('Ctrl Pts',(1.6559622277092,0.790818730238608,8.55717699156402));
#278097=CARTESIAN_POINT('Ctrl Pts',(0.234122699405938,1.82010761366429,
8.66828842013545));
#278098=CARTESIAN_POINT('Ctrl Pts',(-1.40191855683668,1.18415772754004,
8.77939984870686));
#278099=CARTESIAN_POINT('Ctrl Pts',(-1.75532733845545,-0.535192580821834,
8.89051127727831));
#278100=CARTESIAN_POINT('Ctrl Pts',(-0.502765618493741,-1.7648886357378,
9.00162270584972));
#278101=CARTESIAN_POINT('Ctrl Pts',(1.20978252953801,-1.3798664409719,9.11273413442116));
#278102=CARTESIAN_POINT('Ctrl Pts',(1.81548580983413,0.26761247726283,9.22384556299259));
#278103=CARTESIAN_POINT('Ctrl Pts',(0.760178865566043,1.67024945922534,
9.33495699156402));
#278104=CARTESIAN_POINT('Ctrl Pts',(-0.990625042304408,1.54475473433657,
9.44606842013544));
#278105=CARTESIAN_POINT('Ctrl Pts',(-1.83509395429444,0.00594496491354616,
9.55717984870688));
#278106=CARTESIAN_POINT('Ctrl Pts',(-1.00061290996535,-1.53830392579183,
9.6682912772783));
#278107=CARTESIAN_POINT('Ctrl Pts',(0.749341152814527,-1.67513969578493,
9.77940270584973));
#278108=CARTESIAN_POINT('Ctrl Pts',(1.81371380825452,-0.279369621545994,
9.89051413442117));
#278109=CARTESIAN_POINT('Ctrl Pts',(1.21869746509954,1.37199914440783,10.0016255629926));
#278110=CARTESIAN_POINT('Ctrl Pts',(-0.491320129629947,1.76810907296927,
10.112736991564));
#278111=CARTESIAN_POINT('Ctrl Pts',(-1.7518229143681,0.546554334344457,
10.2238484201354));
#278112=CARTESIAN_POINT('Ctrl Pts',(-1.40956143808614,-1.17504966531477,
10.3349598487069));
#278113=CARTESIAN_POINT('Ctrl Pts',(0.222325078573523,-1.82158632052756,
10.4460712772783));
#278114=CARTESIAN_POINT('Ctrl Pts',(1.65080365522765,-0.801531319152839,
10.5571827058497));
#278115=CARTESIAN_POINT('Ctrl Pts',(1.56894172950593,0.951854512575722,
10.6682941344212));
#278116=CARTESIAN_POINT('Ctrl Pts',(0.0516357808464248,1.8343769813842,
10.7794055629926));
#278117=CARTESIAN_POINT('Ctrl Pts',(-1.51291237674398,1.03860546117894,
10.890516991564));
#278118=CARTESIAN_POINT('Ctrl Pts',(-1.69327845313648,-0.70739892835625,
11.0016284201355));
#278119=CARTESIAN_POINT('Ctrl Pts',(-0.324443313821911,-1.80619536590374,
11.1127398487069));
#278120=CARTESIAN_POINT('Ctrl Pts',(1.34122899085663,-1.25248151993613,
11.2238512772783));
#278121=CARTESIAN_POINT('Ctrl Pts',(1.77979444885685,0.447143023555279,
11.3349627058497));
#278122=CARTESIAN_POINT('Ctrl Pts',(0.590004146013124,1.73767093299715,
11.4460741344212));
#278123=CARTESIAN_POINT('Ctrl Pts',(-1.13958818323841,1.43838240267295,
11.5571855629926));
#278124=CARTESIAN_POINT('Ctrl Pts',(-1.82655731273908,-0.176899821863194,
11.668296991564));
#278125=CARTESIAN_POINT('Ctrl Pts',(-0.842386763935508,-1.63033423065398,
11.7794084201354));
#278126=CARTESIAN_POINT('Ctrl Pts',(0.912493762525382,-1.59215586455853,
11.8905198487069));
#278127=CARTESIAN_POINT('Ctrl Pts',(1.83252255883466,-0.0972945787694221,
12.0016312772783));
#278128=CARTESIAN_POINT('Ctrl Pts',(1.07595400005526,1.48658270992936,12.1127427058498));
#278129=CARTESIAN_POINT('Ctrl Pts',(-0.665018064150505,1.71036725239036,
12.2238541344211));
#278130=CARTESIAN_POINT('Ctrl Pts',(-1.79755694860324,0.369315827204919,
12.3349655629926));
#278131=CARTESIAN_POINT('Ctrl Pts',(-1.28548894343276,-1.3096271759581,
12.446076991564));
#278132=CARTESIAN_POINT('Ctrl Pts',(0.402688655676732,-1.79037622031939,
12.5571884201355));
#278133=CARTESIAN_POINT('Ctrl Pts',(1.72244146690194,-0.633088111397257,
12.6682998487069));
#278134=CARTESIAN_POINT('Ctrl Pts',(1.4663114635989,1.10342007205519,12.7794112772783));
#278135=CARTESIAN_POINT('Ctrl Pts',(-0.131364874156623,1.83039570408523,
12.8905227058497));
#278136=CARTESIAN_POINT('Ctrl Pts',(-1.6088538780642,0.882719866511245,
13.0016341344212));
#278137=CARTESIAN_POINT('Ctrl Pts',(-1.61438274501066,-0.872567198734688,
13.1127455629926));
#278138=CARTESIAN_POINT('Ctrl Pts',(-0.142893046844922,-1.82953183652519,
13.223856991564));
#278139=CARTESIAN_POINT('Ctrl Pts',(1.45933125169217,-1.11263536773302,
13.3349684201355));
#278140=CARTESIAN_POINT('Ctrl Pts',(1.72639549722492,0.62222483947312,13.4460798487069));
#278141=CARTESIAN_POINT('Ctrl Pts',(0.413959337412072,1.78780391281181,
13.5571912772783));
#278142=CARTESIAN_POINT('Ctrl Pts',(-1.27721329517889,1.31769926854125,
13.6683027058497));
#278143=CARTESIAN_POINT('Ctrl Pts',(-1.7998478258745,-0.357984590996087,
13.7794141344212));
#278144=CARTESIAN_POINT('Ctrl Pts',(-0.675779515246169,-1.70614395947982,
13.8905255629926));
#278145=CARTESIAN_POINT('Ctrl Pts',(1.06656775867382,-1.49333130277691,
14.001636991564));
#278146=CARTESIAN_POINT('Ctrl Pts',(1.83309911447898,0.0857484704951466,
14.1127484201355));
#278147=CARTESIAN_POINT('Ctrl Pts',(0.922505617368107,1.58637591686842,
14.2238598487069));
#278148=CARTESIAN_POINT('Ctrl Pts',(-0.83209957863139,1.63560858854962,
14.3349712772783));
#278149=CARTESIAN_POINT('Ctrl Pts',(-1.82540666892521,0.1884029106443,14.4460827058497));
#278150=CARTESIAN_POINT('Ctrl Pts',(-1.14862681904651,-1.43117489995561,
14.5571941344212));
#278151=CARTESIAN_POINT('Ctrl Pts',(0.579045789294013,-1.74135324894081,
14.6683055629926));
#278152=CARTESIAN_POINT('Ctrl Pts',(1.77694230613423,-0.458346162159357,
14.779416991564));
#278153=CARTESIAN_POINT('Ctrl Pts',(1.34909252247358,1.24400744752661,14.8905284201355));
#278154=CARTESIAN_POINT('Ctrl Pts',(-0.313058549345564,1.8082033924251,
15.0016398487069));
#278155=CARTESIAN_POINT('Ctrl Pts',(-1.6887885163929,0.718051885726373,
15.1127512772783));
#278156=CARTESIAN_POINT('Ctrl Pts',(-1.51942516590475,-1.02905409425885,
15.2238627058497));
#278157=CARTESIAN_POINT('Ctrl Pts',(0.0400788964287514,-1.83466586760579,
15.3349741344212));
#278158=CARTESIAN_POINT('Ctrl Pts',(1.56291428506798,-0.961719346392447,
15.4460855629926));
#278159=CARTESIAN_POINT('Ctrl Pts',(1.6558202335798,0.791115995137488,15.5571969915641));
#278160=CARTESIAN_POINT('Ctrl Pts',(0.233795950680089,1.82014961394571,
15.6683084201354));
#278161=CARTESIAN_POINT('Ctrl Pts',(-1.40213111374382,1.1839060366265,15.7794198487069));
#278162=CARTESIAN_POINT('Ctrl Pts',(-1.75523123262381,-0.535507687818136,
15.8905312772783));
#278163=CARTESIAN_POINT('Ctrl Pts',(-0.502448778326618,-1.76497886358149,
16.0016427058498));
#278164=CARTESIAN_POINT('Ctrl Pts',(1.21003022308683,-1.37964923906714,
16.1127541344212));
#278165=CARTESIAN_POINT('Ctrl Pts',(1.81543773890125,0.267938388163036,
16.2238655629926));
#278166=CARTESIAN_POINT('Ctrl Pts',(0.759879010835324,1.67038589937133,
16.334976991564));
#278167=CARTESIAN_POINT('Ctrl Pts',(-0.990902340059985,1.54457687272166,
16.4460884201355));
#278168=CARTESIAN_POINT('Ctrl Pts',(-1.83509499196587,0.0056155297747307,
16.5571998487069));
#278169=CARTESIAN_POINT('Ctrl Pts',(-1.00033673816072,-1.53848353109199,
16.6683112772783));
#278170=CARTESIAN_POINT('Ctrl Pts',(0.74964186109952,-1.67500514647217,
16.7794227058498));
#278171=CARTESIAN_POINT('Ctrl Pts',(1.8137639313726,-0.279044021638752,
16.8905341344212));
#278172=CARTESIAN_POINT('Ctrl Pts',(1.21845114470182,1.37221790565629,17.0016455629926));
#278173=CARTESIAN_POINT('Ctrl Pts',(-0.491637531813608,1.76802083661681,
17.112756991564));
#278174=CARTESIAN_POINT('Ctrl Pts',(-1.75192100352765,0.546239850970993,
17.2238684201355));
#278175=CARTESIAN_POINT('Ctrl Pts',(-1.40935047060202,-1.17530271298651,
17.3349798487069));
#278176=CARTESIAN_POINT('Ctrl Pts',(0.222652084736599,-1.82154633622422,
17.4460912772783));
#278177=CARTESIAN_POINT('Ctrl Pts',(1.65094752045689,-0.801235036942007,
17.5572027058497));
#278178=CARTESIAN_POINT('Ctrl Pts',(1.56877082529708,0.952136309552117,
17.6683141344212));
#278179=CARTESIAN_POINT('Ctrl Pts',(0.051306478007515,1.83438592359057,
17.7794255629926));
#278180=CARTESIAN_POINT('Ctrl Pts',(-1.51309881109001,1.03833441378922,
17.8905369915641));
#278181=CARTESIAN_POINT('Ctrl Pts',(-1.69315141732336,-0.707703971899209,
18.0016484201354));
#278182=CARTESIAN_POINT('Ctrl Pts',(-0.324119092688714,-1.80625152908954,
18.1127598487069));
#278183=CARTESIAN_POINT('Ctrl Pts',(1.34145387418529,-1.25224462643346,
18.2238712772783));
#278184=CARTESIAN_POINT('Ctrl Pts',(1.77971403511999,0.447469951372195,
18.3349827058498));
#278185=CARTESIAN_POINT('Ctrl Pts',(0.589692407699955,1.73776269118328,
18.4460941344212));
#278186=CARTESIAN_POINT('Ctrl Pts',(-1.13984679582908,1.43820468768718,
18.5572055629926));
#278187=CARTESIAN_POINT('Ctrl Pts',(-1.82652474031938,-0.177278877971518,
18.668316991564));
#278188=CARTESIAN_POINT('Ctrl Pts',(-0.842095568311332,-1.63038809326605,
18.7794284201355));
#278189=CARTESIAN_POINT('Ctrl Pts',(0.9127824097774,-1.59217725787693,18.8905398487069));
#278190=CARTESIAN_POINT('Ctrl Pts',(1.83253464080909,-0.0966128908919654,
19.0016512772783));
#278191=CARTESIAN_POINT('Ctrl Pts',(1.07569690031554,1.48610228985601,19.1127627058498));
#278192=CARTESIAN_POINT('Ctrl Pts',(-0.665340284739988,1.71155056623269,
19.2238741344212));
#278193=CARTESIAN_POINT('Ctrl Pts',(-1.79764490803661,0.366307003311719,
19.33498769888));
#278194=CARTESIAN_POINT('Ctrl Pts',(-1.45592170589159,-0.746842389038948,
19.4090641204817));
#278195=CARTESIAN_POINT('Ctrl Pts',(-1.08742648045863,-1.10837101401327,
19.4461033992263));
#278196=CARTESIAN_POINT('Ctrl Pts',(0.863566907998541,1.75641557941956,
1.92055572834082E-15));
#278197=CARTESIAN_POINT('Ctrl Pts',(0.902606995688333,1.73244080950236,
2.43072380935166E-15));
#278198=CARTESIAN_POINT('Ctrl Pts',(0.940685126167239,1.70703143391729,
2.63212312969157E-15));
#278199=CARTESIAN_POINT('Ctrl Pts',(0.977710780925362,1.68018273146334,
2.4459601011273E-15));
#278200=CARTESIAN_POINT('Ctrl Pts',(1.03606710713796,1.63786635248171,2.04295423620313E-15));
#278201=CARTESIAN_POINT('Ctrl Pts',(1.09181123604325,1.59197570838927,-9.03406496512887E-16));
#278202=CARTESIAN_POINT('Ctrl Pts',(1.14478006703473,1.54285501782175,9.74914593498966E-16));
#278203=CARTESIAN_POINT('Ctrl Pts',(1.16983151419263,1.51962353694747,1.8632608275243E-15));
#278204=CARTESIAN_POINT('Ctrl Pts',(1.19426155983482,1.49566911335637,1.92711446182748E-16));
#278205=CARTESIAN_POINT('Ctrl Pts',(1.21804938169849,1.47102626716015,6.97358837342676E-16));
#278206=CARTESIAN_POINT('Ctrl Pts',(1.23021944053223,1.45841877035958,8.54673365253237E-16));
#278207=CARTESIAN_POINT('Ctrl Pts',(1.24222136284868,1.44563106829319,-1.63299175600747E-15));
#278208=CARTESIAN_POINT('Ctrl Pts',(1.25405211098615,1.43266770693123,-9.57567358739198E-16));
#278209=CARTESIAN_POINT('Ctrl Pts',(1.26392059005265,1.42185447189777,-4.55923984025048E-16));
#278210=CARTESIAN_POINT('Ctrl Pts',(1.27366323022463,1.41092637478828,3.63847824488057E-16));
#278211=CARTESIAN_POINT('Ctrl Pts',(1.28327753990859,1.39988788299174,4.9960036108132E-16));
#278212=CARTESIAN_POINT('Ctrl Pts',(1.33011375332078,1.34611375104404,1.52177178458909E-15));
#278213=CARTESIAN_POINT('Ctrl Pts',(1.37391850734965,1.28971037306795,-1.41152132602092E-15));
#278214=CARTESIAN_POINT('Ctrl Pts',(1.41452895199254,1.2310109768871,-7.84095011141517E-16));
#278215=CARTESIAN_POINT('Ctrl Pts',(1.45487911675909,1.17268779603001,-1.60689987954089E-16));
#278216=CARTESIAN_POINT('Ctrl Pts',(1.49207610172446,1.11209686113068,-5.01359578401628E-15));
#278217=CARTESIAN_POINT('Ctrl Pts',(1.5259112036015,1.04955135028031,-3.68455266297474E-15));
#278218=CARTESIAN_POINT('Ctrl Pts',(1.53054536577512,1.040984920022,-3.50252272906105E-15));
#278219=CARTESIAN_POINT('Ctrl Pts',(1.53511638288187,1.03238181735526,-3.52147310612354E-15));
#278220=CARTESIAN_POINT('Ctrl Pts',(1.53962364151379,1.02374284391693,-3.58046925441613E-15));
#278221=CARTESIAN_POINT('Ctrl Pts',(1.54538639912254,1.01269748043125,-3.73160264907701E-15));
#278222=CARTESIAN_POINT('Ctrl Pts',(1.5510405224455,1.00160191092775,-9.50044333076555E-16));
#278223=CARTESIAN_POINT('Ctrl Pts',(1.55658450782952,0.990459465485314,
-1.04083408558608E-15));
#278224=CARTESIAN_POINT('Ctrl Pts',(1.58754494280248,0.928234381242756,
-1.95974260143647E-15));
#278225=CARTESIAN_POINT('Ctrl Pts',(1.61508262262489,0.86453306559026,-1.88413048647842E-15));
#278226=CARTESIAN_POINT('Ctrl Pts',(1.63904429710683,0.799662226664679,
-2.2065682614425E-15));
#278227=CARTESIAN_POINT('Ctrl Pts',(1.66267977657407,0.735674487301784,
-2.52461662719312E-15));
#278228=CARTESIAN_POINT('Ctrl Pts',(1.68283613808164,0.670547857459508,
-2.36383228719471E-15));
#278229=CARTESIAN_POINT('Ctrl Pts',(1.69931635736196,0.604571550293125,
-4.16333634234434E-15));
#278230=CARTESIAN_POINT('Ctrl Pts',(1.71527817949359,0.540670575313434,
-5.9062357033828E-15));
#278231=CARTESIAN_POINT('Ctrl Pts',(1.72779149233561,0.475971746451621,
-1.53638505387586E-15));
#278232=CARTESIAN_POINT('Ctrl Pts',(1.73662900130601,0.410745883467762,
-1.76247905159244E-15));
#278233=CARTESIAN_POINT('Ctrl Pts',(1.73865871892773,0.395765408321034,
-1.81440623750726E-15));
#278234=CARTESIAN_POINT('Ctrl Pts',(1.74049433596503,0.380757194592868,
-1.77301121448585E-15));
#278235=CARTESIAN_POINT('Ctrl Pts',(1.74213272345364,0.365724650926664,
-1.70696790036118E-15));
#278236=CARTESIAN_POINT('Ctrl Pts',(1.74338727089007,0.354213919032973,
-1.74377001770268E-15));
#278237=CARTESIAN_POINT('Ctrl Pts',(1.74452611236442,0.342688540754893,
-1.34699067263872E-15));
#278238=CARTESIAN_POINT('Ctrl Pts',(1.74554673034743,0.331165227615983,
-2.02615701994091E-15));
#278239=CARTESIAN_POINT('Ctrl Pts',(1.75129561321446,0.266257320271039,
-4.77896472164434E-15));
#278240=CARTESIAN_POINT('Ctrl Pts',(1.75331133583169,0.201296883564266,
-1.89713026672775E-15));
#278241=CARTESIAN_POINT('Ctrl Pts',(1.75142675830796,0.136544317949457,
-1.45716771982052E-15));
#278242=CARTESIAN_POINT('Ctrl Pts',(1.75088407860913,0.117898280647071,
-1.2709926870932E-15));
#278243=CARTESIAN_POINT('Ctrl Pts',(1.75001766131977,0.099269521756727,
-4.72295564128628E-15));
#278244=CARTESIAN_POINT('Ctrl Pts',(1.74882271567549,0.0806644060278795,
-4.56579218877096E-15));
#278245=CARTESIAN_POINT('Ctrl Pts',(1.74456498482946,0.0143722064518782,
-3.40614148876069E-15));
#278246=CARTESIAN_POINT('Ctrl Pts',(1.73613992417247,-0.0516216682407977,
-2.7009660656099E-15));
#278247=CARTESIAN_POINT('Ctrl Pts',(1.72372303569837,-0.117012374160561,
-1.88737914186277E-15));
#278248=CARTESIAN_POINT('Ctrl Pts',(1.7117534570167,-0.180047425267717,
-1.10310112257602E-15));
#278249=CARTESIAN_POINT('Ctrl Pts',(1.69607360968479,-0.242522628982395,
-2.53169565084214E-15));
#278250=CARTESIAN_POINT('Ctrl Pts',(1.67680428334833,-0.304137057490082,
-2.4980018054066E-15));
#278251=CARTESIAN_POINT('Ctrl Pts',(1.67349444731961,-0.314720388313531,
-2.69394111988223E-15));
#278252=CARTESIAN_POINT('Ctrl Pts',(1.67008022174013,-0.325273006340074,
3.29470571676352E-16));
#278253=CARTESIAN_POINT('Ctrl Pts',(1.66656493085673,-0.335786380672971,
2.4980018054066E-16));
#278254=CARTESIAN_POINT('Ctrl Pts',(1.64601993144971,-0.397231443570826,
4.68513083847165E-17));
#278255=CARTESIAN_POINT('Ctrl Pts',(1.62200297335448,-0.457413864499819,
-2.65433772659743E-15));
#278256=CARTESIAN_POINT('Ctrl Pts',(1.59470046562981,-0.516060019276523,
-1.13797860024079E-15));
#278257=CARTESIAN_POINT('Ctrl Pts',(1.56765678382067,-0.574150212496288,
3.64005544772621E-16));
#278258=CARTESIAN_POINT('Ctrl Pts',(1.53738877393808,-0.630733917539196,
-2.58600310425349E-15));
#278259=CARTESIAN_POINT('Ctrl Pts',(1.50403879475748,-0.685513423969216,
-2.3037127760972E-15));
#278260=CARTESIAN_POINT('Ctrl Pts',(1.4709648894784,-0.739839461088768,
-2.02375927075665E-15));
#278261=CARTESIAN_POINT('Ctrl Pts',(1.43485912858928,-0.792391764160348,
-9.14736882961259E-16));
#278262=CARTESIAN_POINT('Ctrl Pts',(1.39583294870606,-0.842837370270167,
8.60422844084496E-16));
#278263=CARTESIAN_POINT('Ctrl Pts',(1.38892463177069,-0.851767125527953,
1.12372394253433E-15));
#278264=CARTESIAN_POINT('Ctrl Pts',(1.38192474839882,-0.860630742755753,
-1.42167219695244E-15));
#278265=CARTESIAN_POINT('Ctrl Pts',(1.37483385167802,-0.869426208469204,
-1.27675647831893E-15));
#278266=CARTESIAN_POINT('Ctrl Pts',(1.36805999011309,-0.877828427467431,
-1.10795478880039E-15));
#278267=CARTESIAN_POINT('Ctrl Pts',(1.36120614272911,-0.886164561590754,
8.11183197120448E-16));
#278268=CARTESIAN_POINT('Ctrl Pts',(1.35427819652575,-0.89442703186717,
5.55111512312578E-16));
#278269=CARTESIAN_POINT('Ctrl Pts',(1.31436511271567,-0.942028537268739,
-7.1629539480613E-16));
#278270=CARTESIAN_POINT('Ctrl Pts',(1.27194408914578,-0.987251877392324,
1.06778634412269E-17));
#278271=CARTESIAN_POINT('Ctrl Pts',(1.22715435283182,-1.02982897690716,
-1.38777878078145E-16));
#278272=CARTESIAN_POINT('Ctrl Pts',(1.18376706222622,-1.07107291227764,
-2.83553896506172E-16));
#278273=CARTESIAN_POINT('Ctrl Pts',(1.1381563430115,-1.10983414583466,1.71437262194897E-16));
#278274=CARTESIAN_POINT('Ctrl Pts',(1.09042633843192,-1.14582699077891,
-5.55111512312578E-16));
#278275=CARTESIAN_POINT('Ctrl Pts',(1.04308447972006,-1.18152713778282,
-1.27575190891385E-15));
#278276=CARTESIAN_POINT('Ctrl Pts',(0.993657096245488,-1.21450424181457,
5.94987629519964E-16));
#278277=CARTESIAN_POINT('Ctrl Pts',(0.942232789017055,-1.24443055068302,
9.15933995315754E-16));
#278278=CARTESIAN_POINT('Ctrl Pts',(0.929479875758739,-1.25185209200677,
9.75669572373557E-16));
#278279=CARTESIAN_POINT('Ctrl Pts',(0.916604109661386,-1.25908574890519,
1.77947334077032E-15));
#278280=CARTESIAN_POINT('Ctrl Pts',(0.903606778650208,-1.26612599672284,
5.55111512312578E-17));
#278281=CARTESIAN_POINT('Ctrl Pts',(-0.684401294465645,1.39375859696713,
-0.231689979925561));
#278282=CARTESIAN_POINT('Ctrl Pts',(-1.14800519021184,1.16611376614941,
-0.194632647470989));
#278283=CARTESIAN_POINT('Ctrl Pts',(-1.82210733642078,0.215869300640666,
-0.120523386424568));
#278284=CARTESIAN_POINT('Ctrl Pts',(-1.16801489871654,-1.41729336359585,
-0.00936219678629828));
#278285=CARTESIAN_POINT('Ctrl Pts',(0.556977146514337,-1.7482231903558,
0.101793588989252));
#278286=CARTESIAN_POINT('Ctrl Pts',(1.7712308476463,-0.480771985689559,
0.212949374764799));
#278287=CARTESIAN_POINT('Ctrl Pts',(1.36418695589471,1.22803976333708,0.324105160540349));
#278288=CARTESIAN_POINT('Ctrl Pts',(-0.292095232734673,1.81186540287904,
0.435260946315896));
#278289=CARTESIAN_POINT('Ctrl Pts',(-1.68082790602658,0.737104570480516,
0.546416732091446));
#278290=CARTESIAN_POINT('Ctrl Pts',(-1.53068522271668,-1.01270541030781,
0.657572517866994));
#278291=CARTESIAN_POINT('Ctrl Pts',(0.0209552616995192,-1.83521194377032,
0.768728303642543));
#278292=CARTESIAN_POINT('Ctrl Pts',(1.55339315684676,-0.977479777233187,
0.879884089418091));
#278293=CARTESIAN_POINT('Ctrl Pts',(1.66358198078138,0.775239234716729,
0.99103987519364));
#278294=CARTESIAN_POINT('Ctrl Pts',(0.250621806749922,1.81815076116018,
1.10219566096919));
#278295=CARTESIAN_POINT('Ctrl Pts',(-1.39180062373996,1.19640434318354,
1.21335144674473));
#278296=CARTESIAN_POINT('Ctrl Pts',(-1.75991773480115,-0.52075105178842,
1.32450723252028));
#278297=CARTESIAN_POINT('Ctrl Pts',(-0.51668649624412,-1.76111466039208,
1.43566301829583));
#278298=CARTESIAN_POINT('Ctrl Pts',(1.19961287026365,-1.38903568181859,
1.54681880407138));
#278299=CARTESIAN_POINT('Ctrl Pts',(1.81756935651455,0.254818854352526,
1.65797458984693));
#278300=CARTESIAN_POINT('Ctrl Pts',(0.771393309043584,1.66536574983418,
1.76913037562248));
#278301=CARTESIAN_POINT('Ctrl Pts',(-0.981055945000064,1.55113512014234,
1.88028616139803));
#278302=CARTESIAN_POINT('Ctrl Pts',(-1.83526878868891,0.016714169768612,
1.99144194717358));
#278303=CARTESIAN_POINT('Ctrl Pts',(-1.00914391160594,-1.53300992150868,
2.10259773294912));
#278304=CARTESIAN_POINT('Ctrl Pts',(0.740934210662865,-1.67913888064429,
2.21375351872467));
#278305=CARTESIAN_POINT('Ctrl Pts',(1.81262685979311,-0.287879739532146,
2.32490930450022));
#278306=CARTESIAN_POINT('Ctrl Pts',(1.22471232570858,1.36695668999331,2.43606509027577));
#278307=CARTESIAN_POINT('Ctrl Pts',(-0.484525859611966,1.77023319621169,
2.54722087605132));
#278308=CARTESIAN_POINT('Ctrl Pts',(-1.75014124923941,0.552717363477061,
2.65837666182686));
#278309=CARTESIAN_POINT('Ctrl Pts',(-1.41336011130569,-1.17085612758582,
2.76953244760242));
#278310=CARTESIAN_POINT('Ctrl Pts',(0.217467055686965,-1.82241569244561,
2.88068823337796));
#278311=CARTESIAN_POINT('Ctrl Pts',(1.64918546226433,-0.805405604147006,
2.99184401915352));
#278312=CARTESIAN_POINT('Ctrl Pts',(1.57094056800582,0.949018760557804,
3.10299980492906));
#278313=CARTESIAN_POINT('Ctrl Pts',(0.0543719317205851,1.8345393343365,
3.21415559070461));
#278314=CARTESIAN_POINT('Ctrl Pts',(-1.51197862623999,1.04039007585601,
3.32531137648016));
#278315=CARTESIAN_POINT('Ctrl Pts',(-1.6939898909823,-0.70632083743466,
3.43646716225571));
#278316=CARTESIAN_POINT('Ctrl Pts',(-0.325015759708903,-1.80633762959686,
3.54762294803126));
#278317=CARTESIAN_POINT('Ctrl Pts',(1.34153670982427,-1.2525055418417,3.6587787338068));
#278318=CARTESIAN_POINT('Ctrl Pts',(1.779803310452,0.448097146001531,3.76993451958235));
#278319=CARTESIAN_POINT('Ctrl Pts',(0.588515356479842,1.73843048504668,
3.8810903053579));
#278320=CARTESIAN_POINT('Ctrl Pts',(-1.14160622813708,1.43708945303688,
3.99224609113345));
#278321=CARTESIAN_POINT('Ctrl Pts',(-1.82649454585514,-0.180023748746552,
4.103401876909));
#278322=CARTESIAN_POINT('Ctrl Pts',(-0.839078688908557,-1.6323105801198,
4.21455766268455));
#278323=CARTESIAN_POINT('Ctrl Pts',(0.916581889884211,-1.59008443652773,
4.3257134484601));
#278324=CARTESIAN_POINT('Ctrl Pts',(1.83303726855532,-0.0920067836558015,
4.43686923423564));
#278325=CARTESIAN_POINT('Ctrl Pts',(1.07119807827886,1.49031055597253,4.5480250200112));
#278326=CARTESIAN_POINT('Ctrl Pts',(-0.671409996451009,1.7081274814302,
4.65918080578674));
#278327=CARTESIAN_POINT('Ctrl Pts',(-1.79928766176102,0.36201489801663,
4.77033659156229));
#278328=CARTESIAN_POINT('Ctrl Pts',(-1.27977126558102,-1.31555174126471,
4.88149237733784));
#278329=CARTESIAN_POINT('Ctrl Pts',(0.411479716340706,-1.78862386185346,
4.99264816311339));
#278330=CARTESIAN_POINT('Ctrl Pts',(1.72598758178942,-0.624065496290367,
5.10380394888895));
#278331=CARTESIAN_POINT('Ctrl Pts',(1.46021356520572,1.11187554165951,5.21495973466448));
#278332=CARTESIAN_POINT('Ctrl Pts',(-0.142504624869778,1.82980417204742,
5.32611552044004));
#278333=CARTESIAN_POINT('Ctrl Pts',(-1.61474825118621,0.87239839605682,
5.43727130621559));
#278334=CARTESIAN_POINT('Ctrl Pts',(-1.60855864176201,-0.883759001178613,
5.54842709199114));
#278335=CARTESIAN_POINT('Ctrl Pts',(-0.129602886982468,-1.83076322003618,
5.65958287776667));
#278336=CARTESIAN_POINT('Ctrl Pts',(1.46801484214636,-1.10155494615087,
5.77073866354224));
#278337=CARTESIAN_POINT('Ctrl Pts',(1.72154569482533,0.636216391473685,
5.88189444931778));
#278338=CARTESIAN_POINT('Ctrl Pts',(0.398861573927917,1.79147992480942,
5.99305023509333));
#278339=CARTESIAN_POINT('Ctrl Pts',(-1.28901272873415,1.30649801427816,
6.10420602086888));
#278340=CARTESIAN_POINT('Ctrl Pts',(-1.79669113519176,-0.374688992198572,
6.21536180664442));
#278341=CARTESIAN_POINT('Ctrl Pts',(-0.659352811222979,-1.71281777970798,
6.32651759241998));
#278342=CARTESIAN_POINT('Ctrl Pts',(1.0816765893424,-1.48272270914694,6.43767337819552));
#278343=CARTESIAN_POINT('Ctrl Pts',(1.83234317710919,0.104925485240009,
6.54882916397107));
#278344=CARTESIAN_POINT('Ctrl Pts',(0.905350693048038,1.59650587181786,
6.65998494974661));
#278345=CARTESIAN_POINT('Ctrl Pts',(-0.850563917802709,1.62635540331244,
6.77114073552217));
#278346=CARTESIAN_POINT('Ctrl Pts',(-1.82771814648395,0.167144408116774,
6.88229652129771));
#278347=CARTESIAN_POINT('Ctrl Pts',(-1.13144789469704,-1.44510087458871,
6.99345230707328));
#278348=CARTESIAN_POINT('Ctrl Pts',(0.600754844274818,-1.7342388800946,
7.1046080928488));
#278349=CARTESIAN_POINT('Ctrl Pts',(1.78291770696527,-0.435540269482793,
7.21576387862437));
#278350=CARTESIAN_POINT('Ctrl Pts',(1.33267453197674,1.26193084912447,7.3269196643999));
#278351=CARTESIAN_POINT('Ctrl Pts',(-0.337740467970948,1.8040017329388,
7.43807545017548));
#278352=CARTESIAN_POINT('Ctrl Pts',(-1.69892662525787,0.69436244004221,
7.54923123595101));
#278353=CARTESIAN_POINT('Ctrl Pts',(-1.50460740514568,-1.05102208945971,
7.66038702172655));
#278354=CARTESIAN_POINT('Ctrl Pts',(0.0673021562935621,-1.83411049173971,
7.77154280750212));
#278355=CARTESIAN_POINT('Ctrl Pts',(1.57759112478382,-0.937921702038478,
7.88269859327765));
#278356=CARTESIAN_POINT('Ctrl Pts',(1.64346722608163,0.817010619849554,
7.9938543790532));
#278357=CARTESIAN_POINT('Ctrl Pts',(0.204615536465528,1.82390333032986,
8.10501016482876));
#278358=CARTESIAN_POINT('Ctrl Pts',(-1.42157830350579,1.16086433451675,
8.21616595060431));
#278359=CARTESIAN_POINT('Ctrl Pts',(-1.74620169150925,-0.565040289467627,
8.32732173637986));
#278360=CARTESIAN_POINT('Ctrl Pts',(-0.472035537466569,-1.77360461420242,
8.43847752215539));
#278361=CARTESIAN_POINT('Ctrl Pts',(1.23431750795601,-1.35828979444915,
8.54963330793096));
#278362=CARTESIAN_POINT('Ctrl Pts',(1.81055257623992,0.300649704510773,
8.6607890937065));
#278363=CARTESIAN_POINT('Ctrl Pts',(0.729079638460007,1.68431996869195,
8.77194487948205));
#278364=CARTESIAN_POINT('Ctrl Pts',(-1.01992495213898,1.52585843647297,
8.8831006652576));
#278365=CARTESIAN_POINT('Ctrl Pts',(-1.8351053716353,-0.0296504830769352,
8.99425645103314));
#278366=CARTESIAN_POINT('Ctrl Pts',(-0.970097705763678,-1.55801197602055,
9.10541223680869));
#278367=CARTESIAN_POINT('Ctrl Pts',(0.783113238274159,-1.65988690343384,
9.21656802258424));
#278368=CARTESIAN_POINT('Ctrl Pts',(1.81932037818187,-0.242000491081359,
9.32772380835979));
#278369=CARTESIAN_POINT('Ctrl Pts',(1.18979187689078,1.3974570354169,9.43887959413534));
#278370=CARTESIAN_POINT('Ctrl Pts',(-0.52908776821942,1.75742909093711,
9.55003537991088));
#278371=CARTESIAN_POINT('Ctrl Pts',(-1.7635445687253,0.508332007915007,
9.66119116568645));
#278372=CARTESIAN_POINT('Ctrl Pts',(-1.38333301384016,-1.20618433457385,
9.77234695146198));
#278373=CARTESIAN_POINT('Ctrl Pts',(0.263432322574806,-1.81634090621069,
9.88350273723755));
#278374=CARTESIAN_POINT('Ctrl Pts',(1.66900396159649,-0.763489785345338,
9.99465852301308));
#278375=CARTESIAN_POINT('Ctrl Pts',(1.54646685326738,0.98839827392439,10.1058143087887));
#278376=CARTESIAN_POINT('Ctrl Pts',(0.00801367742611086,1.83532739780278,
10.2169700945642));
#278377=CARTESIAN_POINT('Ctrl Pts',(-1.53777667127697,1.00186515331543,
10.3281258803398));
#278378=CARTESIAN_POINT('Ctrl Pts',(-1.67560752022996,-0.748886048942189,
10.4392816661153));
#278379=CARTESIAN_POINT('Ctrl Pts',(-0.279283527308905,-1.81397122014803,
10.5504374518909));
#278380=CARTESIAN_POINT('Ctrl Pts',(1.37274722898226,-1.21821833899879,
10.6615932376664));
#278381=CARTESIAN_POINT('Ctrl Pts',(1.76791634996442,0.492912421916842,
10.7727490234419));
#278382=CARTESIAN_POINT('Ctrl Pts',(0.544414394587412,1.75274180731717,
10.8839048092175));
#278383=CARTESIAN_POINT('Ctrl Pts',(-1.17754317725016,1.40779364321019,
10.995060594993));
#278384=CARTESIAN_POINT('Ctrl Pts',(-1.82136428509877,-0.226103996245259,
11.1062163807686));
#278385=CARTESIAN_POINT('Ctrl Pts',(-0.797578388881661,-1.65298505430036,
11.2173721665441));
#278386=CARTESIAN_POINT('Ctrl Pts',(0.956455332261048,-1.56642397630427,
11.3285279523197));
#278387=CARTESIAN_POINT('Ctrl Pts',(1.83477647673596,-0.0456744629728,11.4396837380952));
#278388=CARTESIAN_POINT('Ctrl Pts',(1.0332106658487,1.51689373264178,11.5508395238708));
#278389=CARTESIAN_POINT('Ctrl Pts',(-0.714343466617656,1.69062245573992,
11.6619953096463));
#278390=CARTESIAN_POINT('Ctrl Pts',(-1.80785810902362,0.316448943415789,
11.7731510954219));
#278391=CARTESIAN_POINT('Ctrl Pts',(-1.24613174905026,-1.34745929072473,
11.8843068811974));
#278392=CARTESIAN_POINT('Ctrl Pts',(0.456529485789276,-1.77765905188718,
11.995462666973));
#278393=CARTESIAN_POINT('Ctrl Pts',(1.74120087955567,-0.580267501404289,
12.1066184527485));
#278394=CARTESIAN_POINT('Ctrl Pts',(1.43166138097717,1.14840609819434,12.2177742385241));
#278395=CARTESIAN_POINT('Ctrl Pts',(-0.188680446328495,1.8256205973106,
12.3289300242996));
#278396=CARTESIAN_POINT('Ctrl Pts',(-1.63626999315856,0.831331092670267,
12.4400858100752));
#278397=CARTESIAN_POINT('Ctrl Pts',(-1.58572140065101,-0.924109579903169,
12.5512415958507));
#278398=CARTESIAN_POINT('Ctrl Pts',(-0.0833160127418071,-1.83345284045492,
12.6623973816263));
#278399=CARTESIAN_POINT('Ctrl Pts',(1.4953719549543,-1.06412104221633,12.7735531674018));
#278400=CARTESIAN_POINT('Ctrl Pts',(1.70492538643103,0.679500038892133,
12.8847089531774));
#278401=CARTESIAN_POINT('Ctrl Pts',(0.353481087205217,1.8009836193424,12.9958647389529));
#278402=CARTESIAN_POINT('Ctrl Pts',(-1.32160387064712,1.27352035132619,
13.1070205247285));
#278403=CARTESIAN_POINT('Ctrl Pts',(-1.78665309357124,-0.419954282492473,
13.218176310504));
#278404=CARTESIAN_POINT('Ctrl Pts',(-0.615876228847231,-1.72892664589692,
13.3293320962796));
#278405=CARTESIAN_POINT('Ctrl Pts',(1.118785368473,-1.454926175255,13.4404878820551));
#278406=CARTESIAN_POINT('Ctrl Pts',(1.82910805030238,0.151177433734229,
13.5516436678307));
#278407=CARTESIAN_POINT('Ctrl Pts',(0.864733681776538,1.61886581771084,
13.6627994536062));
#278408=CARTESIAN_POINT('Ctrl Pts',(-0.891374639248479,1.60435099920687,
13.7739552393818));
#278409=CARTESIAN_POINT('Ctrl Pts',(-1.83135704640849,0.120922474012888,
13.8851110251573));
#278410=CARTESIAN_POINT('Ctrl Pts',(-1.09458326452843,-1.47322040210069,
13.9962668109329));
#278411=CARTESIAN_POINT('Ctrl Pts',(0.644370440058169,-1.71851028863102,
14.1074225967084));
#278412=CARTESIAN_POINT('Ctrl Pts',(1.79335064629233,-0.390364362607969,
14.218578382484));
#278413=CARTESIAN_POINT('Ctrl Pts',(1.30037261113015,1.29519185774694,14.3297341682595));
#278414=CARTESIAN_POINT('Ctrl Pts',(-0.383202215655351,1.79489468718037,
14.440889954035));
#278415=CARTESIAN_POINT('Ctrl Pts',(-1.71592427562836,0.651225580318193,
14.5520457398106));
#278416=CARTESIAN_POINT('Ctrl Pts',(-1.47757822808704,-1.08869346284187,
14.6632015255862));
#278417=CARTESIAN_POINT('Ctrl Pts',(0.113610752837791,-1.83182517533499,
14.7743573113617));
#278418=CARTESIAN_POINT('Ctrl Pts',(1.60077985771719,-0.897772088716452,
14.8855130971372));
#278419=CARTESIAN_POINT('Ctrl Pts',(1.62230492612552,0.858264296601231,
14.9966688829128));
#278420=CARTESIAN_POINT('Ctrl Pts',(0.158478008843229,1.82848997723926,
15.1078246686883));
#278421=CARTESIAN_POINT('Ctrl Pts',(-1.45044840319647,1.12458450363503,
15.2189804544639));
#278422=CARTESIAN_POINT('Ctrl Pts',(-1.73137144106518,-0.608969464929189,
15.3301362402394));
#278423=CARTESIAN_POINT('Ctrl Pts',(-0.427083236250261,-1.78496240449614,
15.441292026015));
#278424=CARTESIAN_POINT('Ctrl Pts',(1.26823437542981,-1.32667721964631,
15.5524478117905));
#278425=CARTESIAN_POINT('Ctrl Pts',(1.80238036177279,0.346288763393393,
15.6636035975661));
#278426=CARTESIAN_POINT('Ctrl Pts',(0.686300668452443,1.70219924469092,
15.7747593833416));
#278427=CARTESIAN_POINT('Ctrl Pts',(-1.05814305448729,1.49960799957408,
15.8859151691172));
#278428=CARTESIAN_POINT('Ctrl Pts',(-1.83377082810206,-0.0759962248318786,
15.9970709548927));
#278429=CARTESIAN_POINT('Ctrl Pts',(-0.930432399362984,-1.58201973006431,
16.1082267406683));
#278430=CARTESIAN_POINT('Ctrl Pts',(0.824792496331553,-1.6395756201318,
16.2193825264438));
#278431=CARTESIAN_POINT('Ctrl Pts',(1.82485284047757,-0.195966800714232,
16.3305383122194));
#278432=CARTESIAN_POINT('Ctrl Pts',(1.15411212440423,1.42706554861312,16.4416940979949));
#278433=CARTESIAN_POINT('Ctrl Pts',(-0.573312022371201,1.7435034273505,
16.5528498837705));
#278434=CARTESIAN_POINT('Ctrl Pts',(-1.77582242710928,0.463622243834642,
16.664005669546));
#278435=CARTESIAN_POINT('Ctrl Pts',(-1.35242309784257,-1.24074277651812,
16.7751614553216));
#278436=CARTESIAN_POINT('Ctrl Pts',(0.309229470154115,-1.80910696534636,
16.8863172410971));
#278437=CARTESIAN_POINT('Ctrl Pts',(1.68775733648514,-0.721086720278873,
16.9974730268726));
#278438=CARTESIAN_POINT('Ctrl Pts',(1.52100620597035,1.02714700757733,17.1086288126482));
#278439=CARTESIAN_POINT('Ctrl Pts',(-0.0383496797956876,1.83494419322939,
17.2197845984237));
#278440=CARTESIAN_POINT('Ctrl Pts',(-1.56259335699694,0.962700851162004,
17.3309403841993));
#278441=CARTESIAN_POINT('Ctrl Pts',(-1.65615576691353,-0.790973320458416,
17.4420961699749));
#278442=CARTESIAN_POINT('Ctrl Pts',(-0.233373138809018,-1.82044719570678,
17.5532519557504));
#278443=CARTESIAN_POINT('Ctrl Pts',(1.40308183362072,-1.18315363838809,
17.6644077415259));
#278444=CARTESIAN_POINT('Ctrl Pts',(1.75490085728126,0.537413028835761,
17.7755635273015));
#278445=CARTESIAN_POINT('Ctrl Pts',(0.499966531306351,1.76593475496119,
17.8867193130771));
#278446=CARTESIAN_POINT('Ctrl Pts',(-1.2127296557621,1.37759903842392,17.9978750988526));
#278447=CARTESIAN_POINT('Ctrl Pts',(-1.81506973055227,-0.272039250033519,
18.1090308846281));
#278448=CARTESIAN_POINT('Ctrl Pts',(-0.755572766356513,-1.67260595256776,
18.2201866704037));
#278449=CARTESIAN_POINT('Ctrl Pts',(0.995725379371007,-1.54176132508072,
18.3313424561792));
#278450=CARTESIAN_POINT('Ctrl Pts',(1.83533145130754,0.000682196077548512,
18.4424982419548));
#278451=CARTESIAN_POINT('Ctrl Pts',(0.994589208429304,1.54251800818852,
18.5536540277304));
#278452=CARTESIAN_POINT('Ctrl Pts',(-0.756869254017628,1.67202109132145,
18.6648098135059));
#278453=CARTESIAN_POINT('Ctrl Pts',(-1.81518310367551,0.27071417263847,
18.7759655992815));
#278454=CARTESIAN_POINT('Ctrl Pts',(-1.21187150681834,-1.37856996990797,
18.887121385057));
#278455=CARTESIAN_POINT('Ctrl Pts',(0.501620277758415,-1.76543975111565,
18.9982771708326));
#278456=CARTESIAN_POINT('Ctrl Pts',(1.75466810626107,-0.536327979791566,
19.1094329566081));
#278457=CARTESIAN_POINT('Ctrl Pts',(1.40342470040972,1.18464272774391,19.2205887423837));
#278458=CARTESIAN_POINT('Ctrl Pts',(-0.237431411965544,1.81947273062068,
19.3317564093966));
#278459=CARTESIAN_POINT('Ctrl Pts',(-1.17973169467503,1.13405785918806,
19.4058721478177));
#278460=CARTESIAN_POINT('Ctrl Pts',(-1.40184687339747,0.667677681709342,
19.4429359576469));
#278461=CARTESIAN_POINT('Ctrl Pts',(-0.74373075200652,1.51458090132225,
-0.153976802596129));
#278462=CARTESIAN_POINT('Ctrl Pts',(-1.24752359518877,1.26720196942433,
-0.116919470141557));
#278463=CARTESIAN_POINT('Ctrl Pts',(-1.98006238519882,0.234582603216642,
-0.0428102090951364));
#278464=CARTESIAN_POINT('Ctrl Pts',(-1.26926790758847,-1.54015585248706,
0.0683509805431339));
#278465=CARTESIAN_POINT('Ctrl Pts',(0.605260444971807,-1.89977336184568,
0.179506766318684));
#278466=CARTESIAN_POINT('Ctrl Pts',(1.92477550955777,-0.522449202466397,
0.290662552094231));
#278467=CARTESIAN_POINT('Ctrl Pts',(1.48244575045285,1.33449621452525,0.40181833786978));
#278468=CARTESIAN_POINT('Ctrl Pts',(-0.317416417613436,1.96893259775306,
0.51297412364533));
#278469=CARTESIAN_POINT('Ctrl Pts',(-1.82653570741519,0.801002775628761,
0.624129909420876));
#278470=CARTESIAN_POINT('Ctrl Pts',(-1.66337743803531,-1.1004949325196,
0.735285695196427));
#278471=CARTESIAN_POINT('Ctrl Pts',(0.0227718338178408,-1.99430300624619,
0.846441480971973));
#278472=CARTESIAN_POINT('Ctrl Pts',(1.68805388015145,-1.06221565574388,
0.957597266747523));
#278473=CARTESIAN_POINT('Ctrl Pts',(1.80779476543365,0.842443261991487,
1.06875305252307));
#278474=CARTESIAN_POINT('Ctrl Pts',(0.272347738542586,1.97576282189037,
1.17990883829862));
#278475=CARTESIAN_POINT('Ctrl Pts',(-1.51245319508847,1.30011837945816,
1.29106462407417));
#278476=CARTESIAN_POINT('Ctrl Pts',(-1.91248168429486,-0.565893978410986,
1.40222040984972));
#278477=CARTESIAN_POINT('Ctrl Pts',(-0.561477074211649,-1.91378236910807,
1.51337619562527));
#278478=CARTESIAN_POINT('Ctrl Pts',(1.30360504770008,-1.50944856556618,
1.62453198140082));
#278479=CARTESIAN_POINT('Ctrl Pts',(1.97513101637244,0.276908620286904,
1.73568776717636));
#278480=CARTESIAN_POINT('Ctrl Pts',(0.838263940274534,1.80973316606173,
1.84684355295191));
#278481=CARTESIAN_POINT('Ctrl Pts',(-1.06610183475038,1.68560009850343,
1.95799933872746));
#278482=CARTESIAN_POINT('Ctrl Pts',(-1.99436477894357,0.0181630896254633,
2.06915512450301));
#278483=CARTESIAN_POINT('Ctrl Pts',(-1.09662469421168,-1.66590366058159,
2.18031091027856));
#278484=CARTESIAN_POINT('Ctrl Pts',(0.805164400096429,-1.82470026360773,
2.2914666960541));
#278485=CARTESIAN_POINT('Ctrl Pts',(1.96976006393103,-0.312835491254928,
2.40262248182966));
#278486=CARTESIAN_POINT('Ctrl Pts',(1.33088032760376,1.48545558757719,2.5137782676052));
#278487=CARTESIAN_POINT('Ctrl Pts',(-0.526528492639934,1.92369137360171,
2.62493405338075));
#278488=CARTESIAN_POINT('Ctrl Pts',(-1.90185769363675,0.600631389376298,
2.7360898391563));
#278489=CARTESIAN_POINT('Ctrl Pts',(-1.53588163397336,-1.27235543723032,
2.84724562493185));
#278490=CARTESIAN_POINT('Ctrl Pts',(0.236318864634813,-1.98039747202593,
2.9584014107074));
#278491=CARTESIAN_POINT('Ctrl Pts',(1.79215023987601,-0.875224697098474,
3.06955719648295));
#278492=CARTESIAN_POINT('Ctrl Pts',(1.70712244329213,1.03128740720606,3.1807129822585));
#278493=CARTESIAN_POINT('Ctrl Pts',(0.0590853319442645,1.99357208956899,
3.29186876803404));
#278494=CARTESIAN_POINT('Ctrl Pts',(-1.64304920198787,1.13057952951509,
3.4030245538096));
#278495=CARTESIAN_POINT('Ctrl Pts',(-1.84083868002521,-0.767550458818608,
3.51418033958514));
#278496=CARTESIAN_POINT('Ctrl Pts',(-0.353190762987942,-1.96292563222959,
3.6253361253607));
#278497=CARTESIAN_POINT('Ctrl Pts',(1.45783199726549,-1.3610828852297,3.73649191113624));
#278498=CARTESIAN_POINT('Ctrl Pts',(1.93409110299773,0.486941842545606,
3.84764769691179));
#278499=CARTESIAN_POINT('Ctrl Pts',(0.63953264288294,1.88913174538087,3.95880348268734));
#278500=CARTESIAN_POINT('Ctrl Pts',(-1.24056991915922,1.56166802758931,
4.06995926846289));
#278501=CARTESIAN_POINT('Ctrl Pts',(-1.98482991354544,-0.195629668028096,
4.18111505423843));
#278502=CARTESIAN_POINT('Ctrl Pts',(-0.911816838075705,-1.77381250602182,
4.29227084001398));
#278503=CARTESIAN_POINT('Ctrl Pts',(0.996038645384761,-1.72792585767379,
4.40342662578953));
#278504=CARTESIAN_POINT('Ctrl Pts',(1.99193981253791,-0.0999826782201581,
4.51458241156508));
#278505=CARTESIAN_POINT('Ctrl Pts',(1.16405821956878,1.61950276757159,4.62573819734063));
#278506=CARTESIAN_POINT('Ctrl Pts',(-0.729613262866601,1.85620183152771,
4.73689398311618));
#278507=CARTESIAN_POINT('Ctrl Pts',(-1.95526451597723,0.393397286820842,
4.84804976889172));
#278508=CARTESIAN_POINT('Ctrl Pts',(-1.39071222314098,-1.4295944407852,
4.95920555466728));
#278509=CARTESIAN_POINT('Ctrl Pts',(0.447150116962367,-1.94367629136597,
5.07036134044282));
#278510=CARTESIAN_POINT('Ctrl Pts',(1.87561019030566,-0.678164557271505,
5.18151712621837));
#278511=CARTESIAN_POINT('Ctrl Pts',(1.58679672543352,1.20826193553845,5.29267291199392));
#278512=CARTESIAN_POINT('Ctrl Pts',(-0.154858082057787,1.98842644499087,
5.40382869776946));
#278513=CARTESIAN_POINT('Ctrl Pts',(-1.75472773191285,0.948024967800771,
5.51498448354502));
#278514=CARTESIAN_POINT('Ctrl Pts',(-1.7480015569203,-0.960370402356234,
5.62614026932056));
#278515=CARTESIAN_POINT('Ctrl Pts',(-0.1408379168437,-1.98946863104116,
5.73729605509613));
#278516=CARTESIAN_POINT('Ctrl Pts',(1.59527428036014,-1.1970466670682,5.84845184087166));
#278517=CARTESIAN_POINT('Ctrl Pts',(1.87078324453736,0.691368790643559,
5.95960762664722));
#278518=CARTESIAN_POINT('Ctrl Pts',(0.433438131579671,1.94677994103349,
6.07076341242275));
#278519=CARTESIAN_POINT('Ctrl Pts',(-1.40075481130689,1.4197558632801,6.18191919819832));
#278520=CARTESIAN_POINT('Ctrl Pts',(-1.95244290141633,-0.40717007432604,
6.29307498397385));
#278521=CARTESIAN_POINT('Ctrl Pts',(-0.716510862989133,-1.86129872291801,
6.40423076974941));
#278522=CARTESIAN_POINT('Ctrl Pts',(1.17544509299558,-1.61125714461419,
6.51538655552495));
#278523=CARTESIAN_POINT('Ctrl Pts',(1.99118555161327,0.114021277682033,
6.62654234130051));
#278524=CARTESIAN_POINT('Ctrl Pts',(0.983833837275154,1.7349039550794,6.73769812707605));
#278525=CARTESIAN_POINT('Ctrl Pts',(-0.924297699803332,1.76734108616756,
6.8488539128516));
#278526=CARTESIAN_POINT('Ctrl Pts',(-1.98615958580523,0.181633841647562,
6.96000969862716));
#278527=CARTESIAN_POINT('Ctrl Pts',(-1.2295309789503,-1.57037394416718,
7.07116548440269));
#278528=CARTESIAN_POINT('Ctrl Pts',(0.652833148793089,-1.88457677810021,
7.18232127017825));
#278529=CARTESIAN_POINT('Ctrl Pts',(1.93747548067146,-0.473296434081779,
7.29347705595379));
#278530=CARTESIAN_POINT('Ctrl Pts',(1.44820157393307,1.37132525462613,7.40463284172934));
#278531=CARTESIAN_POINT('Ctrl Pts',(-0.367018552212401,1.96038724109538,
7.5157886275049));
#278532=CARTESIAN_POINT('Ctrl Pts',(-1.84620337048521,0.754555410507891,
7.62694441328044));
#278533=CARTESIAN_POINT('Ctrl Pts',(-1.63503898363787,-1.14213321232776,
7.738100199056));
#278534=CARTESIAN_POINT('Ctrl Pts',(0.0731364533010753,-1.99310607141621,
7.84925598483153));
#278535=CARTESIAN_POINT('Ctrl Pts',(1.71434952429531,-1.01922836561103,
7.96041177060709));
#278536=CARTESIAN_POINT('Ctrl Pts',(1.78593630058235,0.887835729727017,
8.07156755638263));
#278537=CARTESIAN_POINT('Ctrl Pts',(0.222353271448042,1.98201407043291,
8.18272334215819));
#278538=CARTESIAN_POINT('Ctrl Pts',(-1.54481224575705,1.26149747446308,
8.29387912793374));
#278539=CARTESIAN_POINT('Ctrl Pts',(-1.89757662307636,-0.614022566581862,
8.40503491370928));
#278540=CARTESIAN_POINT('Ctrl Pts',(-0.512955408022568,-1.92735505346007,
8.51619069948484));
#278541=CARTESIAN_POINT('Ctrl Pts',(1.34131816498633,-1.47603737520274,
8.62734648526037));
#278542=CARTESIAN_POINT('Ctrl Pts',(1.96750596464839,0.326712460415384,
8.73850227103594));
#278543=CARTESIAN_POINT('Ctrl Pts',(0.792282177385192,1.83033049040752,
8.84965805681147));
#278544=CARTESIAN_POINT('Ctrl Pts',(-1.10834032281716,1.65813222679472,
8.96081384258703));
#278545=CARTESIAN_POINT('Ctrl Pts',(-1.99418719557377,-0.0322208275386075,
9.07196962836257));
#278546=CARTESIAN_POINT('Ctrl Pts',(-1.05419364642014,-1.69307309604904,
9.18312541413812));
#278547=CARTESIAN_POINT('Ctrl Pts',(0.85099984806814,-1.80377936879921,
9.29428119991367));
#278548=CARTESIAN_POINT('Ctrl Pts',(1.97703383080595,-0.262979057277202,
9.40543698568922));
#278549=CARTESIAN_POINT('Ctrl Pts',(1.29293269093258,1.51859995042656,9.51659277146476));
#278550=CARTESIAN_POINT('Ctrl Pts',(-0.574953389067615,1.90977730458746,
9.62774855724032));
#278551=CARTESIAN_POINT('Ctrl Pts',(-1.91642292161226,0.552398351044574,
9.73890434301587));
#278552=CARTESIAN_POINT('Ctrl Pts',(-1.50325154405505,-1.31074617985853,
9.85006012879141));
#278553=CARTESIAN_POINT('Ctrl Pts',(0.286268773825686,-1.97379607402841,
9.96121591456697));
#278554=CARTESIAN_POINT('Ctrl Pts',(1.81368676754059,-0.829675275011727,
10.0723717003426));
#278555=CARTESIAN_POINT('Ctrl Pts',(1.68052714837671,1.07408065632265,10.183527486118));
#278556=CARTESIAN_POINT('Ctrl Pts',(0.00870836800959076,1.99442846877101,
10.2946832718936));
#278557=CARTESIAN_POINT('Ctrl Pts',(-1.67108363089793,1.08871495409159,
10.4058390576691));
#278558=CARTESIAN_POINT('Ctrl Pts',(-1.8208627762187,-0.813805568240236,
10.5169948434447));
#278559=CARTESIAN_POINT('Ctrl Pts',(-0.303494089605198,-1.97122096434986,
10.6281506292202));
#278560=CARTESIAN_POINT('Ctrl Pts',(1.49174809747102,-1.32382338943276,
10.7393064149959));
#278561=CARTESIAN_POINT('Ctrl Pts',(1.92117368432247,0.535642070215246,
10.8504622007714));
#278562=CARTESIAN_POINT('Ctrl Pts',(0.591608651771739,1.90468368919001,
10.9616179865469));
#278563=CARTESIAN_POINT('Ctrl Pts',(-1.27962217461932,1.52983261925617,
11.0727737723225));
#278564=CARTESIAN_POINT('Ctrl Pts',(-1.97925492015898,-0.245704525282156,
11.183929558098));
#278565=CARTESIAN_POINT('Ctrl Pts',(-0.866718955302711,-1.79627921138019,
11.2950853438736));
#278566=CARTESIAN_POINT('Ctrl Pts',(1.03936864128602,-1.70221431677358,
11.4062411296491));
#278567=CARTESIAN_POINT('Ctrl Pts',(1.99382978939585,-0.0496338960328293,
11.5173969154247));
#278568=CARTESIAN_POINT('Ctrl Pts',(1.12277774999351,1.64839038969449,11.6285527012001));
#278569=CARTESIAN_POINT('Ctrl Pts',(-0.776268554596024,1.83717932817215,
11.7397084869758));
#278570=CARTESIAN_POINT('Ctrl Pts',(-1.96457791915047,0.343881305546085,
11.8508642727512));
#278571=CARTESIAN_POINT('Ctrl Pts',(-1.35415656036116,-1.46426799553513,
11.9620200585268));
#278572=CARTESIAN_POINT('Ctrl Pts',(0.496105165967445,-1.93176096270167,
12.0731758443023));
#278573=CARTESIAN_POINT('Ctrl Pts',(1.8921423001653,-0.630569796805081,
12.184331630078));
#278574=CARTESIAN_POINT('Ctrl Pts',(1.55576940619927,1.24795925712822,12.2954874158536));
#278575=CARTESIAN_POINT('Ctrl Pts',(-0.205036798398212,1.98388020404971,
12.406643201629));
#278576=CARTESIAN_POINT('Ctrl Pts',(-1.77811515311006,0.903397617330303,
12.5177989874045));
#278577=CARTESIAN_POINT('Ctrl Pts',(-1.72318459844495,-1.00421889665539,
12.6289547731801));
#278578=CARTESIAN_POINT('Ctrl Pts',(-0.0905385207650955,-1.99239140958179,
12.7401105589556));
#278579=CARTESIAN_POINT('Ctrl Pts',(1.62500292968607,-1.1563676885962,12.8512663447312));
#278580=CARTESIAN_POINT('Ctrl Pts',(1.85272215295172,0.738404615830361,
12.9624221305067));
#278581=CARTESIAN_POINT('Ctrl Pts',(0.384123696043651,1.95710749292302,
13.0735779162823));
#278582=CARTESIAN_POINT('Ctrl Pts',(-1.43617121785037,1.38391942891767,
13.1847337020578));
#278583=CARTESIAN_POINT('Ctrl Pts',(-1.94153468089794,-0.456359327272094,
13.2958894878334));
#278584=CARTESIAN_POINT('Ctrl Pts',(-0.66926537767743,-1.87880403633801,
13.4070452736089));
#278585=CARTESIAN_POINT('Ctrl Pts',(1.21577076220752,-1.58105098161919,
13.5182010593846));
#278586=CARTESIAN_POINT('Ctrl Pts',(1.98766997776453,0.164282720367103,
13.62935684516));
#278587=CARTESIAN_POINT('Ctrl Pts',(0.939695813894015,1.7592022425144,13.7405126309357));
#278588=CARTESIAN_POINT('Ctrl Pts',(-0.968646225728449,1.74342916176703,
13.8516684167111));
#278589=CARTESIAN_POINT('Ctrl Pts',(-1.99011393510182,0.131405015243721,
13.9628242024868));
#278590=CARTESIAN_POINT('Ctrl Pts',(-1.18947062351344,-1.60093110049002,
14.0739799882622));
#278591=CARTESIAN_POINT('Ctrl Pts',(0.700229698322543,-1.86748470470437,
14.1851357740379));
#278592=CARTESIAN_POINT('Ctrl Pts',(1.94881283183385,-0.424204313034841,
14.2962915598133));
#278593=CARTESIAN_POINT('Ctrl Pts',(1.41309946048478,1.40746959736092,14.407447345589));
#278594=CARTESIAN_POINT('Ctrl Pts',(-0.416421293069648,1.95049072271464,
14.5186031313644));
#278595=CARTESIAN_POINT('Ctrl Pts',(-1.86467451511134,0.707679097763931,
14.6297589171399));
#278596=CARTESIAN_POINT('Ctrl Pts',(-1.60566669819292,-1.18307024602596,
14.7409147029155));
#278597=CARTESIAN_POINT('Ctrl Pts',(0.123459454748778,-1.99062264524212,
14.852070488691));
#278598=CARTESIAN_POINT('Ctrl Pts',(1.73954844475626,-0.975598258026157,
14.9632262744666));
#278599=CARTESIAN_POINT('Ctrl Pts',(1.7629394807519,0.93266560991816,15.0743820602423));
#278600=CARTESIAN_POINT('Ctrl Pts',(0.172216168564502,1.98699832511316,
15.1855378460178));
#278601=CARTESIAN_POINT('Ctrl Pts',(-1.5761850399453,1.22207261346044,15.2966936317933));
#278602=CARTESIAN_POINT('Ctrl Pts',(-1.88146076618887,-0.661759879420467,
15.4078494175689));
#278603=CARTESIAN_POINT('Ctrl Pts',(-0.464106276586993,-1.9396974291753,
15.5190052033444));
#278604=CARTESIAN_POINT('Ctrl Pts',(1.37817522173939,-1.44168436590672,
15.63016098912));
#278605=CARTESIAN_POINT('Ctrl Pts',(1.95862531632066,0.376307883244237,
15.7413167748956));
#278606=CARTESIAN_POINT('Ctrl Pts',(0.745794779142275,1.84975968712525,
15.852472560671));
#278607=CARTESIAN_POINT('Ctrl Pts',(-1.14987148038453,1.62960618902539,
15.9636283464467));
#278608=CARTESIAN_POINT('Ctrl Pts',(-1.99273696297838,-0.0825841942452913,
16.0747841322222));
#278609=CARTESIAN_POINT('Ctrl Pts',(-1.01108982941028,-1.71916203701588,
16.1859399179978));
#278610=CARTESIAN_POINT('Ctrl Pts',(0.896292202405808,-1.7817073386517,
16.2970957037733));
#278611=CARTESIAN_POINT('Ctrl Pts',(1.98304589182469,-0.212954793104663,
16.4082514895487));
#278612=CARTESIAN_POINT('Ctrl Pts',(1.25415992798953,1.55077516979464,16.5194072753243));
#278613=CARTESIAN_POINT('Ctrl Pts',(-0.623011360411622,1.8946444514862,
16.6305630610998));
#278614=CARTESIAN_POINT('Ctrl Pts',(-1.92976512438537,0.503812781831874,
16.7417188468755));
#278615=CARTESIAN_POINT('Ctrl Pts',(-1.46966210573103,-1.34830042796301,
16.8528746326509));
#278616=CARTESIAN_POINT('Ctrl Pts',(0.336035989762217,-1.96593503647267,
16.9640304184265));
#278617=CARTESIAN_POINT('Ctrl Pts',(1.83406583713234,-0.783596368200354,
17.075186204202));
#278618=CARTESIAN_POINT('Ctrl Pts',(1.6528593655804,1.11618844462176,17.1863419899777));
#278619=CARTESIAN_POINT('Ctrl Pts',(-0.0416741412155506,1.99401204491582,
17.2974977757531));
#278620=CARTESIAN_POINT('Ctrl Pts',(-1.69805162830248,1.04615557244237,
17.4086535615287));
#278621=CARTESIAN_POINT('Ctrl Pts',(-1.7997247870903,-0.859541305954033,
17.5198093473042));
#278622=CARTESIAN_POINT('Ctrl Pts',(-0.253603816106239,-1.97825833001708,
17.6309651330799));
#278623=CARTESIAN_POINT('Ctrl Pts',(1.52471235177915,-1.28571899605279,
17.7421209188553));
#278624=CARTESIAN_POINT('Ctrl Pts',(1.90702990312385,0.584000350826615,
17.853276704631));
#278625=CARTESIAN_POINT('Ctrl Pts',(0.543307687044726,1.91902030858541,
17.9644324904065));
#278626=CARTESIAN_POINT('Ctrl Pts',(-1.31785890259713,1.49702050112338,
18.075588276182));
#278627=CARTESIAN_POINT('Ctrl Pts',(-1.97241470254942,-0.295621819594443,
18.1867440619575));
#278628=CARTESIAN_POINT('Ctrl Pts',(-0.821071944577047,-1.81760100831636,
18.2978998477332));
#278629=CARTESIAN_POINT('Ctrl Pts',(1.08204293472263,-1.67541370682546,
18.4090556335087));
#278630=CARTESIAN_POINT('Ctrl Pts',(1.99443287366644,0.000741334369009545,
18.5202114192842));
#278631=CARTESIAN_POINT('Ctrl Pts',(1.08080827126461,1.67623598536489,18.6313672050597));
#278632=CARTESIAN_POINT('Ctrl Pts',(-0.822480822308558,1.81696544655156,
18.7425229908353));
#278633=CARTESIAN_POINT('Ctrl Pts',(-1.97253790377489,0.294181873738879,
18.8536787766108));
#278634=CARTESIAN_POINT('Ctrl Pts',(-1.31692636233974,-1.49807560082679,
18.9648345623864));
#278635=CARTESIAN_POINT('Ctrl Pts',(0.545104793658038,-1.91848239378999,
19.0759903481619));
#278636=CARTESIAN_POINT('Ctrl Pts',(1.90677697535665,-0.582821240926985,
19.1871461339374));
#278637=CARTESIAN_POINT('Ctrl Pts',(1.52508494104348,1.2873371717567,19.298301919713));
#278638=CARTESIAN_POINT('Ctrl Pts',(-0.258013893309452,1.97719939039036,
19.409469586726));
#278639=CARTESIAN_POINT('Ctrl Pts',(-1.28200041049253,1.23236719634106,
19.4835853251471));
#278640=CARTESIAN_POINT('Ctrl Pts',(-1.5233703351831,0.725557400798528,
19.5206491349764));
#278641=CARTESIAN_POINT('Ctrl Pts',(-0.803060209547395,1.63540320567737,
-0.0762636252666968));
#278642=CARTESIAN_POINT('Ctrl Pts',(-1.3470420001657,1.36829017269927,-0.0392062928121253));
#278643=CARTESIAN_POINT('Ctrl Pts',(-2.13801743397685,0.253295905792618,
0.0349029682342957));
#278644=CARTESIAN_POINT('Ctrl Pts',(-1.3705209164604,-1.66301834137826,
0.146064157872566));
#278645=CARTESIAN_POINT('Ctrl Pts',(0.653543743429279,-2.05132353333556,
0.257219943648115));
#278646=CARTESIAN_POINT('Ctrl Pts',(2.07832017146924,-0.564126419243238,
0.368375729423662));
#278647=CARTESIAN_POINT('Ctrl Pts',(1.60070454501101,1.44095266571342,0.479531515199212));
#278648=CARTESIAN_POINT('Ctrl Pts',(-0.342737602492205,2.12599979262709,
0.59068730097476));
#278649=CARTESIAN_POINT('Ctrl Pts',(-1.9722435088038,0.864900980777003,
0.70184308675031));
#278650=CARTESIAN_POINT('Ctrl Pts',(-1.79606965335395,-1.18828445473139,
0.812998872525858));
#278651=CARTESIAN_POINT('Ctrl Pts',(0.0245884059361645,-2.15339406872207,
0.924154658301406));
#278652=CARTESIAN_POINT('Ctrl Pts',(1.82271460345614,-1.14695153425457,
1.03531044407696));
#278653=CARTESIAN_POINT('Ctrl Pts',(1.95200755008591,0.90964728926624,1.14646622985251));
#278654=CARTESIAN_POINT('Ctrl Pts',(0.294073670335253,2.13337488262056,
1.25762201562806));
#278655=CARTESIAN_POINT('Ctrl Pts',(-1.63310576643698,1.40383241573278,
1.3687778014036));
#278656=CARTESIAN_POINT('Ctrl Pts',(-2.06504563378859,-0.61103690503355,
1.47993358717915));
#278657=CARTESIAN_POINT('Ctrl Pts',(-0.606267652179178,-2.06645007782405,
1.5910893729547));
#278658=CARTESIAN_POINT('Ctrl Pts',(1.4075972251365,-1.62986144931378,1.70224515873025));
#278659=CARTESIAN_POINT('Ctrl Pts',(2.13269267623034,0.29899838622128,1.8134009445058));
#278660=CARTESIAN_POINT('Ctrl Pts',(0.905134571505482,1.95410058228929,
1.92455673028135));
#278661=CARTESIAN_POINT('Ctrl Pts',(-1.1511477245007,1.82006507686451,2.0357125160569));
#278662=CARTESIAN_POINT('Ctrl Pts',(-2.15346076919824,0.0196120094823153,
2.14686830183245));
#278663=CARTESIAN_POINT('Ctrl Pts',(-1.18410547681742,-1.79879739965449,
2.25802408760799));
#278664=CARTESIAN_POINT('Ctrl Pts',(0.869394589529993,-1.97026164657118,
2.36917987338354));
#278665=CARTESIAN_POINT('Ctrl Pts',(2.12689326806894,-0.33779124297771,
2.48033565915909));
#278666=CARTESIAN_POINT('Ctrl Pts',(1.43704832949894,1.60395448516108,2.59149144493464));
#278667=CARTESIAN_POINT('Ctrl Pts',(-0.568531125667906,2.07714955099172,
2.70264723071019));
#278668=CARTESIAN_POINT('Ctrl Pts',(-2.05357413803409,0.648545415275535,
2.81380301648574));
#278669=CARTESIAN_POINT('Ctrl Pts',(-1.65840315664103,-1.37385474687483,
2.92495880226128));
#278670=CARTESIAN_POINT('Ctrl Pts',(0.255170673582664,-2.13837925160624,
3.03611458803684));
#278671=CARTESIAN_POINT('Ctrl Pts',(1.93511501748769,-0.945043790049941,
3.14727037381238));
#278672=CARTESIAN_POINT('Ctrl Pts',(1.84330431857845,1.11355605385433,3.25842615958794));
#278673=CARTESIAN_POINT('Ctrl Pts',(0.0637987321679423,2.15260484480149,
3.36958194536347));
#278674=CARTESIAN_POINT('Ctrl Pts',(-1.77411977773575,1.22076898317417,
3.48073773113904));
#278675=CARTESIAN_POINT('Ctrl Pts',(-1.98768746906812,-0.828780080202557,
3.59189351691457));
#278676=CARTESIAN_POINT('Ctrl Pts',(-0.381365766266981,-2.11951363486232,
3.70304930269013));
#278677=CARTESIAN_POINT('Ctrl Pts',(1.57412728470673,-1.46966022861769,
3.81420508846568));
#278678=CARTESIAN_POINT('Ctrl Pts',(2.08837889554347,0.525786539089682,
3.92536087424122));
#278679=CARTESIAN_POINT('Ctrl Pts',(0.690549929286038,2.03983300571505,
4.03651666001678));
#278680=CARTESIAN_POINT('Ctrl Pts',(-1.33953361018136,1.68624660214174,
4.14767244579232));
#278681=CARTESIAN_POINT('Ctrl Pts',(-2.14316528123572,-0.211235587309644,
4.25882823156787));
#278682=CARTESIAN_POINT('Ctrl Pts',(-0.984554987242856,-1.91531443192384,
4.36998401734341));
#278683=CARTESIAN_POINT('Ctrl Pts',(1.07549540088531,-1.86576727881985,
4.48113980311897));
#278684=CARTESIAN_POINT('Ctrl Pts',(2.15084235652051,-0.107958572784515,
4.59229558889452));
#278685=CARTESIAN_POINT('Ctrl Pts',(1.25691836085871,1.74869497917066,4.70345137467006));
#278686=CARTESIAN_POINT('Ctrl Pts',(-0.787816529282194,2.0042761816252,
4.81460716044562));
#278687=CARTESIAN_POINT('Ctrl Pts',(-2.11124137019343,0.424779675625053,
4.92576294622115));
#278688=CARTESIAN_POINT('Ctrl Pts',(-1.50165318070095,-1.54363714030569,
5.03691873199672));
#278689=CARTESIAN_POINT('Ctrl Pts',(0.482820517584028,-2.09872872087849,
5.14807451777225));
#278690=CARTESIAN_POINT('Ctrl Pts',(2.02523279882188,-0.73226361825264,
5.25923030354781));
#278691=CARTESIAN_POINT('Ctrl Pts',(1.71337988566132,1.30464832941739,5.37038608932336));
#278692=CARTESIAN_POINT('Ctrl Pts',(-0.167211539245795,2.14704871793432,
5.48154187509889));
#278693=CARTESIAN_POINT('Ctrl Pts',(-1.89470721263948,1.02365153954472,
5.59269766087446));
#278694=CARTESIAN_POINT('Ctrl Pts',(-1.8874444720786,-1.03698180353386,
5.70385344665));
#278695=CARTESIAN_POINT('Ctrl Pts',(-0.152072946704935,-2.14817404204614,
5.81500923242555));
#278696=CARTESIAN_POINT('Ctrl Pts',(1.72253371857393,-1.29253838798554,
5.9261650182011));
#278697=CARTESIAN_POINT('Ctrl Pts',(2.02002079424938,0.746521189813437,
6.03732080397665));
#278698=CARTESIAN_POINT('Ctrl Pts',(0.468014689231428,2.10207995725757,
6.1484765897522));
#278699=CARTESIAN_POINT('Ctrl Pts',(-1.51249689387964,1.53301371228206,
6.25963237552774));
#278700=CARTESIAN_POINT('Ctrl Pts',(-2.10819466764088,-0.439651156453509,
6.37078816130329));
#278701=CARTESIAN_POINT('Ctrl Pts',(-0.773668914755293,-2.00977966612803,
6.48194394707884));
#278702=CARTESIAN_POINT('Ctrl Pts',(1.26921359664876,-1.73979158008144,
6.59309973285439));
#278703=CARTESIAN_POINT('Ctrl Pts',(2.15002792611735,0.12311707012406,6.70425551862994));
#278704=CARTESIAN_POINT('Ctrl Pts',(1.06231698150227,1.87330203834093,6.81541130440548));
#278705=CARTESIAN_POINT('Ctrl Pts',(-0.998031481803957,1.90832676902269,
6.92656709018103));
#278706=CARTESIAN_POINT('Ctrl Pts',(-2.14460102512651,0.19612327517835,
7.03772287595658));
#278707=CARTESIAN_POINT('Ctrl Pts',(-1.32761406320357,-1.69564701374563,
7.14887866173214));
#278708=CARTESIAN_POINT('Ctrl Pts',(0.704911453311359,-2.03491467610582,
7.26003444750767));
#278709=CARTESIAN_POINT('Ctrl Pts',(2.09203325437767,-0.511052598680766,
7.37119023328324));
#278710=CARTESIAN_POINT('Ctrl Pts',(1.56372861588939,1.4807196601278,7.48234601905876));
#278711=CARTESIAN_POINT('Ctrl Pts',(-0.396296636453853,2.11677274925197,
7.59350180483433));
#278712=CARTESIAN_POINT('Ctrl Pts',(-1.99348011571256,0.814748380973568,
7.70465759060988));
#278713=CARTESIAN_POINT('Ctrl Pts',(-1.76547056213006,-1.23324433519582,
7.81581337638541));
#278714=CARTESIAN_POINT('Ctrl Pts',(0.0789707503085854,-2.15210165109273,
7.92696916216099));
#278715=CARTESIAN_POINT('Ctrl Pts',(1.85110792380678,-1.10053502918357,
8.0381249479365));
#278716=CARTESIAN_POINT('Ctrl Pts',(1.92840537508305,0.95866083960448,8.14928073371208));
#278717=CARTESIAN_POINT('Ctrl Pts',(0.240091006430557,2.14012481053595,
8.26043651948761));
#278718=CARTESIAN_POINT('Ctrl Pts',(-1.6680461880083,1.3621306144094,8.37159230526317));
#278719=CARTESIAN_POINT('Ctrl Pts',(-2.04895155464346,-0.663004843696095,
8.48274809103872));
#278720=CARTESIAN_POINT('Ctrl Pts',(-0.553875278578563,-2.08110549271774,
8.59390387681425));
#278721=CARTESIAN_POINT('Ctrl Pts',(1.44831882201665,-1.59378495595632,
8.70505966258983));
#278722=CARTESIAN_POINT('Ctrl Pts',(2.12445935305686,0.352775216319991,
8.81621544836534));
#278723=CARTESIAN_POINT('Ctrl Pts',(0.855484716310372,1.97634101212309,
8.92737123414092));
#278724=CARTESIAN_POINT('Ctrl Pts',(-1.19675569349533,1.79040601711647,
9.03852701991645));
#278725=CARTESIAN_POINT('Ctrl Pts',(-2.15326901951224,-0.0347911720002775,
9.149682805692));
#278726=CARTESIAN_POINT('Ctrl Pts',(-1.13828958707659,-1.82813421607752,
9.26083859146756));
#278727=CARTESIAN_POINT('Ctrl Pts',(0.918886457862119,-1.94767183416457,
9.37199437724309));
#278728=CARTESIAN_POINT('Ctrl Pts',(2.13474728343003,-0.283957623473044,
9.48315016301865));
#278729=CARTESIAN_POINT('Ctrl Pts',(1.39607350497437,1.63974286543622,9.5943059487942));
#278730=CARTESIAN_POINT('Ctrl Pts',(-0.620819009915808,2.0621255182378,
9.70546173456975));
#278731=CARTESIAN_POINT('Ctrl Pts',(-2.06930127449923,0.596464694174142,
9.81661752034531));
#278732=CARTESIAN_POINT('Ctrl Pts',(-1.62317007426996,-1.41530802514323,
9.92777330612084));
#278733=CARTESIAN_POINT('Ctrl Pts',(0.309105225076564,-2.13125124184614,
10.0389290918964));
#278734=CARTESIAN_POINT('Ctrl Pts',(1.95836957348472,-0.895860764678115,
10.1500848776719));
#278735=CARTESIAN_POINT('Ctrl Pts',(1.81458744348604,1.15976303872091,10.2612406634475));
#278736=CARTESIAN_POINT('Ctrl Pts',(0.00940305859307401,2.15352953973923,
10.372396449223));
#278737=CARTESIAN_POINT('Ctrl Pts',(-1.80439059051889,1.17556475486775,
10.4835522349986));
#278738=CARTESIAN_POINT('Ctrl Pts',(-1.96611803220744,-0.87872508753828,
10.5947080207741));
#278739=CARTESIAN_POINT('Ctrl Pts',(-0.327704651901493,-2.12847070855169,
10.7058638065496));
#278740=CARTESIAN_POINT('Ctrl Pts',(1.61074896595979,-1.42942843986673,
10.8170195923252));
#278741=CARTESIAN_POINT('Ctrl Pts',(2.07443101868052,0.578371718513652,
10.9281753781008));
#278742=CARTESIAN_POINT('Ctrl Pts',(0.638802908956066,2.05662557106286,
11.0393311638763));
#278743=CARTESIAN_POINT('Ctrl Pts',(-1.38170117198847,1.65187159530215,
11.1504869496518));
#278744=CARTESIAN_POINT('Ctrl Pts',(-2.13714555521918,-0.265305054319054,
11.2616427354274));
#278745=CARTESIAN_POINT('Ctrl Pts',(-0.93585952172376,-1.93957336846002,
11.3727985212029));
#278746=CARTESIAN_POINT('Ctrl Pts',(1.122281950311,-1.83800465724289,11.4839543069785));
#278747=CARTESIAN_POINT('Ctrl Pts',(2.15288310205574,-0.0535933290928604,
11.595110092754));
#278748=CARTESIAN_POINT('Ctrl Pts',(1.21234483413833,1.7798870467472,11.7062658785296));
#278749=CARTESIAN_POINT('Ctrl Pts',(-0.838193642574392,1.98373620060436,
11.8174216643051));
#278750=CARTESIAN_POINT('Ctrl Pts',(-2.12129772927731,0.371313667676383,
11.9285774500807));
#278751=CARTESIAN_POINT('Ctrl Pts',(-1.46218137167207,-1.58107670034554,
12.0397332358562));
#278752=CARTESIAN_POINT('Ctrl Pts',(0.535680846145613,-2.08586287351616,
12.1508890216318));
#278753=CARTESIAN_POINT('Ctrl Pts',(2.04308372077493,-0.680872092205875,
12.2620448074073));
#278754=CARTESIAN_POINT('Ctrl Pts',(1.67987743142135,1.34751241606212,12.3732005931829));
#278755=CARTESIAN_POINT('Ctrl Pts',(-0.221393150467926,2.14213981078881,
12.4843563789585));
#278756=CARTESIAN_POINT('Ctrl Pts',(-1.91996031306156,0.975464141990338,
12.595512164734));
#278757=CARTESIAN_POINT('Ctrl Pts',(-1.86064779623888,-1.08432821340761,
12.7066679505095));
#278758=CARTESIAN_POINT('Ctrl Pts',(-0.0977610287883846,-2.15132997870865,
12.8178237362851));
#278759=CARTESIAN_POINT('Ctrl Pts',(1.75463390441784,-1.24861433497609,
12.9289795220606));
#278760=CARTESIAN_POINT('Ctrl Pts',(2.00051891947241,0.797309192768591,
13.0401353078362));
#278761=CARTESIAN_POINT('Ctrl Pts',(0.414766304882087,2.11323136650364,
13.1512910936117));
#278762=CARTESIAN_POINT('Ctrl Pts',(-1.55073856505364,1.49431850650915,
13.2624468793873));
#278763=CARTESIAN_POINT('Ctrl Pts',(-2.09641626822463,-0.492764372051713,
13.3736026651628));
#278764=CARTESIAN_POINT('Ctrl Pts',(-0.72265452650763,-2.02868142677909,
13.4847584509384));
#278765=CARTESIAN_POINT('Ctrl Pts',(1.31275615594204,-1.70717578798336,
13.5959142367139));
#278766=CARTESIAN_POINT('Ctrl Pts',(2.14623190522668,0.177388006999977,
13.7070700224895));
#278767=CARTESIAN_POINT('Ctrl Pts',(1.01465794601149,1.89953866731797,13.818225808265));
#278768=CARTESIAN_POINT('Ctrl Pts',(-1.04591781220841,1.88250732432719,
13.9293815940406));
#278769=CARTESIAN_POINT('Ctrl Pts',(-2.14887082379515,0.141887556474556,
14.0405373798161));
#278770=CARTESIAN_POINT('Ctrl Pts',(-1.28435798249845,-1.72864179887936,
14.1516931655917));
#278771=CARTESIAN_POINT('Ctrl Pts',(0.756088956586916,-2.01645912077772,
14.2628489513672));
#278772=CARTESIAN_POINT('Ctrl Pts',(2.10427501737539,-0.458044263461713,
14.3740047371428));
#278773=CARTESIAN_POINT('Ctrl Pts',(1.52582630983939,1.51974733697488,14.4851605229183));
#278774=CARTESIAN_POINT('Ctrl Pts',(-0.449640370483944,2.10608675824893,
14.5963163086939));
#278775=CARTESIAN_POINT('Ctrl Pts',(-2.01342475459432,0.764132615209665,
14.7074720944694));
#278776=CARTESIAN_POINT('Ctrl Pts',(-1.73375516829879,-1.27744702921006,
14.818627880245));
#278777=CARTESIAN_POINT('Ctrl Pts',(0.133308156659764,-2.14942011514928,
14.9297836660205));
#278778=CARTESIAN_POINT('Ctrl Pts',(1.87831703179533,-1.05342442733586,
15.0409394517961));
#278779=CARTESIAN_POINT('Ctrl Pts',(1.90357403537827,1.00706692323509,15.1520952375716));
#278780=CARTESIAN_POINT('Ctrl Pts',(0.185954328285773,2.14550667298706,
15.2632510233471));
#278781=CARTESIAN_POINT('Ctrl Pts',(-1.70192167669414,1.31956072328585,
15.3744068091227));
#278782=CARTESIAN_POINT('Ctrl Pts',(-2.03155009131257,-0.714550293911744,
15.4855625948982));
#278783=CARTESIAN_POINT('Ctrl Pts',(-0.501129316923725,-2.09443245385447,
15.5967183806738));
#278784=CARTESIAN_POINT('Ctrl Pts',(1.48811606804899,-1.55669151216713,
15.7078741664493));
#278785=CARTESIAN_POINT('Ctrl Pts',(2.11487027086851,0.40632700309508,15.8190299522249));
#278786=CARTESIAN_POINT('Ctrl Pts',(0.805288889832107,1.99732012955959,
15.9301857380004));
#278787=CARTESIAN_POINT('Ctrl Pts',(-1.24159990628178,1.75960437847669,
16.041341523776));
#278788=CARTESIAN_POINT('Ctrl Pts',(-2.1517030978547,-0.0891721636587039,
16.1524973095515));
#278789=CARTESIAN_POINT('Ctrl Pts',(-1.09174725945757,-1.85630434396745,
16.2636530953271));
#278790=CARTESIAN_POINT('Ctrl Pts',(0.967791908480065,-1.92383905717159,
16.3748088811027));
#278791=CARTESIAN_POINT('Ctrl Pts',(2.1412389431718,-0.229942785495091,
16.4859646668782));
#278792=CARTESIAN_POINT('Ctrl Pts',(1.35420773157483,1.67448479097614,16.5971204526538));
#278793=CARTESIAN_POINT('Ctrl Pts',(-0.672710698452041,2.0457854756219,
16.7082762384293));
#278794=CARTESIAN_POINT('Ctrl Pts',(-2.08370782166148,0.544003319829105,
16.8194320242048));
#278795=CARTESIAN_POINT('Ctrl Pts',(-1.58690111361948,-1.45585807940792,
16.9305878099804));
#278796=CARTESIAN_POINT('Ctrl Pts',(0.362842509370316,-2.12276310759897,
17.0417435957559));
#278797=CARTESIAN_POINT('Ctrl Pts',(1.98037433777956,-0.846106016121839,
17.1528993815315));
#278798=CARTESIAN_POINT('Ctrl Pts',(1.78471252519044,1.2052298816662,17.264055167307));
#278799=CARTESIAN_POINT('Ctrl Pts',(-0.0449986026354138,2.15307989660224,
17.3752109530826));
#278800=CARTESIAN_POINT('Ctrl Pts',(-1.83350989960801,1.12961029372276,
17.4863667388581));
#278801=CARTESIAN_POINT('Ctrl Pts',(-1.94329380726708,-0.928109291449652,
17.5975225246337));
#278802=CARTESIAN_POINT('Ctrl Pts',(-0.273834493403462,-2.1360694643274,
17.7086783104092));
#278803=CARTESIAN_POINT('Ctrl Pts',(1.64634286993759,-1.3882843537175,17.8198340961848));
#278804=CARTESIAN_POINT('Ctrl Pts',(2.05915894896643,0.630587672817468,
17.9309898819603));
#278805=CARTESIAN_POINT('Ctrl Pts',(0.586648842783101,2.07210586220963,
18.0421456677359));
#278806=CARTESIAN_POINT('Ctrl Pts',(-1.42298814943216,1.61644196382285,
18.1533014535114));
#278807=CARTESIAN_POINT('Ctrl Pts',(-2.12975967454656,-0.31920438915537,
18.264457239287));
#278808=CARTESIAN_POINT('Ctrl Pts',(-0.886571122797581,-1.96259606406497,
18.3756130250625));
#278809=CARTESIAN_POINT('Ctrl Pts',(1.16836049007425,-1.8090660885702,18.4867688108381));
#278810=CARTESIAN_POINT('Ctrl Pts',(2.15353429602535,0.000800472660472174,
18.5979245966136));
#278811=CARTESIAN_POINT('Ctrl Pts',(1.16702733409992,1.80995396254128,18.7090803823892));
#278812=CARTESIAN_POINT('Ctrl Pts',(-0.888092390599487,1.96190980178168,
18.8202361681647));
#278813=CARTESIAN_POINT('Ctrl Pts',(-2.12989270387429,0.317649574839287,
18.9313919539403));
#278814=CARTESIAN_POINT('Ctrl Pts',(-1.42198121786115,-1.6175812317456,
19.0425477397158));
#278815=CARTESIAN_POINT('Ctrl Pts',(0.588589309557662,-2.07152503646434,
19.1537035254914));
#278816=CARTESIAN_POINT('Ctrl Pts',(2.05888584445224,-0.629314502062404,
19.2648593112669));
#278817=CARTESIAN_POINT('Ctrl Pts',(1.64674518167725,1.39003161576949,19.3760150970424));
#278818=CARTESIAN_POINT('Ctrl Pts',(-0.278596374653366,2.13492605016005,
19.4871827640554));
#278819=CARTESIAN_POINT('Ctrl Pts',(-1.38426912631003,1.33067653349406,
19.5612985024766));
#278820=CARTESIAN_POINT('Ctrl Pts',(-1.64489379696873,0.783437119887715,
19.5983623123059));
#278821=CARTESIAN_POINT('Ctrl Pts',(-0.86238966708827,1.75622551003249,
0.00144955206273537));
#278822=CARTESIAN_POINT('Ctrl Pts',(-1.44656040514264,1.46937837597419,
0.0385068845173068));
#278823=CARTESIAN_POINT('Ctrl Pts',(-2.2959724827549,0.272009208368595,
0.112616145563727));
#278824=CARTESIAN_POINT('Ctrl Pts',(-1.47177392533232,-1.78588083026947,
0.223777335201998));
#278825=CARTESIAN_POINT('Ctrl Pts',(0.701827041886748,-2.20287370482543,
0.334933120977547));
#278826=CARTESIAN_POINT('Ctrl Pts',(2.23186483338071,-0.605803636020076,
0.446088906753094));
#278827=CARTESIAN_POINT('Ctrl Pts',(1.71896333956916,1.5474091169016,0.557244692528645));
#278828=CARTESIAN_POINT('Ctrl Pts',(-0.36805878737097,2.2830669875011,0.668400478304191));
#278829=CARTESIAN_POINT('Ctrl Pts',(-2.1179513101924,0.928799185925246,
0.779556264079742));
#278830=CARTESIAN_POINT('Ctrl Pts',(-1.92876186867258,-1.27607397694317,
0.89071204985529));
#278831=CARTESIAN_POINT('Ctrl Pts',(0.0264049780544867,-2.31248513119795,
1.00186783563084));
#278832=CARTESIAN_POINT('Ctrl Pts',(1.95737532676084,-1.23168741276525,
1.11302362140639));
#278833=CARTESIAN_POINT('Ctrl Pts',(2.09622033473819,0.976851316540996,
1.22417940718193));
#278834=CARTESIAN_POINT('Ctrl Pts',(0.31579960212792,2.29098694335075,1.33533519295748));
#278835=CARTESIAN_POINT('Ctrl Pts',(-1.75375833778551,1.50754645200738,
1.44649097873303));
#278836=CARTESIAN_POINT('Ctrl Pts',(-2.2176095832823,-0.656179831656115,
1.55764676450858));
#278837=CARTESIAN_POINT('Ctrl Pts',(-0.65105823014671,-2.21911778654004,
1.66880255028413));
#278838=CARTESIAN_POINT('Ctrl Pts',(1.51158940257292,-1.75027433306136,
1.77995833605968));
#278839=CARTESIAN_POINT('Ctrl Pts',(2.29025433608824,0.321088152155656,
1.89111412183523));
#278840=CARTESIAN_POINT('Ctrl Pts',(0.972005202736432,2.09846799851684,
2.00226990761077));
#278841=CARTESIAN_POINT('Ctrl Pts',(-1.23619361425102,1.9545300552256,2.11342569338632));
#278842=CARTESIAN_POINT('Ctrl Pts',(-2.31255675945291,0.0210609293391671,
2.22458147916187));
#278843=CARTESIAN_POINT('Ctrl Pts',(-1.27158625942316,-1.9316911387274,
2.33573726493742));
#278844=CARTESIAN_POINT('Ctrl Pts',(0.933624778963557,-2.11582302953462,
2.44689305071297));
#278845=CARTESIAN_POINT('Ctrl Pts',(2.28402647220686,-0.362746994700493,
2.55804883648852));
#278846=CARTESIAN_POINT('Ctrl Pts',(1.54321633139411,1.72245338274497,2.66920462226407));
#278847=CARTESIAN_POINT('Ctrl Pts',(-0.610533758695877,2.23060772838173,
2.78036040803961));
#278848=CARTESIAN_POINT('Ctrl Pts',(-2.20529058243143,0.696459441174774,
2.89151619381516));
#278849=CARTESIAN_POINT('Ctrl Pts',(-1.78092467930869,-1.47535405651934,
3.00267197959071));
#278850=CARTESIAN_POINT('Ctrl Pts',(0.274022482530514,-2.29636103118655,
3.11382776536626));
#278851=CARTESIAN_POINT('Ctrl Pts',(2.07807979509936,-1.01486288300141,
3.22498355114181));
#278852=CARTESIAN_POINT('Ctrl Pts',(1.97948619386476,1.19582470050258,3.33613933691736));
#278853=CARTESIAN_POINT('Ctrl Pts',(0.0685121323916199,2.31163760003399,
3.44729512269291));
#278854=CARTESIAN_POINT('Ctrl Pts',(-1.90519035348363,1.31095843683326,
3.55845090846846));
#278855=CARTESIAN_POINT('Ctrl Pts',(-2.13453625811103,-0.890009701586508,
3.669606694244));
#278856=CARTESIAN_POINT('Ctrl Pts',(-0.409540769546024,-2.27610163749505,
3.78076248001955));
#278857=CARTESIAN_POINT('Ctrl Pts',(1.69042257214797,-1.57823757200569,
3.8919182657951));
#278858=CARTESIAN_POINT('Ctrl Pts',(2.24266668808919,0.564631235633758,
4.00307405157065));
#278859=CARTESIAN_POINT('Ctrl Pts',(0.74156721568914,2.19053426604923,4.1142298373462));
#278860=CARTESIAN_POINT('Ctrl Pts',(-1.43849730120351,1.81082517669416,
4.22538562312174));
#278861=CARTESIAN_POINT('Ctrl Pts',(-2.30150064892601,-0.226841506591189,
4.33654140889729));
#278862=CARTESIAN_POINT('Ctrl Pts',(-1.05729313641001,-2.05681635782586,
4.44769719467285));
#278863=CARTESIAN_POINT('Ctrl Pts',(1.15495215638586,-2.00360869996592,
4.55885298044839));
#278864=CARTESIAN_POINT('Ctrl Pts',(2.3097449005031,-0.115934467348872,
4.67000876622394));
#278865=CARTESIAN_POINT('Ctrl Pts',(1.34977850214863,1.87788719076972,4.78116455199949));
#278866=CARTESIAN_POINT('Ctrl Pts',(-0.846019795697788,2.15235053172271,
4.89232033777504));
#278867=CARTESIAN_POINT('Ctrl Pts',(-2.26721822440964,0.456162064429264,
5.00347612355059));
#278868=CARTESIAN_POINT('Ctrl Pts',(-1.6125941382609,-1.65767983982618,
5.11463190932614));
#278869=CARTESIAN_POINT('Ctrl Pts',(0.51849091820569,-2.253781150391,5.22578769510168));
#278870=CARTESIAN_POINT('Ctrl Pts',(2.17485540733811,-0.786362679233778,
5.33694348087723));
#278871=CARTESIAN_POINT('Ctrl Pts',(1.83996304588912,1.40103472329633,5.44809926665279));
#278872=CARTESIAN_POINT('Ctrl Pts',(-0.179564996433804,2.30567099087778,
5.55925505242832));
#278873=CARTESIAN_POINT('Ctrl Pts',(-2.03468669336613,1.09927811128868,
5.67041083820389));
#278874=CARTESIAN_POINT('Ctrl Pts',(-2.02688738723689,-1.11359320471147,
5.78156662397941));
#278875=CARTESIAN_POINT('Ctrl Pts',(-0.163307976566169,-2.30687945305112,
5.89272240975499));
#278876=CARTESIAN_POINT('Ctrl Pts',(1.84979315678771,-1.38803010890287,
6.00387819553052));
#278877=CARTESIAN_POINT('Ctrl Pts',(2.1692583439614,0.801673588983312,6.11503398130608));
#278878=CARTESIAN_POINT('Ctrl Pts',(0.502591246883182,2.25737997348164,
6.22618976708162));
#278879=CARTESIAN_POINT('Ctrl Pts',(-1.62423897645238,1.646271561284,6.33734555285718));
#278880=CARTESIAN_POINT('Ctrl Pts',(-2.26394643386545,-0.472132238580979,
6.44850133863271));
#278881=CARTESIAN_POINT('Ctrl Pts',(-0.830826966521448,-2.15826060933807,
6.55965712440827));
#278882=CARTESIAN_POINT('Ctrl Pts',(1.36298210030195,-1.8683260155487,6.67081291018381));
#278883=CARTESIAN_POINT('Ctrl Pts',(2.30887030062143,0.132212862566083,
6.78196869595937));
#278884=CARTESIAN_POINT('Ctrl Pts',(1.14080012572939,2.01170012160247,6.89312448173491));
#278885=CARTESIAN_POINT('Ctrl Pts',(-1.07176526380458,2.04931245187782,
7.00428026751046));
#278886=CARTESIAN_POINT('Ctrl Pts',(-2.30304246444779,0.210612708709141,
7.11543605328602));
#278887=CARTESIAN_POINT('Ctrl Pts',(-1.42569714745683,-1.82092008332409,
7.22659183906156));
#278888=CARTESIAN_POINT('Ctrl Pts',(0.756989757829629,-2.18525257411142,
7.33774762483711));
#278889=CARTESIAN_POINT('Ctrl Pts',(2.24659102808386,-0.548808763279752,
7.44890341061265));
#278890=CARTESIAN_POINT('Ctrl Pts',(1.67925565784572,1.59011406562948,7.5600591963882));
#278891=CARTESIAN_POINT('Ctrl Pts',(-0.425574720695307,2.27315825740855,
7.67121498216375));
#278892=CARTESIAN_POINT('Ctrl Pts',(-2.1407568609399,0.87494135143925,7.78237076793931));
#278893=CARTESIAN_POINT('Ctrl Pts',(-1.89590214062225,-1.32435545806388,
7.89352655371484));
#278894=CARTESIAN_POINT('Ctrl Pts',(0.0848050473160995,-2.31109723076924,
8.00468233949041));
#278895=CARTESIAN_POINT('Ctrl Pts',(1.98786632331827,-1.18184169275612,
8.11583812526594));
#278896=CARTESIAN_POINT('Ctrl Pts',(2.07087444958375,1.02948594948194,8.2269939110415));
#278897=CARTESIAN_POINT('Ctrl Pts',(0.25782874141307,2.29823555063899,8.33814969681704));
#278898=CARTESIAN_POINT('Ctrl Pts',(-1.79128013025956,1.46276375435572,
8.4493054825926));
#278899=CARTESIAN_POINT('Ctrl Pts',(-2.20032648621057,-0.711987120810329,
8.56046126836814));
#278900=CARTESIAN_POINT('Ctrl Pts',(-0.594795149134557,-2.23485593197539,
8.67161705414369));
#278901=CARTESIAN_POINT('Ctrl Pts',(1.55531947904698,-1.71153253670991,
8.78277283991924));
#278902=CARTESIAN_POINT('Ctrl Pts',(2.28141274146532,0.378837972224598,
8.89392862569479));
#278903=CARTESIAN_POINT('Ctrl Pts',(0.918687255235554,2.12235153383867,
9.00508441147033));
#278904=CARTESIAN_POINT('Ctrl Pts',(-1.28517106417351,1.92267980743821,
9.11624019724589));
#278905=CARTESIAN_POINT('Ctrl Pts',(-2.31235084345071,-0.0373615164619474,
9.22739598302143));
#278906=CARTESIAN_POINT('Ctrl Pts',(-1.22238552773304,-1.963195336106,9.33855176879698));
#278907=CARTESIAN_POINT('Ctrl Pts',(0.986773067656097,-2.09156429952993,
9.44970755457253));
#278908=CARTESIAN_POINT('Ctrl Pts',(2.29246073605411,-0.304936189668887,
9.56086334034808));
#278909=CARTESIAN_POINT('Ctrl Pts',(1.49921431901616,1.76088578044588,9.67201912612363));
#278910=CARTESIAN_POINT('Ctrl Pts',(-0.666684630764002,2.21447373188816,
9.78317491189918));
#278911=CARTESIAN_POINT('Ctrl Pts',(-2.22217962738618,0.640531037303711,
9.89433069767472));
#278912=CARTESIAN_POINT('Ctrl Pts',(-1.74308860448485,-1.51986987042792,
10.0054864834503));
#278913=CARTESIAN_POINT('Ctrl Pts',(0.331941676327445,-2.28870640966387,
10.1166422692258));
#278914=CARTESIAN_POINT('Ctrl Pts',(2.10305237942883,-0.962046254344501,
10.2277980550014));
#278915=CARTESIAN_POINT('Ctrl Pts',(1.94864773859537,1.24544542111916,10.3389538407769));
#278916=CARTESIAN_POINT('Ctrl Pts',(0.0100977491765532,2.31263061070744,
10.4501096265525));
#278917=CARTESIAN_POINT('Ctrl Pts',(-1.93769755013984,1.26241455564391,
10.561265412328));
#278918=CARTESIAN_POINT('Ctrl Pts',(-2.11137328819618,-0.943644606836327,
10.6724211981036));
#278919=CARTESIAN_POINT('Ctrl Pts',(-0.351915214197786,-2.28572045275351,
10.7835769838791));
#278920=CARTESIAN_POINT('Ctrl Pts',(1.72974983444855,-1.5350334903007,10.8947327696547));
#278921=CARTESIAN_POINT('Ctrl Pts',(2.22768835303858,0.621101366812054,
11.0058885554302));
#278922=CARTESIAN_POINT('Ctrl Pts',(0.685997166140391,2.2085674529357,11.1170443412058));
#278923=CARTESIAN_POINT('Ctrl Pts',(-1.48378016935762,1.77391057134812,
11.2282001269813));
#278924=CARTESIAN_POINT('Ctrl Pts',(-2.29503619027939,-0.284905583355947,
11.3393559127569));
#278925=CARTESIAN_POINT('Ctrl Pts',(-1.00500008814481,-2.08286752553985,
11.4505116985324));
#278926=CARTESIAN_POINT('Ctrl Pts',(1.20519525933597,-1.9737949977122,11.561667484308));
#278927=CARTESIAN_POINT('Ctrl Pts',(2.31193641471564,-0.057552762152893,
11.6728232700835));
#278928=CARTESIAN_POINT('Ctrl Pts',(1.30191191828315,1.9113837037999,11.783979055859));
#278929=CARTESIAN_POINT('Ctrl Pts',(-0.900118730552761,2.13029307303659,
11.8951348416346));
#278930=CARTESIAN_POINT('Ctrl Pts',(-2.27801753940416,0.398746029806683,
12.0062906274101));
#278931=CARTESIAN_POINT('Ctrl Pts',(-1.57020618298296,-1.69788540515596,
12.1174464131857));
#278932=CARTESIAN_POINT('Ctrl Pts',(0.575256526323781,-2.23996478433065,
12.2286021989612));
#278933=CARTESIAN_POINT('Ctrl Pts',(2.19402514138456,-0.731174387606673,
12.3397579847368));
#278934=CARTESIAN_POINT('Ctrl Pts',(1.80398545664344,1.44706557499601,12.4509137705123));
#278935=CARTESIAN_POINT('Ctrl Pts',(-0.237749502537639,2.30039941752791,
12.5620695562879));
#278936=CARTESIAN_POINT('Ctrl Pts',(-2.06180547301307,1.04753066665038,
12.6732253420634));
#278937=CARTESIAN_POINT('Ctrl Pts',(-1.99811099403281,-1.16443753015984,
12.784381127839));
#278938=CARTESIAN_POINT('Ctrl Pts',(-0.104983536811676,-2.31026854783552,
12.8955369136145));
#278939=CARTESIAN_POINT('Ctrl Pts',(1.88426487914961,-1.34086098135597,
13.0066926993901));
#278940=CARTESIAN_POINT('Ctrl Pts',(2.14831568599309,0.856213769706821,
13.1178484851656));
#278941=CARTESIAN_POINT('Ctrl Pts',(0.445408913720521,2.26935524008425,
13.2290042709412));
#278942=CARTESIAN_POINT('Ctrl Pts',(-1.6653059122569,1.60471758410063,13.3401600567167));
#278943=CARTESIAN_POINT('Ctrl Pts',(-2.25129785555133,-0.529169416831332,
13.4513158424923));
#278944=CARTESIAN_POINT('Ctrl Pts',(-0.77604367533783,-2.17855881722017,
13.5624716282678));
#278945=CARTESIAN_POINT('Ctrl Pts',(1.40974154967657,-1.83330059434755,
13.6736274140434));
#278946=CARTESIAN_POINT('Ctrl Pts',(2.30479383268882,0.190493293632852,
13.7847831998189));
#278947=CARTESIAN_POINT('Ctrl Pts',(1.08962007812897,2.03987509212151,13.8959389855945));
#278948=CARTESIAN_POINT('Ctrl Pts',(-1.12318939868838,2.02158548688735,
14.00709477137));
#278949=CARTESIAN_POINT('Ctrl Pts',(-2.30762771248847,0.152370097705391,
14.1182505571456));
#278950=CARTESIAN_POINT('Ctrl Pts',(-1.37924534148346,-1.85635249726869,
14.2294063429211));
#278951=CARTESIAN_POINT('Ctrl Pts',(0.811948214851289,-2.16543353685108,
14.3405621286967));
#278952=CARTESIAN_POINT('Ctrl Pts',(2.25973720291691,-0.491884213888585,
14.4517179144722));
#278953=CARTESIAN_POINT('Ctrl Pts',(1.63855315919402,1.63202507658885,14.5628737002478));
#278954=CARTESIAN_POINT('Ctrl Pts',(-0.482859447898242,2.2616827937832,
14.6740294860233));
#278955=CARTESIAN_POINT('Ctrl Pts',(-2.16217499407731,0.820586132655404,
14.7851852717988));
#278956=CARTESIAN_POINT('Ctrl Pts',(-1.86184363840467,-1.37182381239417,
14.8963410575744));
#278957=CARTESIAN_POINT('Ctrl Pts',(0.143156858570753,-2.30821758505642,
15.0074968433499));
#278958=CARTESIAN_POINT('Ctrl Pts',(2.0170856188344,-1.13125059664556,15.1186526291255));
#278959=CARTESIAN_POINT('Ctrl Pts',(2.04420859000465,1.08146823655202,15.229808414901));
#278960=CARTESIAN_POINT('Ctrl Pts',(0.199692488007044,2.30401502086096,
15.3409642006766));
#278961=CARTESIAN_POINT('Ctrl Pts',(-1.82765831344299,1.41704883311125,
15.4521199864521));
#278962=CARTESIAN_POINT('Ctrl Pts',(-2.18163941643627,-0.767340708403025,
15.5632757722277));
#278963=CARTESIAN_POINT('Ctrl Pts',(-0.538152357260458,-2.24916747853362,
15.6744315580032));
#278964=CARTESIAN_POINT('Ctrl Pts',(1.59805691435858,-1.67169865842755,
15.7855873437788));
#278965=CARTESIAN_POINT('Ctrl Pts',(2.27111522541637,0.436346122945927,
15.8967431295543));
#278966=CARTESIAN_POINT('Ctrl Pts',(0.86478300052194,2.14488057199392,16.0078989153299));
#278967=CARTESIAN_POINT('Ctrl Pts',(-1.33332833217902,1.88960256792799,
16.1190547011054));
#278968=CARTESIAN_POINT('Ctrl Pts',(-2.31066923273102,-0.0957601330721178,
16.230210486881));
#278969=CARTESIAN_POINT('Ctrl Pts',(-1.17240468950486,-1.99344665091902,
16.3413662726565));
#278970=CARTESIAN_POINT('Ctrl Pts',(1.03929161455433,-2.06597077569147,
16.4525220584321));
#278971=CARTESIAN_POINT('Ctrl Pts',(2.29943199451892,-0.246930777885519,
16.5636778442076));
#278972=CARTESIAN_POINT('Ctrl Pts',(1.45425553516014,1.79819441215764,16.6748336299832));
#278973=CARTESIAN_POINT('Ctrl Pts',(-0.722410036492459,2.19692649975759,
16.7859894157587));
#278974=CARTESIAN_POINT('Ctrl Pts',(-2.23765051893758,0.584193857826336,
16.8971452015343));
#278975=CARTESIAN_POINT('Ctrl Pts',(-1.70414012150793,-1.56341573085281,
17.0083009873098));
#278976=CARTESIAN_POINT('Ctrl Pts',(0.389649028978418,-2.27959117872528,
17.1194567730854));
#278977=CARTESIAN_POINT('Ctrl Pts',(2.12668283842677,-0.908615664043321,
17.2306125588609));
#278978=CARTESIAN_POINT('Ctrl Pts',(1.91656568480049,1.29427131871064,17.3417683446365));
#278979=CARTESIAN_POINT('Ctrl Pts',(-0.0483230640552768,2.31214774828866,
17.452924130412));
#278980=CARTESIAN_POINT('Ctrl Pts',(-1.96896817091355,1.21306501500312,
17.5640799161876));
#278981=CARTESIAN_POINT('Ctrl Pts',(-2.08686282744385,-0.99667727694527,
17.6752357019631));
#278982=CARTESIAN_POINT('Ctrl Pts',(-0.294065170700686,-2.29388059863771,
17.7863914877387));
#278983=CARTESIAN_POINT('Ctrl Pts',(1.76797338809603,-1.4908497113822,17.8975472735142));
#278984=CARTESIAN_POINT('Ctrl Pts',(2.21128799480902,0.677174994808322,
18.0087030592898));
#278985=CARTESIAN_POINT('Ctrl Pts',(0.629989998521478,2.22519141583385,
18.1198588450653));
#278986=CARTESIAN_POINT('Ctrl Pts',(-1.52811739626718,1.73586342652233,
18.2310146308409));
#278987=CARTESIAN_POINT('Ctrl Pts',(-2.2871046465437,-0.342786958716292,
18.3421704166164));
#278988=CARTESIAN_POINT('Ctrl Pts',(-0.95207030101812,-2.10759111981359,
18.453326202392));
#278989=CARTESIAN_POINT('Ctrl Pts',(1.25467804542587,-1.94271847031493,
18.5644819881675));
#278990=CARTESIAN_POINT('Ctrl Pts',(2.31263571838425,0.000859610951930963,
18.6756377739431));
#278991=CARTESIAN_POINT('Ctrl Pts',(1.25324639693522,1.94367193971766,18.7867935597186));
#278992=CARTESIAN_POINT('Ctrl Pts',(-0.953703958890417,2.10685415701179,
18.8979493454942));
#278993=CARTESIAN_POINT('Ctrl Pts',(-2.28724750397368,0.341117275939698,
19.0091051312697));
#278994=CARTESIAN_POINT('Ctrl Pts',(-1.52703607338255,-1.73708686266442,
19.1202609170453));
#278995=CARTESIAN_POINT('Ctrl Pts',(0.632073825457285,-2.22456767913867,
19.2314167028208));
#278996=CARTESIAN_POINT('Ctrl Pts',(2.21099471354783,-0.675807763197824,
19.3425724885964));
#278997=CARTESIAN_POINT('Ctrl Pts',(1.768405422311,1.49272605978228,19.4537282743719));
#278998=CARTESIAN_POINT('Ctrl Pts',(-0.299178855997274,2.29265270992973,
19.5648959413849));
#278999=CARTESIAN_POINT('Ctrl Pts',(-1.48653784212754,1.42898587064706,
19.639011679806));
#279000=CARTESIAN_POINT('Ctrl Pts',(-1.76641725875435,0.841316838976901,
19.6760754896353));
#279001=CARTESIAN_POINT('Ctrl Pts',(-0.905547729029968,-1.26791219016627,
3.38487918249974E-16));
#279002=CARTESIAN_POINT('Ctrl Pts',(-0.93771513294814,-1.25071447123035,
-1.97792095906261E-15));
#279003=CARTESIAN_POINT('Ctrl Pts',(-0.96917675062485,-1.23233980165227,
-2.13242252659455E-16));
#279004=CARTESIAN_POINT('Ctrl Pts',(-0.999860368201583,-1.21280268753011,
-9.61036805691151E-16));
#279005=CARTESIAN_POINT('Ctrl Pts',(-1.05019035785126,-1.1807561809833,
-2.25512455836343E-15));
#279006=CARTESIAN_POINT('Ctrl Pts',(-1.09842841594666,-1.1455850368464,
-2.75096923024122E-15));
#279007=CARTESIAN_POINT('Ctrl Pts',(-1.14449463040455,-1.10761563373825,
-2.31065167000111E-15));
#279008=CARTESIAN_POINT('Ctrl Pts',(-1.17053805883182,-1.08614971899119,
-2.06171914970765E-15));
#279009=CARTESIAN_POINT('Ctrl Pts',(-1.19588705872478,-1.063788463934,-8.1926151363717E-16));
#279010=CARTESIAN_POINT('Ctrl Pts',(-1.22052445577263,-1.0405840768243,
-2.02268757298896E-15));
#279011=CARTESIAN_POINT('Ctrl Pts',(-1.23356026960347,-1.0283064782682,
-2.5965085128221E-15));
#279012=CARTESIAN_POINT('Ctrl Pts',(-1.24640012070248,-1.01578919396326,
-1.89951844817313E-15));
#279013=CARTESIAN_POINT('Ctrl Pts',(-1.25902027597637,-1.00306131550636,
-1.97758476261356E-15));
#279014=CARTESIAN_POINT('Ctrl Pts',(-1.30242662502562,-0.959284458330949,
-1.88174753472955E-15));
#279015=CARTESIAN_POINT('Ctrl Pts',(-1.34328094576712,-0.912979946993025,
-1.27617630927406E-15));
#279016=CARTESIAN_POINT('Ctrl Pts',(-1.38149779807473,-0.864485899841547,
-1.29063426612674E-15));
#279017=CARTESIAN_POINT('Ctrl Pts',(-1.42075956301071,-0.81466594437451,
-1.30548752768883E-15));
#279018=CARTESIAN_POINT('Ctrl Pts',(-1.45723839042144,-0.762534493232605,
-3.150204436215E-15));
#279019=CARTESIAN_POINT('Ctrl Pts',(-1.49081464423019,-0.70841114099212,
-2.56739074444567E-15));
#279020=CARTESIAN_POINT('Ctrl Pts',(-1.49552688682915,-0.700815226108965,
-2.48559604747741E-15));
#279021=CARTESIAN_POINT('Ctrl Pts',(-1.50018190566982,-0.693180012726265,
-2.45505863419059E-15));
#279022=CARTESIAN_POINT('Ctrl Pts',(-1.50477931581713,-0.685506323835288,
-2.18575157973078E-15));
#279023=CARTESIAN_POINT('Ctrl Pts',(-1.51106438534805,-0.675015707011237,
-1.67622061700782E-15));
#279024=CARTESIAN_POINT('Ctrl Pts',(-1.5172370080675,-0.664461134174755,
-5.50282080994333E-16));
#279025=CARTESIAN_POINT('Ctrl Pts',(-1.5232955325984,-0.653847043301167,
-4.71844785465692E-16));
#279026=CARTESIAN_POINT('Ctrl Pts',(-1.55549299934074,-0.597439441721034,
2.74586708188979E-16));
#279027=CARTESIAN_POINT('Ctrl Pts',(-1.58448057296325,-0.539337269758026,
-2.67852813923984E-16));
#279028=CARTESIAN_POINT('Ctrl Pts',(-1.61016391944946,-0.47989642590738,
-1.16573417585641E-15));
#279029=CARTESIAN_POINT('Ctrl Pts',(-1.63628474196843,-0.419443099335088,
-2.07890955628107E-15));
#279030=CARTESIAN_POINT('Ctrl Pts',(-1.65898855606191,-0.357604293189553,
-7.61811381027507E-16));
#279031=CARTESIAN_POINT('Ctrl Pts',(-1.67814164180346,-0.294713444473936,
-7.63278329429795E-16));
#279032=CARTESIAN_POINT('Ctrl Pts',(-1.69045739883456,-0.254273568481462,
-7.64221601983552E-16));
#279033=CARTESIAN_POINT('Ctrl Pts',(-1.70130430670316,-0.213397904158502,
1.6222274639253E-16));
#279034=CARTESIAN_POINT('Ctrl Pts',(-1.71063726747206,-0.172168887794852,
-1.92901250528621E-15));
#279035=CARTESIAN_POINT('Ctrl Pts',(-1.71589881203146,-0.148925641400778,
-3.06462610868884E-15));
#279036=CARTESIAN_POINT('Ctrl Pts',(-1.7206790422679,-0.125570016898669,
-7.50804587875827E-17));
#279037=CARTESIAN_POINT('Ctrl Pts',(-1.72496866549233,-0.102116340889781,
-9.57567358739198E-16));
#279038=CARTESIAN_POINT('Ctrl Pts',(-1.72707108291268,-0.0906212947207782,
-1.44338884350977E-15));
#279039=CARTESIAN_POINT('Ctrl Pts',(-1.72905591297498,-0.0791009626866409,
-1.97430438624691E-15));
#279040=CARTESIAN_POINT('Ctrl Pts',(-1.73092110454086,-0.0675624532590521,
-1.83186799063151E-15));
#279041=CARTESIAN_POINT('Ctrl Pts',(-1.74174234252042,-0.000619754863062469,
-5.07256798513496E-16));
#279042=CARTESIAN_POINT('Ctrl Pts',(-1.74849833894868,0.0666674919201606,
7.85842007761142E-16));
#279043=CARTESIAN_POINT('Ctrl Pts',(-1.7510698873627,0.13394129902393,8.74300631892311E-16));
#279044=CARTESIAN_POINT('Ctrl Pts',(-1.75198203547585,0.157803838760529,
1.06041694804641E-15));
#279045=CARTESIAN_POINT('Ctrl Pts',(-1.75236732825439,0.181664982389618,
-3.03227639702671E-16));
#279046=CARTESIAN_POINT('Ctrl Pts',(-1.75221911350936,0.205509592721547,
-4.57966997657877E-16));
#279047=CARTESIAN_POINT('Ctrl Pts',(-1.75181220987844,0.270971760604655,
-1.03286705753963E-15));
#279048=CARTESIAN_POINT('Ctrl Pts',(-1.74738828583053,0.336308629139333,
1.51075324298343E-15));
#279049=CARTESIAN_POINT('Ctrl Pts',(-1.73917033238596,0.401277976570864,
8.32667268468867E-16));
#279050=CARTESIAN_POINT('Ctrl Pts',(-1.73175672467545,0.459888342072993,
2.20950075987451E-16));
#279051=CARTESIAN_POINT('Ctrl Pts',(-1.72125458542747,0.518200223470177,
4.69347102986873E-16));
#279052=CARTESIAN_POINT('Ctrl Pts',(-1.70779140168744,0.576038554497463,
-6.10622663543836E-16));
#279053=CARTESIAN_POINT('Ctrl Pts',(-1.70537963519586,0.586399591782088,
-6.30492532896913E-16));
#279054=CARTESIAN_POINT('Ctrl Pts',(-1.70287252597029,0.596746365633996,
1.79996086398271E-15));
#279055=CARTESIAN_POINT('Ctrl Pts',(-1.70027142920407,0.607074958677167,
1.9151347174784E-15));
#279056=CARTESIAN_POINT('Ctrl Pts',(-1.68381517035749,0.672420470942285,
1.83985930547722E-15));
#279057=CARTESIAN_POINT('Ctrl Pts',(-1.66367353779973,0.736753172822899,
2.48254355522872E-15));
#279058=CARTESIAN_POINT('Ctrl Pts',(-1.64010460098311,0.799821324003097,
2.83106871279415E-15));
#279059=CARTESIAN_POINT('Ctrl Pts',(-1.61575949880483,0.864966417166323,
3.19107139932377E-15));
#279060=CARTESIAN_POINT('Ctrl Pts',(-1.58775758055669,0.928763170627653,
7.18035494846759E-16));
#279061=CARTESIAN_POINT('Ctrl Pts',(-1.556326723057,0.990938813102449,1.0547118733939E-15));
#279062=CARTESIAN_POINT('Ctrl Pts',(-1.5248958655573,1.05311445557725,1.39138825194104E-15));
#279063=CARTESIAN_POINT('Ctrl Pts',(-1.49003568291284,1.11366995051747,
1.65653319858449E-15));
#279064=CARTESIAN_POINT('Ctrl Pts',(-1.45192228062725,1.17232315389904,
2.60902410786912E-15));
#279065=CARTESIAN_POINT('Ctrl Pts',(-1.43661514216392,1.19587950551396,
2.98313285321639E-15));
#279066=CARTESIAN_POINT('Ctrl Pts',(-1.42078271004317,1.21912883273614,
-3.24800180492398E-18));
#279067=CARTESIAN_POINT('Ctrl Pts',(-1.4044342596313,1.24205188600702,1.02695629777827E-15));
#279068=CARTESIAN_POINT('Ctrl Pts',(-1.39840915285019,1.2505000165776,1.16179888517215E-15));
#279069=CARTESIAN_POINT('Ctrl Pts',(-1.39231500560742,1.25890225569876,
-1.49405468388659E-17));
#279070=CARTESIAN_POINT('Ctrl Pts',(-1.38615790425663,1.26725033866967,
1.94289029309402E-16));
#279071=CARTESIAN_POINT('Ctrl Pts',(-1.34330654088438,1.32535020035255,
2.16119872575111E-15));
#279072=CARTESIAN_POINT('Ctrl Pts',(-1.29733814342063,1.38092917463918,
1.37308607647262E-15));
#279073=CARTESIAN_POINT('Ctrl Pts',(-1.2484938594593,1.43370660660493,2.05391259555654E-15));
#279074=CARTESIAN_POINT('Ctrl Pts',(-1.19953661080933,1.48660609965309,
3.06915354955197E-15));
#279075=CARTESIAN_POINT('Ctrl Pts',(-1.14768972594085,1.5366920862558,1.38515409442575E-15));
#279076=CARTESIAN_POINT('Ctrl Pts',(-1.09314642559825,1.58366574341901,
1.85962356624714E-15));
#279077=CARTESIAN_POINT('Ctrl Pts',(-1.03976854854967,1.62963571738155,
2.22260353012378E-15));
#279078=CARTESIAN_POINT('Ctrl Pts',(-0.983807683858392,1.67262579927252,
2.03200015230422E-15));
#279079=CARTESIAN_POINT('Ctrl Pts',(-0.925405164442978,1.71232676209298,
1.55431223447522E-15));
#279080=CARTESIAN_POINT('Ctrl Pts',(-0.904425650494227,1.72658825135077,
1.88961112987798E-15));
#279081=CARTESIAN_POINT('Ctrl Pts',(-0.883130725037691,1.74042497017167,
1.29805087082181E-15));
#279082=CARTESIAN_POINT('Ctrl Pts',(-0.861525859670521,1.75382131162754,
-2.22044604925031E-16));
#279083=CARTESIAN_POINT('Origin',(-0.866025403784439,-1.5,-4.));
#279084=CARTESIAN_POINT('',(-0.866025403784439,-1.5,-4.));
#279085=CARTESIAN_POINT('',(0.866025403784439,-1.5,-4.));
#279086=CARTESIAN_POINT('',(-0.43301270189222,-1.5,-4.));
#279087=CARTESIAN_POINT('',(-0.866025403784439,-1.5,-2.));
#279088=CARTESIAN_POINT('',(-0.866025403784439,-1.5,-4.));
#279089=CARTESIAN_POINT('',(0.866025403784439,-1.5,-2.));
#279090=CARTESIAN_POINT('',(-0.866025403784439,-1.5,-2.));
#279091=CARTESIAN_POINT('',(0.866025403784439,-1.5,-4.));
#279092=CARTESIAN_POINT('Origin',(-1.73205080756888,2.12115047744981E-16,
-4.));
#279093=CARTESIAN_POINT('',(-1.73205080756888,2.12115047744981E-16,-4.));
#279094=CARTESIAN_POINT('',(-1.51554445662277,-0.375,-4.));
#279095=CARTESIAN_POINT('',(-1.73205080756888,2.77555756156289E-16,-2.));
#279096=CARTESIAN_POINT('',(-1.73205080756888,2.12115047744981E-16,-4.));
#279097=CARTESIAN_POINT('',(-1.73205080756888,2.12115047744981E-16,-2.));
#279098=CARTESIAN_POINT('Origin',(-0.866025403784438,1.5,-4.));
#279099=CARTESIAN_POINT('',(-0.866025403784438,1.5,-4.));
#279100=CARTESIAN_POINT('',(-1.08253175473055,1.125,-4.));
#279101=CARTESIAN_POINT('',(-0.866025403784438,1.5,-2.));
#279102=CARTESIAN_POINT('',(-0.866025403784438,1.5,-4.));
#279103=CARTESIAN_POINT('',(-0.866025403784438,1.5,-2.));
#279104=CARTESIAN_POINT('Origin',(0.866025403784439,1.5,-4.));
#279105=CARTESIAN_POINT('',(0.866025403784439,1.5,-4.));
#279106=CARTESIAN_POINT('',(0.43301270189222,1.5,-4.));
#279107=CARTESIAN_POINT('',(0.866025403784439,1.5,-2.));
#279108=CARTESIAN_POINT('',(0.866025403784439,1.5,-4.));
#279109=CARTESIAN_POINT('',(0.866025403784439,1.5,-2.));
#279110=CARTESIAN_POINT('Origin',(1.73205080756888,0.,-4.));
#279111=CARTESIAN_POINT('',(1.73205080756888,0.,-4.));
#279112=CARTESIAN_POINT('',(1.51554445662277,0.375,-4.));
#279113=CARTESIAN_POINT('',(1.73205080756888,0.,-2.));
#279114=CARTESIAN_POINT('',(1.73205080756888,0.,-4.));
#279115=CARTESIAN_POINT('',(1.73205080756888,0.,-2.));
#279116=CARTESIAN_POINT('Origin',(0.866025403784439,-1.5,-4.));
#279117=CARTESIAN_POINT('',(1.08253175473055,-1.125,-4.));
#279118=CARTESIAN_POINT('',(0.866025403784439,-1.5,-2.));
#279119=CARTESIAN_POINT('Origin',(0.,2.77555756156289E-16,-2.));
#279120=CARTESIAN_POINT('Origin',(0.,0.,0.));
#279121=CARTESIAN_POINT('',(-3.5,-4.28626379701574E-16,0.));
#279122=CARTESIAN_POINT('Origin',(0.,0.,0.));
#279123=CARTESIAN_POINT('Origin',(0.,0.,-4.));
#279124=CARTESIAN_POINT('',(-3.5,-4.28626379701574E-16,-4.));
#279125=CARTESIAN_POINT('',(-3.5,-4.28626379701574E-16,-4.));
#279126=CARTESIAN_POINT('Origin',(0.,0.,-4.));
#279127=CARTESIAN_POINT('Origin',(0.,0.,-4.));
#279128=CARTESIAN_POINT('Origin',(0.,0.,20.));
#279129=CARTESIAN_POINT('',(0.,0.,0.));
#279130=CARTESIAN_POINT('Origin',(0.,0.,0.));
#279131=CARTESIAN_POINT('',(-1.95399958625128,0.00127158556192198,0.225869692124231));
#279132=CARTESIAN_POINT('',(0.86152788258768,1.75382031791287,3.93122677751275E-5));
#279133=CARTESIAN_POINT('Ctrl Pts',(-1.95399958625128,0.00127158556192198,
0.225869692124231));
#279134=CARTESIAN_POINT('Ctrl Pts',(-1.95395604885434,0.0681739302723082,
0.222037301306047));
#279135=CARTESIAN_POINT('Ctrl Pts',(-1.95047678667107,0.134971424000874,
0.218204910487863));
#279136=CARTESIAN_POINT('Ctrl Pts',(-1.94359242694592,0.201406250941909,
0.214372519669679));
#279137=CARTESIAN_POINT('Ctrl Pts',(-1.93654044018152,0.269458697209641,
0.21044681409867));
#279138=CARTESIAN_POINT('Ctrl Pts',(-1.92589625907381,0.337273009132259,
0.206521108527662));
#279139=CARTESIAN_POINT('Ctrl Pts',(-1.91168600925926,0.404441098310242,
0.202595402956653));
#279140=CARTESIAN_POINT('Ctrl Pts',(-1.89749720503346,0.471507819867273,
0.19867562191676));
#279141=CARTESIAN_POINT('Ctrl Pts',(-1.87975311483401,0.537929778979427,
0.194755840876867));
#279142=CARTESIAN_POINT('Ctrl Pts',(-1.85853156400509,0.603304587747175,
0.190836059836973));
#279143=CARTESIAN_POINT('Ctrl Pts',(-1.83733531306058,0.668601458049552,
0.186920951877195));
#279144=CARTESIAN_POINT('Ctrl Pts',(-1.81266998680926,0.732853193984308,
0.183005843917416));
#279145=CARTESIAN_POINT('Ctrl Pts',(-1.78466392427241,0.795669955069697,
0.179090735957637));
#279146=CARTESIAN_POINT('Ctrl Pts',(-1.7566757359944,0.858446624726809,
0.17517812673016));
#279147=CARTESIAN_POINT('Ctrl Pts',(-1.72535124054766,0.919789690158248,
0.171265517502682));
#279148=CARTESIAN_POINT('Ctrl Pts',(-1.69086730727631,0.979328213207478,
0.167352908275204));
#279149=CARTESIAN_POINT('Ctrl Pts',(-1.65639367565598,1.0388489498551,0.16344146789162));
#279150=CARTESIAN_POINT('Ctrl Pts',(-1.61876272549717,1.09656579076339,
0.159530027508035));
#279151=CARTESIAN_POINT('Ctrl Pts',(-1.57819694541281,1.15213297908257,
0.155618587124451));
#279152=CARTESIAN_POINT('Ctrl Pts',(-1.53762951278187,1.2077024310675,0.151706987398745));
#279153=CARTESIAN_POINT('Ctrl Pts',(-1.49412730369477,1.26112166244711,
0.14779538767304));
#279154=CARTESIAN_POINT('Ctrl Pts',(-1.44795468666975,1.31207592209868,
0.143883787947335));
#279155=CARTESIAN_POINT('Ctrl Pts',(-1.4017348387758,1.36308230385452,0.139968186970113));
#279156=CARTESIAN_POINT('Ctrl Pts',(-1.35283946070058,1.41161831784349,
0.13605258599289));
#279157=CARTESIAN_POINT('Ctrl Pts',(-1.30157089688553,1.45740495414987,
0.132136985015667));
#279158=CARTESIAN_POINT('Ctrl Pts',(-1.25027274650581,1.50321801345654,
0.128219124385103));
#279159=CARTESIAN_POINT('Ctrl Pts',(-1.1965990661533,1.54627822984259,0.124301263754539));
#279160=CARTESIAN_POINT('Ctrl Pts',(-1.14088434801228,1.58634766191419,
0.120383403123975));
#279161=CARTESIAN_POINT('Ctrl Pts',(-1.08507638548269,1.62648415435723,
0.116458985545244));
#279162=CARTESIAN_POINT('Ctrl Pts',(-1.02722097917664,1.66361960726873,
0.112534567966514));
#279163=CARTESIAN_POINT('Ctrl Pts',(-0.96767980974077,1.69756053966274,
0.108610150387783));
#279164=CARTESIAN_POINT('Ctrl Pts',(-0.94062675434164,1.7129819016053,0.10682705665327));
#279165=CARTESIAN_POINT('Ctrl Pts',(-0.913225994787098,1.72774442491995,
0.105043962918756));
#279166=CARTESIAN_POINT('Ctrl Pts',(-0.885512812090751,1.74183324679004,
0.103260869184242));
#279167=CARTESIAN_POINT('Ctrl Pts',(-0.825177116348573,1.77250669483943,
0.0993788105183649));
#279168=CARTESIAN_POINT('Ctrl Pts',(-0.763117235362137,1.8001066486546,
0.0954967518524874));
#279169=CARTESIAN_POINT('Ctrl Pts',(-0.699682069082541,1.82443443351751,
0.0916146931866098));
#279170=CARTESIAN_POINT('Ctrl Pts',(-0.636353223996944,1.84872144353446,
0.0877391410869908));
#279171=CARTESIAN_POINT('Ctrl Pts',(-0.571654134652549,1.86974699526494,
0.0838635889873719));
#279172=CARTESIAN_POINT('Ctrl Pts',(-0.505957111893772,1.88735884264867,
0.0799880368877529));
#279173=CARTESIAN_POINT('Ctrl Pts',(-0.440321572265943,1.90495420783162,
0.0761161117573211));
#279174=CARTESIAN_POINT('Ctrl Pts',(-0.373690432405684,1.9191420711908,
0.0722441866268893));
#279175=CARTESIAN_POINT('Ctrl Pts',(-0.306453340920287,1.92981925315269,
0.0683722614964574));
#279176=CARTESIAN_POINT('Ctrl Pts',(-0.239255063254954,1.9404902715193,
0.064502571504429));
#279177=CARTESIAN_POINT('Ctrl Pts',(-0.171452022206664,1.94765454848065,
0.0606328815124006));
#279178=CARTESIAN_POINT('Ctrl Pts',(-0.103444394209851,1.95125991536406,
0.0567631915203721));
#279179=CARTESIAN_POINT('Ctrl Pts',(-0.035451640385408,1.9548644937058,
0.0528943478809905));
#279180=CARTESIAN_POINT('Ctrl Pts',(0.0327451105783654,1.95491168108245,
0.049025504241609));
#279181=CARTESIAN_POINT('Ctrl Pts',(0.100742171473057,1.95140129519453,
0.0451566606022274));
#279182=CARTESIAN_POINT('Ctrl Pts',(0.168794206077408,1.94788807125844,
0.0412846891116688));
#279183=CARTESIAN_POINT('Ctrl Pts',(0.236645725644037,1.94081155162635,
0.0374127176211102));
#279184=CARTESIAN_POINT('Ctrl Pts',(0.303895816327973,1.93022364839372,
0.0335407461305516));
#279185=CARTESIAN_POINT('Ctrl Pts',(0.371171480218994,1.91963171889675,
0.0296673022445249));
#279186=CARTESIAN_POINT('Ctrl Pts',(0.4378447675752,1.90552584870393,0.0257938583584982));
#279187=CARTESIAN_POINT('Ctrl Pts',(0.503525519732653,1.88800901771627,
0.0219204144724715));
#279188=CARTESIAN_POINT('Ctrl Pts',(0.569321331754245,1.87046150065808,
0.0180401850684257));
#279189=CARTESIAN_POINT('Ctrl Pts',(0.634120656256508,1.84949124013714,
0.0141599556643799));
#279190=CARTESIAN_POINT('Ctrl Pts',(0.697549773038983,1.82525075376872,
0.010279726260334));
#279191=CARTESIAN_POINT('Ctrl Pts',(0.753348915082634,1.80392618847929,
0.00686625492948106));
#279192=CARTESIAN_POINT('Ctrl Pts',(0.808087758634527,1.78007167123815,
0.00345278359862809));
#279193=CARTESIAN_POINT('Ctrl Pts',(0.86152788258768,1.75382031791287,3.93122677751275E-5));
#279194=CARTESIAN_POINT('',(-0.861525859670574,1.75382131162752,1.38777878078145E-16));
#279195=CARTESIAN_POINT('Origin',(0.,0.,0.));
#279196=CARTESIAN_POINT('',(-1.95399890369145,0.00206987260420434,0.124130307921836));
#279197=CARTESIAN_POINT('Ctrl Pts',(-0.861525859670572,1.75382131162752,
2.28983498828939E-15));
#279198=CARTESIAN_POINT('Ctrl Pts',(-0.924648224743909,1.7228138483964,
0.00400973887597992));
#279199=CARTESIAN_POINT('Ctrl Pts',(-0.986141954375339,1.68837147644998,
0.00801947775195755));
#279200=CARTESIAN_POINT('Ctrl Pts',(-1.04562636415511,1.65069122084773,
0.0120292166279352));
#279201=CARTESIAN_POINT('Ctrl Pts',(-1.10691784192122,1.61186628239718,
0.016160766761403));
#279202=CARTESIAN_POINT('Ctrl Pts',(-1.16607547468266,1.56960374308896,
0.0202923168948708));
#279203=CARTESIAN_POINT('Ctrl Pts',(-1.2227115584002,1.52416942790313,0.0244238670283386));
#279204=CARTESIAN_POINT('Ctrl Pts',(-1.27763825025648,1.48010641248774,
0.0284307186002357));
#279205=CARTESIAN_POINT('Ctrl Pts',(-1.33019308928818,1.43306069927262,
0.0324375701721327));
#279206=CARTESIAN_POINT('Ctrl Pts',(-1.38005457172536,1.38331680357752,
0.0364444217440298));
#279207=CARTESIAN_POINT('Ctrl Pts',(-1.42991716849446,1.3335717961784,0.0404513628632568));
#279208=CARTESIAN_POINT('Ctrl Pts',(-1.47708596403036,1.28112881053544,
0.0444583039824838));
#279209=CARTESIAN_POINT('Ctrl Pts',(-1.52127632765451,1.2263092329906,0.0484652451017108));
#279210=CARTESIAN_POINT('Ctrl Pts',(-1.5654796248828,1.17147361089088,0.0524733589696091));
#279211=CARTESIAN_POINT('Ctrl Pts',(-1.60670246957715,1.11426037168743,
0.0564814728375075));
#279212=CARTESIAN_POINT('Ctrl Pts',(-1.64470141560668,1.05502286871014,
0.0604895867054059));
#279213=CARTESIAN_POINT('Ctrl Pts',(-1.6827217597034,0.995752007753191,
0.0644999576330076));
#279214=CARTESIAN_POINT('Ctrl Pts',(-1.7175143488718,0.934455003168418,
0.0685103285606093));
#279215=CARTESIAN_POINT('Ctrl Pts',(-1.74888057041762,0.871511761490194,
0.072520699488211));
#279216=CARTESIAN_POINT('Ctrl Pts',(-1.78029554444285,0.808470687209157,
0.0765373037303931));
#279217=CARTESIAN_POINT('Ctrl Pts',(-1.80827331765284,0.743778680594848,
0.0805539079725752));
#279218=CARTESIAN_POINT('Ctrl Pts',(-1.83266272864314,0.677837239344568,
0.0845705122147573));
#279219=CARTESIAN_POINT('Ctrl Pts',(-1.85707426487929,0.611835978256916,
0.0885907601839796));
#279220=CARTESIAN_POINT('Ctrl Pts',(-1.87789081935113,0.544583462735634,
0.092611008153202));
#279221=CARTESIAN_POINT('Ctrl Pts',(-1.89501134508785,0.476495542464292,
0.0966312561224243));
#279222=CARTESIAN_POINT('Ctrl Pts',(-1.91216338868066,0.408282276435159,
0.100658905125871));
#279223=CARTESIAN_POINT('Ctrl Pts',(-1.92560573312532,0.339230985221237,
0.104686554129318));
#279224=CARTESIAN_POINT('Ctrl Pts',(-1.9352886455049,0.269766303640422,
0.108714203132765));
#279225=CARTESIAN_POINT('Ctrl Pts',(-1.93726980603249,0.255553566829941,
0.109538275365564));
#279226=CARTESIAN_POINT('Ctrl Pts',(-1.93909376069024,0.241323532685976,
0.110362347598363));
#279227=CARTESIAN_POINT('Ctrl Pts',(-1.94076035206736,0.227079844643627,
0.111186419831162));
#279228=CARTESIAN_POINT('Ctrl Pts',(-1.94948619402753,0.15250357328286,
0.115501049179361));
#279229=CARTESIAN_POINT('Ctrl Pts',(-1.9539191335491,0.0773743671059711,
0.119815678527559));
#279230=CARTESIAN_POINT('Ctrl Pts',(-1.9539989036906,0.0020698734084197,
0.124130307875758));
#279231=CARTESIAN_POINT('',(-1.95389301601064,0.000918145502495154,0.824130263912385));
#279232=CARTESIAN_POINT('Ctrl Pts',(-1.95399890369145,0.00206987260420564,
0.124130307921836));
#279233=CARTESIAN_POINT('Ctrl Pts',(-1.95406962240973,-0.0646899355598776,
0.127955362887828));
#279234=CARTESIAN_POINT('Ctrl Pts',(-1.95071485453637,-0.131608847044638,
0.131780417853821));
#279235=CARTESIAN_POINT('Ctrl Pts',(-1.94391230496763,-0.198295109862623,
0.135605472819813));
#279236=CARTESIAN_POINT('Ctrl Pts',(-1.93712036320297,-0.264877383021508,
0.139424563046665));
#279237=CARTESIAN_POINT('Ctrl Pts',(-1.92689135584406,-0.33122721849863,
0.143243653273517));
#279238=CARTESIAN_POINT('Ctrl Pts',(-1.91325499737006,-0.396952534994404,
0.147062743500369));
#279239=CARTESIAN_POINT('Ctrl Pts',(-1.89963031317816,-0.462621583103922,
0.150878564149294));
#279240=CARTESIAN_POINT('Ctrl Pts',(-1.88260415795907,-0.527666668135914,
0.15469438479822));
#279241=CARTESIAN_POINT('Ctrl Pts',(-1.86225788543312,-0.591702263086903,
0.158510205447145));
#279242=CARTESIAN_POINT('Ctrl Pts',(-1.84192136891004,-0.655707153079655,
0.162324196416597));
#279243=CARTESIAN_POINT('Ctrl Pts',(-1.81826804529352,-0.718703021080917,
0.166138187386048));
#279244=CARTESIAN_POINT('Ctrl Pts',(-1.79142952719964,-0.780318043542037,
0.1699521783555));
#279245=CARTESIAN_POINT('Ctrl Pts',(-1.76459377488551,-0.841926716413331,
0.173765776283169));
#279246=CARTESIAN_POINT('Ctrl Pts',(-1.73457368712652,-0.902154353896972,
0.177579374210839));
#279247=CARTESIAN_POINT('Ctrl Pts',(-1.7015487426134,-0.960649715822971,
0.181392972138508));
#279248=CARTESIAN_POINT('Ctrl Pts',(-1.66849242384863,-1.01920064932472,
0.185210193048224));
#279249=CARTESIAN_POINT('Ctrl Pts',(-1.6324258052211,-1.07601557265378,
0.189027413957941));
#279250=CARTESIAN_POINT('Ctrl Pts',(-1.59357334566683,-1.13076964585198,
0.192844634867658));
#279251=CARTESIAN_POINT('Ctrl Pts',(-1.55470101203149,-1.18555172723556,
0.196663808388835));
#279252=CARTESIAN_POINT('Ctrl Pts',(-1.51304032592502,-1.23827045919599,
0.200482981910012));
#279253=CARTESIAN_POINT('Ctrl Pts',(-1.46885600537764,-1.28863417441338,
0.204302155431189));
#279254=CARTESIAN_POINT('Ctrl Pts',(-1.42459380221032,-1.33908666451838,
0.208128060916016));
#279255=CARTESIAN_POINT('Ctrl Pts',(-1.37779945106309,-1.38717548865719,
0.211953966400843));
#279256=CARTESIAN_POINT('Ctrl Pts',(-1.32877363457237,-1.43264672130478,
0.215779871885671));
#279257=CARTESIAN_POINT('Ctrl Pts',(-1.30061249035615,-1.45876606070468,
0.217977527811222));
#279258=CARTESIAN_POINT('Ctrl Pts',(-1.27171567625023,-1.48402247386527,
0.220175183736774));
#279259=CARTESIAN_POINT('Ctrl Pts',(-1.24214451955084,-1.50837428795038,
0.222372839662326));
#279260=CARTESIAN_POINT('Ctrl Pts',(-1.18934685645933,-1.5518531037709,
0.226296632645057));
#279261=CARTESIAN_POINT('Ctrl Pts',(-1.13416061912592,-1.59264129349927,
0.230220425627789));
#279262=CARTESIAN_POINT('Ctrl Pts',(-1.07689083932768,-1.63046684117529,
0.23414421861052));
#279263=CARTESIAN_POINT('Ctrl Pts',(-1.01970717829159,-1.668235509126,0.238062111235406));
#279264=CARTESIAN_POINT('Ctrl Pts',(-0.960446599313705,-1.70305010949116,
0.241980003860292));
#279265=CARTESIAN_POINT('Ctrl Pts',(-0.89944693364595,-1.73467899438337,
0.245897896485178));
#279266=CARTESIAN_POINT('Ctrl Pts',(-0.838519344608369,-1.76627050688322,
0.249811159765055));
#279267=CARTESIAN_POINT('Ctrl Pts',(-0.775857183549963,-1.79468355593104,
0.253724423044932));
#279268=CARTESIAN_POINT('Ctrl Pts',(-0.711825428870553,-1.81973090285714,
0.25763768632481));
#279269=CARTESIAN_POINT('Ctrl Pts',(-0.64783411101502,-1.84476243208214,
0.261548478331819));
#279270=CARTESIAN_POINT('Ctrl Pts',(-0.582475370960143,-1.8664322977552,
0.265459270338828));
#279271=CARTESIAN_POINT('Ctrl Pts',(-0.516135449431958,-1.88460080596387,
0.269370062345837));
#279272=CARTESIAN_POINT('Ctrl Pts',(-0.449814856770113,-1.9027640205777,
0.273279714900549));
#279273=CARTESIAN_POINT('Ctrl Pts',(-0.38251412278591,-1.91742777368561,
0.277189367455261));
#279274=CARTESIAN_POINT('Ctrl Pts',(-0.314634262868098,-1.9285023413596,
0.281099020009973));
#279275=CARTESIAN_POINT('Ctrl Pts',(-0.246751092056681,-1.93957744920434,
0.285008863261066));
#279276=CARTESIAN_POINT('Ctrl Pts',(-0.178289223454827,-1.94706294757461,
0.288918706512159));
#279277=CARTESIAN_POINT('Ctrl Pts',(-0.109657688950741,-1.95092060096099,
0.292828549763252));
#279278=CARTESIAN_POINT('Ctrl Pts',(-0.0409547879490927,-1.95478226572804,
0.296742458664645));
#279279=CARTESIAN_POINT('Ctrl Pts',(0.0279176406827614,-1.95500852899902,
0.300656367566038));
#279280=CARTESIAN_POINT('Ctrl Pts',(0.0965486492807848,-1.95161327068711,
0.304570276467431));
#279281=CARTESIAN_POINT('Ctrl Pts',(0.165219803870349,-1.94821602630486,
0.308486474825979));
#279282=CARTESIAN_POINT('Ctrl Pts',(0.233648769520342,-1.94119309345488,
0.312402673184526));
#279283=CARTESIAN_POINT('Ctrl Pts',(0.301430589707728,-1.93061016251041,
0.316318871543074));
#279284=CARTESIAN_POINT('Ctrl Pts',(0.369327280566128,-1.92000929654478,
0.320241706730376));
#279285=CARTESIAN_POINT('Ctrl Pts',(0.436574157399652,-1.90583649145238,
0.324164541917678));
#279286=CARTESIAN_POINT('Ctrl Pts',(0.502778157531278,-1.88820817822333,
0.32808737710498));
#279287=CARTESIAN_POINT('Ctrl Pts',(0.533560358420196,-1.88001172063662,
0.329911337901149));
#279288=CARTESIAN_POINT('Ctrl Pts',(0.564117343255775,-1.87106892339258,
0.331735298697319));
#279289=CARTESIAN_POINT('Ctrl Pts',(0.594411056057898,-1.8613950404028,
0.333559259493488));
#279290=CARTESIAN_POINT('Ctrl Pts',(0.659594398880924,-1.84057963109751,
0.337483897673332));
#279291=CARTESIAN_POINT('Ctrl Pts',(0.723807350727231,-1.81629647786615,
0.341408535853176));
#279292=CARTESIAN_POINT('Ctrl Pts',(0.786655984201979,-1.78865546221714,
0.34533317403302));
#279293=CARTESIAN_POINT('Ctrl Pts',(0.849412399165395,-1.76105500454329,
0.349252053546837));
#279294=CARTESIAN_POINT('Ctrl Pts',(0.910808024201147,-1.7301066599176,
0.353170933060653));
#279295=CARTESIAN_POINT('Ctrl Pts',(0.970465215395659,-1.69596971249697,
0.35708981257447));
#279296=CARTESIAN_POINT('Ctrl Pts',(1.03005507208741,-1.66187129512334,
0.361004268886352));
#279297=CARTESIAN_POINT('Ctrl Pts',(1.08790996866424,-1.62459166521176,
0.364918725198235));
#279298=CARTESIAN_POINT('Ctrl Pts',(1.1436749754053,-1.58433694352928,0.368833181510118));
#279299=CARTESIAN_POINT('Ctrl Pts',(1.19940659356289,-1.54410632384575,
0.372745294091427));
#279300=CARTESIAN_POINT('Ctrl Pts',(1.25305040793731,-1.50090443257899,
0.376657406672736));
#279301=CARTESIAN_POINT('Ctrl Pts',(1.30428003732066,-1.45498095666123,
0.380569519254044));
#279302=CARTESIAN_POINT('Ctrl Pts',(1.35549639405906,-1.40906937866266,
0.384480618279684));
#279303=CARTESIAN_POINT('Ctrl Pts',(1.40429944299621,-1.3604379429279,0.388391717305323));
#279304=CARTESIAN_POINT('Ctrl Pts',(1.45039689124339,-1.30937575121563,
0.392302816330962));
#279305=CARTESIAN_POINT('Ctrl Pts',(1.49649805312221,-1.25830944590971,
0.396214230436539));
#279306=CARTESIAN_POINT('Ctrl Pts',(1.53989285511708,-1.20481236120016,
0.400125644542115));
#279307=CARTESIAN_POINT('Ctrl Pts',(1.58032801561469,-1.14920814610032,
0.404037058647691));
#279308=CARTESIAN_POINT('Ctrl Pts',(1.62080705206791,-1.09354359519265,
0.407952717005783));
#279309=CARTESIAN_POINT('Ctrl Pts',(1.65831974925713,-1.03576774794434,
0.411868375363875));
#279310=CARTESIAN_POINT('Ctrl Pts',(1.69265564610032,-0.976234020983042,
0.415784033721968));
#279311=CARTESIAN_POINT('Ctrl Pts',(1.72701253630214,-0.916663894422599,
0.419702086158205));
#279312=CARTESIAN_POINT('Ctrl Pts',(1.75818853823833,-0.855334185779185,
0.423620138594443));
#279313=CARTESIAN_POINT('Ctrl Pts',(1.78602003479096,-0.792621243296755,
0.42753819103068));
#279314=CARTESIAN_POINT('Ctrl Pts',(1.81389969051431,-0.72979978335471,
0.431463023201374));
#279315=CARTESIAN_POINT('Ctrl Pts',(1.83842311533252,-0.665590769809821,
0.435387855372068));
#279316=CARTESIAN_POINT('Ctrl Pts',(1.85947581564609,-0.600387950434814,
0.439312687542762));
#279317=CARTESIAN_POINT('Ctrl Pts',(1.86918995906384,-0.570302045576213,
0.441123684803391));
#279318=CARTESIAN_POINT('Ctrl Pts',(1.8781658653323,-0.54000472245759,0.442934682064021));
#279319=CARTESIAN_POINT('Ctrl Pts',(1.88639596582335,-0.509535337464828,
0.444745679324651));
#279320=CARTESIAN_POINT('Ctrl Pts',(1.90417601728029,-0.443710231972858,
0.44865810111311));
#279321=CARTESIAN_POINT('Ctrl Pts',(1.91854275019372,-0.376819134628719,
0.452570522901568));
#279322=CARTESIAN_POINT('Ctrl Pts',(1.92937313881236,-0.309249561405273,
0.456482944690027));
#279323=CARTESIAN_POINT('Ctrl Pts',(1.9401869556771,-0.241783377485532,
0.460389380018231));
#279324=CARTESIAN_POINT('Ctrl Pts',(1.94747508855052,-0.173641261023044,
0.464295815346436));
#279325=CARTESIAN_POINT('Ctrl Pts',(1.95116474653031,-0.105224198249775,
0.46820225067464));
#279326=CARTESIAN_POINT('Ctrl Pts',(1.95484996606166,-0.0368894373069517,
0.4721039867836));
#279327=CARTESIAN_POINT('Ctrl Pts',(1.95494528057357,0.0317191227619464,
0.47600572289256));
#279328=CARTESIAN_POINT('Ctrl Pts',(1.95142952386527,0.100193878989584,
0.47990745900152));
#279329=CARTESIAN_POINT('Ctrl Pts',(1.94791602675104,0.168624626155676,
0.483806687445553));
#279330=CARTESIAN_POINT('Ctrl Pts',(1.94079608694011,0.236921248335345,
0.487705915889587));
#279331=CARTESIAN_POINT('Ctrl Pts',(1.93010061963535,0.304676218440552,
0.49160514433362));
#279332=CARTESIAN_POINT('Ctrl Pts',(1.9194083283643,0.372411068614334,0.495503214896412));
#279333=CARTESIAN_POINT('Ctrl Pts',(1.90514269399046,0.439604098723601,
0.499401285459204));
#279334=CARTESIAN_POINT('Ctrl Pts',(1.88738626341259,0.505854813836402,
0.503299356021995));
#279335=CARTESIAN_POINT('Ctrl Pts',(1.86962896642995,0.572108761577267,
0.507197616786693));
#279336=CARTESIAN_POINT('Ctrl Pts',(1.84838066534311,0.637419826993278,
0.511095877551392));
#279337=CARTESIAN_POINT('Ctrl Pts',(1.82377413864022,0.701401376693196,
0.514994138316089));
#279338=CARTESIAN_POINT('Ctrl Pts',(1.79914144699063,0.765450960124916,
0.518896544232454));
#279339=CARTESIAN_POINT('Ctrl Pts',(1.77114358069267,0.828167744912018,
0.522798950148818));
#279340=CARTESIAN_POINT('Ctrl Pts',(1.73996160430977,0.889184803923099,
0.526701356065182));
#279341=CARTESIAN_POINT('Ctrl Pts',(1.70876110556513,0.950238107591229,
0.530606080044174));
#279342=CARTESIAN_POINT('Ctrl Pts',(1.6743729803604,1.00958924919398,0.534510804023165));
#279343=CARTESIAN_POINT('Ctrl Pts',(1.63702301426926,1.06689814450714,0.538415528002157));
#279344=CARTESIAN_POINT('Ctrl Pts',(1.59960798031843,1.12430687838912,0.542327054451367));
#279345=CARTESIAN_POINT('Ctrl Pts',(1.55922109804311,1.17966586668971,0.546238580900578));
#279346=CARTESIAN_POINT('Ctrl Pts',(1.51612945757764,1.23266681137497,0.550150107349788));
#279347=CARTESIAN_POINT('Ctrl Pts',(1.49489686758029,1.25878202341652,0.552077437951797));
#279348=CARTESIAN_POINT('Ctrl Pts',(1.47300819005873,1.28432529019343,0.554004768553805));
#279349=CARTESIAN_POINT('Ctrl Pts',(1.45049855981685,1.30926312403934,0.555932099155814));
#279350=CARTESIAN_POINT('Ctrl Pts',(1.40472845234233,1.35997063558188,0.55985104974918));
#279351=CARTESIAN_POINT('Ctrl Pts',(1.35620559048947,1.4083754866274,0.563770000342546));
#279352=CARTESIAN_POINT('Ctrl Pts',(1.30519070746797,1.45416409567121,0.567688950935912));
#279353=CARTESIAN_POINT('Ctrl Pts',(1.25425265348505,1.49988374650905,0.571601999541692));
#279354=CARTESIAN_POINT('Ctrl Pts',(1.20083038977689,1.54299464937113,0.575515048147471));
#279355=CARTESIAN_POINT('Ctrl Pts',(1.14522307837355,1.58321827325249,0.579428096753251));
#279356=CARTESIAN_POINT('Ctrl Pts',(1.08968122685999,1.62339454663409,0.583336538991199));
#279357=CARTESIAN_POINT('Ctrl Pts',(1.03195983261817,1.66069000451881,0.587244981229147));
#279358=CARTESIAN_POINT('Ctrl Pts',(0.972391486925007,1.69486601126926,
0.591153423467096));
#279359=CARTESIAN_POINT('Ctrl Pts',(0.912860539003305,1.72902056188432,
0.595059411934876));
#279360=CARTESIAN_POINT('Ctrl Pts',(0.851485365306069,1.76005930221187,
0.598965400402657));
#279361=CARTESIAN_POINT('Ctrl Pts',(0.788626611815159,1.78778747817993,
0.602871388870437));
#279362=CARTESIAN_POINT('Ctrl Pts',(0.725785787387798,1.81550774530154,
0.606776263241746));
#279363=CARTESIAN_POINT('Ctrl Pts',(0.661462672826329,1.83991912427526,
0.610681137613056));
#279364=CARTESIAN_POINT('Ctrl Pts',(0.596039893333901,1.86087410792738,
0.614586011984365));
#279365=CARTESIAN_POINT('Ctrl Pts',(0.530613362105011,1.88183029326455,
0.618491110284704));
#279366=CARTESIAN_POINT('Ctrl Pts',(0.464087509733959,1.89932954221597,
0.622396208585044));
#279367=CARTESIAN_POINT('Ctrl Pts',(0.396860461678409,1.9132740979683,0.626301306885383));
#279368=CARTESIAN_POINT('Ctrl Pts',(0.329561975791958,1.92723347169709,
0.630210554880824));
#279369=CARTESIAN_POINT('Ctrl Pts',(0.2615612895033,1.93763051365435,0.634119802876266));
#279370=CARTESIAN_POINT('Ctrl Pts',(0.193266079982631,1.94441873636523,
0.638029050871707));
#279371=CARTESIAN_POINT('Ctrl Pts',(0.124930149413867,1.95121100655682,
0.641940629757949));
#279372=CARTESIAN_POINT('Ctrl Pts',(0.0562998373073983,1.95439015220606,
0.645852208644192));
#279373=CARTESIAN_POINT('Ctrl Pts',(-0.012215527754201,1.95396181663862,
0.649763787530434));
#279374=CARTESIAN_POINT('Ctrl Pts',(-0.0808491282404187,1.95353274190212,
0.653682116540391));
#279375=CARTESIAN_POINT('Ctrl Pts',(-0.149366895216171,1.9494837898546,
0.657600445550349));
#279376=CARTESIAN_POINT('Ctrl Pts',(-0.217363844836177,1.94187253931818,
0.661518774560306));
#279377=CARTESIAN_POINT('Ctrl Pts',(-0.249755674678064,1.93824675413756,
0.663385356035863));
#279378=CARTESIAN_POINT('Ctrl Pts',(-0.282029455866692,1.93381332843034,
0.66525193751142));
#279379=CARTESIAN_POINT('Ctrl Pts',(-0.314142410573999,1.9285825224446,
0.667118518986977));
#279380=CARTESIAN_POINT('Ctrl Pts',(-0.381558581303711,1.91760125608019,
0.67103711746488));
#279381=CARTESIAN_POINT('Ctrl Pts',(-0.44853151726403,1.90305909627577,
0.674955715942784));
#279382=CARTESIAN_POINT('Ctrl Pts',(-0.514656430893057,1.88500524087877,
0.678874314420688));
#279383=CARTESIAN_POINT('Ctrl Pts',(-0.580681976046049,1.86697851571149,
0.682787024268459));
#279384=CARTESIAN_POINT('Ctrl Pts',(-0.645861557457656,1.84545069682505,
0.686699734116229));
#279385=CARTESIAN_POINT('Ctrl Pts',(-0.709799023038066,1.82052227311127,
0.690612443964));
#279386=CARTESIAN_POINT('Ctrl Pts',(-0.773661569352443,1.79562305948879,
0.694520569060916));
#279387=CARTESIAN_POINT('Ctrl Pts',(-0.836284434412466,1.7673313324856,
0.698428694157831));
#279388=CARTESIAN_POINT('Ctrl Pts',(-0.897286881557168,1.7357972958227,
0.702336819254747));
#279389=CARTESIAN_POINT('Ctrl Pts',(-0.958251240337448,1.70428294820404,
0.706242504218523));
#279390=CARTESIAN_POINT('Ctrl Pts',(-1.01759675234698,1.66953053205859,
0.710148189182298));
#279391=CARTESIAN_POINT('Ctrl Pts',(-1.07496436257844,1.63173760733346,
0.714053874146073));
#279392=CARTESIAN_POINT('Ctrl Pts',(-1.13231581651118,1.59395532613661,
0.717958459161416));
#279393=CARTESIAN_POINT('Ctrl Pts',(-1.18769006402541,1.55313450665621,
0.721863044176759));
#279394=CARTESIAN_POINT('Ctrl Pts',(-1.24075585318281,1.50951678122259,
0.725767629192101));
#279395=CARTESIAN_POINT('Ctrl Pts',(-1.29382488510409,1.46589639038086,
0.72967245281027));
#279396=CARTESIAN_POINT('Ctrl Pts',(-1.34458480034009,1.41947906847847,
0.73357727642844));
#279397=CARTESIAN_POINT('Ctrl Pts',(-1.39273776541595,1.37054642999943,
0.737482100046609));
#279398=CARTESIAN_POINT('Ctrl Pts',(-1.44094220223177,1.32156148637076,
0.741391097614722));
#279399=CARTESIAN_POINT('Ctrl Pts',(-1.48653378203202,1.27005621153404,
0.745300095182835));
#279400=CARTESIAN_POINT('Ctrl Pts',(-1.5292525883575,1.21634802626629,0.749209092750949));
#279401=CARTESIAN_POINT('Ctrl Pts',(-1.57199701479702,1.16260763013054,
0.753120434695511));
#279402=CARTESIAN_POINT('Ctrl Pts',(-1.61186495341211,1.10666209469884,
0.757031776640074));
#279403=CARTESIAN_POINT('Ctrl Pts',(-1.64863941199854,1.0488584695778,0.760943118584636));
#279404=CARTESIAN_POINT('Ctrl Pts',(-1.68547755590406,0.99095474122068,
0.76486123411797));
#279405=CARTESIAN_POINT('Ctrl Pts',(-1.71921128586498,0.931186928883176,
0.768779349651304));
#279406=CARTESIAN_POINT('Ctrl Pts',(-1.74966961716525,0.869926566308211,
0.772697465184638));
#279407=CARTESIAN_POINT('Ctrl Pts',(-1.76419992629248,0.840701984150862,
0.774566623062472));
#279408=CARTESIAN_POINT('Ctrl Pts',(-1.7779855241982,0.811138014747312,
0.776435780940305));
#279409=CARTESIAN_POINT('Ctrl Pts',(-1.79101180145104,0.781276344876198,
0.778304938818138));
#279410=CARTESIAN_POINT('Ctrl Pts',(-1.82108266615991,0.712341359289296,
0.78261984725843));
#279411=CARTESIAN_POINT('Ctrl Pts',(-1.84720652553836,0.641584118440989,
0.786934755698722));
#279412=CARTESIAN_POINT('Ctrl Pts',(-1.86918209141702,0.56945088385734,
0.791249664139013));
#279413=CARTESIAN_POINT('Ctrl Pts',(-1.89109060934678,0.49753772940508,
0.79555140769599));
#279414=CARTESIAN_POINT('Ctrl Pts',(-1.9088759398764,0.42425724395805,0.799853151252965));
#279415=CARTESIAN_POINT('Ctrl Pts',(-1.92238492518644,0.350074562651913,
0.804154894809942));
#279416=CARTESIAN_POINT('Ctrl Pts',(-1.93582638752964,0.276262674163655,
0.80843513664189));
#279417=CARTESIAN_POINT('Ctrl Pts',(-1.94503401527278,0.201557885078121,
0.812715378473838));
#279418=CARTESIAN_POINT('Ctrl Pts',(-1.94990505686432,0.12643681906369,
0.816995620305786));
#279419=CARTESIAN_POINT('Ctrl Pts',(-1.95261153457162,0.0846975962104973,
0.819373834263172));
#279420=CARTESIAN_POINT('Ctrl Pts',(-1.95398008893921,0.0428301635186168,
0.821752048220558));
#279421=CARTESIAN_POINT('Ctrl Pts',(-1.95399978425297,0.000918226197701749,
0.824130262177944));
#279422=CARTESIAN_POINT('',(-1.95399925675175,-0.00170429269710383,1.52413032610373));
#279423=CARTESIAN_POINT('Ctrl Pts',(-1.95118672945361,0.000916100096969453,
0.824130307875757));
#279424=CARTESIAN_POINT('Ctrl Pts',(-1.94959408276249,-0.382490737583375,
0.845917324800272));
#279425=CARTESIAN_POINT('Ctrl Pts',(-1.65494759972259,-1.42039331085723,
0.904766481668509));
#279426=CARTESIAN_POINT('Ctrl Pts',(0.0320890232727861,-2.30962717925355,
1.00067777848046));
#279427=CARTESIAN_POINT('Ctrl Pts',(1.95839267869744,-1.22482325334232,
1.11186419831163));
#279428=CARTESIAN_POINT('Ctrl Pts',(2.0907344889796,0.982002812028434,1.22305061814279));
#279429=CARTESIAN_POINT('Ctrl Pts',(0.307867124228207,2.28925546628533,
1.33423703797395));
#279430=CARTESIAN_POINT('Ctrl Pts',(-1.55595354203437,1.57636391564955,
1.4345969345516));
#279431=CARTESIAN_POINT('Ctrl Pts',(-1.94903067523895,0.458983666015645,
1.49789469118554));
#279432=CARTESIAN_POINT('Ctrl Pts',(-1.95287184048439,-0.001702989282844,
1.52413030787576));
#279433=CARTESIAN_POINT('',(-1.9539999995111,4.37108594993626E-5,2.22413030791928));
#279434=CARTESIAN_POINT('Ctrl Pts',(-1.95399925675175,-0.00170429269710383,
1.52413032610373));
#279435=CARTESIAN_POINT('Ctrl Pts',(-1.95392656932596,-0.0850416068845222,
1.52887359761229));
#279436=CARTESIAN_POINT('Ctrl Pts',(-1.9485186276568,-0.168144569686724,
1.53361686912084));
#279437=CARTESIAN_POINT('Ctrl Pts',(-1.93788759724531,-0.25041497647464,
1.5383601406294));
#279438=CARTESIAN_POINT('Ctrl Pts',(-1.92709355836742,-0.333946857674933,
1.54317614200369));
#279439=CARTESIAN_POINT('Ctrl Pts',(-1.91091509568121,-0.416620496621874,
1.54799214337797));
#279440=CARTESIAN_POINT('Ctrl Pts',(-1.88951825859737,-0.497832050421777,
1.55280814475226));
#279441=CARTESIAN_POINT('Ctrl Pts',(-1.88388806507971,-0.519201412723879,
1.55407538904693));
#279442=CARTESIAN_POINT('Ctrl Pts',(-1.87789681471551,-0.540469658625722,
1.5553426333416));
#279443=CARTESIAN_POINT('Ctrl Pts',(-1.87154807587892,-0.561626031869897,
1.55660987763628));
#279444=CARTESIAN_POINT('Ctrl Pts',(-1.85192043594831,-0.627032671985691,
1.56052766593411));
#279445=CARTESIAN_POINT('Ctrl Pts',(-1.82882094278616,-0.691539084024109,
1.56444545423193));
#279446=CARTESIAN_POINT('Ctrl Pts',(-1.802350646318,-0.754750387689271,
1.56836324252976));
#279447=CARTESIAN_POINT('Ctrl Pts',(-1.77592026363396,-0.817866376882526,
1.57227512330945));
#279448=CARTESIAN_POINT('Ctrl Pts',(-1.74612935349376,-0.879690683267352,
1.57618700408915));
#279449=CARTESIAN_POINT('Ctrl Pts',(-1.71312871159643,-0.939843613322961,
1.58009888486884));
#279450=CARTESIAN_POINT('Ctrl Pts',(-1.68016694859202,-0.999925675686545,
1.58400615696261));
#279451=CARTESIAN_POINT('Ctrl Pts',(-1.64400319934452,-1.05833984305939,
1.58791342905637));
#279452=CARTESIAN_POINT('Ctrl Pts',(-1.60483556458594,-1.1147281330621,
1.59182070115013));
#279453=CARTESIAN_POINT('Ctrl Pts',(-1.56569253448401,-1.17108100059105,
1.59572551874061));
#279454=CARTESIAN_POINT('Ctrl Pts',(-1.52354964208937,-1.22541011206912,
1.59963033633109));
#279455=CARTESIAN_POINT('Ctrl Pts',(-1.47864914422619,-1.27738510570585,
1.60353515392156));
#279456=CARTESIAN_POINT('Ctrl Pts',(-1.43376144462226,-1.32934528459721,
1.60743885849837));
#279457=CARTESIAN_POINT('Ctrl Pts',(-1.38611802137467,-1.37895230557505,
1.61134256307518));
#279458=CARTESIAN_POINT('Ctrl Pts',(-1.33600123801422,-1.4259090756512,
1.61524626765199));
#279459=CARTESIAN_POINT('Ctrl Pts',(-1.28588154257544,-1.47286857419042,
1.61915019905687));
#279460=CARTESIAN_POINT('Ctrl Pts',(-1.2332885624588,-1.51717718157874,
1.62305413046175));
#279461=CARTESIAN_POINT('Ctrl Pts',(-1.17853998361191,-1.55857611525009,
1.62695806186663));
#279462=CARTESIAN_POINT('Ctrl Pts',(-1.1237330345662,-1.60001918639569,
1.63086615544809));
#279463=CARTESIAN_POINT('Ctrl Pts',(-1.06676629344045,-1.63854609552244,
1.63477424902955));
#279464=CARTESIAN_POINT('Ctrl Pts',(-1.00798804288102,-1.67394029326284,
1.638682342611));
#279465=CARTESIAN_POINT('Ctrl Pts',(-0.949174653644986,-1.70935565027995,
1.64259277251984));
#279466=CARTESIAN_POINT('Ctrl Pts',(-0.888548034036203,-1.74163433747435,
1.64650320242868));
#279467=CARTESIAN_POINT('Ctrl Pts',(-0.826480287686199,-1.77060620524896,
1.65041363233753));
#279468=CARTESIAN_POINT('Ctrl Pts',(-0.764305074334288,-1.79962823627184,
1.65433083294779));
#279469=CARTESIAN_POINT('Ctrl Pts',(-0.700684210020102,-1.82533183617092,
1.65824803355805));
#279470=CARTESIAN_POINT('Ctrl Pts',(-0.636008116819952,-1.84759564714229,
1.66216523416832));
#279471=CARTESIAN_POINT('Ctrl Pts',(-0.605017007693411,-1.85826388885644,
1.66404225526802));
#279472=CARTESIAN_POINT('Ctrl Pts',(-0.573783806829276,-1.86814307416366,
1.66591927636773));
#279473=CARTESIAN_POINT('Ctrl Pts',(-0.542352307151149,-1.87722400765807,
1.66779629746744));
#279474=CARTESIAN_POINT('Ctrl Pts',(-0.4767474116325,-1.89617804100721,
1.67171407976843));
#279475=CARTESIAN_POINT('Ctrl Pts',(-0.410017392047881,-1.91172646298042,
1.67563186206942));
#279476=CARTESIAN_POINT('Ctrl Pts',(-0.34254886834496,-1.92374017808944,
1.67954964437041));
#279477=CARTESIAN_POINT('Ctrl Pts',(-0.275182079368546,-1.93573577790626,
1.68346151910904));
#279478=CARTESIAN_POINT('Ctrl Pts',(-0.207079476767389,-1.94420716324699,
1.68737339384767));
#279479=CARTESIAN_POINT('Ctrl Pts',(-0.138641878894337,-1.94907527546184,
1.6912852685863));
#279480=CARTESIAN_POINT('Ctrl Pts',(-0.0702849098335151,-1.95393765237741,
1.69519253460366));
#279481=CARTESIAN_POINT('Ctrl Pts',(-0.00159421772505816,-1.95520515229954,
1.69909980062101));
#279482=CARTESIAN_POINT('Ctrl Pts',(0.0670219865489309,-1.95285023832321,
1.70300706663836));
#279483=CARTESIAN_POINT('Ctrl Pts',(0.135595086525049,-1.95049680369007,
1.70691187813407));
#279484=CARTESIAN_POINT('Ctrl Pts',(0.204093300905156,-1.9445254859769,
1.71081668962978));
#279485=CARTESIAN_POINT('Ctrl Pts',(0.27210769921077,-1.93496082648467,
1.71472150112549));
#279486=CARTESIAN_POINT('Ctrl Pts',(0.340102710776028,-1.92539889329119,
1.71862519959854));
#279487=CARTESIAN_POINT('Ctrl Pts',(0.407613693072952,-1.91224572006381,
1.72252889807159));
#279488=CARTESIAN_POINT('Ctrl Pts',(0.474237937445677,-1.89557758445474,
1.72643259654464));
#279489=CARTESIAN_POINT('Ctrl Pts',(0.540866053088966,-1.87890848032643,
1.73033652184613));
#279490=CARTESIAN_POINT('Ctrl Pts',(0.606606851861831,-1.85872413021012,
1.73424044714761));
#279491=CARTESIAN_POINT('Ctrl Pts',(0.671070676876058,-1.83515125987944,
1.73814437244909));
#279492=CARTESIAN_POINT('Ctrl Pts',(0.735603230811031,-1.81155325703551,
1.74205245996982));
#279493=CARTESIAN_POINT('Ctrl Pts',(0.798855630951643,-1.78455969333248,
1.74596054749054));
#279494=CARTESIAN_POINT('Ctrl Pts',(0.860457130100616,-1.75434589726742,
1.74986863501126));
#279495=CARTESIAN_POINT('Ctrl Pts',(0.922095456014425,-1.72411403871397,
1.7537790588748));
#279496=CARTESIAN_POINT('Ctrl Pts',(0.982080486999279,-1.69065835612698,
1.75768948273834));
#279497=CARTESIAN_POINT('Ctrl Pts',(1.04006755942586,-1.65419934464681,
1.76159990660188));
#279498=CARTESIAN_POINT('Ctrl Pts',(1.09815503484188,-1.6176772054109,1.76551710125466));
#279499=CARTESIAN_POINT('Ctrl Pts',(1.15423724526712,-1.57814164174512,
1.76943429590743));
#279500=CARTESIAN_POINT('Ctrl Pts',(1.20800060313945,-1.53585498756059,
1.77335149056021));
#279501=CARTESIAN_POINT('Ctrl Pts',(1.23376339898637,-1.5155916989209,1.77522856613967));
#279502=CARTESIAN_POINT('Ctrl Pts',(1.25899425580077,-1.49469726976515,
1.77710564171914));
#279503=CARTESIAN_POINT('Ctrl Pts',(1.28366170827141,-1.47320352250384,
1.7789827172986));
#279504=CARTESIAN_POINT('Ctrl Pts',(1.3351469234973,-1.42834237581362,1.78290049682282));
#279505=CARTESIAN_POINT('Ctrl Pts',(1.38437988714249,-1.38068991879112,
1.78681827634703));
#279506=CARTESIAN_POINT('Ctrl Pts',(1.43104256868493,-1.33050109605804,
1.79073605587124));
#279507=CARTESIAN_POINT('Ctrl Pts',(1.47763488741356,-1.28038795321888,
1.79464792776259));
#279508=CARTESIAN_POINT('Ctrl Pts',(1.52166428365344,-1.22774639247634,
1.79855979965393));
#279509=CARTESIAN_POINT('Ctrl Pts',(1.56284708215548,-1.17287040963531,
1.80247167154528));
#279510=CARTESIAN_POINT('Ctrl Pts',(1.6039813607217,-1.11805907949545,1.80637893462469));
#279511=CARTESIAN_POINT('Ctrl Pts',(1.64227540820047,-1.0610189470505,1.8102861977041));
#279512=CARTESIAN_POINT('Ctrl Pts',(1.67748484117931,-1.0020781444646,1.81419346078352));
#279513=CARTESIAN_POINT('Ctrl Pts',(1.7126721552897,-0.943174368997536,
1.81809826928668));
#279514=CARTESIAN_POINT('Ctrl Pts',(1.74477844706838,-0.882372713324816,
1.82200307778984));
#279515=CARTESIAN_POINT('Ctrl Pts',(1.77360270918012,-0.820030139683255,
1.825907886293));
#279516=CARTESIAN_POINT('Ctrl Pts',(1.80241875488326,-0.757705336906271,
1.82981158172335));
#279517=CARTESIAN_POINT('Ctrl Pts',(1.82795442174516,-0.693840934467796,
1.83371527715371));
#279518=CARTESIAN_POINT('Ctrl Pts',(1.85005555332991,-0.628816705879527,
1.83761897258407));
#279519=CARTESIAN_POINT('Ctrl Pts',(1.87215796886587,-0.563788699749949,
1.84152289479714));
#279520=CARTESIAN_POINT('Ctrl Pts',(1.89082529708749,-0.497601200331658,
1.84542681701021));
#279521=CARTESIAN_POINT('Ctrl Pts',(1.90595285153498,-0.430650354377729,
1.84933073922327));
#279522=CARTESIAN_POINT('Ctrl Pts',(1.92109653424097,-0.363628128707158,
1.85323882360722));
#279523=CARTESIAN_POINT('Ctrl Pts',(1.93269280284966,-0.295841413118037,
1.85714690799117));
#279524=CARTESIAN_POINT('Ctrl Pts',(1.94068806489674,-0.227696804473273,
1.86105499237512));
#279525=CARTESIAN_POINT('Ctrl Pts',(1.94868810662962,-0.159511457974536,
1.86496541306965));
#279526=CARTESIAN_POINT('Ctrl Pts',(1.95308282598641,-0.0909682836632935,
1.86887583376419));
#279527=CARTESIAN_POINT('Ctrl Pts',(1.95387072493651,-0.0224764373531737,
1.87278625445873));
#279528=CARTESIAN_POINT('Ctrl Pts',(1.95465998810928,0.0461340004717905,
1.87670344592584));
#279529=CARTESIAN_POINT('Ctrl Pts',(1.95182998677124,0.11469244159376,1.88062063739294));
#279530=CARTESIAN_POINT('Ctrl Pts',(1.94543122643806,0.182793170549961,
1.88453782886004));
#279531=CARTESIAN_POINT('Ctrl Pts',(1.94236496563336,0.215426772231656,
1.88641493161661));
#279532=CARTESIAN_POINT('Ctrl Pts',(1.93847997567259,0.247955398226014,
1.88829203437319));
#279533=CARTESIAN_POINT('Ctrl Pts',(1.93378594678926,0.280335356315162,
1.89016913712976));
#279534=CARTESIAN_POINT('Ctrl Pts',(1.9239888350599,0.347916974382912,1.89408691988968));
#279535=CARTESIAN_POINT('Ctrl Pts',(1.91062524938797,0.415118643649139,
1.89800470264961));
#279536=CARTESIAN_POINT('Ctrl Pts',(1.89373707840404,0.481534918648398,
1.90192248540953));
#279537=CARTESIAN_POINT('Ctrl Pts',(1.87687437290302,0.547851045294272,
1.90583436058893));
#279538=CARTESIAN_POINT('Ctrl Pts',(1.85649775003331,0.61338365508765,1.90974623576834));
#279539=CARTESIAN_POINT('Ctrl Pts',(1.83270053654601,0.677735009678545,
1.91365811094774));
#279540=CARTESIAN_POINT('Ctrl Pts',(1.80893135959259,0.742010549135241,
1.91756537737658));
#279541=CARTESIAN_POINT('Ctrl Pts',(1.7817497653383,0.805107138040061,1.92147264380543));
#279542=CARTESIAN_POINT('Ctrl Pts',(1.75129906377595,0.86664155751815,1.92537991023427));
#279543=CARTESIAN_POINT('Ctrl Pts',(1.72086749130787,0.928137321147573,
1.92928472212301));
#279544=CARTESIAN_POINT('Ctrl Pts',(1.68717110299145,0.988072422073371,
1.93318953401176));
#279545=CARTESIAN_POINT('Ctrl Pts',(1.65040094626024,1.04608446914353,1.93709434590051));
#279546=CARTESIAN_POINT('Ctrl Pts',(1.61364127062815,1.10407998024896,1.94099804474748));
#279547=CARTESIAN_POINT('Ctrl Pts',(1.57380982914045,1.16015311031874,1.94490174359446));
#279548=CARTESIAN_POINT('Ctrl Pts',(1.53114223179459,1.21396847818017,1.94880544244144));
#279549=CARTESIAN_POINT('Ctrl Pts',(1.48847215542045,1.26778697276604,1.95270936809705));
#279550=CARTESIAN_POINT('Ctrl Pts',(1.44296590369202,1.3193470607829,1.95661329375267));
#279551=CARTESIAN_POINT('Ctrl Pts',(1.39489965817954,1.36834606134947,1.96051721940829));
#279552=CARTESIAN_POINT('Ctrl Pts',(1.34678216663865,1.41739730240515,1.96442530725056));
#279553=CARTESIAN_POINT('Ctrl Pts',(1.29609957951229,1.46388165480261,1.96833339509282));
#279554=CARTESIAN_POINT('Ctrl Pts',(1.24316455237532,1.50753371296216,1.97224148293508));
#279555=CARTESIAN_POINT('Ctrl Pts',(1.19019787973408,1.55121186710139,1.97615190710203));
#279556=CARTESIAN_POINT('Ctrl Pts',(1.13497648281745,1.59205406464089,1.98006233126897));
#279557=CARTESIAN_POINT('Ctrl Pts',(1.07784340175706,1.62983729288809,1.98397275543592));
#279558=CARTESIAN_POINT('Ctrl Pts',(1.02061139683592,1.66768594142666,1.98788995036069));
#279559=CARTESIAN_POINT('Ctrl Pts',(0.961461525323312,1.70246480033226,
1.99180714528546));
#279560=CARTESIAN_POINT('Ctrl Pts',(0.900762120884259,1.73399642490407,
1.99572434021024));
#279561=CARTESIAN_POINT('Ctrl Pts',(0.871675703213898,1.74910599658103,
1.99760141246047));
#279562=CARTESIAN_POINT('Ctrl Pts',(0.842233784874234,1.76347064403427,
1.9994784847107));
#279563=CARTESIAN_POINT('Ctrl Pts',(0.812478334269017,1.7770748313854,2.00135555696093));
#279564=CARTESIAN_POINT('Ctrl Pts',(0.750373447598841,1.80546917583313,
2.00527333864467));
#279565=CARTESIAN_POINT('Ctrl Pts',(0.686654915849971,1.83066036058571,
2.0091911203284));
#279566=CARTESIAN_POINT('Ctrl Pts',(0.621686174808076,1.85246384581522,
2.01310890201214));
#279567=CARTESIAN_POINT('Ctrl Pts',(0.556815399598003,1.87423445374815,
2.017020776105));
#279568=CARTESIAN_POINT('Ctrl Pts',(0.49069861913138,1.89262734494918,2.02093265019786));
#279569=CARTESIAN_POINT('Ctrl Pts',(0.423720670561041,1.90750538487819,
2.02484452429072));
#279570=CARTESIAN_POINT('Ctrl Pts',(0.356821631821588,1.9223658962976,2.0287517896231));
#279571=CARTESIAN_POINT('Ctrl Pts',(0.289063917933306,1.9337196743245,2.03265905495547));
#279572=CARTESIAN_POINT('Ctrl Pts',(0.220847253844517,1.94147945919326,
2.03656632028784));
#279573=CARTESIAN_POINT('Ctrl Pts',(0.152673443490873,1.94923436936211,
2.0404711310746));
#279574=CARTESIAN_POINT('Ctrl Pts',(0.0840417425782409,1.9533997095032,
2.04437594186135));
#279575=CARTESIAN_POINT('Ctrl Pts',(0.0153602452684157,1.95393962620786,
2.04828075264811));
#279576=CARTESIAN_POINT('Ctrl Pts',(-0.0533016747448948,1.95447938901212,
2.05218445038926));
#279577=CARTESIAN_POINT('Ctrl Pts',(-0.122012871243881,1.95139577597591,
2.05608814813042));
#279578=CARTESIAN_POINT('Ctrl Pts',(-0.190363797093479,1.94470502255642,
2.05999184587157));
#279579=CARTESIAN_POINT('Ctrl Pts',(-0.258718694160792,1.93801388040131,
2.06389577041922));
#279580=CARTESIAN_POINT('Ctrl Pts',(-0.326712789629498,1.92771523225302,
2.06779969496686));
#279581=CARTESIAN_POINT('Ctrl Pts',(-0.393942028521599,1.91387713246287,
2.0717036195145));
#279582=CARTESIAN_POINT('Ctrl Pts',(-0.461242944243122,1.90002427910515,
2.07561170625316));
#279583=CARTESIAN_POINT('Ctrl Pts',(-0.527776893161754,1.88262454245478,
2.07951979299182));
#279584=CARTESIAN_POINT('Ctrl Pts',(-0.59315137805678,1.86179683174866,
2.08342787973048));
#279585=CARTESIAN_POINT('Ctrl Pts',(-0.658564945011555,1.8409566698571,
2.08733830279468));
#279586=CARTESIAN_POINT('Ctrl Pts',(-0.72281720814349,1.81668462930955,
2.09124872585889));
#279587=CARTESIAN_POINT('Ctrl Pts',(-0.785534829123767,1.78914813032166,
2.0951591489231));
#279588=CARTESIAN_POINT('Ctrl Pts',(-0.84836104363242,1.76156395277809,
2.09907634275812));
#279589=CARTESIAN_POINT('Ctrl Pts',(-0.909646873401562,1.73070425670226,
2.10299353659315));
#279590=CARTESIAN_POINT('Ctrl Pts',(-0.969043566553686,1.69678241566823,
2.10691073042818));
#279591=CARTESIAN_POINT('Ctrl Pts',(-0.997505898385083,1.68052739127875,
2.10878781254948));
#279592=CARTESIAN_POINT('Ctrl Pts',(-1.02553487068763,1.66356986657697,
2.11066489467079));
#279593=CARTESIAN_POINT('Ctrl Pts',(-1.05309468069113,1.64593669182629,
2.11254197679209));
#279594=CARTESIAN_POINT('Ctrl Pts',(-1.11061657059442,1.6091333344546,2.11645975819579));
#279595=CARTESIAN_POINT('Ctrl Pts',(-1.166321110383,1.56923783920942,2.12037753959948));
#279596=CARTESIAN_POINT('Ctrl Pts',(-1.21985623987019,1.52645561810678,
2.12429532100318));
#279597=CARTESIAN_POINT('Ctrl Pts',(-1.27331064405205,1.48373790806248,
2.12820719480745));
#279598=CARTESIAN_POINT('Ctrl Pts',(-1.32460174890658,1.43814241566986,
2.13211906861172));
#279599=CARTESIAN_POINT('Ctrl Pts',(-1.37340573420718,1.38991823113694,
2.13603094241599));
#279600=CARTESIAN_POINT('Ctrl Pts',(-1.42215222112183,1.34175086189805,
2.1399382074485));
#279601=CARTESIAN_POINT('Ctrl Pts',(-1.4684170595732,1.29096129530906,2.143845472481));
#279602=CARTESIAN_POINT('Ctrl Pts',(-1.51191027484992,1.2378381642215,2.1477527375135));
#279603=CARTESIAN_POINT('Ctrl Pts',(-1.55537616759355,1.18474840520122,
2.15165754799355));
#279604=CARTESIAN_POINT('Ctrl Pts',(-1.59607358003439,1.12932836944604,
2.1555623584736));
#279605=CARTESIAN_POINT('Ctrl Pts',(-1.63375120303759,1.07190158436921,
2.15946716895365));
#279606=CARTESIAN_POINT('Ctrl Pts',(-1.67141808617182,1.01449116858795,
2.16337086638172));
#279607=CARTESIAN_POINT('Ctrl Pts',(-1.70606661888143,0.955075550173974,
2.16727456380979));
#279608=CARTESIAN_POINT('Ctrl Pts',(-1.73748847963734,0.894007708651057,
2.17117826123786));
#279609=CARTESIAN_POINT('Ctrl Pts',(-1.76891216596912,0.832936319153111,
2.1750821854665));
#279610=CARTESIAN_POINT('Ctrl Pts',(-1.79710858533814,0.770212954604344,
2.17898610969513));
#279611=CARTESIAN_POINT('Ctrl Pts',(-1.82191594105054,0.706214063684601,
2.18289003392377));
#279612=CARTESIAN_POINT('Ctrl Pts',(-1.8467497452228,0.64214694009562,2.18679812033657));
#279613=CARTESIAN_POINT('Ctrl Pts',(-1.86818709655051,0.576802035764591,
2.19070620674938));
#279614=CARTESIAN_POINT('Ctrl Pts',(-1.88611520045465,0.510573648569824,
2.19461429316218));
#279615=CARTESIAN_POINT('Ctrl Pts',(-1.90405402208717,0.444305668907904,
2.19852471589616));
#279616=CARTESIAN_POINT('Ctrl Pts',(-1.91847931777625,0.377153636328863,
2.20243513863013));
#279617=CARTESIAN_POINT('Ctrl Pts',(-1.92932944490711,0.30952203962631,
2.2063455613641));
#279618=CARTESIAN_POINT('Ctrl Pts',(-1.94019835867385,0.241773341053369,
2.21026275486556));
#279619=CARTESIAN_POINT('Ctrl Pts',(-1.94747969671305,0.173543910054779,
2.21417994836703));
#279620=CARTESIAN_POINT('Ctrl Pts',(-1.95116376058966,0.105242478883757,
2.21809714186849));
#279621=CARTESIAN_POINT('Ctrl Pts',(-1.95292913182754,0.0725130295219804,
2.21997422678674));
#279622=CARTESIAN_POINT('Ctrl Pts',(-1.95386925313585,0.0397670322126749,
2.221851311705));
#279623=CARTESIAN_POINT('Ctrl Pts',(-1.95398728496305,0.00704912780047304,
2.22372839662325));
#279624=CARTESIAN_POINT('Ctrl Pts',(-1.95399570907482,0.0047140009923209,
2.22386236704075));
#279625=CARTESIAN_POINT('Ctrl Pts',(-1.95399994727307,0.00237885907428622,
2.22399633745825));
#279626=CARTESIAN_POINT('Ctrl Pts',(-1.95399999951108,4.37116182806309E-5,
2.22413030787575));
#279627=CARTESIAN_POINT('',(-1.95399927934589,0.00167818823651517,2.92413028797392));
#279628=CARTESIAN_POINT('Ctrl Pts',(-1.9539999995111,4.3710859498061E-5,
2.22413030791928));
#279629=CARTESIAN_POINT('Ctrl Pts',(-1.95400152612208,-0.0682001511849845,
2.22804554619099));
#279630=CARTESIAN_POINT('Ctrl Pts',(-1.95042359878162,-0.136580523234795,
2.2319607844627));
#279631=CARTESIAN_POINT('Ctrl Pts',(-1.94324927802393,-0.204690604228606,
2.23587602273441));
#279632=CARTESIAN_POINT('Ctrl Pts',(-1.93608577702256,-0.272697966860162,
2.23978535634624));
#279633=CARTESIAN_POINT('Ctrl Pts',(-1.92533669762871,-0.340435361385916,
2.24369468995806));
#279634=CARTESIAN_POINT('Ctrl Pts',(-1.91103711244139,-0.407496202278842,
2.24760402356988));
#279635=CARTESIAN_POINT('Ctrl Pts',(-1.89675434668933,-0.474478164976527,
2.25150875895156));
#279636=CARTESIAN_POINT('Ctrl Pts',(-1.87892947097966,-0.540784674814253,
2.25541349433325));
#279637=CARTESIAN_POINT('Ctrl Pts',(-1.85764911067538,-0.606016321238107,
2.25931822971493));
#279638=CARTESIAN_POINT('Ctrl Pts',(-1.83638206857691,-0.671207142766151,
2.26322052133773));
#279639=CARTESIAN_POINT('Ctrl Pts',(-1.81166398405568,-0.735323967876062,
2.26712281296053));
#279640=CARTESIAN_POINT('Ctrl Pts',(-1.78363171766969,-0.797981137447913,
2.27102510458334));
#279641=CARTESIAN_POINT('Ctrl Pts',(-1.7556073414111,-0.860620671162447,
2.27492629784407));
#279642=CARTESIAN_POINT('Ctrl Pts',(-1.72427083618383,-0.92180091536956,
2.27882749110481));
#279643=CARTESIAN_POINT('Ctrl Pts',(-1.689807040121,-0.981156545693654,
2.28272868436555));
#279644=CARTESIAN_POINT('Ctrl Pts',(-1.65534107616103,-1.0405159097011,
2.28663012302542));
#279645=CARTESIAN_POINT('Ctrl Pts',(-1.61774768050431,-1.09805000720077,
2.29053156168529));
#279646=CARTESIAN_POINT('Ctrl Pts',(-1.57725653045632,-1.15342006100679,
2.29443300034516));
#279647=CARTESIAN_POINT('Ctrl Pts',(-1.53672212888753,-1.20884925956495,
2.29833860641334));
#279648=CARTESIAN_POINT('Ctrl Pts',(-1.49328408741571,-1.26210940305978,
2.30224421248153));
#279649=CARTESIAN_POINT('Ctrl Pts',(-1.44721351258141,-1.31289338828474,
2.30614981854971));
#279650=CARTESIAN_POINT('Ctrl Pts',(-1.40111509400187,-1.36370806590612,
2.31005778505514));
#279651=CARTESIAN_POINT('Ctrl Pts',(-1.35238132578439,-1.4120432602486,
2.31396575156056));
#279652=CARTESIAN_POINT('Ctrl Pts',(-1.30131944495118,-1.45762948042085,
2.31787371806598));
#279653=CARTESIAN_POINT('Ctrl Pts',(-1.25016960736101,-1.50329422523855,
2.32178841624784));
#279654=CARTESIAN_POINT('Ctrl Pts',(-1.1966840380014,-1.54620023786575,
2.3257031144297));
#279655=CARTESIAN_POINT('Ctrl Pts',(-1.1412014931318,-1.58611952641463,
2.32961781261156));
#279656=CARTESIAN_POINT('Ctrl Pts',(-1.11617689440725,-1.60412454366199,
2.33138348055918));
#279657=CARTESIAN_POINT('Ctrl Pts',(-1.09074641105524,-1.62152256671591,
2.3331491485068));
#279658=CARTESIAN_POINT('Ctrl Pts',(-1.06494276013452,-1.63829573570741,
2.33491481645442));
#279659=CARTESIAN_POINT('Ctrl Pts',(-1.00768790033717,-1.67551316055615,
2.33883259813192));
#279660=CARTESIAN_POINT('Ctrl Pts',(-0.948365952049804,-1.70979950585628,
2.34275037980941));
#279661=CARTESIAN_POINT('Ctrl Pts',(-0.887309266746829,-1.74091879912453,
2.34666816148691));
#279662=CARTESIAN_POINT('Ctrl Pts',(-0.826344648363723,-1.77199116784283,
2.35058003557067));
#279663=CARTESIAN_POINT('Ctrl Pts',(-0.76365091914729,-1.79990574067459,
2.35449190965443));
#279664=CARTESIAN_POINT('Ctrl Pts',(-0.699588569647908,-1.82447028839003,
2.35840378373819));
#279665=CARTESIAN_POINT('Ctrl Pts',(-0.635601695046089,-1.84900589544474,
2.36231104905723));
#279666=CARTESIAN_POINT('Ctrl Pts',(-0.570249859649652,-1.87019914048092,
2.36621831437628));
#279667=CARTESIAN_POINT('Ctrl Pts',(-0.503915613413959,-1.88790493790276,
2.37012557969532));
#279668=CARTESIAN_POINT('Ctrl Pts',(-0.437623038422356,-1.90559961252382,
2.37403039046614));
#279669=CARTESIAN_POINT('Ctrl Pts',(-0.370349751079686,-1.9198110587845,
2.37793520123695));
#279670=CARTESIAN_POINT('Ctrl Pts',(-0.302494138213879,-1.93044380812969,
2.38184001200777));
#279671=CARTESIAN_POINT('Ctrl Pts',(-0.234657867275876,-1.94107352665898,
2.38574370973038));
#279672=CARTESIAN_POINT('Ctrl Pts',(-0.166240086147915,-1.94812649717215,
2.38964740745299));
#279673=CARTESIAN_POINT('Ctrl Pts',(-0.0976482778165805,-1.95155856018708,
2.3935511051756));
#279674=CARTESIAN_POINT('Ctrl Pts',(-0.0290524843175811,-1.95499082260404,
2.39745502970211));
#279675=CARTESIAN_POINT('Ctrl Pts',(0.0397168649642915,-1.95480173782241,
2.40135895422863));
#279676=CARTESIAN_POINT('Ctrl Pts',(0.10825010022352,-1.95099920958508,
2.40526287875514));
#279677=CARTESIAN_POINT('Ctrl Pts',(0.176856402509035,-1.94719262726465,
2.40917096546888));
#279678=CARTESIAN_POINT('Ctrl Pts',(0.245225596207588,-1.93976494033833,
2.41307905218261));
#279679=CARTESIAN_POINT('Ctrl Pts',(0.312951966113218,-1.92877605410941,
2.41698713889635));
#279680=CARTESIAN_POINT('Ctrl Pts',(0.380718824040376,-1.91778059852999,
2.42089756193343));
#279681=CARTESIAN_POINT('Ctrl Pts',(0.447841612492412,-1.90321981097262,
2.42480798497051));
#279682=CARTESIAN_POINT('Ctrl Pts',(0.513926434020998,-1.88520439751621,
2.42871840800759));
#279683=CARTESIAN_POINT('Ctrl Pts',(0.580125679224455,-1.8671577909694,
2.43263560181235));
#279684=CARTESIAN_POINT('Ctrl Pts',(0.645282903573845,-1.84564477427755,
2.43655279561712));
#279685=CARTESIAN_POINT('Ctrl Pts',(0.709021772010433,-1.82082512252418,
2.44046998942189));
#279686=CARTESIAN_POINT('Ctrl Pts',(0.739564835988387,-1.80893177973338,
2.44234707170978));
#279687=CARTESIAN_POINT('Ctrl Pts',(0.769782543884459,-1.79627985217198,
2.44422415399768));
#279688=CARTESIAN_POINT('Ctrl Pts',(0.799635534081065,-1.78289063395232,
2.44610123628558));
#279689=CARTESIAN_POINT('Ctrl Pts',(0.86194366948292,-1.75494511773228,
2.45001901794111));
#279690=CARTESIAN_POINT('Ctrl Pts',(0.922908864854092,-1.7236738544009,
2.45393679959663));
#279691=CARTESIAN_POINT('Ctrl Pts',(0.982152683406715,-1.68922825765999,
2.45785458125216));
#279692=CARTESIAN_POINT('Ctrl Pts',(1.0413071686328,-1.65483460118586,2.46176645531299));
#279693=CARTESIAN_POINT('Ctrl Pts',(1.0987450065672,-1.61727635613494,2.46567832937382));
#279694=CARTESIAN_POINT('Ctrl Pts',(1.15410927115323,-1.57675229197175,
2.46959020343466));
#279695=CARTESIAN_POINT('Ctrl Pts',(1.20940830844943,-1.53627597114802,
2.47349746872944));
#279696=CARTESIAN_POINT('Ctrl Pts',(1.26263822904503,-1.49284105985327,
2.47740473402422));
#279697=CARTESIAN_POINT('Ctrl Pts',(1.31346977031877,-1.44669041693749,
2.481311999319));
#279698=CARTESIAN_POINT('Ctrl Pts',(1.36426937915338,-1.40056876591451,
2.48521681006474));
#279699=CARTESIAN_POINT('Ctrl Pts',(1.41267323395259,-1.35173509741243,
2.48912162081047));
#279700=CARTESIAN_POINT('Ctrl Pts',(1.45838518664059,-1.30047247083023,
2.4930264315562));
#279701=CARTESIAN_POINT('Ctrl Pts',(1.50408410933938,-1.24922445643221,
2.49693012925297));
#279702=CARTESIAN_POINT('Ctrl Pts',(1.54709232587545,-1.19554922541606,
2.50083382694973));
#279703=CARTESIAN_POINT('Ctrl Pts',(1.58715187801053,-1.13976528992931,
2.50473752464649));
#279704=CARTESIAN_POINT('Ctrl Pts',(1.62721375758841,-1.08397811341984,
2.50864144914641));
#279705=CARTESIAN_POINT('Ctrl Pts',(1.66432634774585,-1.02608239031074,
2.51254537364634));
#279706=CARTESIAN_POINT('Ctrl Pts',(1.69827425857821,-0.966426687675084,
2.51644929814626));
#279707=CARTESIAN_POINT('Ctrl Pts',(1.73225836312498,-0.906707382849745,
2.52035738483246));
#279708=CARTESIAN_POINT('Ctrl Pts',(1.76307081094299,-0.845224782145801,
2.52426547151866));
#279709=CARTESIAN_POINT('Ctrl Pts',(1.79054205715451,-0.782352312938932,
2.52817355820485));
#279710=CARTESIAN_POINT('Ctrl Pts',(1.8180297261589,-0.719442257467103,
2.53208398121382));
#279711=CARTESIAN_POINT('Ctrl Pts',(1.8421720453558,-0.6551411405343,2.53599440422279));
#279712=CARTESIAN_POINT('Ctrl Pts',(1.86284856742513,-0.589839990880701,
2.53990482723176));
#279713=CARTESIAN_POINT('Ctrl Pts',(1.88356089020309,-0.524425774463525,
2.5438220210078));
#279714=CARTESIAN_POINT('Ctrl Pts',(1.9007953153205,-0.458008545412891,
2.54773921478384));
#279715=CARTESIAN_POINT('Ctrl Pts',(1.91448215111361,-0.390991167505634,
2.55165640855989));
#279716=CARTESIAN_POINT('Ctrl Pts',(1.92104075445974,-0.358877068554237,
2.55353349107884));
#279717=CARTESIAN_POINT('Ctrl Pts',(1.92678551273033,-0.326625259875533,
2.55541057359779));
#279718=CARTESIAN_POINT('Ctrl Pts',(1.93171298819275,-0.294280361640803,
2.55728765611674));
#279719=CARTESIAN_POINT('Ctrl Pts',(1.94199744457105,-0.226771208628695,
2.56120543783516));
#279720=CARTESIAN_POINT('Ctrl Pts',(1.94875912359902,-0.158588169546824,
2.56512321955358));
#279721=CARTESIAN_POINT('Ctrl Pts',(1.95192016769347,-0.0901313427808721,
2.569041001272));
#279722=CARTESIAN_POINT('Ctrl Pts',(1.95507644527331,-0.0217777415491875,
2.57295287539683));
#279723=CARTESIAN_POINT('Ctrl Pts',(1.95464284070292,0.0468483405377008,
2.57686474952166));
#279724=CARTESIAN_POINT('Ctrl Pts',(1.95059295217582,0.115339216756569,
2.58077662364648));
#279725=CARTESIAN_POINT('Ctrl Pts',(1.94654783501475,0.183749400621046,
2.58468388900661));
#279726=CARTESIAN_POINT('Ctrl Pts',(1.93889492419678,0.252024206184032,
2.58859115436673));
#279727=CARTESIAN_POINT('Ctrl Pts',(1.9276598632852,0.319755299376386,2.59249841972685));
#279728=CARTESIAN_POINT('Ctrl Pts',(1.91643186025083,0.387443843824019,
2.59640323053872));
#279729=CARTESIAN_POINT('Ctrl Pts',(1.90162625130672,0.454588869187506,
2.60030804135058));
#279730=CARTESIAN_POINT('Ctrl Pts',(1.88332041162024,0.520788082788541,
2.60421285216245));
#279731=CARTESIAN_POINT('Ctrl Pts',(1.86501978992884,0.5869684266094,2.60811654992603));
#279732=CARTESIAN_POINT('Ctrl Pts',(1.84322104918359,0.652203019899014,
2.61202024768961));
#279733=CARTESIAN_POINT('Ctrl Pts',(1.81805205683821,0.716102449811733,
2.61592394545318));
#279734=CARTESIAN_POINT('Ctrl Pts',(1.79288160218125,0.780005592263864,
2.61982787002053));
#279735=CARTESIAN_POINT('Ctrl Pts',(1.76434068984971,0.842572960514409,
2.62373179458788));
#279736=CARTESIAN_POINT('Ctrl Pts',(1.73260551634365,0.903434626708295,
2.62763571915523));
#279737=CARTESIAN_POINT('Ctrl Pts',(1.70083650823985,0.964361180840896,
2.63154380590929));
#279738=CARTESIAN_POINT('Ctrl Pts',(1.66586667032203,1.02357796654965,2.63545189266335));
#279739=CARTESIAN_POINT('Ctrl Pts',(1.62791793851127,1.08074011005108,2.6393599794174));
#279740=CARTESIAN_POINT('Ctrl Pts',(1.58994652028003,1.13793642608901,2.64327040249458));
#279741=CARTESIAN_POINT('Ctrl Pts',(1.54899295736738,1.19307526035967,2.64718082557175));
#279742=CARTESIAN_POINT('Ctrl Pts',(1.50532058755956,1.24584346074028,2.65109124864892));
#279743=CARTESIAN_POINT('Ctrl Pts',(1.4615726005026,1.29870302749678,2.655008442493));
#279744=CARTESIAN_POINT('Ctrl Pts',(1.41509674402807,1.34918340621439,2.65892563633708));
#279745=CARTESIAN_POINT('Ctrl Pts',(1.36619381046245,1.39700768510917,2.66284283018116));
#279746=CARTESIAN_POINT('Ctrl Pts',(1.34275999120437,1.41992462333875,2.66471991210341));
#279747=CARTESIAN_POINT('Ctrl Pts',(1.31876935571298,1.44223224835895,2.66659699402565));
#279748=CARTESIAN_POINT('Ctrl Pts',(1.29425753923292,1.4639034879864,2.6684740759479));
#279749=CARTESIAN_POINT('Ctrl Pts',(1.24309730769296,1.50913496391558,2.67239185763658));
#279750=CARTESIAN_POINT('Ctrl Pts',(1.18946147848789,1.55177115595393,2.67630963932525));
#279751=CARTESIAN_POINT('Ctrl Pts',(1.13364409416159,1.59152978852818,2.68022742101392));
#279752=CARTESIAN_POINT('Ctrl Pts',(1.07791087645525,1.63122846935516,2.68413929510864));
#279753=CARTESIAN_POINT('Ctrl Pts',(1.02000302965254,1.66805791900372,2.68805116920335));
#279754=CARTESIAN_POINT('Ctrl Pts',(0.960248861394475,1.70177499223329,
2.69196304329807));
#279755=CARTESIAN_POINT('Ctrl Pts',(0.900565092366708,1.73545234177374,
2.69587030862768));
#279756=CARTESIAN_POINT('Ctrl Pts',(0.839039748354085,1.76602435662461,
2.69977757395729));
#279757=CARTESIAN_POINT('Ctrl Pts',(0.77602988848427,1.79329127923466,2.70368483928691));
#279758=CARTESIAN_POINT('Ctrl Pts',(0.713059611479431,1.82054107273321,
2.70758965006804));
#279759=CARTESIAN_POINT('Ctrl Pts',(0.648607119030157,1.84448969764631,
2.71149446084917));
#279760=CARTESIAN_POINT('Ctrl Pts',(0.583052430532476,1.86498414557609,
2.7153992716303));
#279761=CARTESIAN_POINT('Ctrl Pts',(0.517516428098966,1.88547275165721,
2.71930296936297));
#279762=CARTESIAN_POINT('Ctrl Pts',(0.450879322648276,1.9025089885884,2.72320666709565));
#279763=CARTESIAN_POINT('Ctrl Pts',(0.383537675186315,1.91598926189911,
2.72711036482832));
#279764=CARTESIAN_POINT('Ctrl Pts',(0.316192115195746,1.92947031840946,
2.73101428936461));
#279765=CARTESIAN_POINT('Ctrl Pts',(0.248142414838569,1.93939490706247,
2.7349182139009));
#279766=CARTESIAN_POINT('Ctrl Pts',(0.17979495337632,1.94571060919665,2.73882213843719));
#279767=CARTESIAN_POINT('Ctrl Pts',(0.111374622960162,1.95203304484511,
2.74273022516021));
#279768=CARTESIAN_POINT('Ctrl Pts',(0.0426563887231679,1.95473886985672,
2.74663831188322));
#279769=CARTESIAN_POINT('Ctrl Pts',(-0.0259496355521265,1.95382768339859,
2.75054639860624));
#279770=CARTESIAN_POINT('Ctrl Pts',(-0.0945966737171027,1.95291595221715,
2.75445682165234));
#279771=CARTESIAN_POINT('Ctrl Pts',(-0.163130877432424,1.94838293864801,
2.75836724469843));
#279772=CARTESIAN_POINT('Ctrl Pts',(-0.231146352647582,1.94028022812627,
2.76227766774453));
#279773=CARTESIAN_POINT('Ctrl Pts',(-0.299279594391147,1.93216348803131,
2.7661948615578));
#279774=CARTESIAN_POINT('Ctrl Pts',(-0.36689183048276,1.9204647987446,2.77011205537106));
#279775=CARTESIAN_POINT('Ctrl Pts',(-0.433587323431622,1.90528686369255,
2.77402924918433));
#279776=CARTESIAN_POINT('Ctrl Pts',(-0.465547172365731,1.89801374087798,
2.77590633138258));
#279777=CARTESIAN_POINT('Ctrl Pts',(-0.497296741324567,1.88994243911198,
2.77778341358082));
#279778=CARTESIAN_POINT('Ctrl Pts',(-0.528793965500402,1.881088233457,2.77966049577907));
#279779=CARTESIAN_POINT('Ctrl Pts',(-0.594533893257536,1.86260803860376,
2.78357827746733));
#279780=CARTESIAN_POINT('Ctrl Pts',(-0.659434484196362,1.84064078252868,
2.78749605915558));
#279781=CARTESIAN_POINT('Ctrl Pts',(-0.723099151368537,1.81528058913494,
2.79141384084384));
#279782=CARTESIAN_POINT('Ctrl Pts',(-0.786667819059477,1.78995863618945,
2.79532571493803));
#279783=CARTESIAN_POINT('Ctrl Pts',(-0.849003808257224,1.76125408025483,
2.79923758903223));
#279784=CARTESIAN_POINT('Ctrl Pts',(-0.909724845911147,1.72931104915569,
2.80314946312642));
#279785=CARTESIAN_POINT('Ctrl Pts',(-0.970374345217748,1.6974056516633,
2.80705672845538));
#279786=CARTESIAN_POINT('Ctrl Pts',(-1.02941223831299,1.66226958436928,
2.81096399378433));
#279787=CARTESIAN_POINT('Ctrl Pts',(-1.08647713215179,1.62409465281775,
2.81487125911329));
#279788=CARTESIAN_POINT('Ctrl Pts',(-1.14350617775877,1.58594370280205,
2.81877606989368));
#279789=CARTESIAN_POINT('Ctrl Pts',(-1.198564274746,1.54475794831463,2.82268088067407));
#279790=CARTESIAN_POINT('Ctrl Pts',(-1.25131687373763,1.50077382756346,
2.82658569145446));
#279791=CARTESIAN_POINT('Ctrl Pts',(-1.30405443584069,1.456802244286,2.83048938918629));
#279792=CARTESIAN_POINT('Ctrl Pts',(-1.35448742683864,1.41003419312665,
2.83439308691811));
#279793=CARTESIAN_POINT('Ctrl Pts',(-1.40231385925453,1.36074679501465,
2.83829678464993));
#279794=CARTESIAN_POINT('Ctrl Pts',(-1.45014307037028,1.31145653332119,
2.8422007091853));
#279795=CARTESIAN_POINT('Ctrl Pts',(-1.49536508146451,1.25964698892887,
2.84610463372067));
#279796=CARTESIAN_POINT('Ctrl Pts',(-1.53771559154354,1.20563127013358,
2.85000855825604));
#279797=CARTESIAN_POINT('Ctrl Pts',(-1.58011125380827,1.15155796223815,
2.85391664497801));
#279798=CARTESIAN_POINT('Ctrl Pts',(-1.61962900111618,1.09527417369821,
2.85782473169997));
#279799=CARTESIAN_POINT('Ctrl Pts',(-1.65604622383594,1.03712434380779,
2.86173281842194));
#279800=CARTESIAN_POINT('Ctrl Pts',(-1.69248521741219,0.978939750925921,
2.86564324146691));
#279801=CARTESIAN_POINT('Ctrl Pts',(-1.72581975869414,0.918887326763719,
2.86955366451188));
#279802=CARTESIAN_POINT('Ctrl Pts',(-1.75587321392212,0.857336139813785,
2.87346408755686));
#279803=CARTESIAN_POINT('Ctrl Pts',(-1.78597870570537,0.795678379036743,
2.8773812813689));
#279804=CARTESIAN_POINT('Ctrl Pts',(-1.81279158057834,0.732517128725427,
2.88129847518093));
#279805=CARTESIAN_POINT('Ctrl Pts',(-1.83618366859166,0.668240626718617,
2.88521566899297));
#279806=CARTESIAN_POINT('Ctrl Pts',(-1.84739293580489,0.637439935214873,
2.88709275119873));
#279807=CARTESIAN_POINT('Ctrl Pts',(-1.85781745224111,0.606383365739943,
2.88896983340448));
#279808=CARTESIAN_POINT('Ctrl Pts',(-1.86744725673438,0.575114547994793,
2.89084691561023));
#279809=CARTESIAN_POINT('Ctrl Pts',(-1.89195310352142,0.495541919348942,
2.89562369887442));
#279810=CARTESIAN_POINT('Ctrl Pts',(-1.91138829262048,0.41433886039205,
2.90040048213861));
#279811=CARTESIAN_POINT('Ctrl Pts',(-1.92557302732791,0.33209112669148,
2.9051772654028));
#279812=CARTESIAN_POINT('Ctrl Pts',(-1.93956135918817,0.250982200970493,
2.90988790898565));
#279813=CARTESIAN_POINT('Ctrl Pts',(-1.94844357914405,0.168857321384975,
2.9145985525685));
#279814=CARTESIAN_POINT('Ctrl Pts',(-1.9520933534157,0.0862991283284693,
2.91930919615135));
#279815=CARTESIAN_POINT('Ctrl Pts',(-1.95333846968525,0.0581344962967553,
2.92091622675888));
#279816=CARTESIAN_POINT('Ctrl Pts',(-1.95397502425442,0.0299196156356976,
2.9225232573664));
#279817=CARTESIAN_POINT('Ctrl Pts',(-1.95399927934589,0.00167818823651517,
2.92413028797392));
#279818=CARTESIAN_POINT('',(-1.95391614919261,-0.000969648952806235,3.62413035429011));
#279819=CARTESIAN_POINT('Ctrl Pts',(-1.95274315056508,0.00167675988910205,
2.92413030787576));
#279820=CARTESIAN_POINT('Ctrl Pts',(-1.94901804708373,-0.45438081105706,
2.95009798373097));
#279821=CARTESIAN_POINT('Ctrl Pts',(-1.562324701513,-1.56703485389375,3.0131277995299));
#279822=CARTESIAN_POINT('Ctrl Pts',(0.291342892527357,-2.29141958423336,
3.11321975527255));
#279823=CARTESIAN_POINT('Ctrl Pts',(2.08359330569799,-0.997057334412019,
3.22440617510372));
#279824=CARTESIAN_POINT('Ctrl Pts',(1.96718185643315,1.21065268979667,3.33559259493487));
#279825=CARTESIAN_POINT('Ctrl Pts',(0.0487464827200954,2.30935232741887,
3.44677901476604));
#279826=CARTESIAN_POINT('Ctrl Pts',(-1.64937842670566,1.42982133530745,
3.54295825241301));
#279827=CARTESIAN_POINT('Ctrl Pts',(-1.94952253842872,0.387114015523011,
3.60207535011624));
#279828=CARTESIAN_POINT('Ctrl Pts',(-1.95125983814034,-0.000967513988672578,
3.62413030787576));
#279829=CARTESIAN_POINT('',(-1.95399963679489,-0.00119138802316145,4.32413030787576));
#279830=CARTESIAN_POINT('Ctrl Pts',(-1.95399975937833,-0.000969716153049057,
3.62413035575105));
#279831=CARTESIAN_POINT('Ctrl Pts',(-1.95396212499893,-0.0768038332389409,
3.62843403175574));
#279832=CARTESIAN_POINT('Ctrl Pts',(-1.94950568155316,-0.152487481613112,
3.63273770776042));
#279833=CARTESIAN_POINT('Ctrl Pts',(-1.94070759056848,-0.227530323055786,
3.63704138376511));
#279834=CARTESIAN_POINT('Ctrl Pts',(-1.93187850028117,-0.30283757137454,
3.64136022339508));
#279835=CARTESIAN_POINT('Ctrl Pts',(-1.91867725116394,-0.3774991953551,
3.64567906302506));
#279836=CARTESIAN_POINT('Ctrl Pts',(-1.90123179448794,-0.451036210994379,
3.64999790265503));
#279837=CARTESIAN_POINT('Ctrl Pts',(-1.88370328269169,-0.524923324988201,
3.65433730361232));
#279838=CARTESIAN_POINT('Ctrl Pts',(-1.86189020038226,-0.597674812201765,
3.6586767045696));
#279839=CARTESIAN_POINT('Ctrl Pts',(-1.8359705771302,-0.668825866659036,
3.66301610552688));
#279840=CARTESIAN_POINT('Ctrl Pts',(-1.82375412133664,-0.70236083369884,
3.66506135516071));
#279841=CARTESIAN_POINT('Ctrl Pts',(-1.81062610442916,-0.735540604450197,
3.66710660479454));
#279842=CARTESIAN_POINT('Ctrl Pts',(-1.79660870731119,-0.768318392864322,
3.66915185442836));
#279843=CARTESIAN_POINT('Ctrl Pts',(-1.76975765651418,-0.831105945668458,
3.67306963612123));
#279844=CARTESIAN_POINT('Ctrl Pts',(-1.73955787060529,-0.892608953619772,
3.67698741781409));
#279845=CARTESIAN_POINT('Ctrl Pts',(-1.706154118717,-0.952446388614617,
3.68090519950696));
#279846=CARTESIAN_POINT('Ctrl Pts',(-1.67280073609843,-1.01219359518505,
3.68481707360586));
#279847=CARTESIAN_POINT('Ctrl Pts',(-1.63625321359155,-1.07027978709881,
3.68872894770477));
#279848=CARTESIAN_POINT('Ctrl Pts',(-1.5967040452091,-1.12634461512137,
3.69264082180368));
#279849=CARTESIAN_POINT('Ctrl Pts',(-1.55720147158485,-1.1823433905008,
3.69654808713747));
#279850=CARTESIAN_POINT('Ctrl Pts',(-1.51470455759503,-1.23632513147622,
3.70045535247126));
#279851=CARTESIAN_POINT('Ctrl Pts',(-1.46945036390749,-1.28795637659516,
3.70436261780505));
#279852=CARTESIAN_POINT('Ctrl Pts',(-1.4242245989555,-1.33955518690765,
3.70826742859035));
#279853=CARTESIAN_POINT('Ctrl Pts',(-1.37624531381229,-1.38880606126236,
3.71217223937565));
#279854=CARTESIAN_POINT('Ctrl Pts',(-1.32579034293607,-1.43540794430624,
3.71607705016094));
#279855=CARTESIAN_POINT('Ctrl Pts',(-1.27534975401894,-1.48199654369612,
3.71998074789776));
#279856=CARTESIAN_POINT('Ctrl Pts',(-1.22243524148878,-1.5259373170701,
3.72388444563457));
#279857=CARTESIAN_POINT('Ctrl Pts',(-1.16736075532149,-1.56696677276043,
3.72778814337138));
#279858=CARTESIAN_POINT('Ctrl Pts',(-1.11228306934399,-1.60799861224915,
3.73169206791179));
#279859=CARTESIAN_POINT('Ctrl Pts',(-1.0550455566399,-1.64611850636757,
3.7355959924522));
#279860=CARTESIAN_POINT('Ctrl Pts',(-0.995992962315415,-1.68110499940312,
3.73949991699262));
#279861=CARTESIAN_POINT('Ctrl Pts',(-0.936877408802782,-1.71612879344506,
3.74340800371968));
#279862=CARTESIAN_POINT('Ctrl Pts',(-0.87594333574339,-1.74801226809313,
3.74731609044674));
#279863=CARTESIAN_POINT('Ctrl Pts',(-0.813561146877509,-1.77657937067032,
3.75122417717381));
#279864=CARTESIAN_POINT('Ctrl Pts',(-0.751141664840921,-1.80516355116434,
3.75513460022391));
#279865=CARTESIAN_POINT('Ctrl Pts',(-0.687272801642316,-1.83042723289383,
3.75904502327402));
#279866=CARTESIAN_POINT('Ctrl Pts',(-0.622343418737791,-1.8522431452576,
3.76295544632413));
#279867=CARTESIAN_POINT('Ctrl Pts',(-0.557301612772591,-1.87409683114592,
3.76687264014131));
#279868=CARTESIAN_POINT('Ctrl Pts',(-0.491196095925404,-1.89249070112647,
3.77078983395849));
#279869=CARTESIAN_POINT('Ctrl Pts',(-0.424428450934365,-1.90734802541053,
3.77470702777567));
#279870=CARTESIAN_POINT('Ctrl Pts',(-0.392434028086504,-1.91446751443243,
3.77658410993696));
#279871=CARTESIAN_POINT('Ctrl Pts',(-0.360287677037997,-1.92077569274014,
3.77846119209824));
#279872=CARTESIAN_POINT('Ctrl Pts',(-0.328033950954508,-1.92626834242303,
3.78033827425953));
#279873=CARTESIAN_POINT('Ctrl Pts',(-0.260715076915098,-1.93773241299857,
3.78425605595242));
#279874=CARTESIAN_POINT('Ctrl Pts',(-0.192660782914911,-1.94568603633619,
3.78817383764531));
#279875=CARTESIAN_POINT('Ctrl Pts',(-0.124269743834863,-1.95004436635868,
3.7920916193382));
#279876=CARTESIAN_POINT('Ctrl Pts',(-0.0559818310953371,-1.95439612448765,
3.79600349343714));
#279877=CARTESIAN_POINT('Ctrl Pts',(0.0126413319566921,-1.9551633175741,
3.79991536753607));
#279878=CARTESIAN_POINT('Ctrl Pts',(0.0811925829564603,-1.95231241466955,
3.80382724163501));
#279879=CARTESIAN_POINT('Ctrl Pts',(0.149663070463653,-1.94946487054945,
3.80773450696882));
#279880=CARTESIAN_POINT('Ctrl Pts',(0.218061324959097,-1.94300771642214,
3.81164177230263));
#279881=CARTESIAN_POINT('Ctrl Pts',(0.285978626207468,-1.93295944741541,
3.81554903763644));
#279882=CARTESIAN_POINT('Ctrl Pts',(0.353853261730547,-1.92291749074261,
3.81945384842176));
#279883=CARTESIAN_POINT('Ctrl Pts',(0.421247057755176,-1.90928896606093,
3.82335865920708));
#279884=CARTESIAN_POINT('Ctrl Pts',(0.487756429378236,-1.89214419788773,
3.8272634699924));
#279885=CARTESIAN_POINT('Ctrl Pts',(0.554246842808509,-1.87500431675243,
3.83116716772923));
#279886=CARTESIAN_POINT('Ctrl Pts',(0.619852856111499,-1.85435030456257,
3.83507086546606));
#279887=CARTESIAN_POINT('Ctrl Pts',(0.684182878795401,-1.83030319574743,
3.83897456320289));
#279888=CARTESIAN_POINT('Ctrl Pts',(0.748516639033264,-1.80625468980287,
3.84287848774333));
#279889=CARTESIAN_POINT('Ctrl Pts',(0.811573801526584,-1.778812870503,3.84678241228376));
#279890=CARTESIAN_POINT('Ctrl Pts',(0.87298141219139,-1.74814743484877,
3.85068633682419));
#279891=CARTESIAN_POINT('Ctrl Pts',(0.934454492855615,-1.71744930510283,
3.85459442355128));
#279892=CARTESIAN_POINT('Ctrl Pts',(0.994274070876336,-1.6835209202206,
3.85850251027836));
#279893=CARTESIAN_POINT('Ctrl Pts',(1.05209144211596,-1.64657814798641,
3.86241059700544));
#279894=CARTESIAN_POINT('Ctrl Pts',(1.10994337759795,-1.60961329071263,
3.86632102005557));
#279895=CARTESIAN_POINT('Ctrl Pts',(1.1657903240518,-1.5696307461132,3.8702314431057));
#279896=CARTESIAN_POINT('Ctrl Pts',(1.21931456974782,-1.52688833252491,
3.87414186615583));
#279897=CARTESIAN_POINT('Ctrl Pts',(1.27293149088987,-1.48407191187323,
3.87805905997304));
#279898=CARTESIAN_POINT('Ctrl Pts',(1.324217316999,-1.43848641142785,3.88197625379024));
#279899=CARTESIAN_POINT('Ctrl Pts',(1.3728899158051,-1.39042773241929,3.88589344760744));
#279900=CARTESIAN_POINT('Ctrl Pts',(1.39621336397132,-1.36739846880307,
3.88777052976852));
#279901=CARTESIAN_POINT('Ctrl Pts',(1.41893733450694,-1.34380181306207,
3.88964761192961));
#279902=CARTESIAN_POINT('Ctrl Pts',(1.44103413586229,-1.31967292132544,
3.89152469409069));
#279903=CARTESIAN_POINT('Ctrl Pts',(1.48715382397003,-1.26931192366867,
3.8954424757836));
#279904=CARTESIAN_POINT('Ctrl Pts',(1.53072194029792,-1.21643029835566,
3.8993602574765));
#279905=CARTESIAN_POINT('Ctrl Pts',(1.57145110770361,-1.16131710402332,
3.90327803916941));
#279906=CARTESIAN_POINT('Ctrl Pts',(1.61211885989988,-1.1062870144679,3.90718991326836));
#279907=CARTESIAN_POINT('Ctrl Pts',(1.64995586900205,-1.04903242657542,
3.91110178736731));
#279908=CARTESIAN_POINT('Ctrl Pts',(1.68471328268377,-0.989877343486992,
3.91501366146626));
#279909=CARTESIAN_POINT('Ctrl Pts',(1.71942974700163,-0.930791953818331,
3.91892092680009));
#279910=CARTESIAN_POINT('Ctrl Pts',(1.75107357350287,-0.86981093790479,
3.92282819213392));
#279911=CARTESIAN_POINT('Ctrl Pts',(1.77943878785213,-0.807287805114966,
3.92673545746775));
#279912=CARTESIAN_POINT('Ctrl Pts',(1.80778618314172,-0.74480394942772,
3.93064026825309));
#279913=CARTESIAN_POINT('Ctrl Pts',(1.8328588490844,-0.680780345575904,
3.93454507903843));
#279914=CARTESIAN_POINT('Ctrl Pts',(1.85449715161248,-0.615594277638437,
3.93844988982377));
#279915=CARTESIAN_POINT('Ctrl Pts',(1.87612928624121,-0.550426790692054,
3.94235358756062));
#279916=CARTESIAN_POINT('Ctrl Pts',(1.89432884588759,-0.484097964155095,
3.94625728529747));
#279917=CARTESIAN_POINT('Ctrl Pts',(1.90898531342313,-0.417002485765723,
3.95016098303431));
#279918=CARTESIAN_POINT('Ctrl Pts',(1.92364263249479,-0.349903109150335,
3.95406490757476));
#279919=CARTESIAN_POINT('Ctrl Pts',(1.93475634826849,-0.282037473443222,
3.95796883211521));
#279920=CARTESIAN_POINT('Ctrl Pts',(1.94226693980362,-0.213810978543884,
3.96187275665566));
#279921=CARTESIAN_POINT('Ctrl Pts',(1.94978553878959,-0.145511743661093,
3.96578084338277));
#279922=CARTESIAN_POINT('Ctrl Pts',(1.95369329309856,-0.07685137174546,
3.96968893010987));
#279923=CARTESIAN_POINT('Ctrl Pts',(1.95398262631379,-0.00823990678708126,
3.97359701683697));
#279924=CARTESIAN_POINT('Ctrl Pts',(1.95427213249751,0.0604125753129308,
3.97750743988712));
#279925=CARTESIAN_POINT('Ctrl Pts',(1.95093893639689,0.129015600790377,
3.98141786293727));
#279926=CARTESIAN_POINT('Ctrl Pts',(1.94402751373659,0.197162435152151,
3.98532828598742));
#279927=CARTESIAN_POINT('Ctrl Pts',(1.9371041241785,0.265427263484444,3.98924547980464));
#279928=CARTESIAN_POINT('Ctrl Pts',(1.92659021785465,0.333233838271852,
3.99316267362186));
#279929=CARTESIAN_POINT('Ctrl Pts',(1.9125815583624,0.400184685629107,3.99707986743908));
#279930=CARTESIAN_POINT('Ctrl Pts',(1.90586874146888,0.432266897308478,
3.99895694960001));
#279931=CARTESIAN_POINT('Ctrl Pts',(1.89835418863101,0.464152826721439,
4.00083403176094));
#279932=CARTESIAN_POINT('Ctrl Pts',(1.89005243657592,0.495800148238614,
4.00271111392186));
#279933=CARTESIAN_POINT('Ctrl Pts',(1.87272530359401,0.561853355418326,
4.00662889561475));
#279934=CARTESIAN_POINT('Ctrl Pts',(1.85189695753908,0.627128366384856,
4.01054667730764));
#279935=CARTESIAN_POINT('Ctrl Pts',(1.82765456893729,0.691227008039081,
4.01446445900053));
#279936=CARTESIAN_POINT('Ctrl Pts',(1.80344873525345,0.755228995826995,
4.01837633309947));
#279937=CARTESIAN_POINT('Ctrl Pts',(1.77583924855178,0.818057678262382,
4.0222882071984));
#279938=CARTESIAN_POINT('Ctrl Pts',(1.74496352607143,0.879328319048321,
4.02620008129734));
#279939=CARTESIAN_POINT('Ctrl Pts',(1.71412417974974,0.940526773975238,
4.03010734663115));
#279940=CARTESIAN_POINT('Ctrl Pts',(1.68002646034958,1.00017039550476,4.03401461196496));
#279941=CARTESIAN_POINT('Ctrl Pts',(1.64285582086269,1.05789448994575,4.03792187729878));
#279942=CARTESIAN_POINT('Ctrl Pts',(1.60570853201348,1.11558232204545,4.0418266880841));
#279943=CARTESIAN_POINT('Ctrl Pts',(1.56549241812117,1.17135260634642,4.04573149886942));
#279944=CARTESIAN_POINT('Ctrl Pts',(1.52243802768505,1.22486670779251,4.04963630965474));
#279945=CARTESIAN_POINT('Ctrl Pts',(1.47939590970637,1.27836555528828,4.05354000739157));
#279946=CARTESIAN_POINT('Ctrl Pts',(1.43351742949258,1.32960911346225,4.0574437051284));
#279947=CARTESIAN_POINT('Ctrl Pts',(1.38507438176285,1.37829059235862,4.06134740286523));
#279948=CARTESIAN_POINT('Ctrl Pts',(1.3366285195074,1.42697489963347,4.06525132740567));
#279949=CARTESIAN_POINT('Ctrl Pts',(1.28561814275682,1.47309648516515,4.0691552519461));
#279950=CARTESIAN_POINT('Ctrl Pts',(1.23235168747768,1.51638561005139,4.07305917648653));
#279951=CARTESIAN_POINT('Ctrl Pts',(1.1790284419284,1.55972088783222,4.07696726321362));
#279952=CARTESIAN_POINT('Ctrl Pts',(1.12344470004525,1.60021736735284,4.0808753499407));
#279953=CARTESIAN_POINT('Ctrl Pts',(1.06594095345878,1.63764644650162,4.08478343666779));
#279954=CARTESIAN_POINT('Ctrl Pts',(1.00840283012026,1.67509790141285,4.08869385971792));
#279955=CARTESIAN_POINT('Ctrl Pts',(0.948942843700564,1.7094780601652,4.09260428276805));
#279956=CARTESIAN_POINT('Ctrl Pts',(0.887926915685403,1.74060385855065,
4.09651470581818));
#279957=CARTESIAN_POINT('Ctrl Pts',(0.826805340626195,1.77178355021774,
4.10043189963539));
#279958=CARTESIAN_POINT('Ctrl Pts',(0.764122896196409,1.7996974351293,4.10434909345259));
#279959=CARTESIAN_POINT('Ctrl Pts',(0.700265518251073,1.8242105700682,4.10826628726979));
#279960=CARTESIAN_POINT('Ctrl Pts',(0.669665667800006,1.83595703206448,
4.11014336943087));
#279961=CARTESIAN_POINT('Ctrl Pts',(0.638796247998107,1.84692334047467,
4.11202045159194));
#279962=CARTESIAN_POINT('Ctrl Pts',(0.607700707576638,1.85709877228188,
4.11389753375302));
#279963=CARTESIAN_POINT('Ctrl Pts',(0.542799159034894,1.87833658556371,
4.11781531544591));
#279964=CARTESIAN_POINT('Ctrl Pts',(0.476654019198033,1.89621024025539,
4.12173309713881));
#279965=CARTESIAN_POINT('Ctrl Pts',(0.409647154276951,1.91057719262866,
4.1256508788317));
#279966=CARTESIAN_POINT('Ctrl Pts',(0.342741328510495,1.924922481181,4.12956275293064));
#279967=CARTESIAN_POINT('Ctrl Pts',(0.274976833630437,1.93577145929668,
4.13347462702958));
#279968=CARTESIAN_POINT('Ctrl Pts',(0.206751476288704,1.9430310926623,4.13738650112851));
#279969=CARTESIAN_POINT('Ctrl Pts',(0.138606498488652,1.95028217310822,
4.14129376646233));
#279970=CARTESIAN_POINT('Ctrl Pts',(0.0700022234489896,1.9539522553612,
4.14520103179615));
#279971=CARTESIAN_POINT('Ctrl Pts',(0.00134564850247342,1.95399953665043,
4.14910829712997));
#279972=CARTESIAN_POINT('Ctrl Pts',(-0.0672677963061884,1.95404678823751,
4.1530131079153));
#279973=CARTESIAN_POINT('Ctrl Pts',(-0.135932984977147,1.95047575303684,
4.15691791870062));
#279974=CARTESIAN_POINT('Ctrl Pts',(-0.204240378871569,1.94329664941779,
4.16082272948595));
#279975=CARTESIAN_POINT('Ctrl Pts',(-0.272528302055187,1.93611959216945,
4.16472642722279));
#279976=CARTESIAN_POINT('Ctrl Pts',(-0.340458143866954,1.92533655954889,
4.16863012495963));
#279977=CARTESIAN_POINT('Ctrl Pts',(-0.407624773494297,1.91100969229194,
4.17253382269646));
#279978=CARTESIAN_POINT('Ctrl Pts',(-0.474795305481489,1.89668199264854,
4.1764377472369));
#279979=CARTESIAN_POINT('Ctrl Pts',(-0.541202056624897,1.87881015472464,
4.18034167177734));
#279980=CARTESIAN_POINT('Ctrl Pts',(-0.606451174777268,1.85750719315196,
4.18424559631777));
#279981=CARTESIAN_POINT('Ctrl Pts',(-0.671769858569542,1.83618151933128,
4.18815368304486));
#279982=CARTESIAN_POINT('Ctrl Pts',(-0.735927977641656,1.81141757432175,
4.19206176977195));
#279983=CARTESIAN_POINT('Ctrl Pts',(-0.798548877421209,1.78337760734213,
4.19596985649904));
#279984=CARTESIAN_POINT('Ctrl Pts',(-0.861207213077057,1.75532087757662,
4.19988027954918));
#279985=CARTESIAN_POINT('Ctrl Pts',(-0.9223260626507,1.72398445264218,4.20379070259932));
#279986=CARTESIAN_POINT('Ctrl Pts',(-0.981553258851392,1.68957663337246,
4.20770112564945));
#279987=CARTESIAN_POINT('Ctrl Pts',(-1.04088300496669,1.6551092381114,4.21161831946666));
#279988=CARTESIAN_POINT('Ctrl Pts',(-1.09831414899737,1.6175601035556,4.21553551328387));
#279989=CARTESIAN_POINT('Ctrl Pts',(-1.15352411681735,1.57718043099728,
4.21945270710108));
#279990=CARTESIAN_POINT('Ctrl Pts',(-1.17998021027151,1.55783087451258,
4.22132978926211));
#279991=CARTESIAN_POINT('Ctrl Pts',(-1.20592676926254,1.5378319476531,4.22320687142315));
#279992=CARTESIAN_POINT('Ctrl Pts',(-1.23133123397787,1.51721435276316,
4.22508395358418));
#279993=CARTESIAN_POINT('Ctrl Pts',(-1.28366054183447,1.4747452638708,4.22895045545216));
#279994=CARTESIAN_POINT('Ctrl Pts',(-1.33390722678967,1.42947038638983,
4.23281695732014));
#279995=CARTESIAN_POINT('Ctrl Pts',(-1.38174895723329,1.38162434083391,
4.23668345918812));
#279996=CARTESIAN_POINT('Ctrl Pts',(-1.42950834973302,1.33386064064839,
4.24054330661841));
#279997=CARTESIAN_POINT('Ctrl Pts',(-1.47487064950818,1.28353491123766,
4.24440315404871));
#279998=CARTESIAN_POINT('Ctrl Pts',(-1.51754621895637,1.23092220441879,
4.24826300147901));
#279999=CARTESIAN_POINT('Ctrl Pts',(-1.56018088697644,1.17835992305117,
4.2521191495264));
#280000=CARTESIAN_POINT('Ctrl Pts',(-1.60013361002202,1.12351539844574,
4.25597529757378));
#280001=CARTESIAN_POINT('Ctrl Pts',(-1.63715237493145,1.06669963028789,
4.25983144562117));
#280002=CARTESIAN_POINT('Ctrl Pts',(-1.67414915694421,1.00991760110441,
4.26368530376763));
#280003=CARTESIAN_POINT('Ctrl Pts',(-1.70821515935737,0.951167072327578,
4.2675391619141));
#280004=CARTESIAN_POINT('Ctrl Pts',(-1.73914059576239,0.890789530793455,
4.27139302006056));
#280005=CARTESIAN_POINT('Ctrl Pts',(-1.77005894046059,0.830425834814093,
4.27524599445451));
#280006=CARTESIAN_POINT('Ctrl Pts',(-1.79783791881047,0.768436317333705,
4.27909896884846));
#280007=CARTESIAN_POINT('Ctrl Pts',(-1.82231376045984,0.705186896105353,
4.28295194324241));
#280008=CARTESIAN_POINT('Ctrl Pts',(-1.84680713976431,0.641892154820181,
4.286807678405));
#280009=CARTESIAN_POINT('Ctrl Pts',(-1.86799247153181,0.577336179322571,
4.29066341356758));
#280010=CARTESIAN_POINT('Ctrl Pts',(-1.8857547148499,0.511903462990225,
4.29451914873017));
#280011=CARTESIAN_POINT('Ctrl Pts',(-1.90352379915543,0.44644554576498,
4.29837636889864));
#280012=CARTESIAN_POINT('Ctrl Pts',(-1.91786706209594,0.380110710336096,
4.30223358906712));
#280013=CARTESIAN_POINT('Ctrl Pts',(-1.928720466767,0.313294368085472,4.30609080923559));
#280014=CARTESIAN_POINT('Ctrl Pts',(-1.93959038616316,0.246376356952387,
4.30995389861586));
#280015=CARTESIAN_POINT('Ctrl Pts',(-1.94695979284876,0.178975879837656,
4.31381698799612));
#280016=CARTESIAN_POINT('Ctrl Pts',(-1.95081656980679,0.11149309829426,
4.31768007737639));
#280017=CARTESIAN_POINT('Ctrl Pts',(-1.95296313333969,0.0739342558889111,
4.31983015420951));
#280018=CARTESIAN_POINT('Ctrl Pts',(-1.95402252639623,0.0363499266629029,
4.32198023104264));
#280019=CARTESIAN_POINT('Ctrl Pts',(-1.95399963679489,-0.00119138802316145,
4.32413030787576));
#280020=CARTESIAN_POINT('',(-1.95491180920002,0.00168629508682236,5.02413030787576));
#280021=CARTESIAN_POINT('Ctrl Pts',(-1.95628130950281,-0.00119277919923279,
4.32413030787576));
#280022=CARTESIAN_POINT('Ctrl Pts',(-1.95678939935296,-0.0719326340995119,
4.32817699638895));
#280023=CARTESIAN_POINT('Ctrl Pts',(-1.92119163391235,-0.790036186264717,
4.3692858248459));
#280024=CARTESIAN_POINT('Ctrl Pts',(-1.03336074967815,-2.06582911991838,
4.44745679324649));
#280025=CARTESIAN_POINT('Ctrl Pts',(1.17604813820198,-1.98806317010009,
4.55864321307768));
#280026=CARTESIAN_POINT('Ctrl Pts',(2.308145909957,-0.0891451065749571,
4.66982963290883));
#280027=CARTESIAN_POINT('Ctrl Pts',(1.32588189186438,1.89143374203366,4.78101605274001));
#280028=CARTESIAN_POINT('Ctrl Pts',(-0.87094746107776,2.13937722520349,
4.89220247257116));
#280029=CARTESIAN_POINT('Ctrl Pts',(-1.89060957867978,0.891720152086083,
4.97324055761641));
#280030=CARTESIAN_POINT('Ctrl Pts',(-1.95601481281436,0.122766393772507,
5.01721650271795));
#280031=CARTESIAN_POINT('Ctrl Pts',(-1.95491180920002,0.00168629508682236,
5.02413030787576));
#280032=CARTESIAN_POINT('',(-1.95368862328322,0.000190359573322832,5.72413029305739));
#280033=CARTESIAN_POINT('Ctrl Pts',(-1.95491180920002,0.00168629508682236,
5.02413030787576));
#280034=CARTESIAN_POINT('Ctrl Pts',(-1.95010205227512,-0.526295513449078,
5.05427864266167));
#280035=CARTESIAN_POINT('Ctrl Pts',(-1.45672934504036,-1.71125831262365,
5.12148911739128));
#280036=CARTESIAN_POINT('Ctrl Pts',(0.546914192237962,-2.24418565586851,
5.22576173206465));
#280037=CARTESIAN_POINT('Ctrl Pts',(2.18241236833561,-0.756677372605435,
5.33694815189581));
#280038=CARTESIAN_POINT('Ctrl Pts',(1.8187261335199,1.4239802115651,5.44813457172697));
#280039=CARTESIAN_POINT('Ctrl Pts',(-0.210992142997612,2.3002101441543,
5.55932099155813));
#280040=CARTESIAN_POINT('Ctrl Pts',(-1.73051050228896,1.28176270503949,
5.65131951958487));
#280041=CARTESIAN_POINT('Ctrl Pts',(-1.95107685069972,0.314893123742393,
5.70625590766786));
#280042=CARTESIAN_POINT('Ctrl Pts',(-1.95080468628648,0.000192495437545256,
5.72413015580714));
#280043=CARTESIAN_POINT('',(-1.95399919113549,-0.00177793190781093,6.42413030787576));
#280044=CARTESIAN_POINT('Ctrl Pts',(-1.95399999074999,0.000190128972365512,
5.72413030787576));
#280045=CARTESIAN_POINT('Ctrl Pts',(-1.95400695766447,-0.0714104832721157,
5.72819040273808));
#280046=CARTESIAN_POINT('Ctrl Pts',(-1.95007410706244,-0.142947655190763,
5.7322504976004));
#280047=CARTESIAN_POINT('Ctrl Pts',(-1.94224815867481,-0.213981518183981,
5.73631059246272));
#280048=CARTESIAN_POINT('Ctrl Pts',(-1.93440297274652,-0.285189994752401,
5.74038066774353));
#280049=CARTESIAN_POINT('Ctrl Pts',(-1.92264561855474,-0.355892259408381,
5.74445074302434));
#280050=CARTESIAN_POINT('Ctrl Pts',(-1.90707440104829,-0.425656233205034,
5.74852081830515));
#280051=CARTESIAN_POINT('Ctrl Pts',(-1.89148335587747,-0.495509041202204,
5.75259607623058));
#280052=CARTESIAN_POINT('Ctrl Pts',(-1.87206888637711,-0.564420760982678,
5.75667133415601));
#280053=CARTESIAN_POINT('Ctrl Pts',(-1.84897907873107,-0.631974972933889,
5.76074659208144));
#280054=CARTESIAN_POINT('Ctrl Pts',(-1.82582832708131,-0.699707489711552,
5.76483260637773));
#280055=CARTESIAN_POINT('Ctrl Pts',(-1.7989830101632,-0.766074934944469,
5.76891862067403));
#280056=CARTESIAN_POINT('Ctrl Pts',(-1.76863934637469,-0.830680963099129,
5.77300463497032));
#280057=CARTESIAN_POINT('Ctrl Pts',(-1.74713003595734,-0.876477381227694,
5.77590103372036));
#280058=CARTESIAN_POINT('Ctrl Pts',(-1.7238638766991,-0.921389208871823,
5.7787974324704));
#280059=CARTESIAN_POINT('Ctrl Pts',(-1.69892406073975,-0.965283914628009,
5.78169383122045));
#280060=CARTESIAN_POINT('Ctrl Pts',(-1.66518949487991,-1.02465760225439,
5.78561161291334));
#280061=CARTESIAN_POINT('Ctrl Pts',(-1.62827169589097,-1.08237868309912,
5.78952939460623));
#280062=CARTESIAN_POINT('Ctrl Pts',(-1.58835732078115,-1.13808480418681,
5.79344717629913));
#280063=CARTESIAN_POINT('Ctrl Pts',(-1.54850313226142,-1.19370692642781,
5.79735905039807));
#280064=CARTESIAN_POINT('Ctrl Pts',(-1.50566161943795,-1.24731972220939,
5.80127092449702));
#280065=CARTESIAN_POINT('Ctrl Pts',(-1.46006453905744,-1.29858674788672,
5.80518279859596));
#280066=CARTESIAN_POINT('Ctrl Pts',(-1.41452117876825,-1.3497933734402,
5.80909006392978));
#280067=CARTESIAN_POINT('Ctrl Pts',(-1.36622902381806,-1.39865935166361,
5.8129973292636));
#280068=CARTESIAN_POINT('Ctrl Pts',(-1.31546109495625,-1.44487996306147,
5.81690459459742));
#280069=CARTESIAN_POINT('Ctrl Pts',(-1.26472505856466,-1.49107153861907,
5.82080940538275));
#280070=CARTESIAN_POINT('Ctrl Pts',(-1.21151669639395,-1.53462071338429,
5.82471421616808));
#280071=CARTESIAN_POINT('Ctrl Pts',(-1.15614590441891,-1.57525954931096,
5.8286190269534));
#280072=CARTESIAN_POINT('Ctrl Pts',(-1.10079089563535,-1.61588680132298,
5.83252272469024));
#280073=CARTESIAN_POINT('Ctrl Pts',(-1.0432750771052,-1.6536050703696,5.83642642242708));
#280074=CARTESIAN_POINT('Ctrl Pts',(-0.983940011845606,-1.68818780148693,
5.84033012016392));
#280075=CARTESIAN_POINT('Ctrl Pts',(-0.924601499237589,-1.72277254184994,
5.84423404470436));
#280076=CARTESIAN_POINT('Ctrl Pts',(-0.86344395639434,-1.75422113707409,
5.84813796924479));
#280077=CARTESIAN_POINT('Ctrl Pts',(-0.800834824256486,-1.78235226155159,
5.85204189378522));
#280078=CARTESIAN_POINT('Ctrl Pts',(-0.738158941111589,-1.81051337815363,
5.85594998051232));
#280079=CARTESIAN_POINT('Ctrl Pts',(-0.674028829703269,-1.83534976327845,
5.85985806723941));
#280080=CARTESIAN_POINT('Ctrl Pts',(-0.608832326659619,-1.85672808941273,
5.86376615396651));
#280081=CARTESIAN_POINT('Ctrl Pts',(-0.543596847998696,-1.87811919588672,
5.86767657701665));
#280082=CARTESIAN_POINT('Ctrl Pts',(-0.477294183944824,-1.89604800065007,
5.87158700006679));
#280083=CARTESIAN_POINT('Ctrl Pts',(-0.410325031879865,-1.91043172299164,
5.87549742311693));
#280084=CARTESIAN_POINT('Ctrl Pts',(-0.343239924962017,-1.92484035026863,
5.87941461693414));
#280085=CARTESIAN_POINT('Ctrl Pts',(-0.275486512352373,-1.9356915663438,
5.88333181075135));
#280086=CARTESIAN_POINT('Ctrl Pts',(-0.207472454490163,-1.94295424048736,
5.88724900456856));
#280087=CARTESIAN_POINT('Ctrl Pts',(-0.174880762409147,-1.94643444512169,
5.88912608672958));
#280088=CARTESIAN_POINT('Ctrl Pts',(-0.142229245578587,-1.94909140723278,
5.89100316889061));
#280089=CARTESIAN_POINT('Ctrl Pts',(-0.10956264897586,-1.95092594066238,
5.89288025105163));
#280090=CARTESIAN_POINT('Ctrl Pts',(-0.0413820456987845,-1.95475491609815,
5.89679803274453));
#280091=CARTESIAN_POINT('Ctrl Pts',(0.0271349625788011,-1.95501304933571,
5.90071581443743));
#280092=CARTESIAN_POINT('Ctrl Pts',(0.0955826930932434,-1.95166081806779,
5.90463359613032));
#280093=CARTESIAN_POINT('Ctrl Pts',(0.163927211782491,-1.94831364160454,
5.90854547022926));
#280094=CARTESIAN_POINT('Ctrl Pts',(0.232202172605333,-1.94136692891848,
5.9124573443282));
#280095=CARTESIAN_POINT('Ctrl Pts',(0.299999223724627,-1.93083310147838,
5.91636921842713));
#280096=CARTESIAN_POINT('Ctrl Pts',(0.36771639991021,-1.9203116844419,5.92027648376095));
#280097=CARTESIAN_POINT('Ctrl Pts',(0.434956300770375,-1.90621162097472,
5.92418374909477));
#280098=CARTESIAN_POINT('Ctrl Pts',(0.501314871010041,-1.88859720430382,
5.92809101442859));
#280099=CARTESIAN_POINT('Ctrl Pts',(0.567631754720954,-1.87099385302935,
5.93199582521391));
#280100=CARTESIAN_POINT('Ctrl Pts',(0.633067931630309,-1.84988065386142,
5.93590063599924));
#280101=CARTESIAN_POINT('Ctrl Pts',(0.697230271724011,-1.8253728244366,
5.93980544678456));
#280102=CARTESIAN_POINT('Ctrl Pts',(0.761374322635581,-1.80087198085669,
5.94370914452139));
#280103=CARTESIAN_POINT('Ctrl Pts',(0.82424479816093,-1.77297860335807,
5.94761284225823));
#280104=CARTESIAN_POINT('Ctrl Pts',(0.885466183466893,-1.74185695105441,
5.95151653999506));
#280105=CARTESIAN_POINT('Ctrl Pts',(0.946691125716006,-1.71073349059258,
5.95542046453551));
#280106=CARTESIAN_POINT('Ctrl Pts',(1.0062663501162,-1.67638160817138,5.95932438907595));
#280107=CARTESIAN_POINT('Ctrl Pts',(1.06384032697169,-1.63901182384654,
5.96322831361639));
#280108=CARTESIAN_POINT('Ctrl Pts',(1.1214756865807,-1.60160219755862,5.96713640034348));
#280109=CARTESIAN_POINT('Ctrl Pts',(1.17710512704552,-1.56116851643907,
5.97104448707057));
#280110=CARTESIAN_POINT('Ctrl Pts',(1.23040640188764,-1.51796445485193,
5.97495257379766));
#280111=CARTESIAN_POINT('Ctrl Pts',(1.28373954117012,-1.47473456511625,
5.97886299684779));
#280112=CARTESIAN_POINT('Ctrl Pts',(1.33474137947926,-1.4287313283828,5.98277341989792));
#280113=CARTESIAN_POINT('Ctrl Pts',(1.38312517923919,-1.38024662236666,
5.98668384294805));
#280114=CARTESIAN_POINT('Ctrl Pts',(1.43159275393453,-1.33167796669928,
5.99060103676526));
#280115=CARTESIAN_POINT('Ctrl Pts',(1.47743291421019,-1.28061963225268,
5.99451823058246));
#280116=CARTESIAN_POINT('Ctrl Pts',(1.52039855491997,-1.22739734161243,
5.99843542439967));
#280117=CARTESIAN_POINT('Ctrl Pts',(1.54098728284033,-1.20189372422914,
6.00031250656071));
#280118=CARTESIAN_POINT('Ctrl Pts',(1.56091658765482,-1.17589365098658,
6.00218958872174));
#280119=CARTESIAN_POINT('Ctrl Pts',(1.5801629025028,-1.14943516631166,6.00406667088278));
#280120=CARTESIAN_POINT('Ctrl Pts',(1.6203331526561,-1.09421192194183,6.00798445257567));
#280121=CARTESIAN_POINT('Ctrl Pts',(1.6576848181063,-1.03677064632778,6.01190223426856));
#280122=CARTESIAN_POINT('Ctrl Pts',(1.6919648133459,-0.977430851978471,
6.01582001596145));
#280123=CARTESIAN_POINT('Ctrl Pts',(1.72619311803498,-0.918180535664875,
6.0197318900604));
#280124=CARTESIAN_POINT('Ctrl Pts',(1.75735870071082,-0.857037804707003,
6.02364376415934));
#280125=CARTESIAN_POINT('Ctrl Pts',(1.78525068244455,-0.794352567082953,
6.02755563825828));
#280126=CARTESIAN_POINT('Ctrl Pts',(1.81310980330664,-0.731741181921824,
6.0314629035921));
#280127=CARTESIAN_POINT('Ctrl Pts',(1.83770278376103,-0.667591346615471,
6.03537016892591));
#280128=CARTESIAN_POINT('Ctrl Pts',(1.85886466614673,-0.602277471728109,
6.03927743425973));
#280129=CARTESIAN_POINT('Ctrl Pts',(1.880013254614,-0.537004627090752,6.04318224504505));
#280130=CARTESIAN_POINT('Ctrl Pts',(1.89773486933775,-0.470569660400064,
6.04708705583038));
#280131=CARTESIAN_POINT('Ctrl Pts',(1.91191327041299,-0.403365400621706,
6.0509918666157));
#280132=CARTESIAN_POINT('Ctrl Pts',(1.92608762999975,-0.336180297110703,
6.05489556435254));
#280133=CARTESIAN_POINT('Ctrl Pts',(1.93672067937389,-0.268226816978515,
6.05879926208938));
#280134=CARTESIAN_POINT('Ctrl Pts',(1.94374693976471,-0.19990956494203,
6.06270295982621));
#280135=CARTESIAN_POINT('Ctrl Pts',(1.95077360837903,-0.131588343694882,
6.06660688436665));
#280136=CARTESIAN_POINT('Ctrl Pts',(1.95419302418105,-0.0629037982441252,
6.07051080890709));
#280137=CARTESIAN_POINT('Ctrl Pts',(1.9539915851719,0.00573455119522264,
6.07441473344753));
#280138=CARTESIAN_POINT('Ctrl Pts',(1.95378993139764,0.0744460797185567,
6.07832282017462));
#280139=CARTESIAN_POINT('Ctrl Pts',(1.94995972003222,0.143110821006934,
6.08223090690171));
#280140=CARTESIAN_POINT('Ctrl Pts',(1.94253948650132,0.211320475541774,
6.0861389936288));
#280141=CARTESIAN_POINT('Ctrl Pts',(1.93511481702416,0.279570907009037,
6.09004941667894));
#280142=CARTESIAN_POINT('Ctrl Pts',(1.92409593303982,0.347365224592687,
6.09395983972909));
#280143=CARTESIAN_POINT('Ctrl Pts',(1.9095727208377,0.414304264801236,6.09787026277923));
#280144=CARTESIAN_POINT('Ctrl Pts',(1.89502436217815,0.481359207724846,
6.10178745659643));
#280145=CARTESIAN_POINT('Ctrl Pts',(1.8769596945833,0.547555443231403,6.10570465041364));
#280146=CARTESIAN_POINT('Ctrl Pts',(1.8555185272343,0.612508771439441,6.10962184423084));
#280147=CARTESIAN_POINT('Ctrl Pts',(1.84524412299988,0.643633790871349,
6.11149892639188));
#280148=CARTESIAN_POINT('Ctrl Pts',(1.83419510797748,0.674473704393274,
6.11337600855291));
#280149=CARTESIAN_POINT('Ctrl Pts',(1.82239068168999,0.704988087338717,
6.11525309071394));
#280150=CARTESIAN_POINT('Ctrl Pts',(1.79775288683777,0.768676663872773,
6.11917087240684));
#280151=CARTESIAN_POINT('Ctrl Pts',(1.76972346344802,0.831198647850554,
6.12308865409974));
#280152=CARTESIAN_POINT('Ctrl Pts',(1.7384337605741,0.892168179266775,6.12700643579263));
#280153=CARTESIAN_POINT('Ctrl Pts',(1.70719123921109,0.953045775178734,
6.13091830989157));
#280154=CARTESIAN_POINT('Ctrl Pts',(1.67269841792492,1.01237513024198,6.13483018399051));
#280155=CARTESIAN_POINT('Ctrl Pts',(1.63513506494257,1.0697893808574,6.13874205808944));
#280156=CARTESIAN_POINT('Ctrl Pts',(1.59761596713474,1.1271359890107,6.14264932342326));
#280157=CARTESIAN_POINT('Ctrl Pts',(1.55703379014821,1.18257156394681,6.14655658875708));
#280158=CARTESIAN_POINT('Ctrl Pts',(1.51361378233008,1.23575455408444,6.1504638540909));
#280159=CARTESIAN_POINT('Ctrl Pts',(1.47022105100985,1.28890413460766,6.15436866487623));
#280160=CARTESIAN_POINT('Ctrl Pts',(1.4239943356286,1.33980355712585,6.15827347566155));
#280161=CARTESIAN_POINT('Ctrl Pts',(1.37520076718637,1.38814222971928,6.16217828644688));
#280162=CARTESIAN_POINT('Ctrl Pts',(1.32642110712801,1.43646712359483,6.16608198418372));
#280163=CARTESIAN_POINT('Ctrl Pts',(1.27507639582117,1.48223237047387,6.16998568192057));
#280164=CARTESIAN_POINT('Ctrl Pts',(1.2214711719523,1.52516365551028,6.17388937965741));
#280165=CARTESIAN_POINT('Ctrl Pts',(1.16786283363695,1.56809743484071,6.17779330419785));
#280166=CARTESIAN_POINT('Ctrl Pts',(1.11199410761861,1.60819661988606,6.1816972287383));
#280167=CARTESIAN_POINT('Ctrl Pts',(1.05420177961638,1.64522782855557,6.18560115327874));
#280168=CARTESIAN_POINT('Ctrl Pts',(0.996347836064562,1.68229851821421,
6.18950924000583));
#280169=CARTESIAN_POINT('Ctrl Pts',(0.936566612649027,1.71629443770833,
6.19341732673292));
#280170=CARTESIAN_POINT('Ctrl Pts',(0.875222126577904,1.74702668243746,
6.19732541346001));
#280171=CARTESIAN_POINT('Ctrl Pts',(0.813840967693204,1.77777729944346,
6.20123583651014));
#280172=CARTESIAN_POINT('Ctrl Pts',(0.750895137187055,1.80526016178985,
6.20514625956027));
#280173=CARTESIAN_POINT('Ctrl Pts',(0.686768805473429,1.82933447128419,
6.2090566826104));
#280174=CARTESIAN_POINT('Ctrl Pts',(0.622531441155418,1.8534504646424,6.21297387642761));
#280175=CARTESIAN_POINT('Ctrl Pts',(0.557109964922358,1.87414597763536,
6.21689107024481));
#280176=CARTESIAN_POINT('Ctrl Pts',(0.490903029007325,1.89133027684522,
6.22080826406202));
#280177=CARTESIAN_POINT('Ctrl Pts',(0.459177292640448,1.89956483020201,
6.22268534622305));
#280178=CARTESIAN_POINT('Ctrl Pts',(0.427271334890899,1.90699388526211,
6.22456242838408));
#280179=CARTESIAN_POINT('Ctrl Pts',(0.395229534069158,1.91361166786772,
6.22643951054511));
#280180=CARTESIAN_POINT('Ctrl Pts',(0.328352983179174,1.92742407740317,
6.23035729223801));
#280181=CARTESIAN_POINT('Ctrl Pts',(0.260618638799617,1.93775391997469,
6.2342750739309));
#280182=CARTESIAN_POINT('Ctrl Pts',(0.192421963113393,1.94450245258564,
6.2381928556238));
#280183=CARTESIAN_POINT('Ctrl Pts',(0.124328120688549,1.95124080913433,
6.24210472972274));
#280184=CARTESIAN_POINT('Ctrl Pts',(0.0557738161708393,1.95440852512743,
6.24601660382169));
#280185=CARTESIAN_POINT('Ctrl Pts',(-0.0128352105518403,1.95395784431755,
6.24992847792063));
#280186=CARTESIAN_POINT('Ctrl Pts',(-0.0813634057135774,1.95350769447619,
6.25383574325445));
#280187=CARTESIAN_POINT('Ctrl Pts',(-0.149945705409045,1.94944761739019,
6.25774300858827));
#280188=CARTESIAN_POINT('Ctrl Pts',(-0.218172992541176,1.94178179652752,
6.26165027392209));
#280189=CARTESIAN_POINT('Ctrl Pts',(-0.286357419214523,1.93412079134216,
6.26555508470742));
#280190=CARTESIAN_POINT('Ctrl Pts',(-0.354186787917246,1.9228585904466,
6.26945989549274));
#280191=CARTESIAN_POINT('Ctrl Pts',(-0.421255300329508,1.9080513546402,
6.27336470627807));
#280192=CARTESIAN_POINT('Ctrl Pts',(-0.488304695168545,1.89324833956875,
6.27726840401491));
#280193=CARTESIAN_POINT('Ctrl Pts',(-0.55459318406643,1.87490240157934,
6.28117210175175));
#280194=CARTESIAN_POINT('Ctrl Pts',(-0.619725181528424,1.85312079999647,
6.28507579948859));
#280195=CARTESIAN_POINT('Ctrl Pts',(-0.684860963138907,1.83133793290943,
6.28897972402904));
#280196=CARTESIAN_POINT('Ctrl Pts',(-0.748839654142734,1.80611916438945,
6.29288364856949));
#280197=CARTESIAN_POINT('Ctrl Pts',(-0.811282591432585,1.77762103859018,
6.29678757310993));
#280198=CARTESIAN_POINT('Ctrl Pts',(-0.873792102539848,1.74909252938638,
6.30069565983702));
#280199=CARTESIAN_POINT('Ctrl Pts',(-0.934762143815345,1.71727788995467,
6.30460374656412));
#280200=CARTESIAN_POINT('Ctrl Pts',(-0.993836671823604,1.68238065542213,
6.30851183329121));
#280201=CARTESIAN_POINT('Ctrl Pts',(-1.0529465156247,1.64746255870842,6.31242225634134));
#280202=CARTESIAN_POINT('Ctrl Pts',(-1.11015818107475,1.60945847159518,
6.31633267939148));
#280203=CARTESIAN_POINT('Ctrl Pts',(-1.16514513040121,1.56861493844166,
6.32024310244162));
#280204=CARTESIAN_POINT('Ctrl Pts',(-1.22022728779632,1.52770068607284,
6.32416029625883));
#280205=CARTESIAN_POINT('Ctrl Pts',(-1.27307666220068,1.48393748879884,
6.32807749007604));
#280206=CARTESIAN_POINT('Ctrl Pts',(-1.32340094106983,1.43761119541255,
6.33199468389326));
#280207=CARTESIAN_POINT('Ctrl Pts',(-1.34751585867119,1.41541207457285,
6.33387176605426));
#280208=CARTESIAN_POINT('Ctrl Pts',(-1.37105151764471,1.3926249344352,6.33574884821527));
#280209=CARTESIAN_POINT('Ctrl Pts',(-1.39397901335,1.36928394072952,6.33762593037627));
#280210=CARTESIAN_POINT('Ctrl Pts',(-1.44117183502743,1.32123999524655,
6.34148962333414));
#280211=CARTESIAN_POINT('Ctrl Pts',(-1.48598395771404,1.27064520587233,
6.34535331629201));
#280212=CARTESIAN_POINT('Ctrl Pts',(-1.5281218119321,1.21776833917513,6.34921700924988));
#280213=CARTESIAN_POINT('Ctrl Pts',(-1.57020241583544,1.16496331328036,
6.35307545282707));
#280214=CARTESIAN_POINT('Ctrl Pts',(-1.60961563734762,1.10988274487347,
6.35693389640426));
#280215=CARTESIAN_POINT('Ctrl Pts',(-1.64610459419185,1.05283221121909,
6.36079233998145));
#280216=CARTESIAN_POINT('Ctrl Pts',(-1.68255730843301,0.995838342923919,
6.3646469511652));
#280217=CARTESIAN_POINT('Ctrl Pts',(-1.71609124364471,0.936878812047662,
6.36850156234894));
#280218=CARTESIAN_POINT('Ctrl Pts',(-1.74649095490027,0.87629067349342,
6.37235617353269));
#280219=CARTESIAN_POINT('Ctrl Pts',(-1.77687157268618,0.815740589175113,
6.37620836370983));
#280220=CARTESIAN_POINT('Ctrl Pts',(-1.80412164463283,0.753564377846253,
6.38006055388697));
#280221=CARTESIAN_POINT('Ctrl Pts',(-1.82807111724676,0.690124619389999,
6.38391274406411));
#280222=CARTESIAN_POINT('Ctrl Pts',(-1.85202294598191,0.626678619804194,
6.38776531321524));
#280223=CARTESIAN_POINT('Ctrl Pts',(-1.87267333389262,0.561969293509401,
6.39161788236636));
#280224=CARTESIAN_POINT('Ctrl Pts',(-1.88990057293408,0.496378710687146,
6.39547045151749));
#280225=CARTESIAN_POINT('Ctrl Pts',(-1.90712859132636,0.430785160583011,
6.39932319495672));
#280226=CARTESIAN_POINT('Ctrl Pts',(-1.92093303579742,0.36431076788473,
6.40317593839596));
#280227=CARTESIAN_POINT('Ctrl Pts',(-1.93124288827011,0.297349804953888,
6.40702868183519));
#280228=CARTESIAN_POINT('Ctrl Pts',(-1.94156260508316,0.230324774595253,
6.41088511153208));
#280229=CARTESIAN_POINT('Ctrl Pts',(-1.948380995502,0.16281274812497,6.41474154122897));
#280230=CARTESIAN_POINT('Ctrl Pts',(-1.95167885002433,0.0952137929487952,
6.41859797092586));
#280231=CARTESIAN_POINT('Ctrl Pts',(-1.95325585638024,0.0628885398960482,
6.42044208324249));
#280232=CARTESIAN_POINT('Ctrl Pts',(-1.954028600145,0.0305434300892876,
6.42228619555913));
#280233=CARTESIAN_POINT('Ctrl Pts',(-1.95399919113549,-0.00177793190781093,
6.42413030787576));
#280234=CARTESIAN_POINT('',(-1.95675615924934,0.000851174274233985,7.12413030787576));
#280235=CARTESIAN_POINT('Ctrl Pts',(-1.95421427783755,-0.00177812761388513,
6.42413030787576));
#280236=CARTESIAN_POINT('Ctrl Pts',(-1.95554703085897,-0.145994290672205,
6.43235765531965));
#280237=CARTESIAN_POINT('Ctrl Pts',(-1.87512506264653,-0.938395085048426,
6.47764714270725));
#280238=CARTESIAN_POINT('Ctrl Pts',(-0.794746594271796,-2.16883891577301,
6.55999877003861));
#280239=CARTESIAN_POINT('Ctrl Pts',(1.39194049181098,-1.84336270411812,
6.67118518986975));
#280240=CARTESIAN_POINT('Ctrl Pts',(2.30354969961481,0.17071371673631,6.78237160970092));
#280241=CARTESIAN_POINT('Ctrl Pts',(1.10500744564588,2.02840896683697,6.89355802953208));
#280242=CARTESIAN_POINT('Ctrl Pts',(-1.10576956804582,2.02799360306211,
7.00474444936326));
#280243=CARTESIAN_POINT('Ctrl Pts',(-1.9337773035453,0.743553653930807,
7.08160187547781));
#280244=CARTESIAN_POINT('Ctrl Pts',(-1.95701686505733,0.0485985200318871,
7.12139716164864));
#280245=CARTESIAN_POINT('Ctrl Pts',(-1.95675615924934,0.000851174274233985,
7.12413030787576));
#280246=CARTESIAN_POINT('',(-1.95399958925359,0.00126696360743394,7.82413030787576));
#280247=CARTESIAN_POINT('Ctrl Pts',(-1.95675615924934,0.000851174274233985,
7.12413030787576));
#280248=CARTESIAN_POINT('Ctrl Pts',(-1.95348162971424,-0.598867317271105,
7.15845930159236));
#280249=CARTESIAN_POINT('Ctrl Pts',(-1.33749233620385,-1.85186615856446,
7.2298504352527));
#280250=CARTESIAN_POINT('Ctrl Pts',(0.795561506911455,-2.16854012653626,
7.33830370885674));
#280251=CARTESIAN_POINT('Ctrl Pts',(2.25360188555758,-0.506717804195069,
7.44949012868789));
#280252=CARTESIAN_POINT('Ctrl Pts',(1.64724516703786,1.6192800101739,7.56067654851907));
#280253=CARTESIAN_POINT('Ctrl Pts',(-0.468059588377089,2.26194708457213,
7.67186296835022));
#280254=CARTESIAN_POINT('Ctrl Pts',(-1.80012985616923,1.13299355714076,
7.75968060691936));
#280255=CARTESIAN_POINT('Ctrl Pts',(-1.95308798861268,0.242106011541422,
7.8104361055448));
#280256=CARTESIAN_POINT('Ctrl Pts',(-1.95166131896414,0.00128028472646311,
7.8241294642265));
#280257=CARTESIAN_POINT('',(-1.95399942135932,-0.00150377106857099,8.52413030787576));
#280258=CARTESIAN_POINT('Ctrl Pts',(-1.9539995892536,0.00126696360743394,
7.82413030787576));
#280259=CARTESIAN_POINT('Ctrl Pts',(-1.95404443793575,-0.067901800190388,
7.8280585559228));
#280260=CARTESIAN_POINT('Ctrl Pts',(-1.95041224119463,-0.137089327859001,
7.83198680396985));
#280261=CARTESIAN_POINT('Ctrl Pts',(-1.94312353915447,-0.205880818882736,
7.83591505201689));
#280262=CARTESIAN_POINT('Ctrl Pts',(-1.93583412258889,-0.274679053668013,
7.8398436851576));
#280263=CARTESIAN_POINT('Ctrl Pts',(-1.92488754124365,-0.343080694373507,
7.84377231829832));
#280264=CARTESIAN_POINT('Ctrl Pts',(-1.91035611453868,-0.410676899331691,
7.84770095143903));
#280265=CARTESIAN_POINT('Ctrl Pts',(-1.8958068870018,-0.478355908869621,
7.85163439711052));
#280266=CARTESIAN_POINT('Ctrl Pts',(-1.87766414568324,-0.54522703855923,
7.855567842782));
#280267=CARTESIAN_POINT('Ctrl Pts',(-1.85605105652718,-0.610893178521688,
7.85950128845349));
#280268=CARTESIAN_POINT('Ctrl Pts',(-1.83442503942436,-0.676598596921187,
7.8634370869296));
#280269=CARTESIAN_POINT('Ctrl Pts',(-1.80932471570444,-0.741097139190985,
7.86737288540572));
#280270=CARTESIAN_POINT('Ctrl Pts',(-1.78092171510111,-0.804011097362054,
7.87130868388183));
#280271=CARTESIAN_POINT('Ctrl Pts',(-1.75246007613188,-0.867054942221865,
7.87525260786533));
#280272=CARTESIAN_POINT('Ctrl Pts',(-1.72068235784896,-0.928507235402445,
7.87919653184883));
#280273=CARTESIAN_POINT('Ctrl Pts',(-1.68580637056182,-0.988014615769008,
7.88314045583233));
#280274=CARTESIAN_POINT('Ctrl Pts',(-1.65310109503736,-1.04381820505823,
7.88683890655907));
#280275=CARTESIAN_POINT('Ctrl Pts',(-1.61767184319614,-1.09791144835028,
7.89053735728581));
#280276=CARTESIAN_POINT('Ctrl Pts',(-1.57973087609372,-1.15002885142772,
7.89423580801255));
#280277=CARTESIAN_POINT('Ctrl Pts',(-1.53953987794175,-1.20523699741716,
7.89815358970541));
#280278=CARTESIAN_POINT('Ctrl Pts',(-1.49637144867376,-1.25844539685319,
7.90207137139828));
#280279=CARTESIAN_POINT('Ctrl Pts',(-1.4504517700784,-1.30931495931133,
7.90598915309115));
#280280=CARTESIAN_POINT('Ctrl Pts',(-1.40460133342585,-1.3601078159335,
7.90990102719005));
#280281=CARTESIAN_POINT('Ctrl Pts',(-1.35600820786029,-1.40856847255519,
7.91381290128896));
#280282=CARTESIAN_POINT('Ctrl Pts',(-1.3049404788002,-1.45438865052939,
7.91772477538787));
#280283=CARTESIAN_POINT('Ctrl Pts',(-1.25393291506304,-1.50015484557043,
7.92163204072166));
#280284=CARTESIAN_POINT('Ctrl Pts',(-1.2004569023679,-1.54328641317032,
7.92553930605545));
#280285=CARTESIAN_POINT('Ctrl Pts',(-1.14481796507741,-1.58351123356799,
7.92944657138924));
#280286=CARTESIAN_POINT('Ctrl Pts',(-1.0892139802301,-1.62371078468811,
7.93335138217454));
#280287=CARTESIAN_POINT('Ctrl Pts',(-1.03145016389223,-1.66100692322339,
7.93725619295983));
#280288=CARTESIAN_POINT('Ctrl Pts',(-0.971864550243031,-1.69516822055539,
7.94116100374513));
#280289=CARTESIAN_POINT('Ctrl Pts',(-0.91229592120101,-1.72931978036551,
7.94506470148194));
#280290=CARTESIAN_POINT('Ctrl Pts',(-0.85090695233309,-1.76033802825822,
7.94896839921874));
#280291=CARTESIAN_POINT('Ctrl Pts',(-0.788062495477797,-1.7880362141806,
7.95287209695555));
#280292=CARTESIAN_POINT('Ctrl Pts',(-0.725214387379388,-1.81573600935885,
7.95677602149597));
#280293=CARTESIAN_POINT('Ctrl Pts',(-0.660911074630634,-1.84011516352156,
7.96067994603638));
#280294=CARTESIAN_POINT('Ctrl Pts',(-0.595538042169783,-1.86103477676495,
7.9645838705768));
#280295=CARTESIAN_POINT('Ctrl Pts',(-0.530095311957344,-1.88197669354778,
7.96849195730386));
#280296=CARTESIAN_POINT('Ctrl Pts',(-0.463581055431145,-1.8994515581827,
7.97240004403092));
#280297=CARTESIAN_POINT('Ctrl Pts',(-0.396395632058983,-1.91337045625894,
7.97630813075798));
#280298=CARTESIAN_POINT('Ctrl Pts',(-0.329170044057961,-1.92729767529749,
7.98021855380809));
#280299=CARTESIAN_POINT('Ctrl Pts',(-0.261272977100312,-1.93766462274403,
7.9841289768582));
#280300=CARTESIAN_POINT('Ctrl Pts',(-0.193111891627182,-1.94443405578903,
7.98803939990831));
#280301=CARTESIAN_POINT('Ctrl Pts',(-0.124832787508198,-1.95121520988154,
7.99195659372549));
#280302=CARTESIAN_POINT('Ctrl Pts',(-0.0562892437003932,-1.95438639463801,
7.99587378754267));
#280303=CARTESIAN_POINT('Ctrl Pts',(0.0121101626753464,-1.95396247250554,
7.99979098135985));
#280304=CARTESIAN_POINT('Ctrl Pts',(0.0448865101176289,-1.95375933303638,
8.00166806352114));
#280305=CARTESIAN_POINT('Ctrl Pts',(0.0776298214714477,-1.95273144156208,
8.00354514568243));
#280306=CARTESIAN_POINT('Ctrl Pts',(0.110295726423287,-1.95088463337348,
8.00542222784371));
#280307=CARTESIAN_POINT('Ctrl Pts',(0.178474886102253,-1.94703003848094,
8.0093400095367));
#280308=CARTESIAN_POINT('Ctrl Pts',(0.246587176902543,-1.93958941362714,
8.01325779122968));
#280309=CARTESIAN_POINT('Ctrl Pts',(0.314225044159618,-1.92856906063093,
8.01717557292266));
#280310=CARTESIAN_POINT('Ctrl Pts',(0.381760920778319,-1.91756532514327,
8.02108744702169));
#280311=CARTESIAN_POINT('Ctrl Pts',(0.448823311960776,-1.90299265271881,
8.02499932112072));
#280312=CARTESIAN_POINT('Ctrl Pts',(0.515007846170036,-1.88490925998662,
8.02891119521974));
#280313=CARTESIAN_POINT('Ctrl Pts',(0.581114405228445,-1.86684717216037,
8.03281846055364));
#280314=CARTESIAN_POINT('Ctrl Pts',(0.646344688998125,-1.84528270747954,
8.03672572588755));
#280315=CARTESIAN_POINT('Ctrl Pts',(0.710304422502188,-1.82032514331199,
8.04063299122145));
#280316=CARTESIAN_POINT('Ctrl Pts',(0.7742239764295,-1.79538325751442,8.04453780200686));
#280317=CARTESIAN_POINT('Ctrl Pts',(0.836874106082847,-1.76705267894244,
8.04844261279227));
#280318=CARTESIAN_POINT('Ctrl Pts',(0.897877113400025,-1.73549205968579,
8.05234742357768));
#280319=CARTESIAN_POINT('Ctrl Pts',(0.958862732088378,-1.70394043663963,
8.0562511213146));
#280320=CARTESIAN_POINT('Ctrl Pts',(1.01820172371542,-1.66916082660839,
8.06015481905152));
#280321=CARTESIAN_POINT('Ctrl Pts',(1.07553940315965,-1.6313586338543,8.06405851678843));
#280322=CARTESIAN_POINT('Ctrl Pts',(1.13288041390487,-1.59355424480481,
8.06796244132895));
#280323=CARTESIAN_POINT('Ctrl Pts',(1.18821947227951,-1.55272719731684,
8.07186636586947));
#280324=CARTESIAN_POINT('Ctrl Pts',(1.24123092337494,-1.50912616929725,
8.07577029040999));
#280325=CARTESIAN_POINT('Ctrl Pts',(1.29429889286668,-1.46547865584612,
8.07967837713716));
#280326=CARTESIAN_POINT('Ctrl Pts',(1.34503392183809,-1.41905157268594,
8.08358646386434));
#280327=CARTESIAN_POINT('Ctrl Pts',(1.39314430114039,-1.37013318921923,
8.08749455059151));
#280328=CARTESIAN_POINT('Ctrl Pts',(1.44128344167438,-1.32118556148171,
8.09140497364173));
#280329=CARTESIAN_POINT('Ctrl Pts',(1.48679448377884,-1.26974403790752,
8.09531539669194));
#280330=CARTESIAN_POINT('Ctrl Pts',(1.52942529415635,-1.21613086039076,
8.09922581974216));
#280331=CARTESIAN_POINT('Ctrl Pts',(1.57212991835997,-1.16242485344553,
8.10314301355945));
#280332=CARTESIAN_POINT('Ctrl Pts',(1.61194407207022,-1.10654008830249,
8.10706020737674));
#280333=CARTESIAN_POINT('Ctrl Pts',(1.6486588056391,-1.04882798522382,8.11097740119403));
#280334=CARTESIAN_POINT('Ctrl Pts',(1.6662521580787,-1.02117289227349,8.11285448335431));
#280335=CARTESIAN_POINT('Ctrl Pts',(1.68313449029611,-0.993098564907489,
8.1147315655146));
#280336=CARTESIAN_POINT('Ctrl Pts',(1.69928665847842,-0.964645454204422,
8.11660864767488));
#280337=CARTESIAN_POINT('Ctrl Pts',(1.73299891153957,-0.905259094579355,
8.12052642936771));
#280338=CARTESIAN_POINT('Ctrl Pts',(1.76366125052136,-0.843985380605829,
8.12444421106054));
#280339=CARTESIAN_POINT('Ctrl Pts',(1.79105808563739,-0.781170233606551,
8.12836199275337));
#280340=CARTESIAN_POINT('Ctrl Pts',(1.81841360926896,-0.718449805101552,
8.13227386685224));
#280341=CARTESIAN_POINT('Ctrl Pts',(1.8425132063164,-0.654193003792113,
8.13618574095111));
#280342=CARTESIAN_POINT('Ctrl Pts',(1.86318664099535,-0.58877121262547,
8.14009761504998));
#280343=CARTESIAN_POINT('Ctrl Pts',(1.88383571931665,-0.523426497985717,
8.14400488038373));
#280344=CARTESIAN_POINT('Ctrl Pts',(1.90106650428336,-0.456919986223647,
8.14791214571749));
#280345=CARTESIAN_POINT('Ctrl Pts',(1.91475714328836,-0.38964224902621,
8.15181941105124));
#280346=CARTESIAN_POINT('Ctrl Pts',(1.92843918181849,-0.32240677577918,
8.1557242218365));
#280347=CARTESIAN_POINT('Ctrl Pts',(1.93858538801781,-0.254401519164342,
8.15962903262176));
#280348=CARTESIAN_POINT('Ctrl Pts',(1.94512438775213,-0.186029879782499,
8.16353384340702));
#280349=CARTESIAN_POINT('Ctrl Pts',(1.95166152357443,-0.117677729424321,
8.16743754114379));
#280350=CARTESIAN_POINT('Ctrl Pts',(1.95459344727363,-0.0489598931344899,
8.17134123888057));
#280351=CARTESIAN_POINT('Ctrl Pts',(1.95390054740418,0.0197142297250717,
8.17524493661734));
#280352=CARTESIAN_POINT('Ctrl Pts',(1.95320760727746,0.0883923425296247,
8.17914886115773));
#280353=CARTESIAN_POINT('Ctrl Pts',(1.94888943298335,0.157026244931154,
8.18305278569811));
#280354=CARTESIAN_POINT('Ctrl Pts',(1.94097851366729,0.225207480963497,
8.1869567102385));
#280355=CARTESIAN_POINT('Ctrl Pts',(1.93305916008916,0.29346140872608,8.19086479696552));
#280356=CARTESIAN_POINT('Ctrl Pts',(1.92153947388549,0.361261217316709,
8.19477288369255));
#280357=CARTESIAN_POINT('Ctrl Pts',(1.90650361446225,0.42820552079856,8.19868097041958));
#280358=CARTESIAN_POINT('Ctrl Pts',(1.89145876633754,0.495189844763646,
8.20259139346965));
#280359=CARTESIAN_POINT('Ctrl Pts',(1.87289369457593,0.561317172028689,
8.20650181651973));
#280360=CARTESIAN_POINT('Ctrl Pts',(1.8509425580627,0.626200963551082,8.2104122395698));
#280361=CARTESIAN_POINT('Ctrl Pts',(1.82895341388883,0.691197099194167,
8.21432943338695));
#280362=CARTESIAN_POINT('Ctrl Pts',(1.8035666854114,0.75494494486457,8.21824662720409));
#280363=CARTESIAN_POINT('Ctrl Pts',(1.77496445739794,0.817078438691188,
8.22216382102124));
#280364=CARTESIAN_POINT('Ctrl Pts',(1.76125854074122,0.846852220215407,
8.22404090318284));
#280365=CARTESIAN_POINT('Ctrl Pts',(1.74681494509785,0.876255681653442,
8.22591798534444));
#280366=CARTESIAN_POINT('Ctrl Pts',(1.73165728971869,0.905250811081732,
8.22779506750604));
#280367=CARTESIAN_POINT('Ctrl Pts',(1.70002074979301,0.965768453610346,
8.23171284919877));
#280368=CARTESIAN_POINT('Ctrl Pts',(1.66514510420117,1.02474587641108,8.2356306308915));
#280369=CARTESIAN_POINT('Ctrl Pts',(1.62720421763237,1.0818144175964,8.23954841258423));
#280370=CARTESIAN_POINT('Ctrl Pts',(1.58932054184508,1.13879690555163,8.24346028668299));
#280371=CARTESIAN_POINT('Ctrl Pts',(1.54838106833165,1.19387581803668,8.24737216078176));
#280372=CARTESIAN_POINT('Ctrl Pts',(1.5046056404242,1.24670680867784,8.25128403488052));
#280373=CARTESIAN_POINT('Ctrl Pts',(1.46088178643246,1.29947555661371,8.25519130021417));
#280374=CARTESIAN_POINT('Ctrl Pts',(1.41432892603191,1.35000126537272,8.25909856554782));
#280375=CARTESIAN_POINT('Ctrl Pts',(1.36520925125971,1.3979698495586,8.26300583088147));
#280376=CARTESIAN_POINT('Ctrl Pts',(1.31612043352268,1.44590829982572,8.26691064166662));
#280377=CARTESIAN_POINT('Ctrl Pts',(1.2644683512111,1.49129246909334,8.27081545245178));
#280378=CARTESIAN_POINT('Ctrl Pts',(1.21055333592218,1.53384374070102,8.27472026323693));
#280379=CARTESIAN_POINT('Ctrl Pts',(1.15665368886223,1.57638288326297,8.2786239609736));
#280380=CARTESIAN_POINT('Ctrl Pts',(1.10049277533017,1.61609042652526,8.28252765871026));
#280381=CARTESIAN_POINT('Ctrl Pts',(1.0424040224913,1.65272800360312,8.28643135644693));
#280382=CARTESIAN_POINT('Ctrl Pts',(0.98431189471428,1.68936770931261,8.2903352809872));
#280383=CARTESIAN_POINT('Ctrl Pts',(0.924292122746999,1.72293683442513,
8.29423920552746));
#280384=CARTESIAN_POINT('Ctrl Pts',(0.862705578322242,1.75324130830062,
8.29814313006773));
#280385=CARTESIAN_POINT('Ctrl Pts',(0.801053373126938,1.78357809142685,
8.30205121679465));
#280386=CARTESIAN_POINT('Ctrl Pts',(0.737831504082082,1.81064305936345,
8.30595930352158));
#280387=CARTESIAN_POINT('Ctrl Pts',(0.673422905481371,1.83428939657106,
8.3098673902485));
#280388=CARTESIAN_POINT('Ctrl Pts',(0.608975802286412,1.85794986997539,
8.31377781329848));
#280389=CARTESIAN_POINT('Ctrl Pts',(0.543341027819345,1.87818750030037,
8.31768823634846));
#280390=CARTESIAN_POINT('Ctrl Pts',(0.476916137788858,1.89490553788746,
8.32159865939843));
#280391=CARTESIAN_POINT('Ctrl Pts',(0.410376235277159,1.91165252219893,
8.32551585321547));
#280392=CARTESIAN_POINT('Ctrl Pts',(0.343043969273922,1.92486765613821,
8.32943304703251));
#280393=CARTESIAN_POINT('Ctrl Pts',(0.275325661415558,1.93450556478034,
8.33335024084955));
#280394=CARTESIAN_POINT('Ctrl Pts',(0.242875689906377,1.93912395928451,
8.3352273230121));
#280395=CARTESIAN_POINT('Ctrl Pts',(0.210337126602138,1.94292170846408,
8.33710440517465));
#280396=CARTESIAN_POINT('Ctrl Pts',(0.177754717559067,1.94589806012173,
8.3389814873372));
#280397=CARTESIAN_POINT('Ctrl Pts',(0.109749827722278,1.95211019951037,
8.34289926903069));
#280398=CARTESIAN_POINT('Ctrl Pts',(0.0412838019476793,1.95476545318489,
8.34681705072418));
#280399=CARTESIAN_POINT('Ctrl Pts',(-0.0272393081980585,1.95381012897592,
8.35073483241766));
#280400=CARTESIAN_POINT('Ctrl Pts',(-0.0956590928540732,1.95285624529323,
8.35464670651719));
#280401=CARTESIAN_POINT('Ctrl Pts',(-0.16413530308866,1.94830259557962,
8.35855858061671));
#280402=CARTESIAN_POINT('Ctrl Pts',(-0.232259402482933,1.94014730625236,
8.36247045471623));
#280403=CARTESIAN_POINT('Ctrl Pts',(-0.300303241632396,1.93200162505971,
8.36637772005063));
#280404=CARTESIAN_POINT('Ctrl Pts',(-0.367995307640907,1.92026278958752,
8.37028498538504));
#280405=CARTESIAN_POINT('Ctrl Pts',(-0.434929543107837,1.90498091657948,
8.37419225071944));
#280406=CARTESIAN_POINT('Ctrl Pts',(-0.501821730412533,1.88970864366131,
8.37809706150536));
#280407=CARTESIAN_POINT('Ctrl Pts',(-0.567956552980499,1.87089785758528,
8.38200187229127));
#280408=CARTESIAN_POINT('Ctrl Pts',(-0.632937090255617,1.84864995057982,
8.38590668307718));
#280409=CARTESIAN_POINT('Ctrl Pts',(-0.697899105125326,1.82640838523864,
8.38981038081461));
#280410=CARTESIAN_POINT('Ctrl Pts',(-0.7617070226247,1.80073180316959,8.39371407855204));
#280411=CARTESIAN_POINT('Ctrl Pts',(-0.823979810726255,1.77177122437281,
8.39761777628947));
#280412=CARTESIAN_POINT('Ctrl Pts',(-0.886256216856737,1.74280896297573,
8.40152170083048));
#280413=CARTESIAN_POINT('Ctrl Pts',(-0.946996871492811,1.71056253582719,
8.4054256253715));
#280414=CARTESIAN_POINT('Ctrl Pts',(-1.00584309447748,1.6752300347391,8.40932954991251));
#280415=CARTESIAN_POINT('Ctrl Pts',(-1.0647520566267,1.63985986374652,8.41323763664018));
#280416=CARTESIAN_POINT('Ctrl Pts',(-1.12176213366443,1.60139730620336,
8.41714572336785));
#280417=CARTESIAN_POINT('Ctrl Pts',(-1.17654240083538,1.56008460637125,
8.42105381009552));
#280418=CARTESIAN_POINT('Ctrl Pts',(-1.23135541661431,1.51874720907997,
8.42496423314622));
#280419=CARTESIAN_POINT('Ctrl Pts',(-1.28393559288869,1.474556595086,8.42887465619693));
#280420=CARTESIAN_POINT('Ctrl Pts',(-1.33398615540298,1.4277944309995,8.43278507924764));
#280421=CARTESIAN_POINT('Ctrl Pts',(-1.38412337879653,1.38095129978591,
8.4367022730654));
#280422=CARTESIAN_POINT('Ctrl Pts',(-1.43172190553461,1.33152808596602,
8.44061946688316));
#280423=CARTESIAN_POINT('Ctrl Pts',(-1.47652338535857,1.27984166696091,
8.44453666070093));
#280424=CARTESIAN_POINT('Ctrl Pts',(-1.49799182992469,1.25507402478496,
8.44641374285674));
#280425=CARTESIAN_POINT('Ctrl Pts',(-1.51881862517038,1.22978715877023,
8.44829082501255));
#280426=CARTESIAN_POINT('Ctrl Pts',(-1.53897888756308,1.20401826549065,
8.45016790716836));
#280427=CARTESIAN_POINT('Ctrl Pts',(-1.58104064327307,1.15025483360024,
8.45408419404734));
#280428=CARTESIAN_POINT('Ctrl Pts',(-1.62036837644652,1.09417386838946,
8.45800048092632));
#280429=CARTESIAN_POINT('Ctrl Pts',(-1.65669693711659,1.0360845807889,8.4619167678053));
#280430=CARTESIAN_POINT('Ctrl Pts',(-1.69297183985178,0.978081092106694,
8.4658272702584));
#280431=CARTESIAN_POINT('Ctrl Pts',(-1.72625609860507,0.918075577768491,
8.46973777271151));
#280432=CARTESIAN_POINT('Ctrl Pts',(-1.756325419742,0.85640937638964,8.47364827516461));
#280433=CARTESIAN_POINT('Ctrl Pts',(-1.78636063875987,0.794813111679201,
8.47755434265161));
#280434=CARTESIAN_POINT('Ctrl Pts',(-1.8131879412576,0.731560336950756,
8.4814604101386));
#280435=CARTESIAN_POINT('Ctrl Pts',(-1.8366278587371,0.667018821706528,
8.4853664776256));
#280436=CARTESIAN_POINT('Ctrl Pts',(-1.86005037352256,0.602525224559474,
8.48926964509822));
#280437=CARTESIAN_POINT('Ctrl Pts',(-1.88009032732257,0.536745246884614,
8.49317281257085));
#280438=CARTESIAN_POINT('Ctrl Pts',(-1.89661621162106,0.470066958864574,
8.49707598004347));
#280439=CARTESIAN_POINT('Ctrl Pts',(-1.91313511727448,0.403416828133862,
8.50097749926419));
#280440=CARTESIAN_POINT('Ctrl Pts',(-1.92614278481498,0.33586961789548,
8.5048790184849));
#280441=CARTESIAN_POINT('Ctrl Pts',(-1.9355579650531,0.267827115728595,
8.50878053770561));
#280442=CARTESIAN_POINT('Ctrl Pts',(-1.94497445087806,0.199775178225063,
8.51268259794328));
#280443=CARTESIAN_POINT('Ctrl Pts',(-1.95079738608773,0.131228298643438,
8.51658465818095));
#280444=CARTESIAN_POINT('Ctrl Pts',(-1.95299713534415,0.0625954418271417,
8.52048671841862));
#280445=CARTESIAN_POINT('Ctrl Pts',(-1.95368181495021,0.0412332264607191,
8.52170124823767));
#280446=CARTESIAN_POINT('Ctrl Pts',(-1.95401586470436,0.0198627037635852,
8.52291577805671));
#280447=CARTESIAN_POINT('Ctrl Pts',(-1.95399942135932,-0.00150377106857099,
8.52413030787576));
#280448=CARTESIAN_POINT('',(-1.95425084356951,-0.000465081590652265,9.22413026128937));
#280449=CARTESIAN_POINT('Ctrl Pts',(-1.9521545497156,-0.00151646469114672,
8.52413111087899));
#280450=CARTESIAN_POINT('Ctrl Pts',(-1.9537147512388,-0.219593375837535,
8.53653884958584));
#280451=CARTESIAN_POINT('Ctrl Pts',(-1.81934971248804,-1.08720016982708,
8.58600872823641));
#280452=CARTESIAN_POINT('Ctrl Pts',(-0.546070872269969,-2.24439100726284,
8.67254074683069));
#280453=CARTESIAN_POINT('Ctrl Pts',(1.59021074792358,-1.67532509350279,
8.78372716666185));
#280454=CARTESIAN_POINT('Ctrl Pts',(2.26979033427429,0.42841128879651,8.89491358649301));
#280455=CARTESIAN_POINT('Ctrl Pts',(0.870143500653463,2.13970434291615,
9.00610000632417));
#280456=CARTESIAN_POINT('Ctrl Pts',(-1.29798992125702,1.89417448969363,
9.11583872315943));
#280457=CARTESIAN_POINT('Ctrl Pts',(-1.9550702218924,0.621448895034945,
9.18851530005095));
#280458=CARTESIAN_POINT('Ctrl Pts',(-1.95707450182562,-0.000456599506395794,
9.22412973699875));
#280459=CARTESIAN_POINT('',(-1.95399918605333,0.00178350859616108,9.92413029181523));
#280460=CARTESIAN_POINT('Ctrl Pts',(-1.95399994447223,-0.000465835275089229,
9.22413030787576));
#280461=CARTESIAN_POINT('Ctrl Pts',(-1.95399392795271,-0.0257028223412335,
9.22557782057934));
#280462=CARTESIAN_POINT('Ctrl Pts',(-1.9534990074032,-0.0509333767812854,
9.22702533328292));
#280463=CARTESIAN_POINT('Ctrl Pts',(-1.95251580652132,-0.0761447653119341,
9.2284728459865));
#280464=CARTESIAN_POINT('Ctrl Pts',(-1.94985471318939,-0.14438093062052,
9.2323906276671));
#280465=CARTESIAN_POINT('Ctrl Pts',(-1.94360696888932,-0.212612981054866,
9.23630840934769));
#280466=CARTESIAN_POINT('Ctrl Pts',(-1.93377174360208,-0.280433314080482,
9.24022619102828));
#280467=CARTESIAN_POINT('Ctrl Pts',(-1.92395134877935,-0.348151381320416,
9.24413806511444));
#280468=CARTESIAN_POINT('Ctrl Pts',(-1.91055427893775,-0.415458480304355,
9.24804993920061));
#280469=CARTESIAN_POINT('Ctrl Pts',(-1.89363166661572,-0.481949282798708,
9.25196181328677));
#280470=CARTESIAN_POINT('Ctrl Pts',(-1.87672899163178,-0.548361749301861,
9.25586907860717));
#280471=CARTESIAN_POINT('Ctrl Pts',(-1.85630914401874,-0.613959354774945,
9.25977634392756));
#280472=CARTESIAN_POINT('Ctrl Pts',(-1.83247448589422,-0.678345972603016,
9.26368360924796));
#280473=CARTESIAN_POINT('Ctrl Pts',(-1.80865480073123,-0.742692142678599,
9.26758842001948));
#280474=CARTESIAN_POINT('Ctrl Pts',(-1.7814247307963,-0.805828373825665,
9.271493230791));
#280475=CARTESIAN_POINT('Ctrl Pts',(-1.75093629541242,-0.867374249910283,
9.27539804156252));
#280476=CARTESIAN_POINT('Ctrl Pts',(-1.72045655062073,-0.928902582618118,
9.27930173928519));
#280477=CARTESIAN_POINT('Ctrl Pts',(-1.68672050243156,-0.988841019529823,
9.28320543700786));
#280478=CARTESIAN_POINT('Ctrl Pts',(-1.64992731783472,-1.04683133591937,
9.28710913473053));
#280479=CARTESIAN_POINT('Ctrl Pts',(-1.61313199556873,-1.10482502152286,
9.29101305925646));
#280480=CARTESIAN_POINT('Ctrl Pts',(-1.57327944999038,-1.16086994783955,
9.29491698378238));
#280481=CARTESIAN_POINT('Ctrl Pts',(-1.53061262304348,-1.21463615876523,
9.29882090830831));
#280482=CARTESIAN_POINT('Ctrl Pts',(-1.48790030667198,-1.2684596927724,
9.30272899502049));
#280483=CARTESIAN_POINT('Ctrl Pts',(-1.44236802729647,-1.31999927675665,
9.30663708173266));
#280484=CARTESIAN_POINT('Ctrl Pts',(-1.39429890623535,-1.36895820245577,
9.31054516844483));
#280485=CARTESIAN_POINT('Ctrl Pts',(-1.34620104861037,-1.41794639665955,
9.3144555914798));
#280486=CARTESIAN_POINT('Ctrl Pts',(-1.29556369382531,-1.46435052975933,
9.31836601451477));
#280487=CARTESIAN_POINT('Ctrl Pts',(-1.24270462293738,-1.50791286887873,
9.32227643754975));
#280488=CARTESIAN_POINT('Ctrl Pts',(-1.18975402833414,-1.55155063473297,
9.32619363135156));
#280489=CARTESIAN_POINT('Ctrl Pts',(-1.13457443531577,-1.59233649370928,
9.33011082515338));
#280490=CARTESIAN_POINT('Ctrl Pts',(-1.07751355441331,-1.63005537944439,
9.33402801895519));
#280491=CARTESIAN_POINT('Ctrl Pts',(-1.05017051899833,-1.64812991338353,
9.33590510124268));
#280492=CARTESIAN_POINT('Ctrl Pts',(-1.0223958727625,-1.66550087107444,
9.33778218353017));
#280493=CARTESIAN_POINT('Ctrl Pts',(-0.994229725646667,-1.68214840386945,
9.33965926581765));
#280494=CARTESIAN_POINT('Ctrl Pts',(-0.935442307976532,-1.71689456420062,
9.34357704768472));
#280495=CARTESIAN_POINT('Ctrl Pts',(-0.874714461285793,-1.74862429952429,
9.3474948295518));
#280496=CARTESIAN_POINT('Ctrl Pts',(-0.812388281868093,-1.77711600057042,
9.35141261141887));
#280497=CARTESIAN_POINT('Ctrl Pts',(-0.750156083619173,-1.80556473919867,
9.35532448569266));
#280498=CARTESIAN_POINT('Ctrl Pts',(-0.686330779660388,-1.8307849308271,
9.35923635996645));
#280499=CARTESIAN_POINT('Ctrl Pts',(-0.621280717555777,-1.85259986775164,
9.36314823424024));
#280500=CARTESIAN_POINT('Ctrl Pts',(-0.556307294020607,-1.8743891034623,
9.36705549974904));
#280501=CARTESIAN_POINT('Ctrl Pts',(-0.490112442267491,-1.89278089641617,
9.37096276525785));
#280502=CARTESIAN_POINT('Ctrl Pts',(-0.423084542207245,-1.907646578941,
9.37487003076666));
#280503=CARTESIAN_POINT('Ctrl Pts',(-0.356098749147802,-1.92250292282765,
9.37877484172697));
#280504=CARTESIAN_POINT('Ctrl Pts',(-0.288281425102331,-1.93383744402462,
9.38267965268727));
#280505=CARTESIAN_POINT('Ctrl Pts',(-0.220034660137484,-1.94157172114197,
9.38658446364758));
#280506=CARTESIAN_POINT('Ctrl Pts',(-0.151807348605316,-1.94930379363849,
9.39048816155912));
#280507=CARTESIAN_POINT('Ctrl Pts',(-0.0831513277768723,-1.95343760390027,
9.39439185947066));
#280508=CARTESIAN_POINT('Ctrl Pts',(-0.0144755912376161,-1.95394638034372,
9.39829555738221));
#280509=CARTESIAN_POINT('Ctrl Pts',(0.0542041353306073,-1.95445518634685,
9.40219948209682));
#280510=CARTESIAN_POINT('Ctrl Pts',(0.122903087897137,-1.95133853930137,
9.40610340681144));
#280511=CARTESIAN_POINT('Ctrl Pts',(0.191212304539026,-1.94462177674551,
9.41000733152605));
#280512=CARTESIAN_POINT('Ctrl Pts',(0.25959434932033,-1.93789785308689,
9.41391541842532));
#280513=CARTESIAN_POINT('Ctrl Pts',(0.327585338355061,-1.92756620205989,
9.41782350532459));
#280514=CARTESIAN_POINT('Ctrl Pts',(0.394782474607588,-1.91370394725587,
9.42173159222386));
#280515=CARTESIAN_POINT('Ctrl Pts',(0.462019782474208,-1.89983340535539,
9.42564201544529));
#280516=CARTESIAN_POINT('Ctrl Pts',(0.528461817064993,-1.88242818378407,
9.42955243866672));
#280517=CARTESIAN_POINT('Ctrl Pts',(0.593719751138159,-1.86161565773079,
9.43346286188815));
#280518=CARTESIAN_POINT('Ctrl Pts',(0.659090677089639,-1.84076709550131,
9.43738005587349));
#280519=CARTESIAN_POINT('Ctrl Pts',(0.723272950577194,-1.81649962782296,
9.44129724985883));
#280520=CARTESIAN_POINT('Ctrl Pts',(0.785897379849404,-1.78898890671402,
9.44521444384417));
#280521=CARTESIAN_POINT('Ctrl Pts',(0.815906386758424,-1.77580604134623,
9.44709152444572));
#280522=CARTESIAN_POINT('Ctrl Pts',(0.845558037813433,-1.76187913176989,
9.44896860504728));
#280523=CARTESIAN_POINT('Ctrl Pts',(0.874813913746812,-1.74723112847585,
9.45084568564883));
#280524=CARTESIAN_POINT('Ctrl Pts',(0.935875823308645,-1.71665829399845,
9.45476346702694));
#280525=CARTESIAN_POINT('Ctrl Pts',(0.995454422971764,-1.68281990134536,
9.45868124840505));
#280526=CARTESIAN_POINT('Ctrl Pts',(1.05317806525755,-1.6458833381684,9.46259902978317));
#280527=CARTESIAN_POINT('Ctrl Pts',(1.11081466648952,-1.60900247136222,
9.46651090356768));
#280528=CARTESIAN_POINT('Ctrl Pts',(1.16660145045014,-1.56903296867654,
9.47042277735219));
#280529=CARTESIAN_POINT('Ctrl Pts',(1.2201902769734,-1.52618861481128,9.4743346511367));
#280530=CARTESIAN_POINT('Ctrl Pts',(1.27371596797137,-1.48339473790106,
9.47824191615812));
#280531=CARTESIAN_POINT('Ctrl Pts',(1.32504846188176,-1.43773304216034,
9.48214918117953));
#280532=CARTESIAN_POINT('Ctrl Pts',(1.37386913391756,-1.38946018398103,
9.48605644620094));
#280533=CARTESIAN_POINT('Ctrl Pts',(1.42265913676749,-1.3412176508505,9.48996125667529));
#280534=CARTESIAN_POINT('Ctrl Pts',(1.46894009876917,-1.29036755428633,
9.49386606714963));
#280535=CARTESIAN_POINT('Ctrl Pts',(1.51242819112343,-1.23720530498988,
9.49777087762398));
#280536=CARTESIAN_POINT('Ctrl Pts',(1.55590388741544,-1.18405820932551,
9.50167457505172));
#280537=CARTESIAN_POINT('Ctrl Pts',(1.59658798306032,-1.12860064989383,
9.50557827247946));
#280538=CARTESIAN_POINT('Ctrl Pts',(1.63423631380887,-1.07116183213761,
9.5094819699072));
#280539=CARTESIAN_POINT('Ctrl Pts',(1.67188683193616,-1.01371967716972,
9.51338589414087));
#280540=CARTESIAN_POINT('Ctrl Pts',(1.70650096743113,-0.954296448211486,
9.51728981837454));
#280541=CARTESIAN_POINT('Ctrl Pts',(1.73787836531886,-0.893249566110533,
9.52119374260821));
#280542=CARTESIAN_POINT('Ctrl Pts',(1.76928921640753,-0.832137598510083,
9.52510182903412));
#280543=CARTESIAN_POINT('Ctrl Pts',(1.79745621761414,-0.769398961467298,
9.52900991546003));
#280544=CARTESIAN_POINT('Ctrl Pts',(1.82222587580868,-0.705413961821904,
9.53291800188593));
#280545=CARTESIAN_POINT('Ctrl Pts',(1.84701034175947,-0.641390710769463,
9.53682842463763));
#280546=CARTESIAN_POINT('Ctrl Pts',(1.86839326946516,-0.576120081838372,
9.54073884738932));
#280547=CARTESIAN_POINT('Ctrl Pts',(1.88627096818667,-0.509997877030984,
9.54464927014102));
#280548=CARTESIAN_POINT('Ctrl Pts',(1.9041796215831,-0.443761183698757,
9.54856646366713));
#280549=CARTESIAN_POINT('Ctrl Pts',(1.91857082955659,-0.376670452434719,
9.55248365719323));
#280550=CARTESIAN_POINT('Ctrl Pts',(1.92939211486288,-0.309131148713524,
9.55640085071933));
#280551=CARTESIAN_POINT('Ctrl Pts',(1.9345775802555,-0.276766904340046,
9.55827793563955));
#280552=CARTESIAN_POINT('Ctrl Pts',(1.93894407361411,-0.24429972281665,
9.56015502055977));
#280553=CARTESIAN_POINT('Ctrl Pts',(1.94249005994572,-0.211774330389899,
9.56203210547999));
#280554=CARTESIAN_POINT('Ctrl Pts',(1.94989111050475,-0.143888543110564,
9.56594988719119));
#280555=CARTESIAN_POINT('Ctrl Pts',(1.95374388824642,-0.0754794566134533,
9.56986766890239));
#280556=CARTESIAN_POINT('Ctrl Pts',(1.95398763962716,-0.00695012117103305,
9.57378545061359));
#280557=CARTESIAN_POINT('Ctrl Pts',(1.9542310234568,0.0614758793399152,
9.57769732472768));
#280558=CARTESIAN_POINT('Ctrl Pts',(1.9508761796019,0.130021280932181,9.58160919884176));
#280559=CARTESIAN_POINT('Ctrl Pts',(1.9439140867026,0.198277642509685,9.58552107295584));
#280560=CARTESIAN_POINT('Ctrl Pts',(1.93696019618472,0.266453587936497,
9.58942833830012));
#280561=CARTESIAN_POINT('Ctrl Pts',(1.92640754657478,0.334340682531275,
9.59333560364439));
#280562=CARTESIAN_POINT('Ctrl Pts',(1.91229914225534,0.401532054174392,
9.59724286898867));
#280563=CARTESIAN_POINT('Ctrl Pts',(1.89819960086187,0.468681216072203,
9.60114767978155));
#280564=CARTESIAN_POINT('Ctrl Pts',(1.88054883659959,0.535135041591085,
9.60505249057444));
#280565=CARTESIAN_POINT('Ctrl Pts',(1.85944128135171,0.600494896901805,
9.60895730136732));
#280566=CARTESIAN_POINT('Ctrl Pts',(1.83833974273168,0.665836121635859,
9.61286099910883));
#280567=CARTESIAN_POINT('Ctrl Pts',(1.8137835202986,0.730083527240458,9.61676469685034));
#280568=CARTESIAN_POINT('Ctrl Pts',(1.78591694410828,0.792853497657011,
9.62066839459184));
#280569=CARTESIAN_POINT('Ctrl Pts',(1.75804874889923,0.855627114942712,
9.62457231913407));
#280570=CARTESIAN_POINT('Ctrl Pts',(1.72687002005523,0.916922677998517,
9.62847624367631));
#280571=CARTESIAN_POINT('Ctrl Pts',(1.6925725433236,0.976378095610029,9.63238016821854));
#280572=CARTESIAN_POINT('Ctrl Pts',(1.65823850022118,1.03589690181609,9.63628825494313));
#280573=CARTESIAN_POINT('Ctrl Pts',(1.62077931967228,1.09357122025362,9.64019634166771));
#280574=CARTESIAN_POINT('Ctrl Pts',(1.58043141874474,1.14906593833621,9.6441044283923));
#280575=CARTESIAN_POINT('Ctrl Pts',(1.54005939715703,1.20459383210343,9.64801485143748));
#280576=CARTESIAN_POINT('Ctrl Pts',(1.49679552824238,1.25793915013662,9.65192527448265));
#280577=CARTESIAN_POINT('Ctrl Pts',(1.45091624290589,1.30880023535751,9.65583569752783));
#280578=CARTESIAN_POINT('Ctrl Pts',(1.4049575191604,1.35974938480302,9.65975289133639));
#280579=CARTESIAN_POINT('Ctrl Pts',(1.35637468886931,1.408205369227,9.66367008514496));
#280580=CARTESIAN_POINT('Ctrl Pts',(1.30548006065421,1.45390433359086,9.66758727895352));
#280581=CARTESIAN_POINT('Ctrl Pts',(1.28109183753958,1.47580284386788,9.66946436107273));
#280582=CARTESIAN_POINT('Ctrl Pts',(1.25617324331868,1.49706888778729,9.67134144319194));
#280583=CARTESIAN_POINT('Ctrl Pts',(1.23076103348846,1.51767693480741,9.67321852531115));
#280584=CARTESIAN_POINT('Ctrl Pts',(1.17772152207824,1.56068935884959,9.6771363081071));
#280585=CARTESIAN_POINT('Ctrl Pts',(1.12231914613281,1.60100345598076,9.68105409090304));
#280586=CARTESIAN_POINT('Ctrl Pts',(1.06485969922456,1.63834972486566,9.68497187369899));
#280587=CARTESIAN_POINT('Ctrl Pts',(1.00748689488888,1.67563967965451,9.68888374890622));
#280588=CARTESIAN_POINT('Ctrl Pts',(0.948063584768635,1.70997042179073,
9.69279562411345));
#280589=CARTESIAN_POINT('Ctrl Pts',(0.886928130547235,1.74111300358248,
9.69670749932068));
#280590=CARTESIAN_POINT('Ctrl Pts',(0.825864702858087,1.77221889484496,
9.70061476576514));
#280591=CARTESIAN_POINT('Ctrl Pts',(0.763093573443617,1.80014386317943,
9.70452203220959));
#280592=CARTESIAN_POINT('Ctrl Pts',(0.698979982238847,1.82470353329777,
9.70842929865404));
#280593=CARTESIAN_POINT('Ctrl Pts',(0.63490666723961,1.84924777501314,9.71233411055082));
#280594=CARTESIAN_POINT('Ctrl Pts',(0.569493021733619,1.87043073654641,
9.71623892244759));
#280595=CARTESIAN_POINT('Ctrl Pts',(0.50312523483442,1.88811572687503,9.72014373434437));
#280596=CARTESIAN_POINT('Ctrl Pts',(0.436776365779002,1.90579567617546,
9.7240474331918));
#280597=CARTESIAN_POINT('Ctrl Pts',(0.369474370405364,1.9199795070017,9.72795113203924));
#280598=CARTESIAN_POINT('Ctrl Pts',(0.30161986072208,1.93058060168903,9.73185483088668));
#280599=CARTESIAN_POINT('Ctrl Pts',(0.233761408758226,1.94118231228959,
9.73575875653519));
#280600=CARTESIAN_POINT('Ctrl Pts',(0.16535086523266,1.94820080007547,9.73966268218371));
#280601=CARTESIAN_POINT('Ctrl Pts',(0.0967964727854304,1.95160099478769,
9.74356660783222));
#280602=CARTESIAN_POINT('Ctrl Pts',(0.0281689909856538,1.95500481462182,
9.74747469565602));
#280603=CARTESIAN_POINT('Ctrl Pts',(-0.0406021534803314,1.95478261821084,
9.75138278347983));
#280604=CARTESIAN_POINT('Ctrl Pts',(-0.109107201405195,1.95095146495281,
9.75529087130363));
#280605=CARTESIAN_POINT('Ctrl Pts',(-0.177653202756922,1.94711802136933,
9.75920129544561));
#280606=CARTESIAN_POINT('Ctrl Pts',(-0.245932301819509,1.93967138048742,
9.7631117195876));
#280607=CARTESIAN_POINT('Ctrl Pts',(-0.313541168509378,1.92868036119254,
9.76702214372958));
#280608=CARTESIAN_POINT('Ctrl Pts',(-0.381267097335567,1.91767031137308,
9.77093933861963));
#280609=CARTESIAN_POINT('Ctrl Pts',(-0.448319997089675,1.90310373898713,
9.77485653350969));
#280610=CARTESIAN_POINT('Ctrl Pts',(-0.514308861291142,1.88510010216896,
9.77877372839975));
#280611=CARTESIAN_POINT('Ctrl Pts',(-0.545929924096169,1.8764729779195,
9.78065080064727));
#280612=CARTESIAN_POINT('Ctrl Pts',(-0.577306919049007,1.86705735905819,
9.78252787289479));
#280613=CARTESIAN_POINT('Ctrl Pts',(-0.608398470454078,1.85687029734151,
9.78440494514231));
#280614=CARTESIAN_POINT('Ctrl Pts',(-0.673291997182021,1.83560811093022,
9.78832272449265));
#280615=CARTESIAN_POINT('Ctrl Pts',(-0.737198494728991,1.81089776173608,
9.79224050384299));
#280616=CARTESIAN_POINT('Ctrl Pts',(-0.799725743186057,1.78285017196777,
9.79615828319333));
#280617=CARTESIAN_POINT('Ctrl Pts',(-0.862158707222957,1.75484487497267,
9.80007015495037));
#280618=CARTESIAN_POINT('Ctrl Pts',(-0.923216104460824,1.72351252419629,
9.8039820267074));
#280619=CARTESIAN_POINT('Ctrl Pts',(-0.982522144707224,1.68901339105406,
9.80789389846443));
#280620=CARTESIAN_POINT('Ctrl Pts',(-1.04175831382631,1.65455490290033,
9.81180116146849));
#280621=CARTESIAN_POINT('Ctrl Pts',(-1.09924680053732,1.61693728822309,
9.81570842447254));
#280622=CARTESIAN_POINT('Ctrl Pts',(-1.1546347054922,1.57636756401321,9.8196156874766));
#280623=CARTESIAN_POINT('Ctrl Pts',(-1.20998781580716,1.53582332567334,
9.823520495941));
#280624=CARTESIAN_POINT('Ctrl Pts',(-1.26324256596937,1.49233094658935,
9.8274253044054));
#280625=CARTESIAN_POINT('Ctrl Pts',(-1.31407477610489,1.44614089313762,
9.8313301128698));
#280626=CARTESIAN_POINT('Ctrl Pts',(-1.36489249690147,1.39996400581302,
9.83523380829794));
#280627=CARTESIAN_POINT('Ctrl Pts',(-1.41328868452497,1.35109130130369,
9.83913750372606));
#280628=CARTESIAN_POINT('Ctrl Pts',(-1.45897342346685,1.29981250556279,
9.8430411991542));
#280629=CARTESIAN_POINT('Ctrl Pts',(-1.50466081686196,1.24853073033315,
9.84694512140155));
#280630=CARTESIAN_POINT('Ctrl Pts',(-1.5476361234311,1.1948429553569,9.85084904364891));
#280631=CARTESIAN_POINT('Ctrl Pts',(-1.58764861207919,1.13907325689045,
9.85475296589626));
#280632=CARTESIAN_POINT('Ctrl Pts',(-1.62770376064663,1.08324409871732,
9.85866105036931));
#280633=CARTESIAN_POINT('Ctrl Pts',(-1.66478949978036,1.02532898773864,
9.86256913484235));
#280634=CARTESIAN_POINT('Ctrl Pts',(-1.69869808581193,0.965681527864581,
9.8664772193154));
#280635=CARTESIAN_POINT('Ctrl Pts',(-1.73262694316917,0.905998409379368,
9.87038764013043));
#280636=CARTESIAN_POINT('Ctrl Pts',(-1.76337464704755,0.844581320891091,
9.87429806094546));
#280637=CARTESIAN_POINT('Ctrl Pts',(-1.79078043651937,0.781806515820568,
9.87820848176048));
#280638=CARTESIAN_POINT('Ctrl Pts',(-1.81823367859699,0.718923017363106,
9.88212567339514));
#280639=CARTESIAN_POINT('Ctrl Pts',(-1.84233328455078,0.654677570732816,
9.88604286502981));
#280640=CARTESIAN_POINT('Ctrl Pts',(-1.86296772943102,0.589463518038743,
9.88996005666447));
#280641=CARTESIAN_POINT('Ctrl Pts',(-1.87285567397083,0.558213201395993,
9.89183715943414));
#280642=CARTESIAN_POINT('Ctrl Pts',(-1.88194866833356,0.526740643156299,
9.89371426220381));
#280643=CARTESIAN_POINT('Ctrl Pts',(-1.89023861760682,0.495089859023457,
9.89559136497348));
#280644=CARTESIAN_POINT('Ctrl Pts',(-1.91241236797386,0.410431127932456,
9.90061219282851));
#280645=CARTESIAN_POINT('Ctrl Pts',(-1.92890876017623,0.324228031161974,
9.90563302068355));
#280646=CARTESIAN_POINT('Ctrl Pts',(-1.93955619828592,0.237145005620355,
9.91065384853858));
#280647=CARTESIAN_POINT('Ctrl Pts',(-1.94908248889442,0.159231595856335,
9.91514599629746));
#280648=CARTESIAN_POINT('Ctrl Pts',(-1.95392723381153,0.0806138670398988,
9.91963814405634));
#280649=CARTESIAN_POINT('Ctrl Pts',(-1.95399918605333,0.00178350859616108,
9.92413029181523));
#280650=CARTESIAN_POINT('',(-1.95093054978418,-0.000550606481354719,10.6241303078758));
#280651=CARTESIAN_POINT('Ctrl Pts',(-1.9535343393295,0.00178280253715055,
9.92413030787576));
#280652=CARTESIAN_POINT('Ctrl Pts',(-1.94919764294582,-0.481552375812319,
9.95167946685205));
#280653=CARTESIAN_POINT('Ctrl Pts',(-1.523943549881,-1.62193885960754,10.0162907657721));
#280654=CARTESIAN_POINT('Ctrl Pts',(0.388631330803288,-2.27693917494034,
10.1179642046358));
#280655=CARTESIAN_POINT('Ctrl Pts',(2.12415308786741,-0.907447137301165,
10.2291506244669));
#280656=CARTESIAN_POINT('Ctrl Pts',(1.91385514681522,1.29330245229283,10.3403370442982));
#280657=CARTESIAN_POINT('Ctrl Pts',(-0.0496108271125428,2.30933734912718,
10.4515234641293));
#280658=CARTESIAN_POINT('Ctrl Pts',(-1.68147873779689,1.37393834407351,
10.5461212186551));
#280659=CARTESIAN_POINT('Ctrl Pts',(-1.95001820365716,0.359852200961074,
10.6036568332373));
#280660=CARTESIAN_POINT('Ctrl Pts',(-1.95093054978418,-0.000550606481354719,
10.6241303078758));
#280661=CARTESIAN_POINT('',(1.56057659382855,1.17255425406022,11.046));
#280662=CARTESIAN_POINT('Ctrl Pts',(-1.95093054978418,-0.000550606481354719,
10.6241303078758));
#280663=CARTESIAN_POINT('Ctrl Pts',(-1.95166977968097,-0.292567552961119,
10.640718973181));
#280664=CARTESIAN_POINT('Ctrl Pts',(-1.75310453654278,-1.23604956259639,
10.69436977843));
#280665=CARTESIAN_POINT('Ctrl Pts',(-0.290505442625576,-2.29155305943217,
10.7850827236229));
#280666=CARTESIAN_POINT('Ctrl Pts',(1.76839371692331,-1.48603171255786,
10.8962691434539));
#280667=CARTESIAN_POINT('Ctrl Pts',(2.111645059346,0.208752628450599,10.983241568913));
#280668=CARTESIAN_POINT('Ctrl Pts',(1.69759382901609,0.992979671982257,
11.0331518544284));
#280669=CARTESIAN_POINT('Ctrl Pts',(1.56057659382855,1.17255425406022,11.046));
#280670=CARTESIAN_POINT('',(1.88426091070916,-0.517374932107736,11.0459974907899));
#280671=CARTESIAN_POINT('Origin',(0.,0.,11.046));
#280672=CARTESIAN_POINT('',(-1.95388960244062,-0.00113872704447003,10.7258697407189));
#280673=CARTESIAN_POINT('Ctrl Pts',(1.88426091070916,-0.517374932107736,
11.0459974907899));
#280674=CARTESIAN_POINT('Ctrl Pts',(1.86515675297054,-0.586951588078024,
11.0419101437675));
#280675=CARTESIAN_POINT('Ctrl Pts',(1.84221826837054,-0.655383383450449,
11.0378227967452));
#280676=CARTESIAN_POINT('Ctrl Pts',(1.81561644938194,-0.722255431778618,
11.0337354497228));
#280677=CARTESIAN_POINT('Ctrl Pts',(1.78893195159019,-0.78933531931215,
11.0296353991722));
#280678=CARTESIAN_POINT('Ctrl Pts',(1.75856152345182,-0.854845383446217,
11.0255353486216));
#280679=CARTESIAN_POINT('Ctrl Pts',(1.72472347046363,-0.918392590579804,
11.0214352980709));
#280680=CARTESIAN_POINT('Ctrl Pts',(1.69082799031288,-0.982047644810721,
11.0173282892515));
#280681=CARTESIAN_POINT('Ctrl Pts',(1.65345337053807,-1.04373284494727,
11.013221280432));
#280682=CARTESIAN_POINT('Ctrl Pts',(1.61286122882079,-1.10308415661122,
11.0091142716125));
#280683=CARTESIAN_POINT('Ctrl Pts',(1.57215179605288,-1.16260696397377,
11.0049953955853));
#280684=CARTESIAN_POINT('Ctrl Pts',(1.52820651784718,-1.21978207539512,
11.0008765195581));
#280685=CARTESIAN_POINT('Ctrl Pts',(1.48132746950652,-1.27427819885824,
10.9967576435308));
#280686=CARTESIAN_POINT('Ctrl Pts',(1.46404643467158,-1.29436711792273,
10.9952393012729));
#280687=CARTESIAN_POINT('Ctrl Pts',(1.44636708492743,-1.31409236689375,
10.993720959015));
#280688=CARTESIAN_POINT('Ctrl Pts',(1.42830572605192,-1.33343869485151,
10.992202616757));
#280689=CARTESIAN_POINT('Ctrl Pts',(1.38162613769539,-1.38343928625238,
10.9882784606582));
#280690=CARTESIAN_POINT('Ctrl Pts',(1.33222699407779,-1.43108308891436,
10.9843543045593));
#280691=CARTESIAN_POINT('Ctrl Pts',(1.2803753524773,-1.47606062096671,10.9804301484605));
#280692=CARTESIAN_POINT('Ctrl Pts',(1.22860156563048,-1.52097061967643,
10.9765118844453));
#280693=CARTESIAN_POINT('Ctrl Pts',(1.17438295715036,-1.56322197525663,
10.97259362043));
#280694=CARTESIAN_POINT('Ctrl Pts',(1.11802436066742,-1.60254096014867,
10.9686753564148));
#280695=CARTESIAN_POINT('Ctrl Pts',(1.06173221962825,-1.64181358191684,
10.9647617126348));
#280696=CARTESIAN_POINT('Ctrl Pts',(1.0033055027343,-1.67816042176417,10.9608480688548));
#280697=CARTESIAN_POINT('Ctrl Pts',(0.943081743355728,-1.71134824782951,
10.9569344250748));
#280698=CARTESIAN_POINT('Ctrl Pts',(0.882895921614319,-1.74451516740019,
10.9530232466739));
#280699=CARTESIAN_POINT('Ctrl Pts',(0.820915731556803,-1.77452678518832,
10.949112068273));
#280700=CARTESIAN_POINT('Ctrl Pts',(0.757505980477138,-1.80119423981462,
10.9452008898721));
#280701=CARTESIAN_POINT('Ctrl Pts',(0.694114617435391,-1.82785396121128,
10.9412908456642));
#280702=CARTESIAN_POINT('Ctrl Pts',(0.629294967989068,-1.85117125490152,
10.9373808014563));
#280703=CARTESIAN_POINT('Ctrl Pts',(0.563432998143645,-1.87100487882925,
10.9334707572484));
#280704=CARTESIAN_POINT('Ctrl Pts',(0.497567738156177,-1.89083949354788,
10.9295605177138));
#280705=CARTESIAN_POINT('Ctrl Pts',(0.43066052440524,-1.90718995407429,
10.9256502781792));
#280706=CARTESIAN_POINT('Ctrl Pts',(0.363111980267009,-1.91996502306333,
10.9217400386447));
#280707=CARTESIAN_POINT('Ctrl Pts',(0.295493257140132,-1.93275336460226,
10.9178257365998));
#280708=CARTESIAN_POINT('Ctrl Pts',(0.227232356321995,-1.94195880982462,
10.9139114345549));
#280709=CARTESIAN_POINT('Ctrl Pts',(0.158738590832598,-1.94754154250442,
10.90999713251));
#280710=CARTESIAN_POINT('Ctrl Pts',(0.0902047060866323,-1.9531275451911,
10.906080537718));
#280711=CARTESIAN_POINT('Ctrl Pts',(0.0214381751924879,-1.95508659739389,
10.9021639429259));
#280712=CARTESIAN_POINT('Ctrl Pts',(-0.0471508747100471,-1.95343103154784,
10.8982473481339));
#280713=CARTESIAN_POINT('Ctrl Pts',(-0.11585583910553,-1.95177266781969,
10.8943241343538));
#280714=CARTESIAN_POINT('Ctrl Pts',(-0.184382235370864,-1.94648753112932,
10.8904009205737));
#280715=CARTESIAN_POINT('Ctrl Pts',(-0.252325118724455,-1.93763981030033,
10.8864777067936));
#280716=CARTESIAN_POINT('Ctrl Pts',(-0.28342128150148,-1.93359037710698,
10.8846821266196));
#280717=CARTESIAN_POINT('Ctrl Pts',(-0.314395359941127,-1.92879539009223,
10.8828865464456));
#280718=CARTESIAN_POINT('Ctrl Pts',(-0.345209459210633,-1.92326452399858,
10.8810909662716));
#280719=CARTESIAN_POINT('Ctrl Pts',(-0.412565791002198,-1.9111746411031,
10.8771660196782));
#280720=CARTESIAN_POINT('Ctrl Pts',(-0.479414437377039,-1.89551908549188,
10.8732410730847));
#280721=CARTESIAN_POINT('Ctrl Pts',(-0.545350411357199,-1.87635522458636,
10.8693161264912));
#280722=CARTESIAN_POINT('Ctrl Pts',(-0.611189766467242,-1.85721944532544,
10.8653969312939));
#280723=CARTESIAN_POINT('Ctrl Pts',(-0.676118636925346,-1.83458570069962,
10.8614777360966));
#280724=CARTESIAN_POINT('Ctrl Pts',(-0.739741712477614,-1.80856246749198,
10.8575585408992));
#280725=CARTESIAN_POINT('Ctrl Pts',(-0.803293110238869,-1.78256855207282,
10.8536437610693));
#280726=CARTESIAN_POINT('Ctrl Pts',(-0.865541183529176,-1.75319291700574,
10.8497289812394));
#280727=CARTESIAN_POINT('Ctrl Pts',(-0.926107008533286,-1.72059344667633,
10.8458142014094));
#280728=CARTESIAN_POINT('Ctrl Pts',(-0.98663665358324,-1.68801345015648,
10.8419017601352));
#280729=CARTESIAN_POINT('Ctrl Pts',(-1.0454856136025,-1.6522136708149,10.8379893188609));
#280730=CARTESIAN_POINT('Ctrl Pts',(-1.10229756290302,-1.61339892240514,
10.8340768775867));
#280731=CARTESIAN_POINT('Ctrl Pts',(-1.15909486171909,-1.57459418341901,
10.8301654452403));
#280732=CARTESIAN_POINT('Ctrl Pts',(-1.21385578849959,-1.5327762953315,
10.826254012894));
#280733=CARTESIAN_POINT('Ctrl Pts',(-1.26625265023858,-1.48819361165265,
10.8223425805476));
#280734=CARTESIAN_POINT('Ctrl Pts',(-1.31865378746122,-1.44360729011214,
10.8184308290359));
#280735=CARTESIAN_POINT('Ctrl Pts',(-1.36869010521002,-1.39625604443166,
10.8145190775241));
#280736=CARTESIAN_POINT('Ctrl Pts',(-1.41606806015514,-1.34642758773298,
10.8106073260124));
#280737=CARTESIAN_POINT('Ctrl Pts',(-1.46349737566049,-1.2965451139824,
10.8066913339261));
#280738=CARTESIAN_POINT('Ctrl Pts',(-1.50826223907816,-1.24418042568486,
10.8027753418398));
#280739=CARTESIAN_POINT('Ctrl Pts',(-1.55010765966135,-1.18965635519641,
10.7988593497535));
#280740=CARTESIAN_POINT('Ctrl Pts',(-1.59197869446824,-1.13509890968821,
10.7949409606285));
#280741=CARTESIAN_POINT('Ctrl Pts',(-1.63092645233119,-1.0783798550431,
10.7910225715034));
#280742=CARTESIAN_POINT('Ctrl Pts',(-1.66673937701486,-1.01985089552744,
10.7871041823783));
#280743=CARTESIAN_POINT('Ctrl Pts',(-1.70261410256806,-0.961220935028945,
10.7831790314526));
#280744=CARTESIAN_POINT('Ctrl Pts',(-1.7353429648826,-0.900775266527879,
10.7792538805269));
#280745=CARTESIAN_POINT('Ctrl Pts',(-1.7647608287876,-0.838889275874307,
10.7753287296012));
#280746=CARTESIAN_POINT('Ctrl Pts',(-1.77812492871317,-0.81077538678439,
10.7735455916629));
#280747=CARTESIAN_POINT('Ctrl Pts',(-1.79080638760702,-0.782364507779672,
10.7717624537246));
#280748=CARTESIAN_POINT('Ctrl Pts',(-1.80279310312774,-0.753692926406397,
10.7699793157862));
#280749=CARTESIAN_POINT('Ctrl Pts',(-1.83203733004641,-0.683742302288633,
10.7656289588927));
#280750=CARTESIAN_POINT('Ctrl Pts',(-1.85724198247572,-0.612002710327624,
10.7612786019992));
#280751=CARTESIAN_POINT('Ctrl Pts',(-1.8782090960143,-0.538930971135593,
10.7569282451058));
#280752=CARTESIAN_POINT('Ctrl Pts',(-1.89910485491189,-0.466107907456626,
10.7525926932141));
#280753=CARTESIAN_POINT('Ctrl Pts',(-1.91579170679192,-0.39196200964791,
10.7482571413224));
#280754=CARTESIAN_POINT('Ctrl Pts',(-1.92812013154444,-0.316968071472601,
10.7439215894308));
#280755=CARTESIAN_POINT('Ctrl Pts',(-1.9403801743362,-0.242390101487888,
10.7396100855051));
#280756=CARTESIAN_POINT('Ctrl Pts',(-1.94832987646409,-0.166973753229426,
10.7352985815794));
#280757=CARTESIAN_POINT('Ctrl Pts',(-1.95187032663603,-0.0912043200609277,
10.7309870776538));
#280758=CARTESIAN_POINT('Ctrl Pts',(-1.95327104971236,-0.0612273430197019,
10.7292812993631));
#280759=CARTESIAN_POINT('Ctrl Pts',(-1.95398215067413,-0.0311952786312452,
10.7275755210725));
#280760=CARTESIAN_POINT('Ctrl Pts',(-1.95399966813507,-0.00113882749166742,
10.7258697427818));
#280761=CARTESIAN_POINT('',(-1.95399929720026,0.00165726911154443,10.0258696715299));
#280762=CARTESIAN_POINT('Ctrl Pts',(-1.95129684289216,-0.00113636086278679,
10.7258696921242));
#280763=CARTESIAN_POINT('Ctrl Pts',(-1.94942963316978,0.391854106201406,
10.7035356831831));
#280764=CARTESIAN_POINT('Ctrl Pts',(-1.64371581331279,1.43936972202558,
10.6441644574134));
#280765=CARTESIAN_POINT('Ctrl Pts',(0.0645886152005409,2.30833217918205,
10.5477560148154));
#280766=CARTESIAN_POINT('Ctrl Pts',(1.97414006873681,1.19827380577986,10.4366443643299));
#280767=CARTESIAN_POINT('Ctrl Pts',(2.07762111854432,-1.00830526181525,
10.3255327138444));
#280768=CARTESIAN_POINT('Ctrl Pts',(0.280201048116129,-2.29226437530736,
10.2144210633591));
#280769=CARTESIAN_POINT('Ctrl Pts',(-1.56609100264734,-1.56119761498329,
10.1145333894522));
#280770=CARTESIAN_POINT('Ctrl Pts',(-1.94902777514884,-0.451727225472274,
10.051682932374));
#280771=CARTESIAN_POINT('Ctrl Pts',(-1.95268202714777,0.00165579016441021,
10.0258696921242));
#280772=CARTESIAN_POINT('',(-1.95399999964781,3.70990612662463E-5,9.32586969217469));
#280773=CARTESIAN_POINT('Ctrl Pts',(-1.95399929720026,0.00165726911154443,
10.0258696715299));
#280774=CARTESIAN_POINT('Ctrl Pts',(-1.95392946016848,0.0839984592389699,
10.0211847229765));
#280775=CARTESIAN_POINT('Ctrl Pts',(-1.94865101160301,0.166113796242972,
10.0164997744231));
#280776=CARTESIAN_POINT('Ctrl Pts',(-1.93827214842649,0.24742085327267,
10.0118148258697));
#280777=CARTESIAN_POINT('Ctrl Pts',(-1.92775063089284,0.32984545138108,
10.0070654841056));
#280778=CARTESIAN_POINT('Ctrl Pts',(-1.9119876083715,0.411439382463031,
10.0023161423414));
#280779=CARTESIAN_POINT('Ctrl Pts',(-1.89114465504996,0.49161762954147,
9.99756680057726));
#280780=CARTESIAN_POINT('Ctrl Pts',(-1.88329047104473,0.521830944135401,
9.99577712118087));
#280781=CARTESIAN_POINT('Ctrl Pts',(-1.87471542987959,0.551843453374223,
9.99398744178449));
#280782=CARTESIAN_POINT('Ctrl Pts',(-1.86542991659206,0.581624643806756,
9.9921977623881));
#280783=CARTESIAN_POINT('Ctrl Pts',(-1.84510108849325,0.646824776759485,
9.98827960690498));
#280784=CARTESIAN_POINT('Ctrl Pts',(-1.82130956062044,0.711087059136883,
9.98436145142186));
#280785=CARTESIAN_POINT('Ctrl Pts',(-1.79416071012429,0.774017665332199,
9.98044329593874));
#280786=CARTESIAN_POINT('Ctrl Pts',(-1.76705273820747,0.836853515626944,
9.97653104010245));
#280787=CARTESIAN_POINT('Ctrl Pts',(-1.73659766970729,0.898361221218455,
9.97261878426615));
#280788=CARTESIAN_POINT('Ctrl Pts',(-1.70295045843072,0.95816268771572,
9.96870652842986));
#280789=CARTESIAN_POINT('Ctrl Pts',(-1.66934281055982,1.01789383784532,
9.96479887274196));
#280790=CARTESIAN_POINT('Ctrl Pts',(-1.63255071431331,1.07592230667678,
9.96089121705406));
#280791=CARTESIAN_POINT('Ctrl Pts',(-1.59277618877594,1.1318922265253,9.95698356136616));
#280792=CARTESIAN_POINT('Ctrl Pts',(-1.55302658987783,1.18782707010369,
9.95307835460058));
#280793=CARTESIAN_POINT('Ctrl Pts',(-1.51029855364633,1.24170552378917,
9.94917314783501));
#280794=CARTESIAN_POINT('Ctrl Pts',(-1.46483795145502,1.29319982059117,
9.94526794106944));
#280795=CARTESIAN_POINT('Ctrl Pts',(-1.41939024798578,1.34467950670634,
9.94136384234411));
#280796=CARTESIAN_POINT('Ctrl Pts',(-1.37121184308229,1.39377601027969,
9.93745974361878));
#280797=CARTESIAN_POINT('Ctrl Pts',(-1.32058835050876,1.44019526748998,
9.93355564489345));
#280798=CARTESIAN_POINT('Ctrl Pts',(-1.26996186003076,1.48661727363149,
9.92965131496884));
#280799=CARTESIAN_POINT('Ctrl Pts',(-1.21689035867317,1.53036138810924,
9.92574698504423));
#280800=CARTESIAN_POINT('Ctrl Pts',(-1.16169436477441,1.57117223844217,
9.92184265511962));
#280801=CARTESIAN_POINT('Ctrl Pts',(-1.10643958069217,1.61202655709969,
9.9179341666274));
#280802=CARTESIAN_POINT('Ctrl Pts',(-1.04905618441536,1.64994108355012,
9.91402567813517));
#280803=CARTESIAN_POINT('Ctrl Pts',(-0.989894830055331,1.68470300807879,
9.91011718964295));
#280804=CARTESIAN_POINT('Ctrl Pts',(-0.930698064328628,1.71948573955601,
9.90620636170261));
#280805=CARTESIAN_POINT('Ctrl Pts',(-0.869721659241525,1.75111188711872,
9.90229553376227));
#280806=CARTESIAN_POINT('Ctrl Pts',(-0.807339587395694,1.77941529459082,
9.89838470582192));
#280807=CARTESIAN_POINT('Ctrl Pts',(-0.744849809313426,1.80776756952448,
9.89446712561212));
#280808=CARTESIAN_POINT('Ctrl Pts',(-0.680949978412429,1.83278547520301,
9.89054954540231));
#280809=CARTESIAN_POINT('Ctrl Pts',(-0.616031852958404,1.85435184259639,
9.8866319651925));
#280810=CARTESIAN_POINT('Ctrl Pts',(-0.585398453399131,1.86452852506809,
9.88478334742923));
#280811=CARTESIAN_POINT('Ctrl Pts',(-0.554538496038118,1.87393739140249,
9.88293472966596));
#280812=CARTESIAN_POINT('Ctrl Pts',(-0.523493898671034,1.88257008848388,
9.88108611190269));
#280813=CARTESIAN_POINT('Ctrl Pts',(-0.457695228505216,1.90086699152254,
9.87716798763038));
#280814=CARTESIAN_POINT('Ctrl Pts',(-0.390805720697579,1.91574636522992,
9.87324986335807));
#280815=CARTESIAN_POINT('Ctrl Pts',(-0.323213364846653,1.92708306016749,
9.86933173908576));
#280816=CARTESIAN_POINT('Ctrl Pts',(-0.255722787104298,1.93840268472257,
9.86541951458233));
#280817=CARTESIAN_POINT('Ctrl Pts',(-0.187531942915477,1.94619013677017,
9.8615072900789));
#280818=CARTESIAN_POINT('Ctrl Pts',(-0.119042505200818,1.9503704473652,
9.85759506557547));
#280819=CARTESIAN_POINT('Ctrl Pts',(-0.0506336004842804,1.95454584256076,
9.85368744124367));
#280820=CARTESIAN_POINT('Ctrl Pts',(0.0180727118285098,1.95512249004676,
9.84977981691187));
#280821=CARTESIAN_POINT('Ctrl Pts',(0.0866678945075832,1.95207701591449,
9.84587219258007));
#280822=CARTESIAN_POINT('Ctrl Pts',(0.155220088415557,1.94903345038842,
9.84196701716614));
#280823=CARTESIAN_POINT('Ctrl Pts',(0.223660800552973,1.94237228795691,
9.8380618417522));
#280824=CARTESIAN_POINT('Ctrl Pts',(0.291581307004438,1.9321222376976,9.83415666633826));
#280825=CARTESIAN_POINT('Ctrl Pts',(0.359482542861863,1.92187509561092,
9.8302525989115));
#280826=CARTESIAN_POINT('Ctrl Pts',(0.426863379891022,1.90804116046147,
9.82634853148473));
#280827=CARTESIAN_POINT('Ctrl Pts',(0.493321843646891,1.89070081149314,
9.82244446405797));
#280828=CARTESIAN_POINT('Ctrl Pts',(0.559784244811242,1.87335943517581,
9.81854016533022));
#280829=CARTESIAN_POINT('Ctrl Pts',(0.625323688914603,1.85251135926445,
9.81463586660247));
#280830=CARTESIAN_POINT('Ctrl Pts',(0.689551766031441,1.8282872755568,9.81073156787472));
#280831=CARTESIAN_POINT('Ctrl Pts',(0.753848260189182,1.80403738786746,
9.80682311020936));
#280832=CARTESIAN_POINT('Ctrl Pts',(0.816830138475845,1.77640448941032,
9.80291465254399));
#280833=CARTESIAN_POINT('Ctrl Pts',(0.878128394929078,1.74556767901427,
9.79900619487863));
#280834=CARTESIAN_POINT('Ctrl Pts',(0.939463344701322,1.71471240961162,
9.79509539759886));
#280835=CARTESIAN_POINT('Ctrl Pts',(0.999112239694252,1.68064965530552,
9.79118460031908));
#280836=CARTESIAN_POINT('Ctrl Pts',(1.05673261311193,1.64360341456984,9.78727380303931));
#280837=CARTESIAN_POINT('Ctrl Pts',(1.11445248075737,1.60649320536441,9.78335625290925));
#280838=CARTESIAN_POINT('Ctrl Pts',(1.17013643709931,1.56638951518068,9.7794387027792));
#280839=CARTESIAN_POINT('Ctrl Pts',(1.22347351659946,1.52355786046338,9.77552115264914));
#280840=CARTESIAN_POINT('Ctrl Pts',(1.24864607779852,1.50334335941209,9.77367225557184));
#280841=CARTESIAN_POINT('Ctrl Pts',(1.27329641311365,1.48252178617763,9.77182335849455));
#280842=CARTESIAN_POINT('Ctrl Pts',(1.29739475006501,1.4611238354444,9.76997446141725));
#280843=CARTESIAN_POINT('Ctrl Pts',(1.34846286826111,1.41577825498361,9.76605636139788));
#280844=CARTESIAN_POINT('Ctrl Pts',(1.39725203878253,1.36766221144679,9.76213826137852));
#280845=CARTESIAN_POINT('Ctrl Pts',(1.44344663175065,1.31703372063425,9.75822016135916));
#280846=CARTESIAN_POINT('Ctrl Pts',(1.48957165964721,1.2664814719609,9.75430796166039));
#280847=CARTESIAN_POINT('Ctrl Pts',(1.53310953554373,1.21342464541315,9.75039576196162));
#280848=CARTESIAN_POINT('Ctrl Pts',(1.57377935816454,1.15815997678007,9.74648356226285));
#280849=CARTESIAN_POINT('Ctrl Pts',(1.61440135181701,1.10296030110531,9.74257596343183));
#280850=CARTESIAN_POINT('Ctrl Pts',(1.65216170069637,1.04555833430942,9.73866836460082));
#280851=CARTESIAN_POINT('Ctrl Pts',(1.68681912017229,0.986284571420027,
9.7347607657698));
#280852=CARTESIAN_POINT('Ctrl Pts',(1.72145481591177,0.927047962122052,
9.73085561627427));
#280853=CARTESIAN_POINT('Ctrl Pts',(1.75299119270281,0.865942307792211,
9.72695046677873));
#280854=CARTESIAN_POINT('Ctrl Pts',(1.78123061543365,0.803326518074594,
9.72304531728319));
#280855=CARTESIAN_POINT('Ctrl Pts',(1.80946202320625,0.740728500070822,
9.71914127615345));
#280856=CARTESIAN_POINT('Ctrl Pts',(1.83439813240783,0.676621645724216,
9.71523723502371));
#280857=CARTESIAN_POINT('Ctrl Pts',(1.85588837394989,0.611387228716484,
9.71133319389397));
#280858=CARTESIAN_POINT('Ctrl Pts',(1.87737988684293,0.546148952476197,
9.70742892180328));
#280859=CARTESIAN_POINT('Ctrl Pts',(1.89542497588251,0.479783449127808,
9.70352464971259));
#280860=CARTESIAN_POINT('Ctrl Pts',(1.90992269513095,0.412687894932391,
9.6996203776219));
#280861=CARTESIAN_POINT('Ctrl Pts',(1.92443585650675,0.345520874454898,
9.69571194692766));
#280862=CARTESIAN_POINT('Ctrl Pts',(1.93539400338419,0.277622732978139,
9.6918035162334));
#280863=CARTESIAN_POINT('Ctrl Pts',(1.94274738051021,0.209400610125006,
9.68789508553916));
#280864=CARTESIAN_POINT('Ctrl Pts',(1.95010515898673,0.141137653044288,
9.68398431546082));
#280865=CARTESIAN_POINT('Ctrl Pts',(1.95385384678693,0.0725508198725638,
9.68007354538249));
#280866=CARTESIAN_POINT('Ctrl Pts',(1.95399580425165,0.00404931684999055,
9.67616277530415));
#280867=CARTESIAN_POINT('Ctrl Pts',(1.95413800683621,-0.064570468631866,
9.67224525244694));
#280868=CARTESIAN_POINT('Ctrl Pts',(1.95066107432734,-0.133104138904127,
9.66832772958974));
#280869=CARTESIAN_POINT('Ctrl Pts',(1.94361933414002,-0.201146424171811,
9.66441020673253));
#280870=CARTESIAN_POINT('Ctrl Pts',(1.94029552286363,-0.233263444826869,
9.66256107479895));
#280871=CARTESIAN_POINT('Ctrl Pts',(1.93617822033419,-0.265271118839659,
9.66071194286538));
#280872=CARTESIAN_POINT('Ctrl Pts',(1.93127706196271,-0.297127767024027,
9.65886281093181));
#280873=CARTESIAN_POINT('Ctrl Pts',(1.92089200596725,-0.364628763757224,
9.65494468847634));
#280874=CARTESIAN_POINT('Ctrl Pts',(1.90694321368401,-0.431718450463748,
9.65102656602087));
#280875=CARTESIAN_POINT('Ctrl Pts',(1.88947618824516,-0.497991700788822,
9.6471084435654));
#280876=CARTESIAN_POINT('Ctrl Pts',(1.87203546493705,-0.564165155776617,
9.64319622108239));
#280877=CARTESIAN_POINT('Ctrl Pts',(1.85108714710729,-0.629524142503438,
9.63928399859937));
#280878=CARTESIAN_POINT('Ctrl Pts',(1.82672810542462,-0.693671701060218,
9.63537177611637));
#280879=CARTESIAN_POINT('Ctrl Pts',(1.80239770805064,-0.757743827155699,
9.63146415409794));
#280880=CARTESIAN_POINT('Ctrl Pts',(1.77466472600995,-0.820606896584117,
9.6275565320795));
#280881=CARTESIAN_POINT('Ctrl Pts',(1.74367588225073,-0.881878913262543,
9.62364891006107));
#280882=CARTESIAN_POINT('Ctrl Pts',(1.71270646072224,-0.943112527758108,
9.61974373714133));
#280883=CARTESIAN_POINT('Ctrl Pts',(1.6784854468909,-1.0027566296655,9.61583856422158));
#280884=CARTESIAN_POINT('Ctrl Pts',(1.64120711430444,-1.06045047407056,
9.61193339130183));
#280885=CARTESIAN_POINT('Ctrl Pts',(1.6039393601304,-1.1181279467863,9.60802932654672));
#280886=CARTESIAN_POINT('Ctrl Pts',(1.56361627629858,-1.17385584769113,
9.6041252617916));
#280887=CARTESIAN_POINT('Ctrl Pts',(1.52047645787945,-1.22730083558774,
9.60022119703648));
#280888=CARTESIAN_POINT('Ctrl Pts',(1.47733408551607,-1.28074898751064,
9.59631690115467));
#280889=CARTESIAN_POINT('Ctrl Pts',(1.43137495843991,-1.33191357696582,
9.59241260527286));
#280890=CARTESIAN_POINT('Ctrl Pts',(1.38287795279402,-1.38049432004489,
9.58850830939105));
#280891=CARTESIAN_POINT('Ctrl Pts',(1.33432929017605,-1.42912680928965,
9.58459985481736));
#280892=CARTESIAN_POINT('Ctrl Pts',(1.28323770233214,-1.47516961083117,
9.58069140024367));
#280893=CARTESIAN_POINT('Ctrl Pts',(1.22991820784531,-1.5183600370171,9.57678294566998));
#280894=CARTESIAN_POINT('Ctrl Pts',(1.17656679810194,-1.56157631553988,
9.5728721516268));
#280895=CARTESIAN_POINT('Ctrl Pts',(1.12098522577274,-1.60193653173919,
9.56896135758363));
#280896=CARTESIAN_POINT('Ctrl Pts',(1.06351852024582,-1.63922065540126,
9.56505056354045));
#280897=CARTESIAN_POINT('Ctrl Pts',(1.00595258855654,-1.67656915652283,
9.56113301683795));
#280898=CARTESIAN_POINT('Ctrl Pts',(0.946495453155029,-1.71083071894422,
9.55721547013546));
#280899=CARTESIAN_POINT('Ctrl Pts',(0.885517030936552,-1.74183110200769,
9.55329792343296));
#280900=CARTESIAN_POINT('Ctrl Pts',(0.856737722436668,-1.75646200840605,
9.55144900243744));
#280901=CARTESIAN_POINT('Ctrl Pts',(0.827619845882305,-1.77036719945058,
9.54960008144191));
#280902=CARTESIAN_POINT('Ctrl Pts',(0.798203626448538,-1.78353216139334,
9.54775116044638));
#280903=CARTESIAN_POINT('Ctrl Pts',(0.735866635916521,-1.81143051555908,
9.54383304408707));
#280904=CARTESIAN_POINT('Ctrl Pts',(0.671941682099769,-1.83611208857875,
9.53991492772776));
#280905=CARTESIAN_POINT('Ctrl Pts',(0.606793768634314,-1.85739530589117,
9.53599681136844));
#280906=CARTESIAN_POINT('Ctrl Pts',(0.541743956876402,-1.87864647428831,
9.53208459502779));
#280907=CARTESIAN_POINT('Ctrl Pts',(0.475475304134359,-1.89650929158128,
9.52817237868714));
#280908=CARTESIAN_POINT('Ctrl Pts',(0.40837382317573,-1.9108497639911,9.52426016234649));
#280909=CARTESIAN_POINT('Ctrl Pts',(0.341351249028786,-1.92517337297347,
9.52035254650814));
#280910=CARTESIAN_POINT('Ctrl Pts',(0.273498270409407,-1.93598276091421,
9.5164449306698));
#280911=CARTESIAN_POINT('Ctrl Pts',(0.205215377115653,-1.94319392984727,
9.51253731483146));
#280912=CARTESIAN_POINT('Ctrl Pts',(0.136975280478163,-1.95040057914293,
9.50863214811154));
#280913=CARTESIAN_POINT('Ctrl Pts',(0.0683062917338641,-1.95401343149313,
9.50472698139161));
#280914=CARTESIAN_POINT('Ctrl Pts',(-0.000383152612268429,-1.95399996243451,
9.50082181467169));
#280915=CARTESIAN_POINT('Ctrl Pts',(-0.0690531048552257,-1.95398649719803,
9.49691775612659));
#280916=CARTESIAN_POINT('Ctrl Pts',(-0.137743009527492,-1.95034875348325,
9.49301369758149));
#280917=CARTESIAN_POINT('Ctrl Pts',(-0.206043403666329,-1.94310630584268,
9.48910963903639));
#280918=CARTESIAN_POINT('Ctrl Pts',(-0.274347841289605,-1.9358634294385,
9.48520534936524));
#280919=CARTESIAN_POINT('Ctrl Pts',(-0.342262233732601,-1.92501547984492,
9.48130105969409));
#280920=CARTESIAN_POINT('Ctrl Pts',(-0.409383032875655,-1.91063380384456,
9.47739677002295));
#280921=CARTESIAN_POINT('Ctrl Pts',(-0.476575327105888,-1.8962368089089,
9.47348832161808));
#280922=CARTESIAN_POINT('Ctrl Pts',(-0.542971859168175,-1.87829867899792,
9.46957987321322));
#280923=CARTESIAN_POINT('Ctrl Pts',(-0.608181054045808,-1.85694151913832,
9.46567142480836));
#280924=CARTESIAN_POINT('Ctrl Pts',(-0.673429281264656,-1.8355715754995,
9.46176063691914));
#280925=CARTESIAN_POINT('Ctrl Pts',(-0.737488298079319,-1.81077870649935,
9.45784984902991));
#280926=CARTESIAN_POINT('Ctrl Pts',(-0.799986080817993,-1.78273337055698,
9.45393906114068));
#280927=CARTESIAN_POINT('Ctrl Pts',(-0.862591778313896,-1.75463960880675,
9.45002152050428));
#280928=CARTESIAN_POINT('Ctrl Pts',(-0.923630424102178,-1.72328239607513,
9.44610397986789));
#280929=CARTESIAN_POINT('Ctrl Pts',(-0.982754956533872,-1.68887793976004,
9.44218643923149));
#280930=CARTESIAN_POINT('Ctrl Pts',(-1.01066018500859,-1.6726399388062,
9.44033746280797));
#280931=CARTESIAN_POINT('Ctrl Pts',(-1.03813945426592,-1.65572375887166,
9.43848848638446));
#280932=CARTESIAN_POINT('Ctrl Pts',(-1.06515874540712,-1.63815531836353,
9.43663950996094));
#280933=CARTESIAN_POINT('Ctrl Pts',(-1.12238295685082,-1.60094708262117,
9.43272355904791));
#280934=CARTESIAN_POINT('Ctrl Pts',(-1.1777692421661,-1.56066262208641,
9.42880760813489));
#280935=CARTESIAN_POINT('Ctrl Pts',(-1.23096726891726,-1.51750966483063,
9.42489165722186));
#280936=CARTESIAN_POINT('Ctrl Pts',(-1.28408516591199,-1.47442170690219,
9.42098160472672));
#280937=CARTESIAN_POINT('Ctrl Pts',(-1.33502096627577,-1.42847413475499,
9.41707155223158));
#280938=CARTESIAN_POINT('Ctrl Pts',(-1.38345288580186,-1.37991815437239,
9.41316149973645));
#280939=CARTESIAN_POINT('Ctrl Pts',(-1.43182791638115,-1.33141920866056,
9.4092560400547));
#280940=CARTESIAN_POINT('Ctrl Pts',(-1.47770456085395,-1.28031828647394,
9.40535058037296));
#280941=CARTESIAN_POINT('Ctrl Pts',(-1.52079516373974,-1.22690589286457,
9.40144512069121));
#280942=CARTESIAN_POINT('Ctrl Pts',(-1.5638588372244,-1.17352687924241,
9.39754210172004));
#280943=CARTESIAN_POINT('Ctrl Pts',(-1.60413961432025,-1.11783964209058,
9.39363908274887));
#280944=CARTESIAN_POINT('Ctrl Pts',(-1.64138876046339,-1.06016929639773,
9.38973606377771));
#280945=CARTESIAN_POINT('Ctrl Pts',(-1.67862744266192,-1.00251515132597,
9.38583414123367));
#280946=CARTESIAN_POINT('Ctrl Pts',(-1.71283591744884,-0.942879417137435,
9.38193221868963));
#280947=CARTESIAN_POINT('Ctrl Pts',(-1.7438086567614,-0.881616338666651,
9.3780302961456));
#280948=CARTESIAN_POINT('Ctrl Pts',(-1.77478335054919,-0.820349394306968,
9.37412812737823));
#280949=CARTESIAN_POINT('Ctrl Pts',(-1.80252168363909,-0.757455342500285,
9.37022595861086));
#280950=CARTESIAN_POINT('Ctrl Pts',(-1.82686482955528,-0.693311542190061,
9.3663237898435));
#280951=CARTESIAN_POINT('Ctrl Pts',(-1.85123394068469,-0.629099323958101,
9.36241745889248));
#280952=CARTESIAN_POINT('Ctrl Pts',(-1.87220046275567,-0.563635158397182,
9.35851112794145));
#280953=CARTESIAN_POINT('Ctrl Pts',(-1.88965470883647,-0.497313866056611,
9.35460479699043));
#280954=CARTESIAN_POINT('Ctrl Pts',(-1.90711949726443,-0.430952515721802,
9.35069610661942));
#280955=CARTESIAN_POINT('Ctrl Pts',(-1.9210676880021,-0.363733490610373,
9.34678741624842));
#280956=CARTESIAN_POINT('Ctrl Pts',(-1.93144082198622,-0.296061397627586,
9.34287872587741));
#280957=CARTESIAN_POINT('Ctrl Pts',(-1.94183178681567,-0.228272980048507,
9.33896331668318));
#280958=CARTESIAN_POINT('Ctrl Pts',(-1.94863538206911,-0.160030430071143,
9.33504790748895));
#280959=CARTESIAN_POINT('Ctrl Pts',(-1.95184512111298,-0.0917421559996565,
9.33113249829473));
#280960=CARTESIAN_POINT('Ctrl Pts',(-1.95328321978465,-0.061146124705292,
9.32937822958805));
#280961=CARTESIAN_POINT('Ctrl Pts',(-1.95400058020809,-0.0305408923189653,
9.32762396088137));
#280962=CARTESIAN_POINT('Ctrl Pts',(-1.95399999964781,3.70990612790232E-5,
9.32586969217469));
#280963=CARTESIAN_POINT('',(-1.95399927652111,-0.00168147404713564,8.62586971137284));
#280964=CARTESIAN_POINT('Ctrl Pts',(-1.9539999996478,3.7099940636846E-5,
9.32586969212423));
#280965=CARTESIAN_POINT('Ctrl Pts',(-1.95399996193804,0.00202321828658315,
9.32575574790799));
#280966=CARTESIAN_POINT('Ctrl Pts',(-1.95399689608245,0.00400933322525912,
9.32564180369175));
#280967=CARTESIAN_POINT('Ctrl Pts',(-1.95399080210547,0.00599543886719613,
9.32552785947551));
#280968=CARTESIAN_POINT('Ctrl Pts',(-1.95378125295234,0.0742902087533993,
9.32160974260204));
#280969=CARTESIAN_POINT('Ctrl Pts',(-1.94998647820361,0.142709361266959,
9.31769162572858));
#280970=CARTESIAN_POINT('Ctrl Pts',(-1.94259109676834,0.210845513958356,
9.31377350885511));
#280971=CARTESIAN_POINT('Ctrl Pts',(-1.93520685155423,0.278879064874356,
9.30986129201755));
#280972=CARTESIAN_POINT('Ctrl Pts',(-1.92423281289038,0.346629976652652,
9.30594907517999));
#280973=CARTESIAN_POINT('Ctrl Pts',(-1.90970561062772,0.413691286755018,
9.30203685834243));
#280974=CARTESIAN_POINT('Ctrl Pts',(-1.89519549147666,0.480673736810946,
9.29812924203536));
#280975=CARTESIAN_POINT('Ctrl Pts',(-1.87714061055141,0.546967717256504,
9.29422162572828));
#280976=CARTESIAN_POINT('Ctrl Pts',(-1.85562912332395,0.612173632780749,
9.29031400942121));
#280977=CARTESIAN_POINT('Ctrl Pts',(-1.83413111862874,0.677338679868087,
9.28640884225037));
#280978=CARTESIAN_POINT('Ctrl Pts',(-1.80918095895894,0.741416548748044,
9.28250367507953));
#280979=CARTESIAN_POINT('Ctrl Pts',(-1.78091698643134,0.804021571501862,
9.2785985079087));
#280980=CARTESIAN_POINT('Ctrl Pts',(-1.75266103454561,0.866608828442106,
9.27469444893124));
#280981=CARTESIAN_POINT('Ctrl Pts',(-1.72109333892136,0.927723620876592,
9.27079038995378));
#280982=CARTESIAN_POINT('Ctrl Pts',(-1.68640015220877,0.987000773368607,
9.26688633097632));
#280983=CARTESIAN_POINT('Ctrl Pts',(-1.65170491178014,1.04628143486198,
9.26298204089215));
#280984=CARTESIAN_POINT('Ctrl Pts',(-1.61388406360739,1.10372381722284,
9.25907775080797));
#280985=CARTESIAN_POINT('Ctrl Pts',(-1.57316861808235,1.15898943009886,
9.2551734607238));
#280986=CARTESIAN_POINT('Ctrl Pts',(-1.5324098040119,1.21431390980565,9.25126501193819));
#280987=CARTESIAN_POINT('Ctrl Pts',(-1.48875053175819,1.26745659602186,
9.24735656315258));
#280988=CARTESIAN_POINT('Ctrl Pts',(-1.44246315346738,1.31811078854887,
9.24344811436696));
#280989=CARTESIAN_POINT('Ctrl Pts',(-1.39614806910291,1.36879530097824,
9.23953732611487));
#280990=CARTESIAN_POINT('Ctrl Pts',(-1.34720209849604,1.41698801013024,
9.23562653786278));
#280991=CARTESIAN_POINT('Ctrl Pts',(-1.29593362662677,1.46241992443279,
9.23171574961069));
#280992=CARTESIAN_POINT('Ctrl Pts',(-1.24457663004418,1.5079302855281,9.22779820864301));
#280993=CARTESIAN_POINT('Ctrl Pts',(-1.19088951303049,1.5506700313444,9.22388066767533));
#280994=CARTESIAN_POINT('Ctrl Pts',(-1.13521209408202,1.59041173959762,
9.21996312670766));
#280995=CARTESIAN_POINT('Ctrl Pts',(-1.10893386970745,1.60916874281778,
9.21811415413513));
#280996=CARTESIAN_POINT('Ctrl Pts',(-1.08221268097153,1.62725855388008,
9.2162651815626));
#280997=CARTESIAN_POINT('Ctrl Pts',(-1.05508614414225,1.6446608247414,9.21441620899007));
#280998=CARTESIAN_POINT('Ctrl Pts',(-0.99760291608811,1.68153758165571,
9.21049809320841));
#280999=CARTESIAN_POINT('Ctrl Pts',(-0.938070067537558,1.71547013168315,
9.20657997742674));
#281000=CARTESIAN_POINT('Ctrl Pts',(-0.876821466214148,1.74622453206513,
9.20266186164508));
#281001=CARTESIAN_POINT('Ctrl Pts',(-0.815665095345652,1.77693262131058,
9.19874964591));
#281002=CARTESIAN_POINT('Ctrl Pts',(-0.752798535366085,1.80447184003791,
9.19483743017492));
#281003=CARTESIAN_POINT('Ctrl Pts',(-0.688583519414288,1.82865216396969,
9.19092521443984));
#281004=CARTESIAN_POINT('Ctrl Pts',(-0.624444016629962,1.85280405323049,
9.18701759924557));
#281005=CARTESIAN_POINT('Ctrl Pts',(-0.558959665258295,1.8736047196763,
9.18310998405131));
#281006=CARTESIAN_POINT('Ctrl Pts',(-0.492513964600165,1.89091141904475,
9.17920236885705));
#281007=CARTESIAN_POINT('Ctrl Pts',(-0.426109909535906,1.90820727124376,
9.17529720280477));
#281008=CARTESIAN_POINT('Ctrl Pts',(-0.358746175356759,1.92201337669609,
9.1713920367525));
#281009=CARTESIAN_POINT('Ctrl Pts',(-0.290821790346487,1.9322367055461,
9.16748687070022));
#281010=CARTESIAN_POINT('Ctrl Pts',(-0.222916680733751,1.94245713324762,
9.16358281284536));
#281011=CARTESIAN_POINT('Ctrl Pts',(-0.154451722304109,1.94909672951791,
9.1596787549905));
#281012=CARTESIAN_POINT('Ctrl Pts',(-0.085834722571209,1.95211382875106,
9.15577469713565));
#281013=CARTESIAN_POINT('Ctrl Pts',(-0.0172136609901176,1.95513110658425,
9.15187040817639));
#281014=CARTESIAN_POINT('Ctrl Pts',(0.0515589682466065,1.95452544260284,
9.14796611921714));
#281015=CARTESIAN_POINT('Ctrl Pts',(0.120073490884842,1.95030724676568,
9.14406183025789));
#281016=CARTESIAN_POINT('Ctrl Pts',(0.188660992684123,1.94608455786076,
9.14015338259298));
#281017=CARTESIAN_POINT('Ctrl Pts',(0.256989347325235,1.93824168809354,
9.13624493492807));
#281018=CARTESIAN_POINT('Ctrl Pts',(0.324653155537779,1.92684102317741,
9.13233648726316));
#281019=CARTESIAN_POINT('Ctrl Pts',(0.392357465063601,1.91543353420106,
9.128425700131));
#281020=CARTESIAN_POINT('Ctrl Pts',(0.459395956391263,1.90046411903233,
9.12451491299884));
#281021=CARTESIAN_POINT('Ctrl Pts',(0.525375357239391,1.88204589051531,
9.12060412586668));
#281022=CARTESIAN_POINT('Ctrl Pts',(0.591468684253714,1.86359585937299,
9.11668658600596));
#281023=CARTESIAN_POINT('Ctrl Pts',(0.656498805063163,1.84168528654545,
9.11276904614524));
#281024=CARTESIAN_POINT('Ctrl Pts',(0.720090312766324,1.81647624302111,
9.10885150628451));
#281025=CARTESIAN_POINT('Ctrl Pts',(0.750103942494326,1.80457819365156,
9.10700252369122));
#281026=CARTESIAN_POINT('Ctrl Pts',(0.779797435246854,1.79194605366362,
9.10515354109793));
#281027=CARTESIAN_POINT('Ctrl Pts',(0.809133289056376,1.77860038247517,
9.10330455850463));
#281028=CARTESIAN_POINT('Ctrl Pts',(0.871297889362895,1.7503200289992,9.09938644299205));
#281029=CARTESIAN_POINT('Ctrl Pts',(0.93210127792186,1.71872057975743,9.09546832747948));
#281030=CARTESIAN_POINT('Ctrl Pts',(0.991165798830189,1.6839555692563,9.0915502119669));
#281031=CARTESIAN_POINT('Ctrl Pts',(1.05014137802159,1.64924290929786,9.0876379965093));
#281032=CARTESIAN_POINT('Ctrl Pts',(1.1073828657791,1.611374396046,9.0837257810517));
#281033=CARTESIAN_POINT('Ctrl Pts',(1.1625343808032,1.57055079938553,9.07981356559411));
#281034=CARTESIAN_POINT('Ctrl Pts',(1.21762104065478,1.52977520904733,9.07590595068843));
#281035=CARTESIAN_POINT('Ctrl Pts',(1.27062221530796,1.48605172799656,9.07199833578276));
#281036=CARTESIAN_POINT('Ctrl Pts',(1.32120993095599,1.4396250617238,9.06809072087708));
#281037=CARTESIAN_POINT('Ctrl Pts',(1.37176594009198,1.39322749397099,9.06418555512013));
#281038=CARTESIAN_POINT('Ctrl Pts',(1.41991112929024,1.34413043370474,9.06028038936318));
#281039=CARTESIAN_POINT('Ctrl Pts',(1.46535086112881,1.29261860337419,9.05637522360622));
#281040=CARTESIAN_POINT('Ctrl Pts',(1.5107776981295,1.24112139101507,9.05247116605298));
#281041=CARTESIAN_POINT('Ctrl Pts',(1.55350027665158,1.18721113765168,9.04856710849973));
#281042=CARTESIAN_POINT('Ctrl Pts',(1.59326234360062,1.13120780781617,9.04466305094648));
#281043=CARTESIAN_POINT('Ctrl Pts',(1.63302676424328,1.07520116289444,9.04075876229471));
#281044=CARTESIAN_POINT('Ctrl Pts',(1.66983004272211,1.01710159807387,9.03685447364293));
#281045=CARTESIAN_POINT('Ctrl Pts',(1.70345865811394,0.957258899199503,
9.03295018499115));
#281046=CARTESIAN_POINT('Ctrl Pts',(1.7371230934199,0.897352458172525,9.02904173764052));
#281047=CARTESIAN_POINT('Ctrl Pts',(1.767605875719,0.835699607288608,9.02513329028989));
#281048=CARTESIAN_POINT('Ctrl Pts',(1.79473946456196,0.772674740329891,
9.02122484293926));
#281049=CARTESIAN_POINT('Ctrl Pts',(1.82188929464314,0.709612148841472,
9.01731405612572));
#281050=CARTESIAN_POINT('Ctrl Pts',(1.84568577109271,0.645176368338531,
9.01340326931219));
#281051=CARTESIAN_POINT('Ctrl Pts',(1.86601054510086,0.579759127200589,
9.00949248249866));
#281052=CARTESIAN_POINT('Ctrl Pts',(1.88637041373818,0.514228930621264,
9.00557494295996));
#281053=CARTESIAN_POINT('Ctrl Pts',(1.9032464948483,0.447714367617182,9.00165740342125));
#281054=CARTESIAN_POINT('Ctrl Pts',(1.91657125858195,0.380618721002536,
8.99773986388255));
#281055=CARTESIAN_POINT('Ctrl Pts',(1.92286022946874,0.348951175023886,
8.99589087859476));
#281056=CARTESIAN_POINT('Ctrl Pts',(1.92835885313605,0.31715427767523,8.99404189330698));
#281057=CARTESIAN_POINT('Ctrl Pts',(1.9330640536675,0.285270686223748,8.99219290801919));
#281058=CARTESIAN_POINT('Ctrl Pts',(1.94303466914674,0.217707353197879,
8.98827479205196));
#281059=CARTESIAN_POINT('Ctrl Pts',(1.94947863363781,0.149486727575227,
8.98435667608473));
#281060=CARTESIAN_POINT('Ctrl Pts',(1.95232002632467,0.0810093501494835,
8.98043856011751));
#281061=CARTESIAN_POINT('Ctrl Pts',(1.95515714033493,0.0126350885491758,
8.97652634419752));
#281062=CARTESIAN_POINT('Ctrl Pts',(1.95440242879606,-0.0559946700335427,
8.97261412827754));
#281063=CARTESIAN_POINT('Ctrl Pts',(1.95003146360188,-0.124472048921536,
8.96870191235756));
#281064=CARTESIAN_POINT('Ctrl Pts',(1.94566563841341,-0.19286890231836,
8.96479429698032));
#281065=CARTESIAN_POINT('Ctrl Pts',(1.93769203630091,-0.261113243337137,
8.96088668160308));
#281066=CARTESIAN_POINT('Ctrl Pts',(1.92613827731413,-0.328796801482873,
8.95697906622584));
#281067=CARTESIAN_POINT('Ctrl Pts',(1.9145917597799,-0.396437938172902,
8.9530738999919));
#281068=CARTESIAN_POINT('Ctrl Pts',(1.89946961914804,-0.463518505430738,
8.94916873375795));
#281069=CARTESIAN_POINT('Ctrl Pts',(1.88085117725033,-0.529636525398369,
8.94526356752401));
#281070=CARTESIAN_POINT('Ctrl Pts',(1.86223801885084,-0.595735782547756,
8.94135950948908));
#281071=CARTESIAN_POINT('Ctrl Pts',(1.84013066208068,-0.660872561411314,
8.93745545145414));
#281072=CARTESIAN_POINT('Ctrl Pts',(1.81465885824272,-0.724658007753471,
8.93355139341921));
#281073=CARTESIAN_POINT('Ctrl Pts',(1.78918554658959,-0.788447229904536,
8.92964710428176));
#281074=CARTESIAN_POINT('Ctrl Pts',(1.76034757726571,-0.850884504869678,
8.92574281514431));
#281075=CARTESIAN_POINT('Ctrl Pts',(1.72832293633162,-0.911600695343118,
8.92183852600686));
#281076=CARTESIAN_POINT('Ctrl Pts',(1.69626418395759,-0.972381558413157,
8.91793007816784));
#281077=CARTESIAN_POINT('Ctrl Pts',(1.66101221587393,-1.03143724251754,
8.91402163032883));
#281078=CARTESIAN_POINT('Ctrl Pts',(1.62279063585553,-1.08842388442169,
8.91011318248981));
#281079=CARTESIAN_POINT('Ctrl Pts',(1.58454617768734,-1.14544463660933,
8.90620239518563));
#281080=CARTESIAN_POINT('Ctrl Pts',(1.54332886520718,-1.20039348829709,
8.90229160788145));
#281081=CARTESIAN_POINT('Ctrl Pts',(1.49940355228453,-1.25295849388419,
8.89838082057726));
#281082=CARTESIAN_POINT('Ctrl Pts',(1.45540239389377,-1.30561426302401,
8.89446328054956));
#281083=CARTESIAN_POINT('Ctrl Pts',(1.40868423744711,-1.35587761076023,
8.89054574052185));
#281084=CARTESIAN_POINT('Ctrl Pts',(1.3595512142975,-1.40347301210326,8.88662820049415));
#281085=CARTESIAN_POINT('Ctrl Pts',(1.33636165529235,-1.4259368520436,8.88477921950735));
#281086=CARTESIAN_POINT('Ctrl Pts',(1.31263464328404,-1.44780695906798,
8.88293023852055));
#281087=CARTESIAN_POINT('Ctrl Pts',(1.28840434253463,-1.46905760613323,
8.88108125753375));
#281088=CARTESIAN_POINT('Ctrl Pts',(1.23705869622743,-1.51408916472988,
8.87716314175142));
#281089=CARTESIAN_POINT('Ctrl Pts',(1.18324754855695,-1.55651484513038,
8.87324502596909));
#281090=CARTESIAN_POINT('Ctrl Pts',(1.12726617493087,-1.59605356139972,
8.86932691018676));
#281091=CARTESIAN_POINT('Ctrl Pts',(1.07136910020881,-1.63553273875044,
8.86541469445377));
#281092=CARTESIAN_POINT('Ctrl Pts',(1.01330868391549,-1.67213329834028,
8.86150247872078));
#281093=CARTESIAN_POINT('Ctrl Pts',(0.953414300781563,-1.70561342955114,
8.85759026298778));
#281094=CARTESIAN_POINT('Ctrl Pts',(0.893590350061986,-1.73905419001719,
8.8536826477997));
#281095=CARTESIAN_POINT('Ctrl Pts',(0.831937142946086,-1.76938157081715,
8.84977503261162));
#281096=CARTESIAN_POINT('Ctrl Pts',(0.768812623306882,-1.79639726960491,
8.84586741742354));
#281097=CARTESIAN_POINT('Ctrl Pts',(0.705727667714937,-1.82339603598052,
8.84196225137998));
#281098=CARTESIAN_POINT('Ctrl Pts',(0.641173680069429,-1.8470870446482,
8.83805708533643));
#281099=CARTESIAN_POINT('Ctrl Pts',(0.575531368650073,-1.8673188382544,
8.83415191929288));
#281100=CARTESIAN_POINT('Ctrl Pts',(0.509907685070244,-1.88754489052401,
8.83024786144928));
#281101=CARTESIAN_POINT('Ctrl Pts',(0.443196760660883,-1.90431353166343,
8.82634380360568));
#281102=CARTESIAN_POINT('Ctrl Pts',(0.375795639602714,-1.91752278663269,
8.82243974576208));
#281103=CARTESIAN_POINT('Ctrl Pts',(0.308390528715172,-1.93073282352772,
8.81853545681662));
#281104=CARTESIAN_POINT('Ctrl Pts',(0.240295623253851,-1.94038296385983,
8.81463116787115));
#281105=CARTESIAN_POINT('Ctrl Pts',(0.171917574008792,-1.94642244842864,
8.81072687892569));
#281106=CARTESIAN_POINT('Ctrl Pts',(0.103466691034717,-1.9524683660295,
8.80681843127833));
#281107=CARTESIAN_POINT('Ctrl Pts',(0.0347325533016588,-1.9548959092115,
8.80290998363097));
#281108=CARTESIAN_POINT('Ctrl Pts',(-0.0338746698053916,-1.95370635120675,
8.79900153598361));
#281109=CARTESIAN_POINT('Ctrl Pts',(-0.10252295888464,-1.95251608117265,
8.79509074887118));
#281110=CARTESIAN_POINT('Ctrl Pts',(-0.171043691411102,-1.94770443551453,
8.79117996175874));
#281111=CARTESIAN_POINT('Ctrl Pts',(-0.239031129806031,-1.93932465538487,
8.78726917464631));
#281112=CARTESIAN_POINT('Ctrl Pts',(-0.30713596157698,-1.93093040595466,
8.78335163480847));
#281113=CARTESIAN_POINT('Ctrl Pts',(-0.374705177301888,-1.91895581133413,
8.77943409497064));
#281114=CARTESIAN_POINT('Ctrl Pts',(-0.441343409147208,-1.90350518654463,
8.7755165551328));
#281115=CARTESIAN_POINT('Ctrl Pts',(-0.472795019748818,-1.8962128706927,
8.77366757243798));
#281116=CARTESIAN_POINT('Ctrl Pts',(-0.50403946831885,-1.88814695237618,
8.77181858974315));
#281117=CARTESIAN_POINT('Ctrl Pts',(-0.535036607739613,-1.87932217258736,
8.76996960704832));
#281118=CARTESIAN_POINT('Ctrl Pts',(-0.600721581909144,-1.86062188464751,
8.76605149128606));
#281119=CARTESIAN_POINT('Ctrl Pts',(-0.665555182560461,-1.83843670633144,
8.76213337552379));
#281120=CARTESIAN_POINT('Ctrl Pts',(-0.729141090117285,-1.81286217642229,
8.75821525976153));
#281121=CARTESIAN_POINT('Ctrl Pts',(-0.792631247554809,-1.78732615762958,
8.75430304404954));
#281122=CARTESIAN_POINT('Ctrl Pts',(-0.854876988018642,-1.75841109858282,
8.75039082833756));
#281123=CARTESIAN_POINT('Ctrl Pts',(-0.915496483997269,-1.726262490987,
8.74647861262558));
#281124=CARTESIAN_POINT('Ctrl Pts',(-0.976044694849279,-1.69415168835023,
8.7425709974598));
#281125=CARTESIAN_POINT('Ctrl Pts',(-1.03497002672235,-1.65881511829838,
8.73866338229403));
#281126=CARTESIAN_POINT('Ctrl Pts',(-1.09191170032944,-1.6204458765055,
8.73475576712825));
#281127=CARTESIAN_POINT('Ctrl Pts',(-1.14881768505016,-1.5821006831015,
8.7308506011078));
#281128=CARTESIAN_POINT('Ctrl Pts',(-1.20374207078221,-1.54072686271804,
8.72694543508734));
#281129=CARTESIAN_POINT('Ctrl Pts',(-1.25635107871759,-1.49656204916641,
8.72304026906689));
#281130=CARTESIAN_POINT('Ctrl Pts',(-1.30894515736708,-1.45240976862298,
8.71913621124715));
#281131=CARTESIAN_POINT('Ctrl Pts',(-1.35922478603156,-1.40546838332545,
8.7152321534274));
#281132=CARTESIAN_POINT('Ctrl Pts',(-1.40688888954281,-1.35601609595204,
8.71132809560766));
#281133=CARTESIAN_POINT('Ctrl Pts',(-1.45455581453592,-1.30656088124502,
8.70742380668678));
#281134=CARTESIAN_POINT('Ctrl Pts',(-1.4996065674896,-1.25459482530796,
8.70351951776591));
#281135=CARTESIAN_POINT('Ctrl Pts',(-1.54177788401154,-1.20043198739992,
8.69961522884503));
#281136=CARTESIAN_POINT('Ctrl Pts',(-1.58399411982558,-1.14621145728451,
8.6957067812232));
#281137=CARTESIAN_POINT('Ctrl Pts',(-1.62332449552704,-1.08978986428043,
8.69179833360136));
#281138=CARTESIAN_POINT('Ctrl Pts',(-1.65954754646575,-1.03151245315775,
8.68788988597952));
#281139=CARTESIAN_POINT('Ctrl Pts',(-1.69579227929716,-0.973200159148551,
8.68397909889318));
#281140=CARTESIAN_POINT('Ctrl Pts',(-1.72892574844505,-0.913030267195515,
8.68006831180683));
#281141=CARTESIAN_POINT('Ctrl Pts',(-1.7587725482376,-0.851372494015285,
8.67615752472049));
#281142=CARTESIAN_POINT('Ctrl Pts',(-1.78867088426062,-0.789608256851292,
8.67223998490937));
#281143=CARTESIAN_POINT('Ctrl Pts',(-1.8152710338404,-0.726351464104802,
8.66832244509824));
#281144=CARTESIAN_POINT('Ctrl Pts',(-1.8384461208373,-0.661990831340053,
8.66440490528712));
#281145=CARTESIAN_POINT('Ctrl Pts',(-1.84938419468375,-0.631614187917754,
8.66255592237904));
#281146=CARTESIAN_POINT('Ctrl Pts',(-1.8595600260523,-0.600991854473024,
8.66070693947096));
#281147=CARTESIAN_POINT('Ctrl Pts',(-1.86896421628828,-0.570165553356156,
8.65885795656288));
#281148=CARTESIAN_POINT('Ctrl Pts',(-1.89332618263693,-0.490308671304903,
8.65406808542506));
#281149=CARTESIAN_POINT('Ctrl Pts',(-1.91258486915543,-0.408826904120657,
8.64927821428725));
#281150=CARTESIAN_POINT('Ctrl Pts',(-1.92656107311205,-0.326310330160359,
8.64448834314944));
#281151=CARTESIAN_POINT('Ctrl Pts',(-1.94033992247678,-0.244958952760407,
8.63976610862214));
#281152=CARTESIAN_POINT('Ctrl Pts',(-1.94898437599119,-0.162601767940379,
8.63504387409485));
#281153=CARTESIAN_POINT('Ctrl Pts',(-1.95236880609761,-0.0798250898965604,
8.63032163956755));
#281154=CARTESIAN_POINT('Ctrl Pts',(-1.9534323731954,-0.0538122757850696,
8.62883766350265));
#281155=CARTESIAN_POINT('Ctrl Pts',(-1.95397683673528,-0.0277581924780917,
8.62735368743774));
#281156=CARTESIAN_POINT('Ctrl Pts',(-1.95399927652111,-0.00168147404713564,
8.62586971137284));
#281157=CARTESIAN_POINT('',(-1.95392510023955,0.000982308602275455,7.92586964531847));
#281158=CARTESIAN_POINT('Ctrl Pts',(-1.95279013340439,-0.00168009551267251,
8.62586969212423));
#281159=CARTESIAN_POINT('Ctrl Pts',(-1.94903607268958,0.455640131522026,
8.59982856344197));
#281160=CARTESIAN_POINT('Ctrl Pts',(-1.56070656660671,1.56913066960483,
8.53675021793123));
#281161=CARTESIAN_POINT('Ctrl Pts',(0.294270353677477,2.29051751091558,
8.43663465559201));
#281162=CARTESIAN_POINT('Ctrl Pts',(2.08375418707712,0.995506903268704,
8.32552300510657));
#281163=CARTESIAN_POINT('Ctrl Pts',(1.96677879493936,-1.21030850518367,
8.21441135462113));
#281164=CARTESIAN_POINT('Ctrl Pts',(0.050366789813365,-2.30879377455664,
8.1032997041357));
#281165=CARTESIAN_POINT('Ctrl Pts',(-1.64840826021826,-1.43117012984314,
8.00711914997006));
#281166=CARTESIAN_POINT('Ctrl Pts',(-1.94951814111497,-0.387989405753114,
7.94797581263291));
#281167=CARTESIAN_POINT('Ctrl Pts',(-1.95128545551857,0.000980157954364874,
7.92586969212424));
#281168=CARTESIAN_POINT('',(-1.95399967105378,0.00113380850773978,7.22586969217444));
#281169=CARTESIAN_POINT('Ctrl Pts',(-1.95399975305789,0.00098236942558494,
7.92586964399473));
#281170=CARTESIAN_POINT('Ctrl Pts',(-1.95396158680754,0.0768976430830345,
7.92156116990685));
#281171=CARTESIAN_POINT('Ctrl Pts',(-1.94949516076616,0.152661436815141,
7.91725269581898));
#281172=CARTESIAN_POINT('Ctrl Pts',(-1.94067802404546,0.227782367594661,
7.9129442217311));
#281173=CARTESIAN_POINT('Ctrl Pts',(-1.93182936676887,0.303171849670571,
7.90862034519426));
#281174=CARTESIAN_POINT('Ctrl Pts',(-1.91859897376203,0.377913573292325,
7.90429646865743));
#281175=CARTESIAN_POINT('Ctrl Pts',(-1.90111518072707,0.451527484887769,
7.89997259212059));
#281176=CARTESIAN_POINT('Ctrl Pts',(-1.88354776221016,0.525493493927039,
7.89562803435866));
#281177=CARTESIAN_POINT('Ctrl Pts',(-1.86168630271332,0.59832059449387,
7.89128347659673));
#281178=CARTESIAN_POINT('Ctrl Pts',(-1.83570921630156,0.66954288375391,
7.8869389188348));
#281179=CARTESIAN_POINT('Ctrl Pts',(-1.82402478376978,0.701578502392081,
7.88498474694481));
#281180=CARTESIAN_POINT('Ctrl Pts',(-1.81150831947543,0.733289747289453,
7.88303057505482));
#281181=CARTESIAN_POINT('Ctrl Pts',(-1.79817909327187,0.764635827384474,
7.88107640316483));
#281182=CARTESIAN_POINT('Ctrl Pts',(-1.77145398682494,0.827484736574002,
7.8771582873659));
#281183=CARTESIAN_POINT('Ctrl Pts',(-1.74137694789808,0.889055425517929,
7.87324017156697));
#281184=CARTESIAN_POINT('Ctrl Pts',(-1.70809206844313,0.948966535617398,
7.86932205576804));
#281185=CARTESIAN_POINT('Ctrl Pts',(-1.67485731064044,1.00878742926193,
7.86540984001865));
#281186=CARTESIAN_POINT('Ctrl Pts',(-1.63842453608282,1.06695327728761,
7.86149762426926));
#281187=CARTESIAN_POINT('Ctrl Pts',(-1.59898559917462,1.12310331387286,
7.85758540851987));
#281188=CARTESIAN_POINT('Ctrl Pts',(-1.55959304023405,1.17918732117883,
7.85367779331577));
#281189=CARTESIAN_POINT('Ctrl Pts',(-1.51720162104138,1.23325982424866,
7.84977017811167));
#281190=CARTESIAN_POINT('Ctrl Pts',(-1.47204781227257,1.28498686311711,
7.84586256290757));
#281191=CARTESIAN_POINT('Ctrl Pts',(-1.42692230419587,1.33668148144251,
7.84195739684824));
#281192=CARTESIAN_POINT('Ctrl Pts',(-1.37903816375647,1.3860331819478,7.83805223078891));
#281193=CARTESIAN_POINT('Ctrl Pts',(-1.32867269552391,1.43274033522101,
7.83414706472959));
#281194=CARTESIAN_POINT('Ctrl Pts',(-1.27832151990334,1.47943423403155,
7.83024300687048));
#281195=CARTESIAN_POINT('Ctrl Pts',(-1.22549077483517,1.523484741101,7.82633894901138));
#281196=CARTESIAN_POINT('Ctrl Pts',(-1.17049395096475,1.56462772273628,
7.82243489115228));
#281197=CARTESIAN_POINT('Ctrl Pts',(-1.11549387154516,1.60577313983948,
7.81853060219161));
#281198=CARTESIAN_POINT('Ctrl Pts',(-1.05832785415725,1.64401039721329,
7.81462631323094));
#281199=CARTESIAN_POINT('Ctrl Pts',(-0.999340264593367,1.67911733823532,
7.81072202427027));
#281200=CARTESIAN_POINT('Ctrl Pts',(-0.940289843673999,1.71426167384675,
7.80681357660826));
#281201=CARTESIAN_POINT('Ctrl Pts',(-0.879414401895716,1.74626878683899,
7.80290512894625));
#281202=CARTESIAN_POINT('Ctrl Pts',(-0.817084049245728,1.77496187465202,
7.79899668128424));
#281203=CARTESIAN_POINT('Ctrl Pts',(-0.754716387751583,1.80367213717843,
7.79508589415745));
#281204=CARTESIAN_POINT('Ctrl Pts',(-0.690892539313103,1.829064244814,7.79117510703066));
#281205=CARTESIAN_POINT('Ctrl Pts',(-0.626001166910012,1.85101014017409,
7.78726431990388));
#281206=CARTESIAN_POINT('Ctrl Pts',(-0.560997747094305,1.8729939293358,
7.7833467800523));
#281207=CARTESIAN_POINT('Ctrl Pts',(-0.49492359777793,1.89151949716494,
7.77942924020072));
#281208=CARTESIAN_POINT('Ctrl Pts',(-0.42818019704342,1.90650930206487,
7.77551170034915));
#281209=CARTESIAN_POINT('Ctrl Pts',(-0.396678951771866,1.91358412168042,
7.77366271779256));
#281210=CARTESIAN_POINT('Ctrl Pts',(-0.365028733820059,1.91987205894661,
7.77181373523598));
#281211=CARTESIAN_POINT('Ctrl Pts',(-0.333272110538601,1.92536897771236,
7.76996475267939));
#281212=CARTESIAN_POINT('Ctrl Pts',(-0.26597773452622,1.93701731056733,
7.76604663688034));
#281213=CARTESIAN_POINT('Ctrl Pts',(-0.197938535201442,1.9451564360216,
7.7621285210813));
#281214=CARTESIAN_POINT('Ctrl Pts',(-0.129553040639174,1.94970049229648,
7.75821040528225));
#281215=CARTESIAN_POINT('Ctrl Pts',(-0.0612705235860549,1.95423770595657,
7.75429818953274));
#281216=CARTESIAN_POINT('Ctrl Pts',(0.00735676693203037,1.95519056215335,
7.75038597378324));
#281217=CARTESIAN_POINT('Ctrl Pts',(0.0759216882150816,1.9525244933825,
7.74647375803373));
#281218=CARTESIAN_POINT('Ctrl Pts',(0.144405981013923,1.9498615597583,7.74256614282951));
#281219=CARTESIAN_POINT('Ctrl Pts',(0.212827561055752,1.94358817197773,
7.73865852762529));
#281220=CARTESIAN_POINT('Ctrl Pts',(0.28077759711522,1.93372178478658,7.73475091242108));
#281221=CARTESIAN_POINT('Ctrl Pts',(0.34868504467321,1.92386158147214,7.73084574636164));
#281222=CARTESIAN_POINT('Ctrl Pts',(0.41612104883496,1.91041291643297,7.7269405803022));
#281223=CARTESIAN_POINT('Ctrl Pts',(0.482681782852538,1.89344508674065,
7.72303541424276));
#281224=CARTESIAN_POINT('Ctrl Pts',(0.549223628397983,1.87648207214514,
7.71913135638355));
#281225=CARTESIAN_POINT('Ctrl Pts',(0.614890220468014,1.85600199685958,
7.71522729852433));
#281226=CARTESIAN_POINT('Ctrl Pts',(0.679289597316019,1.83212489830203,
7.71132324066511));
#281227=CARTESIAN_POINT('Ctrl Pts',(0.743692786299331,1.80824638633438,
7.70741895170433));
#281228=CARTESIAN_POINT('Ctrl Pts',(0.806828150826173,1.78097062526735,
7.70351466274355));
#281229=CARTESIAN_POINT('Ctrl Pts',(0.868322240017641,1.75046636285612,
7.69961037378277));
#281230=CARTESIAN_POINT('Ctrl Pts',(0.92988183039347,1.71992960845515,7.69570192612065));
#281231=CARTESIAN_POINT('Ctrl Pts',(0.989796215028153,1.68615770877636,
7.69179347845853));
#281232=CARTESIAN_POINT('Ctrl Pts',(1.04771607443799,1.64936564392625,7.68788503079641));
#281233=CARTESIAN_POINT('Ctrl Pts',(1.10567060271965,1.61255155658863,7.68397424366951));
#281234=CARTESIAN_POINT('Ctrl Pts',(1.16162782902405,1.57271399159945,7.68006345654261));
#281235=CARTESIAN_POINT('Ctrl Pts',(1.21526931542516,1.53010996042313,7.67615266941572));
#281236=CARTESIAN_POINT('Ctrl Pts',(1.26900342415086,1.48743236520768,7.67223512956403));
#281237=CARTESIAN_POINT('Ctrl Pts',(1.32041344416103,1.44197909564308,7.66831758971235));
#281238=CARTESIAN_POINT('Ctrl Pts',(1.36921641949976,1.3940453351926,7.66440004986067));
#281239=CARTESIAN_POINT('Ctrl Pts',(1.39225022476467,1.37142177799823,7.6625510673051));
#281240=CARTESIAN_POINT('Ctrl Pts',(1.41470385035661,1.34824616262135,7.66070208474953));
#281241=CARTESIAN_POINT('Ctrl Pts',(1.43655072720674,1.32455200281521,7.65885310219396));
#281242=CARTESIAN_POINT('Ctrl Pts',(1.48284569796856,1.2743425178176,7.65493498639478));
#281243=CARTESIAN_POINT('Ctrl Pts',(1.52659693240248,1.22160346688017,7.6510168705956));
#281244=CARTESIAN_POINT('Ctrl Pts',(1.56751608586576,1.16662304132573,7.64709875479642));
#281245=CARTESIAN_POINT('Ctrl Pts',(1.60837362169326,1.11172540741164,7.64318653904677));
#281246=CARTESIAN_POINT('Ctrl Pts',(1.64640724907164,1.05459348877088,7.63927432329713));
#281247=CARTESIAN_POINT('Ctrl Pts',(1.68136703821542,0.995550542565618,
7.63536210754748));
#281248=CARTESIAN_POINT('Ctrl Pts',(1.71628571661696,0.936577027538358,
7.63145449234313));
#281249=CARTESIAN_POINT('Ctrl Pts',(1.74813748613206,0.875697369287417,
7.62754687713877));
#281250=CARTESIAN_POINT('Ctrl Pts',(1.77671520105431,0.813264467650303,
7.62363926193441));
#281251=CARTESIAN_POINT('Ctrl Pts',(1.80527500455042,0.75087069658433,7.61973409587483));
#281252=CARTESIAN_POINT('Ctrl Pts',(1.83056461981158,0.686926059523024,
7.61582892981525));
#281253=CARTESIAN_POINT('Ctrl Pts',(1.85242316530533,0.621807379049321,
7.61192376375566));
#281254=CARTESIAN_POINT('Ctrl Pts',(1.87427550782471,0.556707177824659,
7.6080197058963));
#281255=CARTESIAN_POINT('Ctrl Pts',(1.89269855700926,0.490434060674127,
7.60411564803694));
#281256=CARTESIAN_POINT('Ctrl Pts',(1.90758049193009,0.423382412019868,
7.60021159017758));
#281257=CARTESIAN_POINT('Ctrl Pts',(1.92246330779034,0.356326794228461,
7.59630730121665));
#281258=CARTESIAN_POINT('Ctrl Pts',(1.93380448915002,0.288493034186758,
7.59240301225573));
#281259=CARTESIAN_POINT('Ctrl Pts',(1.94154317608092,0.220286394072858,
7.5884987232948));
#281260=CARTESIAN_POINT('Ctrl Pts',(1.94929010596925,0.152007102818522,
7.58459027563253));
#281261=CARTESIAN_POINT('Ctrl Pts',(1.95342682792389,0.0833546285307044,
7.58068182797026));
#281262=CARTESIAN_POINT('Ctrl Pts',(1.95394441081184,0.0147390453280266,
7.57677338030799));
#281263=CARTESIAN_POINT('Ctrl Pts',(1.95446230350742,-0.0539176088455757,
7.57286259318095));
#281264=CARTESIAN_POINT('Ctrl Pts',(1.95135676805297,-0.122536836543049,
7.5689518060539));
#281265=CARTESIAN_POINT('Ctrl Pts',(1.94467093540427,-0.190711701250598,
7.56504101892685));
#281266=CARTESIAN_POINT('Ctrl Pts',(1.93797355838192,-0.25900428295056,
7.56112347907502));
#281267=CARTESIAN_POINT('Ctrl Pts',(1.92768361946341,-0.326850484236416,
7.55720593922319));
#281268=CARTESIAN_POINT('Ctrl Pts',(1.91389556563938,-0.393852464542159,
7.55328839937135));
#281269=CARTESIAN_POINT('Ctrl Pts',(1.90738794301336,-0.425475752976507,
7.55143941681707));
#281270=CARTESIAN_POINT('Ctrl Pts',(1.90010180379956,-0.456911188780959,
7.54959043426279));
#281271=CARTESIAN_POINT('Ctrl Pts',(1.89205088566652,-0.488118270553907,
7.54774145170851));
#281272=CARTESIAN_POINT('Ctrl Pts',(1.87499045994153,-0.554248132003628,
7.54382333590944));
#281273=CARTESIAN_POINT('Ctrl Pts',(1.85442504231282,-0.619613578577113,
7.53990522011037));
#281274=CARTESIAN_POINT('Ctrl Pts',(1.83044028258338,-0.683816036588854,
7.5359871043113));
#281275=CARTESIAN_POINT('Ctrl Pts',(1.80649164002804,-0.747921816068889,
7.53207488856176));
#281276=CARTESIAN_POINT('Ctrl Pts',(1.77913404502007,-0.810867625573898,
7.52816267281223));
#281277=CARTESIAN_POINT('Ctrl Pts',(1.74850344534968,-0.872268136297721,
7.52425045706269));
#281278=CARTESIAN_POINT('Ctrl Pts',(1.71790886553865,-0.933596443480497,
7.52034284185845));
#281279=CARTESIAN_POINT('Ctrl Pts',(1.68404914351472,-0.993382622771358,
7.5164352266542));
#281280=CARTESIAN_POINT('Ctrl Pts',(1.64710833992997,-1.05126120280982,
7.51252761144996));
#281281=CARTESIAN_POINT('Ctrl Pts',(1.61019068943766,-1.1091035067529,7.50862244539049));
#281282=CARTESIAN_POINT('Ctrl Pts',(1.57019605212303,-1.16504016945973,
7.50471727933102));
#281283=CARTESIAN_POINT('Ctrl Pts',(1.52735368469385,-1.21873160369793,
7.50081211327155));
#281284=CARTESIAN_POINT('Ctrl Pts',(1.48452347498611,-1.27240780148818,
7.4969080554123));
#281285=CARTESIAN_POINT('Ctrl Pts',(1.43884744607434,-1.32383965135485,
7.49300399755305));
#281286=CARTESIAN_POINT('Ctrl Pts',(1.39059622456031,-1.3727192503344,7.48909993969381));
#281287=CARTESIAN_POINT('Ctrl Pts',(1.34234214680455,-1.4216017427526,7.48519565073299));
#281288=CARTESIAN_POINT('Ctrl Pts',(1.29151292118007,-1.46793133608345,
7.48129136177218));
#281289=CARTESIAN_POINT('Ctrl Pts',(1.23841596040746,-1.51143703441727,
7.47738707281136));
#281290=CARTESIAN_POINT('Ctrl Pts',(1.18526244275497,-1.55498907337999,
7.47347862514921));
#281291=CARTESIAN_POINT('Ctrl Pts',(1.12983675055633,-1.59571090215063,
7.46957017748706));
#281292=CARTESIAN_POINT('Ctrl Pts',(1.07247851226217,-1.63337253580924,
7.46566172982491));
#281293=CARTESIAN_POINT('Ctrl Pts',(1.01508594126359,-1.67105671244992,
7.46175094269797));
#281294=CARTESIAN_POINT('Ctrl Pts',(0.955758946904507,-1.70567680055392,
7.45784015557104));
#281295=CARTESIAN_POINT('Ctrl Pts',(0.894862767837988,-1.73704825112526,
7.45392936844411));
#281296=CARTESIAN_POINT('Ctrl Pts',(0.833861439827212,-1.76847387052884,
7.45001182859239));
#281297=CARTESIAN_POINT('Ctrl Pts',(0.771285967684583,-1.79663945516226,
7.44609428874067));
#281298=CARTESIAN_POINT('Ctrl Pts',(0.707521790321602,-1.82140849789939,
7.44217674888895));
#281299=CARTESIAN_POINT('Ctrl Pts',(0.677426665304581,-1.83309887749109,
7.44032776633366));
#281300=CARTESIAN_POINT('Ctrl Pts',(0.64706696375964,-1.84403336294319,
7.43847878377837));
#281301=CARTESIAN_POINT('Ctrl Pts',(0.616484161285372,-1.85420152057005,
7.43662980122308));
#281302=CARTESIAN_POINT('Ctrl Pts',(0.551677188817107,-1.87574851620365,
7.43271168542399));
#281303=CARTESIAN_POINT('Ctrl Pts',(0.485610740661061,-1.89393649124481,
7.42879356962489));
#281304=CARTESIAN_POINT('Ctrl Pts',(0.418666098724568,-1.90862115093036,
7.4248754538258));
#281305=CARTESIAN_POINT('Ctrl Pts',(0.351822264605887,-1.92328369789031,
7.42096323807624));
#281306=CARTESIAN_POINT('Ctrl Pts',(0.284103337830234,-1.93445329480633,
7.41705102232668));
#281307=CARTESIAN_POINT('Ctrl Pts',(0.215906763008642,-1.94203508456648,
7.41313880657712));
#281308=CARTESIAN_POINT('Ctrl Pts',(0.147790383516518,-1.94960795856906,
7.40923119137285));
#281309=CARTESIAN_POINT('Ctrl Pts',(0.0791979580515704,-1.95360135043905,
7.40532357616858));
#281310=CARTESIAN_POINT('Ctrl Pts',(0.0105363536613027,-1.95397159274426,
7.40141596096431));
#281311=CARTESIAN_POINT('Ctrl Pts',(-0.0580822162435067,-1.95434160299565,
7.39751079490482));
#281312=CARTESIAN_POINT('Ctrl Pts',(-0.126769388294698,-1.95109296568588,
7.39360562884533));
#281313=CARTESIAN_POINT('Ctrl Pts',(-0.19511551808398,-1.94423402259163,
7.38970046278583));
#281314=CARTESIAN_POINT('Ctrl Pts',(-0.263442252745103,-1.93737702591454,
7.38579640492656));
#281315=CARTESIAN_POINT('Ctrl Pts',(-0.331427648077723,-1.92691180640519,
7.38189234706729));
#281316=CARTESIAN_POINT('Ctrl Pts',(-0.398666230450798,-1.91289864778512,
7.37798828920802));
#281317=CARTESIAN_POINT('Ctrl Pts',(-0.46590879302657,-1.89888465965304,
7.37408400024718));
#281318=CARTESIAN_POINT('Ctrl Pts',(-0.532403973866264,-1.88132241831172,
7.37017971128634));
#281319=CARTESIAN_POINT('Ctrl Pts',(-0.597757344296068,-1.86032313250685,
7.3662754223255));
#281320=CARTESIAN_POINT('Ctrl Pts',(-0.663180326671078,-1.83930147905479,
7.36236697466333));
#281321=CARTESIAN_POINT('Ctrl Pts',(-0.727458602252804,-1.81483562565828,
7.35845852700115));
#281322=CARTESIAN_POINT('Ctrl Pts',(-0.79021471437671,-1.78708609338849,
7.35455007933897));
#281323=CARTESIAN_POINT('Ctrl Pts',(-0.853008390190014,-1.7593199511858,
7.35063929221201));
#281324=CARTESIAN_POINT('Ctrl Pts',(-0.914277650453092,-1.72826644080647,
7.34672850508506));
#281325=CARTESIAN_POINT('Ctrl Pts',(-0.973669311359256,-1.69413224752886,
7.3428177179581));
#281326=CARTESIAN_POINT('Ctrl Pts',(-1.03316352337023,-1.65993911501333,
7.33890017810636));
#281327=CARTESIAN_POINT('Ctrl Pts',(-1.0907732527164,-1.62265495005914,
7.33498263825462));
#281328=CARTESIAN_POINT('Ctrl Pts',(-1.14617471264073,-1.58252947148005,
7.33106509840288));
#281329=CARTESIAN_POINT('Ctrl Pts',(-1.17232284049716,-1.56359123148386,
7.3292161158478));
#281330=CARTESIAN_POINT('Ctrl Pts',(-1.1979795396265,-1.54402063518359,
7.32736713329272));
#281331=CARTESIAN_POINT('Ctrl Pts',(-1.22311354317257,-1.52384686255143,
7.32551815073764));
#281332=CARTESIAN_POINT('Ctrl Pts',(-1.27569843014326,-1.48163967690788,
7.32164974439755));
#281333=CARTESIAN_POINT('Ctrl Pts',(-1.32621309543889,-1.43661316524796,
7.31778133805745));
#281334=CARTESIAN_POINT('Ctrl Pts',(-1.3743338022176,-1.38900057598336,
7.31391293171736));
#281335=CARTESIAN_POINT('Ctrl Pts',(-1.4223718768899,-1.34146974629392,
7.31005116814262));
#281336=CARTESIAN_POINT('Ctrl Pts',(-1.4680237975101,-1.29136200687844,
7.30618940456789));
#281337=CARTESIAN_POINT('Ctrl Pts',(-1.51099832301929,-1.23895119671152,
7.30232764099316));
#281338=CARTESIAN_POINT('Ctrl Pts',(-1.5539317360317,-1.18659052646442,
7.29846957185696));
#281339=CARTESIAN_POINT('Ctrl Pts',(-1.59419251060611,-1.13193154021921,
7.29461150272075));
#281340=CARTESIAN_POINT('Ctrl Pts',(-1.6315268499352,-1.07528421263428,
7.29075343358454));
#281341=CARTESIAN_POINT('Ctrl Pts',(-1.6688390587004,-1.01867046371512,
7.28689765138435));
#281342=CARTESIAN_POINT('Ctrl Pts',(-1.70322799382576,-0.960071131503946,
7.28304186918416));
#281343=CARTESIAN_POINT('Ctrl Pts',(-1.73448192833098,-0.899826894626534,
7.27918608698398));
#281344=CARTESIAN_POINT('Ctrl Pts',(-1.76572870765072,-0.839596449890684,
7.27533118751543));
#281345=CARTESIAN_POINT('Ctrl Pts',(-1.79384167895834,-0.777722296975262,
7.27147628804688));
#281346=CARTESIAN_POINT('Ctrl Pts',(-1.81865500239731,-0.71456978823292,
7.26762138857834));
#281347=CARTESIAN_POINT('Ctrl Pts',(-1.8434864034073,-0.651371270177707,
7.26376368065009));
#281348=CARTESIAN_POINT('Ctrl Pts',(-1.86501316883761,-0.586893007186788,
7.25990597272184));
#281349=CARTESIAN_POINT('Ctrl Pts',(-1.88311808384908,-0.521519206051485,
7.2560482647936));
#281350=CARTESIAN_POINT('Ctrl Pts',(-1.90122994604552,-0.456120319800443,
7.2521890765927));
#281351=CARTESIAN_POINT('Ctrl Pts',(-1.91591723290655,-0.389825705105673,
7.2483298883918));
#281352=CARTESIAN_POINT('Ctrl Pts',(-1.92711367637425,-0.32303076994509,
7.2444707001909));
#281353=CARTESIAN_POINT('Ctrl Pts',(-1.9383275135784,-0.256132068485687,
7.24060551671993));
#281354=CARTESIAN_POINT('Ctrl Pts',(-1.94603962377029,-0.188731997572627,
7.23674033324896));
#281355=CARTESIAN_POINT('Ctrl Pts',(-1.95023563501482,-0.121231051790984,
7.23287514977798));
#281356=CARTESIAN_POINT('Ctrl Pts',(-1.95277065731482,-0.0804503215079684,
7.23053999724347));
#281357=CARTESIAN_POINT('Ctrl Pts',(-1.95402332588266,-0.0396328002594552,
7.22820484470895));
#281358=CARTESIAN_POINT('Ctrl Pts',(-1.95399967105378,0.00113380850775126,
7.22586969217444));
#281359=CARTESIAN_POINT('',(-1.95399924719281,-0.00171521716542704,6.52586969212424));
#281360=CARTESIAN_POINT('Ctrl Pts',(-1.95399967105327,0.00113380938422453,
7.22586969212423));
#281361=CARTESIAN_POINT('Ctrl Pts',(-1.9539609640812,0.0678411516748536,
7.22204862816689));
#281362=CARTESIAN_POINT('Ctrl Pts',(-1.9505065413377,0.134447927039275,
7.21822756420955));
#281363=CARTESIAN_POINT('Ctrl Pts',(-1.94366557894286,0.200699071330002,
7.21440650025221));
#281364=CARTESIAN_POINT('Ctrl Pts',(-1.93665086180136,0.268632939501905,
7.2104883844531));
#281365=CARTESIAN_POINT('Ctrl Pts',(-1.92605637388582,0.336333270622923,
7.206570268654));
#281366=CARTESIAN_POINT('Ctrl Pts',(-1.91190740994614,0.403393177672903,
7.20265215285489));
#281367=CARTESIAN_POINT('Ctrl Pts',(-1.89777975206077,0.470352103334573,
7.19873993710531));
#281368=CARTESIAN_POINT('Ctrl Pts',(-1.88010834163168,0.536672041455856,
7.19482772135574));
#281369=CARTESIAN_POINT('Ctrl Pts',(-1.85897018357449,0.601951706186642,
7.19091550560616));
#281370=CARTESIAN_POINT('Ctrl Pts',(-1.83785688280018,0.667154605709812,
7.18700789040187));
#281371=CARTESIAN_POINT('Ctrl Pts',(-1.81328508159823,0.731319195598035,
7.18310027519759));
#281372=CARTESIAN_POINT('Ctrl Pts',(-1.78538231978286,0.794056655539634,
7.1791926599933));
#281373=CARTESIAN_POINT('Ctrl Pts',(-1.75749704635867,0.856754794024498,
7.17528749393379));
#281374=CARTESIAN_POINT('Ctrl Pts',(-1.72628515313261,0.918027128483419,
7.17138232787428));
#281375=CARTESIAN_POINT('Ctrl Pts',(-1.69192272872721,0.977503698211054,
7.16747716181477));
#281376=CARTESIAN_POINT('Ctrl Pts',(-1.65757005562196,1.03696338979655,
7.16357310395548));
#281377=CARTESIAN_POINT('Ctrl Pts',(-1.6200688721345,1.09462790258377,7.15966904609619));
#281378=CARTESIAN_POINT('Ctrl Pts',(-1.57964089664353,1.15015244104911,
7.15576498823691));
#281379=CARTESIAN_POINT('Ctrl Pts',(-1.53921052800964,1.20568026630174,
7.15186069927605));
#281380=CARTESIAN_POINT('Ctrl Pts',(-1.49585331500633,1.25906746960417,
7.1479564103152));
#281381=CARTESIAN_POINT('Ctrl Pts',(-1.44983285152109,1.31000026818708,
7.14405212135435));
#281382=CARTESIAN_POINT('Ctrl Pts',(-1.40376336877392,1.36098731846598,
7.14014367369215));
#281383=CARTESIAN_POINT('Ctrl Pts',(-1.35502530458131,1.40951438094631,
7.13623522602996));
#281384=CARTESIAN_POINT('Ctrl Pts',(-1.30392022058927,1.45530342483567,
7.13232677836777));
#281385=CARTESIAN_POINT('Ctrl Pts',(-1.25278454681981,1.50111987650037,
7.12841599124079));
#281386=CARTESIAN_POINT('Ctrl Pts',(-1.19927941672047,1.5441947393922,7.12450520411382));
#281387=CARTESIAN_POINT('Ctrl Pts',(-1.14373848737084,1.58429109462455,
7.12059441698685));
#281388=CARTESIAN_POINT('Ctrl Pts',(-1.08810165594369,1.62445668391209,
7.11667687713509));
#281389=CARTESIAN_POINT('Ctrl Pts',(-1.03042242271735,1.66163323466832,
7.11275933728333));
#281390=CARTESIAN_POINT('Ctrl Pts',(-0.971061579032576,1.69562832299026,
7.10884179743157));
#281391=CARTESIAN_POINT('Ctrl Pts',(-0.943044719326595,1.71167316940899,
7.10699281487664));
#281392=CARTESIAN_POINT('Ctrl Pts',(-0.91465358830197,1.72700999205061,
7.1051438323217));
#281393=CARTESIAN_POINT('Ctrl Pts',(-0.885927643488578,1.74162229272101,
7.10329484976677));
#281394=CARTESIAN_POINT('Ctrl Pts',(-0.825055474674994,1.77258672013816,
7.09937673396767));
#281395=CARTESIAN_POINT('Ctrl Pts',(-0.762437306951289,1.80041733419865,
7.09545861816858));
#281396=CARTESIAN_POINT('Ctrl Pts',(-0.698428660500115,1.8249146298367,
7.09154050236948));
#281397=CARTESIAN_POINT('Ctrl Pts',(-0.634516400731742,1.84937503650435,
7.08762828661992));
#281398=CARTESIAN_POINT('Ctrl Pts',(-0.569218273449775,1.8705119121578,
7.08371607087036));
#281399=CARTESIAN_POINT('Ctrl Pts',(-0.502913148641049,1.88817222861792,
7.0798038551208));
#281400=CARTESIAN_POINT('Ctrl Pts',(-0.436685994923168,1.90581177754094,
7.07589623991653));
#281401=CARTESIAN_POINT('Ctrl Pts',(-0.369454668522051,1.91998276057471,
7.07198862471225));
#281402=CARTESIAN_POINT('Ctrl Pts',(-0.301614985331262,1.9305813633783,
7.06808100950798));
#281403=CARTESIAN_POINT('Ctrl Pts',(-0.233817821476945,1.94117332338026,
7.06417584344849));
#281404=CARTESIAN_POINT('Ctrl Pts',(-0.165413542095161,1.94819726892558,
7.06027067738899));
#281405=CARTESIAN_POINT('Ctrl Pts',(-0.0968084602488389,1.95160040019064,
7.05636551132949));
#281406=CARTESIAN_POINT('Ctrl Pts',(-0.0282228470155735,1.9550025657219,
7.05246145347022));
#281407=CARTESIAN_POINT('Ctrl Pts',(0.0405629645149766,1.95478593239357,
7.04855739561095));
#281408=CARTESIAN_POINT('Ctrl Pts',(0.109139044682844,1.9509496838529,7.04465333775167));
#281409=CARTESIAN_POINT('Ctrl Pts',(0.177719184226884,1.94711320822464,
7.04074904879083));
#281410=CARTESIAN_POINT('Ctrl Pts',(0.246089076792685,1.93965672202949,
7.03684475982999));
#281411=CARTESIAN_POINT('Ctrl Pts',(0.313842125088751,1.92863141126545,
7.03294047086915));
#281412=CARTESIAN_POINT('Ctrl Pts',(0.381667341376385,1.91759435675624,
7.02903202320697));
#281413=CARTESIAN_POINT('Ctrl Pts',(0.448873915721153,1.90298097046063,
7.02512357554479));
#281414=CARTESIAN_POINT('Ctrl Pts',(0.515064684401739,1.88489372933387,
7.02121512788261));
#281415=CARTESIAN_POINT('Ctrl Pts',(0.581295072641165,1.86679566179539,
7.01730434075565));
#281416=CARTESIAN_POINT('Ctrl Pts',(0.646507978082287,1.84521975569629,
7.01339355362869));
#281417=CARTESIAN_POINT('Ctrl Pts',(0.710323359051366,1.82031775401604,
7.00948276650173));
#281418=CARTESIAN_POINT('Ctrl Pts',(0.774248929527226,1.7953727542491,7.00556522664999));
#281419=CARTESIAN_POINT('Ctrl Pts',(0.836771711459432,1.76709039912909,
7.00164768679825));
#281420=CARTESIAN_POINT('Ctrl Pts',(0.897534318749179,1.73566936559572,
6.9977301469465));
#281421=CARTESIAN_POINT('Ctrl Pts',(0.926212776436969,1.72083940979089,
6.99588116439145));
#281422=CARTESIAN_POINT('Ctrl Pts',(0.954499531921449,1.70531092261739,
6.99403218183639));
#281423=CARTESIAN_POINT('Ctrl Pts',(0.982359318873593,1.68910809856036,
6.99218319928133));
#281424=CARTESIAN_POINT('Ctrl Pts',(1.04139604213431,1.65477324734489,6.98826508348223));
#281425=CARTESIAN_POINT('Ctrl Pts',(1.09874755079015,1.61727148121357,6.98434696768313));
#281426=CARTESIAN_POINT('Ctrl Pts',(1.15405337018907,1.57679320735322,6.98042885188403));
#281427=CARTESIAN_POINT('Ctrl Pts',(1.20927590795705,1.53637588723519,6.97651663613447));
#281428=CARTESIAN_POINT('Ctrl Pts',(1.26245847639234,1.49299124302138,6.9726044203849));
#281429=CARTESIAN_POINT('Ctrl Pts',(1.31326697450054,1.44687451207291,6.96869220463533));
#281430=CARTESIAN_POINT('Ctrl Pts',(1.36401572467772,1.40081201180162,6.96478458943106));
#281431=CARTESIAN_POINT('Ctrl Pts',(1.41239558653464,1.35202413444964,6.96087697422678));
#281432=CARTESIAN_POINT('Ctrl Pts',(1.45810460623655,1.30078705300743,6.95696935902251));
#281433=CARTESIAN_POINT('Ctrl Pts',(1.50378497726122,1.24958208502157,6.95306419296301));
#281434=CARTESIAN_POINT('Ctrl Pts',(1.54679750006817,1.19593132425755,6.9491590269035));
#281435=CARTESIAN_POINT('Ctrl Pts',(1.58687737931631,1.14014743915609,6.945253860844));
#281436=CARTESIAN_POINT('Ctrl Pts',(1.62694588477639,1.08437938429411,6.94134980298473));
#281437=CARTESIAN_POINT('Ctrl Pts',(1.66408311190234,1.02647980606318,6.93744574512545));
#281438=CARTESIAN_POINT('Ctrl Pts',(1.69806597079622,0.966792614175287,
6.93354168726617));
#281439=CARTESIAN_POINT('Ctrl Pts',(1.73205084131295,0.907101889090883,
6.92963739830533));
#281440=CARTESIAN_POINT('Ctrl Pts',(1.7628807317453,0.845623768984775,6.92573310934448));
#281441=CARTESIAN_POINT('Ctrl Pts',(1.79037804360517,0.782727577753921,
6.92182882038364));
#281442=CARTESIAN_POINT('Ctrl Pts',(1.81790464456448,0.719764391872499,
6.91792037272145));
#281443=CARTESIAN_POINT('Ctrl Pts',(1.84209138536074,0.655380571980799,
6.91401192505927));
#281444=CARTESIAN_POINT('Ctrl Pts',(1.86280887148414,0.589965345016128,
6.91010347739709));
#281445=CARTESIAN_POINT('Ctrl Pts',(1.88353875839509,0.524510962705703,
6.90619269027012));
#281446=CARTESIAN_POINT('Ctrl Pts',(1.90079513427067,0.45802442082151,6.90228190314316));
#281447=CARTESIAN_POINT('Ctrl Pts',(1.91449927890125,0.390907292189067,
6.89837111601619));
#281448=CARTESIAN_POINT('Ctrl Pts',(1.92822708636852,0.323674272948614,
6.89445357616445));
#281449=CARTESIAN_POINT('Ctrl Pts',(1.93839034807995,0.255808980028962,
6.8905360363127));
#281450=CARTESIAN_POINT('Ctrl Pts',(1.94496206129787,0.187719418579768,
6.88661849646095));
#281451=CARTESIAN_POINT('Ctrl Pts',(1.94806374846798,0.15558281855454,6.88476951390593));
#281452=CARTESIAN_POINT('Ctrl Pts',(1.95036613437155,0.123396276819736,
6.88292053135091));
#281453=CARTESIAN_POINT('Ctrl Pts',(1.95187040959523,0.0912025446276998,
6.88107154879589));
#281454=CARTESIAN_POINT('Ctrl Pts',(1.95505806785845,0.0229819059899013,
6.87715343299679));
#281455=CARTESIAN_POINT('Ctrl Pts',(1.95467112714343,-0.0455412892431805,
6.87323531719769));
#281456=CARTESIAN_POINT('Ctrl Pts',(1.9506739622135,-0.113960928138913,
6.86931720139859));
#281457=CARTESIAN_POINT('Ctrl Pts',(1.94668281636833,-0.182277538109707,
6.86540498564903));
#281458=CARTESIAN_POINT('Ctrl Pts',(1.93909226412263,-0.250490414134239,
6.86149276989946));
#281459=CARTESIAN_POINT('Ctrl Pts',(1.92791864768824,-0.318191275643976,
6.8575805541499));
#281460=CARTESIAN_POINT('Ctrl Pts',(1.91675817079721,-0.385812524755137,
6.85367293894562));
#281461=CARTESIAN_POINT('Ctrl Pts',(1.90202307747573,-0.452922472114777,
6.84976532374134));
#281462=CARTESIAN_POINT('Ctrl Pts',(1.88378153822363,-0.519117632379996,
6.84585770853707));
#281463=CARTESIAN_POINT('Ctrl Pts',(1.8655514320754,-0.585271304033257,
6.84195254247757));
#281464=CARTESIAN_POINT('Ctrl Pts',(1.84381936993339,-0.650510852804162,
6.83804737641807));
#281465=CARTESIAN_POINT('Ctrl Pts',(1.81870433956832,-0.71444420722359,
6.83414221035857));
#281466=CARTESIAN_POINT('Ctrl Pts',(1.7935964362964,-0.778359418763425,
6.83023815249929));
#281467=CARTESIAN_POINT('Ctrl Pts',(1.76510765035267,-0.84096871418652,
6.82633409464001));
#281468=CARTESIAN_POINT('Ctrl Pts',(1.73340584003042,-0.901898106078744,
6.82243003678074));
#281469=CARTESIAN_POINT('Ctrl Pts',(1.7017021531125,-0.962831104699797,
6.81852574781989));
#281470=CARTESIAN_POINT('Ctrl Pts',(1.66678529352021,-1.02208356719771,
6.81462145885904));
#281471=CARTESIAN_POINT('Ctrl Pts',(1.62886914919724,-1.07930593197363,
6.8107171698982));
#281472=CARTESIAN_POINT('Ctrl Pts',(1.59091261802746,-1.13658924785418,
6.80680872223601));
#281473=CARTESIAN_POINT('Ctrl Pts',(1.54995069865983,-1.1918377397423,6.80290027457383));
#281474=CARTESIAN_POINT('Ctrl Pts',(1.50624015085242,-1.2447315405179,6.79899182691165));
#281475=CARTESIAN_POINT('Ctrl Pts',(1.46250343938723,-1.2976570017364,6.79508103978468));
#281476=CARTESIAN_POINT('Ctrl Pts',(1.41601515810384,-1.34822460463977,
6.79117025265772));
#281477=CARTESIAN_POINT('Ctrl Pts',(1.36706993060505,-1.39615035180151,
6.78725946553075));
#281478=CARTESIAN_POINT('Ctrl Pts',(1.31804018977428,-1.44415885196672,
6.783341925679));
#281479=CARTESIAN_POINT('Ctrl Pts',(1.26654540451618,-1.48951606708082,
6.77942438582726));
#281480=CARTESIAN_POINT('Ctrl Pts',(1.21291366068032,-1.531977954063,6.77550684597551));
#281481=CARTESIAN_POINT('Ctrl Pts',(1.18760079533619,-1.55201892141859,
6.77365786342049));
#281482=CARTESIAN_POINT('Ctrl Pts',(1.16181232286502,-1.57141554837522,
6.77180888086548));
#281483=CARTESIAN_POINT('Ctrl Pts',(1.13558480148282,-1.59014564070126,
6.76995989831046));
#281484=CARTESIAN_POINT('Ctrl Pts',(1.08000695645659,-1.62983593981318,
6.76604178251136));
#281485=CARTESIAN_POINT('Ctrl Pts',(1.02223558446953,-1.66668762344908,
6.76212366671226));
#281486=CARTESIAN_POINT('Ctrl Pts',(0.962592503785318,-1.70045043199039,
6.75820555091316));
#281487=CARTESIAN_POINT('Ctrl Pts',(0.903039235947001,-1.73416239919545,
6.75429333516359));
#281488=CARTESIAN_POINT('Ctrl Pts',(0.841620277728886,-1.76479448221852,
6.75038111941403));
#281489=CARTESIAN_POINT('Ctrl Pts',(0.778687462804387,-1.79213889954748,
6.74646890366446));
#281490=CARTESIAN_POINT('Ctrl Pts',(0.715828653324338,-1.81945116138237,
6.74256128846019));
#281491=CARTESIAN_POINT('Ctrl Pts',(0.651459971661729,-1.84348324058542,
6.73865367325591));
#281492=CARTESIAN_POINT('Ctrl Pts',(0.585957342396771,-1.86407349449836,
6.73474605805164));
#281493=CARTESIAN_POINT('Ctrl Pts',(0.520495767691645,-1.88465084322228,
6.73084089199214));
#281494=CARTESIAN_POINT('Ctrl Pts',(0.453902123407269,-1.9017904986943,
6.72693572593264));
#281495=CARTESIAN_POINT('Ctrl Pts',(0.386570316657824,-1.9153796987227,
6.72303055987314));
#281496=CARTESIAN_POINT('Ctrl Pts',(0.319257617193964,-1.92896504243507,
6.71912650201386));
#281497=CARTESIAN_POINT('Ctrl Pts',(0.251207653039465,-1.93900183358048,
6.71522244415458));
#281498=CARTESIAN_POINT('Ctrl Pts',(0.182825654506691,-1.94542817396433,
6.7113183862953));
#281499=CARTESIAN_POINT('Ctrl Pts',(0.114439608086459,-1.95185489475682,
6.70741409733446));
#281500=CARTESIAN_POINT('Ctrl Pts',(0.045721978226763,-1.95467069700702,
6.70350980837361));
#281501=CARTESIAN_POINT('Ctrl Pts',(-0.0229175501145682,-1.95386560077625,
6.69960551941277));
#281502=CARTESIAN_POINT('Ctrl Pts',(-0.0916301906925765,-1.95305964698735,
6.69569707175059));
#281503=CARTESIAN_POINT('Ctrl Pts',(-0.160264070938615,-1.94862510342967,
6.6917886240884));
#281504=CARTESIAN_POINT('Ctrl Pts',(-0.228411190336413,-1.94060411422039,
6.68788017642622));
#281505=CARTESIAN_POINT('Ctrl Pts',(-0.29659910029851,-1.93257832391784,
6.68396938929926));
#281506=CARTESIAN_POINT('Ctrl Pts',(-0.364299184693671,-1.92096189878078,
6.68005860217229));
#281507=CARTESIAN_POINT('Ctrl Pts',(-0.431113031838807,-1.90584825045929,
6.67614781504533));
#281508=CARTESIAN_POINT('Ctrl Pts',(-0.498042245918241,-1.8907085055224,
6.67223027519358));
#281509=CARTESIAN_POINT('Ctrl Pts',(-0.564081695480184,-1.8720596188736,
6.66831273534183));
#281510=CARTESIAN_POINT('Ctrl Pts',(-0.628848376951741,-1.8500447883241,
6.66439519549009));
#281511=CARTESIAN_POINT('Ctrl Pts',(-0.659416659271667,-1.839654329215,
6.66254621293506));
#281512=CARTESIAN_POINT('Ctrl Pts',(-0.689701714196233,-1.82851476468504,
6.66069723038004));
#281513=CARTESIAN_POINT('Ctrl Pts',(-0.719665063562426,-1.81664476337222,
6.65884824782501));
#281514=CARTESIAN_POINT('Ctrl Pts',(-0.783159374109898,-1.79149144888976,
6.65493013202591));
#281515=CARTESIAN_POINT('Ctrl Pts',(-0.845459247551919,-1.76295544045873,
6.65101201622681));
#281516=CARTESIAN_POINT('Ctrl Pts',(-0.906179858676215,-1.73117129820522,
6.64709390042771));
#281517=CARTESIAN_POINT('Ctrl Pts',(-0.966809034367842,-1.69943501773612,
6.64318168467815));
#281518=CARTESIAN_POINT('Ctrl Pts',(-1.02586323517391,-1.66446053695241,
6.63926946892858));
#281519=CARTESIAN_POINT('Ctrl Pts',(-1.08297703407796,-1.62643067594647,
6.63535725317902));
#281520=CARTESIAN_POINT('Ctrl Pts',(-1.14002367037253,-1.58844553591432,
6.63144963797474));
#281521=CARTESIAN_POINT('Ctrl Pts',(-1.19513402897873,-1.54741242265076,
6.62754202277047));
#281522=CARTESIAN_POINT('Ctrl Pts',(-1.24796837050111,-1.5035594255728,
6.62363440756619));
#281523=CARTESIAN_POINT('Ctrl Pts',(-1.30076959746519,-1.4597339138876,
6.61972924150669));
#281524=CARTESIAN_POINT('Ctrl Pts',(-1.35129725946874,-1.41309233778612,
6.61582407544719));
#281525=CARTESIAN_POINT('Ctrl Pts',(-1.39924292182024,-1.36390441224302,
6.61191890938769));
#281526=CARTESIAN_POINT('Ctrl Pts',(-1.44717497824744,-1.31473044515117,
6.60801485152842));
#281527=CARTESIAN_POINT('Ctrl Pts',(-1.49252614641283,-1.26301191516475,
6.60411079366914));
#281528=CARTESIAN_POINT('Ctrl Pts',(-1.53502457552179,-1.20905564493291,
6.60020673580987));
#281529=CARTESIAN_POINT('Ctrl Pts',(-1.57752552033461,-1.15509618074779,
6.59630244684903));
#281530=CARTESIAN_POINT('Ctrl Pts',(-1.61717308848852,-1.09889910132795,
6.59239815788819));
#281531=CARTESIAN_POINT('Ctrl Pts',(-1.65373662517302,-1.04080313919653,
6.58849386892735));
#281532=CARTESIAN_POINT('Ctrl Pts',(-1.69033910795774,-0.982645295437449,
6.58458542126517));
#281533=CARTESIAN_POINT('Ctrl Pts',(-1.72385074093752,-0.922584949540845,
6.58067697360298));
#281534=CARTESIAN_POINT('Ctrl Pts',(-1.75408556887754,-0.860987698550653,
6.5767685259408));
#281535=CARTESIAN_POINT('Ctrl Pts',(-1.78433849436452,-0.799353577526197,
6.57285773881384));
#281536=CARTESIAN_POINT('Ctrl Pts',(-1.81131051812368,-0.736181172993751,
6.56894695168687));
#281537=CARTESIAN_POINT('Ctrl Pts',(-1.83486395345815,-0.671855841903561,
6.56503616455991));
#281538=CARTESIAN_POINT('Ctrl Pts',(-1.85845805832061,-0.607419440779791,
6.56111862470816));
#281539=CARTESIAN_POINT('Ctrl Pts',(-1.87862164916358,-0.541826609799558,
6.55720108485641));
#281540=CARTESIAN_POINT('Ctrl Pts',(-1.89526722063687,-0.475476773753879,
6.55328354500467));
#281541=CARTESIAN_POINT('Ctrl Pts',(-1.90312352138613,-0.444161281373481,
6.55143456244964));
#281542=CARTESIAN_POINT('Ctrl Pts',(-1.91019688938173,-0.412677286790502,
6.54958557989462));
#281543=CARTESIAN_POINT('Ctrl Pts',(-1.91648213078546,-0.381067241284289,
6.54773659733959));
#281544=CARTESIAN_POINT('Ctrl Pts',(-1.93570543873075,-0.284388434553022,
6.54208151446248));
#281545=CARTESIAN_POINT('Ctrl Pts',(-1.94761790070022,-0.186211271518132,
6.53642643158537));
#281546=CARTESIAN_POINT('Ctrl Pts',(-1.95204230768552,-0.0874461491764296,
6.53077134870826));
#281547=CARTESIAN_POINT('Ctrl Pts',(-1.9533206222037,-0.0589105984917037,
6.52913746318025));
#281548=CARTESIAN_POINT('Ctrl Pts',(-1.95397413257682,-0.0303261369517731,
6.52750357765225));
#281549=CARTESIAN_POINT('Ctrl Pts',(-1.95399924719281,-0.00171521716542704,
6.52586969212424));
#281550=CARTESIAN_POINT('',(-1.95079815420139,-3.45302974047446E-5,5.82586969212423));
#281551=CARTESIAN_POINT('Ctrl Pts',(-1.95470925949157,-0.0017091530386519,
6.52586931036698));
#281552=CARTESIAN_POINT('Ctrl Pts',(-1.94992763104345,0.51940321820411,
6.49612118919603));
#281553=CARTESIAN_POINT('Ctrl Pts',(-1.46756271540364,1.69712511346729,
6.42933585119661));
#281554=CARTESIAN_POINT('Ctrl Pts',(0.521076907609903,2.2497876261868,6.32551329636871));
#281555=CARTESIAN_POINT('Ctrl Pts',(2.17259204728733,0.782885242326123,
6.21440164588327));
#281556=CARTESIAN_POINT('Ctrl Pts',(1.83636881720092,-1.40029106752842,
6.10328999539785));
#281557=CARTESIAN_POINT('Ctrl Pts',(-0.179976902307915,-2.30231922661122,
5.99217834491238));
#281558=CARTESIAN_POINT('Ctrl Pts',(-1.72105200304095,-1.29994935931744,
5.89970491048787));
#281559=CARTESIAN_POINT('Ctrl Pts',(-1.95084923717034,-0.323977343102287,
5.84426869289181));
#281560=CARTESIAN_POINT('Ctrl Pts',(-1.95079815420139,-3.45302974047446E-5,
5.82586969212423));
#281561=CARTESIAN_POINT('',(-1.95399923068592,0.0017339200773292,5.12586969212423));
#281562=CARTESIAN_POINT('Ctrl Pts',(-1.95079815420139,-3.45302974047446E-5,
5.82586969212423));
#281563=CARTESIAN_POINT('Ctrl Pts',(-1.95074640707532,0.328120037045956,
5.80723147606333));
#281564=CARTESIAN_POINT('Ctrl Pts',(-1.71664579075019,1.30844134569539,
5.75155604317396));
#281565=CARTESIAN_POINT('Ctrl Pts',(-0.165142710425363,2.30343078727822,
5.65884339345609));
#281566=CARTESIAN_POINT('Ctrl Pts',(1.84535073495004,1.38843299139978,5.54773174297065));
#281567=CARTESIAN_POINT('Ctrl Pts',(2.16750399418151,-0.796863816342125,
5.43662009248521));
#281568=CARTESIAN_POINT('Ctrl Pts',(0.506574022840454,-2.2530974825717,
5.32550844199979));
#281569=CARTESIAN_POINT('Ctrl Pts',(-1.47389109216557,-1.68893929938375,
5.22192508019049));
#281570=CARTESIAN_POINT('Ctrl Pts',(-1.94982185200388,-0.515279595154487,
5.1553789352097));
#281571=CARTESIAN_POINT('Ctrl Pts',(-1.9545826140287,0.00172892004169586,
5.12587000705737));
#281572=CARTESIAN_POINT('',(-1.95399970461562,-0.00107441242398919,4.42586969212423));
#281573=CARTESIAN_POINT('Ctrl Pts',(-1.95399923068592,0.0017339200773292,
5.12586969212423));
#281574=CARTESIAN_POINT('Ctrl Pts',(-1.95391275218654,0.0991887702010741,
5.12030561986702));
#281575=CARTESIAN_POINT('Ctrl Pts',(-1.94653201774855,0.196330965052306,
5.1147415476098));
#281576=CARTESIAN_POINT('Ctrl Pts',(-1.93201679707086,0.292279140268442,
5.10917747535259));
#281577=CARTESIAN_POINT('Ctrl Pts',(-1.92689293999513,0.326148741523638,
5.10721336391136));
#281578=CARTESIAN_POINT('Ctrl Pts',(-1.92088046947136,0.359869837291548,
5.10524925247014));
#281579=CARTESIAN_POINT('Ctrl Pts',(-1.91398771378947,0.393404412104079,
5.10328514102891));
#281580=CARTESIAN_POINT('Ctrl Pts',(-1.90023767172484,0.460300996804353,
5.09936702522981));
#281581=CARTESIAN_POINT('Ctrl Pts',(-1.88294895453001,0.526608449370511,
5.09544890943072));
#281582=CARTESIAN_POINT('Ctrl Pts',(-1.86218728113428,0.591924429282757,
5.09153079363163));
#281583=CARTESIAN_POINT('Ctrl Pts',(-1.84145687146522,0.657142053879186,
5.08761857788206));
#281584=CARTESIAN_POINT('Ctrl Pts',(-1.81726403252631,0.721370703896118,
5.0837063621325));
#281585=CARTESIAN_POINT('Ctrl Pts',(-1.78972537777022,0.784218765501848,
5.07979414638294));
#281586=CARTESIAN_POINT('Ctrl Pts',(-1.76221910692048,0.846992921328244,
5.07588653117867));
#281587=CARTESIAN_POINT('Ctrl Pts',(-1.7313750306896,0.9083892646335,5.0719789159744));
#281588=CARTESIAN_POINT('Ctrl Pts',(-1.69735880353875,0.968033621342521,
5.06807130077013));
#281589=CARTESIAN_POINT('Ctrl Pts',(-1.66336389646694,1.02764059523439,
5.06416613471064));
#281590=CARTESIAN_POINT('Ctrl Pts',(-1.62620102553603,1.08549733445233,
5.06026096865114));
#281591=CARTESIAN_POINT('Ctrl Pts',(-1.58608227278411,1.14125326898108,
5.05635580259165));
#281592=CARTESIAN_POINT('Ctrl Pts',(-1.54597490485169,1.19699338120212,
5.05245174473238));
#281593=CARTESIAN_POINT('Ctrl Pts',(-1.50291360744137,1.25063347314136,
5.0485476868731));
#281594=CARTESIAN_POINT('Ctrl Pts',(-1.45715335723846,1.30185256211626,
5.04464362901383));
#281595=CARTESIAN_POINT('Ctrl Pts',(-1.41139039824741,1.35307468301649,
5.04073934005299));
#281596=CARTESIAN_POINT('Ctrl Pts',(-1.36292849890078,1.40187515132943,
5.03683505109215));
#281597=CARTESIAN_POINT('Ctrl Pts',(-1.31206121220845,1.44796801602041,
5.0329307621313));
#281598=CARTESIAN_POINT('Ctrl Pts',(-1.261139743601,1.49410997709229,5.02902231446912));
#281599=CARTESIAN_POINT('Ctrl Pts',(-1.2078081396301,1.53753824797739,5.02511386680695));
#281600=CARTESIAN_POINT('Ctrl Pts',(-1.15239416902623,1.57800623547385,
5.02120541914477));
#281601=CARTESIAN_POINT('Ctrl Pts',(-1.09694702949092,1.618498445741,5.01729463201781));
#281602=CARTESIAN_POINT('Ctrl Pts',(-1.03941545472426,1.65602657738826,
5.01338384489085));
#281603=CARTESIAN_POINT('Ctrl Pts',(-0.980155051919915,1.69038814305942,
5.00947305776389));
#281604=CARTESIAN_POINT('Ctrl Pts',(-0.920792324653062,1.72480904057059,
5.00555551791215));
#281605=CARTESIAN_POINT('Ctrl Pts',(-0.859695249169783,1.7560522356547,
5.0016379780604));
#281606=CARTESIAN_POINT('Ctrl Pts',(-0.797241997497702,1.78396221860943,
4.99772043820866));
#281607=CARTESIAN_POINT('Ctrl Pts',(-0.767765597200889,1.79713504480862,
4.9958714556536));
#281608=CARTESIAN_POINT('Ctrl Pts',(-0.737987350060903,1.80956607240149,
4.99402247309853));
#281609=CARTESIAN_POINT('Ctrl Pts',(-0.707948161372474,1.82124281764111,
4.99217349054347));
#281610=CARTESIAN_POINT('Ctrl Pts',(-0.644293142308056,1.84598660977705,
4.98825537474437));
#281611=CARTESIAN_POINT('Ctrl Pts',(-0.579213130476493,1.86743818473269,
4.98433725894526));
#281612=CARTESIAN_POINT('Ctrl Pts',(-0.513081758693453,1.88543446157538,
4.98041914314616));
#281613=CARTESIAN_POINT('Ctrl Pts',(-0.447049970074688,1.90340363893192,
4.97650692739659));
#281614=CARTESIAN_POINT('Ctrl Pts',(-0.379970434354915,1.91792771640892,
4.97259471164702));
#281615=CARTESIAN_POINT('Ctrl Pts',(-0.312235386052087,1.9288921856073,
4.96868249589746));
#281616=CARTESIAN_POINT('Ctrl Pts',(-0.244579990349595,1.93984376120769,
4.96477488069318));
#281617=CARTESIAN_POINT('Ctrl Pts',(-0.17627109623671,1.94724396356192,
4.9608672654889));
#281618=CARTESIAN_POINT('Ctrl Pts',(-0.107712895154416,1.95102894192205,
4.95695965028463));
#281619=CARTESIAN_POINT('Ctrl Pts',(-0.0391976637483059,1.95481154800151,
4.95305448422512));
#281620=CARTESIAN_POINT('Ctrl Pts',(0.0295660746347592,1.95498339782931,
4.94914931816562));
#281621=CARTESIAN_POINT('Ctrl Pts',(0.0981687677183626,1.9515324473461,
4.94524415210612));
#281622=CARTESIAN_POINT('Ctrl Pts',(0.166751992866778,1.94808247616672,
4.94134009424684));
#281623=CARTESIAN_POINT('Ctrl Pts',(0.235173772411825,1.94101177027437,
4.93743603638756));
#281624=CARTESIAN_POINT('Ctrl Pts',(0.303026136125135,1.93036037071451,
4.93353197852828));
#281625=CARTESIAN_POINT('Ctrl Pts',(0.370882516374091,1.9197083406427,4.92962768956744));
#281626=CARTESIAN_POINT('Ctrl Pts',(0.4381689283419,1.90547527490298,4.92572340060659));
#281627=CARTESIAN_POINT('Ctrl Pts',(0.50448590010067,1.88775262590193,4.92181911164575));
#281628=CARTESIAN_POINT('Ctrl Pts',(0.570873510196411,1.87001109940362,
4.91791066398356));
#281629=CARTESIAN_POINT('Ctrl Pts',(0.636289143194882,1.84877269895529,
4.91400221632138));
#281630=CARTESIAN_POINT('Ctrl Pts',(0.700347825399189,1.82417897243078,
4.9100937686592));
#281631=CARTESIAN_POINT('Ctrl Pts',(0.764444850967365,1.79957052493212,
4.90618298153223));
#281632=CARTESIAN_POINT('Ctrl Pts',(0.827182859940686,1.77160295460249,
4.90227219440527));
#281633=CARTESIAN_POINT('Ctrl Pts',(0.888198825250868,1.74046512370199,
4.8983614072783));
#281634=CARTESIAN_POINT('Ctrl Pts',(0.949320146339253,1.70927352735847,
4.89444386742655));
#281635=CARTESIAN_POINT('Ctrl Pts',(1.00871306375764,1.67490099134177,4.89052632757481));
#281636=CARTESIAN_POINT('Ctrl Pts',(1.06604177063362,1.63758082037631,4.88660878772306));
#281637=CARTESIAN_POINT('Ctrl Pts',(1.09309951169722,1.61996661664732,4.88475980516805));
#281638=CARTESIAN_POINT('Ctrl Pts',(1.11969788540273,1.60169639590686,4.88291082261304));
#281639=CARTESIAN_POINT('Ctrl Pts',(1.1458042121979,1.58279774681087,4.88106184005803));
#281640=CARTESIAN_POINT('Ctrl Pts',(1.20112523791307,1.54275026480297,4.87714372425893));
#281641=CARTESIAN_POINT('Ctrl Pts',(1.25445382591107,1.49971958144554,4.87322560845983));
#281642=CARTESIAN_POINT('Ctrl Pts',(1.30545027198386,1.45393108068342,4.86930749266073));
#281643=CARTESIAN_POINT('Ctrl Pts',(1.3563699256459,1.40821153000761,4.86539527691117));
#281644=CARTESIAN_POINT('Ctrl Pts',(1.40496404406613,1.35974272979661,4.8614830611616));
#281645=CARTESIAN_POINT('Ctrl Pts',(1.45092363314304,1.30879204260531,4.85757084541203));
#281646=CARTESIAN_POINT('Ctrl Pts',(1.49682917633276,1.25790127055138,4.85366323020776));
#281647=CARTESIAN_POINT('Ctrl Pts',(1.54010601506789,1.20453477133229,4.84975561500348));
#281648=CARTESIAN_POINT('Ctrl Pts',(1.58048122198482,1.14899743557302,4.84584799979921));
#281649=CARTESIAN_POINT('Ctrl Pts',(1.62083112325575,1.09349490850615,4.84194283373971));
#281650=CARTESIAN_POINT('Ctrl Pts',(1.65828271171005,1.03582464085439,4.8380376676802));
#281651=CARTESIAN_POINT('Ctrl Pts',(1.69260367060217,0.976324133812159,
4.8341325016207));
#281652=CARTESIAN_POINT('Ctrl Pts',(1.72691488996115,0.916840511704942,
4.83022844376143));
#281653=CARTESIAN_POINT('Ctrl Pts',(1.75809699773753,0.855528107148066,
4.82632438590215));
#281654=CARTESIAN_POINT('Ctrl Pts',(1.78596228848867,0.792751350737605,
4.82242032804287));
#281655=CARTESIAN_POINT('Ctrl Pts',(1.81382922873186,0.729970878243186,
4.81851603908202));
#281656=CARTESIAN_POINT('Ctrl Pts',(1.83837876493259,0.66572633241881,4.81461175012118));
#281657=CARTESIAN_POINT('Ctrl Pts',(1.85947098934597,0.60040289787835,4.81070746116033));
#281658=CARTESIAN_POINT('Ctrl Pts',(1.88058568040124,0.535009883279296,
4.80679901349815));
#281659=CARTESIAN_POINT('Ctrl Pts',(1.89823555891359,0.468536155516436,
4.80289056583597));
#281660=CARTESIAN_POINT('Ctrl Pts',(1.91233066466294,0.401381899180544,
4.79898211817378));
#281661=CARTESIAN_POINT('Ctrl Pts',(1.9264342072666,0.334187446574648,4.79507133104682));
#281662=CARTESIAN_POINT('Ctrl Pts',(1.9369786669408,0.266312140827596,4.79116054391985));
#281663=CARTESIAN_POINT('Ctrl Pts',(1.94392573587282,0.198163400786621,
4.78724975679289));
#281664=CARTESIAN_POINT('Ctrl Pts',(1.95088480025308,0.129896988862477,
4.78333221694114));
#281665=CARTESIAN_POINT('Ctrl Pts',(1.95423405256825,0.0613566913681232,
4.77941467708939));
#281666=CARTESIAN_POINT('Ctrl Pts',(1.95398728604934,-0.00704882667864861,
4.77549713723764));
#281667=CARTESIAN_POINT('Ctrl Pts',(1.95387081831553,-0.0393345504547654,
4.77364815468263));
#281668=CARTESIAN_POINT('Ctrl Pts',(1.95295405138724,-0.0715903094458734,
4.77179917212761));
#281669=CARTESIAN_POINT('Ctrl Pts',(1.95124243048703,-0.103773683885063,
4.76995018957259));
#281670=CARTESIAN_POINT('Ctrl Pts',(1.94761539308043,-0.171972373762527,
4.76603207377349));
#281671=CARTESIAN_POINT('Ctrl Pts',(1.94040139983398,-0.240115871687915,
4.76211395797439));
#281672=CARTESIAN_POINT('Ctrl Pts',(1.92960547582867,-0.307796536127403,
4.75819584217529));
#281673=CARTESIAN_POINT('Ctrl Pts',(1.91882580874114,-0.375375284418118,
4.75428362642573));
#281674=CARTESIAN_POINT('Ctrl Pts',(1.90447499255426,-0.442492100594856,
4.75037141067616));
#281675=CARTESIAN_POINT('Ctrl Pts',(1.88660997710864,-0.508742365322707,
4.74645919492659));
#281676=CARTESIAN_POINT('Ctrl Pts',(1.86876596991459,-0.574914723472059,
4.74255157972232));
#281677=CARTESIAN_POINT('Ctrl Pts',(1.84741609813031,-0.640222081285704,
4.73864396451804));
#281678=CARTESIAN_POINT('Ctrl Pts',(1.82266840397388,-0.704269755956704,
4.73473634931377));
#281679=CARTESIAN_POINT('Ctrl Pts',(1.79793622073208,-0.768277287978138,
4.73083118325427));
#281680=CARTESIAN_POINT('Ctrl Pts',(1.76981061650736,-0.831026245226591,
4.72692601719477));
#281681=CARTESIAN_POINT('Ctrl Pts',(1.73844906030112,-0.892138366363726,
4.72302085113527));
#281682=CARTESIAN_POINT('Ctrl Pts',(1.70709640381466,-0.953233145225211,
4.71911679327599));
#281683=CARTESIAN_POINT('Ctrl Pts',(1.67250984278654,-1.01269157266969,
4.71521273541672));
#281684=CARTESIAN_POINT('Ctrl Pts',(1.63489367119866,-1.07015825179015,
4.71130867755744));
#281685=CARTESIAN_POINT('Ctrl Pts',(1.5972752729132,-1.12762833266338,4.7074043885966));
#281686=CARTESIAN_POINT('Ctrl Pts',(1.55662717955417,-1.18310602099055,
4.70350009963575));
#281687=CARTESIAN_POINT('Ctrl Pts',(1.5131970513389,-1.23626481136497,4.69959581067491));
#281688=CARTESIAN_POINT('Ctrl Pts',(1.46972066298917,-1.28948022447783,
4.69568736301272));
#281689=CARTESIAN_POINT('Ctrl Pts',(1.42345663771862,-1.34037142862899,
4.69177891535054));
#281690=CARTESIAN_POINT('Ctrl Pts',(1.37469233479326,-1.38864573763817,
4.68787046768836));
#281691=CARTESIAN_POINT('Ctrl Pts',(1.32589884320296,-1.43694894201848,
4.6839596805614));
#281692=CARTESIAN_POINT('Ctrl Pts',(1.27460246286418,-1.48263180668583,
4.68004889343443));
#281693=CARTESIAN_POINT('Ctrl Pts',(1.22112465363547,-1.5254411100674,4.67613810630747));
#281694=CARTESIAN_POINT('Ctrl Pts',(1.16755450470222,-1.56832433192997,
4.67222056645572));
#281695=CARTESIAN_POINT('Ctrl Pts',(1.11179580870225,-1.60832380307731,
4.66830302660398));
#281696=CARTESIAN_POINT('Ctrl Pts',(1.05419933932767,-1.64522939220071,
4.66438548675223));
#281697=CARTESIAN_POINT('Ctrl Pts',(1.02701522094348,-1.66264792348678,
4.6625365041972));
#281698=CARTESIAN_POINT('Ctrl Pts',(0.999422077750991,-1.67937792344079,
4.66068752164218));
#281699=CARTESIAN_POINT('Ctrl Pts',(0.971458497828496,-1.69540095169161,
4.65883853908715));
#281700=CARTESIAN_POINT('Ctrl Pts',(0.912201830427331,-1.72935480375381,
4.65492042328805));
#281701=CARTESIAN_POINT('Ctrl Pts',(0.851045450939923,-1.76026556654062,
4.65100230748895));
#281702=CARTESIAN_POINT('Ctrl Pts',(0.788334516211265,-1.78791629853021,
4.64708419168985));
#281703=CARTESIAN_POINT('Ctrl Pts',(0.725718014021166,-1.81552539298359,
4.64317197594028));
#281704=CARTESIAN_POINT('Ctrl Pts',(0.661552048916903,-1.83988400257387,
4.63925976019072));
#281705=CARTESIAN_POINT('Ctrl Pts',(0.596207410383258,-1.86082044373015,
4.63534754444115));
#281706=CARTESIAN_POINT('Ctrl Pts',(0.530939613462734,-1.88173226481129,
4.63143992923688));
#281707=CARTESIAN_POINT('Ctrl Pts',(0.464496362042833,-1.89922976036229,
4.6275323140326));
#281708=CARTESIAN_POINT('Ctrl Pts',(0.39726781841187,-1.91318955685376,
4.62362469882833));
#281709=CARTESIAN_POINT('Ctrl Pts',(0.330081411078304,-1.92714060387506,
4.61971953276883));
#281710=CARTESIAN_POINT('Ctrl Pts',(0.262111168410904,-1.93755825046676,
4.61581436670933));
#281711=CARTESIAN_POINT('Ctrl Pts',(0.193760274311138,-1.94436955234823,
4.61190920064983));
#281712=CARTESIAN_POINT('Ctrl Pts',(0.125428776691556,-1.95117892133206,
4.60800514279055));
#281713=CARTESIAN_POINT('Ctrl Pts',(0.0567173313050693,-1.95438392848071,
4.60410108493127));
#281714=CARTESIAN_POINT('Ctrl Pts',(-0.0119646801941463,-1.95396336875282,
4.600197027072));
#281715=CARTESIAN_POINT('Ctrl Pts',(-0.0806507573402421,-1.95354278412979,
4.59629273811115));
#281716=CARTESIAN_POINT('Ctrl Pts',(-0.149306905286468,-1.94949621211857,
4.5923884491503));
#281717=CARTESIAN_POINT('Ctrl Pts',(-0.217524484051122,-1.94185455141169,
4.58848416018946));
#281718=CARTESIAN_POINT('Ctrl Pts',(-0.285814725607615,-1.93420475109606,
4.58457571252727));
#281719=CARTESIAN_POINT('Ctrl Pts',(-0.353664975939816,-1.92295227474412,
4.58066726486509));
#281720=CARTESIAN_POINT('Ctrl Pts',(-0.420673465772656,-1.90817971774014,
4.5767588172029));
#281721=CARTESIAN_POINT('Ctrl Pts',(-0.487722064624607,-1.8933983183824,
4.57284803007594));
#281722=CARTESIAN_POINT('Ctrl Pts',(-0.553927426067727,-1.87509277615426,
4.56893724294897));
#281723=CARTESIAN_POINT('Ctrl Pts',(-0.618902431213532,-1.85339574312611,
4.56502645582201));
#281724=CARTESIAN_POINT('Ctrl Pts',(-0.683989628179872,-1.83166124600495,
4.56110891597026));
#281725=CARTESIAN_POINT('Ctrl Pts',(-0.747841771348525,-1.8065237504166,
4.55719137611851));
#281726=CARTESIAN_POINT('Ctrl Pts',(-0.8100920348914,-1.7781639111751,4.55327383626677));
#281727=CARTESIAN_POINT('Ctrl Pts',(-0.839472629777884,-1.764778763862,
4.55142485371175));
#281728=CARTESIAN_POINT('Ctrl Pts',(-0.868496751906081,-1.75067646673078,
4.54957587115674));
#281729=CARTESIAN_POINT('Ctrl Pts',(-0.897127975177005,-1.73587943018944,
4.54772688860172));
#281730=CARTESIAN_POINT('Ctrl Pts',(-0.957799422801613,-1.70452353529726,
4.54380877280262));
#281731=CARTESIAN_POINT('Ctrl Pts',(-1.01694526252404,-1.66992082367519,
4.53989065700352));
#281732=CARTESIAN_POINT('Ctrl Pts',(-1.07419599511933,-1.63224353699734,
4.53597254120442));
#281733=CARTESIAN_POINT('Ctrl Pts',(-1.1313605173585,-1.59462298622758,
4.53206032545485));
#281734=CARTESIAN_POINT('Ctrl Pts',(-1.18663518852539,-1.55393731717425,
4.52814810970529));
#281735=CARTESIAN_POINT('Ctrl Pts',(-1.23967462057726,-1.51040485800881,
4.52423589395573));
#281736=CARTESIAN_POINT('Ctrl Pts',(-1.29265168124554,-1.46692359056253,
4.52032827875145));
#281737=CARTESIAN_POINT('Ctrl Pts',(-1.3433983446566,-1.42060249210352,
4.51642066354718));
#281738=CARTESIAN_POINT('Ctrl Pts',(-1.39159929401837,-1.37170237474737,
4.5125130483429));
#281739=CARTESIAN_POINT('Ctrl Pts',(-1.43977003285607,-1.32283290612723,
4.5086078822834));
#281740=CARTESIAN_POINT('Ctrl Pts',(-1.48539787819898,-1.27138797461653,
4.5047027162239));
#281741=CARTESIAN_POINT('Ctrl Pts',(-1.52820281048915,-1.21766669085307,
4.5007975501644));
#281742=CARTESIAN_POINT('Ctrl Pts',(-1.57099559568114,-1.1639606520082,
4.49689349230512));
#281743=CARTESIAN_POINT('Ctrl Pts',(-1.61096675172384,-1.10797992780303,
4.49298943444584));
#281744=CARTESIAN_POINT('Ctrl Pts',(-1.64787635895505,-1.05005690588513,
4.48908537658657));
#281745=CARTESIAN_POINT('Ctrl Pts',(-1.68478815105862,-0.992130455201143,
4.48518108762572));
#281746=CARTESIAN_POINT('Ctrl Pts',(-1.71863777238092,-0.932261894735825,
4.48127679866488));
#281747=CARTESIAN_POINT('Ctrl Pts',(-1.74922947427241,-0.870811257584943,
4.47737250970403));
#281748=CARTESIAN_POINT('Ctrl Pts',(-1.77985376129089,-0.80929516553319,
4.47346406204185));
#281749=CARTESIAN_POINT('Ctrl Pts',(-1.80721298377762,-0.746194074899896,
4.46955561437967));
#281750=CARTESIAN_POINT('Ctrl Pts',(-1.83115854742829,-0.681890294827787,
4.46564716671748));
#281751=CARTESIAN_POINT('Ctrl Pts',(-1.85511844408471,-0.617548024684482,
4.46173637959052));
#281752=CARTESIAN_POINT('Ctrl Pts',(-1.87566046823998,-0.552002101823619,
4.45782559246356));
#281753=CARTESIAN_POINT('Ctrl Pts',(-1.89268602308817,-0.485649686509395,
4.45391480533659));
#281754=CARTESIAN_POINT('Ctrl Pts',(-1.90974097582545,-0.419182701011528,
4.44999726548484));
#281755=CARTESIAN_POINT('Ctrl Pts',(-1.9232672438945,-0.351906925699697,
4.4460797256331));
#281756=CARTESIAN_POINT('Ctrl Pts',(-1.93321756400612,-0.284228517602009,
4.44216218578135));
#281757=CARTESIAN_POINT('Ctrl Pts',(-1.93791387061678,-0.252285971856508,
4.44031320322633));
#281758=CARTESIAN_POINT('Ctrl Pts',(-1.94181434939227,-0.220253789367341,
4.43846422067131));
#281759=CARTESIAN_POINT('Ctrl Pts',(-1.94491806301935,-0.188174727689601,
4.43661523811628));
#281760=CARTESIAN_POINT('Ctrl Pts',(-1.95093057648437,-0.126031175333595,
4.43303338945227));
#281761=CARTESIAN_POINT('Ctrl Pts',(-1.95396532753133,-0.0635949222937433,
4.42945154078825));
#281762=CARTESIAN_POINT('Ctrl Pts',(-1.95399970461562,-0.00107441242398919,
4.42586969212423));
#281763=CARTESIAN_POINT('',(-1.95135107115213,-0.00103745302926256,3.72586969212423));
#281764=CARTESIAN_POINT('Ctrl Pts',(-1.95645563342917,-0.00105870546452921,
4.42586871612197));
#281765=CARTESIAN_POINT('Ctrl Pts',(-1.95257657647916,0.583629271897111,
4.3924136732916));
#281766=CARTESIAN_POINT('Ctrl Pts',(-1.36373841242988,1.82237443771501,
4.32192141363275));
#281767=CARTESIAN_POINT('Ctrl Pts',(0.742695215461096,2.18665711155625,
4.21439193714541));
#281768=CARTESIAN_POINT('Ctrl Pts',(2.23979789625715,0.562468568463699,
4.10328028665997));
#281769=CARTESIAN_POINT('Ctrl Pts',(1.68767452724564,-1.57633124585983,
3.99216863617453));
#281770=CARTESIAN_POINT('Ctrl Pts',(-0.408528604769658,-2.272921002955,
3.88105698568911));
#281771=CARTESIAN_POINT('Ctrl Pts',(-1.78456893999856,-1.16809907040787,
3.79229067100566));
#281772=CARTESIAN_POINT('Ctrl Pts',(-1.9525967846073,-0.259527562563923,
3.74056157315071));
#281773=CARTESIAN_POINT('Ctrl Pts',(-1.95135107115213,-0.00103745302926256,
3.72586969212423));
#281774=CARTESIAN_POINT('',(-1.95399929791996,0.00165642032925726,3.02586967147267));
#281775=CARTESIAN_POINT('Ctrl Pts',(-1.95135107115213,-0.00103745302926256,
3.72586969212423));
#281776=CARTESIAN_POINT('Ctrl Pts',(-1.9494564270682,0.392108141373472,
3.70352435632223));
#281777=CARTESIAN_POINT('Ctrl Pts',(-1.64339421395861,1.43960318986175,
3.64414180369176));
#281778=CARTESIAN_POINT('Ctrl Pts',(0.0652379087403862,2.30842143506328,
3.54772203423277));
#281779=CARTESIAN_POINT('Ctrl Pts',(1.97453422882562,1.19761433098204,3.43661038374736));
#281780=CARTESIAN_POINT('Ctrl Pts',(2.07729836817095,-1.00890881459804,
3.32549873326191));
#281781=CARTESIAN_POINT('Ctrl Pts',(0.279509811935439,-2.29236554058799,
3.21438708277647));
#281782=CARTESIAN_POINT('Ctrl Pts',(-1.5663607178597,-1.56079696856402,
3.11451073573059));
#281783=CARTESIAN_POINT('Ctrl Pts',(-1.94902846959061,-0.451530792879088,
3.05167160551317));
#281784=CARTESIAN_POINT('Ctrl Pts',(-1.95267691385146,0.00165493661177622,
3.02586969212423));
#281785=CARTESIAN_POINT('',(-1.95399999957489,4.07595347864031E-5,2.32586969217892));
#281786=CARTESIAN_POINT('Ctrl Pts',(-1.95399929791996,0.00165642032925726,
3.02586967147267));
#281787=CARTESIAN_POINT('Ctrl Pts',(-1.95392951629332,0.0839744449554839,
3.02118607042525));
#281788=CARTESIAN_POINT('Ctrl Pts',(-1.94865405009171,0.166066844841771,
3.01650246937784));
#281789=CARTESIAN_POINT('Ctrl Pts',(-1.93828099351015,0.247351551839267,
3.01181886833043));
#281790=CARTESIAN_POINT('Ctrl Pts',(-1.92776575156035,0.32975044306072,
3.00707106831384));
#281791=CARTESIAN_POINT('Ctrl Pts',(-1.91201229505569,0.411319330749024,
3.00232326829726));
#281792=CARTESIAN_POINT('Ctrl Pts',(-1.89118208470578,0.491473623389805,
2.99757546828068));
#281793=CARTESIAN_POINT('Ctrl Pts',(-1.88326778283756,0.521927721420327,
2.99577157278899));
#281794=CARTESIAN_POINT('Ctrl Pts',(-1.8746211078826,0.552177835310333,
2.9939676772973));
#281795=CARTESIAN_POINT('Ctrl Pts',(-1.86525270256443,0.582192713434385,
2.99216378180561));
#281796=CARTESIAN_POINT('Ctrl Pts',(-1.84490424166246,0.647385940375561,
2.98824566600711));
#281797=CARTESIAN_POINT('Ctrl Pts',(-1.82109343506899,0.711640305956234,
2.98432755020861));
#281798=CARTESIAN_POINT('Ctrl Pts',(-1.79392577154405,0.774562022171296,
2.98040943441011));
#281799=CARTESIAN_POINT('Ctrl Pts',(-1.76679901813221,0.837388988444973,
2.97649721866114));
#281800=CARTESIAN_POINT('Ctrl Pts',(-1.73632563335625,0.898886840098444,
2.97258500291217));
#281801=CARTESIAN_POINT('Ctrl Pts',(-1.70266067811188,0.958677534529514,
2.9686727871632));
#281802=CARTESIAN_POINT('Ctrl Pts',(-1.66903531095797,1.01839791847294,
2.96476517195951));
#281803=CARTESIAN_POINT('Ctrl Pts',(-1.63222606724913,1.07641470557962,
2.96085755675582));
#281804=CARTESIAN_POINT('Ctrl Pts',(-1.59243506670914,1.13237209357837,
2.95694994155213));
#281805=CARTESIAN_POINT('Ctrl Pts',(-1.55266900565673,1.188294409612,2.95304477549321));
#281806=CARTESIAN_POINT('Ctrl Pts',(-1.50992517939374,1.24215948701812,
2.94913960943428));
#281807=CARTESIAN_POINT('Ctrl Pts',(-1.46444955172051,1.2936396370186,2.94523444337536));
#281808=CARTESIAN_POINT('Ctrl Pts',(-1.41898682902996,1.34510517808504,
2.94133038551666));
#281809=CARTESIAN_POINT('Ctrl Pts',(-1.37079416937919,1.39418676681743,
2.93742632765796));
#281810=CARTESIAN_POINT('Ctrl Pts',(-1.32015726901447,1.44059042932689,
2.93352226979925));
#281811=CARTESIAN_POINT('Ctrl Pts',(-1.26951737118713,1.48699683871152,
2.92961798083897));
#281812=CARTESIAN_POINT('Ctrl Pts',(-1.21643330976193,1.53072467672382,
2.92571369187869));
#281813=CARTESIAN_POINT('Ctrl Pts',(-1.16122567402963,1.57151867121407,
2.92180940291841));
#281814=CARTESIAN_POINT('Ctrl Pts',(-1.10595923320594,1.61235611792867,
2.91790095525678));
#281815=CARTESIAN_POINT('Ctrl Pts',(-1.04856510027811,1.6502531916732,2.91399250759515));
#281816=CARTESIAN_POINT('Ctrl Pts',(-0.989393987541334,1.68499719210955,
2.91008405993352));
#281817=CARTESIAN_POINT('Ctrl Pts',(-0.930187456974603,1.7197619891313,
2.9061732728071));
#281818=CARTESIAN_POINT('Ctrl Pts',(-0.869202266529201,1.75136973035253,
2.90226248568068));
#281819=CARTESIAN_POINT('Ctrl Pts',(-0.806812432811743,1.77965437606868,
2.89835169855427));
#281820=CARTESIAN_POINT('Ctrl Pts',(-0.744314871068234,1.80798786065599,
2.89443415870305));
#281821=CARTESIAN_POINT('Ctrl Pts',(-0.680408283207271,1.83298661859123,
2.89051661885183));
#281822=CARTESIAN_POINT('Ctrl Pts',(-0.615484456569281,1.85453360274804,
2.88659907900062));
#281823=CARTESIAN_POINT('Ctrl Pts',(-0.584842005502758,1.86470324988448,
2.88475009644046));
#281824=CARTESIAN_POINT('Ctrl Pts',(-0.553973137488596,1.87410470950349,
2.88290111388031));
#281825=CARTESIAN_POINT('Ctrl Pts',(-0.522919798301886,1.88272963660317,
2.88105213132016));
#281826=CARTESIAN_POINT('Ctrl Pts',(-0.457115727740939,1.90100642506827,
2.87713401552196));
#281827=CARTESIAN_POINT('Ctrl Pts',(-0.390221858888982,1.91586537239888,
2.87321589972376));
#281828=CARTESIAN_POINT('Ctrl Pts',(-0.3226262170164,1.92718144555558,2.86929778392556));
#281829=CARTESIAN_POINT('Ctrl Pts',(-0.255132363262565,1.93848047853386,
2.86538556817691));
#281830=CARTESIAN_POINT('Ctrl Pts',(-0.186939315002833,1.94624714485532,
2.86147335242825));
#281831=CARTESIAN_POINT('Ctrl Pts',(-0.118448765895021,1.95040659603528,
2.8575611366796));
#281832=CARTESIAN_POINT('Ctrl Pts',(-0.0500387578140951,1.95456115593501,
2.85365352147625));
#281833=CARTESIAN_POINT('Ctrl Pts',(0.0186675676677738,1.95511689545972,
2.84974590627289));
#281834=CARTESIAN_POINT('Ctrl Pts',(0.0872616680058097,1.9520505632019,
2.84583829106954));
#281835=CARTESIAN_POINT('Ctrl Pts',(0.155812776167267,1.94898615280466,
2.84193312501097));
#281836=CARTESIAN_POINT('Ctrl Pts',(0.224251308427534,1.94230419585193,
2.8380279589524));
#281837=CARTESIAN_POINT('Ctrl Pts',(0.292168551116957,1.93203352396852,
2.83412279289382));
#281838=CARTESIAN_POINT('Ctrl Pts',(0.360066520386865,1.92176576667587,
2.83021873503548));
#281839=CARTESIAN_POINT('Ctrl Pts',(0.427443007631104,1.90791138966129,
2.82631467717713));
#281840=CARTESIAN_POINT('Ctrl Pts',(0.493896064121049,1.89055089268862,
2.82241061931879));
#281841=CARTESIAN_POINT('Ctrl Pts',(0.56035305431426,1.87318936805752,2.81850633035888));
#281842=CARTESIAN_POINT('Ctrl Pts',(0.625886029970531,1.85232143822732,
2.81460204139897));
#281843=CARTESIAN_POINT('Ctrl Pts',(0.690106621978033,1.82807791144198,
2.81069775243906));
#281844=CARTESIAN_POINT('Ctrl Pts',(0.75439561933792,1.80380856136631,2.80678930477781));
#281845=CARTESIAN_POINT('Ctrl Pts',(0.817368982204935,1.77615661276738,
2.80288085711657));
#281846=CARTESIAN_POINT('Ctrl Pts',(0.878657760003433,1.7453012750771,2.79897240945532));
#281847=CARTESIAN_POINT('Ctrl Pts',(0.939983223194562,1.71442746842368,
2.79506162232929));
#281848=CARTESIAN_POINT('Ctrl Pts',(0.999621667418628,1.68034670070226,
2.79115083520326));
#281849=CARTESIAN_POINT('Ctrl Pts',(1.05723069479197,1.64328307299433,2.78724004807723));
#281850=CARTESIAN_POINT('Ctrl Pts',(1.11493919521126,1.60615544781742,2.78332250822641));
#281851=CARTESIAN_POINT('Ctrl Pts',(1.17061088616287,1.56603497055071,2.77940496837559));
#281852=CARTESIAN_POINT('Ctrl Pts',(1.22393488355458,1.52318725074045,2.77548742852477));
#281853=CARTESIAN_POINT('Ctrl Pts',(1.24910250025779,1.50296417967416,2.77363844596142));
#281854=CARTESIAN_POINT('Ctrl Pts',(1.27374765826116,1.48213413776215,2.77178946339808));
#281855=CARTESIAN_POINT('Ctrl Pts',(1.29784059017172,1.46072783313755,2.76994048083473));
#281856=CARTESIAN_POINT('Ctrl Pts',(1.34889509935635,1.41536646408033,2.76602236503161));
#281857=CARTESIAN_POINT('Ctrl Pts',(1.39766978596067,1.36723531030175,2.76210424922848));
#281858=CARTESIAN_POINT('Ctrl Pts',(1.44384909857897,1.31659248840813,2.75818613342535));
#281859=CARTESIAN_POINT('Ctrl Pts',(1.48995887261158,1.26602592642419,2.75427391767175));
#281860=CARTESIAN_POINT('Ctrl Pts',(1.53348070031946,1.21295556312259,2.75036170191815));
#281861=CARTESIAN_POINT('Ctrl Pts',(1.57413377107873,1.15767822418384,2.74644948616455));
#281862=CARTESIAN_POINT('Ctrl Pts',(1.61473903611734,1.10246588828114,2.74254187095625));
#281863=CARTESIAN_POINT('Ctrl Pts',(1.65248195398085,1.04505212538573,2.73863425574794));
#281864=CARTESIAN_POINT('Ctrl Pts',(1.68712134125316,0.985767508030231,
2.73472664053963));
#281865=CARTESIAN_POINT('Ctrl Pts',(1.72173901787332,0.926520048020952,
2.73082147447611));
#281866=CARTESIAN_POINT('Ctrl Pts',(1.75325677492154,0.865404483324416,
2.72691630841259));
#281867=CARTESIAN_POINT('Ctrl Pts',(1.78147708737339,0.802779787465782,
2.72301114234906));
#281868=CARTESIAN_POINT('Ctrl Pts',(1.80968939152128,0.74017286311841,2.71910708448577));
#281869=CARTESIAN_POINT('Ctrl Pts',(1.83460590669313,0.676058106015654,
2.71520302662248));
#281870=CARTESIAN_POINT('Ctrl Pts',(1.85607618084242,0.610816839084709,
2.71129896875919));
#281871=CARTESIAN_POINT('Ctrl Pts',(1.87754772592922,0.545571710182866,
2.70739467979435));
#281872=CARTESIAN_POINT('Ctrl Pts',(1.89557247365616,0.479200407091641,
2.70349039082952));
#281873=CARTESIAN_POINT('Ctrl Pts',(1.91004960005145,0.412100139945747,
2.69958610186468));
#281874=CARTESIAN_POINT('Ctrl Pts',(1.92454214693551,0.34492840012718,2.69567765419855));
#281875=CARTESIAN_POINT('Ctrl Pts',(1.9354794272508,0.277026628409668,2.69176920653243));
#281876=CARTESIAN_POINT('Ctrl Pts',(1.94281181078051,0.208801982489967,
2.68786075886631));
#281877=CARTESIAN_POINT('Ctrl Pts',(1.95014858322734,0.140536499601684,
2.68394997173543));
#281878=CARTESIAN_POINT('Ctrl Pts',(1.95387613783361,0.0719482491074181,
2.68003918460455));
#281879=CARTESIAN_POINT('Ctrl Pts',(1.95399696060566,0.0034464392987964,
2.67612839747367));
#281880=CARTESIAN_POINT('Ctrl Pts',(1.95411799200142,-0.0651736520342156,
2.67221085761809));
#281881=CARTESIAN_POINT('Ctrl Pts',(1.95061988710443,-0.133706513809952,
2.66829331776251));
#281882=CARTESIAN_POINT('Ctrl Pts',(1.94355709777815,-0.201746890127626,
2.66437577790692));
#281883=CARTESIAN_POINT('Ctrl Pts',(1.9402236348186,-0.233860275325921,
2.66252679538771));
#281884=CARTESIAN_POINT('Ctrl Pts',(1.93609684316677,-0.265864087601263,
2.6606778128685));
#281885=CARTESIAN_POINT('Ctrl Pts',(1.93118636846368,-0.297716661038726,
2.65882883034929));
#281886=CARTESIAN_POINT('Ctrl Pts',(1.92078074899972,-0.365214363028623,
2.65491071455524));
#281887=CARTESIAN_POINT('Ctrl Pts',(1.90681153135665,-0.432299674055665,
2.65099259876119));
#281888=CARTESIAN_POINT('Ctrl Pts',(1.88932434089903,-0.498567482780869,
2.64707448296715));
#281889=CARTESIAN_POINT('Ctrl Pts',(1.87186348332563,-0.564735502889988,
2.64316226722262));
#281890=CARTESIAN_POINT('Ctrl Pts',(1.85089529109169,-0.630087992075255,
2.63925005147809));
#281891=CARTESIAN_POINT('Ctrl Pts',(1.82651675462935,-0.694228020940006,
2.63533783573356));
#281892=CARTESIAN_POINT('Ctrl Pts',(1.80216688595202,-0.758292624745466,
2.63143022053427));
#281893=CARTESIAN_POINT('Ctrl Pts',(1.7744148116385,-0.821147142249368,
2.62752260533498));
#281894=CARTESIAN_POINT('Ctrl Pts',(1.74340736987258,-0.882409622949545,
2.62361499013569));
#281895=CARTESIAN_POINT('Ctrl Pts',(1.71241936239306,-0.943633706654438,
2.61970982408114));
#281896=CARTESIAN_POINT('Ctrl Pts',(1.67818025647906,-1.00326729504705,
2.61580465802659));
#281897=CARTESIAN_POINT('Ctrl Pts',(1.64088443447867,-1.06094970318372,
2.61189949197204));
#281898=CARTESIAN_POINT('Ctrl Pts',(1.60359919621175,-1.11861574232244,
2.60799543411767));
#281899=CARTESIAN_POINT('Ctrl Pts',(1.56325923080096,-1.17433128753308,
2.6040913762633));
#281900=CARTESIAN_POINT('Ctrl Pts',(1.52010323380703,-1.22776307102365,
2.60018731840893));
#281901=CARTESIAN_POINT('Ctrl Pts',(1.47694468218376,-1.28119801742113,
2.59628302945295));
#281902=CARTESIAN_POINT('Ctrl Pts',(1.43097007908696,-1.33234855266104,
2.59237874049696));
#281903=CARTESIAN_POINT('Ctrl Pts',(1.38245839110996,-1.38091447847057,
2.58847445154098));
#281904=CARTESIAN_POINT('Ctrl Pts',(1.33389503031134,-1.42953213487382,
2.58456600388355));
#281905=CARTESIAN_POINT('Ctrl Pts',(1.28278953974889,-1.47555933897962,
2.58065755622612));
#281906=CARTESIAN_POINT('Ctrl Pts',(1.22945701702434,-1.5187334997588,2.57674910856869));
#281907=CARTESIAN_POINT('Ctrl Pts',(1.17609257125198,-1.56193350313323,
2.57283832144643));
#281908=CARTESIAN_POINT('Ctrl Pts',(1.12049883850661,-1.60227677553843,
2.56892753432417));
#281909=CARTESIAN_POINT('Ctrl Pts',(1.06302091419834,-1.63954339252638,
2.56501674720191));
#281910=CARTESIAN_POINT('Ctrl Pts',(1.00544374321688,-1.67687435748447,
2.56109920735473));
#281911=CARTESIAN_POINT('Ctrl Pts',(0.945976313404811,-1.71111781892955,
2.55718166750755));
#281912=CARTESIAN_POINT('Ctrl Pts',(0.884988593721316,-1.74209964955601,
2.55326412766038));
#281913=CARTESIAN_POINT('Ctrl Pts',(0.856203887799534,-1.75672231274344,
2.55141514506154));
#281914=CARTESIAN_POINT('Ctrl Pts',(0.827080811940253,-1.77061910918343,
2.54956616246269));
#281915=CARTESIAN_POINT('Ctrl Pts',(0.797659599874164,-1.78377553597099,
2.54771717986385));
#281916=CARTESIAN_POINT('Ctrl Pts',(0.735314115511668,-1.81165487006191,
2.54379906406891));
#281917=CARTESIAN_POINT('Ctrl Pts',(0.671381648945562,-1.83631694044419,
2.53988094827396));
#281918=CARTESIAN_POINT('Ctrl Pts',(0.606227258951757,-1.85758028373038,
2.53596283247901));
#281919=CARTESIAN_POINT('Ctrl Pts',(0.541170980946729,-1.87881160785565,
2.53205061673367));
#281920=CARTESIAN_POINT('Ctrl Pts',(0.474896895147722,-1.89665421079382,
2.52813840098833));
#281921=CARTESIAN_POINT('Ctrl Pts',(0.407791054982178,-1.9109742163296,
2.52422618524299));
#281922=CARTESIAN_POINT('Ctrl Pts',(0.340764127505167,-1.92527738234539,
2.52031857004302));
#281923=CARTESIAN_POINT('Ctrl Pts',(0.272907866947681,-1.93606607561432,
2.51641095484305));
#281924=CARTESIAN_POINT('Ctrl Pts',(0.204622788546888,-1.94325642013793,
2.51250333964308));
#281925=CARTESIAN_POINT('Ctrl Pts',(0.136380508640256,-1.95044225802664,
2.50859817358794));
#281926=CARTESIAN_POINT('Ctrl Pts',(0.0677104321158824,-1.95403416959126,
2.5046930075328));
#281927=CARTESIAN_POINT('Ctrl Pts',(-0.000978994749919834,-1.95399975475159,
2.50078784147765));
#281928=CARTESIAN_POINT('Ctrl Pts',(-0.0696489290666075,-1.9539653496781,
2.49688378362277));
#281929=CARTESIAN_POINT('Ctrl Pts',(-0.138337711174469,-1.95030666133077,
2.4929797257679));
#281930=CARTESIAN_POINT('Ctrl Pts',(-0.20663588419952,-1.94304338895483,
2.48907566791302));
#281931=CARTESIAN_POINT('Ctrl Pts',(-0.27493810014937,-1.93577968662795,
2.48517137895661));
#281932=CARTESIAN_POINT('Ctrl Pts',(-0.342849172261745,-1.92491103121688,
2.4812670900002));
#281933=CARTESIAN_POINT('Ctrl Pts',(-0.409965574268347,-1.91050889239355,
2.4773628010438));
#281934=CARTESIAN_POINT('Ctrl Pts',(-0.4771534661346,-1.89609141295522,
2.47345435338607));
#281935=CARTESIAN_POINT('Ctrl Pts',(-0.54354451678222,-1.87813304225664,
2.46954590572834));
#281936=CARTESIAN_POINT('Ctrl Pts',(-0.608747188504485,-1.85675600456492,
2.46563745807062));
#281937=CARTESIAN_POINT('Ctrl Pts',(-0.673988888343824,-1.83536617130045,
2.46172667094813));
#281938=CARTESIAN_POINT('Ctrl Pts',(-0.738040334862839,-1.81055377623571,
2.45781588382564));
#281939=CARTESIAN_POINT('Ctrl Pts',(-0.800529556424161,-1.78248939107399,
2.45390509670315));
#281940=CARTESIAN_POINT('Ctrl Pts',(-0.863126677623894,-1.75437654736318,
2.44998755685586));
#281941=CARTESIAN_POINT('Ctrl Pts',(-0.924155752904607,-1.72300073132777,
2.44607001700857));
#281942=CARTESIAN_POINT('Ctrl Pts',(-0.983269786586064,-1.68857825604471,
2.44215247716128));
#281943=CARTESIAN_POINT('Ctrl Pts',(-1.0111701586603,-1.67233169311705,
2.440303494567));
#281944=CARTESIAN_POINT('Ctrl Pts',(-1.03864436191482,-1.65540707644465,
2.43845451197271));
#281945=CARTESIAN_POINT('Ctrl Pts',(-1.06565838499897,-1.6378303350718,
2.43660552937842));
#281946=CARTESIAN_POINT('Ctrl Pts',(-1.12286817424463,-1.60060664327163,
2.43268978886808));
#281947=CARTESIAN_POINT('Ctrl Pts',(-1.1782393626528,-1.56030757388963,
2.42877404835773));
#281948=CARTESIAN_POINT('Ctrl Pts',(-1.23142170315873,-1.51714092588317,
2.42485830784739));
#281949=CARTESIAN_POINT('Ctrl Pts',(-1.28452393606371,-1.47403929902058,
2.42094846554639));
#281950=CARTESIAN_POINT('Ctrl Pts',(-1.33544348490811,-1.42807897357161,
2.4170386232454));
#281951=CARTESIAN_POINT('Ctrl Pts',(-1.38385866196428,-1.37951121913033,
2.41312878094441));
#281952=CARTESIAN_POINT('Ctrl Pts',(-1.43221697663889,-1.33100050626882,
2.40922353065275));
#281953=CARTESIAN_POINT('Ctrl Pts',(-1.47807641473515,-1.27988879327852,
2.40531828036108));
#281954=CARTESIAN_POINT('Ctrl Pts',(-1.52114942784154,-1.22646663965123,
2.40141303006942));
#281955=CARTESIAN_POINT('Ctrl Pts',(-1.56419553052912,-1.17307786220135,
2.3975102196331));
#281956=CARTESIAN_POINT('Ctrl Pts',(-1.60445835293725,-1.11738189000708,
2.39360740919677));
#281957=CARTESIAN_POINT('Ctrl Pts',(-1.64168927749648,-1.05970388135228,
2.38970459876044));
#281958=CARTESIAN_POINT('Ctrl Pts',(-1.67890975389446,-1.00204205894968,
2.38580288357472));
#281959=CARTESIAN_POINT('Ctrl Pts',(-1.71309975449227,-0.942399717911359,
2.38190116838901));
#281960=CARTESIAN_POINT('Ctrl Pts',(-1.74405387701279,-0.881131133303468,
2.37799945320329));
#281961=CARTESIAN_POINT('Ctrl Pts',(-1.77500996482794,-0.819858658718724,
2.37409749029548));
#281962=CARTESIAN_POINT('Ctrl Pts',(-1.80272954693807,-0.756960176404744,
2.37019552738768));
#281963=CARTESIAN_POINT('Ctrl Pts',(-1.82705392995528,-0.692813060670033,
2.36629356447987));
#281964=CARTESIAN_POINT('Ctrl Pts',(-1.85140426136989,-0.628597515045426,
2.36238743909509));
#281965=CARTESIAN_POINT('Ctrl Pts',(-1.87235199103844,-0.563131139338323,
2.35848131371031));
#281966=CARTESIAN_POINT('Ctrl Pts',(-1.88978757097154,-0.496808752541134,
2.35457518832553));
#281967=CARTESIAN_POINT('Ctrl Pts',(-1.90723369128881,-0.430446271669736,
2.35066670155889));
#281968=CARTESIAN_POINT('Ctrl Pts',(-1.92116333674189,-0.363227232231232,
2.34675821479225));
#281969=CARTESIAN_POINT('Ctrl Pts',(-1.93151819040856,-0.29555622159051,
2.34284972802561));
#281970=CARTESIAN_POINT('Ctrl Pts',(-1.94189083526254,-0.227768942032294,
2.33893452589413));
#281971=CARTESIAN_POINT('Ctrl Pts',(-1.94867638232009,-0.159528631298684,
2.33501932376265));
#281972=CARTESIAN_POINT('Ctrl Pts',(-1.95186848814308,-0.0912436572812458,
2.33110412163118));
#281973=CARTESIAN_POINT('Ctrl Pts',(-1.95329105009292,-0.0608124588279669,
2.32935931181376));
#281974=CARTESIAN_POINT('Ctrl Pts',(-1.95400063397863,-0.0303723674190441,
2.32761450199634));
#281975=CARTESIAN_POINT('Ctrl Pts',(-1.95399999957489,4.07595347913703E-5,
2.32586969217892));
#281976=CARTESIAN_POINT('',(-1.9539992755619,-0.00168258835255015,1.62586971130332));
#281977=CARTESIAN_POINT('Ctrl Pts',(-1.95399999957487,4.07604881466012E-5,
2.32586969212423));
#281978=CARTESIAN_POINT('Ctrl Pts',(-1.95399995402589,0.00222431375158761,
2.32574442104715));
#281979=CARTESIAN_POINT('Ctrl Pts',(-1.95399624836735,0.00440786249150779,
2.32561914997006));
#281980=CARTESIAN_POINT('Ctrl Pts',(-1.95398888263491,0.00659139887796774,
2.32549387889298));
#281981=CARTESIAN_POINT('Ctrl Pts',(-1.95375850389951,0.0748860804947652,
2.32157576313438));
#281982=CARTESIAN_POINT('Ctrl Pts',(-1.94994286401812,0.143304051901439,
2.31765764737579));
#281983=CARTESIAN_POINT('Ctrl Pts',(-1.94252670595967,0.211437926194598,
2.31373953161719));
#281984=CARTESIAN_POINT('Ctrl Pts',(-1.93512171543734,0.279469201878615,
2.30982731590804));
#281985=CARTESIAN_POINT('Ctrl Pts',(-1.92412701988573,0.347216744430845,
2.30591510019889));
#281986=CARTESIAN_POINT('Ctrl Pts',(-1.90957937308489,0.414273602693595,
2.30200288448975));
#281987=CARTESIAN_POINT('Ctrl Pts',(-1.89504883349596,0.481251605874107,
2.29809526932556));
#281988=CARTESIAN_POINT('Ctrl Pts',(-1.87697374416079,0.547540059395919,
2.29418765416137));
#281989=CARTESIAN_POINT('Ctrl Pts',(-1.85544238223407,0.612739395020072,
2.29028003899719));
#281990=CARTESIAN_POINT('Ctrl Pts',(-1.83392451534601,0.677897866180661,
2.28637487297755));
#281991=CARTESIAN_POINT('Ctrl Pts',(-1.80895482693705,0.74196810751825,
2.28246970695791));
#281992=CARTESIAN_POINT('Ctrl Pts',(-1.78067177656173,0.804564493472392,
2.27856454093828));
#281993=CARTESIAN_POINT('Ctrl Pts',(-1.75239675229198,0.86714311595353,
2.27466048311858));
#281994=CARTESIAN_POINT('Ctrl Pts',(-1.72081043506945,0.928248265306702,
2.27075642529888));
#281995=CARTESIAN_POINT('Ctrl Pts',(-1.68609918873594,0.987514823050275,
2.26685236747919));
#281996=CARTESIAN_POINT('Ctrl Pts',(-1.6513858876595,1.04678488909601,2.26294807855758));
#281997=CARTESIAN_POINT('Ctrl Pts',(-1.61354754101906,1.10421572431086,
2.25904378963598));
#281998=CARTESIAN_POINT('Ctrl Pts',(-1.57281526226314,1.15946890893724,
2.25513950071438));
#281999=CARTESIAN_POINT('Ctrl Pts',(-1.53203959701168,1.21478094718346,
2.25123105309066));
#282000=CARTESIAN_POINT('Ctrl Pts',(-1.48836414034618,1.26791030904921,
2.24732260546693));
#282001=CARTESIAN_POINT('Ctrl Pts',(-1.44206133777691,1.31855037753173,
2.24341415784321));
#282002=CARTESIAN_POINT('Ctrl Pts',(-1.39573081990885,1.3692207574544,2.23950337075433));
#282003=CARTESIAN_POINT('Ctrl Pts',(-1.34677017694355,1.41739853356051,
2.23559258366544));
#282004=CARTESIAN_POINT('Ctrl Pts',(-1.29548787572475,1.46281480846011,
2.23168179657655));
#282005=CARTESIAN_POINT('Ctrl Pts',(-1.24411702575363,1.50830950328981,
2.22776425676189));
#282006=CARTESIAN_POINT('Ctrl Pts',(-1.19041690134462,1.55103287414906,
2.22384671694722));
#282007=CARTESIAN_POINT('Ctrl Pts',(-1.13472739017928,1.59075760252055,
2.21992917713256));
#282008=CARTESIAN_POINT('Ctrl Pts',(-1.10844330394406,1.60950670202488,
2.21808019422422));
#282009=CARTESIAN_POINT('Ctrl Pts',(-1.08171645180236,1.62758846688301,
2.21623121131588));
#282010=CARTESIAN_POINT('Ctrl Pts',(-1.0545844568764,1.64498256018558,2.21438222840754));
#282011=CARTESIAN_POINT('Ctrl Pts',(-0.997089984035675,1.68184178221119,
2.21046411262223));
#282012=CARTESIAN_POINT('Ctrl Pts',(-0.937546788773812,1.71575617240091,
2.20654599683691));
#282013=CARTESIAN_POINT('Ctrl Pts',(-0.876288810139718,1.74649188982483,
2.2026278810516));
#282014=CARTESIAN_POINT('Ctrl Pts',(-0.815123076134851,1.77718132421884,
2.1987156653163));
#282015=CARTESIAN_POINT('Ctrl Pts',(-0.752248119592166,1.8047013666763,
2.194803449581));
#282016=CARTESIAN_POINT('Ctrl Pts',(-0.688025731581611,1.82886210324387,
2.1908912338457));
#282017=CARTESIAN_POINT('Ctrl Pts',(-0.623878865491443,1.85299442814254,
2.18698361865633));
#282018=CARTESIAN_POINT('Ctrl Pts',(-0.558388172981715,1.87377512024045,
2.18307600346695));
#282019=CARTESIAN_POINT('Ctrl Pts',(-0.491937196864845,1.89106155223482,
2.17916838827758));
#282020=CARTESIAN_POINT('Ctrl Pts',(-0.425527869702247,1.90833714974852,
2.17526322223336));
#282021=CARTESIAN_POINT('Ctrl Pts',(-0.358159927818379,1.92212270800417,
2.17135805618914));
#282022=CARTESIAN_POINT('Ctrl Pts',(-0.290232427847443,1.93232531883888,
2.16745289014492));
#282023=CARTESIAN_POINT('Ctrl Pts',(-0.222324204213047,1.94252503439612,
2.16354883230128));
#282024=CARTESIAN_POINT('Ctrl Pts',(-0.153857223913402,1.9491437479538,
2.15964477445765));
#282025=CARTESIAN_POINT('Ctrl Pts',(-0.085239307148701,1.95213991827349,
2.15574071661401));
#282026=CARTESIAN_POINT('Ctrl Pts',(-0.0166173285370322,1.95513626595189,
2.15183642766913));
#282027=CARTESIAN_POINT('Ctrl Pts',(0.0521551127561943,1.95450962576515,
2.14793213872426));
#282028=CARTESIAN_POINT('Ctrl Pts',(0.120668345670809,1.95027053260646,
2.14402784977938));
#282029=CARTESIAN_POINT('Ctrl Pts',(0.189254556290487,1.94602692412602,
2.14011940213355));
#282030=CARTESIAN_POINT('Ctrl Pts',(0.257580515639657,1.93816321399345,
2.13621095448772));
#282031=CARTESIAN_POINT('Ctrl Pts',(0.325240843492128,1.92674191155031,
2.13230250684189));
#282032=CARTESIAN_POINT('Ctrl Pts',(0.392941670527916,1.9153137727019,2.12839171973152));
#282033=CARTESIAN_POINT('Ctrl Pts',(0.459975593038447,1.90032391089241,
2.12448093262115));
#282034=CARTESIAN_POINT('Ctrl Pts',(0.525949373255067,1.88188555889369,
2.12057014551079));
#282035=CARTESIAN_POINT('Ctrl Pts',(0.592037069866354,1.86341536954115,
2.11665260567583));
#282036=CARTESIAN_POINT('Ctrl Pts',(0.657060504883645,1.84148496292513,
2.11273506584087));
#282037=CARTESIAN_POINT('Ctrl Pts',(0.720644320847418,1.81625652451144,
2.10881752600591));
#282038=CARTESIAN_POINT('Ctrl Pts',(0.750654322105041,1.80434932049974,
2.10696854331131));
#282039=CARTESIAN_POINT('Ctrl Pts',(0.780343962469385,1.79170812344853,
2.1051195606167));
#282040=CARTESIAN_POINT('Ctrl Pts',(0.809675746237423,1.77835350421531,
2.1032705779221));
#282041=CARTESIAN_POINT('Ctrl Pts',(0.871831725778848,1.75005418746022,
2.09935246194773));
#282042=CARTESIAN_POINT('Ctrl Pts',(0.932625480640733,1.71843618955672,
2.09543434597337));
#282043=CARTESIAN_POINT('Ctrl Pts',(0.99167940171878,1.6836531603055,2.091516229999));
#282044=CARTESIAN_POINT('Ctrl Pts',(1.05064439714413,1.64892250866989,2.0876040140735));
#282045=CARTESIAN_POINT('Ctrl Pts',(1.10787433795939,1.61103653218617,2.08369179814801));
#282046=CARTESIAN_POINT('Ctrl Pts',(1.16301340408146,1.5701961093847,2.07977958222251));
#282047=CARTESIAN_POINT('Ctrl Pts',(1.21808762977321,1.52940371261586,2.07587196684218));
#282048=CARTESIAN_POINT('Ctrl Pts',(1.2710754704945,1.48566406084644,2.07196435146185));
#282049=CARTESIAN_POINT('Ctrl Pts',(1.32164902706319,1.43922195969312,2.06805673608152));
#282050=CARTESIAN_POINT('Ctrl Pts',(1.37219088604883,1.39280896668364,2.06415156984599));
#282051=CARTESIAN_POINT('Ctrl Pts',(1.42032110107139,1.34369721618839,2.06024640361046));
#282052=CARTESIAN_POINT('Ctrl Pts',(1.46574512154459,1.29217152060717,2.05634123737493));
#282053=CARTESIAN_POINT('Ctrl Pts',(1.51115625167722,1.24066044688805,2.05243717933991));
#282054=CARTESIAN_POINT('Ctrl Pts',(1.55386238666488,1.18673715677326,2.04853312130489));
#282055=CARTESIAN_POINT('Ctrl Pts',(1.59360737100109,1.13072169303104,2.04462906326987));
#282056=CARTESIAN_POINT('Ctrl Pts',(1.63335470804471,1.07470291344915,2.04072477413383));
#282057=CARTESIAN_POINT('Ctrl Pts',(1.6701402638902,1.01659211700271,2.0368204849978));
#282058=CARTESIAN_POINT('Ctrl Pts',(1.7037506242993,0.956739154733277,2.03291619586177));
#282059=CARTESIAN_POINT('Ctrl Pts',(1.73739678517757,0.896822439379862,
2.02900774802642));
#282060=CARTESIAN_POINT('Ctrl Pts',(1.7678607596992,0.83516028453208,2.02509930019107));
#282061=CARTESIAN_POINT('Ctrl Pts',(1.79497512160515,0.772127135139402,
2.02119085235572));
#282062=CARTESIAN_POINT('Ctrl Pts',(1.82210571324549,0.709056256248384,
2.01728006505649));
#282063=CARTESIAN_POINT('Ctrl Pts',(1.84588253173502,0.644613211141009,
2.01336927775727));
#282064=CARTESIAN_POINT('Ctrl Pts',(1.86618734773961,0.579189764357586,
2.00945849045804));
#282065=CARTESIAN_POINT('Ctrl Pts',(1.88652722388912,0.513653351491413,
2.00554095043722));
#282066=CARTESIAN_POINT('Ctrl Pts',(1.90338301158713,0.447133634847763,
2.0016234104164));
#282067=CARTESIAN_POINT('Ctrl Pts',(1.91668730398203,0.380033917899586,
1.99770587039558));
#282068=CARTESIAN_POINT('Ctrl Pts',(1.9229665975039,0.34836452839387,1.99585688940928));
#282069=CARTESIAN_POINT('Ctrl Pts',(1.92845550807211,0.316566029240909,
1.99400790842298));
#282070=CARTESIAN_POINT('Ctrl Pts',(1.9331509727995,0.284681078339155,1.99215892743667));
#282071=CARTESIAN_POINT('Ctrl Pts',(1.94310097942662,0.217114715647277,
1.98824081194966));
#282072=CARTESIAN_POINT('Ctrl Pts',(1.94952413564899,0.148892135969539,
1.98432269646264));
#282073=CARTESIAN_POINT('Ctrl Pts',(1.95234464277733,0.0804139031428942,
1.98040458097562));
#282074=CARTESIAN_POINT('Ctrl Pts',(1.95516090267743,0.0120387874758331,
1.97649236553776));
#282075=CARTESIAN_POINT('Ctrl Pts',(1.95438526012298,-0.0565907297962358,
1.9725801500999));
#282076=CARTESIAN_POINT('Ctrl Pts',(1.94999341136833,-0.125066764650378,
1.96866793466204));
#282077=CARTESIAN_POINT('Ctrl Pts',(1.94560672717848,-0.193462275575004,
1.96476031976743));
#282078=CARTESIAN_POINT('Ctrl Pts',(1.93761231355979,-0.261704173983213,
1.96085270487283));
#282079=CARTESIAN_POINT('Ctrl Pts',(1.92603791504017,-0.329384197902236,
1.95694508997822));
#282080=CARTESIAN_POINT('Ctrl Pts',(1.91447077091019,-0.397021802574726,
1.95303992422695));
#282081=CARTESIAN_POINT('Ctrl Pts',(1.89932817559024,-0.464097747581249,
1.94913475847568));
#282082=CARTESIAN_POINT('Ctrl Pts',(1.88068957346917,-0.530210079350018,
1.94522959272441));
#282083=CARTESIAN_POINT('Ctrl Pts',(1.86205626056478,-0.596303649923828,
1.94132553517148));
#282084=CARTESIAN_POINT('Ctrl Pts',(1.83992904373194,-0.661433676905025,
1.93742147761854));
#282085=CARTESIAN_POINT('Ctrl Pts',(1.81443779282632,-0.725211345721751,
1.93351742006561));
#282086=CARTESIAN_POINT('Ctrl Pts',(1.78894503294509,-0.788992789910165,
1.92961313140877));
#282087=CARTESIAN_POINT('Ctrl Pts',(1.76008802857329,-0.851421261204326,
1.92570884275193));
#282088=CARTESIAN_POINT('Ctrl Pts',(1.72804487830883,-0.912127676671768,
1.92180455409509));
#282089=CARTESIAN_POINT('Ctrl Pts',(1.69596759684093,-0.972898754414884,
1.91789610673134));
#282090=CARTESIAN_POINT('Ctrl Pts',(1.66069762662193,-1.03194367985739,
1.91398765936759));
#282091=CARTESIAN_POINT('Ctrl Pts',(1.6224586762536,-1.08891865805001,1.91007921200384));
#282092=CARTESIAN_POINT('Ctrl Pts',(1.58419683731237,-1.14592773958304,
1.90616842517257));
#282093=CARTESIAN_POINT('Ctrl Pts',(1.54296277671333,-1.20086401457557,
1.9022576383413));
#282094=CARTESIAN_POINT('Ctrl Pts',(1.49902144341454,-1.25341561829402,
1.89834685151003));
#282095=CARTESIAN_POINT('Ctrl Pts',(1.45500423688004,-1.3060579625503,1.89442931194668));
#282096=CARTESIAN_POINT('Ctrl Pts',(1.40827076263727,-1.35630705747644,
1.89051177238332));
#282097=CARTESIAN_POINT('Ctrl Pts',(1.35912323601593,-1.40388747032004,
1.88659423281997));
#282098=CARTESIAN_POINT('Ctrl Pts',(1.33592677500446,-1.42634429098447,
1.88474524753039));
#282099=CARTESIAN_POINT('Ctrl Pts',(1.3121930395836,-1.44820721209223,1.88289626224081));
#282100=CARTESIAN_POINT('Ctrl Pts',(1.28795620210788,-1.46945051684357,
1.88104727695123));
#282101=CARTESIAN_POINT('Ctrl Pts',(1.2365968232103,-1.51446641212505,1.87712916114264));
#282102=CARTESIAN_POINT('Ctrl Pts',(1.18277273786087,-1.55687567738446,
1.87321104533406));
#282103=CARTESIAN_POINT('Ctrl Pts',(1.12677930717372,-1.59639731674953,
1.86929292952548));
#282104=CARTESIAN_POINT('Ctrl Pts',(1.07087019359426,-1.6358594428774,1.86538071376961));
#282105=CARTESIAN_POINT('Ctrl Pts',(1.01279861651915,-1.67244229158536,
1.86146849801374));
#282106=CARTESIAN_POINT('Ctrl Pts',(0.952894024406714,-1.70590415271491,
1.85755628225787));
#282107=CARTESIAN_POINT('Ctrl Pts',(0.893059876790552,-1.73932666454136,
1.85364866705194));
#282108=CARTESIAN_POINT('Ctrl Pts',(0.831397422435963,-1.76963523894658,
1.84974105184602));
#282109=CARTESIAN_POINT('Ctrl Pts',(0.768264665673746,-1.79663168275448,
1.8458334366401));
#282110=CARTESIAN_POINT('Ctrl Pts',(0.705171478171865,-1.82361120619699,
1.84192827058184));
#282111=CARTESIAN_POINT('Ctrl Pts',(0.640610267537421,-1.84728252404706,
1.83802310452357));
#282112=CARTESIAN_POINT('Ctrl Pts',(0.574961788221266,-1.86749429506101,
1.83411793846531));
#282113=CARTESIAN_POINT('Ctrl Pts',(0.509331938547415,-1.88770033040418,
1.83021388061012));
#282114=CARTESIAN_POINT('Ctrl Pts',(0.442615902587654,-1.90444862317821,
1.82630982275494));
#282115=CARTESIAN_POINT('Ctrl Pts',(0.375210755603282,-1.91763731943233,
1.82240576489975));
#282116=CARTESIAN_POINT('Ctrl Pts',(0.307801618605196,-1.93082679638468,
1.81850147594583));
#282117=CARTESIAN_POINT('Ctrl Pts',(0.23970377281427,-1.94045616655268,
1.8145971869919));
#282118=CARTESIAN_POINT('Ctrl Pts',(0.171323884482255,-1.94647479475228,
1.81069289803798));
#282119=CARTESIAN_POINT('Ctrl Pts',(0.102871160545255,-1.9524998337612,
1.80678445038689));
#282120=CARTESIAN_POINT('Ctrl Pts',(0.0341362854467537,-1.9549064121214,
1.8028760027358));
#282121=CARTESIAN_POINT('Ctrl Pts',(-0.034470571834636,-1.95369592815192,
1.7989675550847));
#282122=CARTESIAN_POINT('Ctrl Pts',(-0.103118494821971,-1.95248471962835,
1.79505676797123));
#282123=CARTESIAN_POINT('Ctrl Pts',(-0.171637756761939,-1.94765217453876,
1.79114598085775));
#282124=CARTESIAN_POINT('Ctrl Pts',(-0.239622636329546,-1.93925165776866,
1.78723519374427));
#282125=CARTESIAN_POINT('Ctrl Pts',(-0.307724904783329,-1.93083663590105,
1.78331765390951));
#282126=CARTESIAN_POINT('Ctrl Pts',(-0.375290465227256,-1.91884143235029,
1.77940011407475));
#282127=CARTESIAN_POINT('Ctrl Pts',(-0.441923981656403,-1.90337048270613,
1.77548257423999));
#282128=CARTESIAN_POINT('Ctrl Pts',(-0.473373364962697,-1.89606857442414,
1.77363359164859));
#282129=CARTESIAN_POINT('Ctrl Pts',(-0.50461535032352,-1.88799312697528,
1.77178460905719));
#282130=CARTESIAN_POINT('Ctrl Pts',(-0.535609795124796,-1.87915889359212,
1.76993562646579));
#282131=CARTESIAN_POINT('Ctrl Pts',(-0.601289082140249,-1.86043856633175,
1.76601750955531));
#282132=CARTESIAN_POINT('Ctrl Pts',(-0.66611593167999,-1.8382336066086,
1.76209939264482));
#282133=CARTESIAN_POINT('Ctrl Pts',(-0.72969405316222,-1.8126396742816,
1.75818127573434));
#282134=CARTESIAN_POINT('Ctrl Pts',(-0.793176436374374,-1.78708428223776,
1.75426905886818));
#282135=CARTESIAN_POINT('Ctrl Pts',(-0.855413370793917,-1.75815022792144,
1.75035684200202));
#282136=CARTESIAN_POINT('Ctrl Pts',(-0.916023073160365,-1.72598311968508,
1.74644462513586));
#282137=CARTESIAN_POINT('Ctrl Pts',(-0.976561501986862,-1.69385383812637,
1.74253700881276));
#282138=CARTESIAN_POINT('Ctrl Pts',(-1.03547606663956,-1.65849928275092,
1.73862939248965));
#282139=CARTESIAN_POINT('Ctrl Pts',(-1.09240604661752,-1.62011265945103,
1.73472177616654));
#282140=CARTESIAN_POINT('Ctrl Pts',(-1.1493003450676,-1.58175009541428,
1.73081660898747));
#282141=CARTESIAN_POINT('Ctrl Pts',(-1.20421211935406,-1.5403595075849,
1.7269114418084));
#282142=CARTESIAN_POINT('Ctrl Pts',(-1.25680766304988,-1.49617863174793,
1.72300627462933));
#282143=CARTESIAN_POINT('Ctrl Pts',(-1.30938828127897,-1.45201029347871,
1.71910221565142));
#282144=CARTESIAN_POINT('Ctrl Pts',(-1.35965359730641,-1.4050535553336,
1.71519815667351));
#282145=CARTESIAN_POINT('Ctrl Pts',(-1.40730262072439,-1.35558671198203,
1.7112940976956));
#282146=CARTESIAN_POINT('Ctrl Pts',(-1.45495446470395,-1.30611694046389,
1.70738980761876));
#282147=CARTESIAN_POINT('Ctrl Pts',(-1.49998936920952,-1.25413712478501,
1.70348551754191));
#282148=CARTESIAN_POINT('Ctrl Pts',(-1.5421441655473,-1.19996140465784,
1.69958122746507));
#282149=CARTESIAN_POINT('Ctrl Pts',(-1.58434386344633,-1.14572797877411,
1.69567277869846));
#282150=CARTESIAN_POINT('Ctrl Pts',(-1.62365702820594,-1.08929436949584,
1.69176432993185));
#282151=CARTESIAN_POINT('Ctrl Pts',(-1.65986230038572,-1.03100588929367,
1.68785588116524));
#282152=CARTESIAN_POINT('Ctrl Pts',(-1.69608924376643,-0.972682519659919,
1.68394509293883));
#282153=CARTESIAN_POINT('Ctrl Pts',(-1.72920435511023,-0.912502500482538,
1.68003430471243));
#282154=CARTESIAN_POINT('Ctrl Pts',(-1.7590323414148,-0.850835602132843,
1.67612351648603));
#282155=CARTESIAN_POINT('Ctrl Pts',(-1.7889118313032,-0.789062224376999,
1.67220597555406));
#282156=CARTESIAN_POINT('Ctrl Pts',(-1.81549267766802,-0.72579729662071,
1.66828843462209));
#282157=CARTESIAN_POINT('Ctrl Pts',(-1.83864812282955,-0.661429573284541,
1.66437089369011));
#282158=CARTESIAN_POINT('Ctrl Pts',(-1.84957686197775,-0.63104976184075,
1.6625219211202));
#282159=CARTESIAN_POINT('Ctrl Pts',(-1.85974329224162,-0.600424495698479,
1.66067294855028));
#282160=CARTESIAN_POINT('Ctrl Pts',(-1.86913802783902,-0.569595499355519,
1.65882397598036));
#282161=CARTESIAN_POINT('Ctrl Pts',(-1.89348479324527,-0.489701144278649,
1.65403230292733));
#282162=CARTESIAN_POINT('Ctrl Pts',(-1.91272391212393,-0.408182349819562,
1.64924062987431));
#282163=CARTESIAN_POINT('Ctrl Pts',(-1.92667621842312,-0.325629773458762,
1.64444895682128));
#282164=CARTESIAN_POINT('Ctrl Pts',(-1.94043089971803,-0.244246498638989,
1.63972515458382));
#282165=CARTESIAN_POINT('Ctrl Pts',(-1.94904743099152,-0.161858499862965,
1.63500135234636));
#282166=CARTESIAN_POINT('Ctrl Pts',(-1.95240023819972,-0.0790525766668212,
1.6302775501089));
#282167=CARTESIAN_POINT('Ctrl Pts',(-1.95344308694579,-0.0532968299717755,
1.62880827050704));
#282168=CARTESIAN_POINT('Ctrl Pts',(-1.95397704349981,-0.0275008065544239,
1.62733899090518));
#282169=CARTESIAN_POINT('Ctrl Pts',(-1.9539992755619,-0.00168258835255015,
1.62586971130332));
#282170=CARTESIAN_POINT('',(-1.95128203910989,0.000979727872364722,0.92586969212423));
#282171=CARTESIAN_POINT('Ctrl Pts',(-1.95279554503994,-0.00168121501241181,
1.62586969212423));
#282172=CARTESIAN_POINT('Ctrl Pts',(-1.94903656010943,0.455834752155161,
1.59981723658113));
#282173=CARTESIAN_POINT('Ctrl Pts',(-1.56043776453642,1.56952521197424,
1.53672756420953));
#282174=CARTESIAN_POINT('Ctrl Pts',(0.294968904732084,2.29042728261437,
1.43660067500948));
#282175=CARTESIAN_POINT('Ctrl Pts',(2.08405785032273,0.994871990457251,
1.32548902452406));
#282176=CARTESIAN_POINT('Ctrl Pts',(1.96640931676784,-1.2109096610648,1.21437737403861));
#282177=CARTESIAN_POINT('Ctrl Pts',(0.049663025814346,-2.30880650358356,
1.10326572355317));
#282178=CARTESIAN_POINT('Ctrl Pts',(-1.64864534346746,-1.43077452179925,
1.00709649624838));
#282179=CARTESIAN_POINT('Ctrl Pts',(-1.94952091996443,-0.387793032173158,
0.947964485772066));
#282180=CARTESIAN_POINT('Ctrl Pts',(-1.95128203910989,0.000979727872364722,
0.92586969212423));
#282181=CARTESIAN_POINT('Ctrl Pts',(-1.95128203910989,0.000979727872364722,
0.92586969212423));
#282182=CARTESIAN_POINT('Ctrl Pts',(-1.9524730612105,0.263901717292074,
0.910927268943587));
#282183=CARTESIAN_POINT('Ctrl Pts',(-1.78055184446198,1.17702392994427,
0.858947628934464));
#282184=CARTESIAN_POINT('Ctrl Pts',(-0.393188016825178,2.2756080016325,
0.769930772096862));
#282185=CARTESIAN_POINT('Ctrl Pts',(1.69827668332872,1.5649425932243,0.658819121611428));
#282186=CARTESIAN_POINT('Ctrl Pts',(2.23594117881619,-0.577629785835539,
0.547707471125989));
#282187=CARTESIAN_POINT('Ctrl Pts',(0.72794696107778,-2.19149774367173,
0.436595820640553));
#282188=CARTESIAN_POINT('Ctrl Pts',(-1.37113779886414,-1.81423119146763,
0.32931688820614));
#282189=CARTESIAN_POINT('Ctrl Pts',(-1.95230360289333,-0.579093481907559,
0.259075172600207));
#282190=CARTESIAN_POINT('Ctrl Pts',(-1.9563354715932,0.00125594757992074,
0.225870673822753));
#282191=CARTESIAN_POINT('Origin',(0.,0.,-1.29405622560369));
#282192=CARTESIAN_POINT('',(-1.55549973622945,-0.00090586429527298,10.9559437744371));
#282193=CARTESIAN_POINT('',(0.499806597877791,1.47301514408978,11.4445));
#282194=CARTESIAN_POINT('Ctrl Pts',(-1.55549973622945,-0.00090586429527298,
10.9559437744371));
#282195=CARTESIAN_POINT('Ctrl Pts',(-1.5554624181148,-0.0649864531813007,
10.9605121932704));
#282196=CARTESIAN_POINT('Ctrl Pts',(-1.55146115138349,-0.128926751081953,
10.9650806121038));
#282197=CARTESIAN_POINT('Ctrl Pts',(-1.54357236633783,-0.192261800361485,
10.9696490309371));
#282198=CARTESIAN_POINT('Ctrl Pts',(-1.53565219727971,-0.255848815940527,
10.9742356243452));
#282199=CARTESIAN_POINT('Ctrl Pts',(-1.52381366620313,-0.318825456507138,
10.9788222177533));
#282200=CARTESIAN_POINT('Ctrl Pts',(-1.50818383456823,-0.380738455041077,
10.9834088111614));
#282201=CARTESIAN_POINT('Ctrl Pts',(-1.49247619331133,-0.442959673594634,
10.9880182378992));
#282202=CARTESIAN_POINT('Ctrl Pts',(-1.47293956753027,-0.504106343920584,
10.992627664637));
#282203=CARTESIAN_POINT('Ctrl Pts',(-1.44975072861387,-0.563740254801405,
10.9972370913749));
#282204=CARTESIAN_POINT('Ctrl Pts',(-1.44502802405396,-0.575885465859958,
10.9981758602693));
#282205=CARTESIAN_POINT('Ctrl Pts',(-1.4401539839899,-0.587968010173575,
10.9991146291638));
#282206=CARTESIAN_POINT('Ctrl Pts',(-1.43513033363107,-0.599984312704903,
11.0000533980582));
#282207=CARTESIAN_POINT('Ctrl Pts',(-1.41288996022962,-0.653182094419901,
11.0042094537666));
#282208=CARTESIAN_POINT('Ctrl Pts',(-1.38764176100762,-0.705251438383512,
11.0083655094749));
#282209=CARTESIAN_POINT('Ctrl Pts',(-1.35952197240883,-0.755830838572767,
11.0125215651832));
#282210=CARTESIAN_POINT('Ctrl Pts',(-1.33145251805152,-0.806319701959642,
11.0166701815784));
#282211=CARTESIAN_POINT('Ctrl Pts',(-1.30052192813529,-0.855323466279215,
11.0208187979737));
#282212=CARTESIAN_POINT('Ctrl Pts',(-1.26691401553271,-0.902501594041128,
11.0249674143689));
#282213=CARTESIAN_POINT('Ctrl Pts',(-1.23333982924824,-0.949632377459965,
11.0291118675315));
#282214=CARTESIAN_POINT('Ctrl Pts',(-1.19709394374559,-0.994940734441594,
11.0332563206942));
#282215=CARTESIAN_POINT('Ctrl Pts',(-1.15840461492088,-1.03811319138618,
11.0374007738569));
#282216=CARTESIAN_POINT('Ctrl Pts',(-1.11973938927939,-1.08125875218987,
11.041542645054));
#282217=CARTESIAN_POINT('Ctrl Pts',(-1.07863408370058,-1.1222706656218,
11.0456845162511));
#282218=CARTESIAN_POINT('Ctrl Pts',(-1.0353571968633,-1.16086852179882,
11.0498263874482));
#282219=CARTESIAN_POINT('Ctrl Pts',(-0.992090804187492,-1.19945701842701,
11.0539672542878));
#282220=CARTESIAN_POINT('Ctrl Pts',(-0.946654262575783,-1.23563227495104,
11.0581081211275));
#282221=CARTESIAN_POINT('Ctrl Pts',(-0.899351290910011,-1.26915227830962,
11.0622489879671));
#282222=CARTESIAN_POINT('Ctrl Pts',(-0.852007614334827,-1.30270112612875,
11.0663934180841));
#282223=CARTESIAN_POINT('Ctrl Pts',(-0.802794721221834,-1.33358985262928,
11.0705378482012));
#282224=CARTESIAN_POINT('Ctrl Pts',(-0.752046543952488,-1.36161897964486,
11.0746822783182));
#282225=CARTESIAN_POINT('Ctrl Pts',(-0.701278443146775,-1.38965911078634,
11.0788283355223));
#282226=CARTESIAN_POINT('Ctrl Pts',(-0.64897432376144,-1.41483717654292,
11.0829743927264));
#282227=CARTESIAN_POINT('Ctrl Pts',(-0.595491192649498,-1.43700051825909,
11.0871204499305));
#282228=CARTESIAN_POINT('Ctrl Pts',(-0.541907029850498,-1.45920572737826,
11.0912743391958));
#282229=CARTESIAN_POINT('Ctrl Pts',(-0.487139895107943,-1.47838465773227,
11.0954282284611));
#282230=CARTESIAN_POINT('Ctrl Pts',(-0.431564295262401,-1.49443384231443,
11.0995821177264));
#282231=CARTESIAN_POINT('Ctrl Pts',(-0.37990761987289,-1.50935131545968,
11.1034430946655));
#282232=CARTESIAN_POINT('Ctrl Pts',(-0.327552956949716,-1.52156533038131,
11.1073040716046));
#282233=CARTESIAN_POINT('Ctrl Pts',(-0.274807223030603,-1.53103273647895,
11.1111650485437));
#282234=CARTESIAN_POINT('Ctrl Pts',(-0.21805856036645,-1.54121863389699,
11.1153190390485));
#282235=CARTESIAN_POINT('Ctrl Pts',(-0.160627328713441,-1.54826587752968,
11.1194730295534));
#282236=CARTESIAN_POINT('Ctrl Pts',(-0.102891144520795,-1.55209331626008,
11.1236270200582));
#282237=CARTESIAN_POINT('Ctrl Pts',(-0.0452553750170186,-1.55591409831451,
11.1277737859487));
#282238=CARTESIAN_POINT('Ctrl Pts',(0.012683780480316,-1.55652615738425,
11.1319205518393));
#282239=CARTESIAN_POINT('Ctrl Pts',(0.0705405746337234,-1.5538996998939,
11.1360673177298));
#282240=CARTESIAN_POINT('Ctrl Pts',(0.128341113208402,-1.55127579617252,
11.1402100516182));
#282241=CARTESIAN_POINT('Ctrl Pts',(0.186058933198519,-1.54541963903664,
11.1443527855066));
#282242=CARTESIAN_POINT('Ctrl Pts',(0.243307004996965,-1.53635345911005,
11.148495519395));
#282243=CARTESIAN_POINT('Ctrl Pts',(0.300521227458064,-1.52729263978641,
11.1526358037896));
#282244=CARTESIAN_POINT('Ctrl Pts',(0.357265740804184,-1.51502564158783,
11.1567760881843));
#282245=CARTESIAN_POINT('Ctrl Pts',(0.413159555535051,-1.49962643070535,
11.1609163725789));
#282246=CARTESIAN_POINT('Ctrl Pts',(0.469041618685836,-1.48423045748094,
11.1650557864857));
#282247=CARTESIAN_POINT('Ctrl Pts',(0.524072838295294,-1.46570371701194,
11.1691952003925));
#282248=CARTESIAN_POINT('Ctrl Pts',(0.577885471001734,-1.44417056901361,
11.1733346142993));
#282249=CARTESIAN_POINT('Ctrl Pts',(0.631747265873237,-1.4226177487539,
11.1774778098935));
#282250=CARTESIAN_POINT('Ctrl Pts',(0.684387765817342,-1.39805322473431,
11.1816210054876));
#282251=CARTESIAN_POINT('Ctrl Pts',(0.735458644606146,-1.37064978461826,
11.1857642010817));
#282252=CARTESIAN_POINT('Ctrl Pts',(0.786551027400648,-1.34323480595527,
11.189909141218));
#282253=CARTESIAN_POINT('Ctrl Pts',(0.836072026975183,-1.31297879814688,
11.1940540813543));
#282254=CARTESIAN_POINT('Ctrl Pts',(0.883700229279736,-1.28009927535756,
11.1981990214906));
#282255=CARTESIAN_POINT('Ctrl Pts',(0.931420843428688,-1.24715595722856,
11.2023520039536));
#282256=CARTESIAN_POINT('Ctrl Pts',(0.977240909000357,-1.21157927010357,
11.2065049864166));
#282257=CARTESIAN_POINT('Ctrl Pts',(1.02087091663919,-1.17362805929317,
11.2106579688796));
#282258=CARTESIAN_POINT('Ctrl Pts',(1.06155856619351,-1.13823623496901,
11.2145308789294));
#282259=CARTESIAN_POINT('Ctrl Pts',(1.10034169991128,-1.1007800021631,11.2184037889793));
#282260=CARTESIAN_POINT('Ctrl Pts',(1.13701614988411,-1.06149636122914,
11.2222766990291));
#282261=CARTESIAN_POINT('Ctrl Pts',(1.17586636956837,-1.01988215620596,
11.2263793755891));
#282262=CARTESIAN_POINT('Ctrl Pts',(1.21252069950925,-0.976033787091652,
11.2304820521491));
#282263=CARTESIAN_POINT('Ctrl Pts',(1.24670795418086,-0.930214774652702,
11.2345847287091));
#282264=CARTESIAN_POINT('Ctrl Pts',(1.28101304438198,-0.8842378347158,11.2387015462426));
#282265=CARTESIAN_POINT('Ctrl Pts',(1.31283360197336,-0.836276988307453,
11.2428183637762));
#282266=CARTESIAN_POINT('Ctrl Pts',(1.34193303162277,-0.786635867882791,
11.2469351813098));
#282267=CARTESIAN_POINT('Ctrl Pts',(1.37085210792835,-0.737302414727498,
11.2510264835045));
#282268=CARTESIAN_POINT('Ctrl Pts',(1.39708339572808,-0.686309906372128,
11.2551177856992));
#282269=CARTESIAN_POINT('Ctrl Pts',(1.4204367528487,-0.633987130119093,
11.2592090878939));
#282270=CARTESIAN_POINT('Ctrl Pts',(1.44377647453577,-0.581694903809472,
11.2632980012809));
#282271=CARTESIAN_POINT('Ctrl Pts',(1.464241376507,-0.528074433640186,11.2673869146679));
#282272=CARTESIAN_POINT('Ctrl Pts',(1.48168787713257,-0.473477860895714,
11.2714758280549));
#282273=CARTESIAN_POINT('Ctrl Pts',(1.49913124686719,-0.4188910858705,11.2755640076591));
#282274=CARTESIAN_POINT('Ctrl Pts',(1.51355712783861,-0.363329063483174,
11.2796521872633));
#282275=CARTESIAN_POINT('Ctrl Pts',(1.52487139541215,-0.307160344858819,
11.2837403668675));
#282276=CARTESIAN_POINT('Ctrl Pts',(1.53632169470053,-0.250316308361276,
11.2878776987548));
#282277=CARTESIAN_POINT('Ctrl Pts',(1.54458491338459,-0.192851429228182,
11.292015030642));
#282278=CARTESIAN_POINT('Ctrl Pts',(1.5496170033841,-0.135156919256407,
11.2961523625293));
#282279=CARTESIAN_POINT('Ctrl Pts',(1.55459709273317,-0.078058613256646,
11.3002469400244));
#282280=CARTESIAN_POINT('Ctrl Pts',(1.5564125824634,-0.0207359431881903,
11.3043415175195));
#282281=CARTESIAN_POINT('Ctrl Pts',(1.5550733198847,0.0364310277481887,
11.3084360950146));
#282282=CARTESIAN_POINT('Ctrl Pts',(1.55371308101812,0.0944933801116644,
11.3125948040979));
#282283=CARTESIAN_POINT('Ctrl Pts',(1.54909845009413,0.152394544073392,
11.3167535131812));
#282284=CARTESIAN_POINT('Ctrl Pts',(1.54129417920738,0.209743898937334,
11.3209122222645));
#282285=CARTESIAN_POINT('Ctrl Pts',(1.53348990832064,0.267093253801277,
11.3250709313479));
#282286=CARTESIAN_POINT('Ctrl Pts',(1.52249618900996,0.323890260715516,
11.3292296404312));
#282287=CARTESIAN_POINT('Ctrl Pts',(1.50843045263315,0.379760213251655,
11.3333883495145));
#282288=CARTESIAN_POINT('Ctrl Pts',(1.49400748347762,0.43704911591291,11.3376526788912));
#282289=CARTESIAN_POINT('Ctrl Pts',(1.47629200845049,0.493613181015604,
11.3419170082678));
#282290=CARTESIAN_POINT('Ctrl Pts',(1.45537425215218,0.549059228291879,
11.3461813376444));
#282291=CARTESIAN_POINT('Ctrl Pts',(1.43450151006181,0.604385957804546,
11.3504364903481));
#282292=CARTESIAN_POINT('Ctrl Pts',(1.41044036062075,0.658599002949918,
11.3546916430517));
#282293=CARTESIAN_POINT('Ctrl Pts',(1.38333089507448,0.711319818880685,
11.3589467957554));
#282294=CARTESIAN_POINT('Ctrl Pts',(1.35625595310978,0.763973495480125,
11.3631965295727));
#282295=CARTESIAN_POINT('Ctrl Pts',(1.32614062312171,0.815138286646112,
11.3674462633901));
#282296=CARTESIAN_POINT('Ctrl Pts',(1.2931727813815,0.864456133932793,11.3716959972074));
#282297=CARTESIAN_POINT('Ctrl Pts',(1.26023691519775,0.913726147769451,
11.3759416092019));
#282298=CARTESIAN_POINT('Ctrl Pts',(1.22445430092607,0.961152373337957,
11.3801872211964));
#282299=CARTESIAN_POINT('Ctrl Pts',(1.18605751251627,1.00640341166141,11.3844328331909));
#282300=CARTESIAN_POINT('Ctrl Pts',(1.14768632431624,1.0516242798555,11.3886756145175));
#282301=CARTESIAN_POINT('Ctrl Pts',(1.10670473881416,1.09467247308709,11.392918395844));
#282302=CARTESIAN_POINT('Ctrl Pts',(1.06338613282229,1.13524895178162,11.3971611771706));
#282303=CARTESIAN_POINT('Ctrl Pts',(1.02007026241049,1.17582286806205,11.4014036905645));
#282304=CARTESIAN_POINT('Ctrl Pts',(0.974418010221406,1.21392503874472,
11.4056462039584));
#282305=CARTESIAN_POINT('Ctrl Pts',(0.926739210629652,1.2492936746344,11.4098887173523));
#282306=CARTESIAN_POINT('Ctrl Pts',(0.87906544940404,1.284658573011,11.4141307824268));
#282307=CARTESIAN_POINT('Ctrl Pts',(0.8293659604616,1.31729022665034,11.4183728475012));
#282308=CARTESIAN_POINT('Ctrl Pts',(0.77798146220205,1.34696885430583,11.4226149125756));
#282309=CARTESIAN_POINT('Ctrl Pts',(0.72655905475185,1.3766693775289,11.4268601072564));
#282310=CARTESIAN_POINT('Ctrl Pts',(0.67344957808929,1.40341228340842,11.4311053019372));
#282311=CARTESIAN_POINT('Ctrl Pts',(0.619019388670748,1.42702321160158,
11.435350496618));
#282312=CARTESIAN_POINT('Ctrl Pts',(0.579915630216658,1.44398578407846,
11.4384003310787));
#282313=CARTESIAN_POINT('Ctrl Pts',(0.540130755853637,1.45933281346944,
11.4414501655393));
#282314=CARTESIAN_POINT('Ctrl Pts',(0.499806597877795,1.47301514408978,
11.4445));
#282315=CARTESIAN_POINT('',(1.55548765964692,0.00619602180124784,11.4445));
#282316=CARTESIAN_POINT('Origin',(0.,0.,11.4445));
#282317=CARTESIAN_POINT('',(-1.55549964551795,-0.00105013977025186,11.0940562256037));
#282318=CARTESIAN_POINT('Ctrl Pts',(-1.55549964551795,-0.00105013977025186,
11.0940562256037));
#282319=CARTESIAN_POINT('Ctrl Pts',(-1.5554467553948,-0.0793926329663125,
11.099684397238));
#282320=CARTESIAN_POINT('Ctrl Pts',(-1.54947416800179,-0.157518393304178,
11.1053125688723));
#282321=CARTESIAN_POINT('Ctrl Pts',(-1.5376858701482,-0.234739035412875,
11.1109407405065));
#282322=CARTESIAN_POINT('Ctrl Pts',(-1.52898608215356,-0.291728027674486,
11.1150943427164));
#282323=CARTESIAN_POINT('Ctrl Pts',(-1.51709613604147,-0.348348961130454,
11.1192479449263));
#282324=CARTESIAN_POINT('Ctrl Pts',(-1.50206118452453,-0.40421831718117,
11.1234015471362));
#282325=CARTESIAN_POINT('Ctrl Pts',(-1.48705242241808,-0.459990354294839,
11.1275479141786));
#282326=CARTESIAN_POINT('Ctrl Pts',(-1.46890966326337,-0.515012915471432,
11.1316942812209));
#282327=CARTESIAN_POINT('Ctrl Pts',(-1.44772929077675,-0.56891137326218,
11.1358406482633));
#282328=CARTESIAN_POINT('Ctrl Pts',(-1.42656954751022,-0.622757335132504,
11.1399829768347));
#282329=CARTESIAN_POINT('Ctrl Pts',(-1.40237824237186,-0.675480882336065,
11.1441253054061));
#282330=CARTESIAN_POINT('Ctrl Pts',(-1.37530140911383,-0.726722976167344,
11.1482676339776));
#282331=CARTESIAN_POINT('Ctrl Pts',(-1.34824062460129,-0.777934698229705,
11.152407507344));
#282332=CARTESIAN_POINT('Ctrl Pts',(-1.3182979446997,-0.827666249677602,
11.1565473807104));
#282333=CARTESIAN_POINT('Ctrl Pts',(-1.285666414579,-0.875581018766156,
11.1606872540768));
#282334=CARTESIAN_POINT('Ctrl Pts',(-1.25304178496714,-0.923485655437193,
11.1648262519944));
#282335=CARTESIAN_POINT('Ctrl Pts',(-1.2177297262288,-0.969573843783421,
11.1689652499121));
#282336=CARTESIAN_POINT('Ctrl Pts',(-1.17996669652475,-1.0135377867117,
11.1731042478297));
#282337=CARTESIAN_POINT('Ctrl Pts',(-1.14216912941584,-1.05754193829136,
11.1772470312023));
#282338=CARTESIAN_POINT('Ctrl Pts',(-1.10191645010097,-1.0994175667123,
11.1813898145749));
#282339=CARTESIAN_POINT('Ctrl Pts',(-1.05948467676934,-1.13889089455091,
11.1855325979474));
#282340=CARTESIAN_POINT('Ctrl Pts',(-1.01703507028913,-1.178380812168,11.1896771224415));
#282341=CARTESIAN_POINT('Ctrl Pts',(-0.972404943244974,-1.2154660829153,
11.1938216469355));
#282342=CARTESIAN_POINT('Ctrl Pts',(-0.925903947025988,-1.24991284931458,
11.1979661714295));
#282343=CARTESIAN_POINT('Ctrl Pts',(-0.879312465587032,-1.28442664488503,
11.2021187606585));
#282344=CARTESIAN_POINT('Ctrl Pts',(-0.83084327445346,-1.31629138864477,
11.2062713498876));
#282345=CARTESIAN_POINT('Ctrl Pts',(-0.780834836710626,-1.34531676856385,
11.2104239391166));
#282346=CARTESIAN_POINT('Ctrl Pts',(-0.733855327658026,-1.37258412903762,
11.2143250128569));
#282347=CARTESIAN_POINT('Ctrl Pts',(-0.68551795147696,-1.3973459328914,
11.2182260865973));
#282348=CARTESIAN_POINT('Ctrl Pts',(-0.636119437584287,-1.41948311406915,
11.2221271603377));
#282349=CARTESIAN_POINT('Ctrl Pts',(-0.584172922826061,-1.44276214248798,
11.2262294534769));
#282350=CARTESIAN_POINT('Ctrl Pts',(-0.530823728255636,-1.46324088760723,
11.230331746616));
#282351=CARTESIAN_POINT('Ctrl Pts',(-0.476408890752611,-1.48074806054638,
11.2344340397552));
#282352=CARTESIAN_POINT('Ctrl Pts',(-0.421759434730541,-1.49833071854027,
11.2385540206058));
#282353=CARTESIAN_POINT('Ctrl Pts',(-0.366035587401732,-1.51291582962675,
11.2426740014564));
#282354=CARTESIAN_POINT('Ctrl Pts',(-0.309602098405575,-1.52437750923545,
11.2467939823069));
#282355=CARTESIAN_POINT('Ctrl Pts',(-0.253566959657262,-1.53575828364062,
11.2508848812166));
#282356=CARTESIAN_POINT('Ctrl Pts',(-0.196832688652311,-1.54405944952486,
11.2549757801262));
#282357=CARTESIAN_POINT('Ctrl Pts',(-0.139771862283216,-1.54920756405134,
11.2590666790359));
#282358=CARTESIAN_POINT('Ctrl Pts',(-0.082744421310311,-1.55435266649661,
11.2631551844246));
#282359=CARTESIAN_POINT('Ctrl Pts',(-0.0253913333222678,-1.55634832320774,
11.2672436898133));
#282360=CARTESIAN_POINT('Ctrl Pts',(0.0319078017594993,-1.55517270493887,
11.2713321952021));
#282361=CARTESIAN_POINT('Ctrl Pts',(0.089196593805501,-1.55399729888021,
11.2754199625769));
#282362=CARTESIAN_POINT('Ctrl Pts',(0.146430919346374,-1.54965176460393,
11.2795077299518));
#282363=CARTESIAN_POINT('Ctrl Pts',(0.203231664787166,-1.54216637897078,
11.2835954973266));
#282364=CARTESIAN_POINT('Ctrl Pts',(0.260802295817886,-1.53457953532876,
11.2877386708968));
#282365=CARTESIAN_POINT('Ctrl Pts',(0.317926943534344,-1.52376712075726,
11.291881844467));
#282366=CARTESIAN_POINT('Ctrl Pts',(0.374219533099056,-1.50981455518455,
11.2960250180372));
#282367=CARTESIAN_POINT('Ctrl Pts',(0.429846320278973,-1.49602701402277,
11.3001191880908));
#282368=CARTESIAN_POINT('Ctrl Pts',(0.48466013278346,-1.47917344225769,
11.3042133581445));
#282369=CARTESIAN_POINT('Ctrl Pts',(0.53830465909531,-1.4593862901906,11.3083075281981));
#282370=CARTESIAN_POINT('Ctrl Pts',(0.592912300176866,-1.43924388662412,
11.3124752035266));
#282371=CARTESIAN_POINT('Ctrl Pts',(0.646307721836913,-1.4160617487065,
11.316642878855));
#282372=CARTESIAN_POINT('Ctrl Pts',(0.698140089099992,-1.39002901624083,
11.3208105541835));
#282373=CARTESIAN_POINT('Ctrl Pts',(0.74997245636307,-1.36399628377517,
11.3249782295119));
#282374=CARTESIAN_POINT('Ctrl Pts',(0.800241316513729,-1.33511331686024,
11.3291459048404));
#282375=CARTESIAN_POINT('Ctrl Pts',(0.848628268415838,-1.30361432641926,
11.3333135801688));
#282376=CARTESIAN_POINT('Ctrl Pts',(0.898135152312619,-1.27138628143345,
11.3375777177203));
#282377=CARTESIAN_POINT('Ctrl Pts',(0.945888563678672,-1.23627928598203,
11.3418418552717));
#282378=CARTESIAN_POINT('Ctrl Pts',(0.991545869198776,-1.19850616989436,
11.3461059928231));
#282379=CARTESIAN_POINT('Ctrl Pts',(1.03710474676417,-1.16081448503697,
11.3503609377529));
#282380=CARTESIAN_POINT('Ctrl Pts',(1.08057613305868,-1.12046841648006,
11.3546158826826));
#282381=CARTESIAN_POINT('Ctrl Pts',(1.1216474100154,-1.07772321938694,11.3588708276123));
#282382=CARTESIAN_POINT('Ctrl Pts',(1.16266629439531,-1.03503255020694,
11.3631203447213));
#282383=CARTESIAN_POINT('Ctrl Pts',(1.20129081374652,-0.989949176777246,
11.3673698618303));
#282384=CARTESIAN_POINT('Ctrl Pts',(1.23724322449347,-0.942766913635077,
11.3716193789393));
#282385=CARTESIAN_POINT('Ctrl Pts',(1.2731606953723,-0.89563050394243,11.375864766212));
#282386=CARTESIAN_POINT('Ctrl Pts',(1.3064109219502,-0.8463996405269,11.3801101534848));
#282387=CARTESIAN_POINT('Ctrl Pts',(1.33675587421288,-0.79540177442433,
11.3843555407576));
#282388=CARTESIAN_POINT('Ctrl Pts',(1.3670805428173,-0.744437997130944,
11.3885980902607));
#282389=CARTESIAN_POINT('Ctrl Pts',(1.39450354811632,-0.691709980582283,
11.3928406397639));
#282390=CARTESIAN_POINT('Ctrl Pts',(1.41883070311814,-0.637573278838822,
11.397083189267));
#282391=CARTESIAN_POINT('Ctrl Pts',(1.44315630177837,-0.583440040517223,
11.401325467351));
#282392=CARTESIAN_POINT('Ctrl Pts',(1.46438623292714,-0.527898733597431,
11.4055677454349));
#282393=CARTESIAN_POINT('Ctrl Pts',(1.48237337026586,-0.471327318459934,
11.4098100235189));
#282394=CARTESIAN_POINT('Ctrl Pts',(1.50035858611496,-0.414761946606878,
11.4140518484183));
#282395=CARTESIAN_POINT('Ctrl Pts',(1.51510155575924,-0.357167150216909,
11.4182936733177));
#282396=CARTESIAN_POINT('Ctrl Pts',(1.52650490708359,-0.298936479289034,
11.422535498217));
#282397=CARTESIAN_POINT('Ctrl Pts',(1.53791669662389,-0.240662719012927,
11.4267804619686));
#282398=CARTESIAN_POINT('Ctrl Pts',(1.54598384210377,-0.181752622457975,
11.4310254257202));
#282399=CARTESIAN_POINT('Ctrl Pts',(1.55066025250447,-0.122609262712029,
11.4352703894718));
#282400=CARTESIAN_POINT('Ctrl Pts',(1.55404948024147,-0.0797451216005902,
11.4383469263145));
#282401=CARTESIAN_POINT('Ctrl Pts',(1.55565876235601,-0.036758661229604,
11.4414234631573));
#282402=CARTESIAN_POINT('Ctrl Pts',(1.55548765964692,0.00619602180124782,
11.4445));
#282403=CARTESIAN_POINT('',(-1.55549927593411,0.00143538631611188,9.6942685916742));
#282404=CARTESIAN_POINT('Ctrl Pts',(-1.55549961664973,-0.00109206342674629,
11.0934258365746));
#282405=CARTESIAN_POINT('Ctrl Pts',(-1.55558866716066,0.125748587234756,
11.084990248375));
#282406=CARTESIAN_POINT('Ctrl Pts',(-1.54016409056307,0.252122806744804,
11.0768042802314));
#282407=CARTESIAN_POINT('Ctrl Pts',(-1.50445838958799,0.395769174174197,
11.0666909871392));
#282408=CARTESIAN_POINT('Ctrl Pts',(-1.49893384134289,0.416203743302519,
11.0652338021612));
#282409=CARTESIAN_POINT('Ctrl Pts',(-1.48805551383009,0.453410142869564,
11.0625418156191));
#282410=CARTESIAN_POINT('Ctrl Pts',(-1.48283063335999,0.470216162081886,
11.0613111268281));
#282411=CARTESIAN_POINT('Ctrl Pts',(-1.47399077411028,0.497035901018334,
11.0593214663562));
#282412=CARTESIAN_POINT('Ctrl Pts',(-1.47055607880628,0.507107777542024,
11.0585683914285));
#282413=CARTESIAN_POINT('Ctrl Pts',(-1.46380312693972,0.526264368494188,
11.0571243754841));
#282414=CARTESIAN_POINT('Ctrl Pts',(-1.46050294052373,0.535354959780714,
11.0564340599115));
#282415=CARTESIAN_POINT('Ctrl Pts',(-1.45278685668432,0.556006975882772,
11.0548538872314));
#282416=CARTESIAN_POINT('Ctrl Pts',(-1.44831736778895,0.567547525712447,
11.0539622813804));
#282417=CARTESIAN_POINT('Ctrl Pts',(-1.43602604252437,0.598193641046168,
11.0515709687516));
#282418=CARTESIAN_POINT('Ctrl Pts',(-1.42796100118238,0.617198291047122,
11.0500632377904));
#282419=CARTESIAN_POINT('Ctrl Pts',(-1.38286882674354,0.717836094444385,
11.0419420526536));
#282420=CARTESIAN_POINT('Ctrl Pts',(-1.33922142003083,0.796301379393232,
11.0351076367119));
#282421=CARTESIAN_POINT('Ctrl Pts',(-1.24506436575965,0.935723017831827,
11.0220893419264));
#282422=CARTESIAN_POINT('Ctrl Pts',(-1.19617983212511,0.997455414915479,
11.0159501097808));
#282423=CARTESIAN_POINT('Ctrl Pts',(-1.12645278358293,1.07297139348107,
11.0081129558573));
#282424=CARTESIAN_POINT('Ctrl Pts',(-1.10965763162062,1.09033185827539,
11.0062866658612));
#282425=CARTESIAN_POINT('Ctrl Pts',(-1.08073608653073,1.11886602995056,
11.0032522375993));
#282426=CARTESIAN_POINT('Ctrl Pts',(-1.06882437267497,1.13025050297403,
11.0020323321105));
#282427=CARTESIAN_POINT('Ctrl Pts',(-1.05162008069498,1.14617800160931,
11.0003150233465));
#282428=CARTESIAN_POINT('Ctrl Pts',(-1.04647486765018,1.15087756161206,
10.9998069618623));
#282429=CARTESIAN_POINT('Ctrl Pts',(-1.04124875384899,1.15558698808154,
10.999296610716));
#282430=CARTESIAN_POINT('Ctrl Pts',(-1.04119938777156,1.15563146777836,
10.9992917904291));
#282431=CARTESIAN_POINT('Ctrl Pts',(-1.04110048648618,1.15572056807992,
10.999282134363));
#282432=CARTESIAN_POINT('Ctrl Pts',(-1.0410509512563,1.15576518866641,10.9992772985851));
#282433=CARTESIAN_POINT('Ctrl Pts',(-1.04095169794807,1.15585458298854,
10.9992676102082));
#282434=CARTESIAN_POINT('Ctrl Pts',(-1.04090197985061,1.15589935670008,
10.9992627576112));
#282435=CARTESIAN_POINT('Ctrl Pts',(-1.04080234683531,1.1559890697291,10.9992530342439));
#282436=CARTESIAN_POINT('Ctrl Pts',(-1.04075243189458,1.15603400902247,
10.9992481634755));
#282437=CARTESIAN_POINT('Ctrl Pts',(-1.04067599346052,1.15610281891718,
10.9992407053068));
#282438=CARTESIAN_POINT('Ctrl Pts',(-1.04064947206665,1.15612669182953,
10.9992381177371));
#282439=CARTESIAN_POINT('Ctrl Pts',(-1.04059561844122,1.15617516416549,
10.9992328637869));
#282440=CARTESIAN_POINT('Ctrl Pts',(-1.04056828616208,1.1561997635296,10.9992301974109));
#282441=CARTESIAN_POINT('Ctrl Pts',(-1.04051277163853,1.15624972367327,
10.999224782059));
#282442=CARTESIAN_POINT('Ctrl Pts',(-1.04048458933168,1.15627508439848,
10.9992220330867));
#282443=CARTESIAN_POINT('Ctrl Pts',(-1.04042733301478,1.1563266044874,10.9992164485009));
#282444=CARTESIAN_POINT('Ctrl Pts',(-1.04039825894877,1.15635276378188,
10.9992136128926));
#282445=CARTESIAN_POINT('Ctrl Pts',(-1.04033917455867,1.15640592073375,
10.9992078507218));
#282446=CARTESIAN_POINT('Ctrl Pts',(-1.04030916416629,1.15643291832303,
10.9992049241642));
#282447=CARTESIAN_POINT('Ctrl Pts',(-1.04024815949679,1.15648779431579,
10.9991989754854));
#282448=CARTESIAN_POINT('Ctrl Pts',(-1.04021716515519,1.15651567263671,
10.9991959533705));
#282449=CARTESIAN_POINT('Ctrl Pts',(-1.04015414162699,1.15657235550215,
10.9991898086465));
#282450=CARTESIAN_POINT('Ctrl Pts',(-1.04012211236437,1.15660115996235,
10.9991866860436));
#282451=CARTESIAN_POINT('Ctrl Pts',(-1.04005696440284,1.15665974373659,
10.9991803350628));
#282452=CARTESIAN_POINT('Ctrl Pts',(-1.04002384561216,1.15668952296706,
10.9991771066909));
#282453=CARTESIAN_POINT('Ctrl Pts',(-1.03995646001558,1.15675010844828,
10.999170538507));
#282454=CARTESIAN_POINT('Ctrl Pts',(-1.03992219312673,1.15678091459261,
10.9991671987032));
#282455=CARTESIAN_POINT('Ctrl Pts',(-1.03985244841962,1.15684360991074,
10.9991604015729));
#282456=CARTESIAN_POINT('Ctrl Pts',(-1.03981697050171,1.15687549897655,
10.9991569442544));
#282457=CARTESIAN_POINT('Ctrl Pts',(-1.03974473606801,1.15694042035925,
10.9991499055544));
#282458=CARTESIAN_POINT('Ctrl Pts',(-1.03970797944307,1.15697345255826,
10.9991463241815));
#282459=CARTESIAN_POINT('Ctrl Pts',(-1.03963311470619,1.1570407250529,10.9991390303295));
#282460=CARTESIAN_POINT('Ctrl Pts',(-1.03959500647224,1.15707496522162,
10.9991353178596));
#282461=CARTESIAN_POINT('Ctrl Pts',(-1.03951735988305,1.15714472358759,
10.9991277542177));
#282462=CARTESIAN_POINT('Ctrl Pts',(-1.03947782140505,1.1571802416356,10.9991239030569));
#282463=CARTESIAN_POINT('Ctrl Pts',(-1.03939722938415,1.15725263127524,
10.99911605383));
#282464=CARTESIAN_POINT('Ctrl Pts',(-1.0393561756972,1.15728950271097,10.9991120557755));
#282465=CARTESIAN_POINT('Ctrl Pts',(-1.03927246134575,1.15736468080535,
10.9991039038881));
#282466=CARTESIAN_POINT('Ctrl Pts',(-1.03922980052158,1.1574029872932,10.9990997500677));
#282467=CARTESIAN_POINT('Ctrl Pts',(-1.0391427722718,1.15748112398872,10.9990912770342));
#282468=CARTESIAN_POINT('Ctrl Pts',(-1.03909840467282,1.15752095400529,
10.9990869578352));
#282469=CARTESIAN_POINT('Ctrl Pts',(-1.03900785470889,1.15760223380232,
10.9990781436092));
#282470=CARTESIAN_POINT('Ctrl Pts',(-1.03896167215727,1.1576436833668,10.9990736485984));
#282471=CARTESIAN_POINT('Ctrl Pts',(-1.0388673746507,1.15772830667017,10.999064471404));
#282472=CARTESIAN_POINT('Ctrl Pts',(-1.03881925948244,1.15777148017534,
10.9990597892376));
#282473=CARTESIAN_POINT('Ctrl Pts',(-1.03872096855693,1.15785966508199,
10.9990502253743));
#282474=CARTESIAN_POINT('Ctrl Pts',(-1.03867079256195,1.15790467622442,
10.9990453436965));
#282475=CARTESIAN_POINT('Ctrl Pts',(-1.03856824002864,1.15799666051055,
10.9990353673234));
#282476=CARTESIAN_POINT('Ctrl Pts',(-1.03851586322621,1.15804363336504,
10.9990302726495));
#282477=CARTESIAN_POINT('Ctrl Pts',(-1.03840875596478,1.158139676783,10.9990198555351));
#282478=CARTESIAN_POINT('Ctrl Pts',(-1.03835402521412,1.15818874702053,
10.9990145331187));
#282479=CARTESIAN_POINT('Ctrl Pts',(-1.0382420421965,1.15828913390693,10.9990036443566));
#282480=CARTESIAN_POINT('Ctrl Pts',(-1.03818478960058,1.15834045019296,
10.9989980780377));
#282481=CARTESIAN_POINT('Ctrl Pts',(-1.03806757845309,1.15844549247949,
10.9989866837189));
#282482=CARTESIAN_POINT('Ctrl Pts',(-1.03800761953384,1.15849921807104,
10.9989808557495));
#282483=CARTESIAN_POINT('Ctrl Pts',(-1.03788479261365,1.15860925871714,
10.9989689185889));
#282484=CARTESIAN_POINT('Ctrl Pts',(-1.03782192419709,1.15866557331252,
10.9989628094317));
#282485=CARTESIAN_POINT('Ctrl Pts',(-1.03769305403018,1.15878099029404,
10.9989502883328));
#282486=CARTESIAN_POINT('Ctrl Pts',(-1.03762705181061,1.15884009216119,
10.9989438764296));
#282487=CARTESIAN_POINT('Ctrl Pts',(-1.03356816846198,1.1624740055239,10.9985496249519));
#282488=CARTESIAN_POINT('Ctrl Pts',(-1.02955685226786,1.16602815711852,
10.9981633425255));
#282489=CARTESIAN_POINT('Ctrl Pts',(-1.0205100596288,1.17396081304609,10.9972996411769));
#282490=CARTESIAN_POINT('Ctrl Pts',(-1.01546470226551,1.17832771980069,
10.9968230691489));
#282491=CARTESIAN_POINT('Ctrl Pts',(-1.00005785387537,1.19149035075042,
10.9953826388546));
#282492=CARTESIAN_POINT('Ctrl Pts',(-0.989608705185513,1.20018315725476,
10.9944259087285));
#282493=CARTESIAN_POINT('Ctrl Pts',(-0.897424173241232,1.27485022514023,
10.9861458830792));
#282494=CARTESIAN_POINT('Ctrl Pts',(-0.809302212751961,1.33253517950121,
10.9793045699599));
#282495=CARTESIAN_POINT('Ctrl Pts',(-0.641516429719631,1.41953553188741,
10.9668683898685));
#282496=CARTESIAN_POINT('Ctrl Pts',(-0.564010858420602,1.45207232399123,
10.9613211039638));
#282497=CARTESIAN_POINT('Ctrl Pts',(-0.45829848584594,1.48670418611114,
10.9536987008877));
#282498=CARTESIAN_POINT('Ctrl Pts',(-0.432114423602015,1.49452460934193,
10.9518072779189));
#282499=CARTESIAN_POINT('Ctrl Pts',(-0.393703126391878,1.5049031676973,
10.9490202284223));
#282500=CARTESIAN_POINT('Ctrl Pts',(-0.38162860725155,1.50801037324325,
10.9481423874465));
#282501=CARTESIAN_POINT('Ctrl Pts',(-0.360238039427589,1.51324158019046,
10.946583522485));
#282502=CARTESIAN_POINT('Ctrl Pts',(-0.350937212327386,1.51542554768599,
10.9459044780075));
#282503=CARTESIAN_POINT('Ctrl Pts',(-0.331390167504047,1.51982587691099,
10.9444744812599));
#282504=CARTESIAN_POINT('Ctrl Pts',(-0.321140518890845,1.52202460437777,
10.9437229973442));
#282505=CARTESIAN_POINT('Ctrl Pts',(-0.293960466217599,1.52756843058981,
10.9417254268116));
#282506=CARTESIAN_POINT('Ctrl Pts',(-0.276995715133783,1.53073557307638,
10.9404737175396));
#282507=CARTESIAN_POINT('Ctrl Pts',(-0.194354385396315,1.54474510341847,
10.9343500417885));
#282508=CARTESIAN_POINT('Ctrl Pts',(-0.128089580697416,1.55164487114233,
10.9293555918289));
#282509=CARTESIAN_POINT('Ctrl Pts',(0.0436706834585422,1.55845158738,10.9162118709234));
#282510=CARTESIAN_POINT('Ctrl Pts',(0.149079943992258,1.55191874261404,
10.90793949041));
#282511=CARTESIAN_POINT('Ctrl Pts',(0.280210361831377,1.53030128256928,
10.8977661398102));
#282512=CARTESIAN_POINT('Ctrl Pts',(0.307282176764719,1.52509596928942,
10.895673952158));
#282513=CARTESIAN_POINT('Ctrl Pts',(0.352199895423476,1.51521452228139,
10.8922302855463));
#282514=CARTESIAN_POINT('Ctrl Pts',(0.370126141399257,1.51093564849712,
10.8908634358028));
#282515=CARTESIAN_POINT('Ctrl Pts',(0.395251312297537,1.50446440173053,
10.8889621362731));
#282516=CARTESIAN_POINT('Ctrl Pts',(0.402516015508042,1.50253705427318,
10.8884141109401));
#282517=CARTESIAN_POINT('Ctrl Pts',(0.414994956898455,1.49912935039154,
10.8874760344921));
#282518=CARTESIAN_POINT('Ctrl Pts',(0.420215827152018,1.49767429228163,
10.8870845765022));
#282519=CARTESIAN_POINT('Ctrl Pts',(0.431278512647751,1.4945287132472,10.8862573136989));
#282520=CARTESIAN_POINT('Ctrl Pts',(0.437118115670375,1.49283119827138,
10.8858219121576));
#282521=CARTESIAN_POINT('Ctrl Pts',(0.453115430075007,1.48807901731567,
10.8846322847013));
#282522=CARTESIAN_POINT('Ctrl Pts',(0.463252323852146,1.48495456346796,
10.8838819431429));
#282523=CARTESIAN_POINT('Ctrl Pts',(0.517000695679873,1.46778394658538,
10.8799180208293));
#282524=CARTESIAN_POINT('Ctrl Pts',(0.560012158111801,1.45191829482634,
10.8767970031312));
#282525=CARTESIAN_POINT('Ctrl Pts',(0.690153591675974,1.397266950416,10.8673308588443));
#282526=CARTESIAN_POINT('Ctrl Pts',(0.774466623102506,1.35235717699037,
10.8611546890569));
#282527=CARTESIAN_POINT('Ctrl Pts',(0.912717935259911,1.26152240260745,
10.8501735948664));
#282528=CARTESIAN_POINT('Ctrl Pts',(0.968620024274432,1.21912515011395,
10.845454042871));
#282529=CARTESIAN_POINT('Ctrl Pts',(1.03438778115328,1.16185868343569,10.8393957405231));
#282530=CARTESIAN_POINT('Ctrl Pts',(1.04711940035235,1.1503975847477,10.8381975466709));
#282531=CARTESIAN_POINT('Ctrl Pts',(1.06736293224256,1.1315597084454,10.836249041304));
#282532=CARTESIAN_POINT('Ctrl Pts',(1.07499400817569,1.12431262355043,10.8355042376461));
#282533=CARTESIAN_POINT('Ctrl Pts',(1.08949589146341,1.11025784971075,10.8340685067181));
#282534=CARTESIAN_POINT('Ctrl Pts',(1.09637791311915,1.10346239365883,10.8333781311068));
#282535=CARTESIAN_POINT('Ctrl Pts',(1.11202725631845,1.08771896865687,10.8317870207963));
#282536=CARTESIAN_POINT('Ctrl Pts',(1.12075064359249,1.07872848828154,10.8308844220105));
#282537=CARTESIAN_POINT('Ctrl Pts',(1.14863268075869,1.04928946500994,10.827947411693));
#282538=CARTESIAN_POINT('Ctrl Pts',(1.16734662431439,1.02842942774217,10.8258944741035));
#282539=CARTESIAN_POINT('Ctrl Pts',(1.26298756999246,0.915845142358684,
10.814952418841));
#282540=CARTESIAN_POINT('Ctrl Pts',(1.3296870433578,0.815985659815655,10.8056690057718));
#282541=CARTESIAN_POINT('Ctrl Pts',(1.41405871655401,0.651370685682743,
10.7913494688679));
#282542=CARTESIAN_POINT('Ctrl Pts',(1.44016148466121,0.591424110158831,
10.7863232048708));
#282543=CARTESIAN_POINT('Ctrl Pts',(1.46750209729009,0.5159848187844,10.7803499922913));
#282544=CARTESIAN_POINT('Ctrl Pts',(1.47238274840529,0.50188825871935,10.7792485677161));
#282545=CARTESIAN_POINT('Ctrl Pts',(1.47924470494201,0.481106950246127,
10.7776484783731));
#282546=CARTESIAN_POINT('Ctrl Pts',(1.48138489519147,0.474476123689844,
10.7771414270284));
#282547=CARTESIAN_POINT('Ctrl Pts',(1.48494939811085,0.463173172550702,
10.7762833042304));
#282548=CARTESIAN_POINT('Ctrl Pts',(1.48639635697944,0.458508424514052,
10.7759309514881));
#282549=CARTESIAN_POINT('Ctrl Pts',(1.48964971023554,0.4478428961885,10.775129473958));
#282550=CARTESIAN_POINT('Ctrl Pts',(1.49144184304489,0.441837924318492,
10.7746811749112));
#282551=CARTESIAN_POINT('Ctrl Pts',(1.49631963863644,0.425125801893591,
10.7734412989697));
#282552=CARTESIAN_POINT('Ctrl Pts',(1.49932669364301,0.414395816687696,
10.7726540559111));
#282553=CARTESIAN_POINT('Ctrl Pts',(1.51893460664779,0.341420391927617,
10.7673536691209));
#282554=CARTESIAN_POINT('Ctrl Pts',(1.53177224071184,0.278219744739171,
10.7630260166086));
#282555=CARTESIAN_POINT('Ctrl Pts',(1.54297133573613,0.197743356954738,
10.757637767271));
#282556=CARTESIAN_POINT('Ctrl Pts',(1.5450187499334,0.181052628470811,10.7565268815939));
#282557=CARTESIAN_POINT('Ctrl Pts',(1.55369601227163,0.0993767274136418,
10.7511102128562));
#282558=CARTESIAN_POINT('Ctrl Pts',(1.55649837239951,0.0340529898274769,
10.7468349833151));
#282559=CARTESIAN_POINT('Ctrl Pts',(1.55433318553348,-0.0736907103521706,
10.7396583767273));
#282560=CARTESIAN_POINT('Ctrl Pts',(1.55174370631422,-0.116073358986913,
10.7368040125552));
#282561=CARTESIAN_POINT('Ctrl Pts',(1.54439432932295,-0.187917833713793,
10.7318664862688));
#282562=CARTESIAN_POINT('Ctrl Pts',(1.54051420598669,-0.21744594718336,
10.7298085794043));
#282563=CARTESIAN_POINT('Ctrl Pts',(1.53373520605703,-0.259623029228178,
10.7268183001497));
#282564=CARTESIAN_POINT('Ctrl Pts',(1.5315217151264,-0.272376610145237,
10.7259073961001));
#282565=CARTESIAN_POINT('Ctrl Pts',(1.52737454149724,-0.294620143452055,
10.7243062061328));
#282566=CARTESIAN_POINT('Ctrl Pts',(1.52551089189618,-0.304122557384738,
10.7236181756145));
#282567=CARTESIAN_POINT('Ctrl Pts',(1.52146151743582,-0.323795155115286,
10.7221851323312));
#282568=CARTESIAN_POINT('Ctrl Pts',(1.51926225801547,-0.333962023513264,
10.7214397185577));
#282569=CARTESIAN_POINT('Ctrl Pts',(1.51328258567308,-0.360322898597827,
10.7194940607842));
#282570=CARTESIAN_POINT('Ctrl Pts',(1.50934425021789,-0.376479308543374,
10.7182888199874));
#282571=CARTESIAN_POINT('Ctrl Pts',(1.49100580577201,-0.446790707899251,
10.7129857514901));
#282572=CARTESIAN_POINT('Ctrl Pts',(1.47394602061114,-0.500201929933816,
10.7088039518584));
#282573=CARTESIAN_POINT('Ctrl Pts',(1.41944362415481,-0.643620434648861,
10.6971509738672));
#282574=CARTESIAN_POINT('Ctrl Pts',(1.37636878239441,-0.73121376627802,
10.6895436084874));
#282575=CARTESIAN_POINT('Ctrl Pts',(1.30470121076244,-0.847878380833579,
10.6789745496787));
#282576=CARTESIAN_POINT('Ctrl Pts',(1.28273120023684,-0.880763354928661,
10.6759440892604));
#282577=CARTESIAN_POINT('Ctrl Pts',(1.25005071238283,-0.925858766696184,
10.6717471414629));
#282578=CARTESIAN_POINT('Ctrl Pts',(1.24036709889929,-0.938792174621642,
10.6705384855767));
#282579=CARTESIAN_POINT('Ctrl Pts',(1.22291440399567,-0.96136033410246,
10.6684237315943));
#282580=CARTESIAN_POINT('Ctrl Pts',(1.21522866596205,-0.971057488813742,
10.6675131415356));
#282581=CARTESIAN_POINT('Ctrl Pts',(1.20336017080253,-0.985670419329448,
10.666139282267));
#282582=CARTESIAN_POINT('Ctrl Pts',(1.1992614023299,-0.99065330419979,10.6656705082037));
#282583=CARTESIAN_POINT('Ctrl Pts',(1.19168908197599,-0.999743122211864,
10.6648150378832));
#282584=CARTESIAN_POINT('Ctrl Pts',(1.18822517346333,-1.00385761812722,
10.664427709035));
#282585=CARTESIAN_POINT('Ctrl Pts',(1.18023073253259,-1.01325420753702,
10.6635428232858));
#282586=CARTESIAN_POINT('Ctrl Pts',(1.17568602174884,-1.01852395864091,
10.6630463078011));
#282587=CARTESIAN_POINT('Ctrl Pts',(1.1615883998763,-1.03465054909685,10.6615254089667));
#282588=CARTESIAN_POINT('Ctrl Pts',(1.15191900523431,-1.04540519137823,
10.6605090877456));
#282589=CARTESIAN_POINT('Ctrl Pts',(1.08021910309249,-1.12294936306196,
10.6531520381283));
#282590=CARTESIAN_POINT('Ctrl Pts',(1.01256557898478,-1.18431594147996,
10.6471632063603));
#282591=CARTESIAN_POINT('Ctrl Pts',(0.880402876411588,-1.28454272709726,
10.6362486238223));
#282592=CARTESIAN_POINT('Ctrl Pts',(0.817718773075237,-1.32532796554308,
10.6313409701965));
#282593=CARTESIAN_POINT('Ctrl Pts',(0.714525528822122,-1.38235347069619,
10.6233812337839));
#282594=CARTESIAN_POINT('Ctrl Pts',(0.675849522873213,-1.4016685465521,
10.6204235424133));
#282595=CARTESIAN_POINT('Ctrl Pts',(0.622909599836934,-1.42540632313544,
10.6163776182191));
#282596=CARTESIAN_POINT('Ctrl Pts',(0.609311445655792,-1.43127184392235,
10.6153386834402));
#282597=CARTESIAN_POINT('Ctrl Pts',(0.586383345584795,-1.44077585255483,
10.6135862902054));
#282598=CARTESIAN_POINT('Ctrl Pts',(0.577098073983648,-1.44452008977695,
10.6128764505064));
#282599=CARTESIAN_POINT('Ctrl Pts',(0.558682321998663,-1.45174024912831,
10.6114679334567));
#282600=CARTESIAN_POINT('Ctrl Pts',(0.549553950336764,-1.45522030478902,
10.6107694336516));
#282601=CARTESIAN_POINT('Ctrl Pts',(0.527196992078277,-1.46350320650752,
10.6090575740427));
#282602=CARTESIAN_POINT('Ctrl Pts',(0.513935066904985,-1.4682128683091,
10.6080411679831));
#282603=CARTESIAN_POINT('Ctrl Pts',(0.467814940902906,-1.4838899297717,
10.6045021427266));
#282604=CARTESIAN_POINT('Ctrl Pts',(0.434657790014992,-1.49393855205032,
10.6019499874408));
#282605=CARTESIAN_POINT('Ctrl Pts',(0.29202626562788,-1.53201438527138,
10.5909310248924));
#282606=CARTESIAN_POINT('Ctrl Pts',(0.180020315406287,-1.54917163311738,
10.5821444849164));
#282607=CARTESIAN_POINT('Ctrl Pts',(0.00402761114676129,-1.55677807437264,
10.5685053928937));
#282608=CARTESIAN_POINT('Ctrl Pts',(-0.0592256624206096,-1.55565683545488,
10.5636452995368));
#282609=CARTESIAN_POINT('Ctrl Pts',(-0.136867693395798,-1.54953630220077,
10.5578485657119));
#282610=CARTESIAN_POINT('Ctrl Pts',(-0.151477981002337,-1.5481763401527,
10.556765306983));
#282611=CARTESIAN_POINT('Ctrl Pts',(-0.172927099247937,-1.54587323690691,
10.5551881468075));
#282612=CARTESIAN_POINT('Ctrl Pts',(-0.179781872361547,-1.54509104245646,
10.5546860947671));
#282613=CARTESIAN_POINT('Ctrl Pts',(-0.191456060092176,-1.54368016263172,
10.5538346968666));
#282614=CARTESIAN_POINT('Ctrl Pts',(-0.19627800046861,-1.54307446884621,
10.5534841028645));
#282615=CARTESIAN_POINT('Ctrl Pts',(-0.207317806202073,-1.54163514826792,
10.5526839009365));
#282616=CARTESIAN_POINT('Ctrl Pts',(-0.213533552442724,-1.54078649683234,
10.5522351381241));
#282617=CARTESIAN_POINT('Ctrl Pts',(-0.230827036101754,-1.53831871250283,
10.5509911023957));
#282618=CARTESIAN_POINT('Ctrl Pts',(-0.241892957051312,-1.53661751851175,
10.5502002241428));
#282619=CARTESIAN_POINT('Ctrl Pts',(-0.324529278761555,-1.52299876042578,
10.5443263422957));
#282620=CARTESIAN_POINT('Ctrl Pts',(-0.395216003340494,-1.50620442150986,
10.5394804033611));
#282621=CARTESIAN_POINT('Ctrl Pts',(-0.471143182596088,-1.48244834337477,
10.5342219939404));
#282622=CARTESIAN_POINT('Ctrl Pts',(-0.477791942356082,-1.48031883388497,
10.5337610927843));
#282623=CARTESIAN_POINT('Ctrl Pts',(-0.594167636441013,-1.44217951342381,
10.5256828403769));
#282624=CARTESIAN_POINT('Ctrl Pts',(-0.699551572562077,-1.39410963233642,
10.5181636623792));
#282625=CARTESIAN_POINT('Ctrl Pts',(-0.820807408283012,-1.32156068433765,
10.5084611466662));
#282626=CARTESIAN_POINT('Ctrl Pts',(-0.842638061758683,-1.30774936762469,
10.5066702783925));
#282627=CARTESIAN_POINT('Ctrl Pts',(-0.874305903834928,-1.28659227587884,
10.5040002592941));
#282628=CARTESIAN_POINT('Ctrl Pts',(-0.884416981160518,-1.27966287980456,
10.5031365743692));
#282629=CARTESIAN_POINT('Ctrl Pts',(-0.902292720529272,-1.26709909218653,
10.5015889021219));
#282630=CARTESIAN_POINT('Ctrl Pts',(-0.910089229686228,-1.26151093907696,
10.5009067032456));
#282631=CARTESIAN_POINT('Ctrl Pts',(-0.926497827399249,-1.24951878614979,
10.4994553240668));
#282632=CARTESIAN_POINT('Ctrl Pts',(-0.935096284482033,-1.24309707954092,
10.4986854804122));
#282633=CARTESIAN_POINT('Ctrl Pts',(-0.958077735723065,-1.22556016042067,
10.4966022283066));
#282634=CARTESIAN_POINT('Ctrl Pts',(-0.972333071261647,-1.21428126929477,
10.4952824313227));
#282635=CARTESIAN_POINT('Ctrl Pts',(-1.05483313371558,-1.14662248259357,
10.4874771233534));
#282636=CARTESIAN_POINT('Ctrl Pts',(-1.11835065451292,-1.08475933374101,
10.480768445215));
#282637=CARTESIAN_POINT('Ctrl Pts',(-1.23177437772815,-0.953682870696902,
10.4673943728585));
#282638=CARTESIAN_POINT('Ctrl Pts',(-1.28195110414912,-0.885088037894109,
10.4607627246729));
#282639=CARTESIAN_POINT('Ctrl Pts',(-1.33936430480862,-0.791397640484429,
10.452378617557));
#282640=CARTESIAN_POINT('Ctrl Pts',(-1.35192822332241,-0.769738392572532,
10.4504841463116));
#282641=CARTESIAN_POINT('Ctrl Pts',(-1.3722360572939,-0.732696731035967,
10.4473277611513));
#282642=CARTESIAN_POINT('Ctrl Pts',(-1.3802571565989,-0.717472329251631,
10.4460535485327));
#282643=CARTESIAN_POINT('Ctrl Pts',(-1.39134474642483,-0.695553130718436,
10.4442548646842));
#282644=CARTESIAN_POINT('Ctrl Pts',(-1.39461857256909,-0.688965459174152,
10.4437188340359));
#282645=CARTESIAN_POINT('Ctrl Pts',(-1.40022480099366,-0.677480753865958,
10.4427925313469));
#282646=CARTESIAN_POINT('Ctrl Pts',(-1.40257850835641,-0.672594377674542,
10.4424009840639));
#282647=CARTESIAN_POINT('Ctrl Pts',(-1.40756918015765,-0.662093441665002,
10.4415651057953));
#282648=CARTESIAN_POINT('Ctrl Pts',(-1.4101981712845,-0.656475318433295,
10.4411212551461));
#282649=CARTESIAN_POINT('Ctrl Pts',(-1.41734560170118,-0.640960260255658,
10.4399043109389));
#282650=CARTESIAN_POINT('Ctrl Pts',(-1.42179403473055,-0.631031180089095,
10.4391353100348));
#282651=CARTESIAN_POINT('Ctrl Pts',(-1.44736783293577,-0.572305759501093,
10.4346397161898));
#282652=CARTESIAN_POINT('Ctrl Pts',(-1.46608657013888,-0.522493105784168,
10.4310385650746));
#282653=CARTESIAN_POINT('Ctrl Pts',(-1.51487353493543,-0.369227272879561,
10.4203083446149));
#282654=CARTESIAN_POINT('Ctrl Pts',(-1.53679023186072,-0.263528494897026,
10.4133551911491));
#282655=CARTESIAN_POINT('Ctrl Pts',(-1.55285780976403,-0.10454766141402,
10.4026385412856));
#282656=CARTESIAN_POINT('Ctrl Pts',(-1.55548860999734,-0.0524581471936984,
10.39909089029));
#282657=CARTESIAN_POINT('Ctrl Pts',(-1.55550339476856,0.0154151398900086,
10.3943653259887));
#282658=CARTESIAN_POINT('Ctrl Pts',(-1.55526749419952,0.0311677294658214,
10.3932614955591));
#282659=CARTESIAN_POINT('Ctrl Pts',(-1.55448434391733,0.0571226334950191,
10.3914297220558));
#282660=CARTESIAN_POINT('Ctrl Pts',(-1.55407576101648,0.0673282314157227,
10.3907061367901));
#282661=CARTESIAN_POINT('Ctrl Pts',(-1.55308009122629,0.0872800231357074,
10.3892846722555));
#282662=CARTESIAN_POINT('Ctrl Pts',(-1.55250168526127,0.0970261894663112,
10.3885870978017));
#282663=CARTESIAN_POINT('Ctrl Pts',(-1.55090798799796,0.120190382918794,
10.3869211766082));
#282664=CARTESIAN_POINT('Ctrl Pts',(-1.54981026824769,0.133601746397285,
10.3859502916934));
#282665=CARTESIAN_POINT('Ctrl Pts',(-1.54541734539986,0.179879020995319,
10.3825771761104));
#282666=CARTESIAN_POINT('Ctrl Pts',(-1.54124965030803,0.212650989996383,
10.3801480862077));
#282667=CARTESIAN_POINT('Ctrl Pts',(-1.52829064496567,0.293811040400294,
10.3740273609555));
#282668=CARTESIAN_POINT('Ctrl Pts',(-1.5182424458844,0.341959457437992,
10.3703014584866));
#282669=CARTESIAN_POINT('Ctrl Pts',(-1.4911687327985,0.446622424415674,
10.3620102574895));
#282670=CARTESIAN_POINT('Ctrl Pts',(-1.47317256477927,0.502809950775666,
10.357431445426));
#282671=CARTESIAN_POINT('Ctrl Pts',(-1.42464954658911,0.629113615484411,
10.3469431409563));
#282672=CARTESIAN_POINT('Ctrl Pts',(-1.39205275426318,0.698285161738727,
10.3410517378102));
#282673=CARTESIAN_POINT('Ctrl Pts',(-1.34897241668961,0.774583881645573,
10.3345696878018));
#282674=CARTESIAN_POINT('Ctrl Pts',(-1.34333577373525,0.784318678359529,
10.3337430898461));
#282675=CARTESIAN_POINT('Ctrl Pts',(-1.33438609337416,0.799395706152846,
10.3324645422152));
#282676=CARTESIAN_POINT('Ctrl Pts',(-1.33114558091394,0.80478021058844,
10.3320082671268));
#282677=CARTESIAN_POINT('Ctrl Pts',(-1.32534085038746,0.814294484233974,
10.3312028404795));
#282678=CARTESIAN_POINT('Ctrl Pts',(-1.32278987113353,0.818431936525194,
10.3308528751958));
#282679=CARTESIAN_POINT('Ctrl Pts',(-1.31657658190223,0.82840437567501,
10.3300099791922));
#282680=CARTESIAN_POINT('Ctrl Pts',(-1.3128948479954,0.834227084533779,
10.3295183238861));
#282681=CARTESIAN_POINT('Ctrl Pts',(-1.30129188637797,0.852310231800497,
10.3279923347766));
#282682=CARTESIAN_POINT('Ctrl Pts',(-1.29323641070349,0.86448419954538,
10.3269663170907));
#282683=CARTESIAN_POINT('Ctrl Pts',(-1.24982904115684,0.928119282113831,
10.3215998339502));
#282684=CARTESIAN_POINT('Ctrl Pts',(-1.21157009261602,0.977536602587193,
10.3174195330472));
#282685=CARTESIAN_POINT('Ctrl Pts',(-1.09744379398282,1.10791693402874,
10.3059468231119));
#282686=CARTESIAN_POINT('Ctrl Pts',(-1.01574965047762,1.18326431312146,
10.2987650513598));
#282687=CARTESIAN_POINT('Ctrl Pts',(-0.897145009003289,1.27124712461845,
10.2887457100352));
#282688=CARTESIAN_POINT('Ctrl Pts',(-0.866777678880776,1.29214338084181,
10.2862141245161));
#282689=CARTESIAN_POINT('Ctrl Pts',(-0.82356489223676,1.31966969156601,
10.2826382766307));
#282690=CARTESIAN_POINT('Ctrl Pts',(-0.81132459788647,1.32723004750484,
10.2816282983451));
#282691=CARTESIAN_POINT('Ctrl Pts',(-0.791309710654248,1.33921213514567,
10.2799804937974));
#282692=CARTESIAN_POINT('Ctrl Pts',(-0.783598559486943,1.34373862510608,
10.2793465135684));
#282693=CARTESIAN_POINT('Ctrl Pts',(-0.767347913949675,1.35309039954303,
10.2780120075182));
#282694=CARTESIAN_POINT('Ctrl Pts',(-0.758800976236422,1.35790188183994,
10.2773110203419));
#282695=CARTESIAN_POINT('Ctrl Pts',(-0.738192999311206,1.36924778767238,
10.2756226222257));
#282696=CARTESIAN_POINT('Ctrl Pts',(-0.726090100142797,1.37570402060775,
10.2746324871337));
#282697=CARTESIAN_POINT('Ctrl Pts',(-0.682987747595944,1.39796954154876,
10.2711103458631));
#282698=CARTESIAN_POINT('Ctrl Pts',(-0.651547022361764,1.41289674927607,
10.268548168706));
#282699=CARTESIAN_POINT('Ctrl Pts',(-0.570968344893476,1.44789174332572,
10.2619944177055));
#282700=CARTESIAN_POINT('Ctrl Pts',(-0.521257455203041,1.46652139839682,
10.2579618043999));
#282701=CARTESIAN_POINT('Ctrl Pts',(-0.433556354551367,1.49436527048542,
10.2508863759753));
#282702=CARTESIAN_POINT('Ctrl Pts',(-0.395987329333671,1.50475663933873,
10.2478678521476));
#282703=CARTESIAN_POINT('Ctrl Pts',(-0.276000358155853,1.53313931874455,
10.2383051808145));
#282704=CARTESIAN_POINT('Ctrl Pts',(-0.192480951828211,1.54584805374588,
10.2317562760017));
#282705=CARTESIAN_POINT('Ctrl Pts',(-0.0934648524612849,1.55276102561773,
10.2243660206077));
#282706=CARTESIAN_POINT('Ctrl Pts',(-0.0785787314062581,1.5535855006278,
10.2232650681283));
#282707=CARTESIAN_POINT('Ctrl Pts',(-0.0567413935722078,1.5544802739144,
10.2216669549433));
#282708=CARTESIAN_POINT('Ctrl Pts',(-0.0497984322582944,1.5547181830929,
10.221161358905));
#282709=CARTESIAN_POINT('Ctrl Pts',(-0.0374754372895732,1.55505780979167,
10.2202687006766));
#282710=CARTESIAN_POINT('Ctrl Pts',(-0.0320962008876879,1.55517813678579,
10.219880649342));
#282711=CARTESIAN_POINT('Ctrl Pts',(-0.02024921028454,1.5553816423701,10.2190295900416));
#282712=CARTESIAN_POINT('Ctrl Pts',(-0.0137814626568731,1.55545239697449,
10.2185672685518));
#282713=CARTESIAN_POINT('Ctrl Pts',(0.00513299666084232,1.55554132578864,
10.2172214876871));
#282714=CARTESIAN_POINT('Ctrl Pts',(0.0175800728929955,1.55545045909689,
10.2163437735013));
#282715=CARTESIAN_POINT('Ctrl Pts',(0.0463027814650971,1.55489593216534,
10.2143338214371));
#282716=CARTESIAN_POINT('Ctrl Pts',(0.0625751415140964,1.55432612642567,
10.2132065688345));
#282717=CARTESIAN_POINT('Ctrl Pts',(0.11879977693695,1.55147286698851,10.2093419542077));
#282718=CARTESIAN_POINT('Ctrl Pts',(0.158673144433685,1.54790333809282,
10.2066540108054));
#282719=CARTESIAN_POINT('Ctrl Pts',(0.326973655330104,1.52626391728274,
10.1953693837633));
#282720=CARTESIAN_POINT('Ctrl Pts',(0.453000507836864,1.49371462508195,
10.1870239642509));
#282721=CARTESIAN_POINT('Ctrl Pts',(0.601465998060656,1.43482480330409,
10.1761157768921));
#282722=CARTESIAN_POINT('Ctrl Pts',(0.629074870052894,1.42293645980539,
10.174040828878));
#282723=CARTESIAN_POINT('Ctrl Pts',(0.667224960076323,1.40518175370018,
10.1710980222386));
#282724=CARTESIAN_POINT('Ctrl Pts',(0.678069805025433,1.3999807975309,10.1702527343258));
#282725=CARTESIAN_POINT('Ctrl Pts',(0.696860472864829,1.39069964189242,
10.1687721919811));
#282726=CARTESIAN_POINT('Ctrl Pts',(0.70483359537619,1.38667574053434,10.1681389110086));
#282727=CARTESIAN_POINT('Ctrl Pts',(0.72150164302638,1.37808276288746,10.1668040745716));
#282728=CARTESIAN_POINT('Ctrl Pts',(0.730188795982824,1.3734995581754,10.1661020439717));
#282729=CARTESIAN_POINT('Ctrl Pts',(0.750962387331102,1.36228696114578,
10.1644076516162));
#282730=CARTESIAN_POINT('Ctrl Pts',(0.763005045205246,1.35557867714106,
10.163412518788));
#282731=CARTESIAN_POINT('Ctrl Pts',(0.805525017865236,1.33114711006379,
10.1598517373085));
#282732=CARTESIAN_POINT('Ctrl Pts',(0.835484987815926,1.31255005556845,
10.1572550385398));
#282733=CARTESIAN_POINT('Ctrl Pts',(0.909749626136563,1.26287850474203,
10.1505868326479));
#282734=CARTESIAN_POINT('Ctrl Pts',(0.953110155757862,1.23048221314794,
10.1464723909431));
#282735=CARTESIAN_POINT('Ctrl Pts',(1.08296112726762,1.12247814855842,10.1334771471873));
#282736=CARTESIAN_POINT('Ctrl Pts',(1.16283087267265,1.03951312353195,10.1244443299217));
#282737=CARTESIAN_POINT('Ctrl Pts',(1.24465143092602,0.933165587419026,
10.1143828479651));
#282738=CARTESIAN_POINT('Ctrl Pts',(1.25617207246346,0.917598502778497,
10.1129446084986));
#282739=CARTESIAN_POINT('Ctrl Pts',(1.27198588404965,0.895374076450525,
10.1109437433006));
#282740=CARTESIAN_POINT('Ctrl Pts',(1.2765229881443,0.888893634761648,10.1103664405932));
#282741=CARTESIAN_POINT('Ctrl Pts',(1.28410432545275,0.877887279353,10.1093966335496));
#282742=CARTESIAN_POINT('Ctrl Pts',(1.28717451057306,0.873379514953184,
10.1090024318707));
#282743=CARTESIAN_POINT('Ctrl Pts',(1.29353197199915,0.86393889998516,10.1081832101091));
#282744=CARTESIAN_POINT('Ctrl Pts',(1.29681485004551,0.859003279009716,
10.1077584764241));
#282745=CARTESIAN_POINT('Ctrl Pts',(1.30550938150789,0.845768093985171,
10.106628653724));
#282746=CARTESIAN_POINT('Ctrl Pts',(1.31087020173034,0.837435216430967,
10.1059268262796));
#282747=CARTESIAN_POINT('Ctrl Pts',(1.33761554398154,0.794975949417039,
10.1023955066197));
#282748=CARTESIAN_POINT('Ctrl Pts',(1.35775067780397,0.760076220453683,
10.0996379220186));
#282749=CARTESIAN_POINT('Ctrl Pts',(1.4117830855697,0.657407811024459,10.0918171268182));
#282750=CARTESIAN_POINT('Ctrl Pts',(1.44211591904419,0.587894183250133,
10.0868684680191));
#282751=CARTESIAN_POINT('Ctrl Pts',(1.49856949249769,0.427504291966573,
10.0756667832826));
#282752=CARTESIAN_POINT('Ctrl Pts',(1.52171870499869,0.335915333446381,
10.0694067945121));
#282753=CARTESIAN_POINT('Ctrl Pts',(1.53926479428324,0.224884800995694,
10.0616103018775));
#282754=CARTESIAN_POINT('Ctrl Pts',(1.54178245938857,0.206920469491736,
10.0603431044049));
#282755=CARTESIAN_POINT('Ctrl Pts',(1.54528735785166,0.17827553037528,10.058311273358));
#282756=CARTESIAN_POINT('Ctrl Pts',(1.54647931767233,0.167621277595261,
10.0575530960274));
#282757=CARTESIAN_POINT('Ctrl Pts',(1.54852860141261,0.147415641208562,
10.0561101577074));
#282758=CARTESIAN_POINT('Ctrl Pts',(1.54940791830335,0.137866949577216,
10.0554261233956));
#282759=CARTESIAN_POINT('Ctrl Pts',(1.55121038825255,0.11609026347054,10.0538609479578));
#282760=CARTESIAN_POINT('Ctrl Pts',(1.55207732900648,0.103858397179467,
10.0529780856248));
#282761=CARTESIAN_POINT('Ctrl Pts',(1.55432356288825,0.0657877608959347,
10.0502180268214));
#282762=CARTESIAN_POINT('Ctrl Pts',(1.55520275199466,0.0399251678423884,
10.0483254570714));
#282763=CARTESIAN_POINT('Ctrl Pts',(1.55629952202834,-0.0814601183507938,
10.0393549435886));
#282764=CARTESIAN_POINT('Ctrl Pts',(1.54836288114979,-0.176835265194943,
10.0320336144696));
#282765=CARTESIAN_POINT('Ctrl Pts',(1.51534653778634,-0.363541902773961,
10.0173396684373));
#282766=CARTESIAN_POINT('Ctrl Pts',(1.49057942071121,-0.454548072093131,
10.0100020859026));
#282767=CARTESIAN_POINT('Ctrl Pts',(1.45313966025916,-0.55510246454981,
10.0020173604628));
#282768=CARTESIAN_POINT('Ctrl Pts',(1.44838860799548,-0.56738354612946,
10.0010445834244));
#282769=CARTESIAN_POINT('Ctrl Pts',(1.44098841786745,-0.585813462746825,
9.9995899563391));
#282770=CARTESIAN_POINT('Ctrl Pts',(1.43845474479215,-0.592007588736285,
9.99910196428355));
#282771=CARTESIAN_POINT('Ctrl Pts',(1.43378124046212,-0.603225845657192,
9.99822003104053));
#282772=CARTESIAN_POINT('Ctrl Pts',(1.43165478088288,-0.608255422204919,
9.99782531888312));
#282773=CARTESIAN_POINT('Ctrl Pts',(1.42717082773411,-0.618707227318865,
9.99700665963995));
#282774=CARTESIAN_POINT('Ctrl Pts',(1.42480884527055,-0.624127360596184,
9.99658298562653));
#282775=CARTESIAN_POINT('Ctrl Pts',(1.41843407464344,-0.638530991334191,
9.99545907575346));
#282776=CARTESIAN_POINT('Ctrl Pts',(1.41436677873941,-0.647490292925158,
9.99476204235993));
#282777=CARTESIAN_POINT('Ctrl Pts',(1.3936234462841,-0.692054694941648,
9.99130225993986));
#282778=CARTESIAN_POINT('Ctrl Pts',(1.37568515912833,-0.727060501835112,
9.98860797429469));
#282779=CARTESIAN_POINT('Ctrl Pts',(1.31899441143588,-0.828061687075055,
9.98079349592539));
#282780=CARTESIAN_POINT('Ctrl Pts',(1.27667870295967,-0.891922289692205,
9.97579523617957));
#282781=CARTESIAN_POINT('Ctrl Pts',(1.1718978683036,-1.02722382843487,9.96452203847612));
#282782=CARTESIAN_POINT('Ctrl Pts',(1.1072657507728,-1.09658215736149,9.95824108126202));
#282783=CARTESIAN_POINT('Ctrl Pts',(1.0232169401654,-1.17172366078031,9.95042154537807));
#282784=CARTESIAN_POINT('Ctrl Pts',(1.00948491285748,-1.18357484204755,
9.94915441897439));
#282785=CARTESIAN_POINT('Ctrl Pts',(0.987312195378336,-1.20204401123956,
9.94712268312834));
#282786=CARTESIAN_POINT('Ctrl Pts',(0.979004589510791,-1.20881974646406,
9.94636452916766));
#282787=CARTESIAN_POINT('Ctrl Pts',(0.963134725257411,-1.22149240653079,
9.94492162386247));
#282788=CARTESIAN_POINT('Ctrl Pts',(0.955586645869443,-1.22740635197405,
9.94423759906924));
#282789=CARTESIAN_POINT('Ctrl Pts',(0.938262409294526,-1.24072328527305,
9.94267242953202));
#282790=CARTESIAN_POINT('Ctrl Pts',(0.928452530916719,-1.24808112762479,
9.9417895634403));
#282791=CARTESIAN_POINT('Ctrl Pts',(0.897674430386662,-1.27060239093662,
9.93902942994074));
#282792=CARTESIAN_POINT('Ctrl Pts',(0.876415121155238,-1.2853583957102,
9.93713678764556));
#282793=CARTESIAN_POINT('Ctrl Pts',(0.774372103184238,-1.35247737553135,
9.92811099901745));
#282794=CARTESIAN_POINT('Ctrl Pts',(0.689221375689425,-1.39778945210965,
9.92073015488553));
#282795=CARTESIAN_POINT('Ctrl Pts',(0.514444930658023,-1.47092410606182,
9.90604592201314));
#282796=CARTESIAN_POINT('Ctrl Pts',(0.425376326242168,-1.49910952664903,
9.89878002623605));
#282797=CARTESIAN_POINT('Ctrl Pts',(0.320155797276616,-1.52226497239393,
9.89076139865152));
#282798=CARTESIAN_POINT('Ctrl Pts',(0.305955122657982,-1.52518257387742,
9.88969105442227));
#282799=CARTESIAN_POINT('Ctrl Pts',(0.284941972115323,-1.52919451663653,
9.88812666765382));
#282800=CARTESIAN_POINT('Ctrl Pts',(0.278160171186423,-1.53044265531156,
9.88762474804067));
#282801=CARTESIAN_POINT('Ctrl Pts',(0.266067371948872,-1.53258520332481,
9.88673531383142));
#282802=CARTESIAN_POINT('Ctrl Pts',(0.260759754289792,-1.53349718148213,
9.88634684936271));
#282803=CARTESIAN_POINT('Ctrl Pts',(0.24911530135477,-1.53543577569523,
9.88549881506956));
#282804=CARTESIAN_POINT('Ctrl Pts',(0.242776749469522,-1.53645075043548,
9.88503989501997));
#282805=CARTESIAN_POINT('Ctrl Pts',(0.224364657230055,-1.53928223982984,
9.88371417741561));
#282806=CARTESIAN_POINT('Ctrl Pts',(0.212275444038127,-1.54099593560062,
9.88285286803188));
#282807=CARTESIAN_POINT('Ctrl Pts',(0.118909473050545,-1.55311130366237,
9.87626247241841));
#282808=CARTESIAN_POINT('Ctrl Pts',(0.0369335631088823,-1.55721996121098,
9.87083135443084));
#282809=CARTESIAN_POINT('Ctrl Pts',(-0.163081408808733,-1.55143187887351,
9.85764352626439));
#282810=CARTESIAN_POINT('Ctrl Pts',(-0.280380362293359,-1.5345747329513,
9.84993633759345));
#282811=CARTESIAN_POINT('Ctrl Pts',(-0.413536328731252,-1.499649870811,
9.84043569419926));
#282812=CARTESIAN_POINT('Ctrl Pts',(-0.432340398125268,-1.49433722832845,
9.83907694735778));
#282813=CARTESIAN_POINT('Ctrl Pts',(-0.462673681735902,-1.48514683230853,
9.83685441804291));
#282814=CARTESIAN_POINT('Ctrl Pts',(-0.474266618038531,-1.48148547388834,
9.8359976382229));
#282815=CARTESIAN_POINT('Ctrl Pts',(-0.494914188618812,-1.47469723573101,
9.83445784658707));
#282816=CARTESIAN_POINT('Ctrl Pts',(-0.503985202632711,-1.47162186012096,
9.83377655828964));
#282817=CARTESIAN_POINT('Ctrl Pts',(-0.523206752306553,-1.46490655629693,
9.83232232789581));
#282818=CARTESIAN_POINT('Ctrl Pts',(-0.533348950617583,-1.46124447316452,
9.83154868078896));
#282819=CARTESIAN_POINT('Ctrl Pts',(-0.560722597449305,-1.4510376154008,
9.82944296332982));
#282820=CARTESIAN_POINT('Ctrl Pts',(-0.577876622449098,-1.44429171136471,
9.82810425701056));
#282821=CARTESIAN_POINT('Ctrl Pts',(-0.615675052637151,-1.42864611932829,
9.82511043111805));
#282822=CARTESIAN_POINT('Ctrl Pts',(-0.6362542261378,-1.41960063724869,
9.82345072033123));
#282823=CARTESIAN_POINT('Ctrl Pts',(-0.700991367835165,-1.38945531904745,
9.8181331384355));
#282824=CARTESIAN_POINT('Ctrl Pts',(-0.744349818166054,-1.36671778785252,
9.81442509219411));
#282825=CARTESIAN_POINT('Ctrl Pts',(-0.862133414366616,-1.29768231610186,
9.80395639880612));
#282826=CARTESIAN_POINT('Ctrl Pts',(-0.933825305300214,-1.24708571469065,
9.79710913659752));
#282827=CARTESIAN_POINT('Ctrl Pts',(-1.03849206906034,-1.15910706510403,
9.78659477604931));
#282828=CARTESIAN_POINT('Ctrl Pts',(-1.07459313835133,-1.12572004079051,
9.78285954456732));
#282829=CARTESIAN_POINT('Ctrl Pts',(-1.11660324698712,-1.08300198079821,
9.7784329799257));
#282830=CARTESIAN_POINT('Ctrl Pts',(-1.12407071720228,-1.07524933926586,
9.77764288208148));
#282831=CARTESIAN_POINT('Ctrl Pts',(-1.13565271219798,-1.06297250389569,
9.77641315521438));
#282832=CARTESIAN_POINT('Ctrl Pts',(-1.13982188411757,-1.05850068620871,
9.77596959824826));
#282833=CARTESIAN_POINT('Ctrl Pts',(-1.14765327146813,-1.0500008817041,
9.77513491876846));
#282834=CARTESIAN_POINT('Ctrl Pts',(-1.1513207249061,-1.04597823713344,
9.77474342841113));
#282835=CARTESIAN_POINT('Ctrl Pts',(-1.16000253613381,-1.03635460913824,
9.7738150371947));
#282836=CARTESIAN_POINT('Ctrl Pts',(-1.16499753073584,-1.0307363965914,
9.77327956561259));
#282837=CARTESIAN_POINT('Ctrl Pts',(-1.18124948554556,-1.01218763466873,
9.77153204968764));
#282838=CARTESIAN_POINT('Ctrl Pts',(-1.19233390553272,-0.999106638871684,
9.7703317402204));
#282839=CARTESIAN_POINT('Ctrl Pts',(-1.22918603261601,-0.954129465201075,
9.76630117487401));
#282840=CARTESIAN_POINT('Ctrl Pts',(-1.2539098806154,-0.921396726955455,
9.76352824382719));
#282841=CARTESIAN_POINT('Ctrl Pts',(-1.33408675807152,-0.806032994620876,
9.7541438788558));
#282842=CARTESIAN_POINT('Ctrl Pts',(-1.38289360906679,-0.719084850558077,
9.7477059230512));
#282843=CARTESIAN_POINT('Ctrl Pts',(-1.44730803479187,-0.573136206360701,
9.73706603456093));
#282844=CARTESIAN_POINT('Ctrl Pts',(-1.46834896484791,-0.516851690831509,
9.73300223399403));
#282845=CARTESIAN_POINT('Ctrl Pts',(-1.49108675389529,-0.443314167285405,
9.72765361427503));
#282846=CARTESIAN_POINT('Ctrl Pts',(-1.49582553401014,-0.427051625814905,
9.72646861026317));
#282847=CARTESIAN_POINT('Ctrl Pts',(-1.50306070278807,-0.400622364920187,
9.7245375812482));
#282848=CARTESIAN_POINT('Ctrl Pts',(-1.50572177123269,-0.390501848271013,
9.72379691693128));
#282849=CARTESIAN_POINT('Ctrl Pts',(-1.51064123726892,-0.370993953502119,
9.72236651387515));
#282850=CARTESIAN_POINT('Ctrl Pts',(-1.51291475001934,-0.36161085810754,
9.72167730004506));
#282851=CARTESIAN_POINT('Ctrl Pts',(-1.51723977373337,-0.343005778881625,
9.72030806124122));
#282852=CARTESIAN_POINT('Ctrl Pts',(-1.51929491002878,-0.333785057158363,
9.71962818588105));
#282853=CARTESIAN_POINT('Ctrl Pts',(-1.52385847318596,-0.312393990993489,
9.71804775800513));
#282854=CARTESIAN_POINT('Ctrl Pts',(-1.52630527757912,-0.300211317062768,
9.71714528760685));
#282855=CARTESIAN_POINT('Ctrl Pts',(-1.53425832795198,-0.257999377946727,
9.71400947844671));
#282856=CARTESIAN_POINT('Ctrl Pts',(-1.53902599631828,-0.227839945848046,
9.71175346709022));
#282857=CARTESIAN_POINT('Ctrl Pts',(-1.55135442567432,-0.131558234917276,
9.70449938697087));
#282858=CARTESIAN_POINT('Ctrl Pts',(-1.55556075073686,-0.0650894167034694,
9.69941056741366));
#282859=CARTESIAN_POINT('Ctrl Pts',(-1.55549933718348,0.00143597414997556,
9.69426865344254));
#282860=CARTESIAN_POINT('',(-1.55403083159801,-0.00119596074553188,8.29405622560371));
#282861=CARTESIAN_POINT('Ctrl Pts',(-1.55549933771838,0.00143539460917734,
9.6942686982367));
#282862=CARTESIAN_POINT('Ctrl Pts',(-1.55541261527942,0.0954142179250701,
9.6870048401175));
#282863=CARTESIAN_POINT('Ctrl Pts',(-1.54680933472033,0.189197638033392,
9.67965256375285));
#282864=CARTESIAN_POINT('Ctrl Pts',(-1.52603212362729,0.302055032806816,
9.67099562326331));
#282865=CARTESIAN_POINT('Ctrl Pts',(-1.52186445503809,0.322397221263767,
9.66944363960071));
#282866=CARTESIAN_POINT('Ctrl Pts',(-1.515606086761,0.350109855788246,9.66734610604476));
#282867=CARTESIAN_POINT('Ctrl Pts',(-1.51386663274056,0.357556353250518,
9.66678416235489));
#282868=CARTESIAN_POINT('Ctrl Pts',(-1.5104498734183,0.371711229618512,
9.66571954545384));
#282869=CARTESIAN_POINT('Ctrl Pts',(-1.50878261662827,0.378421826788227,
9.66521636292153));
#282870=CARTESIAN_POINT('Ctrl Pts',(-1.50586638380403,0.389833736125145,
9.66436353523265));
#282871=CARTESIAN_POINT('Ctrl Pts',(-1.50464003687192,0.394540580464178,
9.66401263320883));
#282872=CARTESIAN_POINT('Ctrl Pts',(-1.50178287494478,0.405299556831327,
9.66321251175281));
#282873=CARTESIAN_POINT('Ctrl Pts',(-1.50013753783908,0.41134766985951,
9.66276413143113));
#282874=CARTESIAN_POINT('Ctrl Pts',(-1.49545766258339,0.428148876994693,
9.66152204775521));
#282875=CARTESIAN_POINT('Ctrl Pts',(-1.49234368629004,0.438879735660125,
9.66073271841768));
#282876=CARTESIAN_POINT('Ctrl Pts',(-1.46960795494937,0.514186385958228,
9.65521534575491));
#282877=CARTESIAN_POINT('Ctrl Pts',(-1.44591458703667,0.577467459906825,
9.65069171557042));
#282878=CARTESIAN_POINT('Ctrl Pts',(-1.38466379563751,0.713402505763742,
9.64081856058279));
#282879=CARTESIAN_POINT('Ctrl Pts',(-1.34534631802599,0.785035170571468,
9.63550513473516));
#282880=CARTESIAN_POINT('Ctrl Pts',(-1.27806998315163,0.887582733140757,
9.62732897832204));
#282881=CARTESIAN_POINT('Ctrl Pts',(-1.25419928031693,0.921004760109985,
9.62456484454457));
#282882=CARTESIAN_POINT('Ctrl Pts',(-1.21135611861394,0.976231820141588,
9.61978282878352));
#282883=CARTESIAN_POINT('Ctrl Pts',(-1.1930469349765,0.998524432871331,
9.61778860776198));
#282884=CARTESIAN_POINT('Ctrl Pts',(-1.16685068066535,1.02867044556686,
9.61499290463235));
#282885=CARTESIAN_POINT('Ctrl Pts',(-1.15948251156927,1.03696850994968,
9.61421253971716));
#282886=CARTESIAN_POINT('Ctrl Pts',(-1.15173553693241,1.04550738413894,
9.61339790587471));
#282887=CARTESIAN_POINT('Ctrl Pts',(-1.15144458739381,1.04582780584705,
9.61336731951908));
#282888=CARTESIAN_POINT('Ctrl Pts',(-1.14454217049321,1.05342304151219,
9.61264189658121));
#282889=CARTESIAN_POINT('Ctrl Pts',(-1.13786216393447,1.06063498539061,
9.61194420402022));
#282890=CARTESIAN_POINT('Ctrl Pts',(-1.12499044511659,1.07427014027379,
9.6106077342234));
#282891=CARTESIAN_POINT('Ctrl Pts',(-1.11881093037791,1.08070436837419,
9.60996949932306));
#282892=CARTESIAN_POINT('Ctrl Pts',(-1.10260748948733,1.09728777135311,
9.60830442022423));
#282893=CARTESIAN_POINT('Ctrl Pts',(-1.0924988964974,1.10735263803247,9.60727388724269));
#282894=CARTESIAN_POINT('Ctrl Pts',(-1.05637096302315,1.14234807365739,
9.6036182849624));
#282895=CARTESIAN_POINT('Ctrl Pts',(-1.02962706589937,1.16651037057111,
9.60096098141674));
#282896=CARTESIAN_POINT('Ctrl Pts',(-0.916655297339226,1.26166351431942,
9.58992208712454));
#282897=CARTESIAN_POINT('Ctrl Pts',(-0.823750934930763,1.32419002778414,
9.58123575563827));
#282898=CARTESIAN_POINT('Ctrl Pts',(-0.669537667954223,1.40542715193257,
9.56774325129167));
#282899=CARTESIAN_POINT('Ctrl Pts',(-0.612382004872291,1.43125682270425,
9.56292653527625));
#282900=CARTESIAN_POINT('Ctrl Pts',(-0.540155656371165,1.45877547520327,
9.55717452124298));
#282901=CARTESIAN_POINT('Ctrl Pts',(-0.526419481355658,1.4637884379101,
9.55609513219524));
#282902=CARTESIAN_POINT('Ctrl Pts',(-0.506105159175053,1.4708791060606,
9.55452215219244));
#282903=CARTESIAN_POINT('Ctrl Pts',(-0.499581101063407,1.47310777104194,
9.55402048680705));
#282904=CARTESIAN_POINT('Ctrl Pts',(-0.488431256707352,1.47683404404708,
9.55316934149036));
#282905=CARTESIAN_POINT('Ctrl Pts',(-0.483813007196752,1.47835342956835,
9.55281861848711));
#282906=CARTESIAN_POINT('Ctrl Pts',(-0.47321102610221,1.48178643472266,
9.55201767192329));
#282907=CARTESIAN_POINT('Ctrl Pts',(-0.467222743311001,1.48368548729067,
9.5515682981928));
#282908=CARTESIAN_POINT('Ctrl Pts',(-0.450491604099716,1.48888005829092,
9.55032073447491));
#282909=CARTESIAN_POINT('Ctrl Pts',(-0.439724031649438,1.49209560972842,
9.54952698047757));
#282910=CARTESIAN_POINT('Ctrl Pts',(-0.356069857420918,1.51609324539627,
9.54342383579048));
#282911=CARTESIAN_POINT('Ctrl Pts',(-0.281776512864256,1.53164283609062,
9.53837347447603));
#282912=CARTESIAN_POINT('Ctrl Pts',(-0.152499314782979,1.54896986194807,
9.52976127771568));
#282913=CARTESIAN_POINT('Ctrl Pts',(-0.0980182946931811,1.55336926948925,
9.52618450954415));
#282914=CARTESIAN_POINT('Ctrl Pts',(0.00872002605207692,1.55634983009207,
9.51912048744014));
#282915=CARTESIAN_POINT('Ctrl Pts',(0.0608954394185542,1.55518228058939,
9.51564107047954));
#282916=CARTESIAN_POINT('Ctrl Pts',(0.147217570034247,1.54889974658509,
9.50975168036049));
#282917=CARTESIAN_POINT('Ctrl Pts',(0.181429699616682,1.54526580399858,
9.50738296166406));
#282918=CARTESIAN_POINT('Ctrl Pts',(0.229019439911564,1.53860876744828,
9.50402443818687));
#282919=CARTESIAN_POINT('Ctrl Pts',(0.242521725054139,1.53653832851592,
9.50306437970104));
#282920=CARTESIAN_POINT('Ctrl Pts',(0.265659963395845,1.53267773956426,
9.5014059562192));
#282921=CARTESIAN_POINT('Ctrl Pts',(0.275309645762535,1.5309738274878,9.50071035225121));
#282922=CARTESIAN_POINT('Ctrl Pts',(0.293745453317072,1.52753855706686,
9.49937348686464));
#282923=CARTESIAN_POINT('Ctrl Pts',(0.302534016375152,1.52582226927122,
9.4987327312353));
#282924=CARTESIAN_POINT('Ctrl Pts',(0.323188960730375,1.52160317257602,
9.49721843208111));
#282925=CARTESIAN_POINT('Ctrl Pts',(0.33504170523239,1.51903731336022,9.49634290748647));
#282926=CARTESIAN_POINT('Ctrl Pts',(0.376762366055451,1.50949366508533,
9.49323725354306));
#282927=CARTESIAN_POINT('Ctrl Pts',(0.406450867280551,1.50177177114491,
9.49098368268089));
#282928=CARTESIAN_POINT('Ctrl Pts',(0.548039896804091,1.4604389700368,9.48001792271427));
#282929=CARTESIAN_POINT('Ctrl Pts',(0.656128923529045,1.41517345486148,
9.47094319001451));
#282930=CARTESIAN_POINT('Ctrl Pts',(0.814419730375271,1.32682288940417,
9.45690475588576));
#282931=CARTESIAN_POINT('Ctrl Pts',(0.868724292907427,1.29192039808412,
9.45194245481959));
#282932=CARTESIAN_POINT('Ctrl Pts',(0.932648220136336,1.24497667928835,
9.44603837431956));
#282933=CARTESIAN_POINT('Ctrl Pts',(0.944461258362085,1.23603908054164,
9.44494463342849));
#282934=CARTESIAN_POINT('Ctrl Pts',(0.961611249896628,1.2226741484721,9.44335488925641));
#282935=CARTESIAN_POINT('Ctrl Pts',(0.967048730602531,1.21837803116929,
9.44285057318998));
#282936=CARTESIAN_POINT('Ctrl Pts',(0.976255024574355,1.21100373719569,
9.44199648321511));
#282937=CARTESIAN_POINT('Ctrl Pts',(0.980038329870864,1.20794403803168,
9.44164544216235));
#282938=CARTESIAN_POINT('Ctrl Pts',(0.988654201724353,1.20090893632097,
9.44084591372869));
#282939=CARTESIAN_POINT('Ctrl Pts',(0.993477207236447,1.19692207193909,
9.44039825758991));
#282940=CARTESIAN_POINT('Ctrl Pts',(1.00680875787069,1.18576564593097,9.43916017138388));
#282941=CARTESIAN_POINT('Ctrl Pts',(1.01526484605332,1.17853356043519,9.43837407030936));
#282942=CARTESIAN_POINT('Ctrl Pts',(1.0718598416443,1.12906932033044,9.43310157432554));
#282943=CARTESIAN_POINT('Ctrl Pts',(1.11743504326533,1.08398438501318,9.42879878823887));
#282944=CARTESIAN_POINT('Ctrl Pts',(1.17157330468898,1.02337314183482,9.42340912187704));
#282945=CARTESIAN_POINT('Ctrl Pts',(1.18282727300556,1.01034462086366,9.4222719093559));
#282946=CARTESIAN_POINT('Ctrl Pts',(1.2356469809701,0.947103750910749,9.41683878014942));
#282947=CARTESIAN_POINT('Ctrl Pts',(1.27424434055381,0.894499915408819,
9.41257332816262));
#282948=CARTESIAN_POINT('Ctrl Pts',(1.3324343652881,0.803750945944138,9.40539605776084));
#282949=CARTESIAN_POINT('Ctrl Pts',(1.35395523379599,0.76694310312271,9.40253056913712));
#282950=CARTESIAN_POINT('Ctrl Pts',(1.38793981918345,0.702919165803043,
9.39757570585457));
#282951=CARTESIAN_POINT('Ctrl Pts',(1.40117953690822,0.67614199760791,9.3955118659821));
#282952=CARTESIAN_POINT('Ctrl Pts',(1.41904492390152,0.637228053124277,
9.39251476415147));
#282953=CARTESIAN_POINT('Ctrl Pts',(1.42430278518711,0.625387596491295,
9.39160313656666));
#282954=CARTESIAN_POINT('Ctrl Pts',(1.43323026758176,0.604586617193399,
9.39000140176424));
#282955=CARTESIAN_POINT('Ctrl Pts',(1.43696531438743,0.595654812045977,
9.38931356106387));
#282956=CARTESIAN_POINT('Ctrl Pts',(1.44453536817917,0.577066518368343,
9.38788162286825));
#282957=CARTESIAN_POINT('Ctrl Pts',(1.44835747433914,0.567405334275767,
9.38713713054527));
#282958=CARTESIAN_POINT('Ctrl Pts',(1.45802967326584,0.542222155424631,
9.38519546708523));
#282959=CARTESIAN_POINT('Ctrl Pts',(1.46372862933815,0.526643953706327,
9.38399333097552));
#282960=CARTESIAN_POINT('Ctrl Pts',(1.48746120477969,0.458407457258115,
9.37872122848307));
#282961=CARTESIAN_POINT('Ctrl Pts',(1.50290816632667,0.404899859479817,
9.37456847200837));
#282962=CARTESIAN_POINT('Ctrl Pts',(1.53744141220164,0.255667694278585,
9.36293798832377));
#282963=CARTESIAN_POINT('Ctrl Pts',(1.55044266502748,0.158797677873854,
9.35532195431415));
#282964=CARTESIAN_POINT('Ctrl Pts',(1.55585038860724,0.0218163286373182,
9.3447405974511));
#282965=CARTESIAN_POINT('Ctrl Pts',(1.55590193998971,-0.0177752250028949,
9.34170697923197));
#282966=CARTESIAN_POINT('Ctrl Pts',(1.55384744497674,-0.0734825912149364,
9.33750617347099));
#282967=CARTESIAN_POINT('Ctrl Pts',(1.55299984398444,-0.0896275954189802,
9.33629678041485));
#282968=CARTESIAN_POINT('Ctrl Pts',(1.55105904912001,-0.118107186202107,
9.33418087119469));
#282969=CARTESIAN_POINT('Ctrl Pts',(1.55007000606673,-0.130447243253486,
9.33326985927595));
#282970=CARTESIAN_POINT('Ctrl Pts',(1.54834132435507,-0.149201361909723,
9.33189544113855));
#282971=CARTESIAN_POINT('Ctrl Pts',(1.54770893220955,-0.155624446302966,
9.33142652715709));
#282972=CARTESIAN_POINT('Ctrl Pts',(1.54647587991665,-0.167396447338708,
9.33057066296337));
#282973=CARTESIAN_POINT('Ctrl Pts',(1.54588742921287,-0.172746275550064,
9.33018308160653));
#282974=CARTESIAN_POINT('Ctrl Pts',(1.54447368052406,-0.185013026508508,
9.32929744618728));
#282975=CARTESIAN_POINT('Ctrl Pts',(1.54362967677005,-0.191927579489049,
9.3288004358046));
#282976=CARTESIAN_POINT('Ctrl Pts',(1.54088858052762,-0.213195298012295,
9.32727787986429));
#282977=CARTESIAN_POINT('Ctrl Pts',(1.53883746737255,-0.227528330313268,
9.32626040585883));
#282978=CARTESIAN_POINT('Ctrl Pts',(1.5224470930103,-0.331672115356008,
9.31891649308499));
#282979=CARTESIAN_POINT('Ctrl Pts',(1.50045367450651,-0.420113078326266,
9.31293983805421));
#282980=CARTESIAN_POINT('Ctrl Pts',(1.4387856521834,-0.599323345085008,
9.30046748363324));
#282981=CARTESIAN_POINT('Ctrl Pts',(1.39793909118043,-0.689243129115332,
9.29399088359443));
#282982=CARTESIAN_POINT('Ctrl Pts',(1.33597429279144,-0.797134128920556,
9.28544828544408));
#282983=CARTESIAN_POINT('Ctrl Pts',(1.32252670961643,-0.819251548559116,
9.28365391706747));
#282984=CARTESIAN_POINT('Ctrl Pts',(1.30190355871589,-0.851338812491502,
9.28097990413411));
#282985=CARTESIAN_POINT('Ctrl Pts',(1.2951512320459,-0.8615764160173,9.28011580559167));
#282986=CARTESIAN_POINT('Ctrl Pts',(1.28290472339639,-0.879674754913353,
9.27856794725283));
#282987=CARTESIAN_POINT('Ctrl Pts',(1.2774575060969,-0.887566626416058,
9.27788598286488));
#282988=CARTESIAN_POINT('Ctrl Pts',(1.26576693508939,-0.904173232263594,
9.2764356982702));
#282989=CARTESIAN_POINT('Ctrl Pts',(1.25950578762102,-0.912874760405781,
9.27566672020235));
#282990=CARTESIAN_POINT('Ctrl Pts',(1.24241129767076,-0.936121426890868,
9.27358734413671));
#282991=CARTESIAN_POINT('Ctrl Pts',(1.23141299239173,-0.950542555011112,
9.27227059129783));
#282992=CARTESIAN_POINT('Ctrl Pts',(1.16564130568487,-1.03372564150277,
9.26451335266591));
#282993=CARTESIAN_POINT('Ctrl Pts',(1.10537936776099,-1.09792524279161,
9.25785280434918));
#282994=CARTESIAN_POINT('Ctrl Pts',(0.976446959897203,-1.21385454430315,
9.2444769008393));
#282995=CARTESIAN_POINT('Ctrl Pts',(0.908258424841598,-1.26568497329169,
9.23779206644919));
#282996=CARTESIAN_POINT('Ctrl Pts',(0.814966809207347,-1.32515688140037,
9.22934916371899));
#282997=CARTESIAN_POINT('Ctrl Pts',(0.79345265834494,-1.33814972577921,
9.22744733510685));
#282998=CARTESIAN_POINT('Ctrl Pts',(0.756652724214756,-1.35917420491084,
9.22428024117004));
#282999=CARTESIAN_POINT('Ctrl Pts',(0.741531341786931,-1.3674827966096,
9.22300256128633));
#283000=CARTESIAN_POINT('Ctrl Pts',(0.719764963415035,-1.37897528145857,
9.22120013134219));
#283001=CARTESIAN_POINT('Ctrl Pts',(0.713231388888479,-1.38236587819077,
9.22066374335529));
#283002=CARTESIAN_POINT('Ctrl Pts',(0.701843830769808,-1.38817321798784,
9.21973720611938));
#283003=CARTESIAN_POINT('Ctrl Pts',(0.697000915441982,-1.39061115111239,
9.21934577644969));
#283004=CARTESIAN_POINT('Ctrl Pts',(0.68659683077379,-1.39578057917449,
9.21851052049622));
#283005=CARTESIAN_POINT('Ctrl Pts',(0.68103198981634,-1.39850422439332,
9.21806717096572));
#283006=CARTESIAN_POINT('Ctrl Pts',(0.665676807117687,-1.40590624536577,
9.2168527553031));
#283007=CARTESIAN_POINT('Ctrl Pts',(0.655853325281988,-1.41051565586234,
9.21608575601693));
#283008=CARTESIAN_POINT('Ctrl Pts',(0.598063277363678,-1.43689781257183,
9.21162672168504));
#283009=CARTESIAN_POINT('Ctrl Pts',(0.5490583116362,-1.4563280183136,9.20805781054925));
#283010=CARTESIAN_POINT('Ctrl Pts',(0.396758994107716,-1.50792951689121,
9.19732686657952));
#283011=CARTESIAN_POINT('Ctrl Pts',(0.291024272551362,-1.53185343434322,
9.19034589876855));
#283012=CARTESIAN_POINT('Ctrl Pts',(0.149056984662356,-1.54873388250611,
9.18075828882264));
#283013=CARTESIAN_POINT('Ctrl Pts',(0.114326432214122,-1.5516841917049,
9.1783983720849));
#283014=CARTESIAN_POINT('Ctrl Pts',(0.0537856195760443,-1.55478350810153,
9.17423568986938));
#283015=CARTESIAN_POINT('Ctrl Pts',(0.0280159601910262,-1.55546122562967,
9.17244851232786));
#283016=CARTESIAN_POINT('Ctrl Pts',(-0.0100017909861832,-1.55551603628207,
9.16978317089332));
#283017=CARTESIAN_POINT('Ctrl Pts',(-0.022245622267092,-1.5553891127206,
9.16892040417147));
#283018=CARTESIAN_POINT('Ctrl Pts',(-0.0440711660815885,-1.55490510827681,
9.16737402000975));
#283019=CARTESIAN_POINT('Ctrl Pts',(-0.0536535873069272,-1.55460395228654,
9.16669218489843));
#283020=CARTESIAN_POINT('Ctrl Pts',(-0.0739546926465336,-1.55377801209777,
9.16524121130815));
#283021=CARTESIAN_POINT('Ctrl Pts',(-0.0846719084071793,-1.55323084719081,
9.16447140655637));
#283022=CARTESIAN_POINT('Ctrl Pts',(-0.113536410014844,-1.55145755565736,
9.1623873677794));
#283023=CARTESIAN_POINT('Ctrl Pts',(-0.13166875170482,-1.55002398401965,
9.16106672949627));
#283024=CARTESIAN_POINT('Ctrl Pts',(-0.241851712891964,-1.53936551224644,
9.15296846430122));
#283025=CARTESIAN_POINT('Ctrl Pts',(-0.332937201156362,-1.52226329235696,
9.14594519050845));
#283026=CARTESIAN_POINT('Ctrl Pts',(-0.488668556344432,-1.47837354284257,
9.13344609047336));
#283027=CARTESIAN_POINT('Ctrl Pts',(-0.5540562156469,-1.4551313005362,9.1280414700007));
#283028=CARTESIAN_POINT('Ctrl Pts',(-0.647096312465075,-1.41487603998816,
9.12025453399286));
#283029=CARTESIAN_POINT('Ctrl Pts',(-0.676118226376044,-1.40123954303452,
9.11781184211173));
#283030=CARTESIAN_POINT('Ctrl Pts',(-0.723018097801362,-1.37740600453737,
9.11386277472675));
#283031=CARTESIAN_POINT('Ctrl Pts',(-0.741151409537471,-1.36773431846762,
9.11233553912384));
#283032=CARTESIAN_POINT('Ctrl Pts',(-0.765964445595221,-1.35386142911248,
9.11025040920396));
#283033=CARTESIAN_POINT('Ctrl Pts',(-0.772810942209479,-1.34996502023214,
9.10967557920964));
#283034=CARTESIAN_POINT('Ctrl Pts',(-0.784388675087898,-1.34325906928833,
9.10870475384096));
#283035=CARTESIAN_POINT('Ctrl Pts',(-0.789135081865346,-1.34047616445362,
9.10830711579856));
#283036=CARTESIAN_POINT('Ctrl Pts',(-0.798989823039099,-1.33462766408329,
9.10748240392973));
#283037=CARTESIAN_POINT('Ctrl Pts',(-0.804095444365979,-1.33155783149172,
9.10705560587412));
#283038=CARTESIAN_POINT('Ctrl Pts',(-0.817761534728267,-1.32323361792594,
9.10591412908604));
#283039=CARTESIAN_POINT('Ctrl Pts',(-0.826289140072323,-1.31792541758583,
9.10520283061206));
#283040=CARTESIAN_POINT('Ctrl Pts',(-0.866290590997002,-1.29248471153181,
9.10186789965414));
#283041=CARTESIAN_POINT('Ctrl Pts',(-0.897086646369665,-1.27130334785427,
9.09930517877944));
#283042=CARTESIAN_POINT('Ctrl Pts',(-0.995957652585755,-1.19791641071497,
9.09098695436034));
#283043=CARTESIAN_POINT('Ctrl Pts',(-1.06048172434973,-1.14119053771222,
9.08540321815311));
#283044=CARTESIAN_POINT('Ctrl Pts',(-1.18066343200416,-1.016491569491,9.07397747411122));
#283045=CARTESIAN_POINT('Ctrl Pts',(-1.23590172778775,-0.948559482264268,
9.06815035866291));
#283046=CARTESIAN_POINT('Ctrl Pts',(-1.295210552105,-0.861585414671342,
9.06084599375461));
#283047=CARTESIAN_POINT('Ctrl Pts',(-1.3050260038456,-0.84664448528441,
9.05959680300931));
#283048=CARTESIAN_POINT('Ctrl Pts',(-1.32028253861523,-0.822525380934137,
9.05758706232532));
#283049=CARTESIAN_POINT('Ctrl Pts',(-1.32589065137397,-0.813454334571488,
9.0568327215374));
#283050=CARTESIAN_POINT('Ctrl Pts',(-1.33636922023038,-0.796109117826926,
9.05539274261717));
#283051=CARTESIAN_POINT('Ctrl Pts',(-1.34125722957913,-0.787846086973782,
9.05470778836685));
#283052=CARTESIAN_POINT('Ctrl Pts',(-1.35226414062597,-0.76883990018957,
9.05313433396118));
#283053=CARTESIAN_POINT('Ctrl Pts',(-1.35833200299605,-0.758068104703732,
9.05224404494274));
#283054=CARTESIAN_POINT('Ctrl Pts',(-1.37399971066364,-0.729462286875039,
9.04988302049727));
#283055=CARTESIAN_POINT('Ctrl Pts',(-1.38338046545114,-0.711511664727011,
9.04840469478335));
#283056=CARTESIAN_POINT('Ctrl Pts',(-1.43960842240988,-0.598598379633111,
9.03912191484671));
#283057=CARTESIAN_POINT('Ctrl Pts',(-1.47699898341463,-0.499258091135512,
9.03099711720682));
#283058=CARTESIAN_POINT('Ctrl Pts',(-1.52075801335195,-0.333442806431975,
9.01769997538751));
#283059=CARTESIAN_POINT('Ctrl Pts',(-1.53347397599849,-0.268974783384797,
9.01259861280046));
#283060=CARTESIAN_POINT('Ctrl Pts',(-1.54495143942652,-0.182168902652506,
9.00594244176158));
#283061=CARTESIAN_POINT('Ctrl Pts',(-1.54736462498052,-0.160384794890064,
9.00429001532586));
#283062=CARTESIAN_POINT('Ctrl Pts',(-1.55070557308965,-0.123026660219925,
9.0014943157176));
#283063=CARTESIAN_POINT('Ctrl Pts',(-1.55186086443734,-0.107476696433552,
9.00034188241117));
#283064=CARTESIAN_POINT('Ctrl Pts',(-1.55320008487744,-0.0848514107250055,
8.99868384497252));
#283065=CARTESIAN_POINT('Ctrl Pts',(-1.5535698237821,-0.0777886458206365,
8.99816892123592));
#283066=CARTESIAN_POINT('Ctrl Pts',(-1.5541364674814,-0.0653387001870624,
8.99726619183106));
#283067=CARTESIAN_POINT('Ctrl Pts',(-1.55435355759496,-0.0599527031948444,
8.9968773084294));
#283068=CARTESIAN_POINT('Ctrl Pts',(-1.5547663019573,-0.0481938131891931,
8.99603192179196));
#283069=CARTESIAN_POINT('Ctrl Pts',(-1.55495077944821,-0.0418207447728264,
8.99557603543462));
#283070=CARTESIAN_POINT('Ctrl Pts',(-1.55536175492209,-0.0237906130767371,
8.99429231133739));
#283071=CARTESIAN_POINT('Ctrl Pts',(-1.55549639283714,-0.0121315776499224,
8.99346932872659));
#283072=CARTESIAN_POINT('Ctrl Pts',(-1.55550453399548,0.014716419385246,
8.9915883067397));
#283073=CARTESIAN_POINT('Ctrl Pts',(-1.55528669166902,0.0299044307063782,
8.99053460238978));
#283074=CARTESIAN_POINT('Ctrl Pts',(-1.55380491416704,0.0810037025495659,
8.98701709161293));
#283075=CARTESIAN_POINT('Ctrl Pts',(-1.55151917532882,0.116875672101914,
8.98459360696074));
#283076=CARTESIAN_POINT('Ctrl Pts',(-1.54151446519784,0.218338976173929,
8.97778925269326));
#283077=CARTESIAN_POINT('Ctrl Pts',(-1.53085981341632,0.283562283574093,
8.9734731750866));
#283078=CARTESIAN_POINT('Ctrl Pts',(-1.49606737764417,0.43517648713866,
8.96321704143038));
#283079=CARTESIAN_POINT('Ctrl Pts',(-1.46854858228056,0.520536306685438,
8.95725838292891));
#283080=CARTESIAN_POINT('Ctrl Pts',(-1.42676383913642,0.619886133613938,
8.94978437978776));
#283081=CARTESIAN_POINT('Ctrl Pts',(-1.41938685814121,0.636596237355085,
8.94850855838314));
#283082=CARTESIAN_POINT('Ctrl Pts',(-1.40720460203217,0.662926064889994,
8.94646614617283));
#283083=CARTESIAN_POINT('Ctrl Pts',(-1.40259072567251,0.672632890436565,
8.94570613140406));
#283084=CARTESIAN_POINT('Ctrl Pts',(-1.39367282829553,0.690903867076421,
8.94426173690647));
#283085=CARTESIAN_POINT('Ctrl Pts',(-1.38938949806302,0.699477605771842,
8.94357810410327));
#283086=CARTESIAN_POINT('Ctrl Pts',(-1.37946685483058,0.718888506099295,
8.94201670420766));
#283087=CARTESIAN_POINT('Ctrl Pts',(-1.37377861601712,0.729699791776197,
8.9411372469085));
#283088=CARTESIAN_POINT('Ctrl Pts',(-1.35576693677747,0.762976270179126,
8.93839909071579));
#283089=CARTESIAN_POINT('Ctrl Pts',(-1.34301590557419,0.785203736968609,
8.93652536815863));
#283090=CARTESIAN_POINT('Ctrl Pts',(-1.28718305678799,0.877189529036339,
8.92857596715251));
#283091=CARTESIAN_POINT('Ctrl Pts',(-1.23917598206827,0.943790674013836,
8.92232767094507));
#283092=CARTESIAN_POINT('Ctrl Pts',(-1.12256427387416,1.08124530357311,
8.9083957359416));
#283093=CARTESIAN_POINT('Ctrl Pts',(-1.05201175014948,1.15000656187652,
8.90070100471601));
#283094=CARTESIAN_POINT('Ctrl Pts',(-0.959015197773904,1.22487331626991,
8.89172853260304));
#283095=CARTESIAN_POINT('Ctrl Pts',(-0.94232358531721,1.23776054422312,
8.89015968218849));
#283096=CARTESIAN_POINT('Ctrl Pts',(-0.918792134835602,1.25517660729986,
8.88801041460191));
#283097=CARTESIAN_POINT('Ctrl Pts',(-0.912171638745465,1.25999611584328,
8.88741240935707));
#283098=CARTESIAN_POINT('Ctrl Pts',(-0.901037459372307,1.26796768389156,
8.8864182273099));
#283099=CARTESIAN_POINT('Ctrl Pts',(-0.896544614606635,1.27114842103992,
8.88602015547349));
#283100=CARTESIAN_POINT('Ctrl Pts',(-0.887256057518737,1.27765056474512,
8.8852036837903));
#283101=CARTESIAN_POINT('Ctrl Pts',(-0.882458397051673,1.28096895266434,
8.88478548329487));
#283102=CARTESIAN_POINT('Ctrl Pts',(-0.869816893373977,1.28960794519267,
8.88369242378091));
#283103=CARTESIAN_POINT('Ctrl Pts',(-0.861942739238357,1.29488408997649,
8.88302046359562));
#283104=CARTESIAN_POINT('Ctrl Pts',(-0.824966977442682,1.3191732607118,
8.87990376746175));
#283105=CARTESIAN_POINT('Ctrl Pts',(-0.795279038712062,1.33728093606542,
8.87751220863644));
#283106=CARTESIAN_POINT('Ctrl Pts',(-0.700346326529784,1.3909026278456,
8.87012317284857));
#283107=CARTESIAN_POINT('Ctrl Pts',(-0.633148845896649,1.42275059406023,
8.86525822716369));
#283108=CARTESIAN_POINT('Ctrl Pts',(-0.476154234957481,1.48382196533134,
8.85417060336886));
#283109=CARTESIAN_POINT('Ctrl Pts',(-0.385470915928925,1.50992040752033,
8.847948801096));
#283110=CARTESIAN_POINT('Ctrl Pts',(-0.272882538937654,1.53151381811522,
8.84004741826831));
#283111=CARTESIAN_POINT('Ctrl Pts',(-0.252701186237536,1.53497280068752,
8.83862510272286));
#283112=CARTESIAN_POINT('Ctrl Pts',(-0.220302834195804,1.5398694879157,
8.83632891608207));
#283113=CARTESIAN_POINT('Ctrl Pts',(-0.20812641744825,1.54156244034849,
8.83546305146916));
#283114=CARTESIAN_POINT('Ctrl Pts',(-0.186390635655043,1.54432227107116,
8.83391165581686));
#283115=CARTESIAN_POINT('Ctrl Pts',(-0.176838923979664,1.54544515702029,
8.83322792501212));
#283116=CARTESIAN_POINT('Ctrl Pts',(-0.156746666562503,1.54761847067169,
8.83178522824136));
#283117=CARTESIAN_POINT('Ctrl Pts',(-0.14620461420192,1.54864994389906,
8.83102570248735));
#283118=CARTESIAN_POINT('Ctrl Pts',(-0.118182496283963,1.55110306176721,
8.82899954667409));
#283119=CARTESIAN_POINT('Ctrl Pts',(-0.100687985346372,1.55233684921951,
8.82772711476697));
#283120=CARTESIAN_POINT('Ctrl Pts',(-0.00466047315678961,1.55747906990809,
8.82069894643226));
#283121=CARTESIAN_POINT('Ctrl Pts',(0.0740487578902953,1.55572359070942,
8.81476931788498));
#283122=CARTESIAN_POINT('Ctrl Pts',(0.204583550436572,1.54288310636638,
8.80468822127711));
#283123=CARTESIAN_POINT('Ctrl Pts',(0.256594318855368,1.53509013777173,
8.80060719742788));
#283124=CARTESIAN_POINT('Ctrl Pts',(0.378404094436337,1.51047469129441,
8.7909729954601));
#283125=CARTESIAN_POINT('Ctrl Pts',(0.447640226323751,1.491423414164,8.78543470018244));
#283126=CARTESIAN_POINT('Ctrl Pts',(0.52949269659049,1.46268361212338,8.77897439549032));
#283127=CARTESIAN_POINT('Ctrl Pts',(0.543592849415666,1.45750222070904,
8.77786493619048));
#283128=CARTESIAN_POINT('Ctrl Pts',(0.564052721661734,1.44964558148286,
8.77626225205672));
#283129=CARTESIAN_POINT('Ctrl Pts',(0.570472696030038,1.44713119400306,
8.77576039979605));
#283130=CARTESIAN_POINT('Ctrl Pts',(0.581877167836612,1.44257693487669,
8.77487103583091));
#283131=CARTESIAN_POINT('Ctrl Pts',(0.586868050399299,1.4405537637008,8.77448257489776));
#283132=CARTESIAN_POINT('Ctrl Pts',(0.59778555683228,1.43606193891327,8.77363449099096));
#283133=CARTESIAN_POINT('Ctrl Pts',(0.60370749847943,1.43358247916766,8.77317551833257));
#283134=CARTESIAN_POINT('Ctrl Pts',(0.62084999349932,1.42628001840185,8.77184948339305));
#283135=CARTESIAN_POINT('Ctrl Pts',(0.632029628093104,1.42136131189933,
8.77098791338006));
#283136=CARTESIAN_POINT('Ctrl Pts',(0.717871076729631,1.38238048649732,
8.76438855391378));
#283137=CARTESIAN_POINT('Ctrl Pts',(0.789800662666339,1.34258464573992,
8.75894963942185));
#283138=CARTESIAN_POINT('Ctrl Pts',(0.956647802313687,1.23220198194696,
8.74576498344532));
#283139=CARTESIAN_POINT('Ctrl Pts',(1.04729850226476,1.15613966665648,8.73806815100407));
#283140=CARTESIAN_POINT('Ctrl Pts',(1.14194019261586,1.05637842939796,8.72857803792099));
#283141=CARTESIAN_POINT('Ctrl Pts',(1.15513198711733,1.04193705347085,8.72721797062166));
#283142=CARTESIAN_POINT('Ctrl Pts',(1.17607983527599,1.01811807066989,8.72499371985817));
#283143=CARTESIAN_POINT('Ctrl Pts',(1.18400456144084,1.0088911577942,8.72413655752578));
#283144=CARTESIAN_POINT('Ctrl Pts',(1.19797534937191,0.992233370933975,
8.72259635260833));
#283145=CARTESIAN_POINT('Ctrl Pts',(1.20406257469083,0.984837706840746,
8.721915037366));
#283146=CARTESIAN_POINT('Ctrl Pts',(1.21685417764382,0.96900070029912,8.72046104330277));
#283147=CARTESIAN_POINT('Ctrl Pts',(1.22353985623163,0.960544978744238,
8.7196876620603));
#283148=CARTESIAN_POINT('Ctrl Pts',(1.24140791579854,0.937457075658295,
8.71758342245968));
#283149=CARTESIAN_POINT('Ctrl Pts',(1.25241888648092,0.922695107135296,
8.716245943866));
#283150=CARTESIAN_POINT('Ctrl Pts',(1.27626706213399,0.88950926273484,8.71325529647892));
#283151=CARTESIAN_POINT('Ctrl Pts',(1.28897242150136,0.870996179180301,
8.71159755147405));
#283152=CARTESIAN_POINT('Ctrl Pts',(1.32803481203978,0.811350700535255,
8.70628863026741));
#283153=CARTESIAN_POINT('Ctrl Pts',(1.35285524483083,0.769251775135271,
8.70258746150893));
#283154=CARTESIAN_POINT('Ctrl Pts',(1.40330163517241,0.673671757338233,
8.69430071706258));
#283155=CARTESIAN_POINT('Ctrl Pts',(1.42793496886137,0.619750189310015,
8.68970032265194));
#283156=CARTESIAN_POINT('Ctrl Pts',(1.47721062546711,0.49324106339723,8.67917612223003));
#283157=CARTESIAN_POINT('Ctrl Pts',(1.49969074285008,0.41996241578308,8.673270266773));
#283158=CARTESIAN_POINT('Ctrl Pts',(1.51918370425405,0.334346747659238,
8.66677445184284));
#283159=CARTESIAN_POINT('Ctrl Pts',(1.5215627676986,0.323347550540598,8.66594751241917));
#283160=CARTESIAN_POINT('Ctrl Pts',(1.52508440065415,0.306165525858772,
8.66466852824798));
#283161=CARTESIAN_POINT('Ctrl Pts',(1.52630915182963,0.300000225202333,
8.66421215452712));
#283162=CARTESIAN_POINT('Ctrl Pts',(1.5284147969853,0.289053784238507,8.66340659259172));
#283163=CARTESIAN_POINT('Ctrl Pts',(1.52931066636584,0.284275867254841,
8.6630565901419));
#283164=CARTESIAN_POINT('Ctrl Pts',(1.53142196672912,0.272716825319416,
8.66221365044807));
#283165=CARTESIAN_POINT('Ctrl Pts',(1.53261476978038,0.265931719159262,
8.66172198822169));
#283166=CARTESIAN_POINT('Ctrl Pts',(1.53619374830058,0.24474884634744,8.66019617291562));
#283167=CARTESIAN_POINT('Ctrl Pts',(1.53842249519941,0.230324763739226,
8.65917033082048));
#283168=CARTESIAN_POINT('Ctrl Pts',(1.54910786158019,0.15407427801638,8.65380621236334));
#283169=CARTESIAN_POINT('Ctrl Pts',(1.55404239431084,0.0918049495432833,
8.64962791033114));
#283170=CARTESIAN_POINT('Ctrl Pts',(1.55731521264481,-0.0813178561447185,
8.63816285679161));
#283171=CARTESIAN_POINT('Ctrl Pts',(1.54757952973813,-0.19193708977623,
8.63098668011777));
#283172=CARTESIAN_POINT('Ctrl Pts',(1.51904261045954,-0.336830157699059,
8.62096800089076));
#283173=CARTESIAN_POINT('Ctrl Pts',(1.51061538381273,-0.372808006338527,
8.61843042713718));
#283174=CARTESIAN_POINT('Ctrl Pts',(1.49713461636587,-0.422345335360386,
8.61484741450703));
#283175=CARTESIAN_POINT('Ctrl Pts',(1.4931604395783,-0.436187481484764,
8.61383643916304));
#283176=CARTESIAN_POINT('Ctrl Pts',(1.48640717639769,-0.458534588154003,
8.61218738954287));
#283177=CARTESIAN_POINT('Ctrl Pts',(1.48374583073281,-0.467074476172627,
8.61155317141504));
#283178=CARTESIAN_POINT('Ctrl Pts',(1.47801237918626,-0.484928701690103,
8.61021847385942));
#283179=CARTESIAN_POINT('Ctrl Pts',(1.47492554808371,-0.494237855922309,
8.60951753535851));
#283180=CARTESIAN_POINT('Ctrl Pts',(1.46731364088471,-0.516487018545973,
8.60782984324266));
#283181=CARTESIAN_POINT('Ctrl Pts',(1.46270520652701,-0.529397409762017,
8.60684037288728));
#283182=CARTESIAN_POINT('Ctrl Pts',(1.44582090851226,-0.574794010099215,
8.60332401463399));
#283183=CARTESIAN_POINT('Ctrl Pts',(1.43262928185464,-0.606926058466518,
8.60076709493563));
#283184=CARTESIAN_POINT('Ctrl Pts',(1.39665754883184,-0.686823306391604,
8.59423082306606));
#283185=CARTESIAN_POINT('Ctrl Pts',(1.37249630289784,-0.733915161615298,
8.59021072725486));
#283186=CARTESIAN_POINT('Ctrl Pts',(1.32463762484317,-0.816534981265038,
8.58286962174845));
#283187=CARTESIAN_POINT('Ctrl Pts',(1.30178541067507,-0.852495602410623,
8.57956835278858));
#283188=CARTESIAN_POINT('Ctrl Pts',(1.23146495878533,-0.953719605307711,
8.57000878788607));
#283189=CARTESIAN_POINT('Ctrl Pts',(1.18035465007434,-1.01629351016106,
8.56375411521788));
#283190=CARTESIAN_POINT('Ctrl Pts',(1.11418764694089,-1.08553857422275,
8.55662092402964));
#283191=CARTESIAN_POINT('Ctrl Pts',(1.10360036379093,-1.09630031961206,
8.555505855995));
#283192=CARTESIAN_POINT('Ctrl Pts',(1.08794173763039,-1.11176020212923,
8.55389665161676));
#283193=CARTESIAN_POINT('Ctrl Pts',(1.08299348962191,-1.1165809768333,8.55339379233873));
#283194=CARTESIAN_POINT('Ctrl Pts',(1.07413009094452,-1.12510168911008,
8.55250333858883));
#283195=CARTESIAN_POINT('Ctrl Pts',(1.07022763570326,-1.12881445513501,
8.55211478547125));
#283196=CARTESIAN_POINT('Ctrl Pts',(1.06163922380611,-1.13690082695788,
8.55126733643126));
#283197=CARTESIAN_POINT('Ctrl Pts',(1.05694544947106,-1.14126581155748,
8.55080908306239));
#283198=CARTESIAN_POINT('Ctrl Pts',(1.04326693419189,-1.15382940244655,
8.54948728025355));
#283199=CARTESIAN_POINT('Ctrl Pts',(1.03421259268092,-1.16195203137534,
8.54862916949874));
#283200=CARTESIAN_POINT('Ctrl Pts',(0.964554830216818,-1.22298244911397,
8.54214573279246));
#283201=CARTESIAN_POINT('Ctrl Pts',(0.90001533547242,-1.27123099095198,
8.53680769466613));
#283202=CARTESIAN_POINT('Ctrl Pts',(0.730608942529068,-1.37847659179953,
8.52358920964173));
#283203=CARTESIAN_POINT('Ctrl Pts',(0.622116615679721,-1.43071813914803,
8.51576600351762));
#283204=CARTESIAN_POINT('Ctrl Pts',(0.4904019445847,-1.47629983373049,8.50614430196203));
#283205=CARTESIAN_POINT('Ctrl Pts',(0.47198552105932,-1.48229041598798,
8.5047973810919));
#283206=CARTESIAN_POINT('Ctrl Pts',(0.441881987335005,-1.49146475968523,
8.50259032314108));
#283207=CARTESIAN_POINT('Ctrl Pts',(0.430260727185607,-1.49485869297977,
8.50173702534028));
#283208=CARTESIAN_POINT('Ctrl Pts',(0.409381385741014,-1.50069276507158,
8.50020105589772));
#283209=CARTESIAN_POINT('Ctrl Pts',(0.400138057161781,-1.50318376183369,
8.49952007370882));
#283210=CARTESIAN_POINT('Ctrl Pts',(0.380405361539547,-1.50830665201224,
8.49806387251919));
#283211=CARTESIAN_POINT('Ctrl Pts',(0.369910411189195,-1.51091477996902,
8.49728792541088));
#283212=CARTESIAN_POINT('Ctrl Pts',(0.341313139977844,-1.51770575746221,
8.49516916887761));
#283213=CARTESIAN_POINT('Ctrl Pts',(0.323162227913809,-1.52167392847343,
8.49381958215409));
#283214=CARTESIAN_POINT('Ctrl Pts',(0.282678070552662,-1.5297676314339,
8.49079752538049));
#283215=CARTESIAN_POINT('Ctrl Pts',(0.260317138806538,-1.53373100216327,
8.48912032865965));
#283216=CARTESIAN_POINT('Ctrl Pts',(0.188744108469357,-1.54480675543285,
8.48372533547588));
#283217=CARTESIAN_POINT('Ctrl Pts',(0.139278054395994,-1.55004936104529,
8.47995570720505));
#283218=CARTESIAN_POINT('Ctrl Pts',(0.0517823189612252,-1.55510050637035,
8.47323157860403));
#283219=CARTESIAN_POINT('Ctrl Pts',(0.0138485648366963,-1.5559007118011,
8.47029814223206));
#283220=CARTESIAN_POINT('Ctrl Pts',(-0.115224157113838,-1.55390275238441,
8.46029082029016));
#283221=CARTESIAN_POINT('Ctrl Pts',(-0.206080788660965,-1.54448182623148,
8.45319223883484));
#283222=CARTESIAN_POINT('Ctrl Pts',(-0.309797628089965,-1.52440641784076,
8.44533004770716));
#283223=CARTESIAN_POINT('Ctrl Pts',(-0.323961062875571,-1.52145941998455,
8.44426199951609));
#283224=CARTESIAN_POINT('Ctrl Pts',(-0.344878705185536,-1.5168017057636,
8.4426949260062));
#283225=CARTESIAN_POINT('Ctrl Pts',(-0.351665366294208,-1.51524262448,8.44218811089947));
#283226=CARTESIAN_POINT('Ctrl Pts',(-0.363678589498723,-1.51239779776459,
8.44129412821897));
#283227=CARTESIAN_POINT('Ctrl Pts',(-0.368909217540298,-1.51113044025227,
8.44090596002896));
#283228=CARTESIAN_POINT('Ctrl Pts',(-0.380399718183411,-1.50828312390999,
8.44005563658089));
#283229=CARTESIAN_POINT('Ctrl Pts',(-0.386656429714188,-1.50669132101865,
8.43959415853569));
#283230=CARTESIAN_POINT('Ctrl Pts',(-0.404889362571955,-1.50193152743612,
8.4382533341363));
#283231=CARTESIAN_POINT('Ctrl Pts',(-0.416838216721867,-1.49865927933808,
8.43737966925648));
#283232=CARTESIAN_POINT('Ctrl Pts',(-0.444301497302848,-1.49078444382009,
8.43538053052546));
#283233=CARTESIAN_POINT('Ctrl Pts',(-0.459785971089976,-1.48608175637665,
8.43425996696124));
#283234=CARTESIAN_POINT('Ctrl Pts',(-0.512934060640443,-1.46903020469825,
8.43042754499172));
#283235=CARTESIAN_POINT('Ctrl Pts',(-0.550199477749753,-1.45548345378508,
8.42776422616033));
#283236=CARTESIAN_POINT('Ctrl Pts',(-0.703801093245219,-1.39290204990904,
8.41673063309731));
#283237=CARTESIAN_POINT('Ctrl Pts',(-0.814456139149638,-1.33122990865694,
8.4086032707209));
#283238=CARTESIAN_POINT('Ctrl Pts',(-0.943100813555837,-1.23742857432828,
8.39776130236525));
#283239=CARTESIAN_POINT('Ctrl Pts',(-0.969130710557461,-1.21714995954985,
8.39548863362209));
#283240=CARTESIAN_POINT('Ctrl Pts',(-1.00510288130866,-1.18723998350902,
8.39221980125609));
#283241=CARTESIAN_POINT('Ctrl Pts',(-1.01559284587807,-1.17827913935506,
8.39125038982909));
#283242=CARTESIAN_POINT('Ctrl Pts',(-1.03327234372118,-1.16276528449421,
8.38958777881137));
#283243=CARTESIAN_POINT('Ctrl Pts',(-1.04052226450031,-1.15628208166506,
8.38889749436198));
#283244=CARTESIAN_POINT('Ctrl Pts',(-1.05475818371208,-1.14330937765328,
8.3875247958195));
#283245=CARTESIAN_POINT('Ctrl Pts',(-1.06174625884392,-1.13682278015591,
8.38684252314824));
#283246=CARTESIAN_POINT('Ctrl Pts',(-1.07893304627083,-1.12057265003051,
8.38514307297146));
#283247=CARTESIAN_POINT('Ctrl Pts',(-1.08905911230751,-1.11073390502356,
8.38412267622768));
#283248=CARTESIAN_POINT('Ctrl Pts',(-1.11070158572051,-1.08912504151811,
8.38189916245897));
#283249=CARTESIAN_POINT('Ctrl Pts',(-1.12216773352817,-1.07730724868828,
8.38069402016327));
#283250=CARTESIAN_POINT('Ctrl Pts',(-1.15438549652802,-1.04302894579015,
8.37722821191461));
#283251=CARTESIAN_POINT('Ctrl Pts',(-1.17466433624008,-1.02013662046442,
8.37494889018055));
#283252=CARTESIAN_POINT('Ctrl Pts',(-1.24688415098179,-0.933599020729825,
8.36645935863183));
#283253=CARTESIAN_POINT('Ctrl Pts',(-1.29443092338352,-0.866471641405444,
8.36010711756891));
#283254=CARTESIAN_POINT('Ctrl Pts',(-1.37745440430075,-0.727063345021788,
8.34752235414539));
#283255=CARTESIAN_POINT('Ctrl Pts',(-1.41307971193189,-0.655141225759011,
8.34131062410142));
#283256=CARTESIAN_POINT('Ctrl Pts',(-1.44860842836483,-0.566867727648813,
8.33422467849016));
#283257=CARTESIAN_POINT('Ctrl Pts',(-1.45400951060219,-0.552866879750471,
8.33311638626311));
#283258=CARTESIAN_POINT('Ctrl Pts',(-1.46162005078161,-0.532255196108869,
8.33150967241274));
#283259=CARTESIAN_POINT('Ctrl Pts',(-1.46398884688373,-0.525704696412887,
8.33100269313486));
#283260=CARTESIAN_POINT('Ctrl Pts',(-1.46810985449827,-0.514064851791627,
8.33010853495586));
#283261=CARTESIAN_POINT('Ctrl Pts',(-1.46987974930401,-0.508982064923382,
8.32972035387279));
#283262=CARTESIAN_POINT('Ctrl Pts',(-1.4737140643189,-0.497783850785474,
8.32887013746383));
#283263=CARTESIAN_POINT('Ctrl Pts',(-1.47576683918818,-0.491664668071929,
8.32840877808154));
#283264=CARTESIAN_POINT('Ctrl Pts',(-1.48164565987713,-0.47377171904175,
8.32706865587837));
#283265=CARTESIAN_POINT('Ctrl Pts',(-1.48536942503124,-0.461964500547456,
8.32619556547948));
#283266=CARTESIAN_POINT('Ctrl Pts',(-1.49363020984236,-0.434638261245243,
8.32419796099838));
#283267=CARTESIAN_POINT('Ctrl Pts',(-1.49806710552977,-0.419090224791675,
8.32307834657289));
#283268=CARTESIAN_POINT('Ctrl Pts',(-1.53749936982175,-0.27227188369062,
8.31264006489354));
#283269=CARTESIAN_POINT('Ctrl Pts',(-1.55539994923164,-0.13701189508263,
8.30398048290367));
#283270=CARTESIAN_POINT('Ctrl Pts',(-1.55549958179694,-0.00114062682748519,
8.2949012130171));
#283271=CARTESIAN_POINT('',(-1.55363820104426,0.00100737127591942,7.59405622560371));
#283272=CARTESIAN_POINT('Ctrl Pts',(-1.55363820104426,0.00100737127591942,
7.59405622560371));
#283273=CARTESIAN_POINT('Ctrl Pts',(-1.55169765832855,-0.326159426902871,
7.6174247256493));
#283274=CARTESIAN_POINT('Ctrl Pts',(-1.29071878250434,-1.17503987929593,
7.67785536563862));
#283275=CARTESIAN_POINT('Ctrl Pts',(0.103792628149562,-1.8358593744105,
7.77534814557165));
#283276=CARTESIAN_POINT('Ctrl Pts',(1.59909575810308,-0.907769413831382,
7.8865345654028));
#283277=CARTESIAN_POINT('Ctrl Pts',(1.62955779866738,0.851876712390422,
7.99772098523398));
#283278=CARTESIAN_POINT('Ctrl Pts',(0.167274199086701,1.83116681231986,
8.10890740506512));
#283279=CARTESIAN_POINT('Ctrl Pts',(-1.26795424285233,1.21093838634352,
8.20768581852172));
#283280=CARTESIAN_POINT('Ctrl Pts',(-1.55156054962447,0.343750973057136,
8.26940209203457));
#283281=CARTESIAN_POINT('Ctrl Pts',(-1.55403083159801,-0.00119596074553188,
8.29405622560371));
#283282=CARTESIAN_POINT('',(-1.5556705629256,-0.00141387709470033,6.19405610964826));
#283283=CARTESIAN_POINT('Ctrl Pts',(-1.55549961880975,0.00108898242830498,
7.59512619280739));
#283284=CARTESIAN_POINT('Ctrl Pts',(-1.55542780661911,0.103665325493169,
7.58741794628577));
#283285=CARTESIAN_POINT('Ctrl Pts',(-1.54520952791527,0.205976189459901,
7.57943937593693));
#283286=CARTESIAN_POINT('Ctrl Pts',(-1.51246140664302,0.368902331225778,
7.56657226291381));
#283287=CARTESIAN_POINT('Ctrl Pts',(-1.49610670180076,0.430458901443685,
7.56167842604611));
#283288=CARTESIAN_POINT('Ctrl Pts',(-1.4713794288958,0.504816380973698,
7.55584579531384));
#283289=CARTESIAN_POINT('Ctrl Pts',(-1.46653533119137,0.518720701921687,
7.55475876047368));
#283290=CARTESIAN_POINT('Ctrl Pts',(-1.45912752412429,0.539050004795983,
7.55317684650052));
#283291=CARTESIAN_POINT('Ctrl Pts',(-1.45671740017356,0.545529522805097,
7.55267376633303));
#283292=CARTESIAN_POINT('Ctrl Pts',(-1.45253811037044,0.556540155140894,
7.55182105128745));
#283293=CARTESIAN_POINT('Ctrl Pts',(-1.45079079298394,0.56107930264104,
7.55147016048475));
#283294=CARTESIAN_POINT('Ctrl Pts',(-1.44674270743863,0.571449984853153,
7.55066998027172));
#283295=CARTESIAN_POINT('Ctrl Pts',(-1.4444279482256,0.577275889665933,
7.55022153070611));
#283296=CARTESIAN_POINT('Ctrl Pts',(-1.43788814092584,0.59344997604703,
7.54897906854654));
#283297=CARTESIAN_POINT('Ctrl Pts',(-1.43358657884975,0.603767107235903,
7.54818943420849));
#283298=CARTESIAN_POINT('Ctrl Pts',(-1.40221127442195,0.676793233376525,
7.54261480746157));
#283299=CARTESIAN_POINT('Ctrl Pts',(-1.37114043650215,0.737714035072817,
7.53803931151013));
#283300=CARTESIAN_POINT('Ctrl Pts',(-1.33014042321069,0.806501676581322,
7.53273819161595));
#283301=CARTESIAN_POINT('Ctrl Pts',(-1.32400607848866,0.816533164272666,
7.53196163448233));
#283302=CARTESIAN_POINT('Ctrl Pts',(-1.2840071852618,0.880307214110137,
7.52699656521615));
#283303=CARTESIAN_POINT('Ctrl Pts',(-1.24699188567161,0.932001233452995,
7.52283984041793));
#283304=CARTESIAN_POINT('Ctrl Pts',(-1.17901055486721,1.01561393170506,
7.51567442521782));
#283305=CARTESIAN_POINT('Ctrl Pts',(-1.14965101778988,1.0487323892171,7.51270426331387));
#283306=CARTESIAN_POINT('Ctrl Pts',(-1.10429504329741,1.09569888510223,
7.50824485195407));
#283307=CARTESIAN_POINT('Ctrl Pts',(-1.08936298922978,1.11054572128396,
7.50679579191809));
#283308=CARTESIAN_POINT('Ctrl Pts',(-1.06170337504077,1.13695276572884,
7.50414091654037));
#283309=CARTESIAN_POINT('Ctrl Pts',(-1.04907660598111,1.14861389596835,
7.50293950593924));
#283310=CARTESIAN_POINT('Ctrl Pts',(-1.02858858986014,1.16691540520328,
7.50100494337827));
#283311=CARTESIAN_POINT('Ctrl Pts',(-1.02084993508036,1.17369137807727,
7.50027750620568));
#283312=CARTESIAN_POINT('Ctrl Pts',(-1.00577755353014,1.18662693197917,
7.49886658949772));
#283313=CARTESIAN_POINT('Ctrl Pts',(-0.998453004049991,1.1927965266716,
7.49818356661102));
#283314=CARTESIAN_POINT('Ctrl Pts',(-0.98171257868298,1.20663504250872,
7.49662810083029));
#283315=CARTESIAN_POINT('Ctrl Pts',(-0.9722630299579,1.21426203843341,7.49575401658594));
#283316=CARTESIAN_POINT('Ctrl Pts',(-0.947415397686373,1.23384125658758,
7.49346519417263));
#283317=CARTESIAN_POINT('Ctrl Pts',(-0.931880672670947,1.2456157233225,
7.49204359639878));
#283318=CARTESIAN_POINT('Ctrl Pts',(-0.820552203385979,1.32674826492543,
7.48191703889393));
#283319=CARTESIAN_POINT('Ctrl Pts',(-0.717360641847691,1.38526170717769,
7.47280087582587));
#283320=CARTESIAN_POINT('Ctrl Pts',(-0.533179306843392,1.46356068592827,
7.45727937821555));
#283321=CARTESIAN_POINT('Ctrl Pts',(-0.455372753775986,1.48960689909923,
7.45093753735175));
#283322=CARTESIAN_POINT('Ctrl Pts',(-0.364022500675698,1.51235475667921,
7.44396181248399));
#283323=CARTESIAN_POINT('Ctrl Pts',(-0.352141223466405,1.51516529609271,
7.44306357367889));
#283324=CARTESIAN_POINT('Ctrl Pts',(-0.333964152894782,1.51923974294616,
7.44170436112457));
#283325=CARTESIAN_POINT('Ctrl Pts',(-0.327691919193283,1.52060496580366,
7.44123805692041));
#283326=CARTESIAN_POINT('Ctrl Pts',(-0.3161419906398,1.52304415409516,7.44038458448527));
#283327=CARTESIAN_POINT('Ctrl Pts',(-0.310867089505607,1.52412955745471,
7.43999681140119));
#283328=CARTESIAN_POINT('Ctrl Pts',(-0.298824969107618,1.5265423151354,
7.43911605114716));
#283329=CARTESIAN_POINT('Ctrl Pts',(-0.292054444104584,1.5278520898811,
7.43862405401858));
#283330=CARTESIAN_POINT('Ctrl Pts',(-0.271023807224473,1.53177560987122,
7.43710508095525));
#283331=CARTESIAN_POINT('Ctrl Pts',(-0.256735206446268,1.5342351502917,
7.43608625225311));
#283332=CARTESIAN_POINT('Ctrl Pts',(-0.150356548579933,1.55101857196858,
7.42858457496211));
#283333=CARTESIAN_POINT('Ctrl Pts',(-0.0571667347852686,1.55724199358747,
7.42246920867134));
#283334=CARTESIAN_POINT('Ctrl Pts',(0.132284669755296,1.55285248151857,
7.4099989402936));
#283335=CARTESIAN_POINT('Ctrl Pts',(0.228112995513905,1.54169120066067,
7.4036639615049));
#283336=CARTESIAN_POINT('Ctrl Pts',(0.347604070680503,1.51638426194872,
7.39527767871498));
#283337=CARTESIAN_POINT('Ctrl Pts',(0.372779537857112,1.51039236725372,
7.3934837170917));
#283338=CARTESIAN_POINT('Ctrl Pts',(0.409647561381616,1.50063969642914,
7.39081019446447));
#283339=CARTESIAN_POINT('Ctrl Pts',(0.421464655097816,1.49736373410331,
7.38994617103066));
#283340=CARTESIAN_POINT('Ctrl Pts',(0.442451176120609,1.49127769320319,
7.38839839572937));
#283341=CARTESIAN_POINT('Ctrl Pts',(0.451635778851122,1.48852185648178,
7.38771643853079));
#283342=CARTESIAN_POINT('Ctrl Pts',(0.471033542818532,1.48250550858444,
7.38626611485995));
#283343=CARTESIAN_POINT('Ctrl Pts',(0.481239606246189,1.47922398985099,
7.38549709005231));
#283344=CARTESIAN_POINT('Ctrl Pts',(0.508620539673677,1.47010693907525,
7.3834174510128));
#283345=CARTESIAN_POINT('Ctrl Pts',(0.525728118581261,1.46407621360948,
7.38210047916107));
#283346=CARTESIAN_POINT('Ctrl Pts',(0.631405474406174,1.42473209069745,
7.37385165039303));
#283347=CARTESIAN_POINT('Ctrl Pts',(0.716871104826995,1.38369943643787,
7.366661701593));
#283348=CARTESIAN_POINT('Ctrl Pts',(0.8632503348941,1.29620451306948,7.35348057692364));
#283349=CARTESIAN_POINT('Ctrl Pts',(0.925494281651514,1.2525206614627,7.34755482009907));
#283350=CARTESIAN_POINT('Ctrl Pts',(1.01512422278765,1.17927426297062,7.33870564676653));
#283351=CARTESIAN_POINT('Ctrl Pts',(1.04497389381006,1.15290726741355,7.33569966005672));
#283352=CARTESIAN_POINT('Ctrl Pts',(1.08092595453072,1.11860486232567,7.3320356796895));
#283353=CARTESIAN_POINT('Ctrl Pts',(1.08800549624715,1.11172020348813,7.33131198262281));
#283354=CARTESIAN_POINT('Ctrl Pts',(1.09922393860948,1.10060075921631,7.33016232940926));
#283355=CARTESIAN_POINT('Ctrl Pts',(1.10340490984098,1.09640909632196,7.32973321926855));
#283356=CARTESIAN_POINT('Ctrl Pts',(1.11139347168942,1.08830812658672,7.32891224795363));
#283357=CARTESIAN_POINT('Ctrl Pts',(1.11520454813528,1.08440252870062,7.32852013223706));
#283358=CARTESIAN_POINT('Ctrl Pts',(1.12363257166192,1.07567405280914,7.32765175921664));
#283359=CARTESIAN_POINT('Ctrl Pts',(1.12823923854861,1.07084128090667,7.32717628043901));
#283360=CARTESIAN_POINT('Ctrl Pts',(1.14179439001396,1.05643623416878,7.32577413313436));
#283361=CARTESIAN_POINT('Ctrl Pts',(1.15065346680217,1.04678009835152,7.32485375923614));
#283362=CARTESIAN_POINT('Ctrl Pts',(1.22249597162214,0.966459515250616,
7.31734510667948));
#283363=CARTESIAN_POINT('Ctrl Pts',(1.27903969228235,0.890282555878519,
7.31113884868504));
#283364=CARTESIAN_POINT('Ctrl Pts',(1.38411449234752,0.717849407659683,
7.2978511130844));
#283365=CARTESIAN_POINT('Ctrl Pts',(1.43029137041731,0.620760130953684,
7.29078630242934));
#283366=CARTESIAN_POINT('Ctrl Pts',(1.47230343403155,0.50224097300336,7.28206979952459));
#283367=CARTESIAN_POINT('Ctrl Pts',(1.47817985169342,0.484672747331978,
7.28077627370905));
#283368=CARTESIAN_POINT('Ctrl Pts',(1.48698415086335,0.456700208026272,
7.27871214211918));
#283369=CARTESIAN_POINT('Ctrl Pts',(1.49011987125119,0.446362748921551,
7.27794836117902));
#283370=CARTESIAN_POINT('Ctrl Pts',(1.49583135898371,0.426802617191487,
7.2765009167782));
#283371=CARTESIAN_POINT('Ctrl Pts',(1.49843014412627,0.417587145625668,
7.27581804135102));
#283372=CARTESIAN_POINT('Ctrl Pts',(1.50412673333248,0.396648510546313,
7.27426405430882));
#283373=CARTESIAN_POINT('Ctrl Pts',(1.50717283608429,0.384912064675614,
7.27339131355366));
#283374=CARTESIAN_POINT('Ctrl Pts',(1.51474212945034,0.354279587782037,
7.271108440597));
#283375=CARTESIAN_POINT('Ctrl Pts',(1.51904890519262,0.335332827720239,
7.26969150745333));
#283376=CARTESIAN_POINT('Ctrl Pts',(1.54727603364526,0.199422653324257,
7.25948831497441));
#283377=CARTESIAN_POINT('Ctrl Pts',(1.5580108230103,0.0801494003488005,
7.25028201781071));
#283378=CARTESIAN_POINT('Ctrl Pts',(1.55296950585114,-0.120087058336532,
7.23474828840498));
#283379=CARTESIAN_POINT('Ctrl Pts',(1.54461557454576,-0.200750759176452,
7.22848303382517));
#283380=CARTESIAN_POINT('Ctrl Pts',(1.52782197636782,-0.292384309470848,
7.22158033598628));
#283381=CARTESIAN_POINT('Ctrl Pts',(1.52548581686377,-0.304338007774974,
7.22068429466812));
#283382=CARTESIAN_POINT('Ctrl Pts',(1.52170554939745,-0.322542392923269,
7.21932770010624));
#283383=CARTESIAN_POINT('Ctrl Pts',(1.52036284955179,-0.32881329650326,
7.21886184666224));
#283384=CARTESIAN_POINT('Ctrl Pts',(1.51782112865239,-0.340335542934345,
7.21800878334559));
#283385=CARTESIAN_POINT('Ctrl Pts',(1.51663359999054,-0.345589041214388,
7.21762097317581));
#283386=CARTESIAN_POINT('Ctrl Pts',(1.513861641275,-0.357562361606684,7.21673961826425));
#283387=CARTESIAN_POINT('Ctrl Pts',(1.51225973715551,-0.36427792078236,
7.21624706901489));
#283388=CARTESIAN_POINT('Ctrl Pts',(1.5070187416916,-0.385618849268429,
7.21468685239591));
#283389=CARTESIAN_POINT('Ctrl Pts',(1.5032116533644,-0.400202641381201,
7.2136281750354));
#283390=CARTESIAN_POINT('Ctrl Pts',(1.47779406465255,-0.492083907991147,
7.20699246044574));
#283391=CARTESIAN_POINT('Ctrl Pts',(1.45043725432645,-0.56767691119827,
7.20168335473523));
#283392=CARTESIAN_POINT('Ctrl Pts',(1.39962252184265,-0.680067241926809,
7.19355825593305));
#283393=CARTESIAN_POINT('Ctrl Pts',(1.38025997076975,-0.718552032129711,
7.19073193657411));
#283394=CARTESIAN_POINT('Ctrl Pts',(1.33362123638254,-0.802390469271581,
7.18438754704369));
#283395=CARTESIAN_POINT('Ctrl Pts',(1.30557913243906,-0.847253519688105,
7.1808622675486));
#283396=CARTESIAN_POINT('Ctrl Pts',(1.25543157955849,-0.919063161975205,
7.17490420635523));
#283397=CARTESIAN_POINT('Ctrl Pts',(1.23460822404052,-0.946851506323747,
7.17251401840584));
#283398=CARTESIAN_POINT('Ctrl Pts',(1.20429209114094,-0.984605850325622,
7.16913019528557));
#283399=CARTESIAN_POINT('Ctrl Pts',(1.19556956901294,-0.995179132476199,
7.16816692762145));
#283400=CARTESIAN_POINT('Ctrl Pts',(1.18036823535781,-1.01311759564374,
7.16650470405919));
#283401=CARTESIAN_POINT('Ctrl Pts',(1.17395728540315,-1.02053942484809,
7.16580854263229));
#283402=CARTESIAN_POINT('Ctrl Pts',(1.16156553857085,-1.03461382519181,
7.16447181138535));
#283403=CARTESIAN_POINT('Ctrl Pts',(1.15559667643018,-1.0412764200319,7.16383175732513));
#283404=CARTESIAN_POINT('Ctrl Pts',(1.13986816810754,-1.05853117478588,
7.16215477068272));
#283405=CARTESIAN_POINT('Ctrl Pts',(1.13001849057908,-1.06903969694249,
7.16111404404092));
#283406=CARTESIAN_POINT('Ctrl Pts',(1.09438122711372,-1.10601788561597,
7.15738061368865));
#283407=CARTESIAN_POINT('Ctrl Pts',(1.06779996547506,-1.13170165850278,
7.15465382946555));
#283408=CARTESIAN_POINT('Ctrl Pts',(0.958004442774669,-1.23047584605486,
7.14360667184893));
#283409=CARTESIAN_POINT('Ctrl Pts',(0.868013087295815,-1.295526901914,7.13499161029401));
#283410=CARTESIAN_POINT('Ctrl Pts',(0.717724395757608,-1.38142875619461,
7.12159252315129));
#283411=CARTESIAN_POINT('Ctrl Pts',(0.661731550788853,-1.40910847796491,
7.11679646779261));
#283412=CARTESIAN_POINT('Ctrl Pts',(0.590774283035635,-1.43902014062864,
7.11106607368267));
#283413=CARTESIAN_POINT('Ctrl Pts',(0.57724705142175,-1.44449960234825,
7.10998874856418));
#283414=CARTESIAN_POINT('Ctrl Pts',(0.557223405980756,-1.45228433228898,
7.10841818067837));
#283415=CARTESIAN_POINT('Ctrl Pts',(0.55078606444337,-1.45473792211662,
7.10791689753226));
#283416=CARTESIAN_POINT('Ctrl Pts',(0.539778674204684,-1.45884984276915,
7.10706617531228));
#283417=CARTESIAN_POINT('Ctrl Pts',(0.535216897708497,-1.46052961480979,
7.1067154966414));
#283418=CARTESIAN_POINT('Ctrl Pts',(0.524738559739492,-1.46433234032395,
7.10591433888086));
#283419=CARTESIAN_POINT('Ctrl Pts',(0.518816923776662,-1.46644084855689,
7.10546471234536));
#283420=CARTESIAN_POINT('Ctrl Pts',(0.502258810971588,-1.47222381688967,
7.10421575038247));
#283421=CARTESIAN_POINT('Ctrl Pts',(0.491594735579027,-1.47581893045395,
7.10342086684222));
#283422=CARTESIAN_POINT('Ctrl Pts',(0.40815602703161,-1.5029432954468,7.09726825633693));
#283423=CARTESIAN_POINT('Ctrl Pts',(0.333763929481463,-1.52119522521214,
7.09217432498568));
#283424=CARTESIAN_POINT('Ctrl Pts',(0.199978159481106,-1.54372582978643,
7.0832182231992));
#283425=CARTESIAN_POINT('Ctrl Pts',(0.141122576585364,-1.5502145244609,
7.0793462469842));
#283426=CARTESIAN_POINT('Ctrl Pts',(0.0331888256996731,-1.55591513787441,
7.07218256896104));
#283427=CARTESIAN_POINT('Ctrl Pts',(-0.0157541790486523,-1.55618914267095,
7.0689109721127));
#283428=CARTESIAN_POINT('Ctrl Pts',(-0.087079990629827,-1.55322322138593,
7.06404632122905));
#283429=CARTESIAN_POINT('Ctrl Pts',(-0.109510074288738,-1.55180306816909,
7.06250268124975));
#283430=CARTESIAN_POINT('Ctrl Pts',(-0.150263484479658,-1.54833483817215,
7.05966709063586));
#283431=CARTESIAN_POINT('Ctrl Pts',(-0.168596386309016,-1.54644595582078,
7.05838006082208));
#283432=CARTESIAN_POINT('Ctrl Pts',(-0.197595010881135,-1.54293639571688,
7.05632389811799));
#283433=CARTESIAN_POINT('Ctrl Pts',(-0.208285265924456,-1.54152967762595,
7.05556149831916));
#283434=CARTESIAN_POINT('Ctrl Pts',(-0.228442570044301,-1.53866370043912,
7.0541151827505));
#283435=CARTESIAN_POINT('Ctrl Pts',(-0.23791249022597,-1.53722790447646,
7.0534320400018));
#283436=CARTESIAN_POINT('Ctrl Pts',(-0.259371688826184,-1.5337712982661,
7.05187538565419));
#283437=CARTESIAN_POINT('Ctrl Pts',(-0.271351614735281,-1.53169721352572,
7.05100022290151));
#283438=CARTESIAN_POINT('Ctrl Pts',(-0.302520998521914,-1.52592371758541,
7.04870662050459));
#283439=CARTESIAN_POINT('Ctrl Pts',(-0.321666678644395,-1.52200283503349,
7.04728127395428));
#283440=CARTESIAN_POINT('Ctrl Pts',(-0.456027776501773,-1.49183842022342,
7.03715763558868));
#283441=CARTESIAN_POINT('Ctrl Pts',(-0.567976871852699,-1.45290568242781,
7.02804907891619));
#283442=CARTESIAN_POINT('Ctrl Pts',(-0.74823727744731,-1.36617426775708,
7.01253481434022));
#283443=CARTESIAN_POINT('Ctrl Pts',(-0.819144449963565,-1.32487604242039,
7.00619243317581));
#283444=CARTESIAN_POINT('Ctrl Pts',(-0.896506468557956,-1.27122202934174,
6.99921619344167));
#283445=CARTESIAN_POINT('Ctrl Pts',(-0.906456506120105,-1.26414632193565,
6.99831793928616));
#283446=CARTESIAN_POINT('Ctrl Pts',(-0.921509546417327,-1.25317261714819,
6.99695870844605));
#283447=CARTESIAN_POINT('Ctrl Pts',(-0.926673155743826,-1.24935916329039,
6.99649240109493));
#283448=CARTESIAN_POINT('Ctrl Pts',(-0.936125383095813,-1.24228761591108,
6.99563892579928));
#283449=CARTESIAN_POINT('Ctrl Pts',(-0.940420754945389,-1.23903916760772,
6.99525115296988));
#283450=CARTESIAN_POINT('Ctrl Pts',(-0.950177717820672,-1.23158032862593,
6.99437039684898));
#283451=CARTESIAN_POINT('Ctrl Pts',(-0.955628277676672,-1.22735585753269,
6.9938784035609));
#283452=CARTESIAN_POINT('Ctrl Pts',(-0.972866559172804,-1.21381082612887,
6.99232182112495));
#283453=CARTESIAN_POINT('Ctrl Pts',(-0.984547834386843,-1.20435529196761,
6.99126616318878));
#283454=CARTESIAN_POINT('Ctrl Pts',(-1.05137410780147,-1.14863981421436,
6.98520954450355));
#283455=CARTESIAN_POINT('Ctrl Pts',(-1.10339892469848,-1.09876038533345,
6.98042240366214));
#283456=CARTESIAN_POINT('Ctrl Pts',(-1.18910481683623,-1.00433706512575,
6.97200740413813));
#283457=CARTESIAN_POINT('Ctrl Pts',(-1.22419430813036,-0.96125514872669,
6.96837133426241));
#283458=CARTESIAN_POINT('Ctrl Pts',(-1.3014736129476,-0.855260106560734,
6.95968454271046));
#283459=CARTESIAN_POINT('Ctrl Pts',(-1.34151771764476,-0.790968612270013,
6.95460719821386));
#283460=CARTESIAN_POINT('Ctrl Pts',(-1.38482145531778,-0.708627165604342,
6.94814717705057));
#283461=CARTESIAN_POINT('Ctrl Pts',(-1.39266012375441,-0.693094986441829,
6.94693073397555));
#283462=CARTESIAN_POINT('Ctrl Pts',(-1.40483643939723,-0.667926938325157,
6.94496116228049));
#283463=CARTESIAN_POINT('Ctrl Pts',(-1.40933943749676,-0.658372353898031,
6.94421380365013));
#283464=CARTESIAN_POINT('Ctrl Pts',(-1.41775922882767,-0.640024738036972,
6.94277892189431));
#283465=CARTESIAN_POINT('Ctrl Pts',(-1.42169240509211,-0.631239727724532,
6.94209200289787));
#283466=CARTESIAN_POINT('Ctrl Pts',(-1.43048613728893,-0.611099194584432,
6.94051712659765));
#283467=CARTESIAN_POINT('Ctrl Pts',(-1.43529341588493,-0.599721275714149,
6.93962740334839));
#283468=CARTESIAN_POINT('Ctrl Pts',(-1.44778640637924,-0.569141907463111,
6.9372354819311));
#283469=CARTESIAN_POINT('Ctrl Pts',(-1.45522526810372,-0.549843006834763,
6.93572516617908));
#283470=CARTESIAN_POINT('Ctrl Pts',(-1.50993290878756,-0.39901842398349,
6.92391095591791));
#283471=CARTESIAN_POINT('Ctrl Pts',(-1.5396562697137,-0.261831358016168,
6.91301637011997));
#283472=CARTESIAN_POINT('Ctrl Pts',(-1.55390189278899,-0.0815961280935081,
6.89905084382698));
#283473=CARTESIAN_POINT('Ctrl Pts',(-1.5555153741194,-0.0405141409409373,
6.89589732999719));
#283474=CARTESIAN_POINT('Ctrl Pts',(-1.5554908803994,0.0244996029640861,
6.890994716635));
#283475=CARTESIAN_POINT('Ctrl Pts',(-1.55493041534923,0.0484114879992756,
6.88921047374986));
#283476=CARTESIAN_POINT('Ctrl Pts',(-1.55341906944806,0.0808910828078689,
6.88682065947192));
#283477=CARTESIAN_POINT('Ctrl Pts',(-1.55294821286529,0.0894764207277253,
6.88619217271994));
#283478=CARTESIAN_POINT('Ctrl Pts',(-1.55208573486681,0.103130794934568,
6.88519817977613));
#283479=CARTESIAN_POINT('Ctrl Pts',(-1.55174041928355,0.1082024141101,6.8848302071354));
#283480=CARTESIAN_POINT('Ctrl Pts',(-1.55096220078562,0.118860840851329,
6.88405958326944));
#283481=CARTESIAN_POINT('Ctrl Pts',(-1.55052396086327,0.124447162873384,
6.88365725459886));
#283482=CARTESIAN_POINT('Ctrl Pts',(-1.54935271741437,0.138409150918347,
6.88265537106138));
#283483=CARTESIAN_POINT('Ctrl Pts',(-1.54858196287555,0.146781636239823,
6.88205787651543));
#283484=CARTESIAN_POINT('Ctrl Pts',(-1.54530324996145,0.179489860371456,
6.87973512480338));
#283485=CARTESIAN_POINT('Ctrl Pts',(-1.54228906330299,0.203772816170861,
6.87803546865865));
#283486=CARTESIAN_POINT('Ctrl Pts',(-1.53263884390513,0.268906015058068,
6.87351875437365));
#283487=CARTESIAN_POINT('Ctrl Pts',(-1.52494347479319,0.309580641335146,
6.87074292738709));
#283488=CARTESIAN_POINT('Ctrl Pts',(-1.48361876100428,0.488582298952724,
6.85853843361351));
#283489=CARTESIAN_POINT('Ctrl Pts',(-1.43272581148776,0.622199651486687,
6.84938874875793));
#283490=CARTESIAN_POINT('Ctrl Pts',(-1.3552318240445,0.76373388184176,6.83824423828892));
#283491=CARTESIAN_POINT('Ctrl Pts',(-1.34578273488005,0.780263747382687,
6.83691951175804));
#283492=CARTESIAN_POINT('Ctrl Pts',(-1.32988166621093,0.80693201361782,
6.8347415024283));
#283493=CARTESIAN_POINT('Ctrl Pts',(-1.32361122482553,0.817176744528968,
6.83389475678209));
#283494=CARTESIAN_POINT('Ctrl Pts',(-1.31213576360208,0.83544686575863,
6.83236591795519));
#283495=CARTESIAN_POINT('Ctrl Pts',(-1.30697411724587,0.843498889742677,
6.83168545001259));
#283496=CARTESIAN_POINT('Ctrl Pts',(-1.29578518121467,0.860604028102614,
6.8302252602346));
#283497=CARTESIAN_POINT('Ctrl Pts',(-1.28973657178683,0.869642508902566,
6.82944476522294));
#283498=CARTESIAN_POINT('Ctrl Pts',(-1.27293562726561,0.894187445005131,
6.82730022024248));
#283499=CARTESIAN_POINT('Ctrl Pts',(-1.26199544649055,0.909562385305535,
6.82592911009729));
#283500=CARTESIAN_POINT('Ctrl Pts',(-1.18882132839201,1.00853640372578,
6.81691541667426));
#283501=CARTESIAN_POINT('Ctrl Pts',(-1.11861068834515,1.08588401662907,
6.80895641393999));
#283502=CARTESIAN_POINT('Ctrl Pts',(-0.968808019565662,1.22085596487664,
6.79333606604023));
#283503=CARTESIAN_POINT('Ctrl Pts',(-0.890427777509494,1.2791481036406,
6.78572857171517));
#283504=CARTESIAN_POINT('Ctrl Pts',(-0.794910671248913,1.33712401923343,
6.77741828086715));
#283505=CARTESIAN_POINT('Ctrl Pts',(-0.782618083607044,1.34435582776144,
6.77636597832437));
#283506=CARTESIAN_POINT('Ctrl Pts',(-0.764296813570521,1.35479785375723,
6.77482470319823));
#283507=CARTESIAN_POINT('Ctrl Pts',(-0.758344083417931,1.35813883665999,
6.77432809777702));
#283508=CARTESIAN_POINT('Ctrl Pts',(-0.747665093598823,1.36404033919229,
6.77344488470922));
#283509=CARTESIAN_POINT('Ctrl Pts',(-0.742947359823282,1.36661566010162,
6.77305737425188));
#283510=CARTESIAN_POINT('Ctrl Pts',(-0.732434203477966,1.37228405831541,
6.77219975293653));
#283511=CARTESIAN_POINT('Ctrl Pts',(-0.726632450264999,1.37536492814084,
6.77173040258224));
#283512=CARTESIAN_POINT('Ctrl Pts',(-0.709339975063412,1.38440767944788,
6.7703425916911));
#283513=CARTESIAN_POINT('Ctrl Pts',(-0.697793807767877,1.39026315990409,
6.76943043409407));
#283514=CARTESIAN_POINT('Ctrl Pts',(-0.67079679777614,1.40353323738401,
6.76732791476882));
#283515=CARTESIAN_POINT('Ctrl Pts',(-0.655293609920436,1.41083813118765,
6.76614320903078));
#283516=CARTESIAN_POINT('Ctrl Pts',(-0.600128098628353,1.43572578067155,
6.76199600262839));
#283517=CARTESIAN_POINT('Ctrl Pts',(-0.559851967281369,1.45190515795145,
6.75909098443087));
#283518=CARTESIAN_POINT('Ctrl Pts',(-0.459811327718358,1.48730935270688,
6.7520510288142));
#283519=CARTESIAN_POINT('Ctrl Pts',(-0.399460777930149,1.50464178253863,
6.74795033485527));
#283520=CARTESIAN_POINT('Ctrl Pts',(-0.258176101446387,1.536115762935,6.73838788083788));
#283521=CARTESIAN_POINT('Ctrl Pts',(-0.176850055963499,1.54758776911403,
6.73290588831504));
#283522=CARTESIAN_POINT('Ctrl Pts',(-0.0770456228605368,1.55369494782263,
6.72596912398444));
#283523=CARTESIAN_POINT('Ctrl Pts',(-0.0590686002445035,1.55448218793097,
6.72471188841707));
#283524=CARTESIAN_POINT('Ctrl Pts',(-0.0303966425756174,1.55523971253574,
6.72269227812918));
#283525=CARTESIAN_POINT('Ctrl Pts',(-0.0197083093384715,1.5554118720076,
6.72193622246404));
#283526=CARTESIAN_POINT('Ctrl Pts',(0.000575805544540651,1.55552948777742,
6.72049493303484));
#283527=CARTESIAN_POINT('Ctrl Pts',(0.0101710045791695,1.55549633942618,
6.71981040235859));
#283528=CARTESIAN_POINT('Ctrl Pts',(0.0320815764149997,1.55521790847319,
6.71824071036492));
#283529=CARTESIAN_POINT('Ctrl Pts',(0.0443954310005491,1.55491511017653,
6.71735379090366));
#283530=CARTESIAN_POINT('Ctrl Pts',(0.0828643422337133,1.55351183496251,
6.71456748617977));
#283531=CARTESIAN_POINT('Ctrl Pts',(0.10899478988918,1.55189738783223,6.71265230357558));
#283532=CARTESIAN_POINT('Ctrl Pts',(0.231503063865512,1.54121914133226,
6.70356164677921));
#283533=CARTESIAN_POINT('Ctrl Pts',(0.32692475806529,1.52383217751525,6.6961362696206));
#283534=CARTESIAN_POINT('Ctrl Pts',(0.508943473883406,1.47277681960009,
6.6814827391431));
#283535=CARTESIAN_POINT('Ctrl Pts',(0.595404065838802,1.43999725000418,
6.67429388807202));
#283536=CARTESIAN_POINT('Ctrl Pts',(0.691474943974453,1.39343173770253,
6.66634834023519));
#283537=CARTESIAN_POINT('Ctrl Pts',(0.704407173364741,1.38693914059612,
6.66528000946877));
#283538=CARTESIAN_POINT('Ctrl Pts',(0.723426933632015,1.37705563357825,
6.66371260251421));
#283539=CARTESIAN_POINT('Ctrl Pts',(0.729584872655285,1.37380299346813,
6.66320573197652));
#283540=CARTESIAN_POINT('Ctrl Pts',(0.740462830659614,1.36796345422184,
6.66231169004866));
#283541=CARTESIAN_POINT('Ctrl Pts',(0.745191513135505,1.36539328675944,
6.66192351751357));
#283542=CARTESIAN_POINT('Ctrl Pts',(0.755562535113961,1.35968642545512,
6.661073230242));
#283543=CARTESIAN_POINT('Ctrl Pts',(0.761198777076861,1.35653910589301,
6.66061179228958));
#283544=CARTESIAN_POINT('Ctrl Pts',(0.777590961902547,1.34725125178266,
6.65927120516224));
#283545=CARTESIAN_POINT('Ctrl Pts',(0.78829367093438,1.34101705926748,6.65839773440212));
#283546=CARTESIAN_POINT('Ctrl Pts',(0.812800896700026,1.32634709877763,
6.65639911412947));
#283547=CARTESIAN_POINT('Ctrl Pts',(0.826550764169178,1.31782237260232,
6.65527887131028));
#283548=CARTESIAN_POINT('Ctrl Pts',(0.873505630584418,1.28768690303119,
6.65144799128946));
#283549=CARTESIAN_POINT('Ctrl Pts',(0.906018412731336,1.26502203098795,
6.64878585163898));
#283550=CARTESIAN_POINT('Ctrl Pts',(1.01541097895417,1.18238017439628,6.63966539926443));
#283551=CARTESIAN_POINT('Ctrl Pts',(1.08749347891351,1.11644108779696,6.63334840350399));
#283552=CARTESIAN_POINT('Ctrl Pts',(1.19028244098421,1.00294760313995,6.6231088990313));
#283553=CARTESIAN_POINT('Ctrl Pts',(1.2253901522336,0.959736464880182,6.61933327626673));
#283554=CARTESIAN_POINT('Ctrl Pts',(1.26785887780604,0.901326359025587,
6.61431224592061));
#283555=CARTESIAN_POINT('Ctrl Pts',(1.27739696154372,0.887756895336745,
6.61315139474784));
#283556=CARTESIAN_POINT('Ctrl Pts',(1.2925537505794,0.865443811728671,6.6112499489345));
#283557=CARTESIAN_POINT('Ctrl Pts',(1.29830518456281,0.85679158939647,6.61051440859563));
#283558=CARTESIAN_POINT('Ctrl Pts',(1.30924786038382,0.839966678105984,
6.6090871108953));
#283559=CARTESIAN_POINT('Ctrl Pts',(1.3144503318504,0.831801837899735,6.60839581553785));
#283560=CARTESIAN_POINT('Ctrl Pts',(1.32643599610891,0.81259809182223,6.60677270042734));
#283561=CARTESIAN_POINT('Ctrl Pts',(1.33315806442328,0.801522093876135,
6.60583868945038));
#283562=CARTESIAN_POINT('Ctrl Pts',(1.35491934506289,0.764634677634679,
6.60273424475909));
#283563=CARTESIAN_POINT('Ctrl Pts',(1.36935252725195,0.738475490855844,
6.60054239623207));
#283564=CARTESIAN_POINT('Ctrl Pts',(1.40253533779561,0.674012245818938,
6.59516062961372));
#283565=CARTESIAN_POINT('Ctrl Pts',(1.4204795248445,0.635322934141587,6.59194637432709));
#283566=CARTESIAN_POINT('Ctrl Pts',(1.46177951877084,0.535750096808311,
6.58372230139521));
#283567=CARTESIAN_POINT('Ctrl Pts',(1.48293885205268,0.47404528648415,6.57866753138253));
#283568=CARTESIAN_POINT('Ctrl Pts',(1.50470799049797,0.394625703168508,
6.57228161227169));
#283569=CARTESIAN_POINT('Ctrl Pts',(1.50897600331429,0.377977529916296,
6.57094972042722));
#283570=CARTESIAN_POINT('Ctrl Pts',(1.52784589732106,0.298950291933647,
6.56466634838832));
#283571=CARTESIAN_POINT('Ctrl Pts',(1.53886264440151,0.235771226002317,
6.55975470473817));
#283572=CARTESIAN_POINT('Ctrl Pts',(1.54718261741522,0.161027932277864,
6.55419261756031));
#283573=CARTESIAN_POINT('Ctrl Pts',(1.54829490310943,0.149956522163682,
6.55337513688733));
#283574=CARTESIAN_POINT('Ctrl Pts',(1.54984698521695,0.132641346906011,
6.55210759563121));
#283575=CARTESIAN_POINT('Ctrl Pts',(1.55036803801667,0.126405517607858,
6.55165332418757));
#283576=CARTESIAN_POINT('Ctrl Pts',(1.55122734902196,0.115315380425145,
6.55084955983854));
#283577=CARTESIAN_POINT('Ctrl Pts',(1.55158046788556,0.110462564113963,
6.55049927385853));
#283578=CARTESIAN_POINT('Ctrl Pts',(1.55238129226738,0.0986944348818104,
6.54965319273492));
#283579=CARTESIAN_POINT('Ctrl Pts',(1.55280556777163,0.0917776751041955,
6.54915869984335));
#283580=CARTESIAN_POINT('Ctrl Pts',(1.55399162184719,0.070068975648567,
6.54761480787361));
#283581=CARTESIAN_POINT('Ctrl Pts',(1.5545883948504,0.0552683169444688,
6.54657400337074));
#283582=CARTESIAN_POINT('Ctrl Pts',(1.55665088349847,-0.0239966576722541,
6.54105215008089));
#283583=CARTESIAN_POINT('Ctrl Pts',(1.55431877384013,-0.088504090703835,
6.53674163935358));
#283584=CARTESIAN_POINT('Ctrl Pts',(1.53652231810634,-0.26892959715407,
6.52474814113756));
#283585=CARTESIAN_POINT('Ctrl Pts',(1.51200157123545,-0.383501638794764,
6.51717781213232));
#283586=CARTESIAN_POINT('Ctrl Pts',(1.46514012928999,-0.523341320002035,
6.50711202862732));
#283587=CARTESIAN_POINT('Ctrl Pts',(1.4545325465319,-0.552138200456382,
6.50499476686973));
#283588=CARTESIAN_POINT('Ctrl Pts',(1.43855369778288,-0.591853549419929,
6.50200160706115));
#283589=CARTESIAN_POINT('Ctrl Pts',(1.43389508192174,-0.603052439437859,
6.50114933806971));
#283590=CARTESIAN_POINT('Ctrl Pts',(1.42557015799808,-0.622422820437998,
6.49966013953967));
#283591=CARTESIAN_POINT('Ctrl Pts',(1.42196331053641,-0.630619362352773,
6.49902524417241));
#283592=CARTESIAN_POINT('Ctrl Pts',(1.41426208104662,-0.647718323930799,
6.49769054626426));
#283593=CARTESIAN_POINT('Ctrl Pts',(1.41015396281183,-0.656614083078789,
6.4969902954529));
#283594=CARTESIAN_POINT('Ctrl Pts',(1.40011921105144,-0.677814852349313,
6.49530697992032));
#283595=CARTESIAN_POINT('Ctrl Pts',(1.39411411400355,-0.690081585187227,
6.49432123440742));
#283596=CARTESIAN_POINT('Ctrl Pts',(1.37242595106076,-0.732945679961526,
6.49083399394285));
#283597=CARTESIAN_POINT('Ctrl Pts',(1.35589181071166,-0.763098561733579,
6.48830312735241));
#283598=CARTESIAN_POINT('Ctrl Pts',(1.31181080101408,-0.83752593281818,
6.4818525563301));
#283599=CARTESIAN_POINT('Ctrl Pts',(1.28301313016479,-0.881007158273952,
6.47789349817351));
#283600=CARTESIAN_POINT('Ctrl Pts',(1.21942477724302,-0.967271539143556,
6.46965782177956));
#283601=CARTESIAN_POINT('Ctrl Pts',(1.18443075747874,-1.00981900766067,
6.46538135871984));
#283602=CARTESIAN_POINT('Ctrl Pts',(1.09631582849073,-1.1060570721497,6.45526805932651));
#283603=CARTESIAN_POINT('Ctrl Pts',(1.04138915749959,-1.1579214011463,6.44945048408799));
#283604=CARTESIAN_POINT('Ctrl Pts',(0.974206759339196,-1.21269431851723,
6.44303829705089));
#283605=CARTESIAN_POINT('Ctrl Pts',(0.965427454652025,-1.21969511326993,
6.4422132049179));
#283606=CARTESIAN_POINT('Ctrl Pts',(0.951620589825,-1.23046249119583,6.44093645477913));
#283607=CARTESIAN_POINT('Ctrl Pts',(0.946644939638089,-1.23429455609448,
6.44048049097239));
#283608=CARTESIAN_POINT('Ctrl Pts',(0.937776127773533,-1.24103981569778,
6.43967528196184));
#283609=CARTESIAN_POINT('Ctrl Pts',(0.9338924602303,-1.24396493673252,6.43932522664153));
#283610=CARTESIAN_POINT('Ctrl Pts',(0.924466642400233,-1.25099530039113,
6.43848168511117));
#283611=CARTESIAN_POINT('Ctrl Pts',(0.918910818049202,-1.25508196059468,
6.43798947915095));
#283612=CARTESIAN_POINT('Ctrl Pts',(0.901480895989794,-1.26772498606289,
6.43646020215657));
#283613=CARTESIAN_POINT('Ctrl Pts',(0.889512680547177,-1.27615111880029,
6.43543149604163));
#283614=CARTESIAN_POINT('Ctrl Pts',(0.825576522175744,-1.31982829869947,
6.43003747486217));
#283615=CARTESIAN_POINT('Ctrl Pts',(0.771622498192837,-1.35208133719632,
6.42583411052176));
#283616=CARTESIAN_POINT('Ctrl Pts',(0.616540474983412,-1.43247097659275,
6.41427011325858));
#283617=CARTESIAN_POINT('Ctrl Pts',(0.511963053506555,-1.47308789695883,
6.40702057564269));
#283618=CARTESIAN_POINT('Ctrl Pts',(0.369411508968676,-1.51142100825604,
6.39699502553451));
#283619=CARTESIAN_POINT('Ctrl Pts',(0.334580409405811,-1.51951108846512,
6.39453727680501));
#283620=CARTESIAN_POINT('Ctrl Pts',(0.285540354399109,-1.52913355756688,
6.39104830430307));
#283621=CARTESIAN_POINT('Ctrl Pts',(0.271540524280211,-1.53168157620455,
6.39004910955775));
#283622=CARTESIAN_POINT('Ctrl Pts',(0.248716085110685,-1.5355129556002,
6.38841398324918));
#283623=CARTESIAN_POINT('Ctrl Pts',(0.239911707522368,-1.53691317073847,
6.38778177690101));
#283624=CARTESIAN_POINT('Ctrl Pts',(0.221368715687206,-1.53969896287266,
6.38644694275585));
#283625=CARTESIAN_POINT('Ctrl Pts',(0.211628056039106,-1.54106799403702,
6.38574382267036));
#283626=CARTESIAN_POINT('Ctrl Pts',(0.188126472050311,-1.54414408278291,
6.38404240596493));
#283627=CARTESIAN_POINT('Ctrl Pts',(0.174354655125536,-1.54575966726496,
6.38304127944408));
#283628=CARTESIAN_POINT('Ctrl Pts',(0.124925284018921,-1.55088932014354,
6.37943231262649));
#283629=CARTESIAN_POINT('Ctrl Pts',(0.0891728657577869,-1.55335502129853,
6.37679228843598));
#283630=CARTESIAN_POINT('Ctrl Pts',(-0.00201351927747187,-1.55648550265918,
6.36997886386016));
#283631=CARTESIAN_POINT('Ctrl Pts',(-0.0574533471240208,-1.55542571916719,
6.36576002701786));
#283632=CARTESIAN_POINT('Ctrl Pts',(-0.232606063064412,-1.54270047770986,
6.35223738972163));
#283633=CARTESIAN_POINT('Ctrl Pts',(-0.351086710665847,-1.52012193412441,
6.34277053373473));
#283634=CARTESIAN_POINT('Ctrl Pts',(-0.478299917337154,-1.48019640715587,
6.33284952173644));
#283635=CARTESIAN_POINT('Ctrl Pts',(-0.490762097551915,-1.47611138054362,
6.33188076843525));
#283636=CARTESIAN_POINT('Ctrl Pts',(-0.509491470964639,-1.46970857618049,
6.33043108797992));
#283637=CARTESIAN_POINT('Ctrl Pts',(-0.515797469385821,-1.46750735357876,
6.32994407484161));
#283638=CARTESIAN_POINT('Ctrl Pts',(-0.527230008477916,-1.46343382178655,
6.32906335022191));
#283639=CARTESIAN_POINT('Ctrl Pts',(-0.5323612407226,-1.46157502232004,
6.32866887512415));
#283640=CARTESIAN_POINT('Ctrl Pts',(-0.543037114109334,-1.45764398130796,
6.3278499845026));
#283641=CARTESIAN_POINT('Ctrl Pts',(-0.548579859251683,-1.45556704576282,
6.32742584796264));
#283642=CARTESIAN_POINT('Ctrl Pts',(-0.563332179360345,-1.44994292982204,
6.32629935979313));
#283643=CARTESIAN_POINT('Ctrl Pts',(-0.572520271662161,-1.44633958527201,
6.3256002363331));
#283644=CARTESIAN_POINT('Ctrl Pts',(-0.618520323465517,-1.42779243717715,
6.32210955204408));
#283645=CARTESIAN_POINT('Ctrl Pts',(-0.654787996334789,-1.4115282324559,
6.31938793102255));
#283646=CARTESIAN_POINT('Ctrl Pts',(-0.758472521619566,-1.36017313397632,
6.31158436026833));
#283647=CARTESIAN_POINT('Ctrl Pts',(-0.823991135252997,-1.32151108657096,
6.3066202900587));
#283648=CARTESIAN_POINT('Ctrl Pts',(-0.964229229278627,-1.22425770914935,
6.29537812268854));
#283649=CARTESIAN_POINT('Ctrl Pts',(-1.03693365902289,-1.1633185252147,
6.28909331355653));
#283650=CARTESIAN_POINT('Ctrl Pts',(-1.11642390976572,-1.08328522163345,
6.28126958470426));
#283651=CARTESIAN_POINT('Ctrl Pts',(-1.12897875900211,-1.07019443634102,
6.28000250653059));
#283652=CARTESIAN_POINT('Ctrl Pts',(-1.14858535129763,-1.04902186168229,
6.27797082086458));
#283653=CARTESIAN_POINT('Ctrl Pts',(-1.15578762361226,-1.04108123325357,
6.27721266798382));
#283654=CARTESIAN_POINT('Ctrl Pts',(-1.16927562919944,-1.02589799954425,
6.2757697471697));
#283655=CARTESIAN_POINT('Ctrl Pts',(-1.17557761212984,-1.01867044366101,
6.27508570562997));
#283656=CARTESIAN_POINT('Ctrl Pts',(-1.18978573513569,-1.00206813112445,
6.27352047261503));
#283657=CARTESIAN_POINT('Ctrl Pts',(-1.19764855280994,-0.992657323995823,
6.27263755948484));
#283658=CARTESIAN_POINT('Ctrl Pts',(-1.22130045408711,-0.963658858554,6.26992931278323));
#283659=CARTESIAN_POINT('Ctrl Pts',(-1.23672559484325,-0.94378115102228,
6.26808969298344));
#283660=CARTESIAN_POINT('Ctrl Pts',(-1.29130671686026,-0.869808036496203,
6.26129998372855));
#283661=CARTESIAN_POINT('Ctrl Pts',(-1.32744612453512,-0.813586944268549,
6.25624217308097));
#283662=CARTESIAN_POINT('Ctrl Pts',(-1.3946170124684,-0.692639009887966,
6.24560291173027));
#283663=CARTESIAN_POINT('Ctrl Pts',(-1.42501285501546,-0.627728688854752,
6.24002190928897));
#283664=CARTESIAN_POINT('Ctrl Pts',(-1.47160752256398,-0.50721913081853,
6.23005026678234));
#283665=CARTESIAN_POINT('Ctrl Pts',(-1.48938646004944,-0.452359877992798,
6.2256487107456));
#283666=CARTESIAN_POINT('Ctrl Pts',(-1.50687443407433,-0.386043601632136,
6.2205782026086));
#283667=CARTESIAN_POINT('Ctrl Pts',(-1.50955553405755,-0.375422868412904,
6.21977368128932));
#283668=CARTESIAN_POINT('Ctrl Pts',(-1.5135826029735,-0.358729179364893,
6.21852183329899));
#283669=CARTESIAN_POINT('Ctrl Pts',(-1.51500465785352,-0.352675219515232,
6.21807045542671));
#283670=CARTESIAN_POINT('Ctrl Pts',(-1.51759742241878,-0.341332176713582,
6.21722979922491));
#283671=CARTESIAN_POINT('Ctrl Pts',(-1.51877682081666,-0.336045474830606,
6.21684006969916));
#283672=CARTESIAN_POINT('Ctrl Pts',(-1.52107136114657,-0.325501222267586,
6.21606677300186));
#283673=CARTESIAN_POINT('Ctrl Pts',(-1.52218688824927,-0.320243986555809,
6.21568318647495));
#283674=CARTESIAN_POINT('Ctrl Pts',(-1.52473626775074,-0.30791496720822,
6.2147879981349));
#283675=CARTESIAN_POINT('Ctrl Pts',(-1.52614822035645,-0.30083870741485,
6.21427757032291));
#283676=CARTESIAN_POINT('Ctrl Pts',(-1.52975391864935,-0.282089114927303,
6.21293338783339));
#283677=CARTESIAN_POINT('Ctrl Pts',(-1.53186334017751,-0.270399792678156,
6.21210382229557));
#283678=CARTESIAN_POINT('Ctrl Pts',(-1.54817398109791,-0.173688750447234,
6.20530145682289));
#283679=CARTESIAN_POINT('Ctrl Pts',(-1.55542054432572,-0.0876372136492061,
6.19963183488464));
#283680=CARTESIAN_POINT('Ctrl Pts',(-1.55549935018888,-0.00142181643757374,
6.19395780777199));
#283681=CARTESIAN_POINT('',(-1.55313101942593,0.000158339568030034,5.49415672523128));
#283682=CARTESIAN_POINT('Ctrl Pts',(-1.5529563387483,0.000151106445085633,
5.49405622560371));
#283683=CARTESIAN_POINT('Ctrl Pts',(-1.55272340811799,-0.268780222436924,
5.5132440667186));
#283684=CARTESIAN_POINT('Ctrl Pts',(-1.35831396530156,-1.05747938365068,
5.56949404777722));
#283685=CARTESIAN_POINT('Ctrl Pts',(-0.103102773360761,-1.83589824620028,
5.66280616877956));
#283686=CARTESIAN_POINT('Ctrl Pts',(1.4869956060099,-1.08166382022474,5.77399258861071));
#283687=CARTESIAN_POINT('Ctrl Pts',(1.71494149863546,0.663421591850831,
5.88517900844189));
#283688=CARTESIAN_POINT('Ctrl Pts',(0.371926577693494,1.80078404398782,
5.99636542827304));
#283689=CARTESIAN_POINT('Ctrl Pts',(-1.18720044783918,1.3264536081355,6.0993244620085));
#283690=CARTESIAN_POINT('Ctrl Pts',(-1.55195178408473,0.400947059710162,
6.16522135580024));
#283691=CARTESIAN_POINT('Ctrl Pts',(-1.5556705629256,-0.00141387709470033,
6.19405610964826));
#283692=CARTESIAN_POINT('',(-1.55731595967384,-0.000935870630138446,4.09405524453403));
#283693=CARTESIAN_POINT('Ctrl Pts',(-1.55549997886283,0.000256432700539262,
5.49551966671036));
#283694=CARTESIAN_POINT('Ctrl Pts',(-1.5554991185824,0.00547482406793109,
5.49514503270296));
#283695=CARTESIAN_POINT('Ctrl Pts',(-1.55547199833197,0.010693128598903,
5.49476957764081));
#283696=CARTESIAN_POINT('Ctrl Pts',(-1.55533490000557,0.0240953838132042,
5.49380312031377));
#283697=CARTESIAN_POINT('Ctrl Pts',(-1.55518658709843,0.0322786808451574,
5.49321093089671));
#283698=CARTESIAN_POINT('Ctrl Pts',(-1.55432199513997,0.065506767024369,
5.49079768122473));
#283699=CARTESIAN_POINT('Ctrl Pts',(-1.55306527454723,0.0905324237099038,
5.48896003392764));
#283700=CARTESIAN_POINT('Ctrl Pts',(-1.5421203365499,0.237506956043084,
5.4780438999739));
#283701=CARTESIAN_POINT('Ctrl Pts',(-1.5186779841696,0.357982530041526,
5.46854438678358));
#283702=CARTESIAN_POINT('Ctrl Pts',(-1.46183840961193,0.53545611450869,
5.45411423925923));
#283703=CARTESIAN_POINT('Ctrl Pts',(-1.43854449778955,0.595211079027277,
5.44918523340074));
#283704=CARTESIAN_POINT('Ctrl Pts',(-1.40542540183141,0.666766672759873,
5.44331588692544));
#283705=CARTESIAN_POINT('Ctrl Pts',(-1.39903129167002,0.680080762315757,
5.44222539821618));
#283706=CARTESIAN_POINT('Ctrl Pts',(-1.3893632167977,0.699498398527043,
5.44063945106656));
#283707=CARTESIAN_POINT('Ctrl Pts',(-1.38623681357353,0.705673904389142,
5.44013573410594));
#283708=CARTESIAN_POINT('Ctrl Pts',(-1.38084301210415,0.716153957993286,
5.43928231124514));
#283709=CARTESIAN_POINT('Ctrl Pts',(-1.37859651498946,0.720468991002216,
5.43893134363674));
#283710=CARTESIAN_POINT('Ctrl Pts',(-1.37341160068452,0.730315033294327,
5.43813150187911));
#283711=CARTESIAN_POINT('Ctrl Pts',(-1.37045998417119,0.735838914583601,
5.4376834631261));
#283712=CARTESIAN_POINT('Ctrl Pts',(-1.36216059912738,0.751147849700196,
5.43644326714848));
#283713=CARTESIAN_POINT('Ctrl Pts',(-1.35674072459185,0.760893694930043,
5.4356554626379));
#283714=CARTESIAN_POINT('Ctrl Pts',(-1.31878746532864,0.827444878589895,
5.43028168349018));
#283715=CARTESIAN_POINT('Ctrl Pts',(-1.28279681546386,0.882213144464907,
5.42588774124978));
#283716=CARTESIAN_POINT('Ctrl Pts',(-1.23434786585122,0.946676002542723,
5.42054324604659));
#283717=CARTESIAN_POINT('Ctrl Pts',(-1.22506217965674,0.958661970525544,
5.41954172012888));
#283718=CARTESIAN_POINT('Ctrl Pts',(-1.17100858354432,1.02636623759926,
5.41382839449819));
#283719=CARTESIAN_POINT('Ctrl Pts',(-1.12261913824008,1.07908047166182,
5.40915502094565));
#283720=CARTESIAN_POINT('Ctrl Pts',(-1.02789304292682,1.16897888008542,
5.40043588478306));
#283721=CARTESIAN_POINT('Ctrl Pts',(-0.982727759685129,1.20719534945809,
5.39642931246848));
#283722=CARTESIAN_POINT('Ctrl Pts',(-0.922435306134706,1.25258165788644,
5.39118043073622));
#283723=CARTESIAN_POINT('Ctrl Pts',(-0.909215639357971,1.26221020015493,
5.39003546580615));
#283724=CARTESIAN_POINT('Ctrl Pts',(-0.887969190220278,1.27717807246545,
5.38820307351456));
#283725=CARTESIAN_POINT('Ctrl Pts',(-0.880040094008858,1.28265448853016,
5.38752091576348));
#283726=CARTESIAN_POINT('Ctrl Pts',(-0.864390056963656,1.29325012679417,
5.3861774777026));
#283727=CARTESIAN_POINT('Ctrl Pts',(-0.856673247449613,1.2983747537971,
5.38551643805449));
#283728=CARTESIAN_POINT('Ctrl Pts',(-0.838831670299249,1.30999479896602,
5.38399098751339));
#283729=CARTESIAN_POINT('Ctrl Pts',(-0.828676525033821,1.31644223046614,
5.38312483817094));
#283730=CARTESIAN_POINT('Ctrl Pts',(-0.801499768435247,1.3332575051954,
5.38081189806941));
#283731=CARTESIAN_POINT('Ctrl Pts',(-0.78435244596338,1.34341677307045,
5.37935765259221));
#283732=CARTESIAN_POINT('Ctrl Pts',(-0.646869350932612,1.42134189100549,
5.3677332023205));
#283733=CARTESIAN_POINT('Ctrl Pts',(-0.518208795480751,1.47312477764943,
5.3569845925563));
#283734=CARTESIAN_POINT('Ctrl Pts',(-0.342673207996331,1.51789780885836,
5.34297909981599));
#283735=CARTESIAN_POINT('Ctrl Pts',(-0.300473239542847,1.52681204362755,
5.33966649560503));
#283736=CARTESIAN_POINT('Ctrl Pts',(-0.241123071012958,1.536792515486,5.3351242002023));
#283737=CARTESIAN_POINT('Ctrl Pts',(-0.224245011447707,1.5393459004059,
5.33384552282526));
#283738=CARTESIAN_POINT('Ctrl Pts',(-0.194536987017095,1.54334123531981,
5.3316214340136));
#283739=CARTESIAN_POINT('Ctrl Pts',(-0.181724929709431,1.54490222564149,
5.33067089668175));
#283740=CARTESIAN_POINT('Ctrl Pts',(-0.162372257850548,1.54701601332483,
5.32924955155693));
#283741=CARTESIAN_POINT('Ctrl Pts',(-0.155845529685681,1.54768713592207,
5.32877267177119));
#283742=CARTESIAN_POINT('Ctrl Pts',(-0.143964175303132,1.54883293463854,
5.3279092801111));
#283743=CARTESIAN_POINT('Ctrl Pts',(-0.138611206851933,1.54932116702434,
5.32752205770599));
#283744=CARTESIAN_POINT('Ctrl Pts',(-0.126445675118673,1.55036720112347,
5.32664598008888));
#283745=CARTESIAN_POINT('Ctrl Pts',(-0.11963185606256,1.55090786018908,
5.3261580764442));
#283746=CARTESIAN_POINT('Ctrl Pts',(-0.0985439974603953,1.55244132106271,
5.32465605497674));
#283747=CARTESIAN_POINT('Ctrl Pts',(-0.0842591641910188,1.55328213994008,
5.32364988218428));
#283748=CARTESIAN_POINT('Ctrl Pts',(0.0511940515907608,1.55938079860967,
5.31419848337449));
#283749=CARTESIAN_POINT('Ctrl Pts',(0.172593295299025,1.55064827680406,
5.30638146696615));
#283750=CARTESIAN_POINT('Ctrl Pts',(0.345726188914309,1.51758766040755,
5.29473689372495));
#283751=CARTESIAN_POINT('Ctrl Pts',(0.399105611911333,1.50443108699072,
5.29107946082504));
#283752=CARTESIAN_POINT('Ctrl Pts',(0.485764512200602,1.47813471516828,
5.28492437537136));
#283753=CARTESIAN_POINT('Ctrl Pts',(0.51948679190479,1.4666228359979,5.28247330611433));
#283754=CARTESIAN_POINT('Ctrl Pts',(0.565716048478519,1.44904695172144,
5.27901783739476));
#283755=CARTESIAN_POINT('Ctrl Pts',(0.578583371567505,1.44395740108128,
5.27804560306345));
#283756=CARTESIAN_POINT('Ctrl Pts',(0.600473572911076,1.43495936809009,
5.27637273532666));
#283757=CARTESIAN_POINT('Ctrl Pts',(0.609530586580863,1.43113568740939,
5.27567499028124));
#283758=CARTESIAN_POINT('Ctrl Pts',(0.626735296029037,1.42367927965112,
5.27433852329056));
#283759=CARTESIAN_POINT('Ctrl Pts',(0.634889205355858,1.42006179914445,
5.27370034454408));
#283760=CARTESIAN_POINT('Ctrl Pts',(0.655996175763244,1.41047957148434,
5.272035641227));
#283761=CARTESIAN_POINT('Ctrl Pts',(0.668898862452639,1.40440659739065,
5.27100543121115));
#283762=CARTESIAN_POINT('Ctrl Pts',(0.714079285919814,1.38237745162958,
5.26735228342539));
#283763=CARTESIAN_POINT('Ctrl Pts',(0.745882424011416,1.36548001171883,
5.26469716888098));
#283764=CARTESIAN_POINT('Ctrl Pts',(0.873787305127055,1.29172033589242,
5.25366277875605));
#283765=CARTESIAN_POINT('Ctrl Pts',(0.964208399238657,1.22570017467944,
5.24497881364308));
#283766=CARTESIAN_POINT('Ctrl Pts',(1.09315990116245,1.10838384784354,5.2314838106662));
#283767=CARTESIAN_POINT('Ctrl Pts',(1.13695926116461,1.06340895670286,5.22666255042126));
#283768=CARTESIAN_POINT('Ctrl Pts',(1.18747986338139,1.00483121506877,5.22090578111305));
#283769=CARTESIAN_POINT('Ctrl Pts',(1.19687656078714,0.99362001597432,5.21982593798354));
#283770=CARTESIAN_POINT('Ctrl Pts',(1.21046831982977,0.976931030925822,
5.21825242662576));
#283771=CARTESIAN_POINT('Ctrl Pts',(1.21478700258578,0.971555626664188,
5.21775067649091));
#283772=CARTESIAN_POINT('Ctrl Pts',(1.22208968608591,0.962341252657412,
5.21689943706303));
#283773=CARTESIAN_POINT('Ctrl Pts',(1.22509160501491,0.958516796510098,
5.21654870392902));
#283774=CARTESIAN_POINT('Ctrl Pts',(1.23193071722327,0.949719122310274,
5.21574780342528));
#283775=CARTESIAN_POINT('Ctrl Pts',(1.23575577394762,0.94473666922855,5.21529848528453));
#283776=CARTESIAN_POINT('Ctrl Pts',(1.24633695493368,0.930779580781612,
5.21405122747741));
#283777=CARTESIAN_POINT('Ctrl Pts',(1.25302637014761,0.921754505370562,
5.21325772033959));
#283778=CARTESIAN_POINT('Ctrl Pts',(1.30398779752879,0.851419334673316,
5.20716654632157));
#283779=CARTESIAN_POINT('Ctrl Pts',(1.34383975871665,0.787017822628581,
5.20212675746629));
#283780=CARTESIAN_POINT('Ctrl Pts',(1.40422697131077,0.671366133002683,
5.19351181872391));
#283781=CARTESIAN_POINT('Ctrl Pts',(1.42701500864217,0.621461211563885,
5.189921919155));
#283782=CARTESIAN_POINT('Ctrl Pts',(1.46624283895116,0.521949135579925,
5.18284559768908));
#283783=CARTESIAN_POINT('Ctrl Pts',(1.48291245496679,0.472513451841354,
5.1793673291509));
#283784=CARTESIAN_POINT('Ctrl Pts',(1.50640488548135,0.389239264348815,
5.17347966139198));
#283785=CARTESIAN_POINT('Ctrl Pts',(1.51464123105902,0.355843404174913,
5.17111148346894));
#283786=CARTESIAN_POINT('Ctrl Pts',(1.52459296377786,0.308841553684111,
5.16775359843802));
#283787=CARTESIAN_POINT('Ctrl Pts',(1.52724600301168,0.295442779178589,
5.16679362211836));
#283788=CARTESIAN_POINT('Ctrl Pts',(1.53149868327036,0.272374830360456,
5.16513529680096));
#283789=CARTESIAN_POINT('Ctrl Pts',(1.5331840540612,0.262722122100428,5.16443970798818));
#283790=CARTESIAN_POINT('Ctrl Pts',(1.53623488061118,0.244218816257638,
5.16310284138545));
#283791=CARTESIAN_POINT('Ctrl Pts',(1.53761532795962,0.235371059481809,
5.16246206913289));
#283792=CARTESIAN_POINT('Ctrl Pts',(1.540685381266,0.214513165538916,5.16094768358292));
#283793=CARTESIAN_POINT('Ctrl Pts',(1.54231104448387,0.20249436730432,5.16007208864091));
#283794=CARTESIAN_POINT('Ctrl Pts',(1.54755220045282,0.160011136346541,
5.15696591940551));
#283795=CARTESIAN_POINT('Ctrl Pts',(1.55040664333606,0.129461854421636,
5.15471189334351));
#283796=CARTESIAN_POINT('Ctrl Pts',(1.55977999635251,-0.0177386591366861,
5.14374606308071));
#283797=CARTESIAN_POINT('Ctrl Pts',(1.55404469942018,-0.134776590449723,
5.13467178316308));
#283798=CARTESIAN_POINT('Ctrl Pts',(1.52490562563184,-0.313689423111976,
5.12063397442985));
#283799=CARTESIAN_POINT('Ctrl Pts',(1.51059153591323,-0.376633997131565,
5.11567183068498));
#283800=CARTESIAN_POINT('Ctrl Pts',(1.48823389725521,-0.452724524602937,
5.10976791550134));
#283801=CARTESIAN_POINT('Ctrl Pts',(1.48385541939011,-0.466875534954578,
5.10867419074575));
#283802=CARTESIAN_POINT('Ctrl Pts',(1.4771326414371,-0.487552487624977,
5.10708446609254));
#283803=CARTESIAN_POINT('Ctrl Pts',(1.47494595016069,-0.494128240054058,
5.10658015365321));
#283804=CARTESIAN_POINT('Ctrl Pts',(1.4711491657838,-0.505296008701843,
5.10572606813904));
#283805=CARTESIAN_POINT('Ctrl Pts',(1.4695613814533,-0.509895355010277,
5.10537502794862));
#283806=CARTESIAN_POINT('Ctrl Pts',(1.46588233436924,-0.520392530646494,
5.10457549899203));
#283807=CARTESIAN_POINT('Ctrl Pts',(1.4637770378746,-0.526285275520889,
5.10412784148784));
#283808=CARTESIAN_POINT('Ctrl Pts',(1.45782968462014,-0.542620175335744,
5.10288974745943));
#283809=CARTESIAN_POINT('Ctrl Pts',(1.45391097166605,-0.553034311068582,
5.10210364001836));
#283810=CARTESIAN_POINT('Ctrl Pts',(1.42668445726724,-0.623099602218949,
5.09683080756177));
#283811=CARTESIAN_POINT('Ctrl Pts',(1.39982059615336,-0.681312062502137,
5.09252771901382));
#283812=CARTESIAN_POINT('Ctrl Pts',(1.36128143755865,-0.752853925609075,
5.08713854163707));
#283813=CARTESIAN_POINT('Ctrl Pts',(1.35287209161084,-0.767862816030155,
5.08600211510296));
#283814=CARTESIAN_POINT('Ctrl Pts',(1.31142712917084,-0.839038070531316,
5.08057126968214));
#283815=CARTESIAN_POINT('Ctrl Pts',(1.27513390224327,-0.893229697464711,
5.07630730798694));
#283816=CARTESIAN_POINT('Ctrl Pts',(1.20964565836676,-0.97885432408689,
5.06913049938858));
#283817=CARTESIAN_POINT('Ctrl Pts',(1.18236146377073,-1.01164190938535,
5.06626388311691));
#283818=CARTESIAN_POINT('Ctrl Pts',(1.13372886978653,-1.06542558085201,
5.06130727619341));
#283819=CARTESIAN_POINT('Ctrl Pts',(1.11305822606272,-1.08700230174605,
5.0592428454919));
#283820=CARTESIAN_POINT('Ctrl Pts',(1.08255134915105,-1.11706342776354,
5.05624503902177));
#283821=CARTESIAN_POINT('Ctrl Pts',(1.07320941846039,-1.12604158507372,
5.05533331207533));
#283822=CARTESIAN_POINT('Ctrl Pts',(1.05669297089046,-1.14152264418962,
5.05373146233934));
#283823=CARTESIAN_POINT('Ctrl Pts',(1.04956776480652,-1.1480772976023,5.05304360706241));
#283824=CARTESIAN_POINT('Ctrl Pts',(1.03467065694356,-1.16152693313058,
5.05161169605077));
#283825=CARTESIAN_POINT('Ctrl Pts',(1.02688995582354,-1.16841139743433,
5.05086724597422));
#283826=CARTESIAN_POINT('Ctrl Pts',(1.0065108514817,-1.18608229512629,5.04892582090416));
#283827=CARTESIAN_POINT('Ctrl Pts',(0.993808162465199,-1.19674583833066,
5.04772388323463));
#283828=CARTESIAN_POINT('Ctrl Pts',(0.937763423603453,-1.24228612118081,
5.04245408933417));
#283829=CARTESIAN_POINT('Ctrl Pts',(0.892743471124306,-1.2750226516954,
5.03830353396108));
#283830=CARTESIAN_POINT('Ctrl Pts',(0.764219343336251,-1.35833129091181,
5.02667427013253));
#283831=CARTESIAN_POINT('Ctrl Pts',(0.677561649835615,-1.40356774020954,
5.01905705579641));
#283832=CARTESIAN_POINT('Ctrl Pts',(0.55059301904567,-1.45533317969305,
5.00847350624125));
#283833=CARTESIAN_POINT('Ctrl Pts',(0.513376369089351,-1.46887455625755,
5.0054389396611));
#283834=CARTESIAN_POINT('Ctrl Pts',(0.460287214164724,-1.48592643013444,
5.00123696655656));
#283835=CARTESIAN_POINT('Ctrl Pts',(0.444816265438071,-1.49063081047118,
5.00002733203459));
#283836=CARTESIAN_POINT('Ctrl Pts',(0.417374359606732,-1.49850998367764,
4.99791104438924));
#283837=CARTESIAN_POINT('Ctrl Pts',(0.405433757298075,-1.50178461218087,
4.99699989338688));
#283838=CARTESIAN_POINT('Ctrl Pts',(0.387210422422518,-1.5065490356495,
4.9956253095767));
#283839=CARTESIAN_POINT('Ctrl Pts',(0.380955753739081,-1.50814277366893,
4.99515636706837));
#283840=CARTESIAN_POINT('Ctrl Pts',(0.369467536380055,-1.51099402943458,
4.99430047626529));
#283841=CARTESIAN_POINT('Ctrl Pts',(0.364237291325487,-1.51226334175097,
4.99391289654182));
#283842=CARTESIAN_POINT('Ctrl Pts',(0.352223206372751,-1.51511305714213,
4.9930272970276));
#283843=CARTESIAN_POINT('Ctrl Pts',(0.345435223296114,-1.51667507215613,
4.99253032057237));
#283844=CARTESIAN_POINT('Ctrl Pts',(0.324508790589972,-1.52134277079016,
4.99100797114073));
#283845=CARTESIAN_POINT('Ctrl Pts',(0.310336811589613,-1.52429684909104,
4.98999066658263));
#283846=CARTESIAN_POINT('Ctrl Pts',(0.205564675119994,-1.54461418795323,
4.98255628363391));
#283847=CARTESIAN_POINT('Ctrl Pts',(0.113608213434321,-1.55408746344118,
4.9764992832139));
#283848=CARTESIAN_POINT('Ctrl Pts',(-0.0754535337835974,-1.55668185656689,
4.96405663635709));
#283849=CARTESIAN_POINT('Ctrl Pts',(-0.17215225755354,-1.54897142935768,
4.95769043733825));
#283850=CARTESIAN_POINT('Ctrl Pts',(-0.293288792738089,-1.52782432209277,
4.9492503123365));
#283851=CARTESIAN_POINT('Ctrl Pts',(-0.318956481770425,-1.52267268330145,
4.94743597031639));
#283852=CARTESIAN_POINT('Ctrl Pts',(-0.356492238879651,-1.51414835814987,
4.94473788398835));
#283853=CARTESIAN_POINT('Ctrl Pts',(-0.368470591445589,-1.5112780599773,
4.94387010277791));
#283854=CARTESIAN_POINT('Ctrl Pts',(-0.389717163372071,-1.50591927113162,
4.94231815531697));
#283855=CARTESIAN_POINT('Ctrl Pts',(-0.398998925965467,-1.50348667041789,
4.94163582065248));
#283856=CARTESIAN_POINT('Ctrl Pts',(-0.418572409065049,-1.49816276130777,
4.94018738014775));
#283857=CARTESIAN_POINT('Ctrl Pts',(-0.428857975441933,-1.49525093122185,
4.93942063934572));
#283858=CARTESIAN_POINT('Ctrl Pts',(-0.456374580165599,-1.48715374975951,
4.9373538772618));
#283859=CARTESIAN_POINT('Ctrl Pts',(-0.473546534744002,-1.4817751724637,
4.93604763405927));
#283860=CARTESIAN_POINT('Ctrl Pts',(-0.568453890697525,-1.45023021837367,
4.92873317869972));
#283861=CARTESIAN_POINT('Ctrl Pts',(-0.644105814605085,-1.41824931098287,
4.92253532239577));
#283862=CARTESIAN_POINT('Ctrl Pts',(-0.772547701739792,-1.35154938722656,
4.91139367169342));
#283863=CARTESIAN_POINT('Ctrl Pts',(-0.826420777600485,-1.3192968067106,
4.90650997392966));
#283864=CARTESIAN_POINT('Ctrl Pts',(-0.914003442042359,-1.25938869739363,
4.89830537373349));
#283865=CARTESIAN_POINT('Ctrl Pts',(-0.948771761555057,-1.23340781261568,
4.89497130406377));
#283866=CARTESIAN_POINT('Ctrl Pts',(-0.995696104886528,-1.19518331195752,
4.89040288505791));
#283867=CARTESIAN_POINT('Ctrl Pts',(-1.0088026157071,-1.18414155438375,
4.88911901589027));
#283868=CARTESIAN_POINT('Ctrl Pts',(-1.03148530664532,-1.16438218851592,
4.88688685041603));
#283869=CARTESIAN_POINT('Ctrl Pts',(-1.04113993849472,-1.15575753356495,
4.88593337946689));
#283870=CARTESIAN_POINT('Ctrl Pts',(-1.05552993935691,-1.14257601314418,
4.88450855907068));
#283871=CARTESIAN_POINT('Ctrl Pts',(-1.06034565932528,-1.13810829259536,
4.88403109481396));
#283872=CARTESIAN_POINT('Ctrl Pts',(-1.06905014763623,-1.12992960906528,
4.88316713854138));
#283873=CARTESIAN_POINT('Ctrl Pts',(-1.07294808194658,-1.12622890885256,
4.88277993021587));
#283874=CARTESIAN_POINT('Ctrl Pts',(-1.08175285965471,-1.11778244525903,
4.88190449956577));
#283875=CARTESIAN_POINT('Ctrl Pts',(-1.08664772735254,-1.11302451259086,
4.88141722244139));
#283876=CARTESIAN_POINT('Ctrl Pts',(-1.10167160019875,-1.09822734859344,
4.87991914450417));
#283877=CARTESIAN_POINT('Ctrl Pts',(-1.11169433882965,-1.08808058468585,
4.8789162288712));
#283878=CARTESIAN_POINT('Ctrl Pts',(-1.18910836532124,-1.00752203534501,
4.87112763911835));
#283879=CARTESIAN_POINT('Ctrl Pts',(-1.24989613273275,-0.931044891407583,
4.86474775779634));
#283880=CARTESIAN_POINT('Ctrl Pts',(-1.35968806954421,-0.762598609926195,
4.85151586146143));
#283881=CARTESIAN_POINT('Ctrl Pts',(-1.40742978767123,-0.670407182538903,
4.84468350877883));
#283882=CARTESIAN_POINT('Ctrl Pts',(-1.45274699049436,-0.556305327441571,
4.83618164536551));
#283883=CARTESIAN_POINT('Ctrl Pts',(-1.45950752898951,-0.538318820045125,
4.83484096630898));
#283884=CARTESIAN_POINT('Ctrl Pts',(-1.46959444259906,-0.509894392674305,
4.83271900722765));
#283885=CARTESIAN_POINT('Ctrl Pts',(-1.47314683743284,-0.499538288553856,
4.83194523389503));
#283886=CARTESIAN_POINT('Ctrl Pts',(-1.47959446841543,-0.480074756832254,
4.83048929757246));
#283887=CARTESIAN_POINT('Ctrl Pts',(-1.48251568695909,-0.470976425674157,
4.82980802932932));
#283888=CARTESIAN_POINT('Ctrl Pts',(-1.48888762285446,-0.450483769486474,
4.82827174048569));
#283889=CARTESIAN_POINT('Ctrl Pts',(-1.49229169359224,-0.439075695804738,
4.82741523826182));
#283890=CARTESIAN_POINT('Ctrl Pts',(-1.50069922795543,-0.409671748049369,
4.82520385673177));
#283891=CARTESIAN_POINT('Ctrl Pts',(-1.50550997191583,-0.391623265476998,
4.82384286320593));
#283892=CARTESIAN_POINT('Ctrl Pts',(-1.54033097574258,-0.250845564800252,
4.81319509430448));
#283893=CARTESIAN_POINT('Ctrl Pts',(-1.55560595750119,-0.12498128167098,
4.80342941955489));
#283894=CARTESIAN_POINT('Ctrl Pts',(-1.55543470816142,0.0780745858892366,
4.78768878259148));
#283895=CARTESIAN_POINT('Ctrl Pts',(-1.54968774875899,0.154736691934658,
4.78176471616885));
#283896=CARTESIAN_POINT('Ctrl Pts',(-1.53663215718487,0.241802853964703,
4.77525159579969));
#283897=CARTESIAN_POINT('Ctrl Pts',(-1.53484169064513,0.252918980925539,
4.77442421834414));
#283898=CARTESIAN_POINT('Ctrl Pts',(-1.53186354482938,0.270210759887601,
4.77314470448401));
#283899=CARTESIAN_POINT('Ctrl Pts',(-1.53075889692148,0.276400032510002,
4.77268823360414));
#283900=CARTESIAN_POINT('Ctrl Pts',(-1.52873363468571,0.287362756983758,
4.77188258784134));
#283901=CARTESIAN_POINT('Ctrl Pts',(-1.5278281586583,0.292138663432025,
4.77153259774745));
#283902=CARTESIAN_POINT('Ctrl Pts',(-1.52558567963406,0.303670900382418,
4.77068979992706));
#283903=CARTESIAN_POINT('Ctrl Pts',(-1.52422617478093,0.310422703041895,
4.77019826598363));
#283904=CARTESIAN_POINT('Ctrl Pts',(-1.51984816121821,0.331443073329807,
4.76867326667872));
#283905=CARTESIAN_POINT('Ctrl Pts',(-1.51667369580976,0.345678875258279,
4.76764809961364));
#283906=CARTESIAN_POINT('Ctrl Pts',(-1.49888426204093,0.420486010195662,
4.76229100936725));
#283907=CARTESIAN_POINT('Ctrl Pts',(-1.48083821774806,0.480190112556536,
4.75811859777211));
#283908=CARTESIAN_POINT('Ctrl Pts',(-1.42100032455901,0.642294885730506,
4.74667672843741));
#283909=CARTESIAN_POINT('Ctrl Pts',(-1.37181519404658,0.741556960023045,
4.73951771499704));
#283910=CARTESIAN_POINT('Ctrl Pts',(-1.29255650026169,0.866177413175332,
4.72950071279298));
#283911=CARTESIAN_POINT('Ctrl Pts',(-1.27146247963229,0.896854733330727,
4.72694455947008));
#283912=CARTESIAN_POINT('Ctrl Pts',(-1.24068543774466,0.938343474394788,
4.72333955694567));
#283913=CARTESIAN_POINT('Ctrl Pts',(-1.23192003715069,0.94982199844864,
4.72232574936717));
#283914=CARTESIAN_POINT('Ctrl Pts',(-1.21746455214268,0.968215088153344,
4.72067334693005));
#283915=CARTESIAN_POINT('Ctrl Pts',(-1.21187221873962,0.975205676774685,
4.72003863991375));
#283916=CARTESIAN_POINT('Ctrl Pts',(-1.20003156996824,0.989747715803581,
4.71870394431058));
#283917=CARTESIAN_POINT('Ctrl Pts',(-1.19377162032332,0.997289135733643,
4.71800350446682));
#283918=CARTESIAN_POINT('Ctrl Pts',(-1.17860989500708,1.0152073063702,4.71631898332029));
#283919=CARTESIAN_POINT('Ctrl Pts',(-1.16964190173228,1.02552667396715,
4.71533221132934));
#283920=CARTESIAN_POINT('Ctrl Pts',(-1.1375830092729,1.06144891412006,4.71183696922541));
#283921=CARTESIAN_POINT('Ctrl Pts',(-1.11377967751207,1.08639927457709,
4.70929894684318));
#283922=CARTESIAN_POINT('Ctrl Pts',(-1.05180330860477,1.14718316029612,
4.70282489201629));
#283923=CARTESIAN_POINT('Ctrl Pts',(-1.01261569743052,1.18191703685438,
4.69884912782438));
#283924=CARTESIAN_POINT('Ctrl Pts',(-0.930800458297922,1.24737394213607,
4.69079606667584));
#283925=CARTESIAN_POINT('Ctrl Pts',(-0.888215171316857,1.27804723004451,
4.68672359706146));
#283926=CARTESIAN_POINT('Ctrl Pts',(-0.783849061468839,1.34548037621719,
4.6770905589045));
#283927=CARTESIAN_POINT('Ctrl Pts',(-0.720901861033794,1.3802316567811,
4.67154484035654));
#283928=CARTESIAN_POINT('Ctrl Pts',(-0.642150315273902,1.41684469961363,
4.66507742698801));
#283929=CARTESIAN_POINT('Ctrl Pts',(-0.628436209930061,1.42298064100923,
4.66396780404464));
#283930=CARTESIAN_POINT('Ctrl Pts',(-0.608233146093668,1.43167079038411,
4.66235953953423));
#283931=CARTESIAN_POINT('Ctrl Pts',(-0.601812992457291,1.43438137856049,
4.66185231776431));
#283932=CARTESIAN_POINT('Ctrl Pts',(-0.590402243656272,1.43910889433745,
4.66095790023241));
#283933=CARTESIAN_POINT('Ctrl Pts',(-0.585419140956528,1.44114317525696,
4.66056969997619));
#283934=CARTESIAN_POINT('Ctrl Pts',(-0.574439705093223,1.44555902622311,
4.65971964110002));
#283935=CARTESIAN_POINT('Ctrl Pts',(-0.568439022966637,1.44792919517864,
4.65925845655269));
#283936=CARTESIAN_POINT('Ctrl Pts',(-0.550893031848742,1.45473367588362,
4.65791936863506));
#283937=CARTESIAN_POINT('Ctrl Pts',(-0.539309042475031,1.45906784705516,
4.65704712436573));
#283938=CARTESIAN_POINT('Ctrl Pts',(-0.512485318052329,1.46874087204005,
4.65505177915966));
#283939=CARTESIAN_POINT('Ctrl Pts',(-0.497211466504593,1.47398159931793,
4.65393356224901));
#283940=CARTESIAN_POINT('Ctrl Pts',(-0.444300682815755,1.49122011826231,
4.65011241441144));
#283941=CARTESIAN_POINT('Ctrl Pts',(-0.406287976774585,1.50202232703985,
4.64745771620777));
#283942=CARTESIAN_POINT('Ctrl Pts',(-0.273333380629268,1.53438665325644,
4.63835391132833));
#283943=CARTESIAN_POINT('Ctrl Pts',(-0.176812993004962,1.54848027342748,
4.63204643070765));
#283944=CARTESIAN_POINT('Ctrl Pts',(-0.0237677265155158,1.55632310336705,
4.62180040172741));
#283945=CARTESIAN_POINT('Ctrl Pts',(0.0321798644021726,1.55617154356592,
4.61800696576614));
#283946=CARTESIAN_POINT('Ctrl Pts',(0.10457807900179,1.55206945897277,4.6129654880601));
#283947=CARTESIAN_POINT('Ctrl Pts',(0.121145923620136,1.55086421332858,
4.61180290187226));
#283948=CARTESIAN_POINT('Ctrl Pts',(0.148044719438292,1.54847378486338,
4.60989933189722));
#283949=CARTESIAN_POINT('Ctrl Pts',(0.158388973653528,1.54744991030415,
4.60916342418869));
#283950=CARTESIAN_POINT('Ctrl Pts',(0.17834423159108,1.54527255697801,4.60773591406529));
#283951=CARTESIAN_POINT('Ctrl Pts',(0.187956282181184,1.54413288562611,
4.60704477823766));
#283952=CARTESIAN_POINT('Ctrl Pts',(0.210394636875548,1.54125982785101,
4.60542281116796));
#283953=CARTESIAN_POINT('Ctrl Pts',(0.223211011486352,1.53945593820858,
4.6044897979831));
#283954=CARTESIAN_POINT('Ctrl Pts',(0.265448718359745,1.53297250649127,
4.60139237091659));
#283955=CARTESIAN_POINT('Ctrl Pts',(0.294756472059076,1.52760797470071,
4.59920667574173));
#283956=CARTESIAN_POINT('Ctrl Pts',(0.365430026832402,1.51256236013031,
4.59384357630822));
#283957=CARTESIAN_POINT('Ctrl Pts',(0.406586544321402,1.50202224198938,
4.59064206042419));
#283958=CARTESIAN_POINT('Ctrl Pts',(0.509876328326764,1.47101357215525,
4.58241568951463));
#283959=CARTESIAN_POINT('Ctrl Pts',(0.571244482837634,1.44828642560361,
4.57734486681293));
#283960=CARTESIAN_POINT('Ctrl Pts',(0.646819371954475,1.41474542474863,
4.57093298301966));
#283961=CARTESIAN_POINT('Ctrl Pts',(0.662523777127389,1.40745947407142,
4.5695913439259));
#283962=CARTESIAN_POINT('Ctrl Pts',(0.735711945631024,1.37200787689559,
4.56330237734785));
#283963=CARTESIAN_POINT('Ctrl Pts',(0.791550219056662,1.34056998133494,
4.55839487213495));
#283964=CARTESIAN_POINT('Ctrl Pts',(0.854636903523957,1.29973065930059,
4.5528367330824));
#283965=CARTESIAN_POINT('Ctrl Pts',(0.863911401415862,1.29358460605336,
4.55201932980882));
#283966=CARTESIAN_POINT('Ctrl Pts',(0.878297931622041,1.28382714759781,
4.55075188222789));
#283967=CARTESIAN_POINT('Ctrl Pts',(0.88345524118723,1.2802836568938,4.55029762802103));
#283968=CARTESIAN_POINT('Ctrl Pts',(0.892584828102444,1.27392945265123,
4.54949387828092));
#283969=CARTESIAN_POINT('Ctrl Pts',(0.896565355039005,1.27113118556369,
4.54914358984694));
#283970=CARTESIAN_POINT('Ctrl Pts',(0.906183280616655,1.26430223233624,
4.54829748239341));
#283971=CARTESIAN_POINT('Ctrl Pts',(0.911806966798369,1.26025248777772,
4.54780296585339));
#283972=CARTESIAN_POINT('Ctrl Pts',(0.929366015300521,1.24742874977715,
4.5462589222856));
#283973=CARTESIAN_POINT('Ctrl Pts',(0.941203658042819,1.23852145415787,
4.54521799223183));
#283974=CARTESIAN_POINT('Ctrl Pts',(1.00389023439881,1.18993465799148,4.53969479933298));
#283975=CARTESIAN_POINT('Ctrl Pts',(1.05236732174618,1.14728598289085,4.5353831657249));
#283976=CARTESIAN_POINT('Ctrl Pts',(1.18083093400292,1.01925197264863,4.52338510029554));
#283977=CARTESIAN_POINT('Ctrl Pts',(1.25403558792925,0.927701089906904,
4.51581133747605));
#283978=CARTESIAN_POINT('Ctrl Pts',(1.33261993648512,0.802896461201215,
4.50574488679024));
#283979=CARTESIAN_POINT('Ctrl Pts',(1.34817177344538,0.776499374406902,
4.50363104306515));
#283980=CARTESIAN_POINT('Ctrl Pts',(1.36877501188676,0.739041362634915,
4.50064194397133));
#283981=CARTESIAN_POINT('Ctrl Pts',(1.37449215557495,0.728353258005944,
4.4997902313057));
#283982=CARTESIAN_POINT('Ctrl Pts',(1.38421399716041,0.709656267277678,
4.49830172602355));
#283983=CARTESIAN_POINT('Ctrl Pts',(1.38827558822821,0.701677484791947,
4.49766696275442));
#283984=CARTESIAN_POINT('Ctrl Pts',(1.39663835865834,0.684892393266995,
4.49633226663884));
#283985=CARTESIAN_POINT('Ctrl Pts',(1.40092562704583,0.676079636286962,
4.49563188342889));
#283986=CARTESIAN_POINT('Ctrl Pts',(1.41099180135527,0.654881044255915,
4.49394772327396));
#283987=CARTESIAN_POINT('Ctrl Pts',(1.41669120541793,0.642458599381583,
4.49296125860456));
#283988=CARTESIAN_POINT('Ctrl Pts',(1.43617727533931,0.598466183395161,
4.48946841393429));
#283989=CARTESIAN_POINT('Ctrl Pts',(1.44907729178986,0.566517074492903,
4.48693253584653));
#283990=CARTESIAN_POINT('Ctrl Pts',(1.47885634310482,0.485073881899158,
4.48046552248606));
#283991=CARTESIAN_POINT('Ctrl Pts',(1.49431945571595,0.435110504478843,
4.47649476903844));
#283992=CARTESIAN_POINT('Ctrl Pts',(1.52040815298188,0.332834474915104,
4.46838259730061));
#283993=CARTESIAN_POINT('Ctrl Pts',(1.53091660082822,0.28055972034888,4.46424454314681));
#283994=CARTESIAN_POINT('Ctrl Pts',(1.54998633850925,0.151778018880049,
4.45415253507051));
#283995=CARTESIAN_POINT('Ctrl Pts',(1.55559546020059,0.074965192388891,
4.4482172689654));
#283996=CARTESIAN_POINT('Ctrl Pts',(1.55548461436945,-0.0132175837387635,
4.441693498677));
#283997=CARTESIAN_POINT('Ctrl Pts',(1.55534814308589,-0.0244798580928371,
4.44086584409795));
#283998=CARTESIAN_POINT('Ctrl Pts',(1.55494488341441,-0.0420261186706838,
4.43958599514133));
#283999=CARTESIAN_POINT('Ctrl Pts',(1.55476229708408,-0.048311369406584,
4.43912946280605));
#284000=CARTESIAN_POINT('Ctrl Pts',(1.55437098798986,-0.0594534306405277,
4.43832376399081));
#284001=CARTESIAN_POINT('Ctrl Pts',(1.55417761105585,-0.0643104435871024,
4.43797378168285));
#284002=CARTESIAN_POINT('Ctrl Pts',(1.55365527217932,-0.0760457813590657,
4.43713107346905));
#284003=CARTESIAN_POINT('Ctrl Pts',(1.55330340146001,-0.0829229368217237,
4.43663962056638));
#284004=CARTESIAN_POINT('Ctrl Pts',(1.55206429760475,-0.104351231650944,
4.43511513660698));
#284005=CARTESIAN_POINT('Ctrl Pts',(1.55101814343185,-0.118892903437067,
4.43409039583858));
#284006=CARTESIAN_POINT('Ctrl Pts',(1.54442838942697,-0.195438475024123,
4.42873774019216));
#284007=CARTESIAN_POINT('Ctrl Pts',(1.53537028147,-0.257089863315302,4.42456904527261));
#284008=CARTESIAN_POINT('Ctrl Pts',(1.50008630229764,-0.426015087996794,
4.41314179106502));
#284009=CARTESIAN_POINT('Ctrl Pts',(1.46611335116958,-0.531279998529964,
4.40599359212514));
#284010=CARTESIAN_POINT('Ctrl Pts',(1.40609737281374,-0.666234863082336,
4.39597761722625));
#284011=CARTESIAN_POINT('Ctrl Pts',(1.38967564211849,-0.699842805111789,
4.39340973176953));
#284012=CARTESIAN_POINT('Ctrl Pts',(1.3652437621685,-0.745586380482985,
4.38979084911775));
#284013=CARTESIAN_POINT('Ctrl Pts',(1.35824998157003,-0.758252295503872,
4.38877526115647));
#284014=CARTESIAN_POINT('Ctrl Pts',(1.34664224445713,-0.778598189148943,
4.38712075006774));
#284015=CARTESIAN_POINT('Ctrl Pts',(1.34213671889124,-0.786339301073113,
4.3864857347491));
#284016=CARTESIAN_POINT('Ctrl Pts',(1.33256359596594,-0.802465259621048,
4.38515103450201));
#284017=CARTESIAN_POINT('Ctrl Pts',(1.32748314939306,-0.810841976073724,
4.38445090319791));
#284018=CARTESIAN_POINT('Ctrl Pts',(1.31513619994485,-0.8307727211485,4.38276835089282));
#284019=CARTESIAN_POINT('Ctrl Pts',(1.30779620016053,-0.842280010065659,
4.38178325536281));
#284020=CARTESIAN_POINT('Ctrl Pts',(1.28146944860901,-0.88237990110766,
4.37830107286448));
#284021=CARTESIAN_POINT('Ctrl Pts',(1.2616900172202,-0.910437365310724,
4.37577472813087));
#284022=CARTESIAN_POINT('Ctrl Pts',(1.20965453380994,-0.979295287330299,
4.36933897560383));
#284023=CARTESIAN_POINT('Ctrl Pts',(1.17625191142208,-1.01917311450902,
4.36539045152064));
#284024=CARTESIAN_POINT('Ctrl Pts',(1.10256354103288,-1.09868922755383,
4.35706004555156));
#284025=CARTESIAN_POINT('Ctrl Pts',(1.06198568596299,-1.13795887084703,
4.3526756896223));
#284026=CARTESIAN_POINT('Ctrl Pts',(0.96323964097279,-1.22363023401444,
4.34254483831109));
#284027=CARTESIAN_POINT('Ctrl Pts',(0.903689484415122,-1.26824662566834,
4.33681767072797));
#284028=CARTESIAN_POINT('Ctrl Pts',(0.831741632032371,-1.3145005784754,
4.3304906127914));
#284029=CARTESIAN_POINT('Ctrl Pts',(0.822246535638912,-1.32046074051187,
4.32966687773631));
#284030=CARTESIAN_POINT('Ctrl Pts',(0.807336141228614,-1.32959692896331,
4.32839176902863));
#284031=CARTESIAN_POINT('Ctrl Pts',(0.801964884730938,-1.3328435638973,
4.3279361065657));
#284032=CARTESIAN_POINT('Ctrl Pts',(0.792397286878072,-1.33854788326975,
4.327131156268));
#284033=CARTESIAN_POINT('Ctrl Pts',(0.788209011774074,-1.34101843795417,
4.3267810613468));
#284034=CARTESIAN_POINT('Ctrl Pts',(0.778047435383273,-1.34694843346628,
4.32593707413112));
#284035=CARTESIAN_POINT('Ctrl Pts',(0.77206259851507,-1.35038781205101,
4.32544446595661));
#284036=CARTESIAN_POINT('Ctrl Pts',(0.753290529527033,-1.36101018635478,
4.32391262502627));
#284037=CARTESIAN_POINT('Ctrl Pts',(0.740424020960603,-1.36805250608677,
4.32288179725083));
#284038=CARTESIAN_POINT('Ctrl Pts',(0.671696510136271,-1.40441589329085,
4.31746553649999));
#284039=CARTESIAN_POINT('Ctrl Pts',(0.614183538120879,-1.43050365102664,
4.31324353211598));
#284040=CARTESIAN_POINT('Ctrl Pts',(0.449946670513132,-1.49326268362635,
4.30160561228447));
#284041=CARTESIAN_POINT('Ctrl Pts',(0.340600440525213,-1.52193152330799,
4.29430114203787));
#284042=CARTESIAN_POINT('Ctrl Pts',(0.19466370851215,-1.54366437774777,
4.28427200773025));
#284043=CARTESIAN_POINT('Ctrl Pts',(0.160049236145983,-1.5476361351099,
4.28187573887825));
#284044=CARTESIAN_POINT('Ctrl Pts',(0.111264604276624,-1.55157972466035,
4.27845801689116));
#284045=CARTESIAN_POINT('Ctrl Pts',(0.0971821213163001,-1.55252538347587,
4.27746676305576));
#284046=CARTESIAN_POINT('Ctrl Pts',(0.0733188511735155,-1.55380189449793,
4.27577817582622));
#284047=CARTESIAN_POINT('Ctrl Pts',(0.063544078102719,-1.55423232608985,
4.27508398960464));
#284048=CARTESIAN_POINT('Ctrl Pts',(0.0437556836804373,-1.55491672392505,
4.27367324633951));
#284049=CARTESIAN_POINT('Ctrl Pts',(0.0337423842981061,-1.55516623581518,
4.27295658361185));
#284050=CARTESIAN_POINT('Ctrl Pts',(0.00893333831269328,-1.55554471687107,
4.27117368451881));
#284051=CARTESIAN_POINT('Ctrl Pts',(-0.00586288286008003,-1.55555931072095,
4.27010392993936));
#284052=CARTESIAN_POINT('Ctrl Pts',(-0.0636815657953153,-1.5547914273841,
4.26589722066373));
#284053=CARTESIAN_POINT('Ctrl Pts',(-0.106660067298875,-1.55243508516749,
4.2627122282642));
#284054=CARTESIAN_POINT('Ctrl Pts',(-0.223262499703083,-1.54117760251042,
4.25390780083761));
#284055=CARTESIAN_POINT('Ctrl Pts',(-0.296431787630441,-1.52879055183406,
4.24819956395364));
#284056=CARTESIAN_POINT('Ctrl Pts',(-0.457770527266698,-1.489457014717,
4.23532677917162));
#284057=CARTESIAN_POINT('Ctrl Pts',(-0.545009895248322,-1.45979564473976,
4.22816388178082));
#284058=CARTESIAN_POINT('Ctrl Pts',(-0.642344017658711,-1.41675098988497,
4.22024337093766));
#284059=CARTESIAN_POINT('Ctrl Pts',(-0.655482707524068,-1.41072026433852,
4.21917608446682));
#284060=CARTESIAN_POINT('Ctrl Pts',(-0.674821472912216,-1.40151513998986,
4.21760990985733));
#284061=CARTESIAN_POINT('Ctrl Pts',(-0.681086930064984,-1.39848107123724,
4.21710324422117));
#284062=CARTESIAN_POINT('Ctrl Pts',(-0.692159857057123,-1.39302690067074,
4.21620942126707));
#284063=CARTESIAN_POINT('Ctrl Pts',(-0.696975383947429,-1.3906237920375,
4.21582126475855));
#284064=CARTESIAN_POINT('Ctrl Pts',(-0.707541417526832,-1.38528231419232,
4.21497084359791));
#284065=CARTESIAN_POINT('Ctrl Pts',(-0.713286189218603,-1.3823330871426,
4.21450925731602));
#284066=CARTESIAN_POINT('Ctrl Pts',(-0.73000429054705,-1.37361844510649,
4.21316779226677));
#284067=CARTESIAN_POINT('Ctrl Pts',(-0.740927591673059,-1.36775737114848,
4.21229360323874));
#284068=CARTESIAN_POINT('Ctrl Pts',(-0.765957179094942,-1.3539394725189,
4.21029306445964));
#284069=CARTESIAN_POINT('Ctrl Pts',(-0.78001180952454,-1.34589157065514,
4.20917163470705));
#284070=CARTESIAN_POINT('Ctrl Pts',(-0.828063660513498,-1.31737070606209,
4.20533504707773));
#284071=CARTESIAN_POINT('Ctrl Pts',(-0.86140348088047,-1.29581615369214,
4.20266854238898));
#284072=CARTESIAN_POINT('Ctrl Pts',(-0.973731308771008,-1.21694149295012,
4.19353831862755));
#284073=CARTESIAN_POINT('Ctrl Pts',(-1.04812538270314,-1.1534872636348,
4.18721573433572));
#284074=CARTESIAN_POINT('Ctrl Pts',(-1.15473183470917,-1.04367278586619,
4.17698003211608));
#284075=CARTESIAN_POINT('Ctrl Pts',(-1.19121625059556,-1.00182896218303,
4.17321484360926));
#284076=CARTESIAN_POINT('Ctrl Pts',(-1.23559210044131,-0.945075131502092,
4.16820579803392));
#284077=CARTESIAN_POINT('Ctrl Pts',(-1.24558950565337,-0.931859211164798,
4.16704597325141));
#284078=CARTESIAN_POINT('Ctrl Pts',(-1.26150635746857,-0.910104298016887,
4.16514578395686));
#284079=CARTESIAN_POINT('Ctrl Pts',(-1.26755492288166,-0.901661040089997,
4.1644104608806));
#284080=CARTESIAN_POINT('Ctrl Pts',(-1.2790780776537,-0.885230633991515,
4.16298328801776));
#284081=CARTESIAN_POINT('Ctrl Pts',(-1.28456354424657,-0.877251672593394,
4.16229189751894));
#284082=CARTESIAN_POINT('Ctrl Pts',(-1.29721848882559,-0.858471031199396,
4.16066809946631));
#284083=CARTESIAN_POINT('Ctrl Pts',(-1.30432802803756,-0.847630046365558,
4.15973349516718));
#284084=CARTESIAN_POINT('Ctrl Pts',(-1.32739575439279,-0.811477698157759,
4.15662487147019));
#284085=CARTESIAN_POINT('Ctrl Pts',(-1.3427582095641,-0.785796223939521,
4.15442935754016));
#284086=CARTESIAN_POINT('Ctrl Pts',(-1.41963045210483,-0.648445274079435,
4.14274517768156));
#284087=CARTESIAN_POINT('Ctrl Pts',(-1.46797072736294,-0.52998375989957,
4.1328079311325));
#284088=CARTESIAN_POINT('Ctrl Pts',(-1.51438303316102,-0.358774672734246,
4.11909872449242));
#284089=CARTESIAN_POINT('Ctrl Pts',(-1.52512344569801,-0.309958979350414,
4.11526721089691));
#284090=CARTESIAN_POINT('Ctrl Pts',(-1.53660480328221,-0.242424902474009,
4.11013593563019));
#284091=CARTESIAN_POINT('Ctrl Pts',(-1.53938594642668,-0.224087354409639,
4.10875963379184));
#284092=CARTESIAN_POINT('Ctrl Pts',(-1.54276828708144,-0.198735207534343,
4.10688406701267));
#284093=CARTESIAN_POINT('Ctrl Pts',(-1.54365072219694,-0.191760588309655,
4.10637090949911));
#284094=CARTESIAN_POINT('Ctrl Pts',(-1.54508557325774,-0.179767371657291,
4.10549363458369));
#284095=CARTESIAN_POINT('Ctrl Pts',(-1.54566088781971,-0.174751705128819,
4.10512828784796));
#284096=CARTESIAN_POINT('Ctrl Pts',(-1.54676072045196,-0.164732605284701,
4.10440167023776));
#284097=CARTESIAN_POINT('Ctrl Pts',(-1.54728540311942,-0.159729272273086,
4.10404040022286));
#284098=CARTESIAN_POINT('Ctrl Pts',(-1.54834500636688,-0.149129461051616,
4.10327822400533));
#284099=CARTESIAN_POINT('Ctrl Pts',(-1.54887388244373,-0.143532413621816,
4.1028776514708));
#284100=CARTESIAN_POINT('Ctrl Pts',(-1.55007154318263,-0.130079294145007,
4.1019190803938));
#284101=CARTESIAN_POINT('Ctrl Pts',(-1.55071097441446,-0.122220669987757,
4.10136260885961));
#284102=CARTESIAN_POINT('Ctrl Pts',(-1.55407073087199,-0.0766445852303563,
4.09815370387891));
#284103=CARTESIAN_POINT('Ctrl Pts',(-1.55547489607258,-0.0388398935252902,
4.09556465134092));
#284104=CARTESIAN_POINT('Ctrl Pts',(-1.55549966639403,-0.00101874828225496,
4.09301352418007));
#284105=CARTESIAN_POINT('',(-1.55331871380611,-0.000780328647907862,3.39405694879054));
#284106=CARTESIAN_POINT('Ctrl Pts',(-1.55331871380611,-0.000780328647907862,
3.39405694879054));
#284107=CARTESIAN_POINT('Ctrl Pts',(-1.55425844430069,-0.210990804352394,
3.40906388991245));
#284108=CARTESIAN_POINT('Ctrl Pts',(-1.41654551139588,-0.939168704500731,
3.4611329709781));
#284109=CARTESIAN_POINT('Ctrl Pts',(-0.308692884081366,-1.81269447386996,
3.55026419198746));
#284110=CARTESIAN_POINT('Ctrl Pts',(1.35606994996762,-1.24186426112907,
3.66145061181863));
#284111=CARTESIAN_POINT('Ctrl Pts',(1.77861387826841,0.466567491694538,
3.77263703164979));
#284112=CARTESIAN_POINT('Ctrl Pts',(0.571870330903418,1.74760318061885,
3.88382345148095));
#284113=CARTESIAN_POINT('Ctrl Pts',(-1.09574000028678,1.43940039381927,
3.99096285577571));
#284114=CARTESIAN_POINT('Ctrl Pts',(-1.55401186045024,0.458497813133281,
4.06104012012673));
#284115=CARTESIAN_POINT('Ctrl Pts',(-1.55731595967384,-0.000935870630138446,
4.09405524453403));
#284116=CARTESIAN_POINT('',(-1.5555004206443,-7.0880047456861E-5,1.99259207059789));
#284117=CARTESIAN_POINT('Ctrl Pts',(-1.55549984885979,-0.000685709247415389,
3.39531142154411));
#284118=CARTESIAN_POINT('Ctrl Pts',(-1.5555077357725,0.0172053890135179,
3.39408737174109));
#284119=CARTESIAN_POINT('Ctrl Pts',(-1.55520695194502,0.0350947961981444,
3.39285526377583));
#284120=CARTESIAN_POINT('Ctrl Pts',(-1.55410834920964,0.0673345056559161,
3.39061728115537));
#284121=CARTESIAN_POINT('Ctrl Pts',(-1.55342009261955,0.0816865283590325,
3.3896147425859));
#284122=CARTESIAN_POINT('Ctrl Pts',(-1.55194765173723,0.105492581273357,
3.38794029322772));
#284123=CARTESIAN_POINT('Ctrl Pts',(-1.55127561405159,0.114952862421567,
3.38727186188798));
#284124=CARTESIAN_POINT('Ctrl Pts',(-1.54978728902936,0.133502364051424,
3.38595496162361));
#284125=CARTESIAN_POINT('Ctrl Pts',(-1.5489774419519,0.142591725889808,
3.38530671933281));
#284126=CARTESIAN_POINT('Ctrl Pts',(-1.54708650425045,0.161892012093361,
3.3839236964601));
#284127=CARTESIAN_POINT('Ctrl Pts',(-1.5459841945952,0.172100365817622,
3.38318827863173));
#284128=CARTESIAN_POINT('Ctrl Pts',(-1.54290446737667,0.198197932717347,
3.38129779779555));
#284129=CARTESIAN_POINT('Ctrl Pts',(-1.5407826724218,0.214068532688995,
3.38013825332279));
#284130=CARTESIAN_POINT('Ctrl Pts',(-1.5309765050801,0.279687368293068,
3.37530117728549));
#284131=CARTESIAN_POINT('Ctrl Pts',(-1.52112534256817,0.329075583013826,
3.37155682340179));
#284132=CARTESIAN_POINT('Ctrl Pts',(-1.4780791946597,0.500954882524119,
3.35815488130927));
#284133=CARTESIAN_POINT('Ctrl Pts',(-1.43232654386424,0.61976506444484,
3.34816705783662));
#284134=CARTESIAN_POINT('Ctrl Pts',(-1.35493077184496,0.764960077943228,
3.33560746827639));
#284135=CARTESIAN_POINT('Ctrl Pts',(-1.33599318579173,0.797573866895534,
3.33276516987259));
#284136=CARTESIAN_POINT('Ctrl Pts',(-1.31070573240019,0.837690369230111,
3.32926984236883));
#284137=CARTESIAN_POINT('Ctrl Pts',(-1.30544700914496,0.84586215831427,
3.32855790040048));
#284138=CARTESIAN_POINT('Ctrl Pts',(-1.29688058081125,0.858903749159421,
3.32742245103605));
#284139=CARTESIAN_POINT('Ctrl Pts',(-1.2936213197627,0.863804824812217,
3.32699591985836));
#284140=CARTESIAN_POINT('Ctrl Pts',(-1.28727696957423,0.873228620293653,
3.32617630295604));
#284141=CARTESIAN_POINT('Ctrl Pts',(-1.28419572108313,0.877753707409507,
3.32578299257696));
#284142=CARTESIAN_POINT('Ctrl Pts',(-1.27726305247355,0.887820299455287,
3.32490837618776));
#284143=CARTESIAN_POINT('Ctrl Pts',(-1.27339927968535,0.893353271823013,
3.32442788908106));
#284144=CARTESIAN_POINT('Ctrl Pts',(-1.25987182350577,0.912458670892332,
3.3227689086591));
#284145=CARTESIAN_POINT('Ctrl Pts',(-1.25002576769631,0.925901439743128,
3.32160188723255));
#284146=CARTESIAN_POINT('Ctrl Pts',(-1.16876716536299,1.0331837407003,3.31226688519429));
#284147=CARTESIAN_POINT('Ctrl Pts',(-1.08710138384595,1.11879571183531,
3.30466126401129));
#284148=CARTESIAN_POINT('Ctrl Pts',(-0.954699006467354,1.22926745527058,
3.29326694676563));
#284149=CARTESIAN_POINT('Ctrl Pts',(-0.911063097020174,1.26194769863122,
3.28963884513134));
#284150=CARTESIAN_POINT('Ctrl Pts',(-0.845813540617006,1.30566411336301,
3.2842997247697));
#284151=CARTESIAN_POINT('Ctrl Pts',(-0.825514625594606,1.3185919866123,
3.2826502510854));
#284152=CARTESIAN_POINT('Ctrl Pts',(-0.788293211595726,1.34110097706447,
3.27963898522203));
#284153=CARTESIAN_POINT('Ctrl Pts',(-0.771475211539229,1.35084564538847,
3.2782831394788));
#284154=CARTESIAN_POINT('Ctrl Pts',(-0.744864579569112,1.36560532348347,
3.27614258959337));
#284155=CARTESIAN_POINT('Ctrl Pts',(-0.735193438539752,1.37083614563701,
3.27536561744406));
#284156=CARTESIAN_POINT('Ctrl Pts',(-0.717019110824374,1.38041843997527,
3.27390685339807));
#284157=CARTESIAN_POINT('Ctrl Pts',(-0.708529673797578,1.38479499153461,
3.2732259897987));
#284158=CARTESIAN_POINT('Ctrl Pts',(-0.689426921675288,1.39442137276481,
3.27169483030861));
#284159=CARTESIAN_POINT('Ctrl Pts',(-0.678792987559742,1.39962870461525,
3.27084309613251));
#284160=CARTESIAN_POINT('Ctrl Pts',(-0.647451473830296,1.41453515094935,
3.26833396158715));
#284161=CARTESIAN_POINT('Ctrl Pts',(-0.626589068691735,1.42389927317071,
3.26666522174483));
#284162=CARTESIAN_POINT('Ctrl Pts',(-0.47704514450221,1.48709942448545,
3.25470739460431));
#284163=CARTESIAN_POINT('Ctrl Pts',(-0.341861119003655,1.52386084678205,
3.24383361008517));
#284164=CARTESIAN_POINT('Ctrl Pts',(-0.162917856204241,1.54748974369895,
3.22989149622495));
#284165=CARTESIAN_POINT('Ctrl Pts',(-0.122004647536606,1.55125177025516,
3.22674017747705));
#284166=CARTESIAN_POINT('Ctrl Pts',(-0.0644585428165128,1.55425201036867,
3.22239485025482));
#284167=CARTESIAN_POINT('Ctrl Pts',(-0.0479156046288272,1.55484994813515,
3.221155811736));
#284168=CARTESIAN_POINT('Ctrl Pts',(-0.0187626979887062,1.55543791491242,
3.21899352337906));
#284169=CARTESIAN_POINT('Ctrl Pts',(-0.00615669853451052,1.55553889957576,
3.21806551281425));
#284170=CARTESIAN_POINT('Ctrl Pts',(0.0129498160357867,1.55545967643265,
3.21667088918707));
#284171=CARTESIAN_POINT('Ctrl Pts',(0.0194498973300509,1.55539197900284,
3.21619852859483));
#284172=CARTESIAN_POINT('Ctrl Pts',(0.0313273775501246,1.55519380619296,
3.21533944719597));
#284173=CARTESIAN_POINT('Ctrl Pts',(0.0367046324515826,1.55507618824834,
3.21495206074781));
#284174=CARTESIAN_POINT('Ctrl Pts',(0.0489860842457927,1.55474381249586,
3.21407073633723));
#284175=CARTESIAN_POINT('Ctrl Pts',(0.055889576398885,1.55451095816053,
3.21357780092795));
#284176=CARTESIAN_POINT('Ctrl Pts',(0.0774708550021125,1.55363906776375,
3.21204387199123));
#284177=CARTESIAN_POINT('Ctrl Pts',(0.092141811009324,1.55283805147473,
3.21101131614066));
#284178=CARTESIAN_POINT('Ctrl Pts',(0.199493253137341,1.54544991648361,
3.20351604297488));
#284179=CARTESIAN_POINT('Ctrl Pts',(0.291442398205,1.53077733632387,3.19741820744105));
#284180=CARTESIAN_POINT('Ctrl Pts',(0.475133818724348,1.48430058569984,
3.18494937272082));
#284181=CARTESIAN_POINT('Ctrl Pts',(0.566307245292282,1.45196201879497,
3.17859810409414));
#284182=CARTESIAN_POINT('Ctrl Pts',(0.677369819467039,1.40050704327046,
3.17019387149855));
#284183=CARTESIAN_POINT('Ctrl Pts',(0.700572678976904,1.38904558568149,
3.168399869624));
#284184=CARTESIAN_POINT('Ctrl Pts',(0.734333446113561,1.37130777567308,
3.16572629846264));
#284185=CARTESIAN_POINT('Ctrl Pts',(0.745120997255188,1.36547622088822,
3.16486226758082));
#284186=CARTESIAN_POINT('Ctrl Pts',(0.764219184268598,1.35485838378746,
3.16331448402803));
#284187=CARTESIAN_POINT('Ctrl Pts',(0.772556723442959,1.35012158832192,
3.16263252609911));
#284188=CARTESIAN_POINT('Ctrl Pts',(0.790121664149505,1.33992646662185,
3.16118220624798));
#284189=CARTESIAN_POINT('Ctrl Pts',(0.799337457735834,1.33444924897875,
3.16041318603725));
#284190=CARTESIAN_POINT('Ctrl Pts',(0.823991568008839,1.31944956363078,
3.1583335729272));
#284191=CARTESIAN_POINT('Ctrl Pts',(0.839320718820421,1.30975185982128,
3.15701662268246));
#284192=CARTESIAN_POINT('Ctrl Pts',(0.933575167464377,1.2477893395441,3.14876533555377));
#284193=CARTESIAN_POINT('Ctrl Pts',(1.0077477123538,1.18868804963577,3.14157270549623));
#284194=CARTESIAN_POINT('Ctrl Pts',(1.13132734685638,1.0702955958185,3.12834476336232));
#284195=CARTESIAN_POINT('Ctrl Pts',(1.18259616088848,1.01336122102882,3.12237405607558));
#284196=CARTESIAN_POINT('Ctrl Pts',(1.25352969060025,0.921838588373931,
3.11352505338146));
#284197=CARTESIAN_POINT('Ctrl Pts',(1.27640936691958,0.889889209922782,
3.11056017698075));
#284198=CARTESIAN_POINT('Ctrl Pts',(1.30347669775379,0.84889663559047,3.10693843966159));
#284199=CARTESIAN_POINT('Ctrl Pts',(1.30881877140536,0.840636923102079,
3.10621761204142));
#284200=CARTESIAN_POINT('Ctrl Pts',(1.31724561325137,0.827332577136293,
3.10507142547053));
#284201=CARTESIAN_POINT('Ctrl Pts',(1.32038048605731,0.822320238110777,
3.10464294449875));
#284202=CARTESIAN_POINT('Ctrl Pts',(1.32635609051508,0.812643583401632,
3.10382231457011));
#284203=CARTESIAN_POINT('Ctrl Pts',(1.32920093092555,0.807982028799622,
3.10342991830714));
#284204=CARTESIAN_POINT('Ctrl Pts',(1.33547792592171,0.797573672101529,
3.10256006181482));
#284205=CARTESIAN_POINT('Ctrl Pts',(1.33889769904679,0.791819429466348,
3.10208338971987));
#284206=CARTESIAN_POINT('Ctrl Pts',(1.34893681546118,0.774676212593677,
3.1006752097505));
#284207=CARTESIAN_POINT('Ctrl Pts',(1.35544895306677,0.763224692712184,
3.09975007237662));
#284208=CARTESIAN_POINT('Ctrl Pts',(1.40725614898601,0.669367257532846,
3.09228123956157));
#284209=CARTESIAN_POINT('Ctrl Pts',(1.44514541329273,0.583079931158479,
3.08611387740205));
#284210=CARTESIAN_POINT('Ctrl Pts',(1.50927023125192,0.391569133807421,
3.07282379119534));
#284211=CARTESIAN_POINT('Ctrl Pts',(1.5327867362558,0.285978395670083,3.06571743832726));
#284212=CARTESIAN_POINT('Ctrl Pts',(1.54730815522713,0.160492373460545,
3.05695976396918));
#284213=CARTESIAN_POINT('Ctrl Pts',(1.54910203369279,0.142137849184999,
3.05567191206115));
#284214=CARTESIAN_POINT('Ctrl Pts',(1.55142717473284,0.113005690679382,
3.05361474084362));
#284215=CARTESIAN_POINT('Ctrl Pts',(1.55217337719482,0.102246570581569,
3.05285216620679));
#284216=CARTESIAN_POINT('Ctrl Pts',(1.55337090001753,0.0819196544109911,
3.051405708391));
#284217=CARTESIAN_POINT('Ctrl Pts',(1.55384584682706,0.0723537113672053,
3.05072260013752));
#284218=CARTESIAN_POINT('Ctrl Pts',(1.55472297659819,0.0506402257133242,
3.04916628665561));
#284219=CARTESIAN_POINT('Ctrl Pts',(1.55507117954116,0.0384912638372372,
3.04829143308399));
#284220=CARTESIAN_POINT('Ctrl Pts',(1.55560764351462,0.0068148427851182,
3.04599920135026));
#284221=CARTESIAN_POINT('Ctrl Pts',(1.55557059610145,-0.0127137285137947,
3.0445749298612));
#284222=CARTESIAN_POINT('Ctrl Pts',(1.55271382631048,-0.150534866323173,
3.03444082460383));
#284223=CARTESIAN_POINT('Ctrl Pts',(1.53677191627025,-0.268146328084544,
3.0253194534284));
#284224=CARTESIAN_POINT('Ctrl Pts',(1.48753633125281,-0.462067242021094,
3.00980268627363));
#284225=CARTESIAN_POINT('Ctrl Pts',(1.46118382423208,-0.539643681000942,
3.00347048282605));
#284226=CARTESIAN_POINT('Ctrl Pts',(1.42402474966382,-0.626005362658659,
2.99650394246048));
#284227=CARTESIAN_POINT('Ctrl Pts',(1.4190690451512,-0.63715953379422,2.99560597781891));
#284228=CARTESIAN_POINT('Ctrl Pts',(1.41130761331136,-0.654088879959099,
2.99424709185941));
#284229=CARTESIAN_POINT('Ctrl Pts',(1.40859671346612,-0.659906618434287,
2.99378084386519));
#284230=CARTESIAN_POINT('Ctrl Pts',(1.40354495235637,-0.67057499291413,
2.99292742251321));
#284231=CARTESIAN_POINT('Ctrl Pts',(1.40121487646781,-0.675430326566563,
2.99253964487023));
#284232=CARTESIAN_POINT('Ctrl Pts',(1.39584331010944,-0.686475978650507,
2.99165881074539));
#284233=CARTESIAN_POINT('Ctrl Pts',(1.39278581615823,-0.692658278493809,
2.99116674498264));
#284234=CARTESIAN_POINT('Ctrl Pts',(1.38317192115517,-0.71177665429668,
2.98964735041963));
#284235=CARTESIAN_POINT('Ctrl Pts',(1.37647543170785,-0.724641976812031,
2.98862817527424));
#284236=CARTESIAN_POINT('Ctrl Pts',(1.3254566038435,-0.81939950202934,2.98113180811487));
#284237=CARTESIAN_POINT('Ctrl Pts',(1.2740342114712,-0.897269485545784,
2.97502141484609));
#284238=CARTESIAN_POINT('Ctrl Pts',(1.15585714585161,-1.04539860130768,
2.96255166626708));
#284239=CARTESIAN_POINT('Ctrl Pts',(1.08890652164362,-1.11496358497814,
2.9562121773926));
#284240=CARTESIAN_POINT('Ctrl Pts',(0.996361347182489,-1.19478612902391,
2.94782092565125));
#284241=CARTESIAN_POINT('Ctrl Pts',(0.976349242542227,-1.21119439063923,
2.9460269529908));
#284242=CARTESIAN_POINT('Ctrl Pts',(0.946264435612997,-1.23463121686905,
2.94335341705531));
#284243=CARTESIAN_POINT('Ctrl Pts',(0.936502176574742,-1.24205244724363,
2.94248939157933));
#284244=CARTESIAN_POINT('Ctrl Pts',(0.918951569554182,-1.25506980458146,
2.94094161401569));
#284245=CARTESIAN_POINT('Ctrl Pts',(0.911197202413649,-1.26071085199513,
2.940259656617));
#284246=CARTESIAN_POINT('Ctrl Pts',(0.89466406161663,-1.27250595202141,
2.93880933399393));
#284247=CARTESIAN_POINT('Ctrl Pts',(0.885872866725031,-1.27864163642749,
2.93804031044704));
#284248=CARTESIAN_POINT('Ctrl Pts',(0.862038411275602,-1.29491275392559,
2.93596067851845));
#284249=CARTESIAN_POINT('Ctrl Pts',(0.846880549033466,-1.30487644882268,
2.93464371259216));
#284250=CARTESIAN_POINT('Ctrl Pts',(0.751916632796548,-1.36494729810438,
2.92642380692789));
#284251=CARTESIAN_POINT('Ctrl Pts',(0.66788293820132,-1.40797233920335,
2.91926510518129));
#284252=CARTESIAN_POINT('Ctrl Pts',(0.512984223212042,-1.47027944405818,
2.90636159479174));
#284253=CARTESIAN_POINT('Ctrl Pts',(0.443657067009222,-1.49266309939074,
2.90068624594157));
#284254=CARTESIAN_POINT('Ctrl Pts',(0.344920027935585,-1.51705241777078,
2.89289475474026));
#284255=CARTESIAN_POINT('Ctrl Pts',(0.3166329020955,-1.52320769413931,2.89069570854083));
#284256=CARTESIAN_POINT('Ctrl Pts',(0.269408842786897,-1.53211107610444,
2.88709520039433));
#284257=CARTESIAN_POINT('Ctrl Pts',(0.250564061370017,-1.53530557624678,
2.885676905425));
#284258=CARTESIAN_POINT('Ctrl Pts',(0.224088845984145,-1.53929306025271,
2.88371441088272));
#284259=CARTESIAN_POINT('Ctrl Pts',(0.216505050316037,-1.54037803995553,
2.88315569828781));
#284260=CARTESIAN_POINT('Ctrl Pts',(0.203497443583866,-1.54214101533942,
2.88220364259416));
#284261=CARTESIAN_POINT('Ctrl Pts',(0.198077583467954,-1.54284652370461,
2.88180880896478));
#284262=CARTESIAN_POINT('Ctrl Pts',(0.186653960671362,-1.5442723557932,
2.88098062801231));
#284263=CARTESIAN_POINT('Ctrl Pts',(0.180649584633809,-1.54498625910023,
2.88054763449921));
#284264=CARTESIAN_POINT('Ctrl Pts',(0.164253699734272,-1.54683879148834,
2.87937118997468));
#284265=CARTESIAN_POINT('Ctrl Pts',(0.153854396828151,-1.54790773789047,
2.87863148498996));
#284266=CARTESIAN_POINT('Ctrl Pts',(0.100578343193231,-1.55284176114131,
2.87487134683168));
#284267=CARTESIAN_POINT('Ctrl Pts',(0.057560981101624,-1.5550308845464,
2.87193239644717));
#284268=CARTESIAN_POINT('Ctrl Pts',(-0.0802648142245121,-1.55631607030563,
2.86266842176333));
#284269=CARTESIAN_POINT('Ctrl Pts',(-0.174919872631605,-1.54853705425943,
2.85652588245585));
#284270=CARTESIAN_POINT('Ctrl Pts',(-0.316172396099735,-1.52380414581933,
2.84701962467554));
#284271=CARTESIAN_POINT('Ctrl Pts',(-0.363640012103181,-1.51317858673255,
2.84376737223043));
#284272=CARTESIAN_POINT('Ctrl Pts',(-0.432120306244923,-1.49444081537108,
2.83892861385407));
#284273=CARTESIAN_POINT('Ctrl Pts',(-0.453580054199092,-1.48806799695418,
2.8373909016512));
#284274=CARTESIAN_POINT('Ctrl Pts',(-0.49238913721764,-1.4756255383185,
2.83456518407256));
#284275=CARTESIAN_POINT('Ctrl Pts',(-0.509782861052893,-1.46970717379218,
2.83328204508058));
#284276=CARTESIAN_POINT('Ctrl Pts',(-0.537200214639746,-1.45983292824975,
2.83123065555264));
#284277=CARTESIAN_POINT('Ctrl Pts',(-0.54729495559382,-1.45607845601704,
2.83046908341117));
#284278=CARTESIAN_POINT('Ctrl Pts',(-0.566293746814791,-1.44878687942852,
2.82902343861246));
#284279=CARTESIAN_POINT('Ctrl Pts',(-0.575205732336879,-1.44527173487081,
2.82834012994576));
#284280=CARTESIAN_POINT('Ctrl Pts',(-0.595371400568232,-1.43710175357742,
2.82678184912631));
#284281=CARTESIAN_POINT('Ctrl Pts',(-0.606603904317917,-1.43239667771578,
2.82590521241934));
#284282=CARTESIAN_POINT('Ctrl Pts',(-0.641104332128772,-1.41746654544249,
2.8231851082517));
#284283=CARTESIAN_POINT('Ctrl Pts',(-0.664176710399475,-1.40680323015921,
2.8213269021009));
#284284=CARTESIAN_POINT('Ctrl Pts',(-0.809354642963557,-1.33533918276053,
2.80937563272502));
#284285=CARTESIAN_POINT('Ctrl Pts',(-0.923259288802169,-1.2592710663737,
2.79873699650454));
#284286=CARTESIAN_POINT('Ctrl Pts',(-1.05639236039929,-1.14248664935626,
2.78505961495368));
#284287=CARTESIAN_POINT('Ctrl Pts',(-1.08595863090926,-1.11442131263817,
2.78193353458773));
#284288=CARTESIAN_POINT('Ctrl Pts',(-1.13128526157298,-1.06787655176599,
2.77703508152702));
#284289=CARTESIAN_POINT('Ctrl Pts',(-1.14777395513107,-1.05013417648145,
2.77522884340045));
#284290=CARTESIAN_POINT('Ctrl Pts',(-1.16940006563642,-1.02574553316021,
2.772834522134));
#284291=CARTESIAN_POINT('Ctrl Pts',(-1.1749068607934,-1.01943331769242,
2.77222253686207));
#284292=CARTESIAN_POINT('Ctrl Pts',(-1.18400778566412,-1.00882958889565,
2.77120768832872));
#284293=CARTESIAN_POINT('Ctrl Pts',(-1.18763016430407,-1.00456267720867,
2.7708028275426));
#284294=CARTESIAN_POINT('Ctrl Pts',(-1.19495567442057,-0.995838722501556,
2.76998233784379));
#284295=CARTESIAN_POINT('Ctrl Pts',(-1.19865706537833,-0.991380384941498,
2.76956682960448));
#284296=CARTESIAN_POINT('Ctrl Pts',(-1.20823410824967,-0.979712755133515,
2.76848896241829));
#284297=CARTESIAN_POINT('Ctrl Pts',(-1.21407028242947,-0.972471132479058,
2.76782935701626));
#284298=CARTESIAN_POINT('Ctrl Pts',(-1.23830678193464,-0.9418397841109,
2.76507628694547));
#284299=CARTESIAN_POINT('Ctrl Pts',(-1.2561002238835,-0.917975153863797,
2.76302090706399));
#284300=CARTESIAN_POINT('Ctrl Pts',(-1.32565405106469,-0.818876427995666,
2.75477523318911));
#284301=CARTESIAN_POINT('Ctrl Pts',(-1.37143103457888,-0.739660153392063,
2.74883143557132));
#284302=CARTESIAN_POINT('Ctrl Pts',(-1.44217690719349,-0.58780357603737,
2.73778741358157));
#284303=CARTESIAN_POINT('Ctrl Pts',(-1.46923468917447,-0.516463806544339,
2.73272630337374));
#284304=CARTESIAN_POINT('Ctrl Pts',(-1.49858463159502,-0.417780610220669,
2.72566456101477));
#284305=CARTESIAN_POINT('Ctrl Pts',(-1.50555047969143,-0.391936401843136,
2.72381048107124));
#284306=CARTESIAN_POINT('Ctrl Pts',(-1.51476830267501,-0.353852462789254,
2.72106456129103));
#284307=CARTESIAN_POINT('Ctrl Pts',(-1.5175459049029,-0.341744036951994,
2.72018953052219));
#284308=CARTESIAN_POINT('Ctrl Pts',(-1.52221393419901,-0.320214452702895,
2.71862948578663));
#284309=CARTESIAN_POINT('Ctrl Pts',(-1.52416267899098,-0.310806495407102,
2.71794637474028));
#284310=CARTESIAN_POINT('Ctrl Pts',(-1.52808424214077,-0.29094992063547,
2.71650132988515));
#284311=CARTESIAN_POINT('Ctrl Pts',(-1.53003731704036,-0.280497959797769,
2.71573880477576));
#284312=CARTESIAN_POINT('Ctrl Pts',(-1.53496036999895,-0.252569121602563,
2.71369577968821));
#284313=CARTESIAN_POINT('Ctrl Pts',(-1.53773891575525,-0.235060582158112,
2.71240930478595));
#284314=CARTESIAN_POINT('Ctrl Pts',(-1.55045903948366,-0.144987277893884,
2.70575909276499));
#284315=CARTESIAN_POINT('Ctrl Pts',(-1.55556419644944,-0.0718441416891806,
2.700246567499));
#284316=CARTESIAN_POINT('Ctrl Pts',(-1.55544729251868,0.0602401063572441,
2.69011614563084));
#284317=CARTESIAN_POINT('Ctrl Pts',(-1.5520539556199,0.119051021593196,
2.68554439663051));
#284318=CARTESIAN_POINT('Ctrl Pts',(-1.53663006928284,0.253314033008511,
2.67506863039724));
#284319=CARTESIAN_POINT('Ctrl Pts',(-1.52235890140084,0.328368855067391,
2.66918272575174));
#284320=CARTESIAN_POINT('Ctrl Pts',(-1.49972766186212,0.412945125829353,
2.66270585087675));
#284321=CARTESIAN_POINT('Ctrl Pts',(-1.49670266745485,0.423778104023444,
2.661879371346));
#284322=CARTESIAN_POINT('Ctrl Pts',(-1.49180463828114,0.440611691103604,
2.66060094330899));
#284323=CARTESIAN_POINT('Ctrl Pts',(-1.4900123593249,0.446635101540851,
2.66014467160318));
#284324=CARTESIAN_POINT('Ctrl Pts',(-1.48676890585172,0.457298703727562,
2.6593391976027));
#284325=CARTESIAN_POINT('Ctrl Pts',(-1.4853324634706,0.461943024553296,
2.65898918209753));
#284326=CARTESIAN_POINT('Ctrl Pts',(-1.48180726043102,0.473154284144634,
2.65814609308023));
#284327=CARTESIAN_POINT('Ctrl Pts',(-1.47969660477804,0.479714181876933,
2.6576542958845));
#284328=CARTESIAN_POINT('Ctrl Pts',(-1.47297701141184,0.500132237796858,
2.65612762176913));
#284329=CARTESIAN_POINT('Ctrl Pts',(-1.46821629617358,0.513940151752502,
2.65510106919811));
#284330=CARTESIAN_POINT('Ctrl Pts',(-1.4420601694539,0.58647138958084,2.64972954543161));
#284331=CARTESIAN_POINT('Ctrl Pts',(-1.41733209103663,0.64393931070276,
2.64554503686816));
#284332=CARTESIAN_POINT('Ctrl Pts',(-1.33926615848179,0.79891891723264,
2.63405552642741));
#284333=CARTESIAN_POINT('Ctrl Pts',(-1.27885508650744,0.8924314543115,2.62686123356053));
#284334=CARTESIAN_POINT('Ctrl Pts',(-1.18594555494629,1.00720237635497,
2.61684072213216));
#284335=CARTESIAN_POINT('Ctrl Pts',(-1.16188747570302,1.0348626129748,2.61432270622732));
#284336=CARTESIAN_POINT('Ctrl Pts',(-1.12707748545336,1.07213932308117,
2.61076285280136));
#284337=CARTESIAN_POINT('Ctrl Pts',(-1.117133854946,1.08249633355764,2.60975487567078));
#284338=CARTESIAN_POINT('Ctrl Pts',(-1.10077025343233,1.09907459922687,
2.60810937311888));
#284339=CARTESIAN_POINT('Ctrl Pts',(-1.09443735536906,1.10538092738372,
2.60747567038608));
#284340=CARTESIAN_POINT('Ctrl Pts',(-1.08103655137211,1.11849745316662,
2.60614095800911));
#284341=CARTESIAN_POINT('Ctrl Pts',(-1.07395785338585,1.12529600512105,
2.60543948094763));
#284342=CARTESIAN_POINT('Ctrl Pts',(-1.05681068718794,1.1414553918644,2.60374837890463));
#284343=CARTESIAN_POINT('Ctrl Pts',(-1.04668169252171,1.15075047344273,
2.60275600912948));
#284344=CARTESIAN_POINT('Ctrl Pts',(-1.01033311566897,1.18322954729875,
2.59921682805568));
#284345=CARTESIAN_POINT('Ctrl Pts',(-0.983457599414899,1.20565996630623,
2.5966394620104));
#284346=CARTESIAN_POINT('Ctrl Pts',(-0.913634231946479,1.26004611805021,
2.59003554245133));
#284347=CARTESIAN_POINT('Ctrl Pts',(-0.869753454586762,1.29072523469317,
2.58596712790093));
#284348=CARTESIAN_POINT('Ctrl Pts',(-0.803422174625369,1.33218018242369,
2.57995082056175));
#284349=CARTESIAN_POINT('Ctrl Pts',(-0.782152239793131,1.34477843965098,
2.57804081056432));
#284350=CARTESIAN_POINT('Ctrl Pts',(-0.674265484009122,1.40525446758967,
2.56846181834126));
#284351=CARTESIAN_POINT('Ctrl Pts',(-0.58351169985323,1.44529976761435,
2.56073222869852));
#284352=CARTESIAN_POINT('Ctrl Pts',(-0.476090414352199,1.48091849584164,
2.55231600459855));
#284353=CARTESIAN_POINT('Ctrl Pts',(-0.462558116849848,1.48520089561385,
2.55126883893735));
#284354=CARTESIAN_POINT('Ctrl Pts',(-0.442445494532603,1.49126411161708,
2.54973358684023));
#284355=CARTESIAN_POINT('Ctrl Pts',(-0.435909494093216,1.49318772560019,
2.54923795007389));
#284356=CARTESIAN_POINT('Ctrl Pts',(-0.424195283152444,1.49655186883216,
2.54835574290757));
#284357=CARTESIAN_POINT('Ctrl Pts',(-0.419022034265604,1.49800856869855,
2.54796827902632));
#284358=CARTESIAN_POINT('Ctrl Pts',(-0.407497936480815,1.5011891892828,
2.54710989502096));
#284359=CARTESIAN_POINT('Ctrl Pts',(-0.401143602755021,1.5028996521565,
2.54663974378318));
#284360=CARTESIAN_POINT('Ctrl Pts',(-0.382201824140878,1.50786971477544,
2.54524710669603));
#284361=CARTESIAN_POINT('Ctrl Pts',(-0.369583771644674,1.5110119708399,
2.54433098938682));
#284362=CARTESIAN_POINT('Ctrl Pts',(-0.280713189210971,1.53196337263462,
2.537950053831));
#284363=CARTESIAN_POINT('Ctrl Pts',(-0.203239994121519,1.54415303591295,
2.53275196510465));
#284364=CARTESIAN_POINT('Ctrl Pts',(-0.00458797329134095,1.56019027201008,
2.5196104806621));
#284365=CARTESIAN_POINT('Ctrl Pts',(0.116702262506103,1.555825071848,2.51172942870284));
#284366=CARTESIAN_POINT('Ctrl Pts',(0.255304162972019,1.5345264418901,2.50204770959194));
#284367=CARTESIAN_POINT('Ctrl Pts',(0.274294662811137,1.53124589740904,
2.50070721532751));
#284368=CARTESIAN_POINT('Ctrl Pts',(0.305081134146674,1.5253365711507,2.49850856577832));
#284369=CARTESIAN_POINT('Ctrl Pts',(0.316916412643089,1.52292157592523,
2.49765716165952));
#284370=CARTESIAN_POINT('Ctrl Pts',(0.338076413499842,1.51834652925434,
2.496123259775));
#284371=CARTESIAN_POINT('Ctrl Pts',(0.34741169198839,1.51623776270051,2.49544243290102));
#284372=CARTESIAN_POINT('Ctrl Pts',(0.367269598647034,1.51155900129803,
2.4939851115908));
#284373=CARTESIAN_POINT('Ctrl Pts',(0.377785980631142,1.50896498114537,
2.493207876223));
#284374=CARTESIAN_POINT('Ctrl Pts',(0.406344508247793,1.50160335146394,
2.4910818224862));
#284375=CARTESIAN_POINT('Ctrl Pts',(0.424328792285771,1.49662069483294,
2.48972614727725));
#284376=CARTESIAN_POINT('Ctrl Pts',(0.464112904334879,1.48482355276228,
2.48668827276499));
#284377=CARTESIAN_POINT('Ctrl Pts',(0.485860690893841,1.47785014809817,
2.48500127003085));
#284378=CARTESIAN_POINT('Ctrl Pts',(0.554863163920925,1.45403689020523,
2.47956263594423));
#284379=CARTESIAN_POINT('Ctrl Pts',(0.601456457976442,1.43539042299075,
2.4757582271719));
#284380=CARTESIAN_POINT('Ctrl Pts',(0.694898986650941,1.39264592092735,
2.46787209068947));
#284381=CARTESIAN_POINT('Ctrl Pts',(0.741591742530025,1.36835249869939,
2.46379071236233));
#284382=CARTESIAN_POINT('Ctrl Pts',(0.801748558382056,1.33306914501531,
2.45838254370962));
#284383=CARTESIAN_POINT('Ctrl Pts',(0.816390589839546,1.32415275192799,
2.45705400918685));
#284384=CARTESIAN_POINT('Ctrl Pts',(0.885058740395803,1.28076467279295,
2.45077228429649));
#284385=CARTESIAN_POINT('Ctrl Pts',(0.937074636785301,1.24321365575638,
2.44585893338128));
#284386=CARTESIAN_POINT('Ctrl Pts',(0.995232487775756,1.19549836943306,
2.44029521771209));
#284387=CARTESIAN_POINT('Ctrl Pts',(1.00375897998477,1.18834842747067,2.43947770530743));
#284388=CARTESIAN_POINT('Ctrl Pts',(1.01695968027796,1.17703543462833,2.43821012564714));
#284389=CARTESIAN_POINT('Ctrl Pts',(1.02168652594923,1.17293480299034,2.437755847137));
#284390=CARTESIAN_POINT('Ctrl Pts',(1.03004471355052,1.16559504685412,2.43695207678753));
#284391=CARTESIAN_POINT('Ctrl Pts',(1.03368565400222,1.16236736660693,2.43660179180238));
#284392=CARTESIAN_POINT('Ctrl Pts',(1.04247515713099,1.15450154304838,2.43575572143484));
#284393=CARTESIAN_POINT('Ctrl Pts',(1.04760795707743,1.14984600677477,2.43526123821138));
#284394=CARTESIAN_POINT('Ctrl Pts',(1.06361304437874,1.13513298420269,2.4337174082857));
#284395=CARTESIAN_POINT('Ctrl Pts',(1.07437330155477,1.12495406619094,2.43267665517642));
#284396=CARTESIAN_POINT('Ctrl Pts',(1.13118559941089,1.06965228880925,2.42715535032028));
#284397=CARTESIAN_POINT('Ctrl Pts',(1.17454943374723,1.02184760044184,2.42284529930123));
#284398=CARTESIAN_POINT('Ctrl Pts',(1.28776257538364,0.880276361759445,
2.41085367028134));
#284399=CARTESIAN_POINT('Ctrl Pts',(1.35019176636595,0.781152620464755,
2.40328474641407));
#284400=CARTESIAN_POINT('Ctrl Pts',(1.41428344615465,0.648325032257788,
2.39321923322024));
#284401=CARTESIAN_POINT('Ctrl Pts',(1.42680423993931,0.620284176525293,
2.39110057009331));
#284402=CARTESIAN_POINT('Ctrl Pts',(1.44310302604166,0.580672973156132,
2.38810574663187));
#284403=CARTESIAN_POINT('Ctrl Pts',(1.44758806243349,0.56939988788068,2.38725325082023));
#284404=CARTESIAN_POINT('Ctrl Pts',(1.45515380227828,0.549716171166069,
2.38576376958492));
#284405=CARTESIAN_POINT('Ctrl Pts',(1.45829462378703,0.541329143191026,
2.38512882029988));
#284406=CARTESIAN_POINT('Ctrl Pts',(1.46471952619258,0.523710756769226,
2.38379412137367));
#284407=CARTESIAN_POINT('Ctrl Pts',(1.4679891484409,0.514474585491307,2.38309392431404));
#284408=CARTESIAN_POINT('Ctrl Pts',(1.47560576324577,0.492294934418385,
2.3814109520692));
#284409=CARTESIAN_POINT('Ctrl Pts',(1.47986994425298,0.479324104288452,
2.38042549890981));
#284410=CARTESIAN_POINT('Ctrl Pts',(1.49426140604352,0.433524341763582,
2.37694053443858));
#284411=CARTESIAN_POINT('Ctrl Pts',(1.50347067842733,0.400419880560053,
2.37441170276013));
#284412=CARTESIAN_POINT('Ctrl Pts',(1.52386131966444,0.316445374706051,
2.36796780238964));
#284413=CARTESIAN_POINT('Ctrl Pts',(1.53359756216837,0.265270722382908,
2.36401348696345));
#284414=CARTESIAN_POINT('Ctrl Pts',(1.54840150330025,0.158540574057791,
2.35573327332648));
#284415=CARTESIAN_POINT('Ctrl Pts',(1.5530847935151,0.103002781284942,2.35140631493147));
#284416=CARTESIAN_POINT('Ctrl Pts',(1.55705900683752,-0.0275335522168997,
2.34128495902298));
#284417=CARTESIAN_POINT('Ctrl Pts',(1.5539277925416,-0.102478945719532,
2.33550989481253));
#284418=CARTESIAN_POINT('Ctrl Pts',(1.54413062484228,-0.18806042157606,
2.32913780045627));
#284419=CARTESIAN_POINT('Ctrl Pts',(1.54273407732375,-0.199192607245574,
2.32831341310625));
#284420=CARTESIAN_POINT('Ctrl Pts',(1.54036835215817,-0.216529449542107,
2.32703751539361));
#284421=CARTESIAN_POINT('Ctrl Pts',(1.53948187890611,-0.222744721809059,
2.32658170805749));
#284422=CARTESIAN_POINT('Ctrl Pts',(1.53784207805529,-0.233764060716008,
2.3257766334589));
#284423=CARTESIAN_POINT('Ctrl Pts',(1.53710384609906,-0.238570032796876,
2.32542655765306));
#284424=CARTESIAN_POINT('Ctrl Pts',(1.53526353409798,-0.250187403079162,
2.32458278504021));
#284425=CARTESIAN_POINT('Ctrl Pts',(1.53413865429954,-0.25699503887627,
2.32409037049015));
#284426=CARTESIAN_POINT('Ctrl Pts',(1.53048377052505,-0.278234329783161,
2.32255976414537));
#284427=CARTESIAN_POINT('Ctrl Pts',(1.527795054908,-0.292638386377204,2.321529958029));
#284428=CARTESIAN_POINT('Ctrl Pts',(1.51247974050745,-0.368710515476358,
2.31612441572394));
#284429=CARTESIAN_POINT('Ctrl Pts',(1.49632063215924,-0.429614799995563,
2.31191139501902));
#284430=CARTESIAN_POINT('Ctrl Pts',(1.44117882102562,-0.595984134309744,
2.30030913946422));
#284431=CARTESIAN_POINT('Ctrl Pts',(1.39440649916283,-0.698443136576814,
2.29303118518171));
#284432=CARTESIAN_POINT('Ctrl Pts',(1.3189907096299,-0.825279993650218,
2.28300485159366));
#284433=CARTESIAN_POINT('Ctrl Pts',(1.29994595318147,-0.854964187806847,
2.28057999181877));
#284434=CARTESIAN_POINT('Ctrl Pts',(1.27185405985485,-0.895638580607973,
2.27712856271953));
#284435=CARTESIAN_POINT('Ctrl Pts',(1.26363899684094,-0.907192195130692,
2.27613302945155));
#284436=CARTESIAN_POINT('Ctrl Pts',(1.25000789089061,-0.925818468415923,
2.27450222272955));
#284437=CARTESIAN_POINT('Ctrl Pts',(1.24468685447152,-0.932959909138211,
2.27387063408778));
#284438=CARTESIAN_POINT('Ctrl Pts',(1.23335462249982,-0.947899554690296,
2.27253571331624));
#284439=CARTESIAN_POINT('Ctrl Pts',(1.22733014337435,-0.955687135811766,
2.27183187833222));
#284440=CARTESIAN_POINT('Ctrl Pts',(1.21261249317965,-0.974343306852397,
2.27012601194322));
#284441=CARTESIAN_POINT('Ctrl Pts',(1.20384673886791,-0.985153259199103,
2.2691211138008));
#284442=CARTESIAN_POINT('Ctrl Pts',(1.17176637082182,-1.02364727816317,
2.26548168322839));
#284443=CARTESIAN_POINT('Ctrl Pts',(1.14763397031588,-1.05063126200674,
2.26281424143582));
#284444=CARTESIAN_POINT('Ctrl Pts',(1.08363814753125,-1.11735138489516,
2.25590806977828));
#284445=CARTESIAN_POINT('Ctrl Pts',(1.04252155941416,-1.15580854313394,
2.25162226449452));
#284446=CARTESIAN_POINT('Ctrl Pts',(0.958807850725194,-1.22600005716313,
2.24320608866604));
#284447=CARTESIAN_POINT('Ctrl Pts',(0.916486581412007,-1.25795101141336,
2.23908670700559));
#284448=CARTESIAN_POINT('Ctrl Pts',(0.813849181162596,-1.32750507491836,
2.22948365112596));
#284449=CARTESIAN_POINT('Ctrl Pts',(0.752414857500839,-1.36326611706069,
2.22402104690798));
#284450=CARTESIAN_POINT('Ctrl Pts',(0.678715557343776,-1.39966087814786,
2.21794115383653));
#284451=CARTESIAN_POINT('Ctrl Pts',(0.668632127924866,-1.40450577724835,
2.21711919550749));
#284452=CARTESIAN_POINT('Ctrl Pts',(0.652815819873923,-1.41189627001839,
2.21584623612641));
#284453=CARTESIAN_POINT('Ctrl Pts',(0.647118576021599,-1.41451656909695,
2.21539096846679));
#284454=CARTESIAN_POINT('Ctrl Pts',(0.636974679417972,-1.41910787537193,
2.21458635620258));
#284455=CARTESIAN_POINT('Ctrl Pts',(0.632534566482635,-1.42109251193333,
2.21423620848391));
#284456=CARTESIAN_POINT('Ctrl Pts',(0.621763302098159,-1.42584655391588,
2.21339163327394));
#284457=CARTESIAN_POINT('Ctrl Pts',(0.615422904301446,-1.42859464259952,
2.21289849500322));
#284458=CARTESIAN_POINT('Ctrl Pts',(0.595531579409114,-1.43705903921313,
2.21136327054586));
#284459=CARTESIAN_POINT('Ctrl Pts',(0.58191727851012,-1.44262568483293,
2.21032964235718));
#284460=CARTESIAN_POINT('Ctrl Pts',(0.509137048520994,-1.47118619296644,
2.20488391180023));
#284461=CARTESIAN_POINT('Ctrl Pts',(0.448677304091412,-1.49073806026603,
2.20063720684499));
#284462=CARTESIAN_POINT('Ctrl Pts',(0.276921853901774,-1.53487966169135,
2.18890085564967));
#284463=CARTESIAN_POINT('Ctrl Pts',(0.163888354734473,-1.55102564251602,
2.18152306847942));
#284464=CARTESIAN_POINT('Ctrl Pts',(0.0163931933713924,-1.55577932307457,
2.17148101105747));
#284465=CARTESIAN_POINT('Ctrl Pts',(-0.0173445752312792,-1.55576891756481,
2.1691586036353));
#284466=CARTESIAN_POINT('Ctrl Pts',(-0.0649586590946392,-1.55420532356505,
2.16583063974348));
#284467=CARTESIAN_POINT('Ctrl Pts',(-0.0788567690295112,-1.55356216580195,
2.16485320768083));
#284468=CARTESIAN_POINT('Ctrl Pts',(-0.102473699758015,-1.55215153763421,
2.16318107921345));
#284469=CARTESIAN_POINT('Ctrl Pts',(-0.112197521997491,-1.55147895993079,
2.16248938264003));
#284470=CARTESIAN_POINT('Ctrl Pts',(-0.131947422865425,-1.54992626137449,
2.16107760189209));
#284471=CARTESIAN_POINT('Ctrl Pts',(-0.141972547270079,-1.54904013024675,
2.16035736121882));
#284472=CARTESIAN_POINT('Ctrl Pts',(-0.166948353356754,-1.5465880066343,
2.15855362777078));
#284473=CARTESIAN_POINT('Ctrl Pts',(-0.181885968749375,-1.54490248229613,
2.15746643547949));
#284474=CARTESIAN_POINT('Ctrl Pts',(-0.241520691198428,-1.53729659197679,
2.15309096897472));
#284475=CARTESIAN_POINT('Ctrl Pts',(-0.285971297224774,-1.52965117479427,
2.14974954994905));
#284476=CARTESIAN_POINT('Ctrl Pts',(-0.408612427058461,-1.50302478682797,
2.14030119736805));
#284477=CARTESIAN_POINT('Ctrl Pts',(-0.485752132933097,-1.47989523383428,
2.13408739593804));
#284478=CARTESIAN_POINT('Ctrl Pts',(-0.637719242717976,-1.42116276919677,
2.12145124514738));
#284479=CARTESIAN_POINT('Ctrl Pts',(-0.712207207957305,-1.38533497941718,
2.11504806129051));
#284480=CARTESIAN_POINT('Ctrl Pts',(-0.796172754182559,-1.33637725621629,
2.10781015404));
#284481=CARTESIAN_POINT('Ctrl Pts',(-0.808734535092781,-1.32881289819332,
2.10672699109953));
#284482=CARTESIAN_POINT('Ctrl Pts',(-0.8270923000943,-1.31740157389273,
2.10514562134577));
#284483=CARTESIAN_POINT('Ctrl Pts',(-0.832972018173072,-1.31369182141907,
2.10463937343352));
#284484=CARTESIAN_POINT('Ctrl Pts',(-0.843234166005635,-1.30712041571836,
2.1037564864348));
#284485=CARTESIAN_POINT('Ctrl Pts',(-0.84762730303555,-1.30427589042998,
2.103378765626));
#284486=CARTESIAN_POINT('Ctrl Pts',(-0.856249026209486,-1.29863142276689,
2.10263799118104));
#284487=CARTESIAN_POINT('Ctrl Pts',(-0.860478318981203,-1.29583294896114,
2.10227483900512));
#284488=CARTESIAN_POINT('Ctrl Pts',(-0.872925706499312,-1.2875088455844,
2.10120646147114));
#284489=CARTESIAN_POINT('Ctrl Pts',(-0.881105008102596,-1.28192522976104,
2.10050497579205));
#284490=CARTESIAN_POINT('Ctrl Pts',(-0.922217986666207,-1.25327995586747,
2.09697871723892));
#284491=CARTESIAN_POINT('Ctrl Pts',(-0.954305219023846,-1.2290235429243,
2.09422560756095));
#284492=CARTESIAN_POINT('Ctrl Pts',(-1.0440451183946,-1.15554795148451,
2.08640678062015));
#284493=CARTESIAN_POINT('Ctrl Pts',(-1.09908878292764,-1.10332520752812,
2.08145604176351));
#284494=CARTESIAN_POINT('Ctrl Pts',(-1.2136248129733,-0.97754509315686,
2.07024919842545));
#284495=CARTESIAN_POINT('Ctrl Pts',(-1.27065470868303,-0.902171097299932,
2.06398616398876));
#284496=CARTESIAN_POINT('Ctrl Pts',(-1.33008984402866,-0.806703352588348,
2.05618629242116));
#284497=CARTESIAN_POINT('Ctrl Pts',(-1.33940635828878,-0.791138326572896,
2.05491907365427));
#284498=CARTESIAN_POINT('Ctrl Pts',(-1.35379251452682,-0.766120755842234,
2.05288721538097));
#284499=CARTESIAN_POINT('Ctrl Pts',(-1.35904045524121,-0.756772234931256,
2.05212903242805));
#284500=CARTESIAN_POINT('Ctrl Pts',(-1.36879850050741,-0.738960666047257,
2.05068608777694));
#284501=CARTESIAN_POINT('Ctrl Pts',(-1.37332781368055,-0.730508664937475,
2.05000205280315));
#284502=CARTESIAN_POINT('Ctrl Pts',(-1.38347042854234,-0.711154125130065,
2.0484368817918));
#284503=CARTESIAN_POINT('Ctrl Pts',(-1.38903346751614,-0.70022612522413,
2.04755402461027));
#284504=CARTESIAN_POINT('Ctrl Pts',(-1.40593148585003,-0.666037838958002,
2.04479400291232));
#284505=CARTESIAN_POINT('Ctrl Pts',(-1.41681515845416,-0.642560817213278,
2.04290146584884));
#284506=CARTESIAN_POINT('Ctrl Pts',(-1.46512328613503,-0.531154601066817,
2.03392809450377));
#284507=CARTESIAN_POINT('Ctrl Pts',(-1.49497334040125,-0.440182381467759,
2.02660365242428));
#284508=CARTESIAN_POINT('Ctrl Pts',(-1.53750718739498,-0.254355614388529,
2.01182994196964));
#284509=CARTESIAN_POINT('Ctrl Pts',(-1.55018181699109,-0.159889735983582,
2.00441474412428));
#284510=CARTESIAN_POINT('Ctrl Pts',(-1.55470317190636,-0.0515354464191655,
1.99635363519677));
#284511=CARTESIAN_POINT('Ctrl Pts',(-1.5550876673794,-0.0382129960173114,
1.9953703679584));
#284512=CARTESIAN_POINT('Ctrl Pts',(-1.55538747575055,-0.0194763737262476,
1.99400003548267));
#284513=CARTESIAN_POINT('Ctrl Pts',(-1.55544581760213,-0.0140655495503116,
1.99360577514135));
#284514=CARTESIAN_POINT('Ctrl Pts',(-1.55549184273964,-0.0057933654377718,
1.99300537652288));
#284515=CARTESIAN_POINT('Ctrl Pts',(-1.5554998676356,-0.00293223911665466,
1.99279814542823));
#284516=CARTESIAN_POINT('Ctrl Pts',(-1.55549999837604,-7.10784117823764E-5,
1.99259135320666));
#284517=CARTESIAN_POINT('',(-1.55549982855345,0.00073032197892629,0.594056225566802));
#284518=CARTESIAN_POINT('Ctrl Pts',(-1.55549999838269,-7.09326402445093E-5,
1.99259134267093));
#284519=CARTESIAN_POINT('Ctrl Pts',(-1.55550011902552,0.00257467473978788,
1.99240012971776));
#284520=CARTESIAN_POINT('Ctrl Pts',(-1.5554934901766,0.00522032312768005,
1.99220929232667));
#284521=CARTESIAN_POINT('Ctrl Pts',(-1.55545344292802,0.0131395633060705,
1.99163920398461));
#284522=CARTESIAN_POINT('Ctrl Pts',(-1.55539995576352,0.0184130683000571,
1.99126108665928));
#284523=CARTESIAN_POINT('Ctrl Pts',(-1.55518583217104,0.0324731182807974,
1.9902567440163));
#284524=CARTESIAN_POINT('Ctrl Pts',(-1.55497755216657,0.0412589119150026,
1.98963309219957));
#284525=CARTESIAN_POINT('Ctrl Pts',(-1.55383195840756,0.0768494635388745,
1.98712095748074));
#284526=CARTESIAN_POINT('Ctrl Pts',(-1.55227585696072,0.103631450805317,
1.9852632676013));
#284527=CARTESIAN_POINT('Ctrl Pts',(-1.54114975071259,0.2359231038927,1.97618943355107));
#284528=CARTESIAN_POINT('Ctrl Pts',(-1.52151073768281,0.340311387440798,
1.96933712843099));
#284529=CARTESIAN_POINT('Ctrl Pts',(-1.47620012588961,0.493234080229205,
1.95879324838937));
#284530=CARTESIAN_POINT('Ctrl Pts',(-1.45835128782466,0.543743970141623,
1.95522551716895));
#284531=CARTESIAN_POINT('Ctrl Pts',(-1.42458280387633,0.625595613504931,
1.9492040281258));
#284532=CARTESIAN_POINT('Ctrl Pts',(-1.41014239559989,0.657498402179297,
1.946794124451));
#284533=CARTESIAN_POINT('Ctrl Pts',(-1.38854981571307,0.701212307064922,
1.94338708375297));
#284534=CARTESIAN_POINT('Ctrl Pts',(-1.38229770795498,0.713457998393686,
1.94242089052324));
#284535=CARTESIAN_POINT('Ctrl Pts',(-1.37130569767732,0.734300529843034,
1.94075519802945));
#284536=CARTESIAN_POINT('Ctrl Pts',(-1.36664515939659,0.74293847986607,
1.94005852379389));
#284537=CARTESIAN_POINT('Ctrl Pts',(-1.35701005350414,0.760398933815207,
1.93863700571577));
#284538=CARTESIAN_POINT('Ctrl Pts',(-1.3520304477732,0.769218098575097,
1.93791200731901));
#284539=CARTESIAN_POINT('Ctrl Pts',(-1.33929165185802,0.791273346973648,
1.93608084505064));
#284540=CARTESIAN_POINT('Ctrl Pts',(-1.33142224798604,0.804444158751699,
1.93497073926801));
#284541=CARTESIAN_POINT('Ctrl Pts',(-1.30029264649927,0.854836645956708,
1.9306573571652));
#284542=CARTESIAN_POINT('Ctrl Pts',(-1.2756579420909,0.891180551142507,
1.927404426962));
#284543=CARTESIAN_POINT('Ctrl Pts',(-1.18737429775381,1.0102528921736,1.91624850390149));
#284544=CARTESIAN_POINT('Ctrl Pts',(-1.11695538469033,1.08760030364894,
1.90811976958717));
#284545=CARTESIAN_POINT('Ctrl Pts',(-1.00614055534385,1.18711931533115,
1.89659803953098));
#284546=CARTESIAN_POINT('Ctrl Pts',(-0.971674071230796,1.21549212942396,
1.89316614859026));
#284547=CARTESIAN_POINT('Ctrl Pts',(-0.922103941136729,1.25284026883781,
1.88847894450689));
#284548=CARTESIAN_POINT('Ctrl Pts',(-0.907998456237183,1.2631006608431,
1.88717165933163));
#284549=CARTESIAN_POINT('Ctrl Pts',(-0.882984045708801,1.28066060027152,
1.8849031171743));
#284550=CARTESIAN_POINT('Ctrl Pts',(-0.872149931336673,1.28806324597573,
1.88393646306876));
#284551=CARTESIAN_POINT('Ctrl Pts',(-0.856752480723873,1.29830052631937,
1.88258625746465));
#284552=CARTESIAN_POINT('Ctrl Pts',(-0.852266537285292,1.30124971530581,
1.88219566455542));
#284553=CARTESIAN_POINT('Ctrl Pts',(-0.843304653615774,1.30707529107742,
1.88142100669883));
#284554=CARTESIAN_POINT('Ctrl Pts',(-0.838829060163154,1.3099520475025,
1.8810369310333));
#284555=CARTESIAN_POINT('Ctrl Pts',(-0.829254704345398,1.31603691838133,
1.88022130734973));
#284556=CARTESIAN_POINT('Ctrl Pts',(-0.824151982743377,1.31923843479728,
1.87979018231144));
#284557=CARTESIAN_POINT('Ctrl Pts',(-0.8101637938208,1.32790197578502,1.87861766428272));
#284558=CARTESIAN_POINT('Ctrl Pts',(-0.801241585030922,1.3333045293833,
1.87787999281922));
#284559=CARTESIAN_POINT('Ctrl Pts',(-0.752195963517563,1.36233235816509,
1.87387651925841));
#284560=CARTESIAN_POINT('Ctrl Pts',(-0.711077348352883,1.38423920806529,
1.87070664351387));
#284561=CARTESIAN_POINT('Ctrl Pts',(-0.584851109755567,1.44437690464246,
1.86133514685087));
#284562=CARTESIAN_POINT('Ctrl Pts',(-0.497230389517025,1.47683406465405,
1.85528933328042));
#284563=CARTESIAN_POINT('Ctrl Pts',(-0.361663326583314,1.51360784052488,
1.84596910989143));
#284564=CARTESIAN_POINT('Ctrl Pts',(-0.315563745840759,1.52388583831371,
1.84280748966478));
#284565=CARTESIAN_POINT('Ctrl Pts',(-0.237444094746595,1.53760581690063,
1.83739824475472));
#284566=CARTESIAN_POINT('Ctrl Pts',(-0.205655107193223,1.54217932751838,
1.83518322890479));
#284567=CARTESIAN_POINT('Ctrl Pts',(-0.160518005571697,1.5472528866153,
1.83200640101201));
#284568=CARTESIAN_POINT('Ctrl Pts',(-0.147268679623912,1.54857012813722,
1.83107008111648));
#284569=CARTESIAN_POINT('Ctrl Pts',(-0.124301642582489,1.55055609370397,
1.82943961692518));
#284570=CARTESIAN_POINT('Ctrl Pts',(-0.114591392886377,1.55130393633264,
1.82874798904557));
#284571=CARTESIAN_POINT('Ctrl Pts',(-0.0946393150333385,1.55265221375609,
1.82732186996137));
#284572=CARTESIAN_POINT('Ctrl Pts',(-0.0843973119566849,1.55324260218084,
1.82658709892692));
#284573=CARTESIAN_POINT('Ctrl Pts',(-0.0581983907073313,1.55449292208767,
1.82470027823698));
#284574=CARTESIAN_POINT('Ctrl Pts',(-0.0422361381574831,1.55500847931637,
1.82354378103776));
#284575=CARTESIAN_POINT('Ctrl Pts',(0.0234933103115159,1.5561186779589,
1.8187514137237));
#284576=CARTESIAN_POINT('Ctrl Pts',(0.0732620038764054,1.55457034310108,
1.81505035108349));
#284577=CARTESIAN_POINT('Ctrl Pts',(0.270407781668295,1.53894934109003,
1.80009810148991));
#284578=CARTESIAN_POINT('Ctrl Pts',(0.415503406604053,1.5062652021141,1.78835395481735));
#284579=CARTESIAN_POINT('Ctrl Pts',(0.5734162539313,1.44610349257725,1.77566162403263));
#284580=CARTESIAN_POINT('Ctrl Pts',(0.592893914943601,1.43822753087092,
1.7740996106817));
#284581=CARTESIAN_POINT('Ctrl Pts',(0.619509805704261,1.42683248928841,
1.77197556856206));
#284582=CARTESIAN_POINT('Ctrl Pts',(0.626788512176499,1.42365006940703,
1.77139579521323));
#284583=CARTESIAN_POINT('Ctrl Pts',(0.639077635127231,1.41816445723189,
1.77041916671233));
#284584=CARTESIAN_POINT('Ctrl Pts',(0.644100701288704,1.41589015891949,
1.77002062206805));
#284585=CARTESIAN_POINT('Ctrl Pts',(0.654502993514511,1.411113487851,1.7691967475409));
#284586=CARTESIAN_POINT('Ctrl Pts',(0.65988014213341,1.40860698752215,1.7687716709764));
#284587=CARTESIAN_POINT('Ctrl Pts',(0.674219644867172,1.40182264905352,
1.76763989295659));
#284588=CARTESIAN_POINT('Ctrl Pts',(0.683155782202183,1.39748955622364,
1.76693647301081));
#284589=CARTESIAN_POINT('Ctrl Pts',(0.724560054180047,1.37692073344363,
1.76368322558629));
#284590=CARTESIAN_POINT('Ctrl Pts',(0.756497812027981,1.35963580973052,
1.76119085517492));
#284591=CARTESIAN_POINT('Ctrl Pts',(0.862428841797037,1.2974154377602,1.75288246817431));
#284592=CARTESIAN_POINT('Ctrl Pts',(0.933270141217674,1.2474290569299,1.74724799126482));
#284593=CARTESIAN_POINT('Ctrl Pts',(1.06692013292578,1.13533438299877,1.73574118046835));
#284594=CARTESIAN_POINT('Ctrl Pts',(1.12933538843239,1.07326660355181,1.72988464500874));
#284595=CARTESIAN_POINT('Ctrl Pts',(1.19774664278753,0.992624458682775,
1.72254716066191));
#284596=CARTESIAN_POINT('Ctrl Pts',(1.20908379401704,0.97878325963177,1.72129694597782));
#284597=CARTESIAN_POINT('Ctrl Pts',(1.22679568110929,0.956381936877579,
1.71928594827722));
#284598=CARTESIAN_POINT('Ctrl Pts',(1.23332564890251,0.947946140825158,
1.71853138833459));
#284599=CARTESIAN_POINT('Ctrl Pts',(1.24556602477969,0.931792726585121,
1.71709124157548));
#284600=CARTESIAN_POINT('Ctrl Pts',(1.25129278423249,0.924088073683303,
1.71640634108907));
#284601=CARTESIAN_POINT('Ctrl Pts',(1.26422733761367,0.906345514949345,
1.71483336758056));
#284602=CARTESIAN_POINT('Ctrl Pts',(1.2713874783141,0.896273851696018,1.71394350963868));
#284603=CARTESIAN_POINT('Ctrl Pts',(1.2899525016156,0.869489591299989,1.71158441954779));
#284604=CARTESIAN_POINT('Ctrl Pts',(1.30115226887173,0.852638438955944,
1.7101076171718));
#284605=CARTESIAN_POINT('Ctrl Pts',(1.36924433004655,0.745720214082705,
1.70077940995386));
#284606=CARTESIAN_POINT('Ctrl Pts',(1.41707688625113,0.650241378874098,
1.69260332749517));
#284607=CARTESIAN_POINT('Ctrl Pts',(1.48710430951796,0.46523276796336,1.67726423463463));
#284608=CARTESIAN_POINT('Ctrl Pts',(1.51185211980472,0.377130338140775,
1.67016002808387));
#284609=CARTESIAN_POINT('Ctrl Pts',(1.53108891465178,0.27479168608536,1.66243553926147));
#284610=CARTESIAN_POINT('Ctrl Pts',(1.53329605643026,0.262196427907781,
1.66149397353666));
#284611=CARTESIAN_POINT('Ctrl Pts',(1.53639653965271,0.243122712002632,
1.66008326283441));
#284612=CARTESIAN_POINT('Ctrl Pts',(1.53740469616542,0.236663864017908,
1.65960817600959));
#284613=CARTESIAN_POINT('Ctrl Pts',(1.53916778456204,0.224881494712323,
1.65874650661287));
#284614=CARTESIAN_POINT('Ctrl Pts',(1.53993585390863,0.219560295911548,
1.65835923127157));
#284615=CARTESIAN_POINT('Ctrl Pts',(1.54162158563639,0.207437311016124,
1.65748112547824));
#284616=CARTESIAN_POINT('Ctrl Pts',(1.54252183966121,0.200633322831078,
1.65699126644039));
#284617=CARTESIAN_POINT('Ctrl Pts',(1.54517839983285,0.179479667371458,
1.65547689251072));
#284618=CARTESIAN_POINT('Ctrl Pts',(1.54677978282656,0.165110814622839,
1.65446051162804));
#284619=CARTESIAN_POINT('Ctrl Pts',(1.55740149024055,0.0560064688572886,
1.6468215302343));
#284620=CARTESIAN_POINT('Ctrl Pts',(1.55791253660047,-0.0393687362579156,
1.64058392966498));
#284621=CARTESIAN_POINT('Ctrl Pts',(1.54046895486907,-0.240796233696122,
1.62727932236513));
#284622=CARTESIAN_POINT('Ctrl Pts',(1.52026721709253,-0.346137046444243,
1.62022915360096));
#284623=CARTESIAN_POINT('Ctrl Pts',(1.48410274825739,-0.466217960032814,
1.6115348493163));
#284624=CARTESIAN_POINT('Ctrl Pts',(1.47847293622781,-0.48377461726748,
1.61024732300868));
#284625=CARTESIAN_POINT('Ctrl Pts',(1.46905773703682,-0.511435145181902,
1.60819055237718));
#284626=CARTESIAN_POINT('Ctrl Pts',(1.46547687093669,-0.521607201512875,
1.60742804816584));
#284627=CARTESIAN_POINT('Ctrl Pts',(1.45851645669041,-0.54074183403431,
1.60598164971215));
#284628=CARTESIAN_POINT('Ctrl Pts',(1.45515931044908,-0.549712069336964,
1.60529852964687));
#284629=CARTESIAN_POINT('Ctrl Pts',(1.44735402371341,-0.569995031256815,
1.60374208655094));
#284630=CARTESIAN_POINT('Ctrl Pts',(1.4428557326985,-0.581287643631238,
1.60286711408027));
#284631=CARTESIAN_POINT('Ctrl Pts',(1.4307849704745,-0.610586742118264,
1.60057435155424));
#284632=CARTESIAN_POINT('Ctrl Pts',(1.42300506046359,-0.628504840817679,
1.59914966287416));
#284633=CARTESIAN_POINT('Ctrl Pts',(1.36575491028151,-0.753843402546534,
1.58901960665432));
#284634=CARTESIAN_POINT('Ctrl Pts',(1.30452108890336,-0.855441697763552,
1.57990319328091));
#284635=CARTESIAN_POINT('Ctrl Pts',(1.18245199558247,-1.0139456456087,1.56438738008204));
#284636=CARTESIAN_POINT('Ctrl Pts',(1.12746941164851,-1.07475309733351,
1.55805122582995));
#284637=CARTESIAN_POINT('Ctrl Pts',(1.0590760648374,-1.13933626586966,1.55108092240368));
#284638=CARTESIAN_POINT('Ctrl Pts',(1.05010271244677,-1.14761211035633,
1.55018284681016));
#284639=CARTESIAN_POINT('Ctrl Pts',(1.03626343600544,-1.16007738416169,
1.54882382951428));
#284640=CARTESIAN_POINT('Ctrl Pts',(1.03146771024912,-1.16434351147904,
1.54835755958695));
#284641=CARTESIAN_POINT('Ctrl Pts',(1.02259969182071,-1.17213443090819,
1.54750411991568));
#284642=CARTESIAN_POINT('Ctrl Pts',(1.01853544046042,-1.1756678153428,1.54711634564948));
#284643=CARTESIAN_POINT('Ctrl Pts',(1.00922479364915,-1.18367779627746,
1.54623554616341));
#284644=CARTESIAN_POINT('Ctrl Pts',(1.00396688956023,-1.18814068990092,
1.545743511371));
#284645=CARTESIAN_POINT('Ctrl Pts',(0.987155811791567,-1.20221860242269,
1.54418665134727));
#284646=CARTESIAN_POINT('Ctrl Pts',(0.975492452644591,-1.21170156537091,
1.54313076188003));
#284647=CARTESIAN_POINT('Ctrl Pts',(0.901765972264607,-1.2698906289622,
1.53659263589172));
#284648=CARTESIAN_POINT('Ctrl Pts',(0.836201816090604,-1.31399159004533,
1.53136919426979));
#284649=CARTESIAN_POINT('Ctrl Pts',(0.728765934765258,-1.37494381213463,
1.5232304284675));
#284650=CARTESIAN_POINT('Ctrl Pts',(0.689036824046572,-1.39527720676207,
1.52030343793704));
#284651=CARTESIAN_POINT('Ctrl Pts',(0.600494544366389,-1.43588809674943,
1.51386135826791));
#284652=CARTESIAN_POINT('Ctrl Pts',(0.551413544326983,-1.45544177468332,
1.5103407697118));
#284653=CARTESIAN_POINT('Ctrl Pts',(0.468602906810515,-1.48364234297905,
1.50438972313286));
#284654=CARTESIAN_POINT('Ctrl Pts',(0.435407203321454,-1.49372137612275,
1.50200172102691));
#284655=CARTESIAN_POINT('Ctrl Pts',(0.388667759609058,-1.50622221594098,
1.49862047343261));
#284656=CARTESIAN_POINT('Ctrl Pts',(0.375385336880381,-1.50958730082631,
1.49765753200508));
#284657=CARTESIAN_POINT('Ctrl Pts',(0.352523444031966,-1.51505895532117,
1.49599569570089));
#284658=CARTESIAN_POINT('Ctrl Pts',(0.342965160317022,-1.51725123413279,
1.49529959190405));
#284659=CARTESIAN_POINT('Ctrl Pts',(0.324648695049365,-1.52127036024526,
1.49396284993019));
#284660=CARTESIAN_POINT('Ctrl Pts',(0.315894201140588,-1.52311231748,1.49332272650682));
#284661=CARTESIAN_POINT('Ctrl Pts',(0.295270020285172,-1.52726621574631,
1.49181160125686));
#284662=CARTESIAN_POINT('Ctrl Pts',(0.283388451122589,-1.52951542948631,
1.49093863893509));
#284663=CARTESIAN_POINT('Ctrl Pts',(0.241492288320197,-1.53694156520723,
1.48785130352396));
#284664=CARTESIAN_POINT('Ctrl Pts',(0.211354839350661,-1.54137496793553,
1.48561384831914));
#284665=CARTESIAN_POINT('Ctrl Pts',(0.0528087382752864,-1.55996107100571,
1.47374876898916));
#284666=CARTESIAN_POINT('Ctrl Pts',(-0.0768491300443284,-1.55895811007058,
1.46366327116439));
#284667=CARTESIAN_POINT('Ctrl Pts',(-0.244469628369181,-1.53668848421321,
1.45060899316746));
#284668=CARTESIAN_POINT('Ctrl Pts',(-0.283864933524152,-1.52990131253699,
1.44754513010654));
#284669=CARTESIAN_POINT('Ctrl Pts',(-0.338868684202275,-1.51822687193035,
1.44330712236147));
#284670=CARTESIAN_POINT('Ctrl Pts',(-0.354726635850338,-1.51460023841246,
1.44209005175325));
#284671=CARTESIAN_POINT('Ctrl Pts',(-0.38260503991278,-1.50776268903657,
1.43996211760959));
#284672=CARTESIAN_POINT('Ctrl Pts',(-0.394649139467748,-1.50465511854824,
1.4390466903879));
#284673=CARTESIAN_POINT('Ctrl Pts',(-0.412896288484655,-1.49971287720815,
1.43766701973659));
#284674=CARTESIAN_POINT('Ctrl Pts',(-0.419126963398019,-1.4979835285174,
1.43719720670766));
#284675=CARTESIAN_POINT('Ctrl Pts',(-0.430522942544951,-1.49474385879403,
1.4363405050839));
#284676=CARTESIAN_POINT('Ctrl Pts',(-0.435691287271443,-1.49324556301258,
1.4359529763684));
#284677=CARTESIAN_POINT('Ctrl Pts',(-0.447517262238299,-1.48975060180827,
1.43506847751558));
#284678=CARTESIAN_POINT('Ctrl Pts',(-0.454169400266483,-1.4877361044164,
1.43457254019766));
#284679=CARTESIAN_POINT('Ctrl Pts',(-0.4750606902839,-1.48125631577529,
1.43301939573248));
#284680=CARTESIAN_POINT('Ctrl Pts',(-0.489249737735284,-1.47663051222814,
1.43197092991726));
#284681=CARTESIAN_POINT('Ctrl Pts',(-0.583033933464068,-1.44455537745482,
1.42506983814199));
#284682=CARTESIAN_POINT('Ctrl Pts',(-0.660364994078612,-1.41088296827782,
1.4195139224779));
#284683=CARTESIAN_POINT('Ctrl Pts',(-0.804495084826273,-1.33366256007784,
1.40874816494985));
#284684=CARTESIAN_POINT('Ctrl Pts',(-0.871421654623025,-1.29092658562996,
1.40355143959259));
#284685=CARTESIAN_POINT('Ctrl Pts',(-0.970550163391214,-1.21639370300923,
1.39518810442193));
#284686=CARTESIAN_POINT('Ctrl Pts',(-1.00512462099946,-1.18798364691941,
1.39212948084136));
#284687=CARTESIAN_POINT('Ctrl Pts',(-1.04958706184484,-1.14811672974715,
1.38796617300013));
#284688=CARTESIAN_POINT('Ctrl Pts',(-1.06060388538366,-1.13794744882559,
1.38691459258498));
#284689=CARTESIAN_POINT('Ctrl Pts',(-1.07876167149295,-1.12069381796013,
1.3851463628521));
#284690=CARTESIAN_POINT('Ctrl Pts',(-1.08598416941231,-1.11369643649439,
1.38443346623776));
#284691=CARTESIAN_POINT('Ctrl Pts',(-1.10007685701575,-1.09977556023671,
1.38302309476224));
#284692=CARTESIAN_POINT('Ctrl Pts',(-1.10695078617103,-1.09285649708828,
1.38232583376938));
#284693=CARTESIAN_POINT('Ctrl Pts',(-1.1234944072443,-1.07588802926341,
1.38062451185305));
#284694=CARTESIAN_POINT('Ctrl Pts',(-1.13309473160344,-1.06577250868071,
1.37961750499015));
#284695=CARTESIAN_POINT('Ctrl Pts',(-1.16556857436224,-1.03062121363665,
1.37614156031102));
#284696=CARTESIAN_POINT('Ctrl Pts',(-1.18775722482965,-1.00496897117351,
1.37364447290536));
#284697=CARTESIAN_POINT('Ctrl Pts',(-1.28060425666047,-0.890255428133158,
1.36263750146825));
#284698=CARTESIAN_POINT('Ctrl Pts',(-1.34220967966605,-0.7943346874261,
1.35380049791934));
#284699=CARTESIAN_POINT('Ctrl Pts',(-1.42104203417698,-0.63579949219518,
1.34009253128453));
#284700=CARTESIAN_POINT('Ctrl Pts',(-1.44578090698632,-0.577339335262993,
1.33521561712965));
#284701=CARTESIAN_POINT('Ctrl Pts',(-1.47177421462297,-0.503663589952632,
1.32940066046637));
#284702=CARTESIAN_POINT('Ctrl Pts',(-1.47646861112187,-0.489731388441157,
1.32831529212413));
#284703=CARTESIAN_POINT('Ctrl Pts',(-1.4830780131398,-0.469156252690684,
1.32673532298303));
#284704=CARTESIAN_POINT('Ctrl Pts',(-1.4851472291247,-0.462564260622396,
1.32623254887302));
#284705=CARTESIAN_POINT('Ctrl Pts',(-1.48859807323881,-0.451308850062166,
1.32538017497586));
#284706=CARTESIAN_POINT('Ctrl Pts',(-1.49000183658651,-0.44665247257127,
1.32502932202018));
#284707=CARTESIAN_POINT('Ctrl Pts',(-1.49316581611957,-0.435976406432577,
1.32422898535905));
#284708=CARTESIAN_POINT('Ctrl Pts',(-1.49491149247583,-0.429952572676887,
1.32378034360659));
#284709=CARTESIAN_POINT('Ctrl Pts',(-1.49967029050861,-0.413151888714799,
1.32253679958487));
#284710=CARTESIAN_POINT('Ctrl Pts',(-1.50260370409731,-0.402352570303646,
1.32174628796744));
#284711=CARTESIAN_POINT('Ctrl Pts',(-1.52349661870134,-0.322018361500382,
1.31592455248651));
#284712=CARTESIAN_POINT('Ctrl Pts',(-1.53674035490596,-0.251335933271153,
1.31112552824004));
#284713=CARTESIAN_POINT('Ctrl Pts',(-1.55196062677587,-0.120678045176283,
1.30242901063917));
#284714=CARTESIAN_POINT('Ctrl Pts',(-1.55544879049007,-0.0610252666929087,
1.29852343257111));
#284715=CARTESIAN_POINT('Ctrl Pts',(-1.55556451017232,0.0753844301872104,
1.28949615929373));
#284716=CARTESIAN_POINT('Ctrl Pts',(-1.54995612352385,0.151978427235645,
1.28435416547317));
#284717=CARTESIAN_POINT('Ctrl Pts',(-1.53610640855601,0.245512772204258,
1.27779331556791));
#284718=CARTESIAN_POINT('Ctrl Pts',(-1.53318543656123,0.263138349608341,
1.27654485595358));
#284719=CARTESIAN_POINT('Ctrl Pts',(-1.52803752297669,0.291196258961756,
1.27453602118211));
#284720=CARTESIAN_POINT('Ctrl Pts',(-1.52600566356196,0.30166311909529,
1.27378184543579));
#284721=CARTESIAN_POINT('Ctrl Pts',(-1.52194001851677,0.321513617165654,
1.27234200819764));
#284722=CARTESIAN_POINT('Ctrl Pts',(-1.51992663286587,0.330900965670557,
1.27165702888136));
#284723=CARTESIAN_POINT('Ctrl Pts',(-1.51512120871579,0.352336367341829,
1.27008326972483));
#284724=CARTESIAN_POINT('Ctrl Pts',(-1.51227215768968,0.364370824160014,
1.26919269832077));
#284725=CARTESIAN_POINT('Ctrl Pts',(-1.50287944293008,0.402036544633793,
1.26638256413903));
#284726=CARTESIAN_POINT('Ctrl Pts',(-1.49582559289182,0.427534372904009,
1.2644468131633));
#284727=CARTESIAN_POINT('Ctrl Pts',(-1.44396539905443,0.597958184317801,
1.25127379158226));
#284728=CARTESIAN_POINT('Ctrl Pts',(-1.37881774665419,0.735821562903013,
1.2393468258457));
#284729=CARTESIAN_POINT('Ctrl Pts',(-1.27040596013088,0.898657001686139,
1.22434587809634));
#284730=CARTESIAN_POINT('Ctrl Pts',(-1.24447989577291,0.934230327061191,
1.22101266279073));
#284731=CARTESIAN_POINT('Ctrl Pts',(-1.21054621632769,0.976866479589994,
1.21698911397459));
#284732=CARTESIAN_POINT('Ctrl Pts',(-1.20393154694693,0.985007160949235,
1.21621955657018));
#284733=CARTESIAN_POINT('Ctrl Pts',(-1.19336971412907,0.997740260143308,
1.21501457181498));
#284734=CARTESIAN_POINT('Ctrl Pts',(-1.18947736801325,1.00237742176221,
1.21457546279458));
#284735=CARTESIAN_POINT('Ctrl Pts',(-1.18202152118981,1.01115538613324,
1.21374391198384));
#284736=CARTESIAN_POINT('Ctrl Pts',(-1.17846326852695,1.01530016114741,
1.21335115067482));
#284737=CARTESIAN_POINT('Ctrl Pts',(-1.16987393422634,1.0251993209713,1.21241261847622));
#284738=CARTESIAN_POINT('Ctrl Pts',(-1.16482214663725,1.03093551828566,
1.21186836536251));
#284739=CARTESIAN_POINT('Ctrl Pts',(-1.14706630145771,1.05079975711348,
1.20998122343407));
#284740=CARTESIAN_POINT('Ctrl Pts',(-1.13414524325496,1.06473277467991,
1.20865325041874));
#284741=CARTESIAN_POINT('Ctrl Pts',(-1.10106927157342,1.09911362797249,
1.2053545529455));
#284742=CARTESIAN_POINT('Ctrl Pts',(-1.08059699787663,1.11924735710697,
1.20340259345937));
#284743=CARTESIAN_POINT('Ctrl Pts',(-1.00609126913938,1.18856974925828,
1.1965566831711));
#284744=CARTESIAN_POINT('Ctrl Pts',(-0.949162167166272,1.23450801561769,
1.19178128620634));
#284745=CARTESIAN_POINT('Ctrl Pts',(-0.811823094013529,1.33019541035699,
1.18075423134217));
#284746=CARTESIAN_POINT('Ctrl Pts',(-0.729701252242791,1.37695647376491,
1.17449221377283));
#284747=CARTESIAN_POINT('Ctrl Pts',(-0.627344598702263,1.42349852551739,
1.16669344762085));
#284748=CARTESIAN_POINT('Ctrl Pts',(-0.610702394312591,1.43071724508431,
1.16542621850667));
#284749=CARTESIAN_POINT('Ctrl Pts',(-0.58402985280599,1.44173656272076,
1.1633943484695));
#284750=CARTESIAN_POINT('Ctrl Pts',(-0.57407953304397,1.44572745170668,
1.16263616431264));
#284751=CARTESIAN_POINT('Ctrl Pts',(-0.555152645091275,1.45309247501296,
1.16119322077914));
#284752=CARTESIAN_POINT('Ctrl Pts',(-0.546184538974721,1.45648708957448,
1.16050918816043));
#284753=CARTESIAN_POINT('Ctrl Pts',(-0.525677952481883,1.46403323180203,
1.15894402753608));
#284754=CARTESIAN_POINT('Ctrl Pts',(-0.514120746931992,1.46813162049813,
1.15806117844692));
#284755=CARTESIAN_POINT('Ctrl Pts',(-0.478029880761631,1.48045167178435,
1.15530120179547));
#284756=CARTESIAN_POINT('Ctrl Pts',(-0.45333986770594,1.48819774726452,
1.15340870242827));
#284757=CARTESIAN_POINT('Ctrl Pts',(-0.33670986053917,1.52161685662852,
1.14444313599912));
#284758=CARTESIAN_POINT('Ctrl Pts',(-0.242739770323382,1.53940351201316,
1.13712706701058));
#284759=CARTESIAN_POINT('Ctrl Pts',(-0.0539903401947642,1.55741320465323,
1.12243307359287));
#284760=CARTESIAN_POINT('Ctrl Pts',(0.0403943634692655,1.55782613260909,
1.11508996816958));
#284761=CARTESIAN_POINT('Ctrl Pts',(0.147353240799339,1.54856076175381,
1.10710082913873));
#284762=CARTESIAN_POINT('Ctrl Pts',(0.160448820150422,1.54725874251856,
1.1061286491597));
#284763=CARTESIAN_POINT('Ctrl Pts',(0.180175331838236,1.5450442903511,1.10467474623197));
#284764=CARTESIAN_POINT('Ctrl Pts',(0.186819093495798,1.54425504371015,
1.10418688994393));
#284765=CARTESIAN_POINT('Ctrl Pts',(0.19887556176696,1.5427438462499,1.10330510814054));
#284766=CARTESIAN_POINT('Ctrl Pts',(0.204289946793778,1.54203621415017,
1.1029104128738));
#284767=CARTESIAN_POINT('Ctrl Pts',(0.215560818039924,1.54050276223701,
1.10209163850011));
#284768=CARTESIAN_POINT('Ctrl Pts',(0.221416478613796,1.5396720341906,1.10166783367192));
#284769=CARTESIAN_POINT('Ctrl Pts',(0.237006849981335,1.53736948363762,
1.10054334525802));
#284770=CARTESIAN_POINT('Ctrl Pts',(0.246732767878881,1.53583857571875,
1.09984586888428));
#284771=CARTESIAN_POINT('Ctrl Pts',(0.295297877051716,1.52772092642333,
1.09638027075595));
#284772=CARTESIAN_POINT('Ctrl Pts',(0.333895189023762,1.51975218066694,
1.093680875597));
#284773=CARTESIAN_POINT('Ctrl Pts',(0.446404473278318,1.4920293200046,1.08586344574943));
#284774=CARTESIAN_POINT('Ctrl Pts',(0.519211249974908,1.46828116653457,
1.08086686669834));
#284775=CARTESIAN_POINT('Ctrl Pts',(0.677453029612676,1.40341546865666,
1.06960056678341));
#284776=CARTESIAN_POINT('Ctrl Pts',(0.761463632359443,1.35966436708586,
1.0633248192028));
#284777=CARTESIAN_POINT('Ctrl Pts',(0.856237170966289,1.2987560169618,1.05551098162959));
#284778=CARTESIAN_POINT('Ctrl Pts',(0.871323554451145,1.28868324274627,
1.05424377363127));
#284779=CARTESIAN_POINT('Ctrl Pts',(0.895040775568518,1.2722410166312,1.05221189446662));
#284780=CARTESIAN_POINT('Ctrl Pts',(0.903788145309655,1.26604193151345,
1.05145367879232));
#284781=CARTESIAN_POINT('Ctrl Pts',(0.920237092274717,1.25412754919312,
1.05001064560518));
#284782=CARTESIAN_POINT('Ctrl Pts',(0.927951290303024,1.24843045897161,
1.04932655460965));
#284783=CARTESIAN_POINT('Ctrl Pts',(0.945409596321133,1.23528593810463,
1.04776121642826));
#284784=CARTESIAN_POINT('Ctrl Pts',(0.955119182492497,1.22779395051074,
1.04687824755671));
#284785=CARTESIAN_POINT('Ctrl Pts',(0.985040158112796,1.20413700063848,
1.04411771195132));
#284786=CARTESIAN_POINT('Ctrl Pts',(1.0049364571286,1.18758266982385,1.04222476646123));
#284787=CARTESIAN_POINT('Ctrl Pts',(1.09777369726286,1.10633529716653,1.03310799557386));
#284788=CARTESIAN_POINT('Ctrl Pts',(1.16492737130343,1.03538551027477,1.02562932804202));
#284789=CARTESIAN_POINT('Ctrl Pts',(1.28173779174257,0.886118993253203,
1.01093700402529));
#284790=CARTESIAN_POINT('Ctrl Pts',(1.33193853823549,0.808703548050602,
1.00376423871194));
#284791=CARTESIAN_POINT('Ctrl Pts',(1.38175212007759,0.714527782444577,
0.99583561286931));
#284792=CARTESIAN_POINT('Ctrl Pts',(1.38832767936271,0.701665994306596,
0.994769189952345));
#284793=CARTESIAN_POINT('Ctrl Pts',(1.39780460524719,0.682474148564347,
0.993204025876144));
#284794=CARTESIAN_POINT('Ctrl Pts',(1.40084395447192,0.676213648275335,
0.992697521384129));
#284795=CARTESIAN_POINT('Ctrl Pts',(1.40615896372874,0.665076069564426,
0.991803888519324));
#284796=CARTESIAN_POINT('Ctrl Pts',(1.40845145157185,0.660207332016687,
0.991415762194369));
#284797=CARTESIAN_POINT('Ctrl Pts',(1.4134395569626,0.649469458187675,0.990565314440879));
#284798=CARTESIAN_POINT('Ctrl Pts',(1.4161239343988,0.643595342384742,0.990103672237949));
#284799=CARTESIAN_POINT('Ctrl Pts',(1.42385621014514,0.626392494568939,
0.988761679621271));
#284800=CARTESIAN_POINT('Ctrl Pts',(1.42880544845994,0.615019577245407,
0.987887027531342));
#284801=CARTESIAN_POINT('Ctrl Pts',(1.43990681850609,0.5886520517134,0.985885216676517));
#284802=CARTESIAN_POINT('Ctrl Pts',(1.44596179006804,0.573617845990316,
0.984762988082385));
#284803=CARTESIAN_POINT('Ctrl Pts',(1.46604606495604,0.521409371128415,
0.98092242534933));
#284804=CARTESIAN_POINT('Ctrl Pts',(1.47888627647228,0.483791936155673,
0.978252864158474));
#284805=CARTESIAN_POINT('Ctrl Pts',(1.51824606616646,0.352192236121999,
0.969116115765335));
#284806=CARTESIAN_POINT('Ctrl Pts',(1.53735256498088,0.256238169444717,
0.962789957058778));
#284807=CARTESIAN_POINT('Ctrl Pts',(1.55300508476299,0.104032516626026,
0.952556490653376));
#284808=CARTESIAN_POINT('Ctrl Pts',(1.55572379976144,0.0486821573415437,
0.948797804397603));
#284809=CARTESIAN_POINT('Ctrl Pts',(1.55541437507945,-0.0232511031328495,
0.943796304505901));
#284810=CARTESIAN_POINT('Ctrl Pts',(1.55507869387626,-0.0398084298318202,
0.942637213105604));
#284811=CARTESIAN_POINT('Ctrl Pts',(1.55410256400944,-0.0667328787470038,
0.940737990149875));
#284812=CARTESIAN_POINT('Ctrl Pts',(1.55362250808619,-0.0771047954220716,
0.940002892249914));
#284813=CARTESIAN_POINT('Ctrl Pts',(1.55249421480392,-0.097137548993712,
0.938575994924655));
#284814=CARTESIAN_POINT('Ctrl Pts',(1.5518595368114,-0.10679869201468,0.937884653237171));
#284815=CARTESIAN_POINT('Ctrl Pts',(1.55016397141644,-0.129383327005083,
0.936260723444656));
#284816=CARTESIAN_POINT('Ctrl Pts',(1.54903160645721,-0.142300551066779,
0.935325935915946));
#284817=CARTESIAN_POINT('Ctrl Pts',(1.54475031973883,-0.18499536391627,
0.932215548937597));
#284818=CARTESIAN_POINT('Ctrl Pts',(1.54090327360402,-0.214694451259772,
0.930018415605765));
#284819=CARTESIAN_POINT('Ctrl Pts',(1.52948480331689,-0.286506930390575,
0.924620485594281));
#284820=CARTESIAN_POINT('Ctrl Pts',(1.52102861647656,-0.328452975793619,
0.921395149483289));
#284821=CARTESIAN_POINT('Ctrl Pts',(1.49539853146159,-0.433112353343308,
0.91317351482875));
#284822=CARTESIAN_POINT('Ctrl Pts',(1.47600221386355,-0.495196527239499,
0.908133147520748));
#284823=CARTESIAN_POINT('Ctrl Pts',(1.44667406404472,-0.571844844974288,
0.901768996687771));
#284824=CARTESIAN_POINT('Ctrl Pts',(1.44030336850702,-0.587706210834056,
0.900444349535024));
#284825=CARTESIAN_POINT('Ctrl Pts',(1.4088024861588,-0.662544623366514,
0.894164782443614));
#284826=CARTESIAN_POINT('Ctrl Pts',(1.38030054117883,-0.720043185061402,
0.889249712250288));
#284827=CARTESIAN_POINT('Ctrl Pts',(1.34277965306335,-0.785268646814441,
0.883684444331667));
#284828=CARTESIAN_POINT('Ctrl Pts',(1.33712818018458,-0.794853629945437,
0.882866966277334));
#284829=CARTESIAN_POINT('Ctrl Pts',(1.32813862447611,-0.80973279034294,
0.88159946622582));
#284830=CARTESIAN_POINT('Ctrl Pts',(1.32487075861659,-0.815068631609816,
0.881145232625444));
#284831=CARTESIAN_POINT('Ctrl Pts',(1.31900480806258,-0.824518183889099,
0.880341549281049));
#284832=CARTESIAN_POINT('Ctrl Pts',(1.31641958748473,-0.828639481330176,
0.879991306410469));
#284833=CARTESIAN_POINT('Ctrl Pts',(1.3101059226096,-0.838600453558989,
0.879145363411839));
#284834=CARTESIAN_POINT('Ctrl Pts',(1.30635774063827,-0.844427443614875,
0.878650964979895));
#284835=CARTESIAN_POINT('Ctrl Pts',(1.29447787244953,-0.862627671368899,
0.877107545084808));
#284836=CARTESIAN_POINT('Ctrl Pts',(1.2862080941584,-0.874910419584213,
0.876067112103536));
#284837=CARTESIAN_POINT('Ctrl Pts',(1.24102146719002,-0.939998393763268,
0.870549118694733));
#284838=CARTESIAN_POINT('Ctrl Pts',(1.20102177002697,-0.990595769730546,
0.866241856853231));
#284839=CARTESIAN_POINT('Ctrl Pts',(1.08011548284486,-1.12540479284887,
0.854262536242355));
#284840=CARTESIAN_POINT('Ctrl Pts',(0.992723629925456,-1.20319720618115,
0.846703145998765));
#284841=CARTESIAN_POINT('Ctrl Pts',(0.872244032368145,-1.28830265682975,
0.83663769092527));
#284842=CARTESIAN_POINT('Ctrl Pts',(0.84650472564177,-1.30535930645551,
0.834507680960866));
#284843=CARTESIAN_POINT('Ctrl Pts',(0.809945483264368,-1.32804985010774,
0.83149939687293));
#284844=CARTESIAN_POINT('Ctrl Pts',(0.799540009872801,-1.33434022949317,
0.83064507628571));
#284845=CARTESIAN_POINT('Ctrl Pts',(0.78133839875095,-1.34505423024224,
0.829153306560477));
#284846=CARTESIAN_POINT('Ctrl Pts',(0.773575680986267,-1.34953371033726,
0.828517909302391));
#284847=CARTESIAN_POINT('Ctrl Pts',(0.757251180852822,-1.35876664387708,
0.827183156970268));
#284848=CARTESIAN_POINT('Ctrl Pts',(0.748682380623921,-1.36350681269444,
0.826483361197453));
#284849=CARTESIAN_POINT('Ctrl Pts',(0.728087465584181,-1.37464703526844,
0.824803042643302));
#284850=CARTESIAN_POINT('Ctrl Pts',(0.71602109872874,-1.38097052586814,
0.823819864040173));
#284851=CARTESIAN_POINT('Ctrl Pts',(0.673425432805196,-1.40258484174555,
0.820352665509381));
#284852=CARTESIAN_POINT('Ctrl Pts',(0.642479214222601,-1.41702723137289,
0.817839726618729));
#284853=CARTESIAN_POINT('Ctrl Pts',(0.563635704947146,-1.45070926516517,
0.81144771297296));
#284854=CARTESIAN_POINT('Ctrl Pts',(0.515211722130124,-1.46860427794763,
0.807530222112154));
#284855=CARTESIAN_POINT('Ctrl Pts',(0.409479535773776,-1.5018040303023,
0.799016768452861));
#284856=CARTESIAN_POINT('Ctrl Pts',(0.352000771426533,-1.51630598873582,
0.794412440130713));
#284857=CARTESIAN_POINT('Ctrl Pts',(0.222994372100513,-1.54112239410058,
0.78423540809957));
#284858=CARTESIAN_POINT('Ctrl Pts',(0.151280085644583,-1.54980693845474,
0.778681197658446));
#284859=CARTESIAN_POINT('Ctrl Pts',(0.0680365170133073,-1.55405165719224,
0.772515785488483));
#284860=CARTESIAN_POINT('Ctrl Pts',(0.0568523321897233,-1.55450099788973,
0.771693367913762));
#284861=CARTESIAN_POINT('Ctrl Pts',(0.0393937461569052,-1.55501373976952,
0.770419802986291));
#284862=CARTESIAN_POINT('Ctrl Pts',(0.0331224372677322,-1.55515996153874,
0.769964384347709));
#284863=CARTESIAN_POINT('Ctrl Pts',(0.021984896215217,-1.55535224089054,
0.76915943880821));
#284864=CARTESIAN_POINT('Ctrl Pts',(0.0171192645325594,-1.55541340510226,
0.768809109064862));
#284865=CARTESIAN_POINT('Ctrl Pts',(0.00533892613749954,-1.55550620574388,
0.767964035816541));
#284866=CARTESIAN_POINT('Ctrl Pts',(-0.00157581618784463,-1.55551457142069,
0.767470582717171));
#284867=CARTESIAN_POINT('Ctrl Pts',(-0.0232057863965961,-1.55539650437889,
0.765934441211598));
#284868=CARTESIAN_POINT('Ctrl Pts',(-0.0379198374659211,-1.55510736659196,
0.764900213633982));
#284869=CARTESIAN_POINT('Ctrl Pts',(-0.116118566170711,-1.55246010154481,
0.759450272660226));
#284870=CARTESIAN_POINT('Ctrl Pts',(-0.179425560112246,-1.5464230653951,
0.755200066184727));
#284871=CARTESIAN_POINT('Ctrl Pts',(-0.354848892399446,-1.51877229410457,
0.743446326297378));
#284872=CARTESIAN_POINT('Ctrl Pts',(-0.465203075819883,-1.4886812068753,
0.736054560396688));
#284873=CARTESIAN_POINT('Ctrl Pts',(-0.602385267824321,-1.43451420336989,
0.726014921118387));
#284874=CARTESIAN_POINT('Ctrl Pts',(-0.633089345697491,-1.42123067018792,
0.723711455681568));
#284875=CARTESIAN_POINT('Ctrl Pts',(-0.675882810235645,-1.40105495214973,
0.720406084278627));
#284876=CARTESIAN_POINT('Ctrl Pts',(-0.688345942198975,-1.3949739761155,
0.719431758614794));
#284877=CARTESIAN_POINT('Ctrl Pts',(-0.70942330680691,-1.38433873349922,
0.717763084697398));
#284878=CARTESIAN_POINT('Ctrl Pts',(-0.718079248868177,-1.37986859584346,
0.717071699792114));
#284879=CARTESIAN_POINT('Ctrl Pts',(-0.735606519807462,-1.37060750871328,
0.715658930312276));
#284880=CARTESIAN_POINT('Ctrl Pts',(-0.744474383518997,-1.36581103318115,
0.714937375691222));
#284881=CARTESIAN_POINT('Ctrl Pts',(-0.766509028440103,-1.35361452179986,
0.713127116897841));
#284882=CARTESIAN_POINT('Ctrl Pts',(-0.779615571380525,-1.34610842625631,
0.712034661526545));
#284883=CARTESIAN_POINT('Ctrl Pts',(-0.807604575825206,-1.32953329199679,
0.709666881177451));
#284884=CARTESIAN_POINT('Ctrl Pts',(-0.822447971733887,-1.32040267113258,
0.708389447992213));
#284885=CARTESIAN_POINT('Ctrl Pts',(-0.865171431028327,-1.29312227989664,
0.70464787802131));
#284886=CARTESIAN_POINT('Ctrl Pts',(-0.892625077539465,-1.27432610304691,
0.702161374564172));
#284887=CARTESIAN_POINT('Ctrl Pts',(-0.988685215355922,-1.20393059419525,
0.693162316415759));
#284888=CARTESIAN_POINT('Ctrl Pts',(-1.05359295540303,-1.14755675013085,
0.686502611333705));
#284889=CARTESIAN_POINT('Ctrl Pts',(-1.16334215407464,-1.03504001332638,
0.674317888887702));
#284890=CARTESIAN_POINT('Ctrl Pts',(-1.20960140150812,-0.980581127914488,
0.668807902385738));
#284891=CARTESIAN_POINT('Ctrl Pts',(-1.26087083271932,-0.911049062565754,
0.662374611058342));
#284892=CARTESIAN_POINT('Ctrl Pts',(-1.26960575501918,-0.898836426917664,
0.661265693583988));
#284893=CARTESIAN_POINT('Ctrl Pts',(-1.28213375016899,-0.880773434201796,
0.659658211864933));
#284894=CARTESIAN_POINT('Ctrl Pts',(-1.28606619168883,-0.875021457631531,
0.659151080474249));
#284895=CARTESIAN_POINT('Ctrl Pts',(-1.29296643676138,-0.864781468675158,
0.658256916712449));
#284896=CARTESIAN_POINT('Ctrl Pts',(-1.29594976810098,-0.860304246706169,
0.65786887823863));
#284897=CARTESIAN_POINT('Ctrl Pts',(-1.30245604872051,-0.85042932259697,
0.657019440137136));
#284898=CARTESIAN_POINT('Ctrl Pts',(-1.30596873679009,-0.845025120396164,
0.65655871192874));
#284899=CARTESIAN_POINT('Ctrl Pts',(-1.31611794131899,-0.829196311699765,
0.655220783822836));
#284900=CARTESIAN_POINT('Ctrl Pts',(-1.32266414012252,-0.818713965021877,
0.654349241911004));
#284901=CARTESIAN_POINT('Ctrl Pts',(-1.3374671408684,-0.794369051698037,
0.652355504380398));
#284902=CARTESIAN_POINT('Ctrl Pts',(-1.34563470015674,-0.780453614269328,
0.651238192052071));
#284903=CARTESIAN_POINT('Ctrl Pts',(-1.37303007173308,-0.732069839464504,
0.647420405751045));
#284904=CARTESIAN_POINT('Ctrl Pts',(-1.39116288887486,-0.69699648300642,
0.644768161173048));
#284905=CARTESIAN_POINT('Ctrl Pts',(-1.45339524223424,-0.564494253885719,
0.635029697397613));
#284906=CARTESIAN_POINT('Ctrl Pts',(-1.48874816292867,-0.463293363835836,
0.628118192579953));
#284907=CARTESIAN_POINT('Ctrl Pts',(-1.5245725570003,-0.312379502804916,
0.617692962149108));
#284908=CARTESIAN_POINT('Ctrl Pts',(-1.53351674771813,-0.265005807328792,
0.614407765930124));
#284909=CARTESIAN_POINT('Ctrl Pts',(-1.54245194867326,-0.201671165547637,
0.609955003993573));
#284910=CARTESIAN_POINT('Ctrl Pts',(-1.5444184294341,-0.186013321596209,
0.608849415306203));
#284911=CARTESIAN_POINT('Ctrl Pts',(-1.54726452085034,-0.160178144410728,
0.607016021853066));
#284912=CARTESIAN_POINT('Ctrl Pts',(-1.54828273566704,-0.150016988513915,
0.606292605833772));
#284913=CARTESIAN_POINT('Ctrl Pts',(-1.55001853938621,-0.130788022989853,
0.604918861160473));
#284914=CARTESIAN_POINT('Ctrl Pts',(-1.55075678723504,-0.121722470209087,
0.604269213089911));
#284915=CARTESIAN_POINT('Ctrl Pts',(-1.55210380397938,-0.103171547151945,
0.602935533875908));
#284916=CARTESIAN_POINT('Ctrl Pts',(-1.55270522115207,-0.0936860459676571,
0.602251299817703));
#284917=CARTESIAN_POINT('Ctrl Pts',(-1.55391914855842,-0.0712918716144281,
0.600630245641894));
#284918=CARTESIAN_POINT('Ctrl Pts',(-1.55445778287666,-0.058380079888536,
0.599691163043238));
#284919=CARTESIAN_POINT('Ctrl Pts',(-1.55528652596405,-0.030037318954975,
0.597619631210879));
#284920=CARTESIAN_POINT('Ctrl Pts',(-1.55550797093957,-0.0146059614368184,
0.596485179220674));
#284921=CARTESIAN_POINT('Ctrl Pts',(-1.5554997809254,0.000825554981074353,
0.595343941296876));
#284922=CARTESIAN_POINT('',(-0.903577283124934,-1.26614704652365,4.13766671841787E-5));
#284923=CARTESIAN_POINT('Ctrl Pts',(-0.903577283124934,-1.26614704652365,
4.13766671842897E-5));
#284924=CARTESIAN_POINT('Ctrl Pts',(-0.854864239968711,-1.30091078056915,
0.00435153502361089));
#284925=CARTESIAN_POINT('Ctrl Pts',(-0.804029053149215,-1.33293958991072,
0.00866169338003741));
#284926=CARTESIAN_POINT('Ctrl Pts',(-0.75141824501022,-1.36196581126905,
0.0129718517364641));
#284927=CARTESIAN_POINT('Ctrl Pts',(-0.701345114626583,-1.38959195536439,
0.0170741099793956));
#284928=CARTESIAN_POINT('Ctrl Pts',(-0.64966423731578,-1.41449818738748,
0.0211763682223272));
#284929=CARTESIAN_POINT('Ctrl Pts',(-0.596706059304791,-1.43649647712375,
0.0252786264652587));
#284930=CARTESIAN_POINT('Ctrl Pts',(-0.543795605076904,-1.45847494288481,
0.0293771879178177));
#284931=CARTESIAN_POINT('Ctrl Pts',(-0.48961061798377,-1.47755045266205,
0.0334757493703768));
#284932=CARTESIAN_POINT('Ctrl Pts',(-0.434504797180995,-1.49358154488689,
0.0375743108229358));
#284933=CARTESIAN_POINT('Ctrl Pts',(-0.379426492987175,-1.50960463212624,
0.0416708256947322));
#284934=CARTESIAN_POINT('Ctrl Pts',(-0.323428775682673,-1.52258616624964,
0.0457673405665284));
#284935=CARTESIAN_POINT('Ctrl Pts',(-0.266881681598629,-1.53243414802304,
0.0498638554383248));
#284936=CARTESIAN_POINT('Ctrl Pts',(-0.21034010396998,-1.54228116907594,
0.0539599706743499));
#284937=CARTESIAN_POINT('Ctrl Pts',(-0.153249779571496,-1.54899515564964,
0.0580560859103751));
#284938=CARTESIAN_POINT('Ctrl Pts',(-0.0959898131972683,-1.55253541207998,
0.0621522011464002));
#284939=CARTESIAN_POINT('Ctrl Pts',(-0.0386749267085929,-1.55607906409891,
0.0662522451153917));
#284940=CARTESIAN_POINT('Ctrl Pts',(0.0188093951990522,-1.55644287993823,
0.0703522890843831));
#284941=CARTESIAN_POINT('Ctrl Pts',(0.0760816915993679,-1.55363825461508,
0.0744523330533746));
#284942=CARTESIAN_POINT('Ctrl Pts',(0.133386106680123,-1.5508320564396,
0.0785546763539856));
#284943=CARTESIAN_POINT('Ctrl Pts',(0.190477731422078,-1.54485393887542,
0.0826570196545963));
#284944=CARTESIAN_POINT('Ctrl Pts',(0.246981163227441,-1.53576709009238,
0.0867593629552073));
#284945=CARTESIAN_POINT('Ctrl Pts',(0.303581603655238,-1.52666464043955,
0.0908687494151384));
#284946=CARTESIAN_POINT('Ctrl Pts',(0.359591319092611,-1.51444292904211,
0.0949781358750698));
#284947=CARTESIAN_POINT('Ctrl Pts',(0.414647503255705,-1.49921569430279,
0.099087522335001));
#284948=CARTESIAN_POINT('Ctrl Pts',(0.434286939269945,-1.49378389210142,
0.100553407297143));
#284949=CARTESIAN_POINT('Ctrl Pts',(0.453805212795988,-1.48797009989777,
0.102019292259285));
#284950=CARTESIAN_POINT('Ctrl Pts',(0.473186488074858,-1.48178095462973,
0.103485177221427));
#284951=CARTESIAN_POINT('Ctrl Pts',(0.528121056988836,-1.46423835114498,
0.107640102906867));
#284952=CARTESIAN_POINT('Ctrl Pts',(0.582189715412371,-1.44360129555919,
0.111795028592307));
#284953=CARTESIAN_POINT('Ctrl Pts',(0.635020698669741,-1.41997498649131,
0.115949954277747));
#284954=CARTESIAN_POINT('Ctrl Pts',(0.687760721448913,-1.39638935545436,
0.12009772631955));
#284955=CARTESIAN_POINT('Ctrl Pts',(0.739266829154363,-1.36982489740558,
0.124245498361353));
#284956=CARTESIAN_POINT('Ctrl Pts',(0.789184128374671,-1.3404359968016,
0.128393270403156));
#284957=CARTESIAN_POINT('Ctrl Pts',(0.839053413900563,-1.31107536434744,
0.132537052848918));
#284958=CARTESIAN_POINT('Ctrl Pts',(0.887336474303002,-1.27889593474542,
0.13668083529468));
#284959=CARTESIAN_POINT('Ctrl Pts',(0.933701655331761,-1.24409865719352,
0.140824617740442));
#284960=CARTESIAN_POINT('Ctrl Pts',(0.980039891137898,-1.20932160215277,
0.144965992018307));
#284961=CARTESIAN_POINT('Ctrl Pts',(1.02446204317353,-1.17193002621499,
0.149107366296172));
#284962=CARTESIAN_POINT('Ctrl Pts',(1.0666660281567,-1.13216775893699,0.153248740574037));
#284963=CARTESIAN_POINT('Ctrl Pts',(1.10886155281276,-1.09241346251265,
0.157389284660604));
#284964=CARTESIAN_POINT('Ctrl Pts',(1.14883941601361,-1.05028977407605,
0.161529828747171));
#284965=CARTESIAN_POINT('Ctrl Pts',(1.18633284133866,-1.00607884361085,
0.165670372833738));
#284966=CARTESIAN_POINT('Ctrl Pts',(1.22386110008989,-0.961826838792772,
0.169814763710389));
#284967=CARTESIAN_POINT('Ctrl Pts',(1.25889997157673,-0.915484113028016,
0.17395915458704));
#284968=CARTESIAN_POINT('Ctrl Pts',(1.29122251180059,-0.867366517119135,
0.178103545463692));
#284969=CARTESIAN_POINT('Ctrl Pts',(1.32355891279799,-0.819228287092538,
0.182249713566483));
#284970=CARTESIAN_POINT('Ctrl Pts',(1.35317639412173,-0.769314116146701,
0.186395881669274));
#284971=CARTESIAN_POINT('Ctrl Pts',(1.37989273735347,-0.717966770400374,
0.190542049772064));
#284972=CARTESIAN_POINT('Ctrl Pts',(1.40666131973601,-0.66651902387262,
0.194696324983634));
#284973=CARTESIAN_POINT('Ctrl Pts',(1.43051721271553,-0.613632976563166,
0.198850600195203));
#284974=CARTESIAN_POINT('Ctrl Pts',(1.45132573982812,-0.559672982117566,
0.203004875406773));
#284975=CARTESIAN_POINT('Ctrl Pts',(1.47080505381337,-0.509159859840303,
0.206893782622042));
#284976=CARTESIAN_POINT('Ctrl Pts',(1.48761426769546,-0.457706128643404,
0.210782689837312));
#284977=CARTESIAN_POINT('Ctrl Pts',(1.50168317545456,-0.405620377393322,
0.214671597052581));
#284978=CARTESIAN_POINT('Ctrl Pts',(1.51666767026187,-0.350144950124534,
0.218813589520731));
#284979=CARTESIAN_POINT('Ctrl Pts',(1.5286062889074,-0.293718260314706,
0.222955581988881));
#284980=CARTESIAN_POINT('Ctrl Pts',(1.53738418093832,-0.236706844431258,
0.227097574457031));
#284981=CARTESIAN_POINT('Ctrl Pts',(1.54614616940765,-0.179798720381579,
0.231232062568538));
#284982=CARTESIAN_POINT('Ctrl Pts',(1.55175871768408,-0.122308484821582,
0.235366550680045));
#284983=CARTESIAN_POINT('Ctrl Pts',(1.55415735577001,-0.0646155051513709,
0.239501038791552));
#284984=CARTESIAN_POINT('Ctrl Pts',(1.55655356090739,-0.00698104370958413,
0.24363133327463));
#284985=CARTESIAN_POINT('Ctrl Pts',(1.555742292153,0.050855235112751,0.247761627757708));
#284986=CARTESIAN_POINT('Ctrl Pts',(1.55171076002969,0.108507913112747,
0.251891922240785));
#284987=CARTESIAN_POINT('Ctrl Pts',(1.5476817547115,0.166124456691066,0.2560196280184));
#284988=CARTESIAN_POINT('Ctrl Pts',(1.54043652274323,0.223557107356094,
0.260147333796014));
#284989=CARTESIAN_POINT('Ctrl Pts',(1.53001434149962,0.28042176236072,0.264275039573629));
#284990=CARTESIAN_POINT('Ctrl Pts',(1.51959465360752,0.337272813344219,
0.268401757859161));
#284991=CARTESIAN_POINT('Ctrl Pts',(1.50599961916479,0.393555624638792,
0.272528476144693));
#284992=CARTESIAN_POINT('Ctrl Pts',(1.48931989462697,0.448894755447546,
0.276655194430224));
#284993=CARTESIAN_POINT('Ctrl Pts',(1.4726251746609,0.504283637315656,0.280785622723546));
#284994=CARTESIAN_POINT('Ctrl Pts',(1.45284037227224,0.558726641250366,
0.284916051016867));
#284995=CARTESIAN_POINT('Ctrl Pts',(1.43010610996875,0.611863354214026,
0.289046479310188));
#284996=CARTESIAN_POINT('Ctrl Pts',(1.4073626044815,0.66502167123926,0.293178586932587));
#284997=CARTESIAN_POINT('Ctrl Pts',(1.38166747992618,0.716872168703091,
0.297310694554986));
#284998=CARTESIAN_POINT('Ctrl Pts',(1.35320828435611,0.767077303242633,
0.301442802177385));
#284999=CARTESIAN_POINT('Ctrl Pts',(1.3246931272864,0.817381159989961,0.305583035080018));
#285000=CARTESIAN_POINT('Ctrl Pts',(1.29340332031575,0.866032746432876,
0.30972326798265));
#285001=CARTESIAN_POINT('Ctrl Pts',(1.25957038880755,0.912722677289872,
0.313863500885282));
#285002=CARTESIAN_POINT('Ctrl Pts',(1.22689834291113,0.957810569348262,
0.317861672884771));
#285003=CARTESIAN_POINT('Ctrl Pts',(1.19185523221823,1.00106898154561,0.321859844884259));
#285004=CARTESIAN_POINT('Ctrl Pts',(1.15468296304764,1.04225117167002,0.325858016883747));
#285005=CARTESIAN_POINT('Ctrl Pts',(1.11610928740658,1.08498594357101,0.330006921250001));
#285006=CARTESIAN_POINT('Ctrl Pts',(1.07507917194319,1.1256659486238,0.334155825616254));
#285007=CARTESIAN_POINT('Ctrl Pts',(1.03184004939355,1.1639958601591,0.338304729982508));
#285008=CARTESIAN_POINT('Ctrl Pts',(0.988677842284126,1.2022575889505,0.342446254115608));
#285009=CARTESIAN_POINT('Ctrl Pts',(0.94331481395107,1.23817717943636,0.346587778248709));
#285010=CARTESIAN_POINT('Ctrl Pts',(0.896036373130515,1.27149481635873,
0.350729302381809));
#285011=CARTESIAN_POINT('Ctrl Pts',(0.848804996947713,1.30477928631355,
0.354866703719621));
#285012=CARTESIAN_POINT('Ctrl Pts',(0.799662409525528,1.33546663634278,
0.359004105057433));
#285013=CARTESIAN_POINT('Ctrl Pts',(0.748926998363193,1.36333730276946,
0.363141506395245));
#285014=CARTESIAN_POINT('Ctrl Pts',(0.698222611097356,1.39119092672716,
0.367276377777983));
#285015=CARTESIAN_POINT('Ctrl Pts',(0.645927786148217,1.41623103119483,
0.371411249160722));
#285016=CARTESIAN_POINT('Ctrl Pts',(0.592387918214518,1.43828258848999,
0.37554612054346));
#285017=CARTESIAN_POINT('Ctrl Pts',(0.538860231172223,1.46032912882051,
0.379680051198826));
#285018=CARTESIAN_POINT('Ctrl Pts',(0.484088544589072,1.47938827365183,
0.383813981854192));
#285019=CARTESIAN_POINT('Ctrl Pts',(0.428438729962962,1.49533290763887,
0.387947912509558));
#285020=CARTESIAN_POINT('Ctrl Pts',(0.37273875664476,1.51129191295837,0.392085569189103));
#285021=CARTESIAN_POINT('Ctrl Pts',(0.316159574878584,1.52413065256782,
0.396223225868648));
#285022=CARTESIAN_POINT('Ctrl Pts',(0.259081434718245,1.53377216697407,
0.400360882548193));
#285023=CARTESIAN_POINT('Ctrl Pts',(0.201979838666644,1.5434176434981,0.404500239570897));
#285024=CARTESIAN_POINT('Ctrl Pts',(0.144379393759639,1.54986321606351,
0.408639596593601));
#285025=CARTESIAN_POINT('Ctrl Pts',(0.0866665186968121,1.55308375966558,
0.412778953616306));
#285026=CARTESIAN_POINT('Ctrl Pts',(0.0288411893126411,1.55631057854063,
0.41692637623242));
#285027=CARTESIAN_POINT('Ctrl Pts',(-0.0290964855246801,1.5562998092828,
0.421073798848535));
#285028=CARTESIAN_POINT('Ctrl Pts',(-0.086759951318526,1.5530785430387,
0.425221221464649));
#285029=CARTESIAN_POINT('Ctrl Pts',(-0.141554429018789,1.55001754767623,
0.429162293214736));
#285030=CARTESIAN_POINT('Ctrl Pts',(-0.196100950596859,1.54405805300416,
0.433103364964823));
#285031=CARTESIAN_POINT('Ctrl Pts',(-0.250076008008153,1.53526617894706,
0.43704443671491));
#285032=CARTESIAN_POINT('Ctrl Pts',(-0.30689233740269,1.52601149657374,
0.441192968304496));
#285033=CARTESIAN_POINT('Ctrl Pts',(-0.363313166993611,1.51357924117281,
0.445341499894082));
#285034=CARTESIAN_POINT('Ctrl Pts',(-0.418956256220377,1.49801732479094,
0.449490031483667));
#285035=CARTESIAN_POINT('Ctrl Pts',(-0.474500677109199,1.48248300336194,
0.453631206747022));
#285036=CARTESIAN_POINT('Ctrl Pts',(-0.52926959769328,1.46383017528532,
0.457772382010377));
#285037=CARTESIAN_POINT('Ctrl Pts',(-0.582890043296543,1.44215791348443,
0.461913557273732));
#285038=CARTESIAN_POINT('Ctrl Pts',(-0.63645729780394,1.42050715041116,
0.46605062452105));
#285039=CARTESIAN_POINT('Ctrl Pts',(-0.688877854292931,1.39584308225942,
0.470187691768368));
#285040=CARTESIAN_POINT('Ctrl Pts',(-0.739794699741476,1.36831431046906,
0.474324759015686));
#285041=CARTESIAN_POINT('Ctrl Pts',(-0.790680597008529,1.34080227116513,
0.47845931167855));
#285042=CARTESIAN_POINT('Ctrl Pts',(-0.840064137935306,1.31042922695258,
0.482593864341414));
#285043=CARTESIAN_POINT('Ctrl Pts',(-0.887611108960229,1.27739060950455,
0.486728417004278));
#285044=CARTESIAN_POINT('Ctrl Pts',(-0.93514744547065,1.24435938158415,
0.49086204491927));
#285045=CARTESIAN_POINT('Ctrl Pts',(-0.98084760021021,1.20866406100027,
0.494995672834262));
#285046=CARTESIAN_POINT('Ctrl Pts',(-1.02440653623954,1.17054324931192,
0.499129300749254));
#285047=CARTESIAN_POINT('Ctrl Pts',(-1.06800502952157,1.13238781890423,
0.50326668254299));
#285048=CARTESIAN_POINT('Ctrl Pts',(-1.10945802465527,1.09180283844611,
0.507404064336726));
#285049=CARTESIAN_POINT('Ctrl Pts',(-1.14849484981261,1.04906617043631,
0.511541446130461));
#285050=CARTESIAN_POINT('Ctrl Pts',(-1.18754785708328,1.00631178660045,
0.515680543011958));
#285051=CARTESIAN_POINT('Ctrl Pts',(-1.22418236682099,0.961404340584704,
0.519819639893454));
#285052=CARTESIAN_POINT('Ctrl Pts',(-1.25816793488278,0.914654960973155,
0.52395873677495));
#285053=CARTESIAN_POINT('Ctrl Pts',(-1.29221996491882,0.867814158553604,
0.528105928049627));
#285054=CARTESIAN_POINT('Ctrl Pts',(-1.32361241689602,0.819124662742743,
0.532253119324303));
#285055=CARTESIAN_POINT('Ctrl Pts',(-1.35215866213414,0.768926005813061,
0.536400310598979));
#285056=CARTESIAN_POINT('Ctrl Pts',(-1.37930295036351,0.72119269444196,
0.540343825914677));
#285057=CARTESIAN_POINT('Ctrl Pts',(-1.40387393461122,0.672095371638328,
0.544287341230373));
#285058=CARTESIAN_POINT('Ctrl Pts',(-1.42575171809473,0.621942351307516,
0.548230856546071));
#285059=CARTESIAN_POINT('Ctrl Pts',(-1.45109454208923,0.563846010423896,
0.552798952516151));
#285060=CARTESIAN_POINT('Ctrl Pts',(-1.47291535250019,0.504123591953479,
0.557367048486231));
#285061=CARTESIAN_POINT('Ctrl Pts',(-1.49102528336013,0.443197308634467,
0.561935144456311));
#285062=CARTESIAN_POINT('Ctrl Pts',(-1.50907657817563,0.382468291461024,
0.566488449918329));
#285063=CARTESIAN_POINT('Ctrl Pts',(-1.52344080755184,0.320543489155571,
0.571041755380347));
#285064=CARTESIAN_POINT('Ctrl Pts',(-1.53397736366261,0.257863719376566,
0.575595060842365));
#285065=CARTESIAN_POINT('Ctrl Pts',(-1.54446015602563,0.195503778894309,
0.580125132644003));
#285066=CARTESIAN_POINT('Ctrl Pts',(-1.55115409873917,0.132396873497183,
0.584655204445641));
#285067=CARTESIAN_POINT('Ctrl Pts',(-1.55396909178788,0.0689950126310516,
0.589185276247278));
#285068=CARTESIAN_POINT('Ctrl Pts',(-1.55497803006196,0.0462707774485264,
0.590808926020452));
#285069=CARTESIAN_POINT('Ctrl Pts',(-1.55548913384293,0.0235087962157958,
0.592432575793627));
#285070=CARTESIAN_POINT('Ctrl Pts',(-1.55549982855345,0.00073032197892629,
0.594056225566802));
#285071=CARTESIAN_POINT('',(0.903606778650206,-1.26612599672284,0.));
#285072=CARTESIAN_POINT('Origin',(0.,0.,0.));
#285073=CARTESIAN_POINT('',(-1.55549967063145,0.00101225759537372,0.455943774396301));
#285074=CARTESIAN_POINT('Ctrl Pts',(0.903606778650206,-1.26612599672284,
-2.66453525910038E-15));
#285075=CARTESIAN_POINT('Ctrl Pts',(0.951852882766262,-1.23169379421253,
0.00424525219639006));
#285076=CARTESIAN_POINT('Ctrl Pts',(0.998166564555117,-1.19447316528589,
0.0084905043927825));
#285077=CARTESIAN_POINT('Ctrl Pts',(1.04222410325038,-1.1547073952322,0.0127357565891753));
#285078=CARTESIAN_POINT('Ctrl Pts',(1.08626041427952,-1.11496078499804,
0.0169789633513723));
#285079=CARTESIAN_POINT('Ctrl Pts',(1.12804237788175,-1.07267179026597,
0.0212221701135694));
#285080=CARTESIAN_POINT('Ctrl Pts',(1.1672798477831,-1.02812353681815,0.0254653768757664));
#285081=CARTESIAN_POINT('Ctrl Pts',(1.20650768566346,-0.9835862190834,0.0297075420148228));
#285082=CARTESIAN_POINT('Ctrl Pts',(1.24319194927828,-0.93679110831928,
0.0339497071538796));
#285083=CARTESIAN_POINT('Ctrl Pts',(1.27708111921595,-0.888056341085483,
0.038191872292936));
#285084=CARTESIAN_POINT('Ctrl Pts',(1.3109722297727,-0.83931878311885,0.0424342803540421));
#285085=CARTESIAN_POINT('Ctrl Pts',(1.34206765177606,-0.78864174716061,
0.0466766884151483));
#285086=CARTESIAN_POINT('Ctrl Pts',(1.37015878773367,-0.736372966910253,
0.0509190964762545));
#285087=CARTESIAN_POINT('Ctrl Pts',(1.39826003751312,-0.684085368014315,
0.055163031957234));
#285088=CARTESIAN_POINT('Ctrl Pts',(1.4233546235329,-0.630205314661143,
0.0594069674382136));
#285089=CARTESIAN_POINT('Ctrl Pts',(1.44528039378935,-0.57510419345377,
0.0636509029191932));
#285090=CARTESIAN_POINT('Ctrl Pts',(1.46723931600862,-0.519919758853032,
0.0679012552689841));
#285091=CARTESIAN_POINT('Ctrl Pts',(1.48601967649052,-0.463511022720185,
0.072151607618775));
#285092=CARTESIAN_POINT('Ctrl Pts',(1.50150818912007,-0.406267655622951,
0.0764019599685659));
#285093=CARTESIAN_POINT('Ctrl Pts',(1.51700870532063,-0.348979925013326,
0.0806556063342175));
#285094=CARTESIAN_POINT('Ctrl Pts',(1.52921219044332,-0.290856750535091,
0.084909252699869));
#285095=CARTESIAN_POINT('Ctrl Pts',(1.53805649602739,-0.232298224332338,
0.0891628990655207));
#285096=CARTESIAN_POINT('Ctrl Pts',(1.54691960323129,-0.17361521179909,
0.0934255880226038));
#285097=CARTESIAN_POINT('Ctrl Pts',(1.55240921601056,-0.11449548309292,
0.0976882769796872));
#285098=CARTESIAN_POINT('Ctrl Pts',(1.55451513276463,-0.0553439428100182,
0.10195096593677));
#285099=CARTESIAN_POINT('Ctrl Pts',(1.55602369846608,-0.0129709550429866,
0.105004527452993));
#285100=CARTESIAN_POINT('Ctrl Pts',(1.55579701690475,0.0294182924525364,
0.108058088969215));
#285101=CARTESIAN_POINT('Ctrl Pts',(1.55384772416179,0.0716763567519665,
0.111111650485437));
#285102=CARTESIAN_POINT('Ctrl Pts',(1.55122696287,0.128490962758032,0.115217065566218));
#285103=CARTESIAN_POINT('Ctrl Pts',(1.54547918115449,0.185306670723197,
0.119322480646998));
#285104=CARTESIAN_POINT('Ctrl Pts',(1.53659989632352,0.241745752017594,
0.123427895727778));
#285105=CARTESIAN_POINT('Ctrl Pts',(1.52769669037597,0.298336882251616,
0.12754437094624));
#285106=CARTESIAN_POINT('Ctrl Pts',(1.51564503470383,0.354548813343556,
0.131660846164702));
#285107=CARTESIAN_POINT('Ctrl Pts',(1.50049316548028,0.410000622373876,
0.135777321383164));
#285108=CARTESIAN_POINT('Ctrl Pts',(1.48542979547808,0.465128547806137,
0.139869753043293));
#285109=CARTESIAN_POINT('Ctrl Pts',(1.46730243414887,0.519504679849655,
0.143962184703423));
#285110=CARTESIAN_POINT('Ctrl Pts',(1.44620997094002,0.572762577298553,
0.148054616363552));
#285111=CARTESIAN_POINT('Ctrl Pts',(1.42513293513202,0.625981520978749,
0.152144054746741));
#285112=CARTESIAN_POINT('Ctrl Pts',(1.40109528796121,0.678083355662404,
0.15623349312993));
#285113=CARTESIAN_POINT('Ctrl Pts',(1.37424533484884,0.728718059091574,
0.160322931513119));
#285114=CARTESIAN_POINT('Ctrl Pts',(1.34740416125953,0.779336205748967,
0.164411032712649));
#285115=CARTESIAN_POINT('Ctrl Pts',(1.31775275451934,0.828487701729929,
0.16849913391218));
#285116=CARTESIAN_POINT('Ctrl Pts',(1.28548597986787,0.875845902863714,
0.17258723511171));
#285117=CARTESIAN_POINT('Ctrl Pts',(1.25283847284091,0.92376290792542,0.176723573933306));
#285118=CARTESIAN_POINT('Ctrl Pts',(1.21751374817111,0.969843534822608,
0.180859912754903));
#285119=CARTESIAN_POINT('Ctrl Pts',(1.17975806830724,1.01378062235572,0.1849962515765));
#285120=CARTESIAN_POINT('Ctrl Pts',(1.14239776976453,1.05725759623762,0.189089274237086));
#285121=CARTESIAN_POINT('Ctrl Pts',(1.10265761423722,1.09863536954959,0.193182296897672));
#285122=CARTESIAN_POINT('Ctrl Pts',(1.06081405722401,1.13765275281869,0.197275319558258));
#285123=CARTESIAN_POINT('Ctrl Pts',(1.01830625923178,1.17728951328015,0.20143331646036));
#285124=CARTESIAN_POINT('Ctrl Pts',(0.973628121102911,1.21448990844618,
0.205591313362462));
#285125=CARTESIAN_POINT('Ctrl Pts',(0.927102762918045,1.24902390569185,
0.209749310264563));
#285126=CARTESIAN_POINT('Ctrl Pts',(0.880577404733179,1.28355790293752,
0.213907307166665));
#285127=CARTESIAN_POINT('Ctrl Pts',(0.832205342047452,1.31542525247013,
0.218065304068767));
#285128=CARTESIAN_POINT('Ctrl Pts',(0.782335877333532,1.34444442988053,
0.222223300970868));
#285129=CARTESIAN_POINT('Ctrl Pts',(0.732509368814128,1.37343861096428,
0.226377716288031));
#285130=CARTESIAN_POINT('Ctrl Pts',(0.680966157084891,1.39971889273661,
0.230532131605194));
#285131=CARTESIAN_POINT('Ctrl Pts',(0.628032950359753,1.42307935943939,
0.234686546922357));
#285132=CARTESIAN_POINT('Ctrl Pts',(0.575193788895018,1.44639832211643,
0.238833581181494));
#285133=CARTESIAN_POINT('Ctrl Pts',(0.520970005675055,1.46680755965869,
0.242980615440632));
#285134=CARTESIAN_POINT('Ctrl Pts',(0.465713586530266,1.48414659158761,
0.247127649699769));
#285135=CARTESIAN_POINT('Ctrl Pts',(0.410512158653983,1.5014683676868,0.251270556824395));
#285136=CARTESIAN_POINT('Ctrl Pts',(0.354280623928115,1.51572583817242,
0.255413463949021));
#285137=CARTESIAN_POINT('Ctrl Pts',(0.297390058907445,1.52680693044767,
0.259556371073646));
#285138=CARTESIAN_POINT('Ctrl Pts',(0.240534433202252,1.53788121727497,
0.263696733833684));
#285139=CARTESIAN_POINT('Ctrl Pts',(0.183021087950222,1.54578289435644,
0.267837096593722));
#285140=CARTESIAN_POINT('Ctrl Pts',(0.125233215870697,1.55045054472649,
0.27197745935376));
#285141=CARTESIAN_POINT('Ctrl Pts',(0.0674588154273806,1.5551171069636,
0.276116856903298));
#285142=CARTESIAN_POINT('Ctrl Pts',(0.00941053221514308,1.55655109758077,
0.280256254452836));
#285143=CARTESIAN_POINT('Ctrl Pts',(-0.0485235526154023,1.55474297388397,
0.284395652002374));
#285144=CARTESIAN_POINT('Ctrl Pts',(-0.106508490692881,1.55293326305655,
0.288538683022716));
#285145=CARTESIAN_POINT('Ctrl Pts',(-0.16437851010345,1.54787576549528,
0.292681714043058));
#285146=CARTESIAN_POINT('Ctrl Pts',(-0.22174712659336,1.53961308835941,
0.296824745063399));
#285147=CARTESIAN_POINT('Ctrl Pts',(-0.279138774167105,1.53134709410659,
0.30096943933624));
#285148=CARTESIAN_POINT('Ctrl Pts',(-0.336028107311789,1.519873455748,0.305114133609081));
#285149=CARTESIAN_POINT('Ctrl Pts',(-0.392038530311958,1.50528603286912,
0.309258827881922));
#285150=CARTESIAN_POINT('Ctrl Pts',(-0.448155821396572,1.49067077713598,
0.31341143024604));
#285151=CARTESIAN_POINT('Ctrl Pts',(-0.503390354672071,1.47293002177716,
0.317564032610157));
#285152=CARTESIAN_POINT('Ctrl Pts',(-0.557381292354335,1.45220740424135,
0.321716634974275));
#285153=CARTESIAN_POINT('Ctrl Pts',(-0.607733958478008,1.43288121568486,
0.325589407134954));
#285154=CARTESIAN_POINT('Ctrl Pts',(-0.657004868931625,1.41096214318115,
0.329462179295632));
#285155=CARTESIAN_POINT('Ctrl Pts',(-0.704920767250419,1.38660266907975,
0.333334951456311));
#285156=CARTESIAN_POINT('Ctrl Pts',(-0.756331651611818,1.36046641472427,
0.337490203652274));
#285157=CARTESIAN_POINT('Ctrl Pts',(-0.806390623719567,1.33141440363412,
0.341645455848236));
#285158=CARTESIAN_POINT('Ctrl Pts',(-0.854747604328637,1.29961024268604,
0.345800708044198));
#285159=CARTESIAN_POINT('Ctrl Pts',(-0.903021453830198,1.26786075668022,
0.349948816892651));
#285160=CARTESIAN_POINT('Ctrl Pts',(-0.949598689923335,1.2333687953876,
0.354096925741104));
#285161=CARTESIAN_POINT('Ctrl Pts',(-0.994153791582626,1.19634380036923,
0.358245034589556));
#285162=CARTESIAN_POINT('Ctrl Pts',(-1.03866610911375,1.1593543586786,0.362389160207941));
#285163=CARTESIAN_POINT('Ctrl Pts',(-1.08115974297499,1.11983703316806,
0.366533285826326));
#285164=CARTESIAN_POINT('Ctrl Pts',(-1.1213395937073,1.07804348965353,0.37067741144471));
#285165=CARTESIAN_POINT('Ctrl Pts',(-1.16149615113547,1.0362741749428,0.374819134605727));
#285166=CARTESIAN_POINT('Ctrl Pts',(-1.19934122602266,0.992231631646827,
0.378960857766743));
#285167=CARTESIAN_POINT('Ctrl Pts',(-1.23461579669431,0.946205096452601,
0.38310258092776));
#285168=CARTESIAN_POINT('Ctrl Pts',(-1.26988333983836,0.900187730831256,
0.387243478959701));
#285169=CARTESIAN_POINT('Ctrl Pts',(-1.30258108037958,0.85218756974644,
0.391384376991643));
#285170=CARTESIAN_POINT('Ctrl Pts',(-1.33249100202178,0.802525999286622,
0.395525275023585));
#285171=CARTESIAN_POINT('Ctrl Pts',(-1.36242868649098,0.752818332230301,
0.399670016697683));
#285172=CARTESIAN_POINT('Ctrl Pts',(-1.38957311222174,0.701446619159402,
0.40381475837178));
#285173=CARTESIAN_POINT('Ctrl Pts',(-1.41375099283611,0.648759108032348,
0.407959500045878));
#285174=CARTESIAN_POINT('Ctrl Pts',(-1.43793926211777,0.596048958319524,
0.412106022618103));
#285175=CARTESIAN_POINT('Ctrl Pts',(-1.45915825416503,0.542022366868642,
0.416252545190328));
#285176=CARTESIAN_POINT('Ctrl Pts',(-1.47728315018204,0.487046963021249,
0.420399067762553));
#285177=CARTESIAN_POINT('Ctrl Pts',(-1.49544339049082,0.4319643548781,0.424553676224122));
#285178=CARTESIAN_POINT('Ctrl Pts',(-1.5104973412724,0.375929739341496,
0.428708284685691));
#285179=CARTESIAN_POINT('Ctrl Pts',(-1.52237057598149,0.319324410883043,
0.43286289314726));
#285180=CARTESIAN_POINT('Ctrl Pts',(-1.53340539788194,0.266716193033383,
0.436724129412089));
#285181=CARTESIAN_POINT('Ctrl Pts',(-1.54169334567415,0.21361545867419,
0.440585365676917));
#285182=CARTESIAN_POINT('Ctrl Pts',(-1.54721495399917,0.160331332313241,
0.444446601941745));
#285183=CARTESIAN_POINT('Ctrl Pts',(-1.55269531303319,0.107445266137791,
0.44827899275993));
#285184=CARTESIAN_POINT('Ctrl Pts',(-1.55546501227888,0.0542704956696049,
0.452111383578116));
#285185=CARTESIAN_POINT('Ctrl Pts',(-1.55549967063145,0.00101225759537372,
0.455943774396301));
#285186=CARTESIAN_POINT('',(-1.55549938660524,-0.00138140172760619,1.85539343273712));
#285187=CARTESIAN_POINT('Ctrl Pts',(-1.55549962201023,0.00108440122680404,
0.457011256470473));
#285188=CARTESIAN_POINT('Ctrl Pts',(-1.5555667906038,-0.0952643664786917,
0.463522872456782));
#285189=CARTESIAN_POINT('Ctrl Pts',(-1.54668208355373,-0.191420635597107,
0.469766099184208));
#285190=CARTESIAN_POINT('Ctrl Pts',(-1.51736458895052,-0.34807208354269,
0.480306286301398));
#285191=CARTESIAN_POINT('Ctrl Pts',(-1.5020245696063,-0.409231530846319,
0.484515805592852));
#285192=CARTESIAN_POINT('Ctrl Pts',(-1.47503044214394,-0.494536919273511,
0.490652697112903));
#285193=CARTESIAN_POINT('Ctrl Pts',(-1.46639774811665,-0.519575857388309,
0.492487163666517));
#285194=CARTESIAN_POINT('Ctrl Pts',(-1.45276447622374,-0.556067682209315,
0.495216689650924));
#285195=CARTESIAN_POINT('Ctrl Pts',(-1.44825804897068,-0.567701063900379,
0.496095351772404));
#285196=CARTESIAN_POINT('Ctrl Pts',(-1.43998888066032,-0.588308542359477,
0.49766770145831));
#285197=CARTESIAN_POINT('Ctrl Pts',(-1.43628090183011,-0.597304010173798,
0.498359507023726));
#285198=CARTESIAN_POINT('Ctrl Pts',(-1.42825833213423,-0.616259849989553,
0.499829221071941));
#285199=CARTESIAN_POINT('Ctrl Pts',(-1.4239234020208,-0.626210986858212,
0.500607795169071));
#285200=CARTESIAN_POINT('Ctrl Pts',(-1.41199445171519,-0.652830300236169,
0.502709913162139));
#285201=CARTESIAN_POINT('Ctrl Pts',(-1.4042097937536,-0.669410587084619,
0.504039955699443));
#285202=CARTESIAN_POINT('Ctrl Pts',(-1.35580405346299,-0.767946755324809,
0.512072867808739));
#285203=CARTESIAN_POINT('Ctrl Pts',(-1.30831836597364,-0.846312187792799,
0.519016683963832));
#285204=CARTESIAN_POINT('Ctrl Pts',(-1.2149772121204,-0.973558347105258,
0.531210936975088));
#285205=CARTESIAN_POINT('Ctrl Pts',(-1.17233508295044,-1.02450765349571,
0.536387174881569));
#285206=CARTESIAN_POINT('Ctrl Pts',(-1.10256064712219,-1.09779441213796,
0.544179981801476));
#285207=CARTESIAN_POINT('Ctrl Pts',(-1.07771061982276,-1.1221999355986,
0.546840678859995));
#285208=CARTESIAN_POINT('Ctrl Pts',(-1.04106387193628,-1.15584997325019,
0.550582626796932));
#285209=CARTESIAN_POINT('Ctrl Pts',(-1.0299216335618,-1.16578926645013,
0.551697646722261));
#285210=CARTESIAN_POINT('Ctrl Pts',(-1.01015004584692,-1.18292149395355,
0.553634444765031));
#285211=CARTESIAN_POINT('Ctrl Pts',(-1.00158281784291,-1.19018412628193,
0.554460358583519));
#285212=CARTESIAN_POINT('Ctrl Pts',(-0.988005322102365,-1.20144362610956,
0.555747556718756));
#285213=CARTESIAN_POINT('Ctrl Pts',(-0.983047944712801,-1.20550323333759,
0.556213073350035));
#285214=CARTESIAN_POINT('Ctrl Pts',(-0.974052946841916,-1.21277686955253,
0.557049506370322));
#285215=CARTESIAN_POINT('Ctrl Pts',(-0.970024368040723,-1.21600148238476,
0.557421154172974));
#285216=CARTESIAN_POINT('Ctrl Pts',(-0.960516268764562,-1.22353476974095,
0.558291472733171));
#285217=CARTESIAN_POINT('Ctrl Pts',(-0.955023736897941,-1.22782673951306,
0.558788968528576));
#285218=CARTESIAN_POINT('Ctrl Pts',(-0.937971839341733,-1.24096776494697,
0.560317971301154));
#285219=CARTESIAN_POINT('Ctrl Pts',(-0.926316560127726,-1.2496918962324,
0.561341294350341));
#285220=CARTESIAN_POINT('Ctrl Pts',(-0.838174312089929,-1.31375667834253,
0.568933312501299));
#285221=CARTESIAN_POINT('Ctrl Pts',(-0.756902700560442,-1.36220270384782,
0.575124928745838));
#285222=CARTESIAN_POINT('Ctrl Pts',(-0.575125304043796,-1.44923517816546,
0.588389690283717));
#285223=CARTESIAN_POINT('Ctrl Pts',(-0.474017020858618,-1.48538058091112,
0.595446141950153));
#285224=CARTESIAN_POINT('Ctrl Pts',(-0.351753700339952,-1.51532262894242,
0.604169862864003));
#285225=CARTESIAN_POINT('Ctrl Pts',(-0.333423697013755,-1.51946106264904,
0.605481795312001));
#285226=CARTESIAN_POINT('Ctrl Pts',(-0.304227608808861,-1.52549905177316,
0.607580183211123));
#285227=CARTESIAN_POINT('Ctrl Pts',(-0.293408151255459,-1.52761691548243,
0.608359683975519));
#285228=CARTESIAN_POINT('Ctrl Pts',(-0.272911744290726,-1.53140322642213,
0.609840380750816));
#285229=CARTESIAN_POINT('Ctrl Pts',(-0.263239683424221,-1.53309540571897,
0.610540785661379));
#285230=CARTESIAN_POINT('Ctrl Pts',(-0.241213080022269,-1.53673449759373,
0.612139982973226));
#285231=CARTESIAN_POINT('Ctrl Pts',(-0.228849916592012,-1.53862417920436,
0.613040533770189));
#285232=CARTESIAN_POINT('Ctrl Pts',(-0.196443564155182,-1.54317820628427,
0.615409372237364));
#285233=CARTESIAN_POINT('Ctrl Pts',(-0.176369447261966,-1.54560111200429,
0.616885063252536));
#285234=CARTESIAN_POINT('Ctrl Pts',(-0.0476575329217699,-1.55859634331593,
0.626403878854123));
#285235=CARTESIAN_POINT('Ctrl Pts',(0.0617727447775499,-1.5580980607613,
0.634787487670447));
#285236=CARTESIAN_POINT('Ctrl Pts',(0.256258299720361,-1.53668565651187,
0.649949991889133));
#285237=CARTESIAN_POINT('Ctrl Pts',(0.341356401174011,-1.52004932154656,
0.656667032904326));
#285238=CARTESIAN_POINT('Ctrl Pts',(0.437570273885015,-1.49274689260988,
0.664092969128434));
#285239=CARTESIAN_POINT('Ctrl Pts',(0.450457470168279,-1.48890870431262,
0.665083810553853));
#285240=CARTESIAN_POINT('Ctrl Pts',(0.469757372351605,-1.48288708445105,
0.666560329559166));
#285241=CARTESIAN_POINT('Ctrl Pts',(0.476207833531309,-1.48082821353068,
0.667052567352394));
#285242=CARTESIAN_POINT('Ctrl Pts',(0.48788234539948,-1.47701774574191,
0.667940931733326));
#285243=CARTESIAN_POINT('Ctrl Pts',(0.493110705210416,-1.47528046116991,
0.66833783413931));
#285244=CARTESIAN_POINT('Ctrl Pts',(0.504941530025822,-1.47127937968552,
0.669233842330833));
#285245=CARTESIAN_POINT('Ctrl Pts',(0.511538104108221,-1.46899888865372,
0.669731973769434));
#285246=CARTESIAN_POINT('Ctrl Pts',(0.531868360863221,-1.46181699428555,
0.671263323820655));
#285247=CARTESIAN_POINT('Ctrl Pts',(0.545549123394672,-1.45676664988181,
0.6722883407645));
#285248=CARTESIAN_POINT('Ctrl Pts',(0.647528959665822,-1.41748189028475,
0.679902469179764));
#285249=CARTESIAN_POINT('Ctrl Pts',(0.732620110252397,-1.3754350492819,
0.686112818056511));
#285250=CARTESIAN_POINT('Ctrl Pts',(0.903823441089378,-1.27041137090509,
0.699334689682724));
#285251=CARTESIAN_POINT('Ctrl Pts',(0.988352246591539,-1.20581825710198,
0.706329223151749));
#285252=CARTESIAN_POINT('Ctrl Pts',(1.07940745208067,-1.1201860486624,0.714990427013295));
#285253=CARTESIAN_POINT('Ctrl Pts',(1.09293354099202,-1.10699297760284,
0.716309400724588));
#285254=CARTESIAN_POINT('Ctrl Pts',(1.11397054148655,-1.08571246882721,
0.71841533495862));
#285255=CARTESIAN_POINT('Ctrl Pts',(1.12164174907549,-1.07778555739638,
0.719195220407781));
#285256=CARTESIAN_POINT('Ctrl Pts',(1.13596162029258,-1.0626698993592,0.720674298863155));
#285257=CARTESIAN_POINT('Ctrl Pts',(1.14262800828263,-1.05549862359959,
0.721372679105271));
#285258=CARTESIAN_POINT('Ctrl Pts',(1.15759924031393,-1.03908547410529,
0.722963914867381));
#285259=CARTESIAN_POINT('Ctrl Pts',(1.16586185040426,-1.02980617245094,
0.723858488477346));
#285260=CARTESIAN_POINT('Ctrl Pts',(1.18712089011909,-1.00534747056702,
0.726204034046302));
#285261=CARTESIAN_POINT('Ctrl Pts',(1.19993715984496,-0.990015296872858,
0.727662213679683));
#285262=CARTESIAN_POINT('Ctrl Pts',(1.29901309735352,-0.866739491199842,
0.739296697016701));
#285263=CARTESIAN_POINT('Ctrl Pts',(1.37082093130347,-0.748001743211682,
0.750050803731656));
#285264=CARTESIAN_POINT('Ctrl Pts',(1.44915592951412,-0.568232994353586,
0.765209965825307));
#285265=CARTESIAN_POINT('Ctrl Pts',(1.46932932540556,-0.513823296881486,
0.769655047176511));
#285266=CARTESIAN_POINT('Ctrl Pts',(1.49061345318299,-0.444808226909711,
0.775026277013295));
#285267=CARTESIAN_POINT('Ctrl Pts',(1.49462124918349,-0.431149840675565,
0.77607648628857));
#285268=CARTESIAN_POINT('Ctrl Pts',(1.50029442656547,-0.41078531242999,
0.777621543818321));
#285269=CARTESIAN_POINT('Ctrl Pts',(1.50210339490843,-0.404120446376975,
0.778123923972071));
#285270=CARTESIAN_POINT('Ctrl Pts',(1.50527014882244,-0.392137916189078,
0.779020985674077));
#285271=CARTESIAN_POINT('Ctrl Pts',(1.50664423998674,-0.38682489987429,
0.779416558839735));
#285272=CARTESIAN_POINT('Ctrl Pts',(1.50965406194167,-0.374927837351514,
0.780297482009525));
#285273=CARTESIAN_POINT('Ctrl Pts',(1.51127486933405,-0.3683402555975,0.780781984877572));
#285274=CARTESIAN_POINT('Ctrl Pts',(1.51602044387741,-0.348493645790211,
0.782232409933254));
#285275=CARTESIAN_POINT('Ctrl Pts',(1.51901429496548,-0.335203538695478,
0.783191294002216));
#285276=CARTESIAN_POINT('Ctrl Pts',(1.54379068837973,-0.218060194606904,
0.791548698154986));
#285277=CARTESIAN_POINT('Ctrl Pts',(1.55507099733175,-0.112254400347374,
0.798459455698855));
#285278=CARTESIAN_POINT('Ctrl Pts',(1.55587052273721,0.0912578720928381,
0.811861676785551));
#285279=CARTESIAN_POINT('Ctrl Pts',(1.54711022833714,0.188433933236837,
0.818314123034896));
#285280=CARTESIAN_POINT('Ctrl Pts',(1.52597396101626,0.302193047239724,
0.826337218270069));
#285281=CARTESIAN_POINT('Ctrl Pts',(1.52230191923734,0.320178051528094,
0.827619264765608));
#285282=CARTESIAN_POINT('Ctrl Pts',(1.51594212305779,0.348738691168585,
0.829679151322305));
#285283=CARTESIAN_POINT('Ctrl Pts',(1.51345978607519,0.35935867903532,0.830450421998017));
#285284=CARTESIAN_POINT('Ctrl Pts',(1.50853616955192,0.379466520340075,
0.831921315337869));
#285285=CARTESIAN_POINT('Ctrl Pts',(1.50611652046251,0.388959167032835,
0.832620209723373));
#285286=CARTESIAN_POINT('Ctrl Pts',(1.500382335635,0.410599112165217,0.834224092354007));
#285287=CARTESIAN_POINT('Ctrl Pts',(1.49700968322077,0.42273014443356,0.835130922750599));
#285288=CARTESIAN_POINT('Ctrl Pts',(1.48773344529977,0.454591641501024,
0.837533702436166));
#285289=CARTESIAN_POINT('Ctrl Pts',(1.48158482280585,0.47424751174372,0.83903747482399));
#285290=CARTESIAN_POINT('Ctrl Pts',(1.43503539622272,0.613304138525477,
0.84983423902332));
#285291=CARTESIAN_POINT('Ctrl Pts',(1.38064881879389,0.727506111240285,
0.859596094983298));
#285292=CARTESIAN_POINT('Ctrl Pts',(1.27703955255074,0.890660294626937,
0.874570790014807));
#285293=CARTESIAN_POINT('Ctrl Pts',(1.23732649886358,0.945055963326695,
0.879755852415531));
#285294=CARTESIAN_POINT('Ctrl Pts',(1.1844633732475,1.008393885516,0.885901408536068));
#285295=CARTESIAN_POINT('Ctrl Pts',(1.1745435130652,1.01993102355494,0.887025422848414));
#285296=CARTESIAN_POINT('Ctrl Pts',(1.15975660654385,1.03662678487482,0.888656557062117));
#285297=CARTESIAN_POINT('Ctrl Pts',(1.1550213922533,1.04190021894522,0.889172437665247));
#285298=CARTESIAN_POINT('Ctrl Pts',(1.14690453652376,1.05081631772866,0.890045555180362));
#285299=CARTESIAN_POINT('Ctrl Pts',(1.14354127878659,1.05447536521609,0.890404117735157));
#285300=CARTESIAN_POINT('Ctrl Pts',(1.13580786444651,1.06280839550965,0.891221232468432));
#285301=CARTESIAN_POINT('Ctrl Pts',(1.13142634310609,1.06747160362377,0.891678914329007));
#285302=CARTESIAN_POINT('Ctrl Pts',(1.11915997915638,1.08036619301065,0.892946119010653));
#285303=CARTESIAN_POINT('Ctrl Pts',(1.11121305249337,1.0885383511476,0.893751105976));
#285304=CARTESIAN_POINT('Ctrl Pts',(1.04939098454774,1.15072989959583,0.89989894688164));
#285305=CARTESIAN_POINT('Ctrl Pts',(0.991689325822598,1.20081487450592,
0.904980637209143));
#285306=CARTESIAN_POINT('Ctrl Pts',(0.882984838000079,1.28196700428943,
0.913937370298206));
#285307=CARTESIAN_POINT('Ctrl Pts',(0.833441039812106,1.31471578876308,
0.917821697021506));
#285308=CARTESIAN_POINT('Ctrl Pts',(0.740216072170568,1.3689461857553,0.924972121924322));
#285309=CARTESIAN_POINT('Ctrl Pts',(0.697169266407,1.39136190415368,0.928217222696012));
#285310=CARTESIAN_POINT('Ctrl Pts',(0.623337585155679,1.42552074065277,
0.933761166256555));
#285311=CARTESIAN_POINT('Ctrl Pts',(0.593099823651336,1.43836416321218,
0.936025565390904));
#285312=CARTESIAN_POINT('Ctrl Pts',(0.549798943921752,1.455158537499,0.939272883801638));
#285313=CARTESIAN_POINT('Ctrl Pts',(0.537054350148807,1.45991022061633,
0.940229177484577));
#285314=CARTESIAN_POINT('Ctrl Pts',(0.514878171840621,1.46784869534701,
0.941894943933038));
#285315=CARTESIAN_POINT('Ctrl Pts',(0.505475130639414,1.471113254714,0.942601797908856));
#285316=CARTESIAN_POINT('Ctrl Pts',(0.487286977595107,1.47723287651671,
0.943970416310896));
#285317=CARTESIAN_POINT('Ctrl Pts',(0.478506468261634,1.48010037599804,
0.944631736441497));
#285318=CARTESIAN_POINT('Ctrl Pts',(0.45516699280603,1.4874930900141,0.946391486587428));
#285319=CARTESIAN_POINT('Ctrl Pts',(0.44056647568861,1.49188264751281,0.947494286903442));
#285320=CARTESIAN_POINT('Ctrl Pts',(0.385939202546553,1.50743418912896,
0.951628997277283));
#285321=CARTESIAN_POINT('Ctrl Pts',(0.345538066029537,1.51720458540493,
0.954704682306651));
#285322=CARTESIAN_POINT('Ctrl Pts',(0.200801540429353,1.54612612969485,
0.965791826674418));
#285323=CARTESIAN_POINT('Ctrl Pts',(0.0949630653714379,1.55621462636507,
0.974047963165034));
#285324=CARTESIAN_POINT('Ctrl Pts',(-0.0559913897572137,1.55514116567435,
0.985724820824158));
#285325=CARTESIAN_POINT('Ctrl Pts',(-0.100889800028146,1.55287503087043,
0.989181178242875));
#285326=CARTESIAN_POINT('Ctrl Pts',(-0.163155952180584,1.54701980245475,
0.993905219898409));
#285327=CARTESIAN_POINT('Ctrl Pts',(-0.180653775625082,1.54507423994506,
0.99522499395512));
#285328=CARTESIAN_POINT('Ctrl Pts',(-0.211274280481429,1.54114224977883,
0.99751688192636));
#285329=CARTESIAN_POINT('Ctrl Pts',(-0.224411383193359,1.53928419010894,
0.998494433833281));
#285330=CARTESIAN_POINT('Ctrl Pts',(-0.244164707031287,1.53623207949619,
0.999954095289645));
#285331=CARTESIAN_POINT('Ctrl Pts',(-0.250799188246721,1.53516291575941,
1.00044260375327));
#285332=CARTESIAN_POINT('Ctrl Pts',(-0.262846802068166,1.53314122423497,
1.00132626850513));
#285333=CARTESIAN_POINT('Ctrl Pts',(-0.268261963517385,1.53220298132465,
1.00172217333455));
#285334=CARTESIAN_POINT('Ctrl Pts',(-0.280556865955555,1.53000555746569,
1.00261819566548));
#285335=CARTESIAN_POINT('Ctrl Pts',(-0.287433207140765,1.52872866047809,
1.00311731744504));
#285336=CARTESIAN_POINT('Ctrl Pts',(-0.308720488495415,1.52462702144165,
1.00465689438221));
#285337=CARTESIAN_POINT('Ctrl Pts',(-0.323100720097368,1.52164445920999,
1.00568899843103));
#285338=CARTESIAN_POINT('Ctrl Pts',(-0.429084344549661,1.49809240321099,
1.01325162524607));
#285339=CARTESIAN_POINT('Ctrl Pts',(-0.518713084477981,1.46946792720439,
1.01941027179441));
#285340=CARTESIAN_POINT('Ctrl Pts',(-0.704128088134424,1.39115465056524,
1.0326582204513));
#285341=CARTESIAN_POINT('Ctrl Pts',(-0.798429144647447,1.33925889842552,
1.03973112062725));
#285342=CARTESIAN_POINT('Ctrl Pts',(-0.901952185799104,1.267442408511,1.04846429388587));
#285343=CARTESIAN_POINT('Ctrl Pts',(-0.917081415561585,1.25653874982622,
1.04976642006812));
#285344=CARTESIAN_POINT('Ctrl Pts',(-0.940797808409407,1.23878981262018,
1.05185145801397));
#285345=CARTESIAN_POINT('Ctrl Pts',(-0.949515132629066,1.23212082116985,
1.05262752910011));
#285346=CARTESIAN_POINT('Ctrl Pts',(-0.965877333017481,1.21932652572685,
1.05410312057771));
#285347=CARTESIAN_POINT('Ctrl Pts',(-0.973536378812643,1.21322014071722,
1.05480186695245));
#285348=CARTESIAN_POINT('Ctrl Pts',(-0.990839102785638,1.19915572142229,
1.05639916425593));
#285349=CARTESIAN_POINT('Ctrl Pts',(-1.00044541603695,1.1911530230881,1.05729948977088));
#285350=CARTESIAN_POINT('Ctrl Pts',(-1.02536546171615,1.16987885457939,
1.05967145602723));
#285351=CARTESIAN_POINT('Ctrl Pts',(-1.04051769312572,1.15642281330667,
1.06115058098789));
#285352=CARTESIAN_POINT('Ctrl Pts',(-1.13576896981674,1.068446458573,1.07069279486908));
#285353=CARTESIAN_POINT('Ctrl Pts',(-1.20806624565432,0.985959662678294,
1.07909938235777));
#285354=CARTESIAN_POINT('Ctrl Pts',(-1.30722649945376,0.84537962799422,
1.09243929040788));
#285355=CARTESIAN_POINT('Ctrl Pts',(-1.34022367375399,0.792028501665256,
1.09730380989563));
#285356=CARTESIAN_POINT('Ctrl Pts',(-1.38007405115606,0.71793869536358,
1.10369493054856));
#285357=CARTESIAN_POINT('Ctrl Pts',(-1.38984354128897,0.69883859904247,
1.10531151582231));
#285358=CARTESIAN_POINT('Ctrl Pts',(-1.40594456819935,0.665685653655146,
1.1080577591964));
#285359=CARTESIAN_POINT('Ctrl Pts',(-1.41246796315006,0.651729866562969,
1.10919604179432));
#285360=CARTESIAN_POINT('Ctrl Pts',(-1.42170473411073,0.631178804893287,
1.11084411979572));
#285361=CARTESIAN_POINT('Ctrl Pts',(-1.42458155922438,0.624658643736115,
1.11136290949679));
#285362=CARTESIAN_POINT('Ctrl Pts',(-1.42939106584519,0.613552113380901,
1.11223941913728));
#285363=CARTESIAN_POINT('Ctrl Pts',(-1.43134667873592,0.608975946136397,
1.11259849044811));
#285364=CARTESIAN_POINT('Ctrl Pts',(-1.43575770227557,0.598515430978733,
1.11341451693047));
#285365=CARTESIAN_POINT('Ctrl Pts',(-1.43819893581681,0.592625282665485,
1.11387062074019));
#285366=CARTESIAN_POINT('Ctrl Pts',(-1.44486673250526,0.576253501019198,
1.11512945363952));
#285367=CARTESIAN_POINT('Ctrl Pts',(-1.4490154930026,0.565740305007305,
1.11592773952806));
#285368=CARTESIAN_POINT('Ctrl Pts',(-1.47657752076345,0.493603674622777,
1.12134284332101));
#285369=CARTESIAN_POINT('Ctrl Pts',(-1.49617058988019,0.430582922156333,
1.12576578668999));
#285370=CARTESIAN_POINT('Ctrl Pts',(-1.51533686452467,0.351527832558421,
1.13115628620731));
#285371=CARTESIAN_POINT('Ctrl Pts',(-1.51874441249173,0.336501188304759,
1.1321739530784));
#285372=CARTESIAN_POINT('Ctrl Pts',(-1.53558372126133,0.256768376439463,
1.13754786909517));
#285373=CARTESIAN_POINT('Ctrl Pts',(-1.54510468653155,0.191307616159485,
1.14187314482944));
#285374=CARTESIAN_POINT('Ctrl Pts',(-1.55379146551128,0.0839399700524597,
1.14905062467077));
#285375=CARTESIAN_POINT('Ctrl Pts',(-1.55548131816251,0.0423238287938353,
1.15185205604702));
#285376=CARTESIAN_POINT('Ctrl Pts',(-1.55551296434398,-0.0287841686642868,
1.15671477152007));
#285377=CARTESIAN_POINT('Ctrl Pts',(-1.55468822481587,-0.0582532439779469,
1.15875216244121));
#285378=CARTESIAN_POINT('Ctrl Pts',(-1.55229908074582,-0.100571042043388,
1.16171912500648));
#285379=CARTESIAN_POINT('Ctrl Pts',(-1.55141079476226,-0.113452627472457,
1.16262775926683));
#285380=CARTESIAN_POINT('Ctrl Pts',(-1.54956025863199,-0.136164559849562,
1.16424024185819));
#285381=CARTESIAN_POINT('Ctrl Pts',(-1.54866453946752,-0.145999720843197,
1.16494197334169));
#285382=CARTESIAN_POINT('Ctrl Pts',(-1.54660747269596,-0.166430726568488,
1.16640724792754));
#285383=CARTESIAN_POINT('Ctrl Pts',(-1.54543074575371,-0.177024464298145,
1.16717123888365));
#285384=CARTESIAN_POINT('Ctrl Pts',(-1.54207507834714,-0.204644394702371,
1.16917458920361));
#285385=CARTESIAN_POINT('Ctrl Pts',(-1.53972307445613,-0.221647661151528,
1.17041931347244));
#285386=CARTESIAN_POINT('Ctrl Pts',(-1.52672751156655,-0.305363885208652,
1.17660671100398));
#285387=CARTESIAN_POINT('Ctrl Pts',(-1.51202855627964,-0.371364042153737,
1.18167485282669));
#285388=CARTESIAN_POINT('Ctrl Pts',(-1.46750389802551,-0.523772371611034,
1.19381273799877));
#285389=CARTESIAN_POINT('Ctrl Pts',(-1.43426224024523,-0.608929817575973,
1.20094413117703));
#285390=CARTESIAN_POINT('Ctrl Pts',(-1.3710025359645,-0.736585035208035,
1.21191077349881));
#285391=CARTESIAN_POINT('Ctrl Pts',(-1.34599517033465,-0.781347317049105,
1.21581086931402));
#285392=CARTESIAN_POINT('Ctrl Pts',(-1.31303049034542,-0.834056615237349,
1.220406305716));
#285393=CARTESIAN_POINT('Ctrl Pts',(-1.30714240766572,-0.843254558249755,
1.22120829486619));
#285394=CARTESIAN_POINT('Ctrl Pts',(-1.29771081646496,-0.857651708381463,
1.22246281191104));
#285395=CARTESIAN_POINT('Ctrl Pts',(-1.29423194176983,-0.862892519792311,
1.22291930738669));
#285396=CARTESIAN_POINT('Ctrl Pts',(-1.28762220543469,-0.872719967603617,
1.22377478192885));
#285397=CARTESIAN_POINT('Ctrl Pts',(-1.28449855785755,-0.877310972128718,
1.22417417738702));
#285398=CARTESIAN_POINT('Ctrl Pts',(-1.27702994394212,-0.88816262092167,
1.22511780225973));
#285399=CARTESIAN_POINT('Ctrl Pts',(-1.27266345419126,-0.894408216474298,
1.22566058594377));
#285400=CARTESIAN_POINT('Ctrl Pts',(-1.25768147751872,-0.915505764924107,
1.22749397917557));
#285401=CARTESIAN_POINT('Ctrl Pts',(-1.24685003006503,-0.93020351679451,
1.22877101727788));
#285402=CARTESIAN_POINT('Ctrl Pts',(-1.21935652090631,-0.96616746207214,
1.23190475083995));
#285403=CARTESIAN_POINT('Ctrl Pts',(-1.20239408396714,-0.987197313793401,
1.23374522635645));
#285404=CARTESIAN_POINT('Ctrl Pts',(-1.13586368164649,-1.06542036572257,
1.24066832882985));
#285405=CARTESIAN_POINT('Ctrl Pts',(-1.08269177466586,-1.11941357724221,
1.24561390154537));
#285406=CARTESIAN_POINT('Ctrl Pts',(-0.955255417888559,-1.23120801735341,
1.25678414448857));
#285407=CARTESIAN_POINT('Ctrl Pts',(-0.879267805452882,-1.28657326453854,
1.26301529545086));
#285408=CARTESIAN_POINT('Ctrl Pts',(-0.783005216485522,-1.34418013835143,
1.27079444114156));
#285409=CARTESIAN_POINT('Ctrl Pts',(-0.767083937934294,-1.3533290789868,
1.27207700421522));
#285410=CARTESIAN_POINT('Ctrl Pts',(-0.741446228486962,-1.36746366784155,
1.27413806744307));
#285411=CARTESIAN_POINT('Ctrl Pts',(-0.731832470041748,-1.37263273218507,
1.27491000285651));
#285412=CARTESIAN_POINT('Ctrl Pts',(-0.713478623286334,-1.38225348486681,
1.27638240945695));
#285413=CARTESIAN_POINT('Ctrl Pts',(-0.704749239279571,-1.38672453787717,
1.27708215383941));
#285414=CARTESIAN_POINT('Ctrl Pts',(-0.684699884456577,-1.39675529755161,
1.27868836683183));
#285415=CARTESIAN_POINT('Ctrl Pts',(-0.673353544311358,-1.40226041803387,
1.27959668393535));
#285416=CARTESIAN_POINT('Ctrl Pts',(-0.637572473563439,-1.41908660158885,
1.28245975648336));
#285417=CARTESIAN_POINT('Ctrl Pts',(-0.612911139429624,-1.42991090978217,
1.28443123317565));
#285418=CARTESIAN_POINT('Ctrl Pts',(-0.51846649577302,-1.46847228254375,
1.2919791936791));
#285419=CARTESIAN_POINT('Ctrl Pts',(-0.446996181757044,-1.49178077546112,
1.2976932427901));
#285420=CARTESIAN_POINT('Ctrl Pts',(-0.286929015755493,-1.53144482291081,
1.31041992715441));
#285421=CARTESIAN_POINT('Ctrl Pts',(-0.198017415474529,-1.54545827418027,
1.31744646766776));
#285422=CARTESIAN_POINT('Ctrl Pts',(-0.0771367020315843,-1.55390213161356,
1.32665242690842));
#285423=CARTESIAN_POINT('Ctrl Pts',(-0.0458199122565539,-1.5551407568817,
1.32900501243914));
#285424=CARTESIAN_POINT('Ctrl Pts',(-0.00489881964357937,-1.55552182446076,
1.33201992615547));
#285425=CARTESIAN_POINT('Ctrl Pts',(0.00468788955820674,-1.5555224784307,
1.33272199149779));
#285426=CARTESIAN_POINT('Ctrl Pts',(0.020211613933411,-1.55538001633029,
1.33385132533914));
#285427=CARTESIAN_POINT('Ctrl Pts',(0.0261486915189897,-1.5552915333344,
1.3342814600661));
#285428=CARTESIAN_POINT('Ctrl Pts',(0.0377972704043039,-1.55505120732822,
1.33512170412584));
#285429=CARTESIAN_POINT('Ctrl Pts',(0.0435086664827107,-1.5549018904,1.33553193138178));
#285430=CARTESIAN_POINT('Ctrl Pts',(0.0577510003757015,-1.55445100810447,
1.33655081701692));
#285431=CARTESIAN_POINT('Ctrl Pts',(0.0662806956698605,-1.55411067587106,
1.33715737041014));
#285432=CARTESIAN_POINT('Ctrl Pts',(0.0994073218862273,-1.5525156980521,
1.33950034896991));
#285433=CARTESIAN_POINT('Ctrl Pts',(0.123977409930485,-1.55074710506303,
1.34121097164783));
#285434=CARTESIAN_POINT('Ctrl Pts',(0.189861032241237,-1.54442862306083,
1.34574992320626));
#285435=CARTESIAN_POINT('Ctrl Pts',(0.231052783091895,-1.53880541340218,
1.34853702695684));
#285436=CARTESIAN_POINT('Ctrl Pts',(0.410932677112957,-1.50686210852141,
1.36067295138658));
#285437=CARTESIAN_POINT('Ctrl Pts',(0.545875724765493,-1.46339231768407,
1.36975238936702));
#285438=CARTESIAN_POINT('Ctrl Pts',(0.690512897958219,-1.39396735512701,
1.38082935574176));
#285439=CARTESIAN_POINT('Ctrl Pts',(0.707761793780437,-1.38528922479972,
1.38217244160508));
#285440=CARTESIAN_POINT('Ctrl Pts',(0.735660538247319,-1.37059595447917,
1.38438393971862));
#285441=CARTESIAN_POINT('Ctrl Pts',(0.746409197767083,-1.36477213931963,
1.38524567247444));
#285442=CARTESIAN_POINT('Ctrl Pts',(0.765621502787687,-1.35406772166482,
1.38680413561767));
#285443=CARTESIAN_POINT('Ctrl Pts',(0.774110013920347,-1.34923287788809,
1.38749920420814));
#285444=CARTESIAN_POINT('Ctrl Pts',(0.792189151700143,-1.33870868298107,
1.38899389547905));
#285445=CARTESIAN_POINT('Ctrl Pts',(0.801765215616671,-1.33299554274951,
1.3897943510423));
#285446=CARTESIAN_POINT('Ctrl Pts',(0.827897292041068,-1.31702152383822,
1.39200341003502));
#285447=CARTESIAN_POINT('Ctrl Pts',(0.84432277875606,-1.30655218104267,
1.39341956971928));
#285448=CARTESIAN_POINT('Ctrl Pts',(0.880546408791246,-1.28249548759209,
1.39660654759216));
#285449=CARTESIAN_POINT('Ctrl Pts',(0.90023488562465,-1.26875280870725,
1.39838279544393));
#285450=CARTESIAN_POINT('Ctrl Pts',(0.963043442986792,-1.22271395950808,
1.40419548675255));
#285451=CARTESIAN_POINT('Ctrl Pts',(1.0048024940037,-1.18863493566952,1.40829255975161));
#285452=CARTESIAN_POINT('Ctrl Pts',(1.12018947394772,-1.08403666708012,
1.42027398422075));
#285453=CARTESIAN_POINT('Ctrl Pts',(1.1887665406834,-1.00836219614682,1.42826516503495));
#285454=CARTESIAN_POINT('Ctrl Pts',(1.26681465376374,-0.903111598444006,
1.43819998393924));
#285455=CARTESIAN_POINT('Ctrl Pts',(1.28351709523609,-0.879212185338064,
1.44038488009582));
#285456=CARTESIAN_POINT('Ctrl Pts',(1.30467656212726,-0.847045868174035,
1.44321977400832));
#285457=CARTESIAN_POINT('Ctrl Pts',(1.30974358964377,-0.839189713646754,
1.443904068003));
#285458=CARTESIAN_POINT('Ctrl Pts',(1.31788474974255,-0.82631390564759,
1.44501188820905));
#285459=CARTESIAN_POINT('Ctrl Pts',(1.32100166720112,-0.821321789944566,
1.44543809144491));
#285460=CARTESIAN_POINT('Ctrl Pts',(1.32710885166144,-0.811415695895693,
1.44627711518188));
#285461=CARTESIAN_POINT('Ctrl Pts',(1.33010032338837,-0.806502614758559,
1.44669000237211));
#285462=CARTESIAN_POINT('Ctrl Pts',(1.33756176764775,-0.794093779853041,
1.44772499070053));
#285463=CARTESIAN_POINT('Ctrl Pts',(1.34199612736557,-0.786576644082907,
1.44834484051555));
#285464=CARTESIAN_POINT('Ctrl Pts',(1.35948221668216,-0.756355822300801,
1.45081006741578));
#285465=CARTESIAN_POINT('Ctrl Pts',(1.3720238183528,-0.73335998998503,1.45262608250589));
#285466=CARTESIAN_POINT('Ctrl Pts',(1.40481737908016,-0.669441689255441,
1.45754273695903));
#285467=CARTESIAN_POINT('Ctrl Pts',(1.42385875274836,-0.627925887114373,
1.46059326815475));
#285468=CARTESIAN_POINT('Ctrl Pts',(1.48191550369624,-0.48506678902023,
1.47080897015905));
#285469=CARTESIAN_POINT('Ctrl Pts',(1.51214302299441,-0.380507574229137,
1.47784531193719));
#285470=CARTESIAN_POINT('Ctrl Pts',(1.5380915965182,-0.235311709009577,
1.4878331823631));
#285471=CARTESIAN_POINT('Ctrl Pts',(1.54350087863081,-0.196728193498538,
1.49050458654459));
#285472=CARTESIAN_POINT('Ctrl Pts',(1.54896732048858,-0.143184568467055,
1.4942583592442));
#285473=CARTESIAN_POINT('Ctrl Pts',(1.55026587102076,-0.128363868896053,
1.49530222521613));
#285474=CARTESIAN_POINT('Ctrl Pts',(1.55202069131992,-0.104384225476753,
1.49700008483808));
#285475=CARTESIAN_POINT('Ctrl Pts',(1.55260892065239,-0.0952356330571008,
1.49764993042762));
#285476=CARTESIAN_POINT('Ctrl Pts',(1.55366955793473,-0.0760994320696083,
1.49901385790617));
#285477=CARTESIAN_POINT('Ctrl Pts',(1.55412660000661,-0.0661114314141855,
1.4997283886078));
#285478=CARTESIAN_POINT('Ctrl Pts',(1.55498820463812,-0.0422455166606131,
1.50144237900248));
#285479=CARTESIAN_POINT('Ctrl Pts',(1.5553033074422,-0.0283654522450213,
1.50244458035445));
#285480=CARTESIAN_POINT('Ctrl Pts',(1.55575604579002,0.020255873733048,
1.50597510563191));
#285481=CARTESIAN_POINT('Ctrl Pts',(1.55491560377014,0.0549935096948878,
1.50853328257311));
#285482=CARTESIAN_POINT('Ctrl Pts',(1.54987777706318,0.142237614018786,
1.51505273970803));
#285483=CARTESIAN_POINT('Ctrl Pts',(1.54417562876676,0.194610662774658,
1.5190539239068));
#285484=CARTESIAN_POINT('Ctrl Pts',(1.51995382481115,0.34547108914028,1.53079979181471));
#285485=CARTESIAN_POINT('Ctrl Pts',(1.49456589202119,0.442586280914189,
1.53865232079548));
#285486=CARTESIAN_POINT('Ctrl Pts',(1.44892060415021,0.566784260805124,
1.54871249385081));
#285487=CARTESIAN_POINT('Ctrl Pts',(1.43688718364285,0.596632964086019,
1.55112983874934));
#285488=CARTESIAN_POINT('Ctrl Pts',(1.4200424895114,0.634943405783003,1.55421372410286));
#285489=CARTESIAN_POINT('Ctrl Pts',(1.4160668124303,0.643761288074544,1.55492220859574));
#285490=CARTESIAN_POINT('Ctrl Pts',(1.40951048026205,0.657948271929512,
1.5560592665619));
#285491=CARTESIAN_POINT('Ctrl Pts',(1.40698086437202,0.663340465383115,
1.55649077658034));
#285492=CARTESIAN_POINT('Ctrl Pts',(1.40196982481974,0.673864489478773,
1.55733147094709));
#285493=CARTESIAN_POINT('Ctrl Pts',(1.39949107190796,0.678997408824249,
1.55774079136288));
#285494=CARTESIAN_POINT('Ctrl Pts',(1.39325890216053,0.691723662517195,
1.55875413331943));
#285495=CARTESIAN_POINT('Ctrl Pts',(1.38947149657993,0.699300337887208,
1.55935609952396));
#285496=CARTESIAN_POINT('Ctrl Pts',(1.3746650186864,0.728325313324788,1.56165844701148));
#285497=CARTESIAN_POINT('Ctrl Pts',(1.36320901522437,0.749548544321978,
1.56333415315856));
#285498=CARTESIAN_POINT('Ctrl Pts',(1.33132508145061,0.805465077072625,
1.56775149698088));
#285499=CARTESIAN_POINT('Ctrl Pts',(1.3100355540923,0.839647414166252,1.57045457043898));
#285500=CARTESIAN_POINT('Ctrl Pts',(1.21323744756987,0.982404134451389,
1.58192323263047));
#285501=CARTESIAN_POINT('Ctrl Pts',(1.12538782026016,1.0819262973633,1.59043357673954));
#285502=CARTESIAN_POINT('Ctrl Pts',(1.00470901529274,1.18783129182071,1.60142706512667));
#285503=CARTESIAN_POINT('Ctrl Pts',(0.98290288403607,1.20593744946568,1.60338770829089));
#285504=CARTESIAN_POINT('Ctrl Pts',(0.950609760612354,1.23129329133685,
1.60626303635411));
#285505=CARTESIAN_POINT('Ctrl Pts',(0.94050828501287,1.23902632540372,1.60715859058409));
#285506=CARTESIAN_POINT('Ctrl Pts',(0.922420091037247,1.25252482069572,
1.60875613879582));
#285507=CARTESIAN_POINT('Ctrl Pts',(0.914471228237063,1.25834002376041,
1.60945614683852));
#285508=CARTESIAN_POINT('Ctrl Pts',(0.89773323729511,1.27034279239836,1.61092626326136));
#285509=CARTESIAN_POINT('Ctrl Pts',(0.888934154772039,1.27651550452427,
1.61169689287338));
#285510=CARTESIAN_POINT('Ctrl Pts',(0.865576464393049,1.29254272059753,
1.61373725446418));
#285511=CARTESIAN_POINT('Ctrl Pts',(0.850913922238565,1.30224220103209,
1.61501272148755));
#285512=CARTESIAN_POINT('Ctrl Pts',(0.773023566605363,1.35189064248421,
1.62176320386917));
#285513=CARTESIAN_POINT('Ctrl Pts',(0.707149446321878,1.3874834157055,1.6273939314499));
#285514=CARTESIAN_POINT('Ctrl Pts',(0.594068773299685,1.43843286369268,
1.6369102049889));
#285515=CARTESIAN_POINT('Ctrl Pts',(0.54822245540609,1.45652278051361,1.64072867946952));
#285516=CARTESIAN_POINT('Ctrl Pts',(0.42737081080698,1.49769268073475,1.65062893832811));
#285517=CARTESIAN_POINT('Ctrl Pts',(0.351331225187655,1.51733252410523,
1.65670267151562));
#285518=CARTESIAN_POINT('Ctrl Pts',(0.259188183155168,1.53382922490932,
1.66367506506825));
#285519=CARTESIAN_POINT('Ctrl Pts',(0.244209164679686,1.53628530389922,
1.66479631358244));
#285520=CARTESIAN_POINT('Ctrl Pts',(0.22218809743989,1.53956581480797,1.66642457852482));
#285521=CARTESIAN_POINT('Ctrl Pts',(0.215173086553863,1.54056190944774,
1.66694029530586));
#285522=CARTESIAN_POINT('Ctrl Pts',(0.202702832726107,1.54224577776568,
1.66785148397202));
#285523=CARTESIAN_POINT('Ctrl Pts',(0.197250467302218,1.54295260257322,
1.66824797533813));
#285524=CARTESIAN_POINT('Ctrl Pts',(0.185207857687381,1.54444888190396,
1.66911948068802));
#285525=CARTESIAN_POINT('Ctrl Pts',(0.178616200459464,1.54522508283851,
1.66959375997708));
#285526=CARTESIAN_POINT('Ctrl Pts',(0.159229282447211,1.54738227458015,
1.67098114426803));
#285527=CARTESIAN_POINT('Ctrl Pts',(0.146421232818584,1.54864673794288,
1.67188809751811));
#285528=CARTESIAN_POINT('Ctrl Pts',(0.116741337360638,1.55120533239833,
1.67397060996629));
#285529=CARTESIAN_POINT('Ctrl Pts',(0.0998608721853694,1.55238345217501,
1.6751407564622));
#285530=CARTESIAN_POINT('Ctrl Pts',(0.0408382982810627,1.55553595321183,
1.67919289210649));
#285531=CARTESIAN_POINT('Ctrl Pts',(-0.00136447965634196,1.55607150533019,
1.68202070158236));
#285532=CARTESIAN_POINT('Ctrl Pts',(-0.183054574874739,1.55098386289037,
1.69408914816562));
#285533=CARTESIAN_POINT('Ctrl Pts',(-0.32139648054752,1.52832012647518,
1.70307427924817));
#285534=CARTESIAN_POINT('Ctrl Pts',(-0.473638613469977,1.48176663257494,
1.71406063104891));
#285535=CARTESIAN_POINT('Ctrl Pts',(-0.492306769605151,1.47566929732042,
1.71542613496786));
#285536=CARTESIAN_POINT('Ctrl Pts',(-0.522491641841563,1.46517389679756,
1.71766697821376));
#285537=CARTESIAN_POINT('Ctrl Pts',(-0.534080683110418,1.4609893469953,
1.71853532928839));
#285538=CARTESIAN_POINT('Ctrl Pts',(-0.554774433803354,1.4532381670657,
1.72010095796282));
#285539=CARTESIAN_POINT('Ctrl Pts',(-0.563897633739579,1.44972248837634,
1.72079650753148));
#285540=CARTESIAN_POINT('Ctrl Pts',(-0.583294025785787,1.44203718565611,
1.72228698529944));
#285541=CARTESIAN_POINT('Ctrl Pts',(-0.593556943234001,1.43784328376957,
1.72308269878754));
#285542=CARTESIAN_POINT('Ctrl Pts',(-0.621444048696768,1.42609788065748,
1.72526476231324));
#285543=CARTESIAN_POINT('Ctrl Pts',(-0.638974304079398,1.41832988004247,
1.72665836313679));
#285544=CARTESIAN_POINT('Ctrl Pts',(-0.751669339079574,1.3658792112092,
1.7357645804769));
#285545=CARTESIAN_POINT('Ctrl Pts',(-0.842221872722308,1.31197832860232,
1.74379837533384));
#285546=CARTESIAN_POINT('Ctrl Pts',(-1.00332520279295,1.19249153917397,
1.75933724312972));
#285547=CARTESIAN_POINT('Ctrl Pts',(-1.07462400233896,1.12866466672871,
1.76678432371324));
#285548=CARTESIAN_POINT('Ctrl Pts',(-1.14948835431144,1.04807769543371,
1.77496802123196));
#285549=CARTESIAN_POINT('Ctrl Pts',(-1.15920491005059,1.03732075509186,
1.77603784584846));
#285550=CARTESIAN_POINT('Ctrl Pts',(-1.17336065019996,1.02120195362672,
1.77760598315025));
#285551=CARTESIAN_POINT('Ctrl Pts',(-1.17791616794025,1.01594397080627,
1.77811213995246));
#285552=CARTESIAN_POINT('Ctrl Pts',(-1.18600484813376,1.00648045928285,
1.77901330801262));
#285553=CARTESIAN_POINT('Ctrl Pts',(-1.18955116860387,1.00228660315738,
1.77940924517836));
#285554=CARTESIAN_POINT('Ctrl Pts',(-1.19740383972254,0.992899693714939,
1.78028786328329));
#285555=CARTESIAN_POINT('Ctrl Pts',(-1.20169869421266,0.9876973271344,1.78076972789808));
#285556=CARTESIAN_POINT('Ctrl Pts',(-1.21443044850802,0.972069340231864,
1.78220273877384));
#285557=CARTESIAN_POINT('Ctrl Pts',(-1.22276677085871,0.961562048103047,
1.78314710764514));
#285558=CARTESIAN_POINT('Ctrl Pts',(-1.2834213639873,0.8830469352148,1.79007523044091));
#285559=CARTESIAN_POINT('Ctrl Pts',(-1.33017595046773,0.810912105934072,
1.79574073476288));
#285560=CARTESIAN_POINT('Ctrl Pts',(-1.41010766359066,0.661899236267086,
1.80687727471846));
#285561=CARTESIAN_POINT('Ctrl Pts',(-1.44351100257382,0.585481861399606,
1.81233333670593));
#285562=CARTESIAN_POINT('Ctrl Pts',(-1.48402225490741,0.467916910113274,
1.82073812119626));
#285563=CARTESIAN_POINT('Ctrl Pts',(-1.49586213260795,0.428560716483626,
1.82355180738951));
#285564=CARTESIAN_POINT('Ctrl Pts',(-1.50992349584839,0.374087793830485,
1.82747336029534));
#285565=CARTESIAN_POINT('Ctrl Pts',(-1.51350182778367,0.35933665216795,
1.82853790909864));
#285566=CARTESIAN_POINT('Ctrl Pts',(-1.51890618730803,0.335543267928228,
1.83026034838203));
#285567=CARTESIAN_POINT('Ctrl Pts',(-1.5208687090463,0.326532775853882,
1.83091385024171));
#285568=CARTESIAN_POINT('Ctrl Pts',(-1.52478328782911,0.307758525152647,
1.83227829957696));
#285569=CARTESIAN_POINT('Ctrl Pts',(-1.5267219405675,0.297992436725351,
1.83298964064143));
#285570=CARTESIAN_POINT('Ctrl Pts',(-1.53038802978201,0.278548667689275,
1.83440929547135));
#285571=CARTESIAN_POINT('Ctrl Pts',(-1.53211774498378,0.268871882569186,
1.83511750068595));
#285572=CARTESIAN_POINT('Ctrl Pts',(-1.53595638774626,0.246155816974868,
1.83678417298149));
#285573=CARTESIAN_POINT('Ctrl Pts',(-1.53799114730412,0.233104959547902,
1.83774492517261));
#285574=CARTESIAN_POINT('Ctrl Pts',(-1.55034034614246,0.146680298957285,
1.84412968162698));
#285575=CARTESIAN_POINT('Ctrl Pts',(-1.55556516654839,0.072688768575606,
1.84970986030065));
#285576=CARTESIAN_POINT('Ctrl Pts',(-1.55549938660524,-0.00138140172760619,
1.85539343273712));
#285577=CARTESIAN_POINT('',(-1.5554992988366,0.00127668674633576,3.25533865702281));
#285578=CARTESIAN_POINT('Ctrl Pts',(-1.55549938782948,-0.00138002250719613,
1.85539332690641));
#285579=CARTESIAN_POINT('Ctrl Pts',(-1.55539766380321,-0.116038776085956,
1.86419135181066));
#285580=CARTESIAN_POINT('Ctrl Pts',(-1.54261929930628,-0.230336009965302,
1.87321326259203));
#285581=CARTESIAN_POINT('Ctrl Pts',(-1.51371361985,-0.358512387846686,1.88312415629134));
#285582=CARTESIAN_POINT('Ctrl Pts',(-1.50977061259033,-0.374770335955011,
1.88437665157453));
#285583=CARTESIAN_POINT('Ctrl Pts',(-1.502359557691,-0.403309745667421,
1.88656365234119));
#285584=CARTESIAN_POINT('Ctrl Pts',(-1.49900126965122,-0.415617869024133,
1.88750297429455));
#285585=CARTESIAN_POINT('Ctrl Pts',(-1.49367239580812,-0.434242755299764,
1.88891709446616));
#285586=CARTESIAN_POINT('Ctrl Pts',(-1.49181241324735,-0.440590200221338,
1.88939773949122));
#285587=CARTESIAN_POINT('Ctrl Pts',(-1.48833177301127,-0.452193576340129,
1.89027376325001));
#285588=CARTESIAN_POINT('Ctrl Pts',(-1.48672369933094,-0.457452883697398,
1.89066981244072));
#285589=CARTESIAN_POINT('Ctrl Pts',(-1.48297157566527,-0.469495646941254,
1.89157444234581));
#285590=CARTESIAN_POINT('Ctrl Pts',(-1.48080884848271,-0.476273048004625,
1.89208193889876));
#285591=CARTESIAN_POINT('Ctrl Pts',(-1.47400589228505,-0.497097288868325,
1.89363700425126));
#285592=CARTESIAN_POINT('Ctrl Pts',(-1.46921155942735,-0.511093455747034,
1.89467617237059));
#285593=CARTESIAN_POINT('Ctrl Pts',(-1.43496540015201,-0.606601947318413,
1.90173991902198));
#285594=CARTESIAN_POINT('Ctrl Pts',(-1.398941372988,-0.685608333104245,
1.90745038881136));
#285595=CARTESIAN_POINT('Ctrl Pts',(-1.3188162463593,-0.828395524329324,
1.91822998347317));
#285596=CARTESIAN_POINT('Ctrl Pts',(-1.27617860128657,-0.892682812343315,
1.92328542963743));
#285597=CARTESIAN_POINT('Ctrl Pts',(-1.2019558003225,-0.988343279150782,
1.93145374223992));
#285598=CARTESIAN_POINT('Ctrl Pts',(-1.17349225906434,-1.02197628038131,
1.93446608983305));
#285599=CARTESIAN_POINT('Ctrl Pts',(-1.13361391707814,-1.0652317240849,
1.9385672398285));
#285600=CARTESIAN_POINT('Ctrl Pts',(-1.12343122537579,-1.0759653314339,
1.93960475333125));
#285601=CARTESIAN_POINT('Ctrl Pts',(-1.1127785721042,-1.0868782395644,1.94068101230253));
#285602=CARTESIAN_POINT('Ctrl Pts',(-1.11245972113799,-1.0872045929896,
1.94071321813696));
#285603=CARTESIAN_POINT('Ctrl Pts',(-1.11182075533274,-1.08785801806167,
1.94077774084313));
#285604=CARTESIAN_POINT('Ctrl Pts',(-1.11150063964671,-1.08818508881249,
1.9408100577495));
#285605=CARTESIAN_POINT('Ctrl Pts',(-1.11085785637062,-1.08884125810893,
1.94087493248099));
#285606=CARTESIAN_POINT('Ctrl Pts',(-1.11053518677012,-1.0891703546118,
1.94090749039098));
#285607=CARTESIAN_POINT('Ctrl Pts',(-1.10988593429973,-1.08983195037405,
1.94097298414055));
#285608=CARTESIAN_POINT('Ctrl Pts',(-1.10955934817187,-1.09016444635479,
1.94100592011898));
#285609=CARTESIAN_POINT('Ctrl Pts',(-1.10913530607355,-1.09059577391743,
1.94104867332845));
#285610=CARTESIAN_POINT('Ctrl Pts',(-1.10903798594903,-1.09069473959835,
1.94105848467777));
#285611=CARTESIAN_POINT('Ctrl Pts',(-1.10883031820993,-1.09090586219629,
1.94107941912415));
#285612=CARTESIAN_POINT('Ctrl Pts',(-1.10871996682877,-1.09101801539249,
1.94109054238435));
#285613=CARTESIAN_POINT('Ctrl Pts',(-1.10848378181274,-1.09125798399325,
1.94111434740593));
#285614=CARTESIAN_POINT('Ctrl Pts',(-1.10835794309461,-1.09138579436876,
1.94112702938747));
#285615=CARTESIAN_POINT('Ctrl Pts',(-1.1080876687569,-1.09166020844547,
1.94115426482042));
#285616=CARTESIAN_POINT('Ctrl Pts',(-1.10794322615939,-1.09180680523697,
1.94116881857421));
#285617=CARTESIAN_POINT('Ctrl Pts',(-1.10763172607929,-1.09212282550781,
1.94120020112357));
#285618=CARTESIAN_POINT('Ctrl Pts',(-1.10746465882821,-1.09229223931097,
1.9412170303429));
#285619=CARTESIAN_POINT('Ctrl Pts',(-1.10710262592472,-1.09265918872381,
1.94125349426287));
#285620=CARTESIAN_POINT('Ctrl Pts',(-1.10690764629187,-1.09285671046684,
1.94127312957035));
#285621=CARTESIAN_POINT('Ctrl Pts',(-1.10648268386012,-1.09328698308489,
1.94131591858198));
#285622=CARTESIAN_POINT('Ctrl Pts',(-1.10625268050981,-1.09351971355331,
1.94133907317904));
#285623=CARTESIAN_POINT('Ctrl Pts',(-1.10574786039744,-1.09403019697703,
1.94138988458568));
#285624=CARTESIAN_POINT('Ctrl Pts',(-1.10547301244669,-1.09430791892531,
1.94141754275191));
#285625=CARTESIAN_POINT('Ctrl Pts',(-1.10486451802979,-1.09492231298259,
1.94147876284793));
#285626=CARTESIAN_POINT('Ctrl Pts',(-1.10453082236997,-1.09525893609783,
1.94151232692011));
#285627=CARTESIAN_POINT('Ctrl Pts',(-1.10378389823267,-1.09601172436885,
1.94158743515946));
#285628=CARTESIAN_POINT('Ctrl Pts',(-1.10337058832985,-1.09642780827496,
1.94162898287835));
#285629=CARTESIAN_POINT('Ctrl Pts',(-1.10084977933089,-1.09896266729653,
1.94188230439833));
#285630=CARTESIAN_POINT('Ctrl Pts',(-1.09873642619557,-1.10107558609246,
1.94209433402723));
#285631=CARTESIAN_POINT('Ctrl Pts',(-1.08967135732866,-1.11008670594664,
1.94300236399372));
#285632=CARTESIAN_POINT('Ctrl Pts',(-1.08266080413106,-1.11692512588829,
1.9437009558404));
#285633=CARTESIAN_POINT('Ctrl Pts',(-1.06656567676514,-1.1323311492053,
1.94529693241653));
#285634=CARTESIAN_POINT('Ctrl Pts',(-1.05744167308058,-1.14085637372283,
1.94619608098515));
#285635=CARTESIAN_POINT('Ctrl Pts',(-1.03328489056309,-1.16288907189579,
1.94856285216569));
#285636=CARTESIAN_POINT('Ctrl Pts',(-1.01809022296345,-1.17621464259349,
1.95003790586758));
#285637=CARTESIAN_POINT('Ctrl Pts',(-0.918484476451701,-1.26019164313763,
1.95962484838615));
#285638=CARTESIAN_POINT('Ctrl Pts',(-0.827049608415514,-1.32199736519118,
1.96808505058503));
#285639=CARTESIAN_POINT('Ctrl Pts',(-0.674941817056807,-1.40282004166848,
1.98144150415998));
#285640=CARTESIAN_POINT('Ctrl Pts',(-0.618299532874221,-1.42869066529152,
1.98626941227193));
#285641=CARTESIAN_POINT('Ctrl Pts',(-0.540329777371615,-1.45879412091462,
1.99261808916061));
#285642=CARTESIAN_POINT('Ctrl Pts',(-0.520244685389792,-1.466077119928,
1.99422778722588));
#285643=CARTESIAN_POINT('Ctrl Pts',(-0.485474015382528,-1.47788058831197,
1.99696362938833));
#285644=CARTESIAN_POINT('Ctrl Pts',(-0.47086009117039,-1.48260138763152,
1.99809831525367));
#285645=CARTESIAN_POINT('Ctrl Pts',(-0.449372939634831,-1.48919269293787,
1.99974223400038));
#285646=CARTESIAN_POINT('Ctrl Pts',(-0.44255351093921,-1.49123348636273,
2.00026039763147));
#285647=CARTESIAN_POINT('Ctrl Pts',(-0.430943404808324,-1.49462128708306,
2.00113624115592));
#285648=CARTESIAN_POINT('Ctrl Pts',(-0.426159967493677,-1.49599221080461,
2.00149526616931));
#285649=CARTESIAN_POINT('Ctrl Pts',(-0.415225589968901,-1.49906927811483,
2.00231174440553));
#285650=CARTESIAN_POINT('Ctrl Pts',(-0.409070633807719,-1.50076054438941,
2.00276834132166));
#285651=CARTESIAN_POINT('Ctrl Pts',(-0.391961307568011,-1.50534878606043,
2.0040297201373));
#285652=CARTESIAN_POINT('Ctrl Pts',(-0.380985159378353,-1.50816410324995,
2.00483003137214));
#285653=CARTESIAN_POINT('Ctrl Pts',(-0.30115048221717,-1.52771399659727,
2.0105933208075));
#285654=CARTESIAN_POINT('Ctrl Pts',(-0.231240828331398,-1.53984808799809,
2.01533146352502));
#285655=CARTESIAN_POINT('Ctrl Pts',(-0.0684365885804611,-1.55676212503987,
2.02615742909475));
#285656=CARTESIAN_POINT('Ctrl Pts',(0.0245348630282996,-1.55807232634197,
2.03219540300838));
#285657=CARTESIAN_POINT('Ctrl Pts',(0.16571045946522,-1.54741717025975,
2.0417127036691));
#285658=CARTESIAN_POINT('Ctrl Pts',(0.214149168785505,-1.54146009386573,
2.04503912423425));
#285659=CARTESIAN_POINT('Ctrl Pts',(0.277625416038463,-1.53060396759468,
2.04952448294937));
#285660=CARTESIAN_POINT('Ctrl Pts',(0.292985301201792,-1.52773818421614,
2.05061961676102));
#285661=CARTESIAN_POINT('Ctrl Pts',(0.318430182148028,-1.52259295551962,
2.05245140719212));
#285662=CARTESIAN_POINT('Ctrl Pts',(0.328540529136187,-1.52044342232063,
2.05318390680175));
#285663=CARTESIAN_POINT('Ctrl Pts',(0.348315016184895,-1.51603278208599,
2.05462608885738));
#285664=CARTESIAN_POINT('Ctrl Pts',(0.357980435145784,-1.51377962283028,
2.05533548510163));
#285665=CARTESIAN_POINT('Ctrl Pts',(0.381252728963373,-1.50811914447127,
2.05705474797271));
#285666=CARTESIAN_POINT('Ctrl Pts',(0.394836136360542,-1.50462001805791,
2.05806752047571));
#285667=CARTESIAN_POINT('Ctrl Pts',(0.440521215259556,-1.49219017973418,
2.06150626528908));
#285668=CARTESIAN_POINT('Ctrl Pts',(0.472380651540062,-1.48241245322546,
2.06395909942711));
#285669=CARTESIAN_POINT('Ctrl Pts',(0.622569341500666,-1.43098613555469,
2.07579301286842));
#285670=CARTESIAN_POINT('Ctrl Pts',(0.735874886143945,-1.37615129242733,
2.0855876369283));
#285671=CARTESIAN_POINT('Ctrl Pts',(0.88774336493013,-1.27848938378069,
2.09952265803288));
#285672=CARTESIAN_POINT('Ctrl Pts',(0.932527325422741,-1.24620122134243,
2.1037394158671));
#285673=CARTESIAN_POINT('Ctrl Pts',(0.985459974905064,-1.20358308071593,
2.10878008222338));
#285674=CARTESIAN_POINT('Ctrl Pts',(0.995316232333132,-1.19544519743005,
2.10972117495512));
#285675=CARTESIAN_POINT('Ctrl Pts',(1.01012316929054,-1.18290965128527,
2.11113739920062));
#285676=CARTESIAN_POINT('Ctrl Pts',(1.01514763618166,-1.17860058600255,
2.11161840291368));
#285677=CARTESIAN_POINT('Ctrl Pts',(1.02429606178485,-1.17065283945922,
2.11249475999196));
#285678=CARTESIAN_POINT('Ctrl Pts',(1.02842831697937,-1.1670242891593,2.11289078748289));
#285679=CARTESIAN_POINT('Ctrl Pts',(1.03785736953752,-1.15865562173357,
2.11379496283577));
#285680=CARTESIAN_POINT('Ctrl Pts',(1.04314101940135,-1.15390103049611,
2.11430203094919));
#285681=CARTESIAN_POINT('Ctrl Pts',(1.05929735111034,-1.13916078328038,
2.11585449457541));
#285682=CARTESIAN_POINT('Ctrl Pts',(1.07006100707179,-1.12905608846639,
2.11689152946694));
#285683=CARTESIAN_POINT('Ctrl Pts',(1.14361667709788,-1.05800659433596,
2.12401166516163));
#285684=CARTESIAN_POINT('Ctrl Pts',(1.20132075686359,-0.992002885792999,
2.12977420013549));
#285685=CARTESIAN_POINT('Ctrl Pts',(1.29848195831708,-0.859868962894762,
2.14057151719666));
#285686=CARTESIAN_POINT('Ctrl Pts',(1.33918239325432,-0.794996562404126,
2.14559206674625));
#285687=CARTESIAN_POINT('Ctrl Pts',(1.39550125711051,-0.688541049955402,
2.15371817552177));
#285688=CARTESIAN_POINT('Ctrl Pts',(1.41439915191265,-0.648835105475695,
2.15672503191962));
#285689=CARTESIAN_POINT('Ctrl Pts',(1.43749296474405,-0.59449311724066,
2.16084148555709));
#285690=CARTESIAN_POINT('Ctrl Pts',(1.44319394585411,-0.580516405219747,
2.1619002543274));
#285691=CARTESIAN_POINT('Ctrl Pts',(1.452415349523,-0.556933143339107,2.16368797581798));
#285692=CARTESIAN_POINT('Ctrl Pts',(1.45604610560108,-0.547370626708334,
2.16441319219326));
#285693=CARTESIAN_POINT('Ctrl Pts',(1.46304097097454,-0.528385706957744,
2.16585402044033));
#285694=CARTESIAN_POINT('Ctrl Pts',(1.46640900760776,-0.518965270367493,
2.16656946070947));
#285695=CARTESIAN_POINT('Ctrl Pts',(1.4744235644756,-0.49584735907924,2.16832671618908));
#285696=CARTESIAN_POINT('Ctrl Pts',(1.47897026979995,-0.482116547920775,
2.16937176081428));
#285697=CARTESIAN_POINT('Ctrl Pts',(1.49417213802951,-0.433967679865874,
2.17304211728533));
#285698=CARTESIAN_POINT('Ctrl Pts',(1.50382173816676,-0.39924693208229,
2.17569940947452));
#285699=CARTESIAN_POINT('Ctrl Pts',(1.54088387259139,-0.24536551774025,
2.18753002070522));
#285700=CARTESIAN_POINT('Ctrl Pts',(1.55539458831865,-0.123557648279827,
2.1970798225649));
#285701=CARTESIAN_POINT('Ctrl Pts',(1.55553296007454,0.0377582192192761,
2.20952720089324));
#285702=CARTESIAN_POINT('Ctrl Pts',(1.55409278180253,0.0768407869833449,
2.21252285128286));
#285703=CARTESIAN_POINT('Ctrl Pts',(1.54942064576688,0.139409496562854,
2.217250422461));
#285704=CARTESIAN_POINT('Ctrl Pts',(1.54712236280516,0.162947526642347,
2.21901321562704));
#285705=CARTESIAN_POINT('Ctrl Pts',(1.54328025722834,0.194774264110559,
2.22136773155015));
#285706=CARTESIAN_POINT('Ctrl Pts',(1.54220469289375,0.203114893769966,
2.22198204573692));
#285707=CARTESIAN_POINT('Ctrl Pts',(1.54028832278048,0.217081747189404,
2.22300573810681));
#285708=CARTESIAN_POINT('Ctrl Pts',(1.53948421314118,0.22271273844153,2.22341708741911));
#285709=CARTESIAN_POINT('Ctrl Pts',(1.53777220045454,0.234249017978596,
2.22425684989843));
#285710=CARTESIAN_POINT('Ctrl Pts',(1.53686113685671,0.24015368447963,2.2246850861318));
#285711=CARTESIAN_POINT('Ctrl Pts',(1.53437277576003,0.255686567157601,
2.22580778999951));
#285712=CARTESIAN_POINT('Ctrl Pts',(1.53273884468729,0.265305639805893,
2.22649917723953));
#285713=CARTESIAN_POINT('Ctrl Pts',(1.52517979735085,0.307403241879653,
2.22951057803652));
#285714=CARTESIAN_POINT('Ctrl Pts',(1.51831160417563,0.339706377809358,
2.23178362614877));
#285715=CARTESIAN_POINT('Ctrl Pts',(1.48924287049191,0.457806530981507,
2.24003649951594));
#285716=CARTESIAN_POINT('Ctrl Pts',(1.46075174486595,0.54188369691448,2.24580624208016));
#285717=CARTESIAN_POINT('Ctrl Pts',(1.39547094697615,0.691208551927479,
2.25655529653191));
#285718=CARTESIAN_POINT('Ctrl Pts',(1.36084505007439,0.757104642076446,
2.26149757570754));
#285719=CARTESIAN_POINT('Ctrl Pts',(1.30745616033011,0.843126567547134,
2.26844084409891));
#285720=CARTESIAN_POINT('Ctrl Pts',(1.29267945993515,0.865611740769411,
2.27030433832295));
#285721=CARTESIAN_POINT('Ctrl Pts',(1.27013384601024,0.898052990519306,
2.2730726045484));
#285722=CARTESIAN_POINT('Ctrl Pts',(1.26281442332016,0.908316506621834,
2.27396051022109));
#285723=CARTESIAN_POINT('Ctrl Pts',(1.24958069110846,0.926404077567346,
2.27554767344445));
#285724=CARTESIAN_POINT('Ctrl Pts',(1.24371553872132,0.934263383220231,
2.27624500702461));
#285725=CARTESIAN_POINT('Ctrl Pts',(1.23116497526757,0.950753506638161,
2.27772481333258));
#285726=CARTESIAN_POINT('Ctrl Pts',(1.22446225836271,0.959370415066531,
2.27850794189771));
#285727=CARTESIAN_POINT('Ctrl Pts',(1.20623766986802,0.982297538656482,
2.2806187450607));
#285728=CARTESIAN_POINT('Ctrl Pts',(1.19455237199734,0.99647496081217,2.28195289011951));
#285729=CARTESIAN_POINT('Ctrl Pts',(1.12378142793482,1.07930516013351,2.28992465464507));
#285730=CARTESIAN_POINT('Ctrl Pts',(1.05905206007119,1.14288568392219,2.29679616853486));
#285731=CARTESIAN_POINT('Ctrl Pts',(0.938808884967153,1.24196486926266,
2.30882495251858));
#285732=CARTESIAN_POINT('Ctrl Pts',(0.885884504091287,1.28025289650019,
2.31390917683055));
#285733=CARTESIAN_POINT('Ctrl Pts',(0.800764486532074,1.33402068692155,
2.32166102547224));
#285734=CARTESIAN_POINT('Ctrl Pts',(0.770177471462459,1.35191048144166,
2.32436784422616));
#285735=CARTESIAN_POINT('Ctrl Pts',(0.719547973294031,1.37924612293637,
2.32869535335961));
#285736=CARTESIAN_POINT('Ctrl Pts',(0.699868450528997,1.38933560946832,
2.33034137323948));
#285737=CARTESIAN_POINT('Ctrl Pts',(0.672602661587294,1.40258802859208,
2.3325666139198));
#285738=CARTESIAN_POINT('Ctrl Pts',(0.66519764102275,1.40611508229561,2.33316546535463));
#285739=CARTESIAN_POINT('Ctrl Pts',(0.652646288225694,1.41197201713396,
2.33417084305072));
#285740=CARTESIAN_POINT('Ctrl Pts',(0.64751460216541,1.41433270448369,2.33457918998582));
#285741=CARTESIAN_POINT('Ctrl Pts',(0.637552528365851,1.41884988742301,
2.33536654013391));
#285742=CARTESIAN_POINT('Ctrl Pts',(0.632723873011264,1.42100975796641,
2.33574576479558));
#285743=CARTESIAN_POINT('Ctrl Pts',(0.619389434832095,1.42689284297884,
2.33678664153988));
#285744=CARTESIAN_POINT('Ctrl Pts',(0.610861010176141,1.43056467689743,
2.33744526832366));
#285745=CARTESIAN_POINT('Ctrl Pts',(0.575934502633639,1.44523265874609,
2.34011576202334));
#285746=CARTESIAN_POINT('Ctrl Pts',(0.549266616642322,1.45557701021844,
2.34209279048607));
#285747=CARTESIAN_POINT('Ctrl Pts',(0.426108367136655,1.49948205331072,
2.35100945428563));
#285748=CARTESIAN_POINT('Ctrl Pts',(0.326736865578115,1.52422494240192,
2.35762719296997));
#285749=CARTESIAN_POINT('Ctrl Pts',(0.172105757888236,1.54689636808768,
2.36795670534419));
#285750=CARTESIAN_POINT('Ctrl Pts',(0.118193038426011,1.55194667340341,
2.37156112276727));
#285751=CARTESIAN_POINT('Ctrl Pts',(0.040072717003073,1.55517013570473,
2.37687622538465));
#285752=CARTESIAN_POINT('Ctrl Pts',(0.0159970198222962,1.55560405338306,
2.37852660299121));
#285753=CARTESIAN_POINT('Ctrl Pts',(-0.0275986947589804,1.55537764775832,
2.38154457177184));
#285754=CARTESIAN_POINT('Ctrl Pts',(-0.0471148847599626,1.55490882164833,
2.38290630049015));
#285755=CARTESIAN_POINT('Ctrl Pts',(-0.0777660575102398,1.55359493905898,
2.38506441648142));
#285756=CARTESIAN_POINT('Ctrl Pts',(-0.0889100284350443,1.55299703462569,
2.38585309266295));
#285757=CARTESIAN_POINT('Ctrl Pts',(-0.109793925943065,1.55165104126194,
2.3873391381327));
#285758=CARTESIAN_POINT('Ctrl Pts',(-0.119535163569938,1.55093100965304,
2.38803559434104));
#285759=CARTESIAN_POINT('Ctrl Pts',(-0.141438166121551,1.54910445715876,
2.38960930408768));
#285760=CARTESIAN_POINT('Ctrl Pts',(-0.153594853992635,1.54794637473847,
2.39048813320202));
#285761=CARTESIAN_POINT('Ctrl Pts',(-0.184889446118301,1.5445928903599,
2.39276494020047));
#285762=CARTESIAN_POINT('Ctrl Pts',(-0.20400194867309,1.54218495892787,
2.39416945296401));
#285763=CARTESIAN_POINT('Ctrl Pts',(-0.343858009883367,1.52191966394549,
2.40455402296631));
#285764=CARTESIAN_POINT('Ctrl Pts',(-0.462149943665086,1.49026296231562,
2.41397497573814));
#285765=CARTESIAN_POINT('Ctrl Pts',(-0.646620728020674,1.416799962059,2.42936872344793));
#285766=CARTESIAN_POINT('Ctrl Pts',(-0.71556105113216,1.3832626028976,2.43528505050216));
#285767=CARTESIAN_POINT('Ctrl Pts',(-0.793277116467618,1.33808415915099,
2.44195952771564));
#285768=CARTESIAN_POINT('Ctrl Pts',(-0.80471084533521,1.33123938023058,
2.44294146355601));
#285769=CARTESIAN_POINT('Ctrl Pts',(-0.821784025259197,1.32071819122326,
2.44440610512512));
#285770=CARTESIAN_POINT('Ctrl Pts',(-0.82748952939745,1.31715094354143,
2.44489528191534));
#285771=CARTESIAN_POINT('Ctrl Pts',(-0.837810349862731,1.31060453215268,
2.44577941074295));
#285772=CARTESIAN_POINT('Ctrl Pts',(-0.842433162973482,1.30763786661403,
2.44617511979236));
#285773=CARTESIAN_POINT('Ctrl Pts',(-0.852891450730796,1.30084783457559,
2.44706971098408));
#285774=CARTESIAN_POINT('Ctrl Pts',(-0.858717021864208,1.29700963635568,
2.44756760826211));
#285775=CARTESIAN_POINT('Ctrl Pts',(-0.876650846225012,1.28502007324017,
2.44909973684198));
#285776=CARTESIAN_POINT('Ctrl Pts',(-0.888670764131352,1.27673709437543,
2.45012572940544));
#285777=CARTESIAN_POINT('Ctrl Pts',(-0.977694610603518,1.21352384745478,
2.45773244897799));
#285778=CARTESIAN_POINT('Ctrl Pts',(-1.04967218386716,1.15183346022872,
2.4639348035101));
#285779=CARTESIAN_POINT('Ctrl Pts',(-1.19008112911974,1.00732757317931,
2.47719636364454));
#285780=CARTESIAN_POINT('Ctrl Pts',(-1.25644942980204,0.923218634373557,
2.48423891499443));
#285781=CARTESIAN_POINT('Ctrl Pts',(-1.32364145012773,0.81725167992026,
2.49293631527651));
#285782=CARTESIAN_POINT('Ctrl Pts',(-1.33332957760313,0.8013483529362,2.49423658732745));
#285783=CARTESIAN_POINT('Ctrl Pts',(-1.3482675063486,0.77580623721678,2.49631933710385));
#285784=CARTESIAN_POINT('Ctrl Pts',(-1.35370501926065,0.766278863154737,
2.49709499990096));
#285785=CARTESIAN_POINT('Ctrl Pts',(-1.36380664970438,0.748136108161155,
2.49857024215581));
#285786=CARTESIAN_POINT('Ctrl Pts',(-1.36849105313386,0.739532584500603,
2.49926905194541));
#285787=CARTESIAN_POINT('Ctrl Pts',(-1.37897292911854,0.719840584258869,
2.5008670937725));
#285788=CARTESIAN_POINT('Ctrl Pts',(-1.38471842951952,0.70872537696288,
2.50176810696074));
#285789=CARTESIAN_POINT('Ctrl Pts',(-1.39943089255954,0.679400756655263,
2.50414319899922));
#285790=CARTESIAN_POINT('Ctrl Pts',(-1.40817635435763,0.661083575841854,
2.50562479456309));
#285791=CARTESIAN_POINT('Ctrl Pts',(-1.46139610257825,0.543765114623971,
2.51510572608007));
#285792=CARTESIAN_POINT('Ctrl Pts',(-1.49575663871181,0.440525656554097,
2.52344245407549));
#285793=CARTESIAN_POINT('Ctrl Pts',(-1.53269384923529,0.272816253003401,
2.53675796073022));
#285794=CARTESIAN_POINT('Ctrl Pts',(-1.54251754667993,0.210284498665895,
2.54166745801651));
#285795=CARTESIAN_POINT('Ctrl Pts',(-1.55054931629728,0.125864307528075,
2.54811066000505));
#285796=CARTESIAN_POINT('Ctrl Pts',(-1.55214488539939,0.104361688238147,
2.54973559341003));
#285797=CARTESIAN_POINT('Ctrl Pts',(-1.55411634820297,0.0673920468857548,
2.5524944570358));
#285798=CARTESIAN_POINT('Ctrl Pts',(-1.55470948410108,0.0519401563658736,
2.55363710890477));
#285799=CARTESIAN_POINT('Ctrl Pts',(-1.55523953592187,0.0293458324678964,
2.55529029927697));
#285800=CARTESIAN_POINT('Ctrl Pts',(-1.5553578205403,0.0222091742669988,
2.55580990630177));
#285801=CARTESIAN_POINT('Ctrl Pts',(-1.55547521635391,0.010093767225684,
2.55668736398283));
#285802=CARTESIAN_POINT('Ctrl Pts',(-1.55549955549121,0.00511551151385498,
2.557046573119));
#285803=CARTESIAN_POINT('Ctrl Pts',(-1.55550055500129,-0.00623305962615394,
2.55786233385983));
#285804=CARTESIAN_POINT('Ctrl Pts',(-1.55546198620683,-0.012603212781979,
2.55831803909298));
#285805=CARTESIAN_POINT('Ctrl Pts',(-1.55524298703307,-0.0305564130730573,
2.55959663681348));
#285806=CARTESIAN_POINT('Ctrl Pts',(-1.55497229327071,-0.0421382398781189,
2.56041475226322));
#285807=CARTESIAN_POINT('Ctrl Pts',(-1.55151865201902,-0.14208785809607,
2.56742536402354));
#285808=CARTESIAN_POINT('Ctrl Pts',(-1.54093473269642,-0.230052205931801,
2.57326556273727));
#285809=CARTESIAN_POINT('Ctrl Pts',(-1.50025345598643,-0.425708079098914,
2.58642749510838));
#285810=CARTESIAN_POINT('Ctrl Pts',(-1.46593299070998,-0.532000676093453,
2.59371962145271));
#285811=CARTESIAN_POINT('Ctrl Pts',(-1.41234607174449,-0.652123656267256,
2.60278982029931));
#285812=CARTESIAN_POINT('Ctrl Pts',(-1.40377590850392,-0.670372899502131,
2.60419084196302));
#285813=CARTESIAN_POINT('Ctrl Pts',(-1.38933344545103,-0.699634476207907,
2.60647811831808));
#285814=CARTESIAN_POINT('Ctrl Pts',(-1.38367888090329,-0.71075210965624,
2.60735688284124));
#285815=CARTESIAN_POINT('Ctrl Pts',(-1.37334759914768,-0.730474164112806,
2.60893391649939));
#285816=CARTESIAN_POINT('Ctrl Pts',(-1.36872211959065,-0.739104785436426,
2.609630353344));
#285817=CARTESIAN_POINT('Ctrl Pts',(-1.35873155424431,-0.757330612515072,
2.61111483964458));
#285818=CARTESIAN_POINT('Ctrl Pts',(-1.35334564165858,-0.766913721265497,
2.61190360352719));
#285819=CARTESIAN_POINT('Ctrl Pts',(-1.33850956452036,-0.792668408354602,
2.61404625489145));
#285820=CARTESIAN_POINT('Ctrl Pts',(-1.32886841967543,-0.808727226098879,
2.61540695696289));
#285821=CARTESIAN_POINT('Ctrl Pts',(-1.26290386521413,-0.914235969747585,
2.62451671066246));
#285822=CARTESIAN_POINT('Ctrl Pts',(-1.19788859299908,-0.997901965547171,
2.63259193483123));
#285823=CARTESIAN_POINT('Ctrl Pts',(-1.05876675300837,-1.14357546689536,
2.64819660719498));
#285824=CARTESIAN_POINT('Ctrl Pts',(-0.98636330789025,-1.20658296999755,
2.65566661867988));
#285825=CARTESIAN_POINT('Ctrl Pts',(-0.896877519961867,-1.27098395511725,
2.66386892084485));
#285826=CARTESIAN_POINT('Ctrl Pts',(-0.88501863454347,-1.2792699309887,
2.66493658310487));
#285827=CARTESIAN_POINT('Ctrl Pts',(-0.86729223401037,-1.29129111760527,
2.66650218660591));
#285828=CARTESIAN_POINT('Ctrl Pts',(-0.861512901900403,-1.29515408134049,
2.6670079367547));
#285829=CARTESIAN_POINT('Ctrl Pts',(-0.851121331254836,-1.3019995747806,
2.6679086862076));
#285830=CARTESIAN_POINT('Ctrl Pts',(-0.846518999023105,-1.30499655187472,
2.668304607402));
#285831=CARTESIAN_POINT('Ctrl Pts',(-0.836224045776677,-1.31162310505729,
2.66918356046608));
#285832=CARTESIAN_POINT('Ctrl Pts',(-0.830523578087623,-1.31524005992995,
2.66966577232733));
#285833=CARTESIAN_POINT('Ctrl Pts',(-0.813407597652296,-1.32594451933331,
2.67110088586049));
#285834=CARTESIAN_POINT('Ctrl Pts',(-0.801923252731891,-1.33292157194271,
2.67204698064825));
#285835=CARTESIAN_POINT('Ctrl Pts',(-0.715163636109373,-1.3841031007335,
2.67908063328668));
#285836=CARTESIAN_POINT('Ctrl Pts',(-0.636366223611446,-1.42205584958139,
2.6848387232741));
#285837=CARTESIAN_POINT('Ctrl Pts',(-0.452738611381837,-1.49215965588439,
2.69778134061773));
#285838=CARTESIAN_POINT('Ctrl Pts',(-0.346879587030923,-1.5202577847029,
2.70494050612235));
#285839=CARTESIAN_POINT('Ctrl Pts',(-0.218929636560006,-1.54014961246158,
2.71386820928867));
#285840=CARTESIAN_POINT('Ctrl Pts',(-0.198844780007939,-1.54287125297838,
2.71527649834339));
#285841=CARTESIAN_POINT('Ctrl Pts',(-0.166292301277465,-1.54663617706073,
2.71757326615754));
#285842=CARTESIAN_POINT('Ctrl Pts',(-0.153854817415822,-1.54792288974287,
2.71845415010745));
#285843=CARTESIAN_POINT('Ctrl Pts',(-0.131648827777653,-1.54994992901314,
2.72003352291209));
#285844=CARTESIAN_POINT('Ctrl Pts',(-0.121886182132722,-1.55074818938852,
2.72073015823583));
#285845=CARTESIAN_POINT('Ctrl Pts',(-0.101170665819472,-1.55224520970062,
2.72221351316046));
#285846=CARTESIAN_POINT('Ctrl Pts',(-0.090216684847592,-1.55292035629755,
2.72300093331751));
#285847=CARTESIAN_POINT('Ctrl Pts',(-0.0606365381526791,-1.55442950124089,
2.7251359829264));
#285848=CARTESIAN_POINT('Ctrl Pts',(-0.0420015573161472,-1.55504459009035,
2.7264903441582));
#285849=CARTESIAN_POINT('Ctrl Pts',(0.0832035800980689,-1.55692515335418,
2.73565654078751));
#285850=CARTESIAN_POINT('Ctrl Pts',(0.189629552180823,-1.54756939757743,
2.74380067338946));
#285851=CARTESIAN_POINT('Ctrl Pts',(0.387439694919848,-1.5094630316795,
2.75940790943861));
#285852=CARTESIAN_POINT('Ctrl Pts',(0.478805181620457,-1.4830161427106,
2.76680866590746));
#285853=CARTESIAN_POINT('Ctrl Pts',(0.58075284263949,-1.44309333117666,
2.7749553681401));
#285854=CARTESIAN_POINT('Ctrl Pts',(0.594235285658215,-1.43759406390524,
2.77603009763281));
#285855=CARTESIAN_POINT('Ctrl Pts',(0.614054524904569,-1.42918363373173,
2.7776039844008));
#285856=CARTESIAN_POINT('Ctrl Pts',(0.620451694047221,-1.4264180729525,
2.77811106574666));
#285857=CARTESIAN_POINT('Ctrl Pts',(0.631857142329225,-1.42139613435803,
2.77901319204208));
#285858=CARTESIAN_POINT('Ctrl Pts',(0.636872279363323,-1.4191561301606,
2.77940917197704));
#285859=CARTESIAN_POINT('Ctrl Pts',(0.648010399062634,-1.41411036719839,
2.78028705356704));
#285860=CARTESIAN_POINT('Ctrl Pts',(0.654127126092434,-1.41129136443887,
2.78076814714088));
#285861=CARTESIAN_POINT('Ctrl Pts',(0.672318521165484,-1.40276385484631,
2.78219648133684));
#285862=CARTESIAN_POINT('Ctrl Pts',(0.68433856242492,-1.39693929351222,
2.78313701008648));
#285863=CARTESIAN_POINT('Ctrl Pts',(0.767404857507903,-1.35535822626818,
2.78962435781514));
#285864=CARTESIAN_POINT('Ctrl Pts',(0.835702109495037,-1.31434836909438,
2.79489841887045));
#285865=CARTESIAN_POINT('Ctrl Pts',(0.99702095342509,-1.19980111192904,
2.80794189397891));
#285866=CARTESIAN_POINT('Ctrl Pts',(1.08533392765734,-1.12054457248056,
2.81565897009086));
#285867=CARTESIAN_POINT('Ctrl Pts',(1.17684048033486,-1.01735563020484,
2.82517657911611));
#285868=CARTESIAN_POINT('Ctrl Pts',(1.18959156249913,-1.00241600632822,
2.82654226451089));
#285869=CARTESIAN_POINT('Ctrl Pts',(1.20987641695494,-0.977717310240944,
2.82878334579099));
#285870=CARTESIAN_POINT('Ctrl Pts',(1.21758330809194,-0.968102760741714,
2.82965175090586));
#285871=CARTESIAN_POINT('Ctrl Pts',(1.23119906186796,-0.950696962391031,
2.83121743917183));
#285872=CARTESIAN_POINT('Ctrl Pts',(1.23715028524705,-0.942939556906977,
2.83191299375885));
#285873=CARTESIAN_POINT('Ctrl Pts',(1.24969262166492,-0.926267513191243,
2.83340344113505));
#285874=CARTESIAN_POINT('Ctrl Pts',(1.25626231689482,-0.917337524578084,
2.83419911884223));
#285875=CARTESIAN_POINT('Ctrl Pts',(1.2739308659039,-0.892775408800065,
2.83638097617753));
#285876=CARTESIAN_POINT('Ctrl Pts',(1.28483673297722,-0.877007577101856,
2.83777440425378));
#285877=CARTESIAN_POINT('Ctrl Pts',(1.35324907908477,-0.774080487737208,
2.84682827946445));
#285878=CARTESIAN_POINT('Ctrl Pts',(1.40213587293735,-0.681535629227672,
2.8548051814281));
#285879=CARTESIAN_POINT('Ctrl Pts',(1.47759110572958,-0.495561895356006,
2.87035177757698));
#285880=CARTESIAN_POINT('Ctrl Pts',(1.50543778992949,-0.40313434349261,
2.87786602469441));
#285881=CARTESIAN_POINT('Ctrl Pts',(1.52741839930122,-0.294586442780442,
2.88610490051894));
#285882=CARTESIAN_POINT('Ctrl Pts',(1.53008350546317,-0.280415129016086,
2.88716901798968));
#285883=CARTESIAN_POINT('Ctrl Pts',(1.53373938815161,-0.259368336220924,
2.88873046445844));
#285884=CARTESIAN_POINT('Ctrl Pts',(1.5348817094358,-0.252520469656944,
2.88923554488033));
#285885=CARTESIAN_POINT('Ctrl Pts',(1.53684552288602,-0.240242064227605,
2.89013560374212));
#285886=CARTESIAN_POINT('Ctrl Pts',(1.53768414161506,-0.234814595174138,
2.89053149747706));
#285887=CARTESIAN_POINT('Ctrl Pts',(1.53949076964472,-0.222697339799118,
2.89141099888998));
#285888=CARTESIAN_POINT('Ctrl Pts',(1.54044393938668,-0.216005576654915,
2.89189378049337));
#285889=CARTESIAN_POINT('Ctrl Pts',(1.54316703302176,-0.195952559333154,
2.89333235461984));
#285890=CARTESIAN_POINT('Ctrl Pts',(1.54480701410226,-0.182573871970163,
2.89428129150704));
#285891=CARTESIAN_POINT('Ctrl Pts',(1.55619948955721,-0.078445722021177,
2.90159492216196));
#285892=CARTESIAN_POINT('Ctrl Pts',(1.55812277664384,0.0129950524360213,
2.9075991633634));
#285893=CARTESIAN_POINT('Ctrl Pts',(1.54499353158286,0.208760255190567,
2.92051469334018));
#285894=CARTESIAN_POINT('Ctrl Pts',(1.52740396972473,0.312441301828331,
2.92740588520839));
#285895=CARTESIAN_POINT('Ctrl Pts',(1.49408736732152,0.43324382785128,2.93604388757908));
#285896=CARTESIAN_POINT('Ctrl Pts',(1.48827110621277,0.452820410129335,
2.93746262765813));
#285897=CARTESIAN_POINT('Ctrl Pts',(1.47826158420891,0.484231753921325,
2.93977303930185));
#285898=CARTESIAN_POINT('Ctrl Pts',(1.47430736753666,0.496140577344502,
2.940656964417));
#285899=CARTESIAN_POINT('Ctrl Pts',(1.46700908661723,0.517262631852202,
2.94223970377167));
#285900=CARTESIAN_POINT('Ctrl Pts',(1.46372116829506,0.526494657129671,
2.9429366339863));
#285901=CARTESIAN_POINT('Ctrl Pts',(1.45657552064951,0.545974256252145,
2.94441841501438));
#285902=CARTESIAN_POINT('Ctrl Pts',(1.45269639984995,0.556213353270231,
2.94520394678798));
#285903=CARTESIAN_POINT('Ctrl Pts',(1.44196425145482,0.583663001433325,
2.94732832183653));
#285904=CARTESIAN_POINT('Ctrl Pts',(1.43491153687599,0.600792999314781,
2.94867378131963));
#285905=CARTESIAN_POINT('Ctrl Pts',(1.41861542388964,0.638449013400624,
2.95167675658858));
#285906=CARTESIAN_POINT('Ctrl Pts',(1.40922911693774,0.658908236596135,
2.9533387911244));
#285907=CARTESIAN_POINT('Ctrl Pts',(1.37815767813013,0.722931045069323,
2.95863818788996));
#285908=CARTESIAN_POINT('Ctrl Pts',(1.35487234529474,0.765681400764424,
2.96232482689632));
#285909=CARTESIAN_POINT('Ctrl Pts',(1.29890812074448,0.857858324668858,
2.97059220564359));
#285910=CARTESIAN_POINT('Ctrl Pts',(1.2653307724911,0.906653576759187,2.97518796305924));
#285911=CARTESIAN_POINT('Ctrl Pts',(1.18235978619529,1.01361231563654,2.98567925259935));
#285912=CARTESIAN_POINT('Ctrl Pts',(1.13129763027273,1.07030509337,2.99155700391633));
#285913=CARTESIAN_POINT('Ctrl Pts',(1.06805415707966,1.13091572828657,2.99803860412343));
#285914=CARTESIAN_POINT('Ctrl Pts',(1.05974147901181,1.13870895527512,2.99887601786343));
#285915=CARTESIAN_POINT('Ctrl Pts',(1.04662901232294,1.15073406208911,3.00017348630406));
#285916=CARTESIAN_POINT('Ctrl Pts',(1.04188768452709,1.15502866970968,3.00063794667816));
#285917=CARTESIAN_POINT('Ctrl Pts',(1.03341311851624,1.16261012951901,3.00145961257004));
#285918=CARTESIAN_POINT('Ctrl Pts',(1.02969055468353,1.16590837955585,3.00181764508412));
#285919=CARTESIAN_POINT('Ctrl Pts',(1.02061760574342,1.17386980558304,3.00268336971854));
#285920=CARTESIAN_POINT('Ctrl Pts',(1.01525103571093,1.17851430086269,3.0031896939099));
#285921=CARTESIAN_POINT('Ctrl Pts',(0.998259434841465,1.19301746632251,
3.00477554750283));
#285922=CARTESIAN_POINT('Ctrl Pts',(0.986520752139677,1.20274246012717,
3.00584598639344));
#285923=CARTESIAN_POINT('Ctrl Pts',(0.922036760475447,1.25458526120429,
3.01160343496773));
#285924=CARTESIAN_POINT('Ctrl Pts',(0.866729441571061,1.29341341674157,
3.01610499621465));
#285925=CARTESIAN_POINT('Ctrl Pts',(0.700724577967221,1.39450961375287,
3.0289487991788));
#285926=CARTESIAN_POINT('Ctrl Pts',(0.58472926498728,1.44698325229681,3.03717895612942));
#285927=CARTESIAN_POINT('Ctrl Pts',(0.444616677790696,1.49073607025549,
3.0473039978929));
#285928=CARTESIAN_POINT('Ctrl Pts',(0.42546728813207,1.49631398651695,3.04869033409328));
#285929=CARTESIAN_POINT('Ctrl Pts',(0.394236965006558,1.50476293232934,
3.05095842104059));
#285930=CARTESIAN_POINT('Ctrl Pts',(0.382219221502569,1.50786031114583,
3.05183289105533));
#285931=CARTESIAN_POINT('Ctrl Pts',(0.360661518525709,1.51314218671221,
3.05340520323229));
#285932=CARTESIAN_POINT('Ctrl Pts',(0.351135471216502,1.51538110091543,
3.05410125611887));
#285933=CARTESIAN_POINT('Ctrl Pts',(0.33082778656826,1.5199522689229,3.05558812439613));
#285934=CARTESIAN_POINT('Ctrl Pts',(0.320041246530315,1.52226000179959,
3.0563796828771));
#285935=CARTESIAN_POINT('Ctrl Pts',(0.290700729305727,1.52821165035157,
3.05853816200943));
#285936=CARTESIAN_POINT('Ctrl Pts',(0.27210392994007,1.53163218662357,3.05991207103515));
#285937=CARTESIAN_POINT('Ctrl Pts',(0.152424391623346,1.55139666412117,
3.06879487980418));
#285938=CARTESIAN_POINT('Ctrl Pts',(0.0500174042206302,1.5580614854054,
3.07660765917065));
#285939=CARTESIAN_POINT('Ctrl Pts',(-0.151265261186869,1.55129228761786,
3.09220214510162));
#285940=CARTESIAN_POINT('Ctrl Pts',(-0.249711572484758,1.5385175650785,
3.09993692614429));
#285941=CARTESIAN_POINT('Ctrl Pts',(-0.36020133242299,1.51328752380114,
3.10836592528096));
#285942=CARTESIAN_POINT('Ctrl Pts',(-0.374077901651606,1.50991718033658,
3.10941953550798));
#285943=CARTESIAN_POINT('Ctrl Pts',(-0.39460370976266,1.50463151166356,
3.11096865103442));
#285944=CARTESIAN_POINT('Ctrl Pts',(-0.401289287039485,1.50286226469941,
3.11147173846072));
#285945=CARTESIAN_POINT('Ctrl Pts',(-0.413262071626968,1.49960823696858,
3.11236975085337));
#285946=CARTESIAN_POINT('Ctrl Pts',(-0.41855342979647,1.49813999125748,
3.11276557145872));
#285947=CARTESIAN_POINT('Ctrl Pts',(-0.43036432674885,1.49479524236072,
3.113646742671));
#285948=CARTESIAN_POINT('Ctrl Pts',(-0.436879472812004,1.49290408304393,
3.11413124888338));
#285949=CARTESIAN_POINT('Ctrl Pts',(-0.456420685281606,1.48709295071666,
3.11558032605132));
#285950=CARTESIAN_POINT('Ctrl Pts',(-0.469408332446109,1.48304454974816,
3.11653789236266));
#285951=CARTESIAN_POINT('Ctrl Pts',(-0.499638140100143,1.47318463524574,
3.11875742298126));
#285952=CARTESIAN_POINT('Ctrl Pts',(-0.516835054623095,1.46723986842436,
3.12001292420044));
#285953=CARTESIAN_POINT('Ctrl Pts',(-0.578441692784673,1.44472554956781,
3.12449832805364));
#285954=CARTESIAN_POINT('Ctrl Pts',(-0.622195490663908,1.42642916181906,
3.127660990113));
#285955=CARTESIAN_POINT('Ctrl Pts',(-0.768868037623708,1.35705995177762,
3.13839893840018));
#285956=CARTESIAN_POINT('Ctrl Pts',(-0.866923512173226,1.29661556168341,
3.14584365517639));
#285957=CARTESIAN_POINT('Ctrl Pts',(-0.982950057962604,1.20600076044267,
3.15587400533882));
#285958=CARTESIAN_POINT('Ctrl Pts',(-1.00783865995165,1.1852804045838,3.15810525264408));
#285959=CARTESIAN_POINT('Ctrl Pts',(-1.04143270502985,1.15548910081853,
3.16124265130202));
#285960=CARTESIAN_POINT('Ctrl Pts',(-1.05070319900776,1.14706578394168,
3.16212234648344));
#285961=CARTESIAN_POINT('Ctrl Pts',(-1.0665910842775,1.13227558941044,3.16365503861152));
#285962=CARTESIAN_POINT('Ctrl Pts',(-1.07325578841065,1.12596028239409,
3.16430583382692));
#285963=CARTESIAN_POINT('Ctrl Pts',(-1.08705242355571,1.11265314534313,
3.16566986609521));
#285964=CARTESIAN_POINT('Ctrl Pts',(-1.09417368295046,1.1056509107157,3.16638353736243));
#285965=CARTESIAN_POINT('Ctrl Pts',(-1.10133637441836,1.09847096658192,
3.1671113628377));
#285966=CARTESIAN_POINT('Ctrl Pts',(-1.1014458626608,1.09836118179211,3.16712249070733));
#285967=CARTESIAN_POINT('Ctrl Pts',(-1.10165197161736,1.09815445278218,
3.16714344316502));
#285968=CARTESIAN_POINT('Ctrl Pts',(-1.10174859596465,1.09805751216576,
3.16715326759318));
#285969=CARTESIAN_POINT('Ctrl Pts',(-1.10217388008621,1.09763072336411,
3.16719651723325));
#285970=CARTESIAN_POINT('Ctrl Pts',(-1.10250240423269,1.09730074067112,
3.16722994841665));
#285971=CARTESIAN_POINT('Ctrl Pts',(-1.10315555665418,1.09664409901889,
3.16729645740822));
#285972=CARTESIAN_POINT('Ctrl Pts',(-1.10348018813518,1.09631744329928,
3.16732953507058));
#285973=CARTESIAN_POINT('Ctrl Pts',(-1.10412692923241,1.09566609116397,
3.16739547572099));
#285974=CARTESIAN_POINT('Ctrl Pts',(-1.1044490408081,1.09534139675261,3.16742833861797));
#285975=CARTESIAN_POINT('Ctrl Pts',(-1.10509204237063,1.0946926673083,3.16749398163268));
#285976=CARTESIAN_POINT('Ctrl Pts',(-1.10541293315803,1.09436863312852,
3.16752676171061));
#285977=CARTESIAN_POINT('Ctrl Pts',(-1.11613713336564,1.0835298511363,3.16862297261422));
#285978=CARTESIAN_POINT('Ctrl Pts',(-1.12638973211028,1.07286773746764,
3.16969294893012));
#285979=CARTESIAN_POINT('Ctrl Pts',(-1.16653057742277,1.02991390597024,
3.17397206823615));
#285980=CARTESIAN_POINT('Ctrl Pts',(-1.19519221515717,0.996509461924799,
3.17723161271355));
#285981=CARTESIAN_POINT('Ctrl Pts',(-1.26996313341132,0.901493203385047,
3.18632775768287));
#285982=CARTESIAN_POINT('Ctrl Pts',(-1.31297533672047,0.837609561656838,
3.19226036085286));
#285983=CARTESIAN_POINT('Ctrl Pts',(-1.39412737780445,0.695366349155964,
3.20495741208171));
#285984=CARTESIAN_POINT('Ctrl Pts',(-1.43078035342767,0.616438087350189,
3.21170935005537));
#285985=CARTESIAN_POINT('Ctrl Pts',(-1.46573798987217,0.520971233778383,
3.21927935009162));
#285986=CARTESIAN_POINT('Ctrl Pts',(-1.47062420942662,0.507014159832948,
3.22037151192684));
#285987=CARTESIAN_POINT('Ctrl Pts',(-1.47756506522608,0.48624306196291,
3.22197331956063));
#285988=CARTESIAN_POINT('Ctrl Pts',(-1.47977300648383,0.479481690862227,
3.22249107366785));
#285989=CARTESIAN_POINT('Ctrl Pts',(-1.48360582688244,0.467465769476506,
3.22340442581184));
#285990=CARTESIAN_POINT('Ctrl Pts',(-1.48524930984756,0.462217466200462,
3.22380106321185));
#285991=CARTESIAN_POINT('Ctrl Pts',(-1.48880835674623,0.450636979885078,
3.22467118189785));
#285992=CARTESIAN_POINT('Ctrl Pts',(-1.49071139651586,0.444301189905672,
3.22514394494026));
#285993=CARTESIAN_POINT('Ctrl Pts',(-1.49616723767508,0.425707319864655,
3.22652230342076));
#285994=CARTESIAN_POINT('Ctrl Pts',(-1.49960977716647,0.413417064395333,
3.22742186735222));
#285995=CARTESIAN_POINT('Ctrl Pts',(-1.50721625996785,0.384914926079717,
3.22948454254925));
#285996=CARTESIAN_POINT('Ctrl Pts',(-1.51127066093205,0.368675190079421,
3.230642384677));
#285997=CARTESIAN_POINT('Ctrl Pts',(-1.54183408149476,0.237264552494566,
3.23989532945207));
#285998=CARTESIAN_POINT('Ctrl Pts',(-1.55540235308476,0.119474178713039,
3.24749806769915));
#285999=CARTESIAN_POINT('Ctrl Pts',(-1.55549947486934,0.00127815539530785,
3.25533825218605));
#286000=CARTESIAN_POINT('',(-1.55745492001379,-0.000856371120316864,4.65594377439631));
#286001=CARTESIAN_POINT('Ctrl Pts',(-1.55549947609198,0.00127666658565867,
3.25533835094186));
#286002=CARTESIAN_POINT('Ctrl Pts',(-1.55555636301431,-0.068034756513225,
3.25993592059349));
#286003=CARTESIAN_POINT('Ctrl Pts',(-1.5509806632431,-0.137266448596484,
3.26459545993076));
#286004=CARTESIAN_POINT('Ctrl Pts',(-1.54000197289467,-0.219452747316245,
3.27034228132855));
#286005=CARTESIAN_POINT('Ctrl Pts',(-1.53802239591289,-0.232922035318707,
3.27129093017571));
#286006=CARTESIAN_POINT('Ctrl Pts',(-1.5342860329217,-0.256215095950785,
3.27294431259784));
#286007=CARTESIAN_POINT('Ctrl Pts',(-1.53261100875688,-0.266051299250875,
3.2736464905484));
#286008=CARTESIAN_POINT('Ctrl Pts',(-1.52906086660576,-0.285751502078462,
3.27506123479516));
#286009=CARTESIAN_POINT('Ctrl Pts',(-1.527184642059,-0.295614808819637,
3.27577380436043));
#286010=CARTESIAN_POINT('Ctrl Pts',(-1.52342183017665,-0.314403218942805,
3.27713961400922));
#286011=CARTESIAN_POINT('Ctrl Pts',(-1.52155195041569,-0.323331273436458,
3.27779229414113));
#286012=CARTESIAN_POINT('Ctrl Pts',(-1.51648168317265,-0.346521575533898,
3.27949743458108));
#286013=CARTESIAN_POINT('Ctrl Pts',(-1.51315866393737,-0.360755773846104,
3.28055377093904));
#286014=CARTESIAN_POINT('Ctrl Pts',(-1.50067230704378,-0.411030004087195,
3.28432044354167));
#286015=CARTESIAN_POINT('Ctrl Pts',(-1.49041848385317,-0.446783336945632,
3.2870651047785));
#286016=CARTESIAN_POINT('Ctrl Pts',(-1.45422352076932,-0.557807889208187,
3.29580263104219));
#286017=CARTESIAN_POINT('Ctrl Pts',(-1.42378348872899,-0.631469236309211,
3.30192359216912));
#286018=CARTESIAN_POINT('Ctrl Pts',(-1.35044173655222,-0.776368094074657,
3.31450909850219));
#286019=CARTESIAN_POINT('Ctrl Pts',(-1.3071924930239,-0.847165847015035,
3.32095745088693));
#286020=CARTESIAN_POINT('Ctrl Pts',(-1.24595308124008,-0.93147063269499,
3.32878976067696));
#286021=CARTESIAN_POINT('Ctrl Pts',(-1.23304232537736,-0.948495314694816,
3.33037949802974));
#286022=CARTESIAN_POINT('Ctrl Pts',(-1.21466800451578,-0.971714908216085,
3.33255321819721));
#286023=CARTESIAN_POINT('Ctrl Pts',(-1.20950040489606,-0.978139561962613,
3.33315526586101));
#286024=CARTESIAN_POINT('Ctrl Pts',(-1.200701706323,-0.988902248617583,
3.33416441677587));
#286025=CARTESIAN_POINT('Ctrl Pts',(-1.19709763246799,-0.993262053784068,
3.33457337170336));
#286026=CARTESIAN_POINT('Ctrl Pts',(-1.19008433822079,-1.0016523257877,
3.33536056396761));
#286027=CARTESIAN_POINT('Ctrl Pts',(-1.18667829302194,-1.0056852116544,
3.33573903357952));
#286028=CARTESIAN_POINT('Ctrl Pts',(-1.17726103923134,-1.01672113648853,
3.33677522908943));
#286029=CARTESIAN_POINT('Ctrl Pts',(-1.1712078082803,-1.02368828493918,
3.33742997574959));
#286030=CARTESIAN_POINT('Ctrl Pts',(-1.14646344119339,-1.05166174111665,
3.3400631875505));
#286031=CARTESIAN_POINT('Ctrl Pts',(-1.12726506000858,-1.07221479757286,
3.34200802260382));
#286032=CARTESIAN_POINT('Ctrl Pts',(-1.03558854550464,-1.16517391154232,
3.35091688400592));
#286033=CARTESIAN_POINT('Ctrl Pts',(-0.956623215333674,-1.23083300241658,
3.35755332282966));
#286034=CARTESIAN_POINT('Ctrl Pts',(-0.826791936735691,-1.31869046926926,
3.36791364693219));
#286035=CARTESIAN_POINT('Ctrl Pts',(-0.780255727280477,-1.34674784641127,
3.37153026591221));
#286036=CARTESIAN_POINT('Ctrl Pts',(-0.701055197233776,-1.38901409910495,
3.37763249794857));
#286037=CARTESIAN_POINT('Ctrl Pts',(-0.669200171694033,-1.40463851742739,
3.38007317469693));
#286038=CARTESIAN_POINT('Ctrl Pts',(-0.624076741214118,-1.42488743515708,
3.38352849780757));
#286039=CARTESIAN_POINT('Ctrl Pts',(-0.611236276924471,-1.43044264934545,
3.38451149394211));
#286040=CARTESIAN_POINT('Ctrl Pts',(-0.58907611692635,-1.43967702308222,
3.38620846075533));
#286041=CARTESIAN_POINT('Ctrl Pts',(-0.579792439598855,-1.44344079226404,
3.38691952834639));
#286042=CARTESIAN_POINT('Ctrl Pts',(-0.560827180617548,-1.45091716856823,
3.38837278597361));
#286043=CARTESIAN_POINT('Ctrl Pts',(-0.551143553121849,-1.45462315765944,
3.38911515553482));
#286044=CARTESIAN_POINT('Ctrl Pts',(-0.526629839128992,-1.46372480176176,
3.39099567970757));
#286045=CARTESIAN_POINT('Ctrl Pts',(-0.511753661466734,-1.46899198045441,
3.39213802629635));
#286046=CARTESIAN_POINT('Ctrl Pts',(-0.453035621932517,-1.48878202011007,
3.39665307910348));
#286047=CARTESIAN_POINT('Ctrl Pts',(-0.408640205822372,-1.50157435847985,
3.40008095443692));
#286048=CARTESIAN_POINT('Ctrl Pts',(-0.255513450740731,-1.53840337355354,
3.41195667891545));
#286049=CARTESIAN_POINT('Ctrl Pts',(-0.144807330525522,-1.55273876693325,
3.42065880800892));
#286050=CARTESIAN_POINT('Ctrl Pts',(0.004132861190327,-1.55595081339322,
3.43214501955476));
#286051=CARTESIAN_POINT('Ctrl Pts',(0.0418235546820907,-1.55539422096193,
3.43502941324711));
#286052=CARTESIAN_POINT('Ctrl Pts',(0.10249371456765,-1.55229097424402,
3.4396036949247));
#286053=CARTESIAN_POINT('Ctrl Pts',(0.125500868627657,-1.55060049933973,
3.44132227232295));
#286054=CARTESIAN_POINT('Ctrl Pts',(0.156757604052148,-1.54760354399071,
3.44362797298079));
#286055=CARTESIAN_POINT('Ctrl Pts',(0.165045507128445,-1.54674162829495,
3.44423654443791));
#286056=CARTESIAN_POINT('Ctrl Pts',(0.178963991088941,-1.54518099998449,
3.44525341771928));
#286057=CARTESIAN_POINT('Ctrl Pts',(0.184598319631074,-1.54451801459293,
3.44566363465049));
#286058=CARTESIAN_POINT('Ctrl Pts',(0.196182702561097,-1.54309059385179,
3.44650397005745));
#286059=CARTESIAN_POINT('Ctrl Pts',(0.202132152454718,-1.54232254403329,
3.44693388769497));
#286060=CARTESIAN_POINT('Ctrl Pts',(0.217855738457863,-1.54020014619171,
3.44806607293528));
#286061=CARTESIAN_POINT('Ctrl Pts',(0.227621885920454,-1.53878715340594,
3.44876516564103));
#286062=CARTESIAN_POINT('Ctrl Pts',(0.271145959533851,-1.53206652598437,
3.45186502830363));
#286063=CARTESIAN_POINT('Ctrl Pts',(0.3047397487805,-1.52573984587856,3.45421536161804));
#286064=CARTESIAN_POINT('Ctrl Pts',(0.423769812313167,-1.4992339788108,
3.46247986473848));
#286065=CARTESIAN_POINT('Ctrl Pts',(0.50767681155227,-1.47293921695385,
3.46819518351669));
#286066=CARTESIAN_POINT('Ctrl Pts',(0.657267589050469,-1.41174791254404,
3.47885653038172));
#286067=CARTESIAN_POINT('Ctrl Pts',(0.723528001101439,-1.37896278804597,
3.48376618340053));
#286068=CARTESIAN_POINT('Ctrl Pts',(0.810393459367767,-1.32799303095066,
3.49067338773692));
#286069=CARTESIAN_POINT('Ctrl Pts',(0.83322345134701,-1.31378901710073,
3.49253566037138));
#286070=CARTESIAN_POINT('Ctrl Pts',(0.866197374562894,-1.29206856901142,
3.49530245564349));
#286071=CARTESIAN_POINT('Ctrl Pts',(0.876637011429837,-1.2850084094341,
3.49619013832473));
#286072=CARTESIAN_POINT('Ctrl Pts',(0.895045087005136,-1.27223060150572,
3.49777705307115));
#286073=CARTESIAN_POINT('Ctrl Pts',(0.903047502523863,-1.26656291250153,
3.4984743634031));
#286074=CARTESIAN_POINT('Ctrl Pts',(0.919845763184944,-1.25442546117433,
3.4999542773811));
#286075=CARTESIAN_POINT('Ctrl Pts',(0.928628107287691,-1.24793801640575,
3.50073753825502));
#286076=CARTESIAN_POINT('Ctrl Pts',(0.952009400812185,-1.23028296758673,
3.50284908880825));
#286077=CARTESIAN_POINT('Ctrl Pts',(0.96647950255674,-1.21894848002039,
3.50418385694387));
#286078=CARTESIAN_POINT('Ctrl Pts',(1.04910836862365,-1.15182866070994,
3.51197338114825));
#286079=CARTESIAN_POINT('Ctrl Pts',(1.11261984906035,-1.09060062878491,
3.51864824440964));
#286080=CARTESIAN_POINT('Ctrl Pts',(1.21422681537294,-0.974485543846351,
3.53055160158723));
#286081=CARTESIAN_POINT('Ctrl Pts',(1.25462195207191,-0.92189613788677,
3.53571338341064));
#286082=CARTESIAN_POINT('Ctrl Pts',(1.31181505121666,-0.836686860943733,
3.54361973557424));
#286083=CARTESIAN_POINT('Ctrl Pts',(1.33102451339317,-0.805777715987354,
3.54640173933781));
#286084=CARTESIAN_POINT('Ctrl Pts',(1.36034198325775,-0.754690032562884,
3.5508340548911));
#286085=CARTESIAN_POINT('Ctrl Pts',(1.37112573231021,-0.734916131178003,
3.5525110996419));
#286086=CARTESIAN_POINT('Ctrl Pts',(1.38527243511559,-0.707579484864783,
3.55477079903634));
#286087=CARTESIAN_POINT('Ctrl Pts',(1.38900955555442,-0.700214902430107,
3.55537385257168));
#286088=CARTESIAN_POINT('Ctrl Pts',(1.3952084484232,-0.687754068677631,
3.55638419238375));
#286089=CARTESIAN_POINT('Ctrl Pts',(1.39770134830342,-0.682673581395842,
3.55679334010321));
#286090=CARTESIAN_POINT('Ctrl Pts',(1.40279022515602,-0.672157802693309,
3.55763432365127));
#286091=CARTESIAN_POINT('Ctrl Pts',(1.40538244155005,-0.666720873983832,
3.55806593501159));
#286092=CARTESIAN_POINT('Ctrl Pts',(1.412185309762,-0.6522365225579,3.55920766714626));
#286093=CARTESIAN_POINT('Ctrl Pts',(1.41634067935657,-0.643163217408742,
3.55991451678114));
#286094=CARTESIAN_POINT('Ctrl Pts',(1.43485049291289,-0.601697263365362,
3.56310988445278));
#286095=CARTESIAN_POINT('Ctrl Pts',(1.44818417662808,-0.568857264653831,
3.56554405044368));
#286096=CARTESIAN_POINT('Ctrl Pts',(1.49425029679426,-0.443248864300203,
3.57459958442957));
#286097=CARTESIAN_POINT('Ctrl Pts',(1.5192831974232,-0.347900607583221,
3.58097242439141));
#286098=CARTESIAN_POINT('Ctrl Pts',(1.54342790764834,-0.20012347509704,
3.59088301926671));
#286099=CARTESIAN_POINT('Ctrl Pts',(1.54919415116144,-0.149050211108787,
3.59431165320413));
#286100=CARTESIAN_POINT('Ctrl Pts',(1.55388797615725,-0.0745339383343615,
3.59939324396655));
#286101=CARTESIAN_POINT('Ctrl Pts',(1.5548300263918,-0.0512508509370472,
3.60099195633002));
#286102=CARTESIAN_POINT('Ctrl Pts',(1.55559076982541,-0.008929635308371,
3.60392421222815));
#286103=CARTESIAN_POINT('Ctrl Pts',(1.55558358735467,0.0101009605514342,
3.60525240250771));
#286104=CARTESIAN_POINT('Ctrl Pts',(1.55502026716753,0.0401803687480065,
3.60736939480889));
#286105=CARTESIAN_POINT('Ctrl Pts',(1.55469539221525,0.0512320155038053,
3.60815098067865));
#286106=CARTESIAN_POINT('Ctrl Pts',(1.55386110397078,0.072052751544113,
3.60963101894076));
#286107=CARTESIAN_POINT('Ctrl Pts',(1.55337729501805,0.0818223730589093,
3.61032863566028));
#286108=CARTESIAN_POINT('Ctrl Pts',(1.55207311622877,0.10393402554231,3.61191500533818));
#286109=CARTESIAN_POINT('Ctrl Pts',(1.55119761624159,0.116272003274297,
3.61280544138234));
#286110=CARTESIAN_POINT('Ctrl Pts',(1.54853805511277,0.148331510439461,
3.6151334898225));
#286111=CARTESIAN_POINT('Ctrl Pts',(1.54652442686002,0.168031173773354,
3.61657814104813));
#286112=CARTESIAN_POINT('Ctrl Pts',(1.53007923902965,0.303329315987584,
3.62660155423526));
#286113=CARTESIAN_POINT('Ctrl Pts',(1.50307908287751,0.417006390805818,
3.6355763257446));
#286114=CARTESIAN_POINT('Ctrl Pts',(1.43600468167521,0.603442703668241,
3.65094057835458));
#286115=CARTESIAN_POINT('Ctrl Pts',(1.40233782785666,0.678014777586669,
3.65726679036765));
#286116=CARTESIAN_POINT('Ctrl Pts',(1.35671870508305,0.760961646743699,
3.66429079966784));
#286117=CARTESIAN_POINT('Ctrl Pts',(1.3503300756,0.772241535201837,3.66524552776955));
#286118=CARTESIAN_POINT('Ctrl Pts',(1.34044864771552,0.789190707527497,
3.66667793867374));
#286119=CARTESIAN_POINT('Ctrl Pts',(1.33705943048695,0.794919262412172,
3.66716169082696));
#286120=CARTESIAN_POINT('Ctrl Pts',(1.33080429584923,0.805338679960141,
3.66804062519395));
#286121=CARTESIAN_POINT('Ctrl Pts',(1.32795022312521,0.81003621538047,3.66843650954346));
#286122=CARTESIAN_POINT('Ctrl Pts',(1.32137249300323,0.820734336989193,
3.66933730214877));
#286123=CARTESIAN_POINT('Ctrl Pts',(1.31763280997389,0.826724803318949,
3.66984116374378));
#286124=CARTESIAN_POINT('Ctrl Pts',(1.30579495149924,0.845403066585856,
3.67141119406506));
#286125=CARTESIAN_POINT('Ctrl Pts',(1.2975530429848,0.857999385199282,3.6724685275511));
#286126=CARTESIAN_POINT('Ctrl Pts',(1.24269319555203,0.939244057838746,
3.67929249444921));
#286127=CARTESIAN_POINT('Ctrl Pts',(1.19082224234533,1.00419713148771,3.68477259516927));
#286128=CARTESIAN_POINT('Ctrl Pts',(1.07953499067042,1.12272804470259,3.69548070074411));
#286129=CARTESIAN_POINT('Ctrl Pts',(1.02069138965888,1.17647871004343,3.70069560540467));
#286130=CARTESIAN_POINT('Ctrl Pts',(0.922573193418669,1.25318014357146,
3.70909199998385));
#286131=CARTESIAN_POINT('Ctrl Pts',(0.885969910606948,1.2793195337588,3.71216547836994));
#286132=CARTESIAN_POINT('Ctrl Pts',(0.835539459915452,1.3121301025144,3.71635906223002));
#286133=CARTESIAN_POINT('Ctrl Pts',(0.822669699609553,1.32023714978015,
3.71742576513364));
#286134=CARTESIAN_POINT('Ctrl Pts',(0.800930067702131,1.33349029856865,
3.71922308037209));
#286135=CARTESIAN_POINT('Ctrl Pts',(0.792124272593447,1.33873988413531,
3.71994986578926));
#286136=CARTESIAN_POINT('Ctrl Pts',(0.774640299040049,1.34893008217025,
3.72139085839308));
#286137=CARTESIAN_POINT('Ctrl Pts',(0.765965153526019,1.35387493310429,
3.7221048682509));
#286138=CARTESIAN_POINT('Ctrl Pts',(0.744697785910184,1.36572754566991,
3.72385326496467));
#286139=CARTESIAN_POINT('Ctrl Pts',(0.732056561704041,1.37254496687758,
3.72489080527215));
#286140=CARTESIAN_POINT('Ctrl Pts',(0.68799732726288,1.39552433507698,3.72850230566189));
#286141=CARTESIAN_POINT('Ctrl Pts',(0.656126503702749,1.41078918793012,
3.73110687668809));
#286142=CARTESIAN_POINT('Ctrl Pts',(0.51104245775799,1.4742989105341,3.7429366879226));
#286143=CARTESIAN_POINT('Ctrl Pts',(0.392873733313165,1.51008711481171,
3.75254761875624));
#286144=CARTESIAN_POINT('Ctrl Pts',(0.233165331413972,1.53842448422345,
3.76506406446787));
#286145=CARTESIAN_POINT('Ctrl Pts',(0.194332170346677,1.54381066942751,
3.76806725649022));
#286146=CARTESIAN_POINT('Ctrl Pts',(0.131768949098832,1.5500897167826,3.77280518281364));
#286147=CARTESIAN_POINT('Ctrl Pts',(0.108150609741525,1.55191648905868,
3.77457093955468));
#286148=CARTESIAN_POINT('Ctrl Pts',(0.0760961965679511,1.55366033000777,
3.77692872170522));
#286149=CARTESIAN_POINT('Ctrl Pts',(0.067690391582637,1.55404925006199,
3.77754341612601));
#286150=CARTESIAN_POINT('Ctrl Pts',(0.0535968243735233,1.55458675989007,
3.7785675607031));
#286151=CARTESIAN_POINT('Ctrl Pts',(0.0479107405784851,1.55477238805508,
3.77897898570384));
#286152=CARTESIAN_POINT('Ctrl Pts',(0.0362529875301706,1.55508895085637,
3.7798187137457));
#286153=CARTESIAN_POINT('Ctrl Pts',(0.0302813823038815,1.5552166940008,
3.78024684141266));
#286154=CARTESIAN_POINT('Ctrl Pts',(0.0145610975131198,1.55546239759026,
3.78136893310438));
#286155=CARTESIAN_POINT('Ctrl Pts',(0.00481159307827026,1.55552311372443,
3.7820598227982));
#286156=CARTESIAN_POINT('Ctrl Pts',(-0.0378791804796244,1.5553875848365,
3.78506565517926));
#286157=CARTESIAN_POINT('Ctrl Pts',(-0.0708115042965037,1.5542366239092,
3.78733384626596));
#286158=CARTESIAN_POINT('Ctrl Pts',(-0.192146242715132,1.54613076872397,
3.79558602115116));
#286159=CARTESIAN_POINT('Ctrl Pts',(-0.279946816427306,1.53266851477264,
3.80135920426103));
#286160=CARTESIAN_POINT('Ctrl Pts',(-0.438421594734923,1.49428903064163,
3.81211379406688));
#286161=CARTESIAN_POINT('Ctrl Pts',(-0.509359238614342,1.47161972996556,
3.81705812668869));
#286162=CARTESIAN_POINT('Ctrl Pts',(-0.603373620719994,1.433961071814,3.82400366610278));
#286163=CARTESIAN_POINT('Ctrl Pts',(-0.628083494394794,1.4233113002842,
3.82586723775084));
#286164=CARTESIAN_POINT('Ctrl Pts',(-0.663947013090571,1.40673861449331,
3.82863559706412));
#286165=CARTESIAN_POINT('Ctrl Pts',(-0.675325429118334,1.40131178324793,
3.82952351672298));
#286166=CARTESIAN_POINT('Ctrl Pts',(-0.695435761739544,1.39141852806241,
3.83111069536805));
#286167=CARTESIAN_POINT('Ctrl Pts',(-0.70419386320616,1.38700663802407,
3.8318080302416));
#286168=CARTESIAN_POINT('Ctrl Pts',(-0.722612125356986,1.37750903461496,
3.83328782927408));
#286169=CARTESIAN_POINT('Ctrl Pts',(-0.732261593166479,1.37240386624409,
3.83407094918143));
#286170=CARTESIAN_POINT('Ctrl Pts',(-0.758003556853467,1.35843599722655,
3.83618170406055));
#286171=CARTESIAN_POINT('Ctrl Pts',(-0.773993651662779,1.349389315307,3.83751580898132));
#286172=CARTESIAN_POINT('Ctrl Pts',(-0.867912742242529,1.29403433782016,
3.84549280420195));
#286173=CARTESIAN_POINT('Ctrl Pts',(-0.941819358241475,1.24127688537395,
3.85236999399862));
#286174=CARTESIAN_POINT('Ctrl Pts',(-1.06046185601247,1.13986230438382,
3.86442027611628));
#286175=CARTESIAN_POINT('Ctrl Pts',(-1.10748649053048,1.09422989997088,
3.86952048497875));
#286176=CARTESIAN_POINT('Ctrl Pts',(-1.17519305250935,1.01967832718774,
3.87727363263458));
#286177=CARTESIAN_POINT('Ctrl Pts',(-1.19799771081896,0.992786187595589,
3.8799667157724));
#286178=CARTESIAN_POINT('Ctrl Pts',(-1.22922439433509,0.953317847773736,
3.88375158797986));
#286179=CARTESIAN_POINT('Ctrl Pts',(-1.23840652782861,0.941359039846569,
3.88487746700926));
#286180=CARTESIAN_POINT('Ctrl Pts',(-1.25444861533644,0.919824759463701,
3.88686537699504));
#286181=CARTESIAN_POINT('Ctrl Pts',(-1.2613763252139,0.910301436390494,
3.88773113941705));
#286182=CARTESIAN_POINT('Ctrl Pts',(-1.27190747065873,0.895473467697975,
3.88905754314952));
#286183=CARTESIAN_POINT('Ctrl Pts',(-1.2755871992015,0.89022393051287,3.88952301757761));
#286184=CARTESIAN_POINT('Ctrl Pts',(-1.28237846404818,0.880406874625131,
3.8903856460625));
#286185=CARTESIAN_POINT('Ctrl Pts',(-1.28549814657052,0.875845480949425,
3.89078331274325));
#286186=CARTESIAN_POINT('Ctrl Pts',(-1.29267178610846,0.865235756789333,
3.89170115675782));
#286187=CARTESIAN_POINT('Ctrl Pts',(-1.296707673361,0.859175463389674,3.89222013882502));
#286188=CARTESIAN_POINT('Ctrl Pts',(-1.30986283085658,0.839117804373722,
3.89392125255312));
#286189=CARTESIAN_POINT('Ctrl Pts',(-1.31879955375557,0.825001285624095,
3.89509216559827));
#286190=CARTESIAN_POINT('Ctrl Pts',(-1.3889888555903,0.710073554214989,
3.90443856161685));
#286191=CARTESIAN_POINT('Ctrl Pts',(-1.43882834576127,0.602723390326337,
3.9120491754229));
#286192=CARTESIAN_POINT('Ctrl Pts',(-1.49322458637397,0.439115322474908,
3.92344314042068));
#286193=CARTESIAN_POINT('Ctrl Pts',(-1.50767126371583,0.386611679851463,
3.92706709070472));
#286194=CARTESIAN_POINT('Ctrl Pts',(-1.52695175419809,0.298764894657836,
3.93318024184384));
#286195=CARTESIAN_POINT('Ctrl Pts',(-1.53337567603653,0.263819700083939,
3.93562428435745));
#286196=CARTESIAN_POINT('Ctrl Pts',(-1.54065543975724,0.214841804074365,
3.93908357142496));
#286197=CARTESIAN_POINT('Ctrl Pts',(-1.54252631174179,0.200969499884393,
3.94006706569299));
#286198=CARTESIAN_POINT('Ctrl Pts',(-1.54541459944443,0.177128044713284,
3.94176462251039));
#286199=CARTESIAN_POINT('Ctrl Pts',(-1.54652338701966,0.167170671057837,
3.94247577667004));
#286200=CARTESIAN_POINT('Ctrl Pts',(-1.54846004680897,0.148105887376254,
3.94384185183636));
#286201=CARTESIAN_POINT('Ctrl Pts',(-1.5493039488103,0.139000496565293,
3.9444962381434));
#286202=CARTESIAN_POINT('Ctrl Pts',(-1.55110068309366,0.117558550688944,
3.94604205657141));
#286203=CARTESIAN_POINT('Ctrl Pts',(-1.55198668479284,0.10521718357475,
3.94693554192459));
#286204=CARTESIAN_POINT('Ctrl Pts',(-1.55459300703015,0.0616397275709051,
3.95010443167856));
#286205=CARTESIAN_POINT('Ctrl Pts',(-1.55551809585118,0.0303655654496407,
3.95240415978236));
#286206=CARTESIAN_POINT('Ctrl Pts',(-1.55547231161344,-0.0476181484890411,
3.95820590104762));
#286207=CARTESIAN_POINT('Ctrl Pts',(-1.55334140971594,-0.0942939081123456,
3.96173918062137));
#286208=CARTESIAN_POINT('Ctrl Pts',(-1.54073147060111,-0.233032009695838,
3.97240384497363));
#286209=CARTESIAN_POINT('Ctrl Pts',(-1.52412881540005,-0.32432620919854,
3.97964783186824));
#286210=CARTESIAN_POINT('Ctrl Pts',(-1.4869309447167,-0.459187395178376,
3.99039505726241));
#286211=CARTESIAN_POINT('Ctrl Pts',(-1.47228260805344,-0.504184070953742,
3.99398587024141));
#286212=CARTESIAN_POINT('Ctrl Pts',(-1.45179123062934,-0.558569120201987,
3.99827969010788));
#286213=CARTESIAN_POINT('Ctrl Pts',(-1.44787199215751,-0.568650992428621,
3.99907364317118));
#286214=CARTESIAN_POINT('Ctrl Pts',(-1.44153915635084,-0.584451553349586,
4.00031384539995));
#286215=CARTESIAN_POINT('Ctrl Pts',(-1.43919604853425,-0.590197843946866,
4.00076401621179));
#286216=CARTESIAN_POINT('Ctrl Pts',(-1.43468118832606,-0.601083407594687,
4.00161495703086));
#286217=CARTESIAN_POINT('Ctrl Pts',(-1.43251616607369,-0.606225049022795,
4.00201607337361));
#286218=CARTESIAN_POINT('Ctrl Pts',(-1.42725963287987,-0.618523207418431,
4.00297374024622));
#286219=CARTESIAN_POINT('Ctrl Pts',(-1.42414190776367,-0.625668323590043,
4.00352871988585));
#286220=CARTESIAN_POINT('Ctrl Pts',(-1.41309686450117,-0.650470680257412,
4.00545127401956));
#286221=CARTESIAN_POINT('Ctrl Pts',(-1.40489343614958,-0.668004024275859,
4.00680343264835));
#286222=CARTESIAN_POINT('Ctrl Pts',(-1.38345455373738,-0.71168265731973,
4.01016573946192));
#286223=CARTESIAN_POINT('Ctrl Pts',(-1.36980329919845,-0.737616328855921,
4.01215644565738));
#286224=CARTESIAN_POINT('Ctrl Pts',(-1.29513009721513,-0.870242934748685,
4.02238746669098));
#286225=CARTESIAN_POINT('Ctrl Pts',(-1.22235378308397,-0.969813704185752,
4.03027642134697));
#286226=CARTESIAN_POINT('Ctrl Pts',(-1.10615650274413,-1.09465400701222,
4.04174466215157));
#286227=CARTESIAN_POINT('Ctrl Pts',(-1.07211847421113,-1.12801190828714,
4.04499321356094));
#286228=CARTESIAN_POINT('Ctrl Pts',(-1.02472604408822,-1.17037202627195,
4.04941813880094));
#286229=CARTESIAN_POINT('Ctrl Pts',(-1.01268380604388,-1.18080719063618,
4.05053449303518));
#286230=CARTESIAN_POINT('Ctrl Pts',(-0.992520155394636,-1.19774461326445,
4.05239209867542));
#286231=CARTESIAN_POINT('Ctrl Pts',(-0.984489831481499,-1.20435384321748,
4.05312894092772));
#286232=CARTESIAN_POINT('Ctrl Pts',(-0.968611105441615,-1.21715764586873,
4.05458055688707));
#286233=CARTESIAN_POINT('Ctrl Pts',(-0.960768049935251,-1.22335806455184,
4.05529504774315));
#286234=CARTESIAN_POINT('Ctrl Pts',(-0.941895262668087,-1.23798473778365,
4.05700872623285));
#286235=CARTESIAN_POINT('Ctrl Pts',(-0.930811624898668,-1.24633967784649,
4.05801065270189));
#286236=CARTESIAN_POINT('Ctrl Pts',(-0.891619971065352,-1.27506830212165,
4.06153897143121));
#286237=CARTESIAN_POINT('Ctrl Pts',(-0.862944986432265,-1.29464703513419,
4.06409516576382));
#286238=CARTESIAN_POINT('Ctrl Pts',(-0.789237489385882,-1.34143603405404,
4.07060808817145));
#286239=CARTESIAN_POINT('Ctrl Pts',(-0.743437111667417,-1.3673502593512,
4.07460461377696));
#286240=CARTESIAN_POINT('Ctrl Pts',(-0.606938331285853,-1.43569481976947,
4.086339297418));
#286241=CARTESIAN_POINT('Ctrl Pts',(-0.513348007765128,-1.471756596708,
4.09418535212595));
#286242=CARTESIAN_POINT('Ctrl Pts',(-0.385807390659938,-1.50724164016124,
4.10425171739215));
#286243=CARTESIAN_POINT('Ctrl Pts',(-0.354406796487647,-1.51493263491683,
4.10668027535148));
#286244=CARTESIAN_POINT('Ctrl Pts',(-0.313310687500327,-1.5236503866108,
4.1097760943613));
#286245=CARTESIAN_POINT('Ctrl Pts',(-0.303815677927547,-1.52557206783121,
4.11048568510528));
#286246=CARTESIAN_POINT('Ctrl Pts',(-0.288451463368745,-1.52853247109323,
4.11162408486959));
#286247=CARTESIAN_POINT('Ctrl Pts',(-0.282593345493416,-1.52962634856159,
4.11205584242167));
#286248=CARTESIAN_POINT('Ctrl Pts',(-0.271122003646222,-1.53170022346064,
4.11289663437999));
#286249=CARTESIAN_POINT('Ctrl Pts',(-0.265509466965103,-1.53268308531037,
4.11330580794468));
#286250=CARTESIAN_POINT('Ctrl Pts',(-0.251551126431596,-1.53504848181344,
4.11431824254814));
#286251=CARTESIAN_POINT('Ctrl Pts',(-0.24319903622933,-1.5363938453776,
4.11491945637877));
#286252=CARTESIAN_POINT('Ctrl Pts',(-0.21108226003102,-1.54129878239369,
4.1172152163504));
#286253=CARTESIAN_POINT('Ctrl Pts',(-0.18724582537996,-1.54437586755347,
4.11888526746431));
#286254=CARTESIAN_POINT('Ctrl Pts',(-0.123523976250556,-1.55110462430929,
4.12328307603711));
#286255=CARTESIAN_POINT('Ctrl Pts',(-0.0835514152619075,-1.55377068897858,
4.12597268762222));
#286256=CARTESIAN_POINT('Ctrl Pts',(0.0867945690688311,-1.55853828223923,
4.13730572784092));
#286257=CARTESIAN_POINT('Ctrl Pts',(0.217040533817466,-1.54579031712021,
4.1456981263094));
#286258=CARTESIAN_POINT('Ctrl Pts',(0.372688360659897,-1.51047633387656,
4.15660861019962));
#286259=CARTESIAN_POINT('Ctrl Pts',(0.401016193033821,-1.50320364404451,
4.1586288487825));
#286260=CARTESIAN_POINT('Ctrl Pts',(0.44066172065978,-1.49182494396618,
4.16151431790095));
#286261=CARTESIAN_POINT('Ctrl Pts',(0.452163641438075,-1.48837913268049,
4.16235842387365));
#286262=CARTESIAN_POINT('Ctrl Pts',(0.473135331305632,-1.4818307895587,
4.16391094319124));
#286263=CARTESIAN_POINT('Ctrl Pts',(0.482617461309397,-1.47876972793605,
4.16461797554794));
#286264=CARTESIAN_POINT('Ctrl Pts',(0.501821237273909,-1.47236590919811,
4.16606058684343));
#286265=CARTESIAN_POINT('Ctrl Pts',(0.511540444756746,-1.46901745692718,
4.16679632310891));
#286266=CARTESIAN_POINT('Ctrl Pts',(0.535686612504368,-1.46042996291988,
4.16863860241251));
#286267=CARTESIAN_POINT('Ctrl Pts',(0.550070273671818,-1.45507336105971,
4.16974899183166));
#286268=CARTESIAN_POINT('Ctrl Pts',(0.607420527841876,-1.43274375911232,
4.17423007916018));
#286269=CARTESIAN_POINT('Ctrl Pts',(0.649696643971826,-1.4140749054633,
4.17765648196432));
#286270=CARTESIAN_POINT('Ctrl Pts',(0.765968103723009,-1.35641488122914,
4.18743699152699));
#286271=CARTESIAN_POINT('Ctrl Pts',(0.837737361423566,-1.31330187714632,
4.19390679510054));
#286272=CARTESIAN_POINT('Ctrl Pts',(0.968460980688698,-1.21968235243341,
4.20637475262519));
#286273=CARTESIAN_POINT('Ctrl Pts',(1.02780604910925,-1.17011060104426,
4.21235210903685));
#286274=CARTESIAN_POINT('Ctrl Pts',(1.09307680214227,-1.10677534448577,
4.21912667166947));
#286275=CARTESIAN_POINT('Ctrl Pts',(1.10279858796273,-1.09708881425005,
4.22014128701344));
#286276=CARTESIAN_POINT('Ctrl Pts',(1.1172146170892,-1.08233976404249,4.22165260112901));
#286277=CARTESIAN_POINT('Ctrl Pts',(1.12200513677592,-1.07737288961849,
4.2221559742804));
#286278=CARTESIAN_POINT('Ctrl Pts',(1.13061904688261,-1.06832210152479,
4.22306293666984));
#286279=CARTESIAN_POINT('Ctrl Pts',(1.13445375662044,-1.06424913435824,
4.22346736411819));
#286280=CARTESIAN_POINT('Ctrl Pts',(1.14237104355563,-1.05574851009407,
4.22430361062023));
#286281=CARTESIAN_POINT('Ctrl Pts',(1.14645000402595,-1.05131770140907,
4.22473516563412));
#286282=CARTESIAN_POINT('Ctrl Pts',(1.1572166626495,-1.03948513793583,4.22587658019079));
#286283=CARTESIAN_POINT('Ctrl Pts',(1.16385920863137,-1.03204239861211,
4.22658317181343));
#286284=CARTESIAN_POINT('Ctrl Pts',(1.19636563296458,-0.994907060185455,
4.23005604184625));
#286285=CARTESIAN_POINT('Ctrl Pts',(1.22116957323579,-0.964300927551207,
4.23275401298611));
#286286=CARTESIAN_POINT('Ctrl Pts',(1.30195294417028,-0.856496563878149,
4.24184214171614));
#286287=CARTESIAN_POINT('Ctrl Pts',(1.35198784658911,-0.775112208608297,
4.24802346935023));
#286288=CARTESIAN_POINT('Ctrl Pts',(1.42777754541445,-0.621889939401246,
4.25934114650452));
#286289=CARTESIAN_POINT('Ctrl Pts',(1.45630764139306,-0.551780416484015,
4.26441171813131));
#286290=CARTESIAN_POINT('Ctrl Pts',(1.48519418118801,-0.462713944126869,
4.27090767291552));
#286291=CARTESIAN_POINT('Ctrl Pts',(1.49046244341471,-0.445452138387839,
4.27216870564984));
#286292=CARTESIAN_POINT('Ctrl Pts',(1.4984145121989,-0.417674362722119,
4.27420332569781));
#286293=CARTESIAN_POINT('Ctrl Pts',(1.50129077436602,-0.407214837291524,
4.27497064562625));
#286294=CARTESIAN_POINT('Ctrl Pts',(1.50656243274258,-0.38722907859397,
4.27643953320159));
#286295=CARTESIAN_POINT('Ctrl Pts',(1.50897746215083,-0.377708530013534,
4.27714042670784));
#286296=CARTESIAN_POINT('Ctrl Pts',(1.5143165043891,-0.355792038500418,
4.27875689460406));
#286297=CARTESIAN_POINT('Ctrl Pts',(1.51717872458511,-0.343381930037367,
4.27967440354252));
#286298=CARTESIAN_POINT('Ctrl Pts',(1.52576696915168,-0.303939028265735,
4.28259821991962));
#286299=CARTESIAN_POINT('Ctrl Pts',(1.53092493928949,-0.276789499428705,
4.28462228312947));
#286300=CARTESIAN_POINT('Ctrl Pts',(1.54846620686007,-0.168853212719599,
4.29271972697537));
#286301=CARTESIAN_POINT('Ctrl Pts',(1.55519629308363,-0.0872919911474576,
4.29895896746634));
#286302=CARTESIAN_POINT('Ctrl Pts',(1.55586346478858,0.098326730918669,
4.31331337322562));
#286303=CARTESIAN_POINT('Ctrl Pts',(1.54582262077034,0.202026372092642,
4.32144838887056));
#286304=CARTESIAN_POINT('Ctrl Pts',(1.52252841199517,0.318937057322911,
4.330329074781));
#286305=CARTESIAN_POINT('Ctrl Pts',(1.51932265387485,0.333874724630308,
4.33145775846546));
#286306=CARTESIAN_POINT('Ctrl Pts',(1.51430454115261,0.355685905525536,
4.3330946850782));
#286307=CARTESIAN_POINT('Ctrl Pts',(1.51266444930041,0.362597539780806,
4.33361175561433));
#286308=CARTESIAN_POINT('Ctrl Pts',(1.50967078006561,0.374839465202833,
4.33452437947045));
#286309=CARTESIAN_POINT('Ctrl Pts',(1.50833621821043,0.380174098199845,
4.33492096549748));
#286310=CARTESIAN_POINT('Ctrl Pts',(1.50533208384289,0.391917623420193,
4.33579154021094));
#286311=CARTESIAN_POINT('Ctrl Pts',(1.50364984899622,0.398323037392287,
4.3362648051862));
#286312=CARTESIAN_POINT('Ctrl Pts',(1.49859695868434,0.417074556115698,
4.3376461494757));
#286313=CARTESIAN_POINT('Ctrl Pts',(1.49511469013908,0.42939040640479,4.33854815762039));
#286314=CARTESIAN_POINT('Ctrl Pts',(1.46968026487253,0.515281698378234,
4.34481117080252));
#286315=CARTESIAN_POINT('Ctrl Pts',(1.44245579916602,0.587196603964978,
4.3499152653411));
#286316=CARTESIAN_POINT('Ctrl Pts',(1.35815914445827,0.768161681067344,
4.36308715390869));
#286317=CARTESIAN_POINT('Ctrl Pts',(1.29329237660476,0.872960396127775,
4.37108256010794));
#286318=CARTESIAN_POINT('Ctrl Pts',(1.20483247410068,0.984035915579096,
4.38088829476144));
#286319=CARTESIAN_POINT('Ctrl Pts',(1.19261036136383,0.998813518399144,
4.38222240886461));
#286320=CARTESIAN_POINT('Ctrl Pts',(1.17217969383585,1.02260623851326,4.38442215672389));
#286321=CARTESIAN_POINT('Ctrl Pts',(1.16413258591279,1.03175775308362,4.38528123277082));
#286322=CARTESIAN_POINT('Ctrl Pts',(1.14944449943468,1.04807106811368,4.38683684102738));
#286323=CARTESIAN_POINT('Ctrl Pts',(1.14284195322776,1.05526673551619,4.3875317380446));
#286324=CARTESIAN_POINT('Ctrl Pts',(1.12853796545918,1.07056398665135,4.3890282227934));
#286325=CARTESIAN_POINT('Ctrl Pts',(1.12081611614997,1.0786456372188,4.38983066314579));
#286326=CARTESIAN_POINT('Ctrl Pts',(1.09931235063688,1.10067114118755,4.3920510435793));
#286327=CARTESIAN_POINT('Ctrl Pts',(1.08535330708724,1.11443830647471,4.39347666956744));
#286328=CARTESIAN_POINT('Ctrl Pts',(1.05358204312197,1.14460967918957,4.39668845242944));
#286329=CARTESIAN_POINT('Ctrl Pts',(1.03563977848757,1.16086888616069,4.39848016864262));
#286330=CARTESIAN_POINT('Ctrl Pts',(0.976023545371014,1.21241053459215,
4.40436428628152));
#286331=CARTESIAN_POINT('Ctrl Pts',(0.93287347035545,1.2459162415818,4.40851899233695));
#286332=CARTESIAN_POINT('Ctrl Pts',(0.788461193608527,1.34633746460596,
4.42205685030198));
#286333=CARTESIAN_POINT('Ctrl Pts',(0.68110640947927,1.40370646831769,4.43161176280327));
#286334=CARTESIAN_POINT('Ctrl Pts',(0.554857044827869,1.45324413927628,
4.44169873445635));
#286335=CARTESIAN_POINT('Ctrl Pts',(0.541468875106046,1.45828541939911,
4.44275428887964));
#286336=CARTESIAN_POINT('Ctrl Pts',(0.521502921761343,1.46549064989815,
4.44430568706108));
#286337=CARTESIAN_POINT('Ctrl Pts',(0.514977623360456,1.46779637371578,
4.44480914414829));
#286338=CARTESIAN_POINT('Ctrl Pts',(0.503247241294266,1.47185346396776,
4.4457075351346));
#286339=CARTESIAN_POINT('Ctrl Pts',(0.498048062421503,1.47362089275558,
4.44610336832191));
#286340=CARTESIAN_POINT('Ctrl Pts',(0.486409431881543,1.47750873836931,
4.44698422546984));
#286341=CARTESIAN_POINT('Ctrl Pts',(0.479965373711866,1.47961462956449,
4.44746840846465));
#286342=CARTESIAN_POINT('Ctrl Pts',(0.460572748866469,1.48581203060468,
4.44891551400076));
#286343=CARTESIAN_POINT('Ctrl Pts',(0.447583751237351,1.48977631402793,
4.44987145998965));
#286344=CARTESIAN_POINT('Ctrl Pts',(0.417114737421031,1.49864106330821,
4.45208657303177));
#286345=CARTESIAN_POINT('Ctrl Pts',(0.399597260356206,1.50340674288423,
4.45333931247084));
#286346=CARTESIAN_POINT('Ctrl Pts',(0.336223622955492,1.51946169591212,
4.45781029859209));
#286347=CARTESIAN_POINT('Ctrl Pts',(0.289939783824997,1.52896885616167,
4.4609617607184));
#286348=CARTESIAN_POINT('Ctrl Pts',(0.130450489089249,1.5542250205593,4.47164957218641));
#286349=CARTESIAN_POINT('Ctrl Pts',(0.015991750870176,1.55960751440904,
4.47905534009747));
#286350=CARTESIAN_POINT('Ctrl Pts',(-0.130992605140568,1.55032659356239,
4.48908360602945));
#286351=CARTESIAN_POINT('Ctrl Pts',(-0.163885808665665,1.5471951356909,
4.4913590915998));
#286352=CARTESIAN_POINT('Ctrl Pts',(-0.210532257092109,1.54125020519325,
4.49464430575546));
#286353=CARTESIAN_POINT('Ctrl Pts',(-0.224387083733287,1.53929413707484,
4.49562741106794));
#286354=CARTESIAN_POINT('Ctrl Pts',(-0.248014680780174,1.53563255479586,
4.49731747701489));
#286355=CARTESIAN_POINT('Ctrl Pts',(-0.257801149013188,1.53401994267171,
4.49802147490781));
#286356=CARTESIAN_POINT('Ctrl Pts',(-0.277762879412105,1.53053424259463,
4.49946591602658));
#286357=CARTESIAN_POINT('Ctrl Pts',(-0.287936193238695,1.52865300967978,
4.50020658472581));
#286358=CARTESIAN_POINT('Ctrl Pts',(-0.313469873230396,1.52366743572125,
4.50207734904723));
#286359=CARTESIAN_POINT('Ctrl Pts',(-0.328803182672927,1.52043225754525,
4.5032115476481));
#286360=CARTESIAN_POINT('Ctrl Pts',(-0.392093831705592,1.50607641205929,
4.5079395589005));
#286361=CARTESIAN_POINT('Ctrl Pts',(-0.439553805427336,1.49291500489612,
4.51159724810286));
#286362=CARTESIAN_POINT('Ctrl Pts',(-0.565851344477908,1.45134609599004,
4.52164103805286));
#286363=CARTESIAN_POINT('Ctrl Pts',(-0.643145931642067,1.41878608896666,
4.52813243896421));
#286364=CARTESIAN_POINT('Ctrl Pts',(-0.782514091629438,1.34634000438426,
4.54030951863989));
#286365=CARTESIAN_POINT('Ctrl Pts',(-0.845124405740421,1.30794748917469,
4.54597778303221));
#286366=CARTESIAN_POINT('Ctrl Pts',(-0.91595310478424,1.25729800457961,
4.55246374315616));
#286367=CARTESIAN_POINT('Ctrl Pts',(-0.927004001535046,1.24917251690668,
4.55347781972311));
#286368=CARTESIAN_POINT('Ctrl Pts',(-0.943449858177091,1.23674177033131,
4.55498847274661));
#286369=CARTESIAN_POINT('Ctrl Pts',(-0.948925667629875,1.23254530280128,
4.55549171582995));
#286370=CARTESIAN_POINT('Ctrl Pts',(-0.958790440415365,1.2248805771586,
4.55639851608721));
#286371=CARTESIAN_POINT('Ctrl Pts',(-0.963188954090369,1.22142481543671,
4.55680291048711));
#286372=CARTESIAN_POINT('Ctrl Pts',(-0.972177367732558,1.21428417488792,
4.55762929282815));
#286373=CARTESIAN_POINT('Ctrl Pts',(-0.976765131178521,1.21059686655703,
4.55805110505833));
#286374=CARTESIAN_POINT('Ctrl Pts',(-0.988254807495022,1.20125446829591,
4.55910787151927));
#286375=CARTESIAN_POINT('Ctrl Pts',(-0.995129312439812,1.19556577551092,
4.5597404979481));
#286376=CARTESIAN_POINT('Ctrl Pts',(-1.01055285188049,1.18257749752043,
4.56116163803271));
#286377=CARTESIAN_POINT('Ctrl Pts',(-1.01907256729912,1.17524368717213,
4.5619479184038));
#286378=CARTESIAN_POINT('Ctrl Pts',(-1.04456400227764,1.15281487924561,
4.56430706176713));
#286379=CARTESIAN_POINT('Ctrl Pts',(-1.06128600675228,1.1374393293851,4.56586357498902));
#286380=CARTESIAN_POINT('Ctrl Pts',(-1.12781625365688,1.07352094294783,
4.57212286691856));
#286381=CARTESIAN_POINT('Ctrl Pts',(-1.17468248355205,1.02202701168424,
4.57669151303501));
#286382=CARTESIAN_POINT('Ctrl Pts',(-1.27994257098291,0.889528242054865,
4.58782939772139));
#286383=CARTESIAN_POINT('Ctrl Pts',(-1.33428664738122,0.805722903756993,
4.59439430221794));
#286384=CARTESIAN_POINT('Ctrl Pts',(-1.38971605353195,0.699065029421539,
4.60267843433187));
#286385=CARTESIAN_POINT('Ctrl Pts',(-1.39883052236613,0.680643612435232,
4.60410603977543));
#286386=CARTESIAN_POINT('Ctrl Pts',(-1.41293361117383,0.650659092704301,
4.60642801993813));
#286387=CARTESIAN_POINT('Ctrl Pts',(-1.41815165344996,0.639206160628075,
4.60731451849287));
#286388=CARTESIAN_POINT('Ctrl Pts',(-1.4271863137001,0.618720937621211,
4.60890011559736));
#286389=CARTESIAN_POINT('Ctrl Pts',(-1.43105762849586,0.609713398697462,
4.60959730430087));
#286390=CARTESIAN_POINT('Ctrl Pts',(-1.43906345737749,0.590589569964072,
4.6110777975717));
#286391=CARTESIAN_POINT('Ctrl Pts',(-1.44317700958168,0.580465143000246,
4.61186176678974));
#286392=CARTESIAN_POINT('Ctrl Pts',(-1.45393870893787,0.553156365958523,
4.61397731623647));
#286393=CARTESIAN_POINT('Ctrl Pts',(-1.4603885804072,0.53589632822872,4.6153154177468));
#286394=CARTESIAN_POINT('Ctrl Pts',(-1.50010621636561,0.423564340365713,
4.62403424400703));
#286395=CARTESIAN_POINT('Ctrl Pts',(-1.52437313714131,0.325583720036536,
4.63170932982582));
#286396=CARTESIAN_POINT('Ctrl Pts',(-1.55002255233211,0.150890432230857,
4.64537475581589));
#286397=CARTESIAN_POINT('Ctrl Pts',(-1.55553734988942,0.0751104264812811,
4.65128965469626));
#286398=CARTESIAN_POINT('Ctrl Pts',(-1.55549980963818,-0.00076955545019349,
4.65706464148559));
#286399=CARTESIAN_POINT('',(-1.55596383579478,0.00138071545366179,5.3559437743963));
#286400=CARTESIAN_POINT('Ctrl Pts',(-1.55745492001379,-0.000856371120316864,
4.65594377439631));
#286401=CARTESIAN_POINT('Ctrl Pts',(-1.5577850741697,-0.0506891626144068,
4.65952562306032));
#286402=CARTESIAN_POINT('Ctrl Pts',(-1.53301192978291,-0.615473136307116,
4.70014468855281));
#286403=CARTESIAN_POINT('Ctrl Pts',(-0.844041411881997,-1.63316067010957,
4.77780097087378));
#286404=CARTESIAN_POINT('Ctrl Pts',(0.913973507436636,-1.59507746114991,
4.88891262135923));
#286405=CARTESIAN_POINT('Ctrl Pts',(1.83577980123458,-0.0976329900371924,
5.00002427184466));
#286406=CARTESIAN_POINT('Ctrl Pts',(1.0780025055099,1.48913742733129,5.1111359223301));
#286407=CARTESIAN_POINT('Ctrl Pts',(-0.666056105926533,1.7134727727987,
5.22224757281553));
#286408=CARTESIAN_POINT('Ctrl Pts',(-1.49938299705611,0.726891414718789,
5.30385019017093));
#286409=CARTESIAN_POINT('Ctrl Pts',(-1.55693038683329,0.106378444150779,
5.34841559069786));
#286410=CARTESIAN_POINT('Ctrl Pts',(-1.55596383579478,0.00138071545366179,
5.3559437743963));
#286411=CARTESIAN_POINT('',(-1.5554995157997,-0.00134118142063625,6.75626796741665));
#286412=CARTESIAN_POINT('Ctrl Pts',(-1.55549937213162,0.0013976044270106,
5.35621070370163));
#286413=CARTESIAN_POINT('Ctrl Pts',(-1.55558531673232,-0.0942566235089736,
5.3625138632035));
#286414=CARTESIAN_POINT('Ctrl Pts',(-1.54684820960077,-0.189710805692918,
5.36876803926013));
#286415=CARTESIAN_POINT('Ctrl Pts',(-1.52501392228005,-0.307393315677365,
5.37690504084912));
#286416=CARTESIAN_POINT('Ctrl Pts',(-1.5200816041754,-0.330922850003075,
5.37855285049613));
#286417=CARTESIAN_POINT('Ctrl Pts',(-1.5113927892051,-0.368063987588195,
5.38119346912254));
#286418=CARTESIAN_POINT('Ctrl Pts',(-1.50799268936484,-0.381755535595127,
5.38217551296266));
#286419=CARTESIAN_POINT('Ctrl Pts',(-1.50113613180991,-0.407843269366331,
5.38406447062459));
#286420=CARTESIAN_POINT('Ctrl Pts',(-1.49771113072265,-0.420246558421885,
5.3849703301972));
#286421=CARTESIAN_POINT('Ctrl Pts',(-1.491396389121,-0.442056405599685,
5.3865776675289));
#286422=CARTESIAN_POINT('Ctrl Pts',(-1.48857049217765,-0.45148082674486,
5.38727704048428));
#286423=CARTESIAN_POINT('Ctrl Pts',(-1.48246071469624,-0.471175912638168,
5.38874902987812));
#286424=CARTESIAN_POINT('Ctrl Pts',(-1.47915907633452,-0.481440471221005,
5.38952219552156));
#286425=CARTESIAN_POINT('Ctrl Pts',(-1.47014353531056,-0.508500702703793,
5.39157685581394));
#286426=CARTESIAN_POINT('Ctrl Pts',(-1.46424869983214,-0.525233924775626,
5.39286423208727));
#286427=CARTESIAN_POINT('Ctrl Pts',(-1.43385982406354,-0.607005814791225,
5.39924124640113));
#286428=CARTESIAN_POINT('Ctrl Pts',(-1.40531565354724,-0.670444175584406,
5.40446337431976));
#286429=CARTESIAN_POINT('Ctrl Pts',(-1.32600998858741,-0.819206405149396,
5.41736928707314));
#286430=CARTESIAN_POINT('Ctrl Pts',(-1.27114121913679,-0.901997980377709,
5.42513387974268));
#286431=CARTESIAN_POINT('Ctrl Pts',(-1.18266814132577,-1.01123511881884,
5.43589568734301));
#286432=CARTESIAN_POINT('Ctrl Pts',(-1.15528336216924,-1.04241135930595,
5.43903275673746));
#286433=CARTESIAN_POINT('Ctrl Pts',(-1.11981458544122,-1.0796734544794,
5.44283018234965));
#286434=CARTESIAN_POINT('Ctrl Pts',(-1.11287737747529,-1.08682263064699,
5.44356105654601));
#286435=CARTESIAN_POINT('Ctrl Pts',(-1.10218029217275,-1.09763673717239,
5.44466946420265));
#286436=CARTESIAN_POINT('Ctrl Pts',(-1.09846991186274,-1.10134992538673,
5.44505057771528));
#286437=CARTESIAN_POINT('Ctrl Pts',(-1.09083577014417,-1.1089128852218,
5.44582776885242));
#286438=CARTESIAN_POINT('Ctrl Pts',(-1.08691040384544,-1.11276063934723,
5.44622365859345));
#286439=CARTESIAN_POINT('Ctrl Pts',(-1.07789402754417,-1.12150551048198,
5.44712459352676));
#286440=CARTESIAN_POINT('Ctrl Pts',(-1.07278996803996,-1.12638884684528,
5.44762859065801));
#286441=CARTESIAN_POINT('Ctrl Pts',(-1.05669881880009,-1.14157554345909,
5.44919948917127));
#286442=CARTESIAN_POINT('Ctrl Pts',(-1.04559483499751,-1.15175457463726,
5.45025754140244));
#286443=CARTESIAN_POINT('Ctrl Pts',(-0.972198027713824,-1.21710097263523,
5.45709802230677));
#286444=CARTESIAN_POINT('Ctrl Pts',(-0.905703620700305,-1.26736280163341,
5.4625923547523));
#286445=CARTESIAN_POINT('Ctrl Pts',(-0.768516086060986,-1.35472109603187,
5.47330367461397));
#286446=CARTESIAN_POINT('Ctrl Pts',(-0.698369563857121,-1.39218001083551,
5.47850761995188));
#286447=CARTESIAN_POINT('Ctrl Pts',(-0.584559364932492,-1.44218137832236,
5.4868888329545));
#286448=CARTESIAN_POINT('Ctrl Pts',(-0.542687119889451,-1.45845358293211,
5.48995862669651));
#286449=CARTESIAN_POINT('Ctrl Pts',(-0.485776403117846,-1.47777964827052,
5.49414794795821));
#286450=CARTESIAN_POINT('Ctrl Pts',(-0.471309695152091,-1.4824569286404,
5.49521421705987));
#286451=CARTESIAN_POINT('Ctrl Pts',(-0.446978573678549,-1.4899313669626,
5.49701100742747));
#286452=CARTESIAN_POINT('Ctrl Pts',(-0.437150661268289,-1.49284447074134,
5.49773770674514));
#286453=CARTESIAN_POINT('Ctrl Pts',(-0.417692586986589,-1.49840344449549,
5.49917868836068));
#286454=CARTESIAN_POINT('Ctrl Pts',(-0.408064305743027,-1.50105412743808,
5.49989277472525));
#286455=CARTESIAN_POINT('Ctrl Pts',(-0.384523034735545,-1.50729184764809,
5.50164164707594));
#286456=CARTESIAN_POINT('Ctrl Pts',(-0.370584826813751,-1.51077911642587,
5.50267959058349));
#286457=CARTESIAN_POINT('Ctrl Pts',(-0.322180536323446,-1.52217949740251,
5.50629381664485));
#286458=CARTESIAN_POINT('Ctrl Pts',(-0.287496681634273,-1.52910954706044,
5.50890077050358));
#286459=CARTESIAN_POINT('Ctrl Pts',(-0.13122929556239,-1.5548283845244,
5.52073050285651));
#286460=CARTESIAN_POINT('Ctrl Pts',(-0.00792084691592195,-1.56033358620807,
5.53033853746785));
#286461=CARTESIAN_POINT('Ctrl Pts',(0.153798402359041,-1.54837387686308,
5.54285171111443));
#286462=CARTESIAN_POINT('Ctrl Pts',(0.1927549427831,-1.54400827494375,5.54585454690231));
#286463=CARTESIAN_POINT('Ctrl Pts',(0.254925886865817,-1.53465106498951,
5.55059198419846));
#286464=CARTESIAN_POINT('Ctrl Pts',(0.278262517331183,-1.53059179008015,
5.5523576010522));
#286465=CARTESIAN_POINT('Ctrl Pts',(0.309753500900875,-1.5243699737273,
5.55471522904924));
#286466=CARTESIAN_POINT('Ctrl Pts',(0.317994975877967,-1.52267207631725,
5.55532990553891));
#286467=CARTESIAN_POINT('Ctrl Pts',(0.331784854154872,-1.51971425722947,
5.55635402879094));
#286468=CARTESIAN_POINT('Ctrl Pts',(0.337340772573969,-1.51849063887314,
5.5567654502225));
#286469=CARTESIAN_POINT('Ctrl Pts',(0.348715976276974,-1.51591988342108,
5.55760517987894));
#286470=CARTESIAN_POINT('Ctrl Pts',(0.354534411427445,-1.51456966806042,
5.55803331265621));
#286471=CARTESIAN_POINT('Ctrl Pts',(0.369829327204941,-1.51092738779717,
5.55915543317448));
#286472=CARTESIAN_POINT('Ctrl Pts',(0.379292476112181,-1.50857964088849,
5.55984634629906));
#286473=CARTESIAN_POINT('Ctrl Pts',(0.420632491226343,-1.49790984510663,
5.56285244064451));
#286474=CARTESIAN_POINT('Ctrl Pts',(0.452264978096047,-1.4886646255289,
5.56512086021581));
#286475=CARTESIAN_POINT('Ctrl Pts',(0.567845195753168,-1.45085902982517,
5.5733730678543));
#286476=CARTESIAN_POINT('Ctrl Pts',(0.64960364070555,-1.41614182337517,
5.57914608903986));
#286477=CARTESIAN_POINT('Ctrl Pts',(0.793697844034987,-1.33983458289773,
5.58990041838939));
#286478=CARTESIAN_POINT('Ctrl Pts',(0.856843679048442,-1.30035770027303,
5.59484465442616));
#286479=CARTESIAN_POINT('Ctrl Pts',(0.938652431895123,-1.24065937744863,
5.60179008700938));
#286480=CARTESIAN_POINT('Ctrl Pts',(0.959968982974912,-1.22423996106562,
5.60365365500379));
#286481=CARTESIAN_POINT('Ctrl Pts',(0.990632091123183,-1.19932782236166,
5.60642200991812));
#286482=CARTESIAN_POINT('Ctrl Pts',(1.00031891218933,-1.19126035053432,
5.6073099289106));
#286483=CARTESIAN_POINT('Ctrl Pts',(1.0173650090175,-1.17670933426509,5.6088971068135));
#286484=CARTESIAN_POINT('Ctrl Pts',(1.02476312004483,-1.17027217290432,
5.60959444161794));
#286485=CARTESIAN_POINT('Ctrl Pts',(1.04026717331089,-1.15652221440282,
5.61107424097318));
#286486=CARTESIAN_POINT('Ctrl Pts',(1.04835795131679,-1.14919320348493,
5.61185736127656));
#286487=CARTESIAN_POINT('Ctrl Pts',(1.06985570951289,-1.12930355197775,
5.61396811839095));
#286488=CARTESIAN_POINT('Ctrl Pts',(1.08311804401966,-1.11658989818164,
5.61530222517486));
#286489=CARTESIAN_POINT('Ctrl Pts',(1.16046536077529,-1.03976773436914,
5.62327898012649));
#286490=CARTESIAN_POINT('Ctrl Pts',(1.21906098424805,-0.970402868061441,
5.6301559091766));
#286491=CARTESIAN_POINT('Ctrl Pts',(1.30899372531837,-0.842852099371245,
5.64220522456008));
#286492=CARTESIAN_POINT('Ctrl Pts',(1.34329585058496,-0.787032700459085,
5.64730472036477));
#286493=CARTESIAN_POINT('Ctrl Pts',(1.39050724397153,-0.698077903848779,
5.65505781487955));
#286494=CARTESIAN_POINT('Ctrl Pts',(1.40597239169172,-0.666382110462548,
5.65775151512342));
#286495=CARTESIAN_POINT('Ctrl Pts',(1.42933346770172,-0.614061740775941,
5.66206068763612));
#286496=CARTESIAN_POINT('Ctrl Pts',(1.43789093100254,-0.593747238334971,
5.66370124748263));
#286497=CARTESIAN_POINT('Ctrl Pts',(1.44903321819478,-0.565641305514525,
5.66592041504713));
#286498=CARTESIAN_POINT('Ctrl Pts',(1.45199203502418,-0.558002233052944,
5.66651851958697));
#286499=CARTESIAN_POINT('Ctrl Pts',(1.45688822315515,-0.545058564772707,
5.667523016475));
#286500=CARTESIAN_POINT('Ctrl Pts',(1.4588572819491,-0.539766216982017,
5.66793122226028));
#286501=CARTESIAN_POINT('Ctrl Pts',(1.46287492950057,-0.528785159327553,
5.66877287389834));
#286502=CARTESIAN_POINT('Ctrl Pts',(1.46491923413133,-0.523095062967969,
5.66920607350375));
#286503=CARTESIAN_POINT('Ctrl Pts',(1.47028443648326,-0.507883459298711,
5.67035675746368));
#286504=CARTESIAN_POINT('Ctrl Pts',(1.47354608337174,-0.498341134917042,
5.67107087943219));
#286505=CARTESIAN_POINT('Ctrl Pts',(1.48822300225059,-0.453997707047249,
5.67435682347362));
#286506=CARTESIAN_POINT('Ctrl Pts',(1.49850070941619,-0.418829025386111,
5.67687044951284));
#286507=CARTESIAN_POINT('Ctrl Pts',(1.52872485273135,-0.299965156299139,
5.685161907478));
#286508=CARTESIAN_POINT('Ctrl Pts',(1.54297212330114,-0.214983277069093,
5.69076351474443));
#286509=CARTESIAN_POINT('Ctrl Pts',(1.55616805129081,-0.056727371821594,
5.70124165488428));
#286510=CARTESIAN_POINT('Ctrl Pts',(1.55711760750708,0.016127356831905,
5.70608323596208));
#286511=CARTESIAN_POINT('Ctrl Pts',(1.55143230707139,0.115580607876705,
5.71291532420794));
#286512=CARTESIAN_POINT('Ctrl Pts',(1.54920637812199,0.142339492025496,
5.71477511687613));
#286513=CARTESIAN_POINT('Ctrl Pts',(1.54492050773076,0.181547617547816,
5.717538925979));
#286514=CARTESIAN_POINT('Ctrl Pts',(1.54339975958793,0.194051740965268,
5.7184261559439));
#286515=CARTESIAN_POINT('Ctrl Pts',(1.54042541914366,0.21625430506051,5.7200125667303));
#286516=CARTESIAN_POINT('Ctrl Pts',(1.53903163929107,0.225960177073611,
5.72070983036372));
#286517=CARTESIAN_POINT('Ctrl Pts',(1.53589154316561,0.246448195176311,
5.72218996484407));
#286518=CARTESIAN_POINT('Ctrl Pts',(1.53412324306125,0.257226377156094,
5.72297349575075));
#286519=CARTESIAN_POINT('Ctrl Pts',(1.5290721040272,0.286106991555049,5.72508657061025));
#286520=CARTESIAN_POINT('Ctrl Pts',(1.52558146109087,0.304170777022648,
5.72642260932998));
#286521=CARTESIAN_POINT('Ctrl Pts',(1.5034801599464,0.408567112708702,5.73423103027641));
#286522=CARTESIAN_POINT('Ctrl Pts',(1.47786753119561,0.493236482940582,
5.74092477707952));
#286523=CARTESIAN_POINT('Ctrl Pts',(1.42078531439761,0.636642508259966,
5.75283336754041));
#286524=CARTESIAN_POINT('Ctrl Pts',(1.39246843390347,0.696402296672161,
5.7579807637065));
#286525=CARTESIAN_POINT('Ctrl Pts',(1.3428273672816,0.785947982165514,5.76586842651184));
#286526=CARTESIAN_POINT('Ctrl Pts',(1.32410800354323,0.817091129403761,
5.76864603584951));
#286527=CARTESIAN_POINT('Ctrl Pts',(1.29593763783856,0.860443043205675,
5.77253633624833));
#286528=CARTESIAN_POINT('Ctrl Pts',(1.28737003745574,0.873209608348753,
5.77368500032928));
#286529=CARTESIAN_POINT('Ctrl Pts',(1.27180601621621,0.895674396455829,
5.77570892759108));
#286530=CARTESIAN_POINT('Ctrl Pts',(1.26488448940693,0.905422784695,5.7765881080773));
#286531=CARTESIAN_POINT('Ctrl Pts',(1.25405753382366,0.920305129523615,
5.77793055892267));
#286532=CARTESIAN_POINT('Ctrl Pts',(1.25023160654899,0.925495955461203,
5.77839884126318));
#286533=CARTESIAN_POINT('Ctrl Pts',(1.24307092910497,0.935085762268642,
5.77926383393281));
#286534=CARTESIAN_POINT('Ctrl Pts',(1.23974500886189,0.939490836605487,
5.7796610865468));
#286535=CARTESIAN_POINT('Ctrl Pts',(1.23201267474367,0.949619497351625,
5.78057443674902));
#286536=CARTESIAN_POINT('Ctrl Pts',(1.22758975599729,0.955330213560184,
5.78108937954889));
#286537=CARTESIAN_POINT('Ctrl Pts',(1.21301351235378,0.973882151080955,
5.78276294149331));
#286538=CARTESIAN_POINT('Ctrl Pts',(1.20269682720201,0.986594457165662,
5.78391083554846));
#286539=CARTESIAN_POINT('Ctrl Pts',(1.11614808355367,1.08986479951813,5.7932679704173));
#286540=CARTESIAN_POINT('Ctrl Pts',(1.02999733747858,1.17162513625742,5.80090448671055));
#286541=CARTESIAN_POINT('Ctrl Pts',(0.891871292510244,1.27558337587649,
5.81232872904528));
#286542=CARTESIAN_POINT('Ctrl Pts',(0.846662041159824,1.30602834453988,
5.81595586007929));
#286543=CARTESIAN_POINT('Ctrl Pts',(0.77921752453907,1.34647123623106,5.82130104505155));
#286544=CARTESIAN_POINT('Ctrl Pts',(0.758197237054425,1.35841878339606,
5.82295798458011));
#286545=CARTESIAN_POINT('Ctrl Pts',(0.719661920385412,1.37914845594972,
5.82598682054461));
#286546=CARTESIAN_POINT('Ctrl Pts',(0.702242964093857,1.38809888082407,
5.82735278810835));
#286547=CARTESIAN_POINT('Ctrl Pts',(0.674627860022165,1.40163559327147,
5.82951610025713));
#286548=CARTESIAN_POINT('Ctrl Pts',(0.664542927173833,1.40644508321132,
5.83030567018541));
#286549=CARTESIAN_POINT('Ctrl Pts',(0.64554730742276,1.41525414854056,5.8317924916393));
#286550=CARTESIAN_POINT('Ctrl Pts',(0.636649015966238,1.41927927257646,
5.83248882043665));
#286551=CARTESIAN_POINT('Ctrl Pts',(0.616557656453333,1.42814059917551,
5.83406102660246));
#286552=CARTESIAN_POINT('Ctrl Pts',(0.605344556061724,1.43292947051775,
5.83493846667957));
#286553=CARTESIAN_POINT('Ctrl Pts',(0.576333307597518,1.44491825256296,
5.8372091670389));
#286554=CARTESIAN_POINT('Ctrl Pts',(0.558456550749057,1.45192116106146,
5.838608903285));
#286555=CARTESIAN_POINT('Ctrl Pts',(0.407609661955568,1.50781484236892,
5.85042914943818));
#286556=CARTESIAN_POINT('Ctrl Pts',(0.26868330361232,1.53864988422778,5.86146444892349));
#286557=CARTESIAN_POINT('Ctrl Pts',(0.0863364101492555,1.55365253157216,
5.87559775140957));
#286558=CARTESIAN_POINT('Ctrl Pts',(0.0450028621525554,1.5553987795473,
5.87877149858463));
#286559=CARTESIAN_POINT('Ctrl Pts',(-0.0209021069935472,1.55555327188271,
5.88374242399738));
#286560=CARTESIAN_POINT('Ctrl Pts',(-0.045450296293988,1.55502968586492,
5.88557408704744));
#286561=CARTESIAN_POINT('Ctrl Pts',(-0.0784947149493644,1.55354160546452,
5.88800432310237));
#286562=CARTESIAN_POINT('Ctrl Pts',(-0.0870089019708607,1.55308802070189,
5.88862732159931));
#286563=CARTESIAN_POINT('Ctrl Pts',(-0.101219370355704,1.55221374306362,
5.88966136026361));
#286564=CARTESIAN_POINT('Ctrl Pts',(-0.106917745895264,1.55183164830491,
5.89007445664075));
#286565=CARTESIAN_POINT('Ctrl Pts',(-0.118538214655707,1.55098814375979,
5.89091353501011));
#286566=CARTESIAN_POINT('Ctrl Pts',(-0.124459981987208,1.55052418442428,
5.89133937497956));
#286567=CARTESIAN_POINT('Ctrl Pts',(-0.139943306781881,1.54922181837421,
5.89244855361125));
#286568=CARTESIAN_POINT('Ctrl Pts',(-0.14950020318254,1.54832880009703,
5.89312894484608));
#286569=CARTESIAN_POINT('Ctrl Pts',(-0.190333666649957,1.54413161534271,
5.89602028030618));
#286570=CARTESIAN_POINT('Ctrl Pts',(-0.22151677520207,1.5399675336043,5.89818875342736));
#286571=CARTESIAN_POINT('Ctrl Pts',(-0.341118895516244,1.52028751652238,
5.90642758635648));
#286572=CARTESIAN_POINT('Ctrl Pts',(-0.428262739292278,1.4980754079734,
5.91227207783509));
#286573=CARTESIAN_POINT('Ctrl Pts',(-0.583852471675827,1.44372008845948,
5.92314084936476));
#286574=CARTESIAN_POINT('Ctrl Pts',(-0.652803918329675,1.41388000833656,
5.92812719440873));
#286575=CARTESIAN_POINT('Ctrl Pts',(-0.743204149788014,1.36673075384221,
5.93511923856452));
#286576=CARTESIAN_POINT('Ctrl Pts',(-0.766751060834749,1.35366097080675,
5.93698441954035));
#286577=CARTESIAN_POINT('Ctrl Pts',(-0.800809040487302,1.33358320104073,
5.93975471640259));
#286578=CARTESIAN_POINT('Ctrl Pts',(-0.811593754188938,1.32704741247412,
5.94064292950013));
#286579=CARTESIAN_POINT('Ctrl Pts',(-0.83062223454267,1.3151969936329,5.94223043501111));
#286580=CARTESIAN_POINT('Ctrl Pts',(-0.838897539471974,1.30993409712202,
5.94292780036533));
#286581=CARTESIAN_POINT('Ctrl Pts',(-0.856276182275182,1.29864948023584,
5.94440745751945));
#286582=CARTESIAN_POINT('Ctrl Pts',(-0.865366974146432,1.29260951631273,
5.94519040323862));
#286583=CARTESIAN_POINT('Ctrl Pts',(-0.889577974643689,1.27615374142328,
5.94730017499007));
#286584=CARTESIAN_POINT('Ctrl Pts',(-0.904578155033677,1.26556534899134,
5.94863346046612));
#286585=CARTESIAN_POINT('Ctrl Pts',(-0.995295577312708,1.19909252703306,
5.95686249562552));
#286586=CARTESIAN_POINT('Ctrl Pts',(-1.06598621673972,1.1367073447424,5.96401237613621));
#286587=CARTESIAN_POINT('Ctrl Pts',(-1.18009144516023,1.01595161050615,
5.97685118783924));
#286588=CARTESIAN_POINT('Ctrl Pts',(-1.2258862259353,0.960196185592179,
5.98247047858549));
#286589=CARTESIAN_POINT('Ctrl Pts',(-1.28446663821339,0.877819813031491,
5.99021451888064));
#286590=CARTESIAN_POINT('Ctrl Pts',(-1.30061847700068,0.853706012913974,
5.99241941237853));
#286591=CARTESIAN_POINT('Ctrl Pts',(-1.32633260302091,0.812890831728273,
5.99603418944769));
#286592=CARTESIAN_POINT('Ctrl Pts',(-1.33627635010345,0.796439126779588,
5.99746081153981));
#286593=CARTESIAN_POINT('Ctrl Pts',(-1.34981064983257,0.773079492025513,
5.99943988121767));
#286594=CARTESIAN_POINT('Ctrl Pts',(-1.3536577553296,0.766323286649535,
6.00000691104201));
#286595=CARTESIAN_POINT('Ctrl Pts',(-1.3601766443748,0.754672665979396,
6.00097517289035));
#286596=CARTESIAN_POINT('Ctrl Pts',(-1.36287302262578,0.749792281335528,
6.00137791891593));
#286597=CARTESIAN_POINT('Ctrl Pts',(-1.36851951928948,0.739441142460499,
6.00222599980405));
#286598=CARTESIAN_POINT('Ctrl Pts',(-1.37146316051516,0.733967084274369,
6.00267093668019));
#286599=CARTESIAN_POINT('Ctrl Pts',(-1.37946041295764,0.71887911336415,
6.00388796944352));
#286600=CARTESIAN_POINT('Ctrl Pts',(-1.38444638839404,0.709229459137353,
6.00465599552949));
#286601=CARTESIAN_POINT('Ctrl Pts',(-1.41102523810121,0.65644126384849,
6.00880589471036));
#286602=CARTESIAN_POINT('Ctrl Pts',(-1.43070583210502,0.612363637095453,
6.01208537771746));
#286603=CARTESIAN_POINT('Ctrl Pts',(-1.48216328983869,0.481025496373257,
6.0215280720004));
#286604=CARTESIAN_POINT('Ctrl Pts',(-1.5082185515259,0.391754536142064,
6.02754730405343));
#286605=CARTESIAN_POINT('Ctrl Pts',(-1.53504658811036,0.255588328982511,
6.03676405215725));
#286606=CARTESIAN_POINT('Ctrl Pts',(-1.54192852476428,0.210117463223652,
6.03984552260478));
#286607=CARTESIAN_POINT('Ctrl Pts',(-1.5501299691439,0.132957920080517,
6.04513988470019));
#286608=CARTESIAN_POINT('Ctrl Pts',(-1.55251282870585,0.10141209130756,
6.04732246046617));
#286609=CARTESIAN_POINT('Ctrl Pts',(-1.55453412009693,0.056423960080094,
6.05047241574247));
#286610=CARTESIAN_POINT('Ctrl Pts',(-1.55496267751271,0.0430237781187197,
6.05141533463132));
#286611=CARTESIAN_POINT('Ctrl Pts',(-1.55540682487816,0.0197035962003662,
6.05306524379105));
#286612=CARTESIAN_POINT('Ctrl Pts',(-1.55550083692798,0.00978573443703066,
6.05376975090866));
#286613=CARTESIAN_POINT('Ctrl Pts',(-1.55549909763968,-0.0106881064554486,
6.05523024010196));
#286614=CARTESIAN_POINT('Ctrl Pts',(-1.55539074839895,-0.0212435405207699,
6.05598657912256));
#286615=CARTESIAN_POINT('Ctrl Pts',(-1.55483411414781,-0.0484683925111042,
6.05794646875803));
#286616=CARTESIAN_POINT('Ctrl Pts',(-1.55422520519461,-0.0651327792238609,
6.05915495677717));
#286617=CARTESIAN_POINT('Ctrl Pts',(-1.55016624014936,-0.142226349352791,
6.06478876843065));
#286618=CARTESIAN_POINT('Ctrl Pts',(-1.54345929040669,-0.202423744467183,
6.06931341446638));
#286619=CARTESIAN_POINT('Ctrl Pts',(-1.52176676867994,-0.329337445247056,
6.07911553554798));
#286620=CARTESIAN_POINT('Ctrl Pts',(-1.50585582606494,-0.395770526459621,
6.08440585842539));
#286621=CARTESIAN_POINT('Ctrl Pts',(-1.48108355806372,-0.475613061167336,
6.09088764160246));
#286622=CARTESIAN_POINT('Ctrl Pts',(-1.47631370872973,-0.490218450630519,
6.09207832059499));
#286623=CARTESIAN_POINT('Ctrl Pts',(-1.44986360236758,-0.567319435010784,
6.09838467393077));
#286624=CARTESIAN_POINT('Ctrl Pts',(-1.42442700875866,-0.628462864214943,
6.1034618624759));
#286625=CARTESIAN_POINT('Ctrl Pts',(-1.39017211730538,-0.697946658725506,
6.10919291824926));
#286626=CARTESIAN_POINT('Ctrl Pts',(-1.3850626921306,-0.708032070463512,
6.11002369241933));
#286627=CARTESIAN_POINT('Ctrl Pts',(-1.37689970307731,-0.723718264022471,
6.11131312762399));
#286628=CARTESIAN_POINT('Ctrl Pts',(-1.37392100609101,-0.729357245068671,
6.11177611064862));
#286629=CARTESIAN_POINT('Ctrl Pts',(-1.36855596925432,-0.739364308122387,
6.11259653487212));
#286630=CARTESIAN_POINT('Ctrl Pts',(-1.36618331313805,-0.743739320669714,
6.11295478783968));
#286631=CARTESIAN_POINT('Ctrl Pts',(-1.36036212388585,-0.754351330746923,
6.11382281394205));
#286632=CARTESIAN_POINT('Ctrl Pts',(-1.35689166803833,-0.760576126899796,
6.11433119889839));
#286633=CARTESIAN_POINT('Ctrl Pts',(-1.34578569962224,-0.780178407881677,
6.11593037418026));
#286634=CARTESIAN_POINT('Ctrl Pts',(-1.33799392398079,-0.793466951915784,
6.11701185621647));
#286635=CARTESIAN_POINT('Ctrl Pts',(-1.31888299194205,-0.824977544242013,
6.11957552335834));
#286636=CARTESIAN_POINT('Ctrl Pts',(-1.30738158604779,-0.843085869274714,
6.12104814451345));
#286637=CARTESIAN_POINT('Ctrl Pts',(-1.26082544157125,-0.913140795127486,
6.12676661893265));
#286638=CARTESIAN_POINT('Ctrl Pts',(-1.22301747645506,-0.963190711970936,
6.13090094481871));
#286639=CARTESIAN_POINT('Ctrl Pts',(-1.11122641123908,-1.0939446321787,
6.14222872492545));
#286640=CARTESIAN_POINT('Ctrl Pts',(-1.03160466908351,-1.16932770880662,
6.14939532639174));
#286641=CARTESIAN_POINT('Ctrl Pts',(-0.928644949325772,-1.24804220952798,
6.15833102810828));
#286642=CARTESIAN_POINT('Ctrl Pts',(-0.912309961394032,-1.2600322489267,
6.15973895539476));
#286643=CARTESIAN_POINT('Ctrl Pts',(-0.885524878100282,-1.27889884101396,
6.16203525080687));
#286644=CARTESIAN_POINT('Ctrl Pts',(-0.87521754050084,-1.28597464821886,
6.16291602934773));
#286645=CARTESIAN_POINT('Ctrl Pts',(-0.856684683270905,-1.2983711127966,
6.16449528568368));
#286646=CARTESIAN_POINT('Ctrl Pts',(-0.848491990772424,-1.30373982322956,
6.16519191100446));
#286647=CARTESIAN_POINT('Ctrl Pts',(-0.831012775589663,-1.31495949789832,
6.1666753215411));
#286648=CARTESIAN_POINT('Ctrl Pts',(-0.821713975969679,-1.32079023488473,
6.16746280799881));
#286649=CARTESIAN_POINT('Ctrl Pts',(-0.796451019078721,-1.3362611255164,
6.16959823254077));
#286650=CARTESIAN_POINT('Ctrl Pts',(-0.780374387270222,-1.34571311240985,
6.17095290647922));
#286651=CARTESIAN_POINT('Ctrl Pts',(-0.670629947093092,-1.40760765918242,
6.18017595688249));
#286652=CARTESIAN_POINT('Ctrl Pts',(-0.571938099225301,-1.4505109901271,
6.18838189143427));
#286653=CARTESIAN_POINT('Ctrl Pts',(-0.380077221206418,-1.51127334080108,
6.20397566409862));
#286654=CARTESIAN_POINT('Ctrl Pts',(-0.288123983018666,-1.5314677451081,
6.21129864726842));
#286655=CARTESIAN_POINT('Ctrl Pts',(-0.180338789975893,-1.54508048030575,
6.21938415874202));
#286656=CARTESIAN_POINT('Ctrl Pts',(-0.165747872438668,-1.54671375959143,
6.22046800520865));
#286657=CARTESIAN_POINT('Ctrl Pts',(-0.144176343286324,-1.54881965415474,
6.22205256878175));
#286658=CARTESIAN_POINT('Ctrl Pts',(-0.137212671830504,-1.54945210536004,
6.22256135961418));
#286659=CARTESIAN_POINT('Ctrl Pts',(-0.124770650079497,-1.5504975693983,
6.22346526205088));
#286660=CARTESIAN_POINT('Ctrl Pts',(-0.119294127819881,-1.55092854183307,
6.22386132542982));
#286661=CARTESIAN_POINT('Ctrl Pts',(-0.107118547973533,-1.55182181725444,
6.22473786655048));
#286662=CARTESIAN_POINT('Ctrl Pts',(-0.100418670971426,-1.552269767414,
6.22521755127845));
#286663=CARTESIAN_POINT('Ctrl Pts',(-0.0804855581062721,-1.55347288536532,
6.22663736911018));
#286664=CARTESIAN_POINT('Ctrl Pts',(-0.0672449320482256,-1.55410233912994,
6.22757090877339));
#286665=CARTESIAN_POINT('Ctrl Pts',(-0.0364232754980438,-1.55517292097122,
6.2297251461664));
#286666=CARTESIAN_POINT('Ctrl Pts',(-0.0188393123344847,-1.55548532891337,
6.23093989416172));
#286667=CARTESIAN_POINT('Ctrl Pts',(0.0436076222808084,-1.55553563222086,
6.2352153177454));
#286668=CARTESIAN_POINT('Ctrl Pts',(0.0884522904674536,-1.55363107599078,
6.23821524926752));
#286669=CARTESIAN_POINT('Ctrl Pts',(0.238513135872617,-1.54073814325777,
6.24819780976266));
#286670=CARTESIAN_POINT('Ctrl Pts',(0.342669068901392,-1.52096676111891,
6.2550530850836));
#286671=CARTESIAN_POINT('Ctrl Pts',(0.484235677872064,-1.47880269779657,
6.26502955175859));
#286672=CARTESIAN_POINT('Ctrl Pts',(0.523953538708725,-1.46520093882124,
6.26790195922347));
#286673=CARTESIAN_POINT('Ctrl Pts',(0.577331201005106,-1.44447325192899,
6.27189252533987));
#286674=CARTESIAN_POINT('Ctrl Pts',(0.591509182244664,-1.43872552953729,
6.27296529032807));
#286675=CARTESIAN_POINT('Ctrl Pts',(0.614113879890847,-1.42917103096822,
6.27469751492509));
#286676=CARTESIAN_POINT('Ctrl Pts',(0.622595689112525,-1.42549650804733,
6.27535248902964));
#286677=CARTESIAN_POINT('Ctrl Pts',(0.640130815558017,-1.41771351974834,
6.27671727888139));
#286678=CARTESIAN_POINT('Ctrl Pts',(0.64917847608371,-1.41359342911686,
6.27742746704519));
#286679=CARTESIAN_POINT('Ctrl Pts',(0.670463164444214,-1.40365344777023,
6.27911275370506));
#286680=CARTESIAN_POINT('Ctrl Pts',(0.682664681716703,-1.39775991037981,
6.28009035503571));
#286681=CARTESIAN_POINT('Ctrl Pts',(0.723900558677622,-1.37717357638062,
6.28343456857516));
#286682=CARTESIAN_POINT('Ctrl Pts',(0.752548418749775,-1.36173039328814,
6.2858269663938));
#286683=CARTESIAN_POINT('Ctrl Pts',(0.822092391067357,-1.32137647037919,
6.29181216249458));
#286684=CARTESIAN_POINT('Ctrl Pts',(0.8623608136677,-1.2954554156237,6.29543678593333));
#286685=CARTESIAN_POINT('Ctrl Pts',(0.978225544185035,-1.21307403237337,
6.30632981229798));
#286686=CARTESIAN_POINT('Ctrl Pts',(1.0499512268174,-1.15155337491335,6.31371105405096));
#286687=CARTESIAN_POINT('Ctrl Pts',(1.14630439332128,-1.05237833928184,
6.32431404357605));
#286688=CARTESIAN_POINT('Ctrl Pts',(1.17559860995362,-1.01955021373039,
6.32764598769831));
#286689=CARTESIAN_POINT('Ctrl Pts',(1.21020919732241,-0.977285661478002,
6.33168047380303));
#286690=CARTESIAN_POINT('Ctrl Pts',(1.21686908622495,-0.968980499864533,
6.33246162700637));
#286691=CARTESIAN_POINT('Ctrl Pts',(1.22725272037933,-0.955755752651247,
6.33368641295464));
#286692=CARTESIAN_POINT('Ctrl Pts',(1.2310332082275,-0.950881455385524,
6.33413381294903));
#286693=CARTESIAN_POINT('Ctrl Pts',(1.23818564166113,-0.941545452995228,
6.33498290087094));
#286694=CARTESIAN_POINT('Ctrl Pts',(1.24156254484114,-0.937088027678857,
6.33538490402003));
#286695=CARTESIAN_POINT('Ctrl Pts',(1.24963916014926,-0.926306802196228,
6.33634931514273));
#286696=CARTESIAN_POINT('Ctrl Pts',(1.25431499805997,-0.919965333614888,
6.33691009243683));
#286697=CARTESIAN_POINT('Ctrl Pts',(1.27062739148011,-0.897486539030024,
6.3388762481788));
#286698=CARTESIAN_POINT('Ctrl Pts',(1.28200292409924,-0.881160969669723,
6.34026526410836));
#286699=CARTESIAN_POINT('Ctrl Pts',(1.30999075605402,-0.839304436537132,
6.34374179873587));
#286700=CARTESIAN_POINT('Ctrl Pts',(1.3261727321144,-0.813494833954837,
6.34580814461137));
#286701=CARTESIAN_POINT('Ctrl Pts',(1.41207755286116,-0.667096016959532,
6.35720222918962));
#286702=CARTESIAN_POINT('Ctrl Pts',(1.46611358120125,-0.53804619447234,
6.36610160924919));
#286703=CARTESIAN_POINT('Ctrl Pts',(1.51096540254233,-0.371069968189813,
6.3778680522512));
#286704=CARTESIAN_POINT('Ctrl Pts',(1.51862798041751,-0.33834619855023,
6.38018166426069));
#286705=CARTESIAN_POINT('Ctrl Pts',(1.52798580398463,-0.291611770038952,
6.383510999614));
#286706=CARTESIAN_POINT('Ctrl Pts',(1.53055982170805,-0.27778526046897,
6.38449903724833));
#286707=CARTESIAN_POINT('Ctrl Pts',(1.53463098715914,-0.254138961044634,
6.38619493638745));
#286708=CARTESIAN_POINT('Ctrl Pts',(1.53622223312982,-0.244336080824954,
6.38689978236669));
#286709=CARTESIAN_POINT('Ctrl Pts',(1.53927634060736,-0.22431056581014,
6.38834363687092));
#286710=CARTESIAN_POINT('Ctrl Pts',(1.54073148577742,-0.214087276413975,
6.38908285116062));
#286711=CARTESIAN_POINT('Ctrl Pts',(1.54412595618445,-0.18840884348777,
6.3909452461585));
#286712=CARTESIAN_POINT('Ctrl Pts',(1.54593508591862,-0.172937960586361,
6.3920724539712));
#286713=CARTESIAN_POINT('Ctrl Pts',(1.55240177881252,-0.109376671855721,
6.39672618905824));
#286714=CARTESIAN_POINT('Ctrl Pts',(1.55504942575179,-0.0611138412537209,
6.40031406956253));
#286715=CARTESIAN_POINT('Ctrl Pts',(1.55619706319746,0.078231641107936,
6.41083300909571));
#286716=CARTESIAN_POINT('Ctrl Pts',(1.54895208455727,0.169155897202332,
6.4179044551809));
#286717=CARTESIAN_POINT('Ctrl Pts',(1.5216212421582,0.331063378447491,6.43062504940875));
#286718=CARTESIAN_POINT('Ctrl Pts',(1.50436476533654,0.402272736222639,
6.43626143208353));
#286719=CARTESIAN_POINT('Ctrl Pts',(1.47871397640773,0.482818715153832,
6.44251551563358));
#286720=CARTESIAN_POINT('Ctrl Pts',(1.47515342250538,0.493590250884616,
6.44334920409742));
#286721=CARTESIAN_POINT('Ctrl Pts',(1.46940479591095,0.510363179346324,
6.44464216588145));
#286722=CARTESIAN_POINT('Ctrl Pts',(1.46729715338321,0.516391418078666,
6.44510579784246));
#286723=CARTESIAN_POINT('Ctrl Pts',(1.46348139463083,0.527093173282791,
6.44592676553356));
#286724=CARTESIAN_POINT('Ctrl Pts',(1.46178795700808,0.531771544571668,
6.44628491972709));
#286725=CARTESIAN_POINT('Ctrl Pts',(1.45761880402742,0.54311902387671,6.44715192629896));
#286726=CARTESIAN_POINT('Ctrl Pts',(1.45511974709323,0.549779391066904,
6.44765939945809));
#286727=CARTESIAN_POINT('Ctrl Pts',(1.44709070011319,0.57073970807169,6.44925267136657));
#286728=CARTESIAN_POINT('Ctrl Pts',(1.44139473368578,0.584975706143436,
6.45032925865656));
#286729=CARTESIAN_POINT('Ctrl Pts',(1.42727863467998,0.618797488116978,
6.45287909081194));
#286730=CARTESIAN_POINT('Ctrl Pts',(1.41866439451288,0.638299354561281,
6.45434290943217));
#286731=CARTESIAN_POINT('Ctrl Pts',(1.38344938703752,0.713785144098534,
6.46000702449176));
#286732=CARTESIAN_POINT('Ctrl Pts',(1.35391175207459,0.768339489650345,
6.46409796101389));
#286733=CARTESIAN_POINT('Ctrl Pts',(1.26294173033783,0.914735046839377,
6.47544856891413));
#286734=CARTESIAN_POINT('Ctrl Pts',(1.19488373283583,1.00200366986148,6.48267785933118));
#286735=CARTESIAN_POINT('Ctrl Pts',(1.10411636862351,1.09586308642367,6.49168086023593));
#286736=CARTESIAN_POINT('Ctrl Pts',(1.08978286835239,1.11011805464705,6.49308553341458));
#286737=CARTESIAN_POINT('Ctrl Pts',(1.06615141036347,1.13272122797636,6.49537757916382));
#286738=CARTESIAN_POINT('Ctrl Pts',(1.05702322604058,1.14124409903041,6.49625740907143));
#286739=CARTESIAN_POINT('Ctrl Pts',(1.04055528899516,1.15625293726304,6.49783561782297));
#286740=CARTESIAN_POINT('Ctrl Pts',(1.03325494969245,1.1627813058819,6.49853215370037));
#286741=CARTESIAN_POINT('Ctrl Pts',(1.01763735108328,1.17648421730729,6.50001606767491));
#286742=CARTESIAN_POINT('Ctrl Pts',(1.00930480794283,1.18364043741981,6.50080415320396));
#286743=CARTESIAN_POINT('Ctrl Pts',(0.986593000568982,1.20273176379965,
6.50294296633643));
#286744=CARTESIAN_POINT('Ctrl Pts',(0.972073723275396,1.21449663007365,
6.5043004666651));
#286745=CARTESIAN_POINT('Ctrl Pts',(0.939406467759112,1.24000557966923,
6.50733462873188));
#286746=CARTESIAN_POINT('Ctrl Pts',(0.921161902605812,1.25361836297864,
6.50901595731434));
#286747=CARTESIAN_POINT('Ctrl Pts',(0.862297848461558,1.29555960697576,
6.51440042743986));
#286748=CARTESIAN_POINT('Ctrl Pts',(0.820624309325186,1.32234911374503,
6.51815464351103));
#286749=CARTESIAN_POINT('Ctrl Pts',(0.741133028161882,1.36824325540462,
6.52519607614092));
#286750=CARTESIAN_POINT('Ctrl Pts',(0.703672843656824,1.38788041956314,
6.52846828671478));
#286751=CARTESIAN_POINT('Ctrl Pts',(0.587665381173473,1.4427881279482,6.5384196612024));
#286752=CARTESIAN_POINT('Ctrl Pts',(0.506940802201569,1.47309266588005,
6.54510772098529));
#286753=CARTESIAN_POINT('Ctrl Pts',(0.409686326087777,1.50065396704992,
6.55263478671519));
#286754=CARTESIAN_POINT('Ctrl Pts',(0.395196675119465,1.50453476088218,
6.55374258475157));
#286755=CARTESIAN_POINT('Ctrl Pts',(0.373815036447922,1.50993122257484,
6.55535515005548));
#286756=CARTESIAN_POINT('Ctrl Pts',(0.366965774705469,1.51161043386029,
6.55586839007227));
#286757=CARTESIAN_POINT('Ctrl Pts',(0.354758378299096,1.51451541753442,
6.5567769554744));
#286758=CARTESIAN_POINT('Ctrl Pts',(0.349404902511015,1.5157594380868,6.55717327619879));
#286759=CARTESIAN_POINT('Ctrl Pts',(0.33754580152315,1.51844904080439,6.55804650678551));
#286760=CARTESIAN_POINT('Ctrl Pts',(0.331037374574748,1.51988121860436,
6.55852266160173));
#286761=CARTESIAN_POINT('Ctrl Pts',(0.311803573228189,1.52398420010299,
6.55992125836218));
#286762=CARTESIAN_POINT('Ctrl Pts',(0.299053300794659,1.52653740958012,
6.56083739751321));
#286763=CARTESIAN_POINT('Ctrl Pts',(0.209158548276875,1.5433690098154,6.56722907994443));
#286764=CARTESIAN_POINT('Ctrl Pts',(0.131051990876703,1.55195489855696,
6.57243730879988));
#286765=CARTESIAN_POINT('Ctrl Pts',(-0.06762881234151,1.55867999008879,
6.58554757648713));
#286766=CARTESIAN_POINT('Ctrl Pts',(-0.187931072268608,1.54878509231677,
6.59338895931649));
#286767=CARTESIAN_POINT('Ctrl Pts',(-0.324949528546164,1.52130407281854,
6.6030355771444));
#286768=CARTESIAN_POINT('Ctrl Pts',(-0.343938707067638,1.51712372151877,
6.60438783855577));
#286769=CARTESIAN_POINT('Ctrl Pts',(-0.374769925576929,1.50972784593649,
6.60661135180177));
#286770=CARTESIAN_POINT('Ctrl Pts',(-0.386661439848873,1.50672611363478,
6.60747579851123));
#286771=CARTESIAN_POINT('Ctrl Pts',(-0.407961925842405,1.50108054819163,
6.60903719294024));
#286772=CARTESIAN_POINT('Ctrl Pts',(-0.417383928199067,1.49848803585847,
6.60973245171103));
#286773=CARTESIAN_POINT('Ctrl Pts',(-0.43747790596324,1.49275486189797,
6.61122537882337));
#286774=CARTESIAN_POINT('Ctrl Pts',(-0.448141814171445,1.48958816402604,
6.61202386028917));
#286775=CARTESIAN_POINT('Ctrl Pts',(-0.47726051154654,1.48060025102701,
6.61422166631972));
#286776=CARTESIAN_POINT('Ctrl Pts',(-0.495641514521877,1.47454878713076,
6.61562841909124));
#286777=CARTESIAN_POINT('Ctrl Pts',(-0.609296137251965,1.43476584402496,
6.62445215960411));
#286778=CARTESIAN_POINT('Ctrl Pts',(-0.701188979346341,1.39216437900338,
6.63216340705928));
#286779=CARTESIAN_POINT('Ctrl Pts',(-0.874252612711406,1.2904288646669,
6.6477065476552));
#286780=CARTESIAN_POINT('Ctrl Pts',(-0.95516678188034,1.23174021493512,
6.65549629929759));
#286781=CARTESIAN_POINT('Ctrl Pts',(-1.04053293827773,1.15631846625218,
6.66396676215639));
#286782=CARTESIAN_POINT('Ctrl Pts',(-1.0510277820373,1.14678761331466,6.66501260687379));
#286783=CARTESIAN_POINT('Ctrl Pts',(-1.0664322061526,1.13240900239201,6.66655260043478));
#286784=CARTESIAN_POINT('Ctrl Pts',(-1.07144185506442,1.12767023331067,
6.66705420733686));
#286785=CARTESIAN_POINT('Ctrl Pts',(-1.08038382572163,1.119098382594,6.6679507080363));
#286786=CARTESIAN_POINT('Ctrl Pts',(-1.08432752013084,1.11527764821498,
6.66834648284114));
#286787=CARTESIAN_POINT('Ctrl Pts',(-1.08832564946389,1.11136292074297,
6.66874812933775));
#286788=CARTESIAN_POINT('Ctrl Pts',(-1.0884001832469,1.11128992706291,6.66875561705156));
#286789=CARTESIAN_POINT('Ctrl Pts',(-1.08854596694684,1.11114712697881,
6.66877026288232));
#286790=CARTESIAN_POINT('Ctrl Pts',(-1.08861721749292,1.11107732121913,
6.66877742104919));
#286791=CARTESIAN_POINT('Ctrl Pts',(-1.08875667137687,1.11094066882643,
6.66879143152402));
#286792=CARTESIAN_POINT('Ctrl Pts',(-1.0888248752721,1.11087382276696,6.66879828387612));
#286793=CARTESIAN_POINT('Ctrl Pts',(-1.08895845027991,1.11074288291457,
6.66881170423066));
#286794=CARTESIAN_POINT('Ctrl Pts',(-1.08902382188681,1.11067878963472,
6.66881827227216));
#286795=CARTESIAN_POINT('Ctrl Pts',(-1.08915192705843,1.11055316734779,
6.66883114354127));
#286796=CARTESIAN_POINT('Ctrl Pts',(-1.08921466106545,1.11049163879851,
6.66883744680381));
#286797=CARTESIAN_POINT('Ctrl Pts',(-1.08933766832161,1.11037097472219,
6.66884980630065));
#286798=CARTESIAN_POINT('Ctrl Pts',(-1.08939794196289,1.11031183960944,
6.6688558625658));
#286799=CARTESIAN_POINT('Ctrl Pts',(-1.08951619020484,1.11019580609909,
6.66886774429265));
#286800=CARTESIAN_POINT('Ctrl Pts',(-1.08957416516664,1.11013890806507,
6.66887356978293));
#286801=CARTESIAN_POINT('Ctrl Pts',(-1.08968796390896,1.11002720571694,
6.6688850047953));
#286802=CARTESIAN_POINT('Ctrl Pts',(-1.08974378801396,1.10997240173115,
6.66889061434301));
#286803=CARTESIAN_POINT('Ctrl Pts',(-1.0898534204975,1.10986475640839,6.6689016310616));
#286804=CARTESIAN_POINT('Ctrl Pts',(-1.08990722916613,1.10981191537079,
6.6689070382553));
#286805=CARTESIAN_POINT('Ctrl Pts',(-1.0900129551008,1.10970807558055,6.66891766274094));
#286806=CARTESIAN_POINT('Ctrl Pts',(-1.09006487262972,1.10965707709861,
6.66892288005357));
#286807=CARTESIAN_POINT('Ctrl Pts',(-1.09016693060908,1.10955681168099,
6.66893313624929));
#286808=CARTESIAN_POINT('Ctrl Pts',(-1.09021707129827,1.10950754499062,
6.66893817515116));
#286809=CARTESIAN_POINT('Ctrl Pts',(-1.09031568091837,1.10941064108924,
6.66894808509454));
#286810=CARTESIAN_POINT('Ctrl Pts',(-1.09036415006567,1.10936300410195,
6.66895295615304));
#286811=CARTESIAN_POINT('Ctrl Pts',(-1.0904595137815,1.10926926538505,6.66896254016237));
#286812=CARTESIAN_POINT('Ctrl Pts',(-1.09050640855141,1.10922316385513,
6.66896725312908));
#286813=CARTESIAN_POINT('Ctrl Pts',(-1.09059871335894,1.10913240890158,
6.66897652997197));
#286814=CARTESIAN_POINT('Ctrl Pts',(-1.09064412357299,1.10908775566756,
6.66898109386188));
#286815=CARTESIAN_POINT('Ctrl Pts',(-1.09073354242938,1.10899981660498,
6.66899008089764));
#286816=CARTESIAN_POINT('Ctrl Pts',(-1.09077755123862,1.10895653094443,
6.66899450405661));
#286817=CARTESIAN_POINT('Ctrl Pts',(-1.0908642444119,1.10887125215194,6.66900321737164));
#286818=CARTESIAN_POINT('Ctrl Pts',(-1.0909069289252,1.10882925917761,6.66900750753934));
#286819=CARTESIAN_POINT('Ctrl Pts',(-1.09099104510587,1.10874649621885,
6.66901596205854));
#286820=CARTESIAN_POINT('Ctrl Pts',(-1.09103247691917,1.10870572637034,
6.6690201264216));
#286821=CARTESIAN_POINT('Ctrl Pts',(-1.09111415430529,1.10862534494907,
6.66902833601719));
#286822=CARTESIAN_POINT('Ctrl Pts',(-1.09115440000655,1.10858573350695,
6.66903238125977));
#286823=CARTESIAN_POINT('Ctrl Pts',(-1.09123376718447,1.10850760862078,
6.66904035883964));
#286824=CARTESIAN_POINT('Ctrl Pts',(-1.09127288877918,1.10846909529735,
6.66904429118615));
#286825=CARTESIAN_POINT('Ctrl Pts',(-1.09135006558836,1.1083931104047,6.66905204878057));
#286826=CARTESIAN_POINT('Ctrl Pts',(-1.09138812090421,1.10835563895416,
6.66905587403622));
#286827=CARTESIAN_POINT('Ctrl Pts',(-1.09146321913879,1.10828168529951,
6.66906342286819));
#286828=CARTESIAN_POINT('Ctrl Pts',(-1.09150026216013,1.10824520319625,
6.66906714645256));
#286829=CARTESIAN_POINT('Ctrl Pts',(-1.09157338629161,1.10817317911278,
6.66907449701031));
#286830=CARTESIAN_POINT('Ctrl Pts',(-1.09160946749354,1.10813763722904,
6.66907812399084));
#286831=CARTESIAN_POINT('Ctrl Pts',(-1.09168071522846,1.10806744760209,
6.6690852860838));
#286832=CARTESIAN_POINT('Ctrl Pts',(-1.09171588185033,1.10803279994453,
6.66908882120322));
#286833=CARTESIAN_POINT('Ctrl Pts',(-1.09178534471715,1.10796435564476,
6.66909580402081));
#286834=CARTESIAN_POINT('Ctrl Pts',(-1.0918196410374,1.10793055908906,6.66909925172475));
#286835=CARTESIAN_POINT('Ctrl Pts',(-1.09188740482526,1.10786377655022,
6.66910606388045));
#286836=CARTESIAN_POINT('Ctrl Pts',(-1.0919208723733,1.10783079063713,6.66910942833863));
#286837=CARTESIAN_POINT('Ctrl Pts',(-1.09198701764736,1.10776559135729,
6.66911607792168));
#286838=CARTESIAN_POINT('Ctrl Pts',(-1.09201969543987,1.10773337806394,
6.66911936305166));
#286839=CARTESIAN_POINT('Ctrl Pts',(-1.09208429787825,1.10766968828154,
6.6691258576608));
#286840=CARTESIAN_POINT('Ctrl Pts',(-1.09211622259116,1.10763821185582,
6.66912906714524));
#286841=CARTESIAN_POINT('Ctrl Pts',(-1.09217935341624,1.10757596213176,
6.66913541393205));
#286842=CARTESIAN_POINT('Ctrl Pts',(-1.09221055958131,1.10754518890197,
6.66913855123838));
#286843=CARTESIAN_POINT('Ctrl Pts',(-1.09227228583246,1.10748431385728,
6.6691447569346));
#286844=CARTESIAN_POINT('Ctrl Pts',(-1.09230280597647,1.10745421209797,
6.66914782532903));
#286845=CARTESIAN_POINT('Ctrl Pts',(-1.09746371224851,1.10236363310358,
6.66966669057766));
#286846=CARTESIAN_POINT('Ctrl Pts',(-1.1025590053112,1.09726743526625,6.67017975877982));
#286847=CARTESIAN_POINT('Ctrl Pts',(-1.11983656254871,1.07974493821374,
6.6719230686367));
#286848=CARTESIAN_POINT('Ctrl Pts',(-1.131846175951,1.06714917334659,6.67314095470289));
#286849=CARTESIAN_POINT('Ctrl Pts',(-1.16121950359434,1.03528834536938,
6.6761434115943));
#286850=CARTESIAN_POINT('Ctrl Pts',(-1.17831805758621,1.01578512041306,
6.67791273848272));
#286851=CARTESIAN_POINT('Ctrl Pts',(-1.2529751205085,0.92620510722277,6.68578611546857));
#286852=CARTESIAN_POINT('Ctrl Pts',(-1.30482965855053,0.851600981969717,
6.69167789013816));
#286853=CARTESIAN_POINT('Ctrl Pts',(-1.39013041861455,0.702620807524076,
6.70302339135113));
#286854=CARTESIAN_POINT('Ctrl Pts',(-1.42481485192995,0.629315990117589,
6.70843894290526));
#286855=CARTESIAN_POINT('Ctrl Pts',(-1.46010886109509,0.536650090761397,
6.71531674934382));
#286856=CARTESIAN_POINT('Ctrl Pts',(-1.4662850396723,0.519537621729463,
6.71658770015387));
#286857=CARTESIAN_POINT('Ctrl Pts',(-1.4756725230675,0.492025608169173,
6.71863448457448));
#286858=CARTESIAN_POINT('Ctrl Pts',(-1.47907739622488,0.481693512081849,
6.71940391419971));
#286859=CARTESIAN_POINT('Ctrl Pts',(-1.48534750426522,0.461973346459717,
6.72087436026123));
#286860=CARTESIAN_POINT('Ctrl Pts',(-1.48823281057048,0.452592172591282,
6.72157467808227));
#286861=CARTESIAN_POINT('Ctrl Pts',(-1.49464083950695,0.431033302250648,
6.72318624572058));
#286862=CARTESIAN_POINT('Ctrl Pts',(-1.49810381557494,0.418838736108049,
6.72409938942112));
#286863=CARTESIAN_POINT('Ctrl Pts',(-1.50503386946227,0.393248937519981,
6.72601937915204));
#286864=CARTESIAN_POINT('Ctrl Pts',(-1.50847202054401,0.379847094819705,
6.72702706863294));
#286865=CARTESIAN_POINT('Ctrl Pts',(-1.51722895557466,0.343716984974257,
6.72975006165938));
#286866=CARTESIAN_POINT('Ctrl Pts',(-1.5222154932883,0.320912691410175,
6.73147549490136));
#286867=CARTESIAN_POINT('Ctrl Pts',(-1.54593999569257,0.199371862087244,
6.74070921023653));
#286868=CARTESIAN_POINT('Ctrl Pts',(-1.55558598292837,0.0991205215353596,
6.74847856869965));
#286869=CARTESIAN_POINT('Ctrl Pts',(-1.55549942258976,-0.00134026972157471,
6.75626805975221));
#286870=CARTESIAN_POINT('',(-1.55549984414273,0.000696327469871839,8.15470034727716));
#286871=CARTESIAN_POINT('Ctrl Pts',(-1.55549942181485,-0.00134116877393629,
6.75626812946259));
#286872=CARTESIAN_POINT('Ctrl Pts',(-1.5554461534246,-0.063122319539924,
6.76105849302685));
#286873=CARTESIAN_POINT('Ctrl Pts',(-1.55171219940939,-0.124851075365541,
6.7658402330438));
#286874=CARTESIAN_POINT('Ctrl Pts',(-1.54162423982075,-0.208519539276235,
6.77220341735004));
#286875=CARTESIAN_POINT('Ctrl Pts',(-1.53844928112679,-0.230780488588829,
6.77388458400084));
#286876=CARTESIAN_POINT('Ctrl Pts',(-1.53357353590428,-0.260362541119816,
6.77609637094553));
#286877=CARTESIAN_POINT('Ctrl Pts',(-1.53230097168609,-0.267750220934243,
6.77664686579246));
#286878=CARTESIAN_POINT('Ctrl Pts',(-1.52999610729815,-0.280575822450825,
6.7775989942437));
#286879=CARTESIAN_POINT('Ctrl Pts',(-1.52898811242992,-0.286017892866135,
6.77800187249552));
#286880=CARTESIAN_POINT('Ctrl Pts',(-1.52691077494489,-0.296908337838535,
6.77880569152405));
#286881=CARTESIAN_POINT('Ctrl Pts',(-1.52584126543406,-0.302356598336974,
6.77920660629134));
#286882=CARTESIAN_POINT('Ctrl Pts',(-1.52349706924055,-0.313969022474034,
6.78005841743401));
#286883=CARTESIAN_POINT('Ctrl Pts',(-1.52221411771467,-0.32013130216559,
6.78050884911209));
#286884=CARTESIAN_POINT('Ctrl Pts',(-1.51859979672911,-0.336978491869008,
6.78173635807546));
#286885=CARTESIAN_POINT('Ctrl Pts',(-1.51619304242764,-0.347647123527009,
6.78250934340579));
#286886=CARTESIAN_POINT('Ctrl Pts',(-1.50178050697461,-0.408536028846398,
6.78690077674055));
#286887=CARTESIAN_POINT('Ctrl Pts',(-1.48739118857214,-0.458164901468319,
6.79040158755986));
#286888=CARTESIAN_POINT('Ctrl Pts',(-1.44623515003946,-0.577540401726483,
6.79883400490558));
#286889=CARTESIAN_POINT('Ctrl Pts',(-1.41686658450207,-0.646249833735386,
6.80370107320709));
#286890=CARTESIAN_POINT('Ctrl Pts',(-1.34588956625881,-0.783971014842977,
6.8139381989304));
#286891=CARTESIAN_POINT('Ctrl Pts',(-1.30363297067819,-0.852389494143139,
6.81930503997048));
#286892=CARTESIAN_POINT('Ctrl Pts',(-1.24530166720978,-0.932282754148224,
6.82615841330256));
#286893=CARTESIAN_POINT('Ctrl Pts',(-1.23404625924128,-0.947131012362532,
6.82745871579829));
#286894=CARTESIAN_POINT('Ctrl Pts',(-1.21564554086568,-0.970520502722886,
6.82955235875172));
#286895=CARTESIAN_POINT('Ctrl Pts',(-1.20867027774878,-0.979193686331489,
6.83033898558679));
#286896=CARTESIAN_POINT('Ctrl Pts',(-1.19539754825953,-0.995339355260532,
6.83182326719274));
#286897=CARTESIAN_POINT('Ctrl Pts',(-1.18912154120859,-1.00282884020603,
6.83252003109609));
#286898=CARTESIAN_POINT('Ctrl Pts',(-1.17481580233906,-1.01957750102682,
6.83409726426136));
#286899=CARTESIAN_POINT('Ctrl Pts',(-1.1667464491589,-1.02880180668721,
6.83497933916206));
#286900=CARTESIAN_POINT('Ctrl Pts',(-1.14561563383917,-1.05238867783107,
6.83727043639612));
#286901=CARTESIAN_POINT('Ctrl Pts',(-1.13239314314989,-1.06660340145885,
6.83868613242321));
#286902=CARTESIAN_POINT('Ctrl Pts',(-1.02081250534313,-1.18214330882122,
6.85049203245228));
#286903=CARTESIAN_POINT('Ctrl Pts',(-0.909356587658479,-1.26987193777603,
6.86149158030753));
#286904=CARTESIAN_POINT('Ctrl Pts',(-0.739278683446118,-1.36974166954489,
6.87672737289926));
#286905=CARTESIAN_POINT('Ctrl Pts',(-0.689414015507849,-1.39550522593221,
6.88102175348416));
#286906=CARTESIAN_POINT('Ctrl Pts',(-0.625480108252798,-1.42427221183914,
6.88623352718092));
#286907=CARTESIAN_POINT('Ctrl Pts',(-0.612620589762229,-1.42985060362415,
6.88726739355208));
#286908=CARTESIAN_POINT('Ctrl Pts',(-0.593352770495425,-1.43790120118648,
6.88879330201121));
#286909=CARTESIAN_POINT('Ctrl Pts',(-0.587001087161837,-1.44050584972729,
6.88929261253773));
#286910=CARTESIAN_POINT('Ctrl Pts',(-0.575538372071205,-1.44511798138018,
6.8901867834907));
#286911=CARTESIAN_POINT('Ctrl Pts',(-0.570433768911676,-1.44714053075377,
6.89058250217757));
#286912=CARTESIAN_POINT('Ctrl Pts',(-0.558952956790455,-1.4516192771095,
6.89146700014445));
#286913=CARTESIAN_POINT('Ctrl Pts',(-0.552571169897768,-1.4540605353574,
6.89195489916148));
#286914=CARTESIAN_POINT('Ctrl Pts',(-0.533204469464826,-1.46132306061495,
6.89342476323711));
#286915=CARTESIAN_POINT('Ctrl Pts',(-0.520170625972542,-1.46601318153408,
6.89439942409662));
#286916=CARTESIAN_POINT('Ctrl Pts',(-0.409268263025892,-1.50425510388419,
6.90258403153818));
#286917=CARTESIAN_POINT('Ctrl Pts',(-0.308325178944143,-1.52814462107105,
6.90933314052739));
#286918=CARTESIAN_POINT('Ctrl Pts',(-0.110563328351952,-1.55453426958151,
6.92247001865898));
#286919=CARTESIAN_POINT('Ctrl Pts',(-0.0144229815356042,-1.55839329633926,
6.92882376640449));
#286920=CARTESIAN_POINT('Ctrl Pts',(0.101786994824133,-1.55229967286303,
6.93686995498935));
#286921=CARTESIAN_POINT('Ctrl Pts',(0.122097436235896,-1.55083429676156,
6.93828908533171));
#286922=CARTESIAN_POINT('Ctrl Pts',(0.153660673008433,-1.54793318575309,
6.94051752941965));
#286923=CARTESIAN_POINT('Ctrl Pts',(0.164936918928933,-1.54677230081224,
6.94131825185264));
#286924=CARTESIAN_POINT('Ctrl Pts',(0.185888506627563,-1.54438363625017,
6.94281506713614));
#286925=CARTESIAN_POINT('Ctrl Pts',(0.195566996028052,-1.54318790007325,
6.94351011855532));
#286926=CARTESIAN_POINT('Ctrl Pts',(0.217103300699262,-1.54032132929337,
6.94506508747444));
#286927=CARTESIAN_POINT('Ctrl Pts',(0.228954240663342,-1.53860442656739,
6.94592641826281));
#286928=CARTESIAN_POINT('Ctrl Pts',(0.259021359296099,-1.53389339806876,
6.94812667599386));
#286929=CARTESIAN_POINT('Ctrl Pts',(0.27720576871111,-1.5307115759328,6.94947141671542));
#286930=CARTESIAN_POINT('Ctrl Pts',(0.42186162728375,-1.50273828642227,
6.96028519078677));
#286931=CARTESIAN_POINT('Ctrl Pts',(0.544839975684998,-1.4626433210855,
6.97025463646216));
#286932=CARTESIAN_POINT('Ctrl Pts',(0.723153844803379,-1.37886851131739,
6.98551999840515));
#286933=CARTESIAN_POINT('Ctrl Pts',(0.78290315444691,-1.34584338039981,
6.99077787995999));
#286934=CARTESIAN_POINT('Ctrl Pts',(0.85318161246795,-1.30072895182504,
6.99699966905268));
#286935=CARTESIAN_POINT('Ctrl Pts',(0.865943926294487,-1.29226770958556,
6.99813095822854));
#286936=CARTESIAN_POINT('Ctrl Pts',(0.88444683298687,-1.27960329672584,
6.99977092028087));
#286937=CARTESIAN_POINT('Ctrl Pts',(0.890286378098173,-1.275547320818,7.00028846548509));
#286938=CARTESIAN_POINT('Ctrl Pts',(0.900164546658569,-1.26858534958289,
7.00116361802363));
#286939=CARTESIAN_POINT('Ctrl Pts',(0.904217298551562,-1.26569983801713,
7.00152256475879));
#286940=CARTESIAN_POINT('Ctrl Pts',(0.913442605078443,-1.2590646008625,
7.00233935437786));
#286941=CARTESIAN_POINT('Ctrl Pts',(0.91860598346655,-1.25530239900733,
7.00279633666392));
#286942=CARTESIAN_POINT('Ctrl Pts',(0.932882436973186,-1.24476485961514,
7.00405984158212));
#286943=CARTESIAN_POINT('Ctrl Pts',(0.941944947884429,-1.23792121392969,
7.00486186928048));
#286944=CARTESIAN_POINT('Ctrl Pts',(1.00960641433873,-1.18565267516654,
7.01085659277416));
#286945=CARTESIAN_POINT('Ctrl Pts',(1.06497373604432,-1.1361828360166,7.01580269717447));
#286946=CARTESIAN_POINT('Ctrl Pts',(1.15701988429581,-1.04127556060515,
7.02453770223003));
#286947=CARTESIAN_POINT('Ctrl Pts',(1.19506866054603,-0.997376911891578,
7.02833733818701));
#286948=CARTESIAN_POINT('Ctrl Pts',(1.2615472873886,-0.911395998857486,
7.03553371262308));
#286949=CARTESIAN_POINT('Ctrl Pts',(1.29054306154434,-0.86985183864208,
7.03891526839405));
#286950=CARTESIAN_POINT('Ctrl Pts',(1.33544449265191,-0.798318612393778,
7.0446653053254));
#286951=CARTESIAN_POINT('Ctrl Pts',(1.35248838172107,-0.769090043153864,
7.04699565563088));
#286952=CARTESIAN_POINT('Ctrl Pts',(1.37509926747398,-0.727235348715366,
7.05032079150911));
#286953=CARTESIAN_POINT('Ctrl Pts',(1.38147270935295,-0.715054109673106,
7.05128711639731));
#286954=CARTESIAN_POINT('Ctrl Pts',(1.39219044984248,-0.693891562426556,
7.05296440412041));
#286955=CARTESIAN_POINT('Ctrl Pts',(1.39661141823699,-0.684949842730259,
7.05367264010257));
#286956=CARTESIAN_POINT('Ctrl Pts',(1.40494274349596,-0.667683102002845,
7.05503970456329));
#286957=CARTESIAN_POINT('Ctrl Pts',(1.40886587335198,-0.659364680123545,
7.05569805382979));
#286958=CARTESIAN_POINT('Ctrl Pts',(1.41901046871758,-0.637350617893801,
7.0574399643089));
#286959=CARTESIAN_POINT('Ctrl Pts',(1.42510729624343,-0.623598977807107,
7.05852773630491));
#286960=CARTESIAN_POINT('Ctrl Pts',(1.44672500392886,-0.572866002357884,
7.06254081203293));
#286961=CARTESIAN_POINT('Ctrl Pts',(1.4610122504768,-0.53537964254208,7.06550665087176));
#286962=CARTESIAN_POINT('Ctrl Pts',(1.50820098166086,-0.395551934121399,
7.07657829489497));
#286963=CARTESIAN_POINT('Ctrl Pts',(1.53191714611827,-0.290440505160677,
7.08494381894474));
#286964=CARTESIAN_POINT('Ctrl Pts',(1.5499660541996,-0.13871442806981,7.0967654060606));
#286965=CARTESIAN_POINT('Ctrl Pts',(1.5533512935746,-0.0934706506448398,
7.10025472282028));
#286966=CARTESIAN_POINT('Ctrl Pts',(1.55530273950125,-0.0304469370594353,
7.10501849250146));
#286967=CARTESIAN_POINT('Ctrl Pts',(1.55554854580069,-0.0127440085792736,
7.10634592338557));
#286968=CARTESIAN_POINT('Ctrl Pts',(1.55544961069072,0.0182822335078583,
7.10864957770304));
#286969=CARTESIAN_POINT('Ctrl Pts',(1.55523598122924,0.0316038878512167,
7.10963131904691));
#286970=CARTESIAN_POINT('Ctrl Pts',(1.55465690701263,0.0516470650495497,
7.11109573057003));
#286971=CARTESIAN_POINT('Ctrl Pts',(1.55441896580523,0.0583712354638141,
7.1115848688986));
#286972=CARTESIAN_POINT('Ctrl Pts',(1.55390753036541,0.0705819334814889,
7.11246896045836));
#286973=CARTESIAN_POINT('Ctrl Pts',(1.55364860129789,0.0760687070226881,
7.11286467031391));
#286974=CARTESIAN_POINT('Ctrl Pts',(1.55299481536975,0.0885213367051223,
7.11375930351815));
#286975=CARTESIAN_POINT('Ctrl Pts',(1.5525821546926,0.0954860279716213,
7.1142572415791));
#286976=CARTESIAN_POINT('Ctrl Pts',(1.55116111292197,0.117015326536737,
7.11578962725523));
#286977=CARTESIAN_POINT('Ctrl Pts',(1.54999450654879,0.131569202084861,
7.11681583215761));
#286978=CARTESIAN_POINT('Ctrl Pts',(1.53974108027983,0.240249081211163,
7.12442100428678));
#286979=CARTESIAN_POINT('Ctrl Pts',(1.52229140561027,0.333400992599896,
7.13062182459849));
#286980=CARTESIAN_POINT('Ctrl Pts',(1.46738249672422,0.527015586073728,
7.14386785359154));
#286981=CARTESIAN_POINT('Ctrl Pts',(1.42780875150913,0.626350462337095,
7.15089630805442));
#286982=CARTESIAN_POINT('Ctrl Pts',(1.36970155750898,0.737461390088812,
7.15958611006952));
#286983=CARTESIAN_POINT('Ctrl Pts',(1.36071510038732,0.753913802449323,
7.16089490724103));
#286984=CARTESIAN_POINT('Ctrl Pts',(1.34598909408515,0.779752862347507,
7.16298811388938));
#286985=CARTESIAN_POINT('Ctrl Pts',(1.3404433191501,0.789248290915252,7.16376558695342));
#286986=CARTESIAN_POINT('Ctrl Pts',(1.32977000644003,0.807086024440945,
7.16524227182624));
#286987=CARTESIAN_POINT('Ctrl Pts',(1.32466343817452,0.815440303385207,
7.1659406936499));
#286988=CARTESIAN_POINT('Ctrl Pts',(1.31287620534347,0.834321131196367,
7.16753505349304));
#286989=CARTESIAN_POINT('Ctrl Pts',(1.30614724688797,0.844816567760487,
7.16843274181945));
#286990=CARTESIAN_POINT('Ctrl Pts',(1.2882195287874,0.872052945351897,7.17079300903609));
#286991=CARTESIAN_POINT('Ctrl Pts',(1.27682083104916,0.888658758411981,
7.1722629524625));
#286992=CARTESIAN_POINT('Ctrl Pts',(1.17454986339862,1.0316178025739,7.18519621331196));
#286993=CARTESIAN_POINT('Ctrl Pts',(1.06552141325516,1.14387302927968,7.19741501249752));
#286994=CARTESIAN_POINT('Ctrl Pts',(0.91678408692183,1.25700729940031,7.21176019804354));
#286995=CARTESIAN_POINT('Ctrl Pts',(0.891297579510339,1.27520558687315,
7.21414430629795));
#286996=CARTESIAN_POINT('Ctrl Pts',(0.848418544825087,1.30390866680067,
7.21801628748301));
#286997=CARTESIAN_POINT('Ctrl Pts',(0.831339228286008,1.31486388221512,
7.2195238040548));
#286998=CARTESIAN_POINT('Ctrl Pts',(0.807285267109387,1.32963670194696,
7.22159416573021));
#286999=CARTESIAN_POINT('Ctrl Pts',(0.800489201953259,1.33373921981135,
7.22217337559145));
#287000=CARTESIAN_POINT('Ctrl Pts',(0.788844012330722,1.34064788634173,
7.22315573553395));
#287001=CARTESIAN_POINT('Ctrl Pts',(0.784010655969847,1.34348015489775,
7.22356051666608));
#287002=CARTESIAN_POINT('Ctrl Pts',(0.773845011574412,1.34936351149828,
7.2244055706674));
#287003=CARTESIAN_POINT('Ctrl Pts',(0.768509819067769,1.35240920197694,
7.22484550841922));
#287004=CARTESIAN_POINT('Ctrl Pts',(0.753981903448509,1.3605889897133,7.22603421809655));
#287005=CARTESIAN_POINT('Ctrl Pts',(0.744754662762928,1.36566160448789,
7.22677922900553));
#287006=CARTESIAN_POINT('Ctrl Pts',(0.698107372090106,1.39069222419757,
7.23049932084285));
#287007=CARTESIAN_POINT('Ctrl Pts',(0.659930055083606,1.40920964891525,
7.23339576843256));
#287008=CARTESIAN_POINT('Ctrl Pts',(0.545944016999929,1.45884685987556,
7.24175640378814));
#287009=CARTESIAN_POINT('Ctrl Pts',(0.468378955896553,1.48556777449472,
7.24709229992554));
#287010=CARTESIAN_POINT('Ctrl Pts',(0.334221626280769,1.52022527930509,
7.25624034812825));
#287011=CARTESIAN_POINT('Ctrl Pts',(0.278647292390724,1.5313862766584,7.26000631870906));
#287012=CARTESIAN_POINT('Ctrl Pts',(0.186483670670424,1.54471197640523,
7.26633022502652));
#287013=CARTESIAN_POINT('Ctrl Pts',(0.150206402729706,1.54866036859675,
7.26883858345569));
#287014=CARTESIAN_POINT('Ctrl Pts',(0.0997294027288756,1.55236403055502,
7.2723735322636));
#287015=CARTESIAN_POINT('Ctrl Pts',(0.0856196713792035,1.5532061311441,
7.27336642884897));
#287016=CARTESIAN_POINT('Ctrl Pts',(0.0614677129091435,1.5543174858183,
7.27507514200355));
#287017=CARTESIAN_POINT('Ctrl Pts',(0.0514305857802329,1.55468196512904,
7.27578794969664));
#287018=CARTESIAN_POINT('Ctrl Pts',(0.0322759468910776,1.55519183815218,
7.27715372660993));
#287019=CARTESIAN_POINT('Ctrl Pts',(0.023159276908928,1.55535431061846,
7.27780613172199));
#287020=CARTESIAN_POINT('Ctrl Pts',(-0.000553231564165983,1.55556837799962,
7.27950946372619));
#287021=CARTESIAN_POINT('Ctrl Pts',(-0.0151489966573689,1.55549470125027,
7.28056425039159));
#287022=CARTESIAN_POINT('Ctrl Pts',(-0.0667810235600491,1.55450731797242,
7.28431912917103));
#287023=CARTESIAN_POINT('Ctrl Pts',(-0.103780676694103,1.55247603922006,
7.28705326288367));
#287024=CARTESIAN_POINT('Ctrl Pts',(-0.261313325322442,1.53817114189868,
7.29888731682209));
#287025=CARTESIAN_POINT('Ctrl Pts',(-0.380251889264255,1.5131607554368,
7.30835074828367));
#287026=CARTESIAN_POINT('Ctrl Pts',(-0.531991375132014,1.46221852397795,
7.32070051715428));
#287027=CARTESIAN_POINT('Ctrl Pts',(-0.568445691944159,1.44843630701681,
7.32368542879435));
#287028=CARTESIAN_POINT('Ctrl Pts',(-0.626082748846818,1.42413381267385,
7.32839824742832));
#287029=CARTESIAN_POINT('Ctrl Pts',(-0.647609502019456,1.41447474822365,
7.33015681355987));
#287030=CARTESIAN_POINT('Ctrl Pts',(-0.676495098052812,1.400715969086,7.33250666972219));
#287031=CARTESIAN_POINT('Ctrl Pts',(-0.684051391025945,1.39704135468515,
7.3331204407238));
#287032=CARTESIAN_POINT('Ctrl Pts',(-0.696671307009299,1.39077736394873,
7.33414348733103));
#287033=CARTESIAN_POINT('Ctrl Pts',(-0.701751099595855,1.3882211583261,
7.33455472875851));
#287034=CARTESIAN_POINT('Ctrl Pts',(-0.712140880833589,1.38292130492553,
7.33539454117485));
#287035=CARTESIAN_POINT('Ctrl Pts',(-0.717449253388401,1.38017482291993,
7.33582293299826));
#287036=CARTESIAN_POINT('Ctrl Pts',(-0.731390111351289,1.37285984033884,
7.33694651467597));
#287037=CARTESIAN_POINT('Ctrl Pts',(-0.739995802063121,1.36824042553676,
7.33763861543021));
#287038=CARTESIAN_POINT('Ctrl Pts',(-0.777589174214755,1.34760237597381,
7.3406580269201));
#287039=CARTESIAN_POINT('Ctrl Pts',(-0.806106843720715,1.33074010629666,
7.34293806361482));
#287040=CARTESIAN_POINT('Ctrl Pts',(-0.908793134003266,1.26550887248818,
7.3511919498657));
#287041=CARTESIAN_POINT('Ctrl Pts',(-0.979336279307801,1.21174277756471,
7.35695674714405));
#287042=CARTESIAN_POINT('Ctrl Pts',(-1.09996902735297,1.10234735628645,
7.36769784063798));
#287043=CARTESIAN_POINT('Ctrl Pts',(-1.15135916420681,1.04855705397842,
7.37263716354117));
#287044=CARTESIAN_POINT('Ctrl Pts',(-1.21584980242207,0.970573639225771,
7.37957716228632));
#287045=CARTESIAN_POINT('Ctrl Pts',(-1.23245212984931,0.949402723122586,
7.38144054469549));
#287046=CARTESIAN_POINT('Ctrl Pts',(-1.2560153264828,0.917695294021819,
7.3842086761662));
#287047=CARTESIAN_POINT('Ctrl Pts',(-1.26341079399149,0.907486805436926,
7.38509656130911));
#287048=CARTESIAN_POINT('Ctrl Pts',(-1.27633744167304,0.889178920574204,
7.38668370151301));
#287049=CARTESIAN_POINT('Ctrl Pts',(-1.28191769549825,0.88111487998841,
7.38738103280793));
#287050=CARTESIAN_POINT('Ctrl Pts',(-1.29354818165743,0.863963270014136,
7.38886084856189));
#287051=CARTESIAN_POINT('Ctrl Pts',(-1.29957971122609,0.854863727807574,
7.38964398898473));
#287052=CARTESIAN_POINT('Ctrl Pts',(-1.31550366685818,0.830281820279892,
7.39175485965898));
#287053=CARTESIAN_POINT('Ctrl Pts',(-1.3252181205689,0.814686858752893,
7.39308906109718));
#287054=CARTESIAN_POINT('Ctrl Pts',(-1.38112082003019,0.721297830649551,
7.40105319270122));
#287055=CARTESIAN_POINT('Ctrl Pts',(-1.42071875397584,0.639779763202748,
7.4079164272815));
#287056=CARTESIAN_POINT('Ctrl Pts',(-1.47619111437831,0.494629401103293,
7.41991277673608));
#287057=CARTESIAN_POINT('Ctrl Pts',(-1.4955541711107,0.432569230404838,
7.42497258904737));
#287058=CARTESIAN_POINT('Ctrl Pts',(-1.51945786923799,0.334815686785833,
7.43272222755207));
#287059=CARTESIAN_POINT('Ctrl Pts',(-1.52673963748886,0.299866931441088,
7.4354498277595));
#287060=CARTESIAN_POINT('Ctrl Pts',(-1.53659501046379,0.242796113886426,
7.43980635398641));
#287061=CARTESIAN_POINT('Ctrl Pts',(-1.53990737905204,0.220815704077361,
7.44146099457647));
#287062=CARTESIAN_POINT('Ctrl Pts',(-1.54379780838238,0.190620313889035,
7.4436958183619));
#287063=CARTESIAN_POINT('Ctrl Pts',(-1.54478331648398,0.182461750367341,
7.4442958443289));
#287064=CARTESIAN_POINT('Ctrl Pts',(-1.54633739006574,0.168679766933739,
7.44530260772742));
#287065=CARTESIAN_POINT('Ctrl Pts',(-1.54694003935443,0.163060438509517,
7.44571117722064));
#287066=CARTESIAN_POINT('Ctrl Pts',(-1.54812309547542,0.151431755106252,
7.44655255939499));
#287067=CARTESIAN_POINT('Ctrl Pts',(-1.54869916490068,0.145422127491667,
7.44698513435231));
#287068=CARTESIAN_POINT('Ctrl Pts',(-1.55014029299135,0.129407013327003,
7.44813229750346));
#287069=CARTESIAN_POINT('Ctrl Pts',(-1.55094348823809,0.119396035769288,
7.44884355931561));
#287070=CARTESIAN_POINT('Ctrl Pts',(-1.55419254797389,0.0733043232473564,
7.45209444553764));
#287071=CARTESIAN_POINT('Ctrl Pts',(-1.55547689677781,0.03714985694327,
7.45457737297868));
#287072=CARTESIAN_POINT('Ctrl Pts',(-1.5555513709279,-0.0810240234271968,
7.46257013240316));
#287073=CARTESIAN_POINT('Ctrl Pts',(-1.54911823340247,-0.162909520585166,
7.46792058479099));
#287074=CARTESIAN_POINT('Ctrl Pts',(-1.52192293400986,-0.334197663141845,
7.47935317486277));
#287075=CARTESIAN_POINT('Ctrl Pts',(-1.49965905356957,-0.423032999341945,
7.48543149064005));
#287076=CARTESIAN_POINT('Ctrl Pts',(-1.46371375611712,-0.526744266357612,
7.49304283651953));
#287077=CARTESIAN_POINT('Ctrl Pts',(-1.45739341552974,-0.543987007957729,
7.49432552451019));
#287078=CARTESIAN_POINT('Ctrl Pts',(-1.44683212535322,-0.571293437162566,
7.49638670543128));
#287079=CARTESIAN_POINT('Ctrl Pts',(-1.44278777097378,-0.581431704756804,
7.49715863115549));
#287080=CARTESIAN_POINT('Ctrl Pts',(-1.43490777296516,-0.600596460508967,
7.49863096473053));
#287081=CARTESIAN_POINT('Ctrl Pts',(-1.43109278785405,-0.609630912723666,
7.49933064529748));
#287082=CARTESIAN_POINT('Ctrl Pts',(-1.42217806111985,-0.630197428803772,
7.50093663195371));
#287083=CARTESIAN_POINT('Ctrl Pts',(-1.41702307255711,-0.641704629294601,
7.5018447855074));
#287084=CARTESIAN_POINT('Ctrl Pts',(-1.40042535175481,-0.677579342446644,
7.50470699906612));
#287085=CARTESIAN_POINT('Ctrl Pts',(-1.38849017358543,-0.70171205067251,
7.5066777683561));
#287086=CARTESIAN_POINT('Ctrl Pts',(-1.34103754593463,-0.791704899204001,
7.51420521668325));
#287087=CARTESIAN_POINT('Ctrl Pts',(-1.30141481402088,-0.855274793738121,
7.51989834770173));
#287088=CARTESIAN_POINT('Ctrl Pts',(-1.20475689529122,-0.987993235384248,
7.53256831975693));
#287089=CARTESIAN_POINT('Ctrl Pts',(-1.1460051573368,-1.05557690613899,
7.5395589441975));
#287090=CARTESIAN_POINT('Ctrl Pts',(-1.05880874894783,-1.13996738602274,
7.54878307542085));
#287091=CARTESIAN_POINT('Ctrl Pts',(-1.03516251649051,-1.16148203738401,
7.55118395917232));
#287092=CARTESIAN_POINT('Ctrl Pts',(-1.00353337876584,-1.18852603655466,
7.55425033113436));
#287093=CARTESIAN_POINT('Ctrl Pts',(-0.996140091383027,-1.19472938896165,
7.55495719813143));
#287094=CARTESIAN_POINT('Ctrl Pts',(-0.984094901973606,-1.20464637581517,
7.55609230597254));
#287095=CARTESIAN_POINT('Ctrl Pts',(-0.979478727972305,-1.20840270254495,
7.55652346566215));
#287096=CARTESIAN_POINT('Ctrl Pts',(-0.970396769641774,-1.21570674330437,
7.55736403231715));
#287097=CARTESIAN_POINT('Ctrl Pts',(-0.965932861434693,-1.21925652966422,
7.55777357082743));
#287098=CARTESIAN_POINT('Ctrl Pts',(-0.954778355079439,-1.22802710076918,
7.55878826695374));
#287099=CARTESIAN_POINT('Ctrl Pts',(-0.948064229904457,-1.23321794189664,
7.55939135704702));
#287100=CARTESIAN_POINT('Ctrl Pts',(-0.922011138562466,-1.25302163480796,
7.56170362067648));
#287101=CARTESIAN_POINT('Ctrl Pts',(-0.902372933958467,-1.26723755121632,
7.56338784598552));
#287102=CARTESIAN_POINT('Ctrl Pts',(-0.849001025717572,-1.30400276616839,
7.56783471311015));
#287103=CARTESIAN_POINT('Ctrl Pts',(-0.814702932386624,-1.32570191464811,
7.57055815280981));
#287104=CARTESIAN_POINT('Ctrl Pts',(-0.662687990100577,-1.41374545896751,
7.58223612868556));
#287105=CARTESIAN_POINT('Ctrl Pts',(-0.537469250331609,-1.46593227017965,
7.59092905023762));
#287106=CARTESIAN_POINT('Ctrl Pts',(-0.381882709023447,-1.50812056240722,
7.60199460211515));
#287107=CARTESIAN_POINT('Ctrl Pts',(-0.356515026886978,-1.51431797641573,
7.60380447243743));
#287108=CARTESIAN_POINT('Ctrl Pts',(-0.318827794595403,-1.52252566310758,
7.60650810347402));
#287109=CARTESIAN_POINT('Ctrl Pts',(-0.306619877987969,-1.52503107895591,
7.60738613661701));
#287110=CARTESIAN_POINT('Ctrl Pts',(-0.284769565861887,-1.52924242853323,
7.60896236440718));
#287111=CARTESIAN_POINT('Ctrl Pts',(-0.275138572552282,-1.53100452930566,
7.60965873409149));
#287112=CARTESIAN_POINT('Ctrl Pts',(-0.2546539793997,-1.53455289357511,
7.61114361740713));
#287113=CARTESIAN_POINT('Ctrl Pts',(-0.243796832459268,-1.53631517774726,
7.61193285029291));
#287114=CARTESIAN_POINT('Ctrl Pts',(-0.214373890643901,-1.5407712401609,
7.61407815630462));
#287115=CARTESIAN_POINT('Ctrl Pts',(-0.195777108267731,-1.5432444544636,
7.61544107303951));
#287116=CARTESIAN_POINT('Ctrl Pts',(-0.154413535732602,-1.5479857973929,
7.61848928410685));
#287117=CARTESIAN_POINT('Ctrl Pts',(-0.131632635095191,-1.55008913241173,
7.62017931283));
#287118=CARTESIAN_POINT('Ctrl Pts',(-0.0590287607748288,-1.55518059515145,
7.62560235588266));
#287119=CARTESIAN_POINT('Ctrl Pts',(-0.00910832029281636,-1.55627351729704,
7.62938727075242));
#287120=CARTESIAN_POINT('Ctrl Pts',(0.0929951525243039,-1.55359616997825,
7.63722483980242));
#287121=CARTESIAN_POINT('Ctrl Pts',(0.145112248932143,-1.54959711217791,
7.64127699848221));
#287122=CARTESIAN_POINT('Ctrl Pts',(0.212169227030735,-1.54103879626259,
7.64651840754183));
#287123=CARTESIAN_POINT('Ctrl Pts',(0.227381658070818,-1.53886774617074,
7.64770919577214));
#287124=CARTESIAN_POINT('Ctrl Pts',(0.307615593882776,-1.52620138516531,
7.65399313510563));
#287125=CARTESIAN_POINT('Ctrl Pts',(0.371961783305136,-1.51180835518359,
7.65904759351741));
#287126=CARTESIAN_POINT('Ctrl Pts',(0.446058225091606,-1.49021476074776,
7.66475716154708));
#287127=CARTESIAN_POINT('Ctrl Pts',(0.456873985479725,-1.48693448223988,
7.66558766799229));
#287128=CARTESIAN_POINT('Ctrl Pts',(0.473734796253627,-1.48161946890251,
7.66687677917958));
#287129=CARTESIAN_POINT('Ctrl Pts',(0.479804450955065,-1.47966502984727,
7.66733970255103));
#287130=CARTESIAN_POINT('Ctrl Pts',(0.490590236162439,-1.47611864114055,
7.6681600769714));
#287131=CARTESIAN_POINT('Ctrl Pts',(0.49531081325639,-1.47454135985071,
7.66851833917315));
#287132=CARTESIAN_POINT('Ctrl Pts',(0.506773444915998,-1.47065010491476,
7.66938645968036));
#287133=CARTESIAN_POINT('Ctrl Pts',(0.513507283768295,-1.46831240898391,
7.66989492897863));
#287134=CARTESIAN_POINT('Ctrl Pts',(0.534747093206801,-1.460774878972,7.67149465106212));
#287135=CARTESIAN_POINT('Ctrl Pts',(0.549192535884902,-1.45540554701198,
7.67257658656303));
#287136=CARTESIAN_POINT('Ctrl Pts',(0.583559429438671,-1.44204688353981,
7.6751415364512));
#287137=CARTESIAN_POINT('Ctrl Pts',(0.603400397423282,-1.43385804113288,
7.67661497406404));
#287138=CARTESIAN_POINT('Ctrl Pts',(0.68054152992792,-1.40013504638731,
7.68233851202091));
#287139=CARTESIAN_POINT('Ctrl Pts',(0.736448527313433,-1.37155374683397,
7.68647688210462));
#287140=CARTESIAN_POINT('Ctrl Pts',(0.884582049499695,-1.28414682087576,
7.69780258632168));
#287141=CARTESIAN_POINT('Ctrl Pts',(0.972560631730535,-1.21886864259515,
7.70496338385475));
#287142=CARTESIAN_POINT('Ctrl Pts',(1.06788731059356,-1.13119744487014,
7.71389284280486));
#287143=CARTESIAN_POINT('Ctrl Pts',(1.08253394429636,-1.1171889554314,7.71530105289325));
#287144=CARTESIAN_POINT('Ctrl Pts',(1.1057674805973,-1.09408174472268,7.71759771759689));
#287145=CARTESIAN_POINT('Ctrl Pts',(1.1145259252083,-1.08515829771355,7.71847857854332));
#287146=CARTESIAN_POINT('Ctrl Pts',(1.1299521531551,-1.06905768187899,7.72005792593536));
#287147=CARTESIAN_POINT('Ctrl Pts',(1.13666158080587,-1.06192120155306,
7.72075455908065));
#287148=CARTESIAN_POINT('Ctrl Pts',(1.15074467697954,-1.04665533360013,
7.72223792615393));
#287149=CARTESIAN_POINT('Ctrl Pts',(1.15810056914642,-1.03851035587509,
7.72302536078774));
#287150=CARTESIAN_POINT('Ctrl Pts',(1.177719257509,-1.01631946203229,7.72516049224144));
#287151=CARTESIAN_POINT('Ctrl Pts',(1.18981634614515,-1.00213018353396,
7.72651492173042));
#287152=CARTESIAN_POINT('Ctrl Pts',(1.26926309661583,-0.905476410857493,
7.73567349159042));
#287153=CARTESIAN_POINT('Ctrl Pts',(1.32823469294344,-0.816517360817221,
7.7438092111462));
#287154=CARTESIAN_POINT('Ctrl Pts',(1.42178126464292,-0.638083298918485,
7.75941790586602));
#287155=CARTESIAN_POINT('Ctrl Pts',(1.45810601545017,-0.550038393187028,
7.76682888831033));
#287156=CARTESIAN_POINT('Ctrl Pts',(1.49046192045692,-0.44532577921856,
7.7749836965357));
#287157=CARTESIAN_POINT('Ctrl Pts',(1.49456084870292,-0.431369558442356,
7.77605728670087));
#287158=CARTESIAN_POINT('Ctrl Pts',(1.50033272054773,-0.410646448948991,
7.77762983851331));
#287159=CARTESIAN_POINT('Ctrl Pts',(1.5021567811821,-0.403922997776245,
7.77813670561533));
#287160=CARTESIAN_POINT('Ctrl Pts',(1.50533814549645,-0.391876875812767,
7.77903860995055));
#287161=CARTESIAN_POINT('Ctrl Pts',(1.50671249092974,-0.386559039042714,
7.77943458006285));
#287162=CARTESIAN_POINT('Ctrl Pts',(1.50970996293511,-0.374701841867542,
7.78031263245902));
#287163=CARTESIAN_POINT('Ctrl Pts',(1.51131880057658,-0.368159109667949,
7.78079390475368));
#287164=CARTESIAN_POINT('Ctrl Pts',(1.51599291411936,-0.348603578420759,
7.78222332123121));
#287165=CARTESIAN_POINT('Ctrl Pts',(1.51893309825835,-0.335561089913032,
7.78316473841743));
#287166=CARTESIAN_POINT('Ctrl Pts',(1.53845080418241,-0.243462269281697,
7.7897393407578));
#287167=CARTESIAN_POINT('Ctrl Pts',(1.54901867961024,-0.163246841870398,
7.79509104627263));
#287168=CARTESIAN_POINT('Ctrl Pts',(1.55950571733998,0.0340502686216471,
7.80811324795337));
#287169=CARTESIAN_POINT('Ctrl Pts',(1.55255264310236,0.150977429643399,
7.81573728681553));
#287170=CARTESIAN_POINT('Ctrl Pts',(1.52920179332225,0.285505201450163,
7.82515788400288));
#287171=CARTESIAN_POINT('Ctrl Pts',(1.52544855874996,0.304922906700598,
7.82653279637999));
#287172=CARTESIAN_POINT('Ctrl Pts',(1.51874938263034,0.336353045303748,
7.82878594711245));
#287173=CARTESIAN_POINT('Ctrl Pts',(1.51602850376104,0.348411564697607,
7.82965706579577));
#287174=CARTESIAN_POINT('Ctrl Pts',(1.51089786303221,0.369950757964319,
7.83122571118637));
#287175=CARTESIAN_POINT('Ctrl Pts',(1.50854181984313,0.379443652777201,
7.83192148216959));
#287176=CARTESIAN_POINT('Ctrl Pts',(1.5033309345747,0.399623193459529,7.83341029611257));
#287177=CARTESIAN_POINT('Ctrl Pts',(1.50045132583116,0.410302818299376,
7.83420410507415));
#287178=CARTESIAN_POINT('Ctrl Pts',(1.49230236339194,0.439291328708979,
7.83637534902949));
#287179=CARTESIAN_POINT('Ctrl Pts',(1.48681029719465,0.457535021158104,
7.83775991389872));
#287180=CARTESIAN_POINT('Ctrl Pts',(1.44877234586852,0.575964455032252,
7.8468707477336));
#287181=CARTESIAN_POINT('Ctrl Pts',(1.40646200060367,0.672705693894223,
7.85491989568598));
#287182=CARTESIAN_POINT('Ctrl Pts',(1.30778304293573,0.847587322118531,
7.87047604210372));
#287183=CARTESIAN_POINT('Ctrl Pts',(1.25328731124673,0.926269299289943,
7.87792447945845));
#287184=CARTESIAN_POINT('Ctrl Pts',(1.18260211194869,1.01056544755285,7.88610926774412));
#287185=CARTESIAN_POINT('Ctrl Pts',(1.17313508720526,1.02154020292545,7.88717895359027));
#287186=CARTESIAN_POINT('Ctrl Pts',(1.15889869909463,1.03758491031854,7.88874692947949));
#287187=CARTESIAN_POINT('Ctrl Pts',(1.15424681022674,1.0427573768373,7.88925306132998));
#287188=CARTESIAN_POINT('Ctrl Pts',(1.14586027631459,1.05195752860724,7.89015420499997));
#287189=CARTESIAN_POINT('Ctrl Pts',(1.14213884291817,1.05599681874827,7.89055014246653));
#287190=CARTESIAN_POINT('Ctrl Pts',(1.1337985691925,1.06495378605565,7.89142878577568));
#287191=CARTESIAN_POINT('Ctrl Pts',(1.12916905785518,1.06986120840961,7.89191067504753));
#287192=CARTESIAN_POINT('Ctrl Pts',(1.11524012903284,1.0844351604403,7.8933438311839));
#287193=CARTESIAN_POINT('Ctrl Pts',(1.10584716269768,1.09401199589192,7.89428831866406));
#287194=CARTESIAN_POINT('Ctrl Pts',(1.03599564171551,1.16341182818986,7.9011641271682));
#287195=CARTESIAN_POINT('Ctrl Pts',(0.970836239312873,1.21831653324784,
7.90678287780732));
#287196=CARTESIAN_POINT('Ctrl Pts',(0.810435518104754,1.33238994065278,
7.91974692427541));
#287197=CARTESIAN_POINT('Ctrl Pts',(0.712662931901051,1.38714695490054,
7.92706141074413));
#287198=CARTESIAN_POINT('Ctrl Pts',(0.591346288453293,1.43885212137053,
7.93615545534466));
#287199=CARTESIAN_POINT('Ctrl Pts',(0.572668214387081,1.44638753890662,
7.93755507885279));
#287200=CARTESIAN_POINT('Ctrl Pts',(0.542199911901414,1.45799688965956,
7.93984052878458));
#287201=CARTESIAN_POINT('Ctrl Pts',(0.53049737390352,1.46229552242961,7.94071888509545));
#287202=CARTESIAN_POINT('Ctrl Pts',(0.509513904668546,1.46971823876505,
7.94229546886922));
#287203=CARTESIAN_POINT('Ctrl Pts',(0.500252654652554,1.47289626040478,
7.94299186813151));
#287204=CARTESIAN_POINT('Ctrl Pts',(0.480527921212848,1.47945736257899,
7.94447657556078));
#287205=CARTESIAN_POINT('Ctrl Pts',(0.470057377665715,1.48281732555132,
7.94526560084619));
#287206=CARTESIAN_POINT('Ctrl Pts',(0.441642575568518,1.49160434402932,
7.94740973175514));
#287207=CARTESIAN_POINT('Ctrl Pts',(0.423634920188506,1.49681831932147,
7.94877166813593));
#287208=CARTESIAN_POINT('Ctrl Pts',(0.302521331243627,1.52952525422715,
7.95795630718059));
#287209=CARTESIAN_POINT('Ctrl Pts',(0.196935323411867,1.54666569120924,
7.96611192945075));
#287210=CARTESIAN_POINT('Ctrl Pts',(-0.00390681945205614,1.55836388938543,
7.98169933301478));
#287211=CARTESIAN_POINT('Ctrl Pts',(-0.0985739899200065,1.55524903061796,
7.98906823861353));
#287212=CARTESIAN_POINT('Ctrl Pts',(-0.206875574613135,1.54175100192689,
7.99718983681705));
#287213=CARTESIAN_POINT('Ctrl Pts',(-0.221346353541598,1.53974007158688,
7.99826825123573));
#287214=CARTESIAN_POINT('Ctrl Pts',(-0.242685096764264,1.5364676670645,
7.99984645460042));
#287215=CARTESIAN_POINT('Ctrl Pts',(-0.249575844972282,1.53536342628076,
8.00035422795687));
#287216=CARTESIAN_POINT('Ctrl Pts',(-0.261876878809404,1.53330718474823,
8.00125707217658));
#287217=CARTESIAN_POINT('Ctrl Pts',(-0.267289795028401,1.53237286287216,
8.00165308482519));
#287218=CARTESIAN_POINT('Ctrl Pts',(-0.279320346272054,1.53023058430116,
8.00253041906046));
#287219=CARTESIAN_POINT('Ctrl Pts',(-0.28593520371646,1.52900835862683,
8.00301093869851));
#287220=CARTESIAN_POINT('Ctrl Pts',(-0.305618946486915,1.52523918910693,
8.00443580022308));
#287221=CARTESIAN_POINT('Ctrl Pts',(-0.31866369107744,1.52256724238022,
8.00537347865366));
#287222=CARTESIAN_POINT('Ctrl Pts',(-0.348955226882635,1.51595626523493,
8.00753893098474));
#287223=CARTESIAN_POINT('Ctrl Pts',(-0.366172609857623,1.51188982013678,
8.00876066864415));
#287224=CARTESIAN_POINT('Ctrl Pts',(-0.427210254618112,1.49636986165555,
8.01307169110106));
#287225=CARTESIAN_POINT('Ctrl Pts',(-0.470597868001205,1.48329687655853,
8.0160991524277));
#287226=CARTESIAN_POINT('Ctrl Pts',(-0.614607642109122,1.43294894634925,
8.02620787291912));
#287227=CARTESIAN_POINT('Ctrl Pts',(-0.711921568214003,1.38717418581404,
8.03316094890744));
#287228=CARTESIAN_POINT('Ctrl Pts',(-0.838274930346336,1.31091624865259,
8.0431425903796));
#287229=CARTESIAN_POINT('Ctrl Pts',(-0.871972577936714,1.28874731296504,
8.04590556222786));
#287230=CARTESIAN_POINT('Ctrl Pts',(-0.917029715459742,1.25652853007427,
8.04976740445225));
#287231=CARTESIAN_POINT('Ctrl Pts',(-0.929162140221522,1.24758371870021,
8.05082470820076));
#287232=CARTESIAN_POINT('Ctrl Pts',(-0.94848931411271,1.23289616757936,
8.05253853125497));
#287233=CARTESIAN_POINT('Ctrl Pts',(-0.955766624526113,1.22726325287917,
8.05319074679607));
#287234=CARTESIAN_POINT('Ctrl Pts',(-0.970413826315627,1.21571647106866,
8.05451784000496));
#287235=CARTESIAN_POINT('Ctrl Pts',(-0.97778065784544,1.20979936775441,
8.05519282822235));
#287236=CARTESIAN_POINT('Ctrl Pts',(-0.985345748986534,1.20360878678822,
8.05589395168651));
#287237=CARTESIAN_POINT('Ctrl Pts',(-0.985598456674946,1.20340186092564,
8.05591738159988));
#287238=CARTESIAN_POINT('Ctrl Pts',(-0.986078891436294,1.20300821135571,
8.05596194298151));
#287239=CARTESIAN_POINT('Ctrl Pts',(-0.986306630725689,1.20282150251473,
8.05598307384691));
#287240=CARTESIAN_POINT('Ctrl Pts',(-0.986741923097343,1.20246442745936,
8.05602347702826));
#287241=CARTESIAN_POINT('Ctrl Pts',(-0.986949485137246,1.20229407213467,
8.05604274890235));
#287242=CARTESIAN_POINT('Ctrl Pts',(-0.987348100502012,1.20196673813331,
8.05607977190504));
#287243=CARTESIAN_POINT('Ctrl Pts',(-0.987539160547177,1.20180976761274,
8.05609752270271));
#287244=CARTESIAN_POINT('Ctrl Pts',(-0.98790765202604,1.20150687631958,
8.05613176839118));
#287245=CARTESIAN_POINT('Ctrl Pts',(-0.988085088591989,1.20136096177498,
8.05614826302903));
#287246=CARTESIAN_POINT('Ctrl Pts',(-0.988428630944044,1.20107832293102,
8.05618020790503));
#287247=CARTESIAN_POINT('Ctrl Pts',(-0.988594740713639,1.2009416034587,
8.05619565794715));
#287248=CARTESIAN_POINT('Ctrl Pts',(-0.988917493974861,1.20067584355609,
8.05622568541747));
#287249=CARTESIAN_POINT('Ctrl Pts',(-0.989074140596858,1.2005468069139,
8.05624026269183));
#287250=CARTESIAN_POINT('Ctrl Pts',(-0.998454038716651,1.19281709461721,
8.0571133559649));
#287251=CARTESIAN_POINT('Ctrl Pts',(-1.00758916450935,1.18511060639413,
8.05797615331686));
#287252=CARTESIAN_POINT('Ctrl Pts',(-1.02801729112677,1.16747029511556,
8.05993446047416));
#287253=CARTESIAN_POINT('Ctrl Pts',(-1.03925669487236,1.15747653699761,
8.0610323816227));
#287254=CARTESIAN_POINT('Ctrl Pts',(-1.06987351089627,1.12944748090326,
8.06408110609895));
#287255=CARTESIAN_POINT('Ctrl Pts',(-1.0889373863849,1.11107882622648,8.06604538081485));
#287256=CARTESIAN_POINT('Ctrl Pts',(-1.15188035877378,1.04725480346682,
8.07276042185629));
#287257=CARTESIAN_POINT('Ctrl Pts',(-1.19345259803146,0.999620106691458,
8.07759476834797));
#287258=CARTESIAN_POINT('Ctrl Pts',(-1.29219645310379,0.871509226434835,
8.09009538011309));
#287259=CARTESIAN_POINT('Ctrl Pts',(-1.34482501263367,0.787875389821688,
8.09781153203347));
#287260=CARTESIAN_POINT('Ctrl Pts',(-1.39839427240826,0.681537055315809,
8.10675293324725));
#287261=CARTESIAN_POINT('Ctrl Pts',(-1.40724282557082,0.663073927503623,
8.10827520824093));
#287262=CARTESIAN_POINT('Ctrl Pts',(-1.419116621202,0.63698923790651,8.1103788183201));
#287263=CARTESIAN_POINT('Ctrl Pts',(-1.42244962090517,0.629511205367611,
8.11097655834293));
#287264=CARTESIAN_POINT('Ctrl Pts',(-1.42795877747326,0.616883478913417,
8.11197657550083));
#287265=CARTESIAN_POINT('Ctrl Pts',(-1.43016646545815,0.61174780908894,
8.11238069557206));
#287266=CARTESIAN_POINT('Ctrl Pts',(-1.43469800364895,0.601047625838393,
8.11321717362903));
#287267=CARTESIAN_POINT('Ctrl Pts',(-1.43701725409301,0.595481338882939,
8.11364926039198));
#287268=CARTESIAN_POINT('Ctrl Pts',(-1.44310041794644,0.58063899370963,
8.11479367197184));
#287269=CARTESIAN_POINT('Ctrl Pts',(-1.44680733610097,0.571339656755301,
8.11550269843994));
#287270=CARTESIAN_POINT('Ctrl Pts',(-1.46482332166732,0.524843930637855,
8.11901123415298));
#287271=CARTESIAN_POINT('Ctrl Pts',(-1.47779032283321,0.487139524542371,
8.1217407347615));
#287272=CARTESIAN_POINT('Ctrl Pts',(-1.53312829995789,0.303577830989263,
8.1346691234551));
#287273=CARTESIAN_POINT('Ctrl Pts',(-1.55543186361473,0.152555481804566,
8.14431660589831));
#287274=CARTESIAN_POINT('Ctrl Pts',(-1.55549984414273,0.000696327469871839,
8.15470034727716));
#287275=CARTESIAN_POINT('',(-1.55550041530219,0.000134622242225962,9.55740376032212));
#287276=CARTESIAN_POINT('Ctrl Pts',(-1.55549984491818,0.000694593054951367,
8.15470046587205));
#287277=CARTESIAN_POINT('Ctrl Pts',(-1.55550789932647,-0.0173427753760322,
8.15593381561504));
#287278=CARTESIAN_POINT('Ctrl Pts',(-1.55520221524335,-0.0353784498513321,
8.15717529386514));
#287279=CARTESIAN_POINT('Ctrl Pts',(-1.55407751783141,-0.0681180456271037,
8.15944677560594));
#287280=CARTESIAN_POINT('Ctrl Pts',(-1.55336320788016,-0.0828234183071387,
8.16047359035147));
#287281=CARTESIAN_POINT('Ctrl Pts',(-1.55183252403885,-0.107191674461253,
8.16218719584306));
#287282=CARTESIAN_POINT('Ctrl Pts',(-1.55113432076261,-0.116861238739419,
8.16287032808959));
#287283=CARTESIAN_POINT('Ctrl Pts',(-1.54958746702436,-0.135815496798352,
8.16421594324766));
#287284=CARTESIAN_POINT('Ctrl Pts',(-1.54874563751119,-0.145100346403286,
8.16487818631273));
#287285=CARTESIAN_POINT('Ctrl Pts',(-1.54677937881439,-0.164814536897871,
8.16629115273489));
#287286=CARTESIAN_POINT('Ctrl Pts',(-1.54563281818133,-0.175241147263789,
8.16704253907163));
#287287=CARTESIAN_POINT('Ctrl Pts',(-1.54242831844991,-0.201897928479157,
8.1689744158036));
#287288=CARTESIAN_POINT('Ctrl Pts',(-1.54021966572537,-0.218108308930377,
8.17015957596642));
#287289=CARTESIAN_POINT('Ctrl Pts',(-1.52994400754783,-0.285555100941246,
8.17513580191733));
#287290=CARTESIAN_POINT('Ctrl Pts',(-1.51957346751206,-0.336401149508222,
8.17899776991617));
#287291=CARTESIAN_POINT('Ctrl Pts',(-1.48985770269308,-0.452202683826596,
8.18805121703722));
#287292=CARTESIAN_POINT('Ctrl Pts',(-1.46876949574899,-0.516602353441209,
8.19328085267065));
#287293=CARTESIAN_POINT('Ctrl Pts',(-1.41043894159779,-0.661926396868684,
8.20542274563435));
#287294=CARTESIAN_POINT('Ctrl Pts',(-1.37030552364181,-0.741451667115688,
8.2123306731396));
#287295=CARTESIAN_POINT('Ctrl Pts',(-1.31681441785143,-0.828098144743771,
8.21988540359756));
#287296=CARTESIAN_POINT('Ctrl Pts',(-1.30989947395352,-0.838993531187833,
8.22083570997917));
#287297=CARTESIAN_POINT('Ctrl Pts',(-1.29921975718629,-0.855366829972393,
8.22226287435499));
#287298=CARTESIAN_POINT('Ctrl Pts',(-1.29555435560631,-0.860908419824876,
8.2227457374602));
#287299=CARTESIAN_POINT('Ctrl Pts',(-1.28879133369826,-0.870992175824483,
8.2236238340034));
#287300=CARTESIAN_POINT('Ctrl Pts',(-1.2857050757125,-0.875541508126171,
8.22401976053202));
#287301=CARTESIAN_POINT('Ctrl Pts',(-1.27859092378134,-0.885909461752462,
8.22492162905039));
#287302=CARTESIAN_POINT('Ctrl Pts',(-1.27454737289478,-0.891717065127561,
8.22542651381292));
#287303=CARTESIAN_POINT('Ctrl Pts',(-1.26173412767695,-0.909855030229361,
8.22700310585555));
#287304=CARTESIAN_POINT('Ctrl Pts',(-1.25282375534327,-0.922085607569688,
8.22806587248533));
#287305=CARTESIAN_POINT('Ctrl Pts',(-1.19475916485722,-0.999390457200208,
8.23479492143033));
#287306=CARTESIAN_POINT('Ctrl Pts',(-1.14072354820114,-1.06065267076033,
8.24018524836666));
#287307=CARTESIAN_POINT('Ctrl Pts',(-1.02428064791024,-1.17341960409298,
8.25086293022408));
#287308=CARTESIAN_POINT('Ctrl Pts',(-0.962176487646554,-1.22485911072379,
8.25613659489299));
#287309=CARTESIAN_POINT('Ctrl Pts',(-0.85938465009403,-1.29733822138711,
8.26461426825687));
#287310=CARTESIAN_POINT('Ctrl Pts',(-0.821280375199611,-1.32178907331104,
8.26770735680118));
#287311=CARTESIAN_POINT('Ctrl Pts',(-0.768991019466856,-1.35220761261962,
8.27192362055029));
#287312=CARTESIAN_POINT('Ctrl Pts',(-0.755703274372199,-1.35967832514947,
8.27299262245724));
#287313=CARTESIAN_POINT('Ctrl Pts',(-0.73329318486691,-1.37184787549385,
8.27479271996333));
#287314=CARTESIAN_POINT('Ctrl Pts',(-0.724230075700085,-1.37665401491575,
8.27551996227547));
#287315=CARTESIAN_POINT('Ctrl Pts',(-0.706257365825941,-1.3859582917455,
8.27696101693094));
#287316=CARTESIAN_POINT('Ctrl Pts',(-0.697350690679561,-1.39046102386508,
8.27767462457068));
#287317=CARTESIAN_POINT('Ctrl Pts',(-0.677576600253739,-1.40021995392109,
8.27925808608104));
#287318=CARTESIAN_POINT('Ctrl Pts',(-0.666690180041657,-1.40543593135386,
8.28012928626409));
#287319=CARTESIAN_POINT('Ctrl Pts',(-0.629052693515328,-1.42293337402991,
8.28314005458366));
#287320=CARTESIAN_POINT('Ctrl Pts',(-0.602015903255887,-1.43458123279422,
8.28530088053537));
#287321=CARTESIAN_POINT('Ctrl Pts',(-0.465104128100968,-1.48901298903855,
8.2962403884792));
#287322=CARTESIAN_POINT('Ctrl Pts',(-0.350959888586336,-1.51996699525761,
8.30539361817135));
#287323=CARTESIAN_POINT('Ctrl Pts',(-0.186788787898854,-1.54499634215574,
8.31825302904556));
#287324=CARTESIAN_POINT('Ctrl Pts',(-0.138821582300288,-1.55004287622289,
8.32196849289158));
#287325=CARTESIAN_POINT('Ctrl Pts',(-0.0723439043108329,-1.55392551594971,
8.32700493941629));
#287326=CARTESIAN_POINT('Ctrl Pts',(-0.0539746445923887,-1.55467197642273,
8.32838467067837));
#287327=CARTESIAN_POINT('Ctrl Pts',(-0.0218890474583254,-1.55540640586726,
8.33076924654886));
#287328=CARTESIAN_POINT('Ctrl Pts',(-0.0081783201653691,-1.55553893141146,
8.33178012429151));
#287329=CARTESIAN_POINT('Ctrl Pts',(0.0123379068037048,-1.5554659538887,
8.33327895178847));
#287330=CARTESIAN_POINT('Ctrl Pts',(0.0191427772446983,-1.55539709283925,
8.33377381204244));
#287331=CARTESIAN_POINT('Ctrl Pts',(0.0314373418294043,-1.55519197984305,
8.33466352279674));
#287332=CARTESIAN_POINT('Ctrl Pts',(0.0369269454464578,-1.55507131791174,
8.3350591872781));
#287333=CARTESIAN_POINT('Ctrl Pts',(0.0493066609723958,-1.5547336165818,
8.33594789664946));
#287334=CARTESIAN_POINT('Ctrl Pts',(0.056196084585162,-1.55449984568892,
8.33644001693328));
#287335=CARTESIAN_POINT('Ctrl Pts',(0.0772349659554132,-1.55364590321822,
8.33793598121373));
#287336=CARTESIAN_POINT('Ctrl Pts',(0.0913781826362051,-1.55287826224807,
8.33893213609745));
#287337=CARTESIAN_POINT('Ctrl Pts',(0.206080142448297,-1.54508006660263,
8.34694835371305));
#287338=CARTESIAN_POINT('Ctrl Pts',(0.305763377152901,-1.52848167420207,
8.35353398011342));
#287339=CARTESIAN_POINT('Ctrl Pts',(0.499790012124531,-1.47641521859007,
8.36675914983694));
#287340=CARTESIAN_POINT('Ctrl Pts',(0.593688804644002,-1.44122234889674,
8.37337290950411));
#287341=CARTESIAN_POINT('Ctrl Pts',(0.70089965393884,-1.38877388193005,
8.3816376002143));
#287342=CARTESIAN_POINT('Ctrl Pts',(0.718087195331355,-1.37996519616769,
8.38298509626837));
#287343=CARTESIAN_POINT('Ctrl Pts',(0.744902065041766,-1.3655858560405,
8.38512576287522));
#287344=CARTESIAN_POINT('Ctrl Pts',(0.754641652658585,-1.36022784167536,
8.385911434107));
#287345=CARTESIAN_POINT('Ctrl Pts',(0.772834740893855,-1.34996378790021,
8.38739490066712));
#287346=CARTESIAN_POINT('Ctrl Pts',(0.781301096684744,-1.34508154165039,
8.3880918155283));
#287347=CARTESIAN_POINT('Ctrl Pts',(0.800297376091972,-1.33388720388864,
8.38967072826186));
#287348=CARTESIAN_POINT('Ctrl Pts',(0.810799595851049,-1.3275296464506,
8.39055434606303));
#287349=CARTESIAN_POINT('Ctrl Pts',(0.83777279452743,-1.31076185302639,
8.39285224675202));
#287350=CARTESIAN_POINT('Ctrl Pts',(0.854124928356442,-1.30016554084484,
8.39427326989057));
#287351=CARTESIAN_POINT('Ctrl Pts',(0.986580949639623,-1.21075577806206,
8.40602053909226));
#287352=CARTESIAN_POINT('Ctrl Pts',(1.0917106366282,-1.11688086927927,8.41694725144853));
#287353=CARTESIAN_POINT('Ctrl Pts',(1.21001101499556,-0.978370159168645,
8.43102144626592));
#287354=CARTESIAN_POINT('Ctrl Pts',(1.23591920897715,-0.945430590600515,
8.43423753821548));
#287355=CARTESIAN_POINT('Ctrl Pts',(1.27497556301943,-0.891420528739818,
8.43926596791238));
#287356=CARTESIAN_POINT('Ctrl Pts',(1.28900356018931,-0.871012769643257,
8.44111366988778));
#287357=CARTESIAN_POINT('Ctrl Pts',(1.30721427303261,-0.843115791546194,
8.44356148666245));
#287358=CARTESIAN_POINT('Ctrl Pts',(1.31183024314161,-0.835915555375306,
8.44418646337852));
#287359=CARTESIAN_POINT('Ctrl Pts',(1.31943202967484,-0.823839817605614,
8.44522286413904));
#287360=CARTESIAN_POINT('Ctrl Pts',(1.32245072723011,-0.818985350292293,
8.4456363638395));
#287361=CARTESIAN_POINT('Ctrl Pts',(1.32854745899736,-0.809059385910118,
8.44647531519638));
#287362=CARTESIAN_POINT('Ctrl Pts',(1.33162335783473,-0.803986739181109,
8.44690063258554));
#287363=CARTESIAN_POINT('Ctrl Pts',(1.33958195959829,-0.790690763075715,
8.44800685852535));
#287364=CARTESIAN_POINT('Ctrl Pts',(1.34441807327124,-0.78243962434958,
8.44868484839293));
#287365=CARTESIAN_POINT('Ctrl Pts',(1.36466579533613,-0.747151906283429,
8.45155076805521));
#287366=CARTESIAN_POINT('Ctrl Pts',(1.37934146314878,-0.719698658256215,
8.45369714682017));
#287367=CARTESIAN_POINT('Ctrl Pts',(1.43321319824275,-0.611212154762289,
8.461933278924));
#287368=CARTESIAN_POINT('Ctrl Pts',(1.46617350063791,-0.527274455043451,
8.46779373993058));
#287369=CARTESIAN_POINT('Ctrl Pts',(1.51300475933065,-0.368849314355551,
8.47868795308771));
#287370=CARTESIAN_POINT('Ctrl Pts',(1.52906075300844,-0.295304345720388,
8.48368357691161));
#287371=CARTESIAN_POINT('Ctrl Pts',(1.54356074658807,-0.194231487423029,
8.49068590181256));
#287372=CARTESIAN_POINT('Ctrl Pts',(1.54669217211062,-0.167477834887401,
8.49255144384527));
#287373=CARTESIAN_POINT('Ctrl Pts',(1.55026778747953,-0.128097949607766,
8.49532217538646));
#287374=CARTESIAN_POINT('Ctrl Pts',(1.55125536968243,-0.115525144391394,
8.49621045429779));
#287375=CARTESIAN_POINT('Ctrl Pts',(1.5527389743589,-0.093156364518863,
8.49779803313694));
#287376=CARTESIAN_POINT('Ctrl Pts',(1.55329543336722,-0.0833649769455995,
8.49849540534467));
#287377=CARTESIAN_POINT('Ctrl Pts',(1.55427543747475,-0.0626675819157516,
8.49997503075666));
#287378=CARTESIAN_POINT('Ctrl Pts',(1.55467685939939,-0.0517611144316235,
8.50075793747042));
#287379=CARTESIAN_POINT('Ctrl Pts',(1.55544559298367,-0.0225002465624098,
8.50286748907059));
#287380=CARTESIAN_POINT('Ctrl Pts',(1.55560278968477,-0.00414258205714366,
8.50420059104922));
#287381=CARTESIAN_POINT('Ctrl Pts',(1.55463357602343,0.101926799566723,
8.51196198292895));
#287382=CARTESIAN_POINT('Ctrl Pts',(1.54641432805462,0.189400200672458,
8.51860848978389));
#287383=CARTESIAN_POINT('Ctrl Pts',(1.51909684984382,0.341084462446118,
8.53049728121093));
#287384=CARTESIAN_POINT('Ctrl Pts',(1.50314530908757,0.405645059236957,
8.53567384546174));
#287385=CARTESIAN_POINT('Ctrl Pts',(1.4721060671133,0.503802815110005,8.54360586213524));
#287386=CARTESIAN_POINT('Ctrl Pts',(1.45987363367625,0.538221958689364,
8.54639856521226));
#287387=CARTESIAN_POINT('Ctrl Pts',(1.43813562604342,0.593174403285674,
8.55084575647337));
#287388=CARTESIAN_POINT('Ctrl Pts',(1.42937433132269,0.61398624621075,8.55252717964612));
#287389=CARTESIAN_POINT('Ctrl Pts',(1.41679015050072,0.642148150083101,
8.55479173543142));
#287390=CARTESIAN_POINT('Ctrl Pts',(1.41335763392529,0.64966821068319,8.5553953764301));
#287391=CARTESIAN_POINT('Ctrl Pts',(1.40747384319376,0.662291228272542,
8.55640641090681));
#287392=CARTESIAN_POINT('Ctrl Pts',(1.40505439815322,0.667408744921052,
8.55681567153365));
#287393=CARTESIAN_POINT('Ctrl Pts',(1.40000407879043,0.677941793140445,
8.55765658133414));
#287394=CARTESIAN_POINT('Ctrl Pts',(1.3973696222168,0.683355425621348,8.55808800858732));
#287395=CARTESIAN_POINT('Ctrl Pts',(1.39029055462063,0.697690305206675,
8.55922870305827));
#287396=CARTESIAN_POINT('Ctrl Pts',(1.38579142696881,0.706584547595514,
8.55993470965056));
#287397=CARTESIAN_POINT('Ctrl Pts',(1.36497523401698,0.746771931834281,
8.5631195439091));
#287398=CARTESIAN_POINT('Ctrl Pts',(1.34768023294315,0.777550098557509,
8.56554445887448));
#287399=CARTESIAN_POINT('Ctrl Pts',(1.27824321606583,0.891830634970399,
8.57459670166496));
#287400=CARTESIAN_POINT('Ctrl Pts',(1.21926362112187,0.970910193946696,
8.58097414490483));
#287401=CARTESIAN_POINT('Ctrl Pts',(1.11869031000628,1.08201518316962,8.59089288868535));
#287402=CARTESIAN_POINT('Ctrl Pts',(1.08231164326513,1.11840321165451,8.59432511128414));
#287403=CARTESIAN_POINT('Ctrl Pts',(1.02691804581631,1.16857315893815,8.59941148175886));
#287404=CARTESIAN_POINT('Ctrl Pts',(1.00928724422376,1.18383405482935,8.60101126459226));
#287405=CARTESIAN_POINT('Ctrl Pts',(0.976648320505758,1.21082650637596,
8.60394529911898));
#287406=CARTESIAN_POINT('Ctrl Pts',(0.961754856679362,1.22268978533247,
8.6052741872532));
#287407=CARTESIAN_POINT('Ctrl Pts',(0.937873092328922,1.24100628676697,
8.60739203540446));
#287408=CARTESIAN_POINT('Ctrl Pts',(0.929026930832726,1.24764237325617,
8.60817376911543));
#287409=CARTESIAN_POINT('Ctrl Pts',(0.912224438010216,1.25996924476657,
8.60965392979712));
#287410=CARTESIAN_POINT('Ctrl Pts',(0.904283681356347,1.26568042517313,
8.61035151946417));
#287411=CARTESIAN_POINT('Ctrl Pts',(0.88618340533644,1.27844128805939,8.61193761119209));
#287412=CARTESIAN_POINT('Ctrl Pts',(0.875992734348781,1.28544539669486,
8.61282779399249));
#287413=CARTESIAN_POINT('Ctrl Pts',(0.849278497968918,1.30334105688226,
8.61515472024469));
#287414=CARTESIAN_POINT('Ctrl Pts',(0.832629135382617,1.31403977634249,
8.6165984913052));
#287415=CARTESIAN_POINT('Ctrl Pts',(0.697553084560162,1.39724047358835,
8.62826538245604));
#287416=CARTESIAN_POINT('Ctrl Pts',(0.570125491654899,1.45389208150353,
8.6390735936983));
#287417=CARTESIAN_POINT('Ctrl Pts',(0.381753700185515,1.5090221115347,8.65424259549516));
#287418=CARTESIAN_POINT('Ctrl Pts',(0.325734187225226,1.52209797177998,
8.65864752384775));
#287419=CARTESIAN_POINT('Ctrl Pts',(0.255152161441555,1.53449619624826,
8.66397636768922));
#287420=CARTESIAN_POINT('Ctrl Pts',(0.241156642648422,1.53675785767554,
8.6650222409215));
#287421=CARTESIAN_POINT('Ctrl Pts',(0.220309776059693,1.5398348621197,8.66656226798937));
#287422=CARTESIAN_POINT('Ctrl Pts',(0.213481236270425,1.5407964066184,8.66706388033754));
#287423=CARTESIAN_POINT('Ctrl Pts',(0.201204049630122,1.54244200254902,
8.66796038657841));
#287424=CARTESIAN_POINT('Ctrl Pts',(0.195757964186956,1.54314264505527,
8.6683561615325));
#287425=CARTESIAN_POINT('Ctrl Pts',(0.1835565293768,1.54464673160189,8.66923860614164));
#287426=CARTESIAN_POINT('Ctrl Pts',(0.176799509071621,1.54543471656513,
8.66972441757734));
#287427=CARTESIAN_POINT('Ctrl Pts',(0.156421548857741,1.54767573531601,
8.67118147184432));
#287428=CARTESIAN_POINT('Ctrl Pts',(0.142785931209658,1.54899325183235,
8.67214559580656));
#287429=CARTESIAN_POINT('Ctrl Pts',(0.0240229169080802,1.55888683988535,
8.68046273685936));
#287430=CARTESIAN_POINT('Ctrl Pts',(-0.0817228579438755,1.55693077959304,
8.68733513725257));
#287431=CARTESIAN_POINT('Ctrl Pts',(-0.268925198803245,1.53432641936511,
8.69975312058207));
#287432=CARTESIAN_POINT('Ctrl Pts',(-0.350442402690428,1.51778336001912,
8.70524861461504));
#287433=CARTESIAN_POINT('Ctrl Pts',(-0.456504556424705,1.48725604946076,
8.71281404820483));
#287434=CARTESIAN_POINT('Ctrl Pts',(-0.482559388059072,1.47900752154215,
8.71470617284041));
#287435=CARTESIAN_POINT('Ctrl Pts',(-0.520367358752097,1.46593276970139,
8.71750888924652));
#287436=CARTESIAN_POINT('Ctrl Pts',(-0.532301083738477,1.46164175251112,
8.71840199064116));
#287437=CARTESIAN_POINT('Ctrl Pts',(-0.55337589662852,1.45377154672822,
8.71999495598603));
#287438=CARTESIAN_POINT('Ctrl Pts',(-0.562538185983711,1.45025079703295,
8.72069284375275));
#287439=CARTESIAN_POINT('Ctrl Pts',(-0.581781212988799,1.44264658080963,
8.72217020973442));
#287440=CARTESIAN_POINT('Ctrl Pts',(-0.591853629546439,1.43854364097082,
8.72295031184206));
#287441=CARTESIAN_POINT('Ctrl Pts',(-0.618645656081329,1.42730105697286,
8.72504404333851));
#287442=CARTESIAN_POINT('Ctrl Pts',(-0.635284050530813,1.41997354839179,
8.72636396175765));
#287443=CARTESIAN_POINT('Ctrl Pts',(-0.724744393648343,1.37868841794125,
8.73357123115145));
#287444=CARTESIAN_POINT('Ctrl Pts',(-0.794968748179386,1.33942413747065,
8.73963931795514));
#287445=CARTESIAN_POINT('Ctrl Pts',(-0.937779908103882,1.24437575792694,
8.75283722603123));
#287446=CARTESIAN_POINT('Ctrl Pts',(-1.00912732119861,1.18725063529203,
8.75997645945678));
#287447=CARTESIAN_POINT('Ctrl Pts',(-1.10295736605274,1.0975224650092,8.76989314995933));
#287448=CARTESIAN_POINT('Ctrl Pts',(-1.12985742006599,1.0698099378153,8.77280589558643));
#287449=CARTESIAN_POINT('Ctrl Pts',(-1.16233838856556,1.0337543563618,8.77638399635461));
#287450=CARTESIAN_POINT('Ctrl Pts',(-1.16890568760591,1.02632261301053,
8.77711076706121));
#287451=CARTESIAN_POINT('Ctrl Pts',(-1.17933783730091,1.0142872522371,8.77826992712943));
#287452=CARTESIAN_POINT('Ctrl Pts',(-1.18324773225751,1.0097233145516,8.77870545473933));
#287453=CARTESIAN_POINT('Ctrl Pts',(-1.19075037221299,1.00086221388954,
8.77954309742359));
#287454=CARTESIAN_POINT('Ctrl Pts',(-1.19434649017885,0.996568152637631,
8.7799454396193));
#287455=CARTESIAN_POINT('Ctrl Pts',(-1.20233871083706,0.98691938397058,
8.78084176798652));
#287456=CARTESIAN_POINT('Ctrl Pts',(-1.20672245168547,0.981554468899952,
8.78133488193624));
#287457=CARTESIAN_POINT('Ctrl Pts',(-1.22188528180436,0.962742749985558,
8.78304642720241));
#287458=CARTESIAN_POINT('Ctrl Pts',(-1.23247710915692,0.949145659971507,
8.78425260627023));
#287459=CARTESIAN_POINT('Ctrl Pts',(-1.30389110065943,0.854257197454036,
8.79248184156941));
#287460=CARTESIAN_POINT('Ctrl Pts',(-1.35686107882212,0.767346663813942,
8.79909480062707));
#287461=CARTESIAN_POINT('Ctrl Pts',(-1.43592233579858,0.603466613057719,
8.81108054674577));
#287462=CARTESIAN_POINT('Ctrl Pts',(-1.46518769883072,0.528458079462683,
8.81640542802211));
#287463=CARTESIAN_POINT('Ctrl Pts',(-1.49658769105761,0.424943899054878,
8.82381653768517));
#287464=CARTESIAN_POINT('Ctrl Pts',(-1.5039378269491,0.398149324621662,
8.82573942539005));
#287465=CARTESIAN_POINT('Ctrl Pts',(-1.51361151957026,0.358780277640172,
8.82857911276239));
#287466=CARTESIAN_POINT('Ctrl Pts',(-1.5165040808245,0.346350220762187,
8.82947773903295));
#287467=CARTESIAN_POINT('Ctrl Pts',(-1.52135229534149,0.324289964423222,
8.83107690729861));
#287468=CARTESIAN_POINT('Ctrl Pts',(-1.52337028038935,0.314674066788449,
8.83177541749129));
#287469=CARTESIAN_POINT('Ctrl Pts',(-1.52742165169151,0.294415915114111,
8.8332503521401));
#287470=CARTESIAN_POINT('Ctrl Pts',(-1.5294352057216,0.283770283209744,
8.83402736751941));
#287471=CARTESIAN_POINT('Ctrl Pts',(-1.5344949024693,0.255399838837611,
8.83610370420844));
#287472=CARTESIAN_POINT('Ctrl Pts',(-1.53734504865251,0.237642240322826,
8.83740913182853));
#287473=CARTESIAN_POINT('Ctrl Pts',(-1.55034894906355,0.146555351651667,
8.844137688748));
#287474=CARTESIAN_POINT('Ctrl Pts',(-1.55556494302191,0.0726289945413549,
8.84971241101516));
#287475=CARTESIAN_POINT('Ctrl Pts',(-1.55545559872507,-0.0508161200096765,
8.8591839896776));
#287476=CARTESIAN_POINT('Ctrl Pts',(-1.55305489340057,-0.100222515723241,
8.86301643856976));
#287477=CARTESIAN_POINT('Ctrl Pts',(-1.54079505185045,-0.227252872359269,
8.87291270117633));
#287478=CARTESIAN_POINT('Ctrl Pts',(-1.52742644059319,-0.304407879625256,
8.87896817315404));
#287479=CARTESIAN_POINT('Ctrl Pts',(-1.50463960339592,-0.394797945060312,
8.88591181063912));
#287480=CARTESIAN_POINT('Ctrl Pts',(-1.50075795258871,-0.409305955730549,
8.88702133829879));
#287481=CARTESIAN_POINT('Ctrl Pts',(-1.49473726770902,-0.430570444029356,
8.88863806432052));
#287482=CARTESIAN_POINT('Ctrl Pts',(-1.49276135315609,-0.437371643462518,
8.88915371062199));
#287483=CARTESIAN_POINT('Ctrl Pts',(-1.48916679969669,-0.4494361014576,
8.89006554240398));
#287484=CARTESIAN_POINT('Ctrl Pts',(-1.48756658044811,-0.454704562127828,
8.89046274207021));
#287485=CARTESIAN_POINT('Ctrl Pts',(-1.48400217523509,-0.466219546884688,
8.8913286712128));
#287486=CARTESIAN_POINT('Ctrl Pts',(-1.48202649345555,-0.472462272430623,
8.89179673404072));
#287487=CARTESIAN_POINT('Ctrl Pts',(-1.47618525454244,-0.490522092497547,
8.89314728161087));
#287488=CARTESIAN_POINT('Ctrl Pts',(-1.47221725523811,-0.502305890862283,
8.89402409831666));
#287489=CARTESIAN_POINT('Ctrl Pts',(-1.44026567050328,-0.593560001747837,
8.90078925802264));
#287490=CARTESIAN_POINT('Ctrl Pts',(-1.40600423576108,-0.67069733572262,
8.9063642692095));
#287491=CARTESIAN_POINT('Ctrl Pts',(-1.31084544323477,-0.845205587778962,
8.91946061275635));
#287492=CARTESIAN_POINT('Ctrl Pts',(-1.24511116240763,-0.93935236463195,
8.92694386450749));
#287493=CARTESIAN_POINT('Ctrl Pts',(-1.15648847941476,-1.04043885966709,
8.93621673542934));
#287494=CARTESIAN_POINT('Ctrl Pts',(-1.14304362355007,-1.05519184816699,
8.9376040974822));
#287495=CARTESIAN_POINT('Ctrl Pts',(-1.1207818101676,-1.07869481768303,
8.93987352530442));
#287496=CARTESIAN_POINT('Ctrl Pts',(-1.1121371096373,-1.08760535543687,
8.94074829579854));
#287497=CARTESIAN_POINT('Ctrl Pts',(-1.09648909755583,-1.10335292430509,
8.94232093749023));
#287498=CARTESIAN_POINT('Ctrl Pts',(-1.08952609157742,-1.11022921255347,
8.94301701640312));
#287499=CARTESIAN_POINT('Ctrl Pts',(-1.07457941684572,-1.1247137155052,
8.94450371394265));
#287500=CARTESIAN_POINT('Ctrl Pts',(-1.06657882820045,-1.13230360618835,
8.94529507362878));
#287501=CARTESIAN_POINT('Ctrl Pts',(-1.04465267493276,-1.15266563746746,
8.9474524260925));
#287502=CARTESIAN_POINT('Ctrl Pts',(-1.03057440483791,-1.16526976308204,
8.94882539481354));
#287503=CARTESIAN_POINT('Ctrl Pts',(-0.936382059385998,-1.24655694697754,
8.95793631250069));
#287504=CARTESIAN_POINT('Ctrl Pts',(-0.849700825360943,-1.30717863360615,
8.96599879509881));
#287505=CARTESIAN_POINT('Ctrl Pts',(-0.674056926382212,-1.4051230872358,
8.98157838686325));
#287506=CARTESIAN_POINT('Ctrl Pts',(-0.586419684209652,-1.44389706417766,
8.98903648189428));
#287507=CARTESIAN_POINT('Ctrl Pts',(-0.482044933432753,-1.47899378079796,
8.99722908585923));
#287508=CARTESIAN_POINT('Ctrl Pts',(-0.468255611205701,-1.48341721845791,
8.99829784352748));
#287509=CARTESIAN_POINT('Ctrl Pts',(-0.447755222496817,-1.48967911608659,
8.99986473128859));
#287510=CARTESIAN_POINT('Ctrl Pts',(-0.441090837923369,-1.49166601015651,
9.00037068809168));
#287511=CARTESIAN_POINT('Ctrl Pts',(-0.429139527054664,-1.49514202683466,
9.00127165087781));
#287512=CARTESIAN_POINT('Ctrl Pts',(-0.423857813767576,-1.49664791139053,
9.00166758078572));
#287513=CARTESIAN_POINT('Ctrl Pts',(-0.412068493232733,-1.49994178134671,
9.00254636574887));
#287514=CARTESIAN_POINT('Ctrl Pts',(-0.405557120928173,-1.50171542469041,
9.00302840265932));
#287515=CARTESIAN_POINT('Ctrl Pts',(-0.386059649779417,-1.50689030643539,
9.00446245463701));
#287516=CARTESIAN_POINT('Ctrl Pts',(-0.373040440789776,-1.51016598763882,
9.00540767773905));
#287517=CARTESIAN_POINT('Ctrl Pts',(-0.276239289390641,-1.53319320803928,
9.01235569803947));
#287518=CARTESIAN_POINT('Ctrl Pts',(-0.190977073683469,-1.54613115934851,
9.01803824575437));
#287519=CARTESIAN_POINT('Ctrl Pts',(0.00526735481943303,-1.55941752721037,
9.03099179324028));
#287520=CARTESIAN_POINT('Ctrl Pts',(0.116075057310498,-1.55509929444758,
9.03823470341701));
#287521=CARTESIAN_POINT('Ctrl Pts',(0.245472384173217,-1.5361418286467,
9.04725229260812));
#287522=CARTESIAN_POINT('Ctrl Pts',(0.265402162241918,-1.53282420298211,
9.04865620854486));
#287523=CARTESIAN_POINT('Ctrl Pts',(0.297534359347984,-1.52682986439947,
9.05094726526467));
#287524=CARTESIAN_POINT('Ctrl Pts',(0.309779460582336,-1.52439260017255,
9.05182687428356));
#287525=CARTESIAN_POINT('Ctrl Pts',(0.331574715545322,-1.51978102559053,
9.05340483923315));
#287526=CARTESIAN_POINT('Ctrl Pts',(0.341136281786932,-1.51766339712417,
9.05410135441048));
#287527=CARTESIAN_POINT('Ctrl Pts',(0.36137980920108,-1.51297903717607,
9.05558538630136));
#287528=CARTESIAN_POINT('Ctrl Pts',(0.372055801783793,-1.51038915592122,
9.05637361189284));
#287529=CARTESIAN_POINT('Ctrl Pts',(0.400824203664722,-1.50308673584154,
9.05851321757652));
#287530=CARTESIAN_POINT('Ctrl Pts',(0.418860021404101,-1.49816087374273,
9.05987137903083));
#287531=CARTESIAN_POINT('Ctrl Pts',(0.458661291428838,-1.48651565897887,
9.06290725528484));
#287532=CARTESIAN_POINT('Ctrl Pts',(0.480376406638293,-1.47964096791976,
9.06458964514343));
#287533=CARTESIAN_POINT('Ctrl Pts',(0.548845831861736,-1.45629847076299,
9.0699788135836));
#287534=CARTESIAN_POINT('Ctrl Pts',(0.594964248751368,-1.43807290661367,
9.07373676694237));
#287535=CARTESIAN_POINT('Ctrl Pts',(0.680172577348673,-1.39959844174086,
9.08090911479182));
#287536=CARTESIAN_POINT('Ctrl Pts',(0.719429430918415,-1.37983026599528,
9.08431073520318));
#287537=CARTESIAN_POINT('Ctrl Pts',(0.831416159786573,-1.31735875548053,
9.09425416416553));
#287538=CARTESIAN_POINT('Ctrl Pts',(0.901583456898515,-1.27036881126108,
9.10079992945036));
#287539=CARTESIAN_POINT('Ctrl Pts',(0.979362171192709,-1.20857585190162,
9.10819715770035));
#287540=CARTESIAN_POINT('Ctrl Pts',(0.990987156479298,-1.19906228034851,
9.10930655468245));
#287541=CARTESIAN_POINT('Ctrl Pts',(1.00786813627616,-1.18483410405858,
9.11092098686409));
#287542=CARTESIAN_POINT('Ctrl Pts',(1.01323234630829,-1.18025008021331,
9.11143452175219));
#287543=CARTESIAN_POINT('Ctrl Pts',(1.02271934901546,-1.17203054240051,
9.11234339823121));
#287544=CARTESIAN_POINT('Ctrl Pts',(1.02685427425019,-1.16840950088539,
9.11273973804126));
#287545=CARTESIAN_POINT('Ctrl Pts',(1.03595766139387,-1.1603518164743,9.11361275820906));
#287546=CARTESIAN_POINT('Ctrl Pts',(1.04091690355532,-1.15590510789968,
9.11408868597484));
#287547=CARTESIAN_POINT('Ctrl Pts',(1.05546030235224,-1.14269525292822,
9.11548592291274));
#287548=CARTESIAN_POINT('Ctrl Pts',(1.06496375016334,-1.13384352128698,
9.11640094770386));
#287549=CARTESIAN_POINT('Ctrl Pts',(1.12892734049978,-1.07275252073659,
9.12258270795883));
#287550=CARTESIAN_POINT('Ctrl Pts',(1.17964167411803,-1.01672196453946,
9.12760259375878));
#287551=CARTESIAN_POINT('Ctrl Pts',(1.30247235737939,-0.859390027855182,
9.14077559040882));
#287552=CARTESIAN_POINT('Ctrl Pts',(1.36685990545847,-0.752778764298437,
9.14884941363933));
#287553=CARTESIAN_POINT('Ctrl Pts',(1.42572013302073,-0.622305849264656,
9.15873592958155));
#287554=CARTESIAN_POINT('Ctrl Pts',(1.4332271386558,-0.604815990782045,
9.16006023968811));
#287555=CARTESIAN_POINT('Ctrl Pts',(1.44499532662816,-0.575948112668915,
9.16224714112165));
#287556=CARTESIAN_POINT('Ctrl Pts',(1.44944759382522,-0.564649785544136,
9.16310330671459));
#287557=CARTESIAN_POINT('Ctrl Pts',(1.45723963980532,-0.544176617881382,
9.16465579956939));
#287558=CARTESIAN_POINT('Ctrl Pts',(1.46062622350875,-0.535020173938064,
9.16535052078373));
#287559=CARTESIAN_POINT('Ctrl Pts',(1.46771504655266,-0.515284779554326,
9.16684903180084));
#287560=CARTESIAN_POINT('Ctrl Pts',(1.47138956619141,-0.504696536779223,
9.16765369625496));
#287561=CARTESIAN_POINT('Ctrl Pts',(1.48122184527803,-0.475344178389458,
9.16988678856115));
#287562=CARTESIAN_POINT('Ctrl Pts',(1.4871369784435,-0.456501679747827,
9.17132304912216));
#287563=CARTESIAN_POINT('Ctrl Pts',(1.52144092028485,-0.339475245154242,
9.18026432157958));
#287564=CARTESIAN_POINT('Ctrl Pts',(1.54044887664108,-0.238821746275747,
9.18806984095129));
#287565=CARTESIAN_POINT('Ctrl Pts',(1.55805036066665,-0.0398255174791783,
9.20354201709145));
#287566=CARTESIAN_POINT('Ctrl Pts',(1.55748067516752,0.0580012572155893,
9.21116058399213));
#287567=CARTESIAN_POINT('Ctrl Pts',(1.54631385281266,0.169409241380123,
9.2194888158955));
#287568=CARTESIAN_POINT('Ctrl Pts',(1.54468575206923,0.183662703703547,
9.2205473994175));
#287569=CARTESIAN_POINT('Ctrl Pts',(1.54197921662684,0.204764119960254,
9.2221023531579));
#287570=CARTESIAN_POINT('Ctrl Pts',(1.54105188629223,0.211630191640074,
9.22260638542932));
#287571=CARTESIAN_POINT('Ctrl Pts',(1.53930733016324,0.223927109390988,
9.22350536639301));
#287572=CARTESIAN_POINT('Ctrl Pts',(1.53850719155381,0.229360047427546,
9.2239012200487));
#287573=CARTESIAN_POINT('Ctrl Pts',(1.53665607893202,0.241483343524967,
9.22478159245966));
#287574=CARTESIAN_POINT('Ctrl Pts',(1.53559017230701,0.248171185720242,
9.22526527555621));
#287575=CARTESIAN_POINT('Ctrl Pts',(1.53226172003992,0.26821201339908,9.22670933491812));
#287576=CARTESIAN_POINT('Ctrl Pts',(1.52986836143609,0.281543055646231,
9.22766277792094));
#287577=CARTESIAN_POINT('Ctrl Pts',(1.523872505236,0.312602016824603,9.2298710710745));
#287578=CARTESIAN_POINT('Ctrl Pts',(1.5201342272213,0.330302025422514,9.23111954816163));
#287579=CARTESIAN_POINT('Ctrl Pts',(1.5055854065519,0.393697133375123,9.23556833773222));
#287580=CARTESIAN_POINT('Ctrl Pts',(1.49301542596418,0.438965203867435,
9.23870256483593));
#287581=CARTESIAN_POINT('Ctrl Pts',(1.44320280133831,0.591248144581873,
9.24930896669776));
#287582=CARTESIAN_POINT('Ctrl Pts',(1.39634062154498,0.694723156850064,
9.25665074390169));
#287583=CARTESIAN_POINT('Ctrl Pts',(1.32130906296903,0.821512875097195,
9.26667267481212));
#287584=CARTESIAN_POINT('Ctrl Pts',(1.30300006271734,0.850253840643107,
9.26901771711631));
#287585=CARTESIAN_POINT('Ctrl Pts',(1.27578285860249,0.89003262793136,9.2723840879517));
#287586=CARTESIAN_POINT('Ctrl Pts',(1.26764401822494,0.901586712954113,
9.27337684839587));
#287587=CARTESIAN_POINT('Ctrl Pts',(1.25351259275861,0.921078337115501,
9.27507834237803));
#287588=CARTESIAN_POINT('Ctrl Pts',(1.24759914577311,0.929072379543192,
9.27578400964369));
#287589=CARTESIAN_POINT('Ctrl Pts',(1.23540005641152,0.945237118723911,
9.27722735330804));
#287590=CARTESIAN_POINT('Ctrl Pts',(1.22910903178765,0.953403109143462,
9.27796521689099));
#287591=CARTESIAN_POINT('Ctrl Pts',(1.21316389620452,0.973680381061063,
9.2798198185778));
#287592=CARTESIAN_POINT('Ctrl Pts',(1.20340938401956,0.985710883445157,
9.28094051350126));
#287593=CARTESIAN_POINT('Ctrl Pts',(1.16302603929184,1.03402375681874,9.28552640879167));
#287594=CARTESIAN_POINT('Ctrl Pts',(1.13092613215031,1.06903690548297,9.28905070695363));
#287595=CARTESIAN_POINT('Ctrl Pts',(1.03489264340217,1.16461346403174,9.29927157467036));
#287596=CARTESIAN_POINT('Ctrl Pts',(0.967355057445862,1.22128967359131,
9.30609817576178));
#287597=CARTESIAN_POINT('Ctrl Pts',(0.837087772050156,1.31299241714589,
9.31844614138079));
#287598=CARTESIAN_POINT('Ctrl Pts',(0.776019212408873,1.34998566256816,
9.32395163925735));
#287599=CARTESIAN_POINT('Ctrl Pts',(0.699170476427338,1.38959343072602,
9.33039078529338));
#287600=CARTESIAN_POINT('Ctrl Pts',(0.685617845643648,1.39633000139551,
9.33150868630128));
#287601=CARTESIAN_POINT('Ctrl Pts',(0.665586009007611,1.40592517429502,
9.33313304221567));
#287602=CARTESIAN_POINT('Ctrl Pts',(0.659182656701938,1.40893880684659,
9.33364814072776));
#287603=CARTESIAN_POINT('Ctrl Pts',(0.64776885286771,1.41421567834306,9.33455867012328));
#287604=CARTESIAN_POINT('Ctrl Pts',(0.642766716140116,1.41649617840138,
9.33495511449354));
#287605=CARTESIAN_POINT('Ctrl Pts',(0.631692865473461,1.4214740624084,9.33582703408055));
#287606=CARTESIAN_POINT('Ctrl Pts',(0.625615862558263,1.42415911444394,
9.33630176960807));
#287607=CARTESIAN_POINT('Ctrl Pts',(0.607687486877178,1.43194365122322,
9.33769188091329));
#287608=CARTESIAN_POINT('Ctrl Pts',(0.595789301424893,1.43693487631924,
9.33860106833154));
#287609=CARTESIAN_POINT('Ctrl Pts',(0.502918919003025,1.47454157886878,
9.34560492749991));
#287610=CARTESIAN_POINT('Ctrl Pts',(0.419381089387667,1.50044135749048,
9.35136624647298));
#287611=CARTESIAN_POINT('Ctrl Pts',(0.226487766854592,1.54286231940791,
9.36437252715744));
#287612=CARTESIAN_POINT('Ctrl Pts',(0.116678221269466,1.55502524433712,
9.37159029038982));
#287613=CARTESIAN_POINT('Ctrl Pts',(-0.0137123308395208,1.55557102222298,
9.38058093610173));
#287614=CARTESIAN_POINT('Ctrl Pts',(-0.0339343744951911,1.55526127293766,
9.38198623677536));
#287615=CARTESIAN_POINT('Ctrl Pts',(-0.0666273556906808,1.55412260523556,
9.3842791019133));
#287616=CARTESIAN_POINT('Ctrl Pts',(-0.0791048237691668,1.55353747534766,
9.38515911467119));
#287617=CARTESIAN_POINT('Ctrl Pts',(-0.101350456054294,1.55222558118922,
9.38673752505595));
#287618=CARTESIAN_POINT('Ctrl Pts',(-0.111121464161474,1.5515566963633,
9.38743407788133));
#287619=CARTESIAN_POINT('Ctrl Pts',(-0.131834230012033,1.54994212576025,
9.38891789371985));
#287620=CARTESIAN_POINT('Ctrl Pts',(-0.142773543295223,1.54897274388154,
9.3897058629668));
#287621=CARTESIAN_POINT('Ctrl Pts',(-0.172289361347515,1.54604189602942,
9.39184401902448));
#287622=CARTESIAN_POINT('Ctrl Pts',(-0.190841759719558,1.54386156589375,
9.3932009714092));
#287623=CARTESIAN_POINT('Ctrl Pts',(-0.314803920101082,1.52702471841547,
9.40235893958102));
#287624=CARTESIAN_POINT('Ctrl Pts',(-0.418489423159696,1.501920196554,9.4104911160021));
#287625=CARTESIAN_POINT('Ctrl Pts',(-0.608357177766115,1.4347507566862,
9.42609442251736));
#287626=CARTESIAN_POINT('Ctrl Pts',(-0.6948480687262,1.39491844748509,9.43350368512298));
#287627=CARTESIAN_POINT('Ctrl Pts',(-0.789771283779657,1.34016910635176,
9.44165728796694));
#287628=CARTESIAN_POINT('Ctrl Pts',(-0.802271966389811,1.33272339468468,
9.44273120997891));
#287629=CARTESIAN_POINT('Ctrl Pts',(-0.820485633861986,1.32152572022651,
9.44429416106357));
#287630=CARTESIAN_POINT('Ctrl Pts',(-0.82628086758431,1.31791002620485,
9.44479119336549));
#287631=CARTESIAN_POINT('Ctrl Pts',(-0.836615876545272,1.31136695837279,
9.44567684195061));
#287632=CARTESIAN_POINT('Ctrl Pts',(-0.8411644329706,1.30845398242295,9.44606634853175));
#287633=CARTESIAN_POINT('Ctrl Pts',(-0.850097735729817,1.30266709905092,
9.44683077419142));
#287634=CARTESIAN_POINT('Ctrl Pts',(-0.854483163905904,1.29979469763431,
9.44720579083778));
#287635=CARTESIAN_POINT('Ctrl Pts',(-0.867930352825474,1.29088948377031,
9.44835523725316));
#287636=CARTESIAN_POINT('Ctrl Pts',(-0.876943623113277,1.28478350555915,
9.44912500378277));
#287637=CARTESIAN_POINT('Ctrl Pts',(-0.93143150457099,1.24703046789405,
9.45377927582328));
#287638=CARTESIAN_POINT('Ctrl Pts',(-0.975258198709604,1.21306330787374,
9.45752690921468));
#287639=CARTESIAN_POINT('Ctrl Pts',(-1.10046609302112,1.10484048345856,
9.46855628744581));
#287640=CARTESIAN_POINT('Ctrl Pts',(-1.17587112179077,1.02421962032387,
9.47566566622093));
#287641=CARTESIAN_POINT('Ctrl Pts',(-1.27067079520889,0.898456128274266,
9.48625767730017));
#287642=CARTESIAN_POINT('Ctrl Pts',(-1.29745878035107,0.859318154727518,
9.4894909768463));
#287643=CARTESIAN_POINT('Ctrl Pts',(-1.3307928331916,0.805495984516705,
9.49389829471147));
#287644=CARTESIAN_POINT('Ctrl Pts',(-1.33896116278301,0.791843619551476,
9.49501292822677));
#287645=CARTESIAN_POINT('Ctrl Pts',(-1.35211810995498,0.769067569125502,
9.49686843918668));
#287646=CARTESIAN_POINT('Ctrl Pts',(-1.35722733700829,0.760014641526437,
9.49760492812731));
#287647=CARTESIAN_POINT('Ctrl Pts',(-1.3670733164703,0.742152827294967,
9.49905642597725));
#287648=CARTESIAN_POINT('Ctrl Pts',(-1.37181661075697,0.733348109364659,
9.49977115720044));
#287649=CARTESIAN_POINT('Ctrl Pts',(-1.38294757765584,0.71220038588984,
9.50148637954612));
#287650=CARTESIAN_POINT('Ctrl Pts',(-1.38925527638184,0.699816508779698,
9.50248962237845));
#287651=CARTESIAN_POINT('Ctrl Pts',(-1.41078930501414,0.65610007401676,
9.50602815580005));
#287652=CARTESIAN_POINT('Ctrl Pts',(-1.42512726145782,0.624344218053379,
9.50859348032644));
#287653=CARTESIAN_POINT('Ctrl Pts',(-1.45851085004043,0.543250538412328,
9.51513643617743));
#287654=CARTESIAN_POINT('Ctrl Pts',(-1.47612825565984,0.493375546600439,
9.51915435051762));
#287655=CARTESIAN_POINT('Ctrl Pts',(-1.52306954352178,0.335262319226742,
9.53183527623317));
#287656=CARTESIAN_POINT('Ctrl Pts',(-1.54326198076776,0.224688153151286,
9.54064684326322));
#287657=CARTESIAN_POINT('Ctrl Pts',(-1.55302328018702,0.090558628642934,
9.55077008522699));
#287658=CARTESIAN_POINT('Ctrl Pts',(-1.5541665917424,0.0681800065310494,
9.55243931009175));
#287659=CARTESIAN_POINT('Ctrl Pts',(-1.55507076579162,0.0374735963420742,
9.55469598994108));
#287660=CARTESIAN_POINT('Ctrl Pts',(-1.55524883532423,0.0291620558589066,
9.55530343709561));
#287661=CARTESIAN_POINT('Ctrl Pts',(-1.55541955031962,0.0164266618512413,
9.55622861817319));
#287662=CARTESIAN_POINT('Ctrl Pts',(-1.55545997167684,0.0120037731757019,
9.55654889399728));
#287663=CARTESIAN_POINT('Ctrl Pts',(-1.55549362403694,0.00509865374687671,
9.55704724459287));
#287664=CARTESIAN_POINT('Ctrl Pts',(-1.55549977947085,0.00261661648208582,
9.55722603653157));
#287665=CARTESIAN_POINT('Ctrl Pts',(-1.55549999418008,0.00013455773656679,
9.55740449471797));
#287666=CARTESIAN_POINT('Ctrl Pts',(-1.55549999416998,0.000134674404654651,
9.55740448632962));
#287667=CARTESIAN_POINT('Ctrl Pts',(-1.55550028275703,-0.00319852879888876,
9.55764414118653));
#287668=CARTESIAN_POINT('Ctrl Pts',(-1.55548985752322,-0.00653175413623187,
9.55788319559715));
#287669=CARTESIAN_POINT('Ctrl Pts',(-1.55542442647104,-0.0168486752841418,
9.55862131983953));
#287670=CARTESIAN_POINT('Ctrl Pts',(-1.55533310121566,-0.0238321943166356,
9.55911841508268));
#287671=CARTESIAN_POINT('Ctrl Pts',(-1.55484660076764,-0.0483852383419172,
9.56085794921163));
#287672=CARTESIAN_POINT('Ctrl Pts',(-1.55420071026617,-0.065949245704217,
9.56208759395479));
#287673=CARTESIAN_POINT('Ctrl Pts',(-1.54805448062489,-0.180281405398427,
9.57001808780353));
#287674=CARTESIAN_POINT('Ctrl Pts',(-1.5338168189047,-0.276378287126682,
9.57634799938035));
#287675=CARTESIAN_POINT('Ctrl Pts',(-1.48751312522304,-0.465165108089252,
9.58914636655361));
#287676=CARTESIAN_POINT('Ctrl Pts',(-1.45546675969386,-0.557392943394599,
9.59559222354331));
#287677=CARTESIAN_POINT('Ctrl Pts',(-1.4067695810451,-0.664058094325602,
9.60370561485795));
#287678=CARTESIAN_POINT('Ctrl Pts',(-1.39818644981023,-0.681944569926769,
9.6050890059814));
#287679=CARTESIAN_POINT('Ctrl Pts',(-1.38421426204623,-0.709688073390144,
9.60727367126598));
#287680=CARTESIAN_POINT('Ctrl Pts',(-1.37905631298897,-0.719659612948166,
9.60806690705878));
#287681=CARTESIAN_POINT('Ctrl Pts',(-1.36921291790003,-0.738194762983717,
9.60955694979241));
#287682=CARTESIAN_POINT('Ctrl Pts',(-1.36455389470005,-0.746771841414218,
9.61025279463671));
#287683=CARTESIAN_POINT('Ctrl Pts',(-1.35393055336266,-0.765897607857494,
9.61181902503619));
#287684=CARTESIAN_POINT('Ctrl Pts',(-1.34792312654067,-0.776421482549624,
9.61269092195181));
#287685=CARTESIAN_POINT('Ctrl Pts',(-1.32991218075718,-0.807134119624555,
9.61526591720306));
#287686=CARTESIAN_POINT('Ctrl Pts',(-1.31757413248082,-0.827121629256503,
9.61698098357961));
#287687=CARTESIAN_POINT('Ctrl Pts',(-1.22124045786773,-0.975553332951358,
9.63002451022965));
#287688=CARTESIAN_POINT('Ctrl Pts',(-1.11910905297119,-1.09119547725724,
9.64207494651825));
#287689=CARTESIAN_POINT('Ctrl Pts',(-0.966342264906726,-1.21979727589253,
9.65740266118593));
#287690=CARTESIAN_POINT('Ctrl Pts',(-0.92961465222333,-1.24801453638141,
9.66091330023262));
#287691=CARTESIAN_POINT('Ctrl Pts',(-0.883131909495307,-1.28053391111836,
9.66510097441098));
#287692=CARTESIAN_POINT('Ctrl Pts',(-0.874524204746792,-1.28642780527455,
9.66586617488866));
#287693=CARTESIAN_POINT('Ctrl Pts',(-0.861533629118204,-1.29513209601409,
9.66700494227328));
#287694=CARTESIAN_POINT('Ctrl Pts',(-0.857195108438537,-1.2980076611573,
9.66738261280559));
#287695=CARTESIAN_POINT('Ctrl Pts',(-0.848450635142817,-1.30374052026392,
9.66813839148692));
#287696=CARTESIAN_POINT('Ctrl Pts',(-0.84404467001667,-1.30659726805992,
9.66851642975427));
#287697=CARTESIAN_POINT('Ctrl Pts',(-0.833789058088379,-1.31317329521972,
9.66939007640199));
#287698=CARTESIAN_POINT('Ctrl Pts',(-0.827928917189494,-1.31687585201734,
9.6698845932109));
#287699=CARTESIAN_POINT('Ctrl Pts',(-0.809227138278142,-1.32851782860721,
9.67144858787554));
#287700=CARTESIAN_POINT('Ctrl Pts',(-0.796294097619465,-1.33630982063883,
9.67250907340737));
#287701=CARTESIAN_POINT('Ctrl Pts',(-0.711245429827733,-1.38587724385318,
9.67936076999321));
#287702=CARTESIAN_POINT('Ctrl Pts',(-0.635975539747113,-1.42199319855628,
9.68486316652766));
#287703=CARTESIAN_POINT('Ctrl Pts',(-0.484166678993637,-1.48035397093751,
9.69557424374132));
#287704=CARTESIAN_POINT('Ctrl Pts',(-0.408106357669183,-1.50310128049723,
9.70076991348448));
#287705=CARTESIAN_POINT('Ctrl Pts',(-0.28680767924149,-1.52948827046994,
9.70913966347121));
#287706=CARTESIAN_POINT('Ctrl Pts',(-0.242580871023528,-1.53712293636007,
9.71220667406262));
#287707=CARTESIAN_POINT('Ctrl Pts',(-0.183013920608756,-1.54477090919968,
9.71639277502204));
#287708=CARTESIAN_POINT('Ctrl Pts',(-0.167911679392819,-1.54648533660861,
9.71745871552899));
#287709=CARTESIAN_POINT('Ctrl Pts',(-0.142587194684603,-1.54898489195791,
9.7192551076888));
#287710=CARTESIAN_POINT('Ctrl Pts',(-0.132377717971789,-1.54989078140122,
9.7199817411418));
#287711=CARTESIAN_POINT('Ctrl Pts',(-0.112203871375268,-1.55148003079474,
9.72142271268743));
#287712=CARTESIAN_POINT('Ctrl Pts',(-0.102240387568914,-1.55216844745509,
9.72213685589999));
#287713=CARTESIAN_POINT('Ctrl Pts',(-0.0801930284376602,-1.55347858851698,
9.72372290994633));
#287714=CARTESIAN_POINT('Ctrl Pts',(-0.0681072447501606,-1.55405535121208,
9.72459618306495));
#287715=CARTESIAN_POINT('Ctrl Pts',(-0.0261057610140671,-1.55556887977297,
9.72764507763219));
#287716=CARTESIAN_POINT('Ctrl Pts',(0.00382758342683263,-1.55578313791769,
9.72984280232344));
#287717=CARTESIAN_POINT('Ctrl Pts',(0.151206225656134,-1.55258499732075,
9.74079278736408));
#287718=CARTESIAN_POINT('Ctrl Pts',(0.267982377506082,-1.53673682528635,
9.74991476694166));
#287719=CARTESIAN_POINT('Ctrl Pts',(0.428458664110106,-1.49610035093421,
9.76273301789542));
#287720=CARTESIAN_POINT('Ctrl Pts',(0.474509705273616,-1.48213839622278,
9.76643971178456));
#287721=CARTESIAN_POINT('Ctrl Pts',(0.537143204565791,-1.45992957982976,
9.77146562513602));
#287722=CARTESIAN_POINT('Ctrl Pts',(0.554334921684502,-1.45348892721974,
9.77284336640256));
#287723=CARTESIAN_POINT('Ctrl Pts',(0.584147358572455,-1.44171414628763,
9.7752248709841));
#287724=CARTESIAN_POINT('Ctrl Pts',(0.596818888367281,-1.4365149023813,
9.77623464742721));
#287725=CARTESIAN_POINT('Ctrl Pts',(0.615678977299141,-1.42848378201638,
9.77773217667228));
#287726=CARTESIAN_POINT('Ctrl Pts',(0.621919909112617,-1.42577773509687,
9.77822682300302));
#287727=CARTESIAN_POINT('Ctrl Pts',(0.63316646840462,-1.42081336738367,
9.77911632509012));
#287728=CARTESIAN_POINT('Ctrl Pts',(0.638178053092129,-1.41856941199675,
9.77951199264671));
#287729=CARTESIAN_POINT('Ctrl Pts',(0.649457053639494,-1.41344732629456,
9.78040092670502));
#287730=CARTESIAN_POINT('Ctrl Pts',(0.655717318166121,-1.41055400896892,
9.78089326634564));
#287731=CARTESIAN_POINT('Ctrl Pts',(0.674789019925197,-1.40158519680976,
9.78239057054935));
#287732=CARTESIAN_POINT('Ctrl Pts',(0.687537243998021,-1.39537588506913,
9.78338782621608));
#287733=CARTESIAN_POINT('Ctrl Pts',(0.790024926813116,-1.34371124855323,
9.79139032860938));
#287734=CARTESIAN_POINT('Ctrl Pts',(0.875259958601092,-1.28981599892396,
9.79796311152944));
#287735=CARTESIAN_POINT('Ctrl Pts',(1.03232468202175,-1.16771266684552,
9.81105993526825));
#287736=CARTESIAN_POINT('Ctrl Pts',(1.1040417640007,-1.10015245984276,9.81755717733517));
#287737=CARTESIAN_POINT('Ctrl Pts',(1.1823535400239,-1.01095805281637,9.8257637803017));
#287738=CARTESIAN_POINT('Ctrl Pts',(1.19550440325007,-0.995371906852973,
9.82718493865666));
#287739=CARTESIAN_POINT('Ctrl Pts',(1.215486898086,-0.970721634816739,9.82941587123197));
#287740=CARTESIAN_POINT('Ctrl Pts',(1.22253247013869,-0.961833269833098,
9.83021702244878));
#287741=CARTESIAN_POINT('Ctrl Pts',(1.23545379987884,-0.9451609681197,9.83171424143816));
#287742=CARTESIAN_POINT('Ctrl Pts',(1.24135480810615,-0.937397236895416,
9.83240926335743));
#287743=CARTESIAN_POINT('Ctrl Pts',(1.2543339186761,-0.919983630970535,
9.83396365329924));
#287744=CARTESIAN_POINT('Ctrl Pts',(1.26137437478862,-0.910306614591972,
9.83482442937653));
#287745=CARTESIAN_POINT('Ctrl Pts',(1.27897485068468,-0.885518724345106,
9.8370222560162));
#287746=CARTESIAN_POINT('Ctrl Pts',(1.28937891783265,-0.870299966685399,
9.8383650979098));
#287747=CARTESIAN_POINT('Ctrl Pts',(1.3704516946631,-0.74706356939018,9.84919143650503));
#287748=CARTESIAN_POINT('Ctrl Pts',(1.4276817383381,-0.630835247412634,
9.85917718260273));
#287749=CARTESIAN_POINT('Ctrl Pts',(1.49216082625455,-0.444598579366025,
9.87444765146964));
#287750=CARTESIAN_POINT('Ctrl Pts',(1.5101842585719,-0.378889464329262,
9.8796949560682));
#287751=CARTESIAN_POINT('Ctrl Pts',(1.52691694778779,-0.297218614441416,
9.88590578026204));
#287752=CARTESIAN_POINT('Ctrl Pts',(1.5297662692152,-0.282186956512261,
9.88703608545995));
#287753=CARTESIAN_POINT('Ctrl Pts',(1.53361398350782,-0.260113269747403,
9.88867490303611));
#287754=CARTESIAN_POINT('Ctrl Pts',(1.53478649749467,-0.253103093448858,
9.88919227078725));
#287755=CARTESIAN_POINT('Ctrl Pts',(1.53669795941808,-0.241172923148172,
9.89006722415167));
#287756=CARTESIAN_POINT('Ctrl Pts',(1.53746140704036,-0.236257109770576,
9.89042614754676));
#287757=CARTESIAN_POINT('Ctrl Pts',(1.53915161729373,-0.225018621974873,
9.89124301996263));
#287758=CARTESIAN_POINT('Ctrl Pts',(1.54006301989316,-0.218693804004924,
9.8917001071892));
#287759=CARTESIAN_POINT('Ctrl Pts',(1.54248670461875,-0.201107243806639,
9.89296421256612));
#287760=CARTESIAN_POINT('Ctrl Pts',(1.54391464499911,-0.189833996497205,
9.89376672873699));
#287761=CARTESIAN_POINT('Ctrl Pts',(1.55378472154521,-0.104413676074503,
9.89979568497269));
#287762=CARTESIAN_POINT('Ctrl Pts',(1.55700586552081,-0.0297502730893351,
9.90477226802757));
#287763=CARTESIAN_POINT('Ctrl Pts',(1.55233898235879,0.131985944113632,
9.91546073616916));
#287764=CARTESIAN_POINT('Ctrl Pts',(1.54250761532666,0.218737898493034,
9.9211420544111));
#287765=CARTESIAN_POINT('Ctrl Pts',(1.5156306293346,0.353513332928016,9.93037052954646));
#287766=CARTESIAN_POINT('Ctrl Pts',(1.50341463739465,0.402307690465278,
9.93379561904323));
#287767=CARTESIAN_POINT('Ctrl Pts',(1.48429066455844,0.465521597197536,
9.93839436636857));
#287768=CARTESIAN_POINT('Ctrl Pts',(1.47949313175148,0.480550908392065,
9.93949988649892));
#287769=CARTESIAN_POINT('Ctrl Pts',(1.47116544608461,0.505331538667625,
9.94134429503418));
#287770=CARTESIAN_POINT('Ctrl Pts',(1.46776480940656,0.515125410530437,
9.94207890347509));
#287771=CARTESIAN_POINT('Ctrl Pts',(1.46092442894339,0.534207977393643,
9.94352170547116));
#287772=CARTESIAN_POINT('Ctrl Pts',(1.45749335683181,0.543499270120955,
9.94422958146824));
#287773=CARTESIAN_POINT('Ctrl Pts',(1.44902953093396,0.565762547329572,
9.94593906895808));
#287774=CARTESIAN_POINT('Ctrl Pts',(1.4439110803823,0.578700794932979,9.94694350416619));
#287775=CARTESIAN_POINT('Ctrl Pts',(1.42630147643978,0.621525146083746,
9.95030579230358));
#287776=CARTESIAN_POINT('Ctrl Pts',(1.41305126254654,0.651087744507704,
9.95268881102911));
#287777=CARTESIAN_POINT('Ctrl Pts',(1.34866117365497,0.783508821890407,
9.96365567864379));
#287778=CARTESIAN_POINT('Ctrl Pts',(1.28715315627535,0.880909658696088,
9.97258013580306));
#287779=CARTESIAN_POINT('Ctrl Pts',(1.18593295854578,1.00766496968798,9.98513811393158));
#287780=CARTESIAN_POINT('Ctrl Pts',(1.15468543650378,1.04332535705893,9.98878890275042));
#287781=CARTESIAN_POINT('Ctrl Pts',(1.10925603859308,1.09062467435328,9.99374758269093));
#287782=CARTESIAN_POINT('Ctrl Pts',(1.09642565374744,1.10352253732243,9.99511255768981));
#287783=CARTESIAN_POINT('Ctrl Pts',(1.07361146293197,1.12566587766457,9.99747433841182));
#287784=CARTESIAN_POINT('Ctrl Pts',(1.06372729469394,1.13501080060207,9.9984770299408));
#287785=CARTESIAN_POINT('Ctrl Pts',(1.04873150021597,1.14882048434801,9.9999661922508));
#287786=CARTESIAN_POINT('Ctrl Pts',(1.04371148565885,1.153383112477,10.0004594481348));
#287787=CARTESIAN_POINT('Ctrl Pts',(1.03457401949868,1.16157952864541,10.0013475609652));
#287788=CARTESIAN_POINT('Ctrl Pts',(1.03046704893257,1.16522447050142,10.0017432159499));
#287789=CARTESIAN_POINT('Ctrl Pts',(1.02114409405221,1.17341076103271,10.0026334939973));
#287790=CARTESIAN_POINT('Ctrl Pts',(1.01591704021907,1.1779391525821,10.0031271760292));
#287791=CARTESIAN_POINT('Ctrl Pts',(0.999805033205883,1.19171055702188,
10.0046328970824));
#287792=CARTESIAN_POINT('Ctrl Pts',(0.988822490618536,1.20083898842838,
10.0056371002573));
#287793=CARTESIAN_POINT('Ctrl Pts',(0.900689036249659,1.27206426212623,
10.0135364493857));
#287794=CARTESIAN_POINT('Ctrl Pts',(0.817882172923474,1.32682430962124,
10.0200134381943));
#287795=CARTESIAN_POINT('Ctrl Pts',(0.640431825087845,1.42120215557,10.0332436049806));
#287796=CARTESIAN_POINT('Ctrl Pts',(0.545971357085858,1.46009587175521,
10.039974704033));
#287797=CARTESIAN_POINT('Ctrl Pts',(0.430043180694643,1.49499509881758,
10.0483599537802));
#287798=CARTESIAN_POINT('Ctrl Pts',(0.411593542487943,1.50017938344392,
10.0496972668633));
#287799=CARTESIAN_POINT('Ctrl Pts',(0.382328657470157,1.50782224269089,
10.051825445954));
#287800=CARTESIAN_POINT('Ctrl Pts',(0.371574417018773,1.510508377687,10.0526089625023));
#287801=CARTESIAN_POINT('Ctrl Pts',(0.351281845404221,1.51534712632508,
10.0540906072181));
#287802=CARTESIAN_POINT('Ctrl Pts',(0.341750091707609,1.51752519418082,
10.0547878784527));
#287803=CARTESIAN_POINT('Ctrl Pts',(0.320158435165672,1.52224528924209,
10.0563706590364));
#287804=CARTESIAN_POINT('Ctrl Pts',(0.308087711444384,1.52473410470632,
10.0572578211574));
#287805=CARTESIAN_POINT('Ctrl Pts',(0.276699017408507,1.53081807765217,
10.0595713809875));
#287806=CARTESIAN_POINT('Ctrl Pts',(0.257340775937371,1.53419098966539,
10.0610046732927));
#287807=CARTESIAN_POINT('Ctrl Pts',(0.121106731183515,1.55527706552206,
10.0711407283076));
#287808=CARTESIAN_POINT('Ctrl Pts',(0.00262974571132385,1.5599795374538,
10.080252988605));
#287809=CARTESIAN_POINT('Ctrl Pts',(-0.195502670443402,1.54526418999826,
10.0956585921149));
#287810=CARTESIAN_POINT('Ctrl Pts',(-0.275220110826221,1.53307515730967,
10.1018899876751));
#287811=CARTESIAN_POINT('Ctrl Pts',(-0.366109826532087,1.51185573010769,
10.1088132266375));
#287812=CARTESIAN_POINT('Ctrl Pts',(-0.378541194094416,1.50879115398084,
10.1097559589325));
#287813=CARTESIAN_POINT('Ctrl Pts',(-0.397344710575575,1.50390867454509,
10.1111741372148));
#287814=CARTESIAN_POINT('Ctrl Pts',(-0.403745052507108,1.50220306793325,
10.1116554787919));
#287815=CARTESIAN_POINT('Ctrl Pts',(-0.415439262475882,1.49900657525242,
10.1125321810081));
#287816=CARTESIAN_POINT('Ctrl Pts',(-0.420736229318641,1.49752847075871,
10.1129282189027));
#287817=CARTESIAN_POINT('Ctrl Pts',(-0.432856925525221,1.49407683358175,
10.1138320753268));
#287818=CARTESIAN_POINT('Ctrl Pts',(-0.43967510077126,1.49208462013105,
10.114338817767));
#287819=CARTESIAN_POINT('Ctrl Pts',(-0.461109158996897,1.48566208631213,
10.1159271972903));
#287820=CARTESIAN_POINT('Ctrl Pts',(-0.475674120412569,1.48106301966805,
10.1169997046496));
#287821=CARTESIAN_POINT('Ctrl Pts',(-0.563831049768818,1.45179165246312,
10.123463092541));
#287822=CARTESIAN_POINT('Ctrl Pts',(-0.635568541283272,1.42185098505046,
10.1286057260794));
#287823=CARTESIAN_POINT('Ctrl Pts',(-0.778950850787198,1.34897684784595,
10.1392071448373));
#287824=CARTESIAN_POINT('Ctrl Pts',(-0.849975172472318,1.30539045520361,
10.1446482553512));
#287825=CARTESIAN_POINT('Ctrl Pts',(-0.954387770436467,1.22916535658077,
10.1533563840111));
#287826=CARTESIAN_POINT('Ctrl Pts',(-0.990375298541162,1.20035811270532,
10.1565039690023));
#287827=CARTESIAN_POINT('Ctrl Pts',(-1.03656408924026,1.15989237962767,
10.1607832418634));
#287828=CARTESIAN_POINT('Ctrl Pts',(-1.04794889928893,1.14961668330011,
10.1618585899196));
#287829=CARTESIAN_POINT('Ctrl Pts',(-1.06670656595603,1.1321762167919,10.1636664099232));
#287830=CARTESIAN_POINT('Ctrl Pts',(-1.07416384505524,1.12510351013287,
10.1643949561803));
#287831=CARTESIAN_POINT('Ctrl Pts',(-1.08871355923758,1.11102761985242,
10.1658363195881));
#287832=CARTESIAN_POINT('Ctrl Pts',(-1.09580986223409,1.10402913161156,
10.1665489121025));
#287833=CARTESIAN_POINT('Ctrl Pts',(-1.11289300223572,1.08685449654158,
10.1682882549027));
#287834=CARTESIAN_POINT('Ctrl Pts',(-1.12280795345046,1.0766084736797,10.1693180804695));
#287835=CARTESIAN_POINT('Ctrl Pts',(-1.15640672191953,1.04091881975398,
10.1728797906328));
#287836=CARTESIAN_POINT('Ctrl Pts',(-1.17937615148186,1.01482019878623,
10.1754412064161));
#287837=CARTESIAN_POINT('Ctrl Pts',(-1.28899456197786,0.881516246348095,
10.1883249848979));
#287838=CARTESIAN_POINT('Ctrl Pts',(-1.36199198907029,0.763900554405123,
10.1991542943032));
#287839=CARTESIAN_POINT('Ctrl Pts',(-1.4309878576702,0.61055382567494,10.2120521911623));
#287840=CARTESIAN_POINT('Ctrl Pts',(-1.44263400513142,0.58250286191313,
10.214362459187));
#287841=CARTESIAN_POINT('Ctrl Pts',(-1.46052457114569,0.535576671132989,
10.2181288594078));
#287842=CARTESIAN_POINT('Ctrl Pts',(-1.46724161869346,0.516891209679864,
10.2196034149299));
#287843=CARTESIAN_POINT('Ctrl Pts',(-1.47612025574444,0.490623292072964,
10.2216366663696));
#287844=CARTESIAN_POINT('Ctrl Pts',(-1.4785844581269,0.483146180167272,
10.2222109891023));
#287845=CARTESIAN_POINT('Ctrl Pts',(-1.48270149809656,0.470327307820379,
10.2231876683119));
#287846=CARTESIAN_POINT('Ctrl Pts',(-1.48438247181777,0.464994828593312,
10.2235916089882));
#287847=CARTESIAN_POINT('Ctrl Pts',(-1.48785803909051,0.453758500868902,
10.2244377245585));
#287848=CARTESIAN_POINT('Ctrl Pts',(-1.48964630277208,0.447852897469462,
10.2248795401082));
#287849=CARTESIAN_POINT('Ctrl Pts',(-1.4944269536241,0.43171968122671,10.2260790576758));
#287850=CARTESIAN_POINT('Ctrl Pts',(-1.49734952991703,0.421471475563612,
10.2268328806923));
#287851=CARTESIAN_POINT('Ctrl Pts',(-1.5118473082501,0.368578921152341,
10.2306856283154));
#287852=CARTESIAN_POINT('Ctrl Pts',(-1.52170810815697,0.325481136059841,
10.2336990399143));
#287853=CARTESIAN_POINT('Ctrl Pts',(-1.54679324570656,0.18941422676566,
10.2429895469406));
#287854=CARTESIAN_POINT('Ctrl Pts',(-1.55542223528351,0.0954485765964083,
10.2490946175472));
#287855=CARTESIAN_POINT('Ctrl Pts',(-1.55555778339162,-0.0698115119313443,
10.2600558083044));
#287856=CARTESIAN_POINT('Ctrl Pts',(-1.55074307203602,-0.140810644178326,
10.2648357607052));
#287857=CARTESIAN_POINT('Ctrl Pts',(-1.53866980533155,-0.228896468480794,
10.2710059133485));
#287858=CARTESIAN_POINT('Ctrl Pts',(-1.53594418862713,-0.246523359982548,
10.2722524768428));
#287859=CARTESIAN_POINT('Ctrl Pts',(-1.53108222236097,-0.274743801026789,
10.2742692838235));
#287860=CARTESIAN_POINT('Ctrl Pts',(-1.52913747026924,-0.285369084247679,
10.2750334554457));
#287861=CARTESIAN_POINT('Ctrl Pts',(-1.52521148618826,-0.305625325018494,
10.2764999494272));
#287862=CARTESIAN_POINT('Ctrl Pts',(-1.52324928150381,-0.315259472701574,
10.2772016334052));
#287863=CARTESIAN_POINT('Ctrl Pts',(-1.51851787066576,-0.337413905063551,
10.2788252310613));
#287864=CARTESIAN_POINT('Ctrl Pts',(-1.51568494839313,-0.349919684767954,
10.2797491400094));
#287865=CARTESIAN_POINT('Ctrl Pts',(-1.50614370277902,-0.38974714783133,
10.2827160883936));
#287866=CARTESIAN_POINT('Ctrl Pts',(-1.49884901282413,-0.416921022803087,
10.2847776408498));
#287867=CARTESIAN_POINT('Ctrl Pts',(-1.47968117304966,-0.48129832678765,
10.2897543422745));
#287868=CARTESIAN_POINT('Ctrl Pts',(-1.46713648761081,-0.518280359918293,
10.2926888874893));
#287869=CARTESIAN_POINT('Ctrl Pts',(-1.42833735818726,-0.619918213160373,
10.3009612327957));
#287870=CARTESIAN_POINT('Ctrl Pts',(-1.39910567361655,-0.683336087076675,
10.3063673298517));
#287871=CARTESIAN_POINT('Ctrl Pts',(-1.36023814559239,-0.754628106988403,
10.3126634426789));
#287872=CARTESIAN_POINT('Ctrl Pts',(-1.35464563125508,-0.764621872736702,
10.3135511450327));
#287873=CARTESIAN_POINT('Ctrl Pts',(-1.31372492335823,-0.835888412696872,
10.3199151809774));
#287874=CARTESIAN_POINT('Ctrl Pts',(-1.27435988941164,-0.894757989023516,
10.3253566874165));
#287875=CARTESIAN_POINT('Ctrl Pts',(-1.22419529206447,-0.959715834888923,
10.3314287263364));
#287876=CARTESIAN_POINT('Ctrl Pts',(-1.21717276664652,-0.968606768963859,
10.3322613007936));
#287877=CARTESIAN_POINT('Ctrl Pts',(-1.20604325932987,-0.982385177079956,
10.3335528757858));
#287878=CARTESIAN_POINT('Ctrl Pts',(-1.20200244626771,-0.987325226353898,
10.3340162217376));
#287879=CARTESIAN_POINT('Ctrl Pts',(-1.194757449722,-0.996072106540608,
10.3348368982606));
#287880=CARTESIAN_POINT('Ctrl Pts',(-1.19156536120063,-0.999888491878426,
10.3351950448079));
#287881=CARTESIAN_POINT('Ctrl Pts',(-1.18376258670696,-1.00912687038524,
10.3360622932033));
#287882=CARTESIAN_POINT('Ctrl Pts',(-1.17913292166726,-1.01453263157986,
10.336570013035));
#287883=CARTESIAN_POINT('Ctrl Pts',(-1.16439966563491,-1.03149860840886,
10.3381650227622));
#287884=CARTESIAN_POINT('Ctrl Pts',(-1.15416156682199,-1.04294155382191,
10.3392430712287));
#287885=CARTESIAN_POINT('Ctrl Pts',(-1.12928139194888,-1.06993451257986,
10.3417970393092));
#287886=CARTESIAN_POINT('Ctrl Pts',(-1.11448492323738,-1.08533855444128,
10.3432634902233));
#287887=CARTESIAN_POINT('Ctrl Pts',(-1.05538592764409,-1.14438069470012,
10.3489436974122));
#287888=CARTESIAN_POINT('Ctrl Pts',(-1.0087976994095,-1.18565383025421,
10.3530474331675));
#287889=CARTESIAN_POINT('Ctrl Pts',(-0.873212322475403,-1.29197727348091,
10.364393838861));
#287890=CARTESIAN_POINT('Ctrl Pts',(-0.779605273994225,-1.35052475871853,
10.3716071232752));
#287891=CARTESIAN_POINT('Ctrl Pts',(-0.662415596436684,-1.40754932852141,
10.3805932530735));
#287892=CARTESIAN_POINT('Ctrl Pts',(-0.644053977505205,-1.41604517734656,
10.3819990632949));
#287893=CARTESIAN_POINT('Ctrl Pts',(-0.61409390588095,-1.42920432766385,
10.3842926099728));
#287894=CARTESIAN_POINT('Ctrl Pts',(-0.602595412565447,-1.43409033467969,
10.3851727873525));
#287895=CARTESIAN_POINT('Ctrl Pts',(-0.581979842104226,-1.44255871369994,
10.3867513972379));
#287896=CARTESIAN_POINT('Ctrl Pts',(-0.572885326888024,-1.44619451434073,
10.3874479834532));
#287897=CARTESIAN_POINT('Ctrl Pts',(-0.553522629852327,-1.45372402325419,
10.3889317681512));
#287898=CARTESIAN_POINT('Ctrl Pts',(-0.543246382123762,-1.45759534659028,
10.3897196719726));
#287899=CARTESIAN_POINT('Ctrl Pts',(-0.515386205198999,-1.46775544187331,
10.3918573921451));
#287900=CARTESIAN_POINT('Ctrl Pts',(-0.497729115683304,-1.4738367103225,
10.3932139686503));
#287901=CARTESIAN_POINT('Ctrl Pts',(-0.458334857396247,-1.48661582965281,
10.3962457433056));
#287902=CARTESIAN_POINT('Ctrl Pts',(-0.436551981836944,-1.49315763917231,
10.3979255965166));
#287903=CARTESIAN_POINT('Ctrl Pts',(-0.366971135532644,-1.51240140275147,
10.403303589534));
#287904=CARTESIAN_POINT('Ctrl Pts',(-0.318710678453787,-1.52330183641062,
10.4070526584185));
#287905=CARTESIAN_POINT('Ctrl Pts',(-0.230601105354797,-1.53883243756245,
10.4139156864411));
#287906=CARTESIAN_POINT('Ctrl Pts',(-0.190932980983744,-1.54425597800546,
10.4170117432303));
#287907=CARTESIAN_POINT('Ctrl Pts',(-0.0629510142981618,-1.55674722084487,
10.4269803588373));
#287908=CARTESIAN_POINT('Ctrl Pts',(0.0257810817923055,-1.55780710454275,
10.4338694696636));
#287909=CARTESIAN_POINT('Ctrl Pts',(0.127536771487344,-1.55032106198754,
10.4414656322018));
#287910=CARTESIAN_POINT('Ctrl Pts',(0.140932970232763,-1.5491607252896,
10.4424593313239));
#287911=CARTESIAN_POINT('Ctrl Pts',(0.161112251171879,-1.54714892033522,
10.4439449990884));
#287912=CARTESIAN_POINT('Ctrl Pts',(0.167907121701986,-1.54642624857865,
10.4444433426678));
#287913=CARTESIAN_POINT('Ctrl Pts',(0.180240509369209,-1.54503227469975,
10.4453441393797));
#287914=CARTESIAN_POINT('Ctrl Pts',(0.185780590031195,-1.54437590878461,
10.4457473914912));
#287915=CARTESIAN_POINT('Ctrl Pts',(0.197331351165391,-1.54294436485019,
10.4465851282527));
#287916=CARTESIAN_POINT('Ctrl Pts',(0.203341199504102,-1.54216384833866,
10.4470193163872));
#287917=CARTESIAN_POINT('Ctrl Pts',(0.21939040513181,-1.53998403944075,
10.448174675313));
#287918=CARTESIAN_POINT('Ctrl Pts',(0.229421117952308,-1.53852167895274,
10.4488924417808));
#287919=CARTESIAN_POINT('Ctrl Pts',(0.280510396077361,-1.53056268096855,
10.4525294553288));
#287920=CARTESIAN_POINT('Ctrl Pts',(0.321314980448829,-1.52251949090368,
10.455372461685));
#287921=CARTESIAN_POINT('Ctrl Pts',(0.467373679116573,-1.48759398349703,
10.4654843255016));
#287922=CARTESIAN_POINT('Ctrl Pts',(0.570063614919924,-1.4513455813214,
10.472489895161));
#287923=CARTESIAN_POINT('Ctrl Pts',(0.72348968866107,-1.37836824980115,
10.4838139316509));
#287924=CARTESIAN_POINT('Ctrl Pts',(0.777224774687447,-1.34879822267972,
10.4879584466551));
#287925=CARTESIAN_POINT('Ctrl Pts',(0.843654765564453,-1.30695215884026,
10.4934122914425));
#287926=CARTESIAN_POINT('Ctrl Pts',(0.858083750356122,-1.29752439095823,
10.4946178069833));
#287927=CARTESIAN_POINT('Ctrl Pts',(0.881193362177257,-1.28187071438337,
10.4965845935519));
#287928=CARTESIAN_POINT('Ctrl Pts',(0.889972003179118,-1.27579155556228,
10.497340344943));
#287929=CARTESIAN_POINT('Ctrl Pts',(0.906749213119442,-1.26391600854525,
10.4988018365269));
#287930=CARTESIAN_POINT('Ctrl Pts',(0.91475654647108,-1.25813284853416,
10.4995070456327));
#287931=CARTESIAN_POINT('Ctrl Pts',(0.933267382592734,-1.2444935818224,
10.5011556291431));
#287932=CARTESIAN_POINT('Ctrl Pts',(0.943727532569405,-1.23658020658337,
10.5021011980458));
#287933=CARTESIAN_POINT('Ctrl Pts',(0.977643529692664,-1.21024089886292,
10.5052141879077));
#287934=CARTESIAN_POINT('Ctrl Pts',(1.00066829970582,-1.19127353389988,
10.5074027681746));
#287935=CARTESIAN_POINT('Ctrl Pts',(1.05500848846734,-1.14382177209762,
10.5127577380176));
#287936=CARTESIAN_POINT('Ctrl Pts',(1.08573282367552,-1.11469943753933,
10.51594775182));
#287937=CARTESIAN_POINT('Ctrl Pts',(1.16078419878238,-1.0375117210223,10.5241592268994));
#287938=CARTESIAN_POINT('Ctrl Pts',(1.20333872351954,-0.98783879239174,
10.5292267054032));
#287939=CARTESIAN_POINT('Ctrl Pts',(1.25148938714117,-0.92388904017262,
10.5354332311974));
#287940=CARTESIAN_POINT('Ctrl Pts',(1.2601706465525,-0.912012385686716,
10.5365732070718));
#287941=CARTESIAN_POINT('Ctrl Pts',(1.30698159082118,-0.846026533774559,
10.5428325413802));
#287942=CARTESIAN_POINT('Ctrl Pts',(1.3418005616862,-0.789642386365013,
10.5479132722681));
#287943=CARTESIAN_POINT('Ctrl Pts',(1.37823881746493,-0.721225245647919,
10.5536477762503));
#287944=CARTESIAN_POINT('Ctrl Pts',(1.38344510682597,-0.711187562539177,
10.5544786739812));
#287945=CARTESIAN_POINT('Ctrl Pts',(1.3914163810047,-0.695400161104967,
10.5557682950819));
#287946=CARTESIAN_POINT('Ctrl Pts',(1.39425611027449,-0.689688938764902,
10.556231341307));
#287947=CARTESIAN_POINT('Ctrl Pts',(1.39924754260943,-0.679493413981871,
10.557051565937));
#287948=CARTESIAN_POINT('Ctrl Pts',(1.40141290371434,-0.675016192103785,
10.5574095589381));
#287949=CARTESIAN_POINT('Ctrl Pts',(1.40662502700094,-0.664106123636475,
10.5582766773427));
#287950=CARTESIAN_POINT('Ctrl Pts',(1.40964916408628,-0.657662641111094,
10.5587844182476));
#287951=CARTESIAN_POINT('Ctrl Pts',(1.41906740637651,-0.637231876266187,
10.5603812663252));
#287952=CARTESIAN_POINT('Ctrl Pts',(1.4252986042657,-0.623169883307742,
10.5614610829948));
#287953=CARTESIAN_POINT('Ctrl Pts',(1.43970296880999,-0.5893165438916,10.5640203863862));
#287954=CARTESIAN_POINT('Ctrl Pts',(1.44767825100385,-0.569443946417325,
10.5654903335902));
#287955=CARTESIAN_POINT('Ctrl Pts',(1.47730900861638,-0.490960225240623,
10.5711935793446));
#287956=CARTESIAN_POINT('Ctrl Pts',(1.49583688236512,-0.431227383744786,
10.5753157532356));
#287957=CARTESIAN_POINT('Ctrl Pts',(1.53686570831554,-0.26394852550015,
10.5866559109783));
#287958=CARTESIAN_POINT('Ctrl Pts',(1.55165267317818,-0.154904759903231,
10.5938458883134));
#287959=CARTESIAN_POINT('Ctrl Pts',(1.55543111817508,-0.0249825338918657,
10.6028071309361));
#287960=CARTESIAN_POINT('Ctrl Pts',(1.55562449791537,-0.00473785627870441,
10.6042137983517));
#287961=CARTESIAN_POINT('Ctrl Pts',(1.55529823443904,0.0279940667465249,
10.6065079895558));
#287962=CARTESIAN_POINT('Ctrl Pts',(1.5550233035138,0.0404817879896868,
10.6073879277963));
#287963=CARTESIAN_POINT('Ctrl Pts',(1.55426484255743,0.0627438938977422,
10.6089656125016));
#287964=CARTESIAN_POINT('Ctrl Pts',(1.55383940084023,0.072519689933121,
10.609661507439));
#287965=CARTESIAN_POINT('Ctrl Pts',(1.55274178298795,0.0932383780253285,
10.611143270734));
#287966=CARTESIAN_POINT('Ctrl Pts',(1.55204609293042,0.104179430716684,
10.6119298388837));
#287967=CARTESIAN_POINT('Ctrl Pts',(1.54985664885033,0.133684113697593,
10.6140624736075));
#287968=CARTESIAN_POINT('Ctrl Pts',(1.54814510913308,0.152229232863489,
10.6154152635268));
#287969=CARTESIAN_POINT('Ctrl Pts',(1.53430153034745,0.277588079512021,
10.624647245127));
#287970=CARTESIAN_POINT('Ctrl Pts',(1.51145983887872,0.382905877595805,
10.6328654629736));
#287971=CARTESIAN_POINT('Ctrl Pts',(1.44869778326232,0.574159241408667,
10.6484632636017));
#287972=CARTESIAN_POINT('Ctrl Pts',(1.41143287498937,0.660488014155566,
10.6557775164042));
#287973=CARTESIAN_POINT('Ctrl Pts',(1.35959387539875,0.755844274568032,
10.6638557143908));
#287974=CARTESIAN_POINT('Ctrl Pts',(1.35239435741742,0.768651817858647,
10.6649403832672));
#287975=CARTESIAN_POINT('Ctrl Pts',(1.34150285625015,0.787400278453324,
10.666525625232));
#287976=CARTESIAN_POINT('Ctrl Pts',(1.3379507952754,0.793420938917952,10.667034294153));
#287977=CARTESIAN_POINT('Ctrl Pts',(1.33153668505157,0.804127133513199,
10.6679378426498));
#287978=CARTESIAN_POINT('Ctrl Pts',(1.32869029290779,0.808821673148615,
10.6683336747954));
#287979=CARTESIAN_POINT('Ctrl Pts',(1.32231089122076,0.819218622424716,
10.6692095155771));
#287980=CARTESIAN_POINT('Ctrl Pts',(1.31876579616933,0.824913343140161,
10.6696887336866));
#287981=CARTESIAN_POINT('Ctrl Pts',(1.30812217912994,0.841766900617,10.6711060364384));
#287982=CARTESIAN_POINT('Ctrl Pts',(1.30091784767906,0.852858683873841,
10.6720375599177));
#287983=CARTESIAN_POINT('Ctrl Pts',(1.24708471021245,0.933470422840288,
10.6788090708455));
#287984=CARTESIAN_POINT('Ctrl Pts',(1.19504641977618,0.999227379502725,
10.6843451181547));
#287985=CARTESIAN_POINT('Ctrl Pts',(1.06033010348591,1.14378589566827,10.6973622566328));
#287986=CARTESIAN_POINT('Ctrl Pts',(0.973797002134742,1.21830287971126,
10.70480712362));
#287987=CARTESIAN_POINT('Ctrl Pts',(0.863392823299522,1.29403800647458,
10.7140413685535));
#287988=CARTESIAN_POINT('Ctrl Pts',(0.846657264207012,1.30504901972728,
10.7154337115358));
#287989=CARTESIAN_POINT('Ctrl Pts',(0.819192654105145,1.32236847232441,
10.7177098923828));
#287990=CARTESIAN_POINT('Ctrl Pts',(0.808592003837131,1.32887694557807,
10.7185863683123));
#287991=CARTESIAN_POINT('Ctrl Pts',(0.789508591017037,1.34028069101927,
10.7201611970957));
#287992=CARTESIAN_POINT('Ctrl Pts',(0.781055409056963,1.34522436269302,
10.7208577439249));
#287993=CARTESIAN_POINT('Ctrl Pts',(0.762989615306636,1.35556209231758,
10.7223445026011));
#287994=CARTESIAN_POINT('Ctrl Pts',(0.753365263535971,1.36093442432579,
10.7231354474182));
#287995=CARTESIAN_POINT('Ctrl Pts',(0.727126487152051,1.37521734410045,
10.725289284484));
#287996=CARTESIAN_POINT('Ctrl Pts',(0.710406330958108,1.38392863212785,
10.7266591039591));
#287997=CARTESIAN_POINT('Ctrl Pts',(0.598033178483485,1.43990261176447,
10.7358518109454));
#287998=CARTESIAN_POINT('Ctrl Pts',(0.497911531314452,1.4775110747223,10.7440068925978));
#287999=CARTESIAN_POINT('Ctrl Pts',(0.303732709501313,1.52845716939883,
10.7595594139434));
#288000=CARTESIAN_POINT('Ctrl Pts',(0.210727454962227,1.54403105497301,
10.766893875974));
#288001=CARTESIAN_POINT('Ctrl Pts',(0.102257955602408,1.55220440760566,
10.7749886226034));
#288002=CARTESIAN_POINT('Ctrl Pts',(0.0876222453373523,1.55309935159465,
10.7760709706367));
#288003=CARTESIAN_POINT('Ctrl Pts',(0.065988560427154,1.55411540216812,
10.777654221212));
#288004=CARTESIAN_POINT('Ctrl Pts',(0.0589994227280295,1.55439642515554,
10.7781631591538));
#288005=CARTESIAN_POINT('Ctrl Pts',(0.0465016608314698,1.55481452404732,
10.7790683765666));
#288006=CARTESIAN_POINT('Ctrl Pts',(0.0409939780867431,1.55496948688485,
10.7794655952343));
#288007=CARTESIAN_POINT('Ctrl Pts',(0.0287296902881134,1.55524934234485,
10.7803463327242));
#288008=CARTESIAN_POINT('Ctrl Pts',(0.021972984108787,1.5553594775743,10.7808290399741));
#288009=CARTESIAN_POINT('Ctrl Pts',(0.00183837887307059,1.55555643990433,
10.7822605704648));
#288010=CARTESIAN_POINT('Ctrl Pts',(-0.0115405695724038,1.55551472639249,
10.7832027000114));
#288011=CARTESIAN_POINT('Ctrl Pts',(-0.105004327787419,1.55401731784783,
10.7897313233805));
#288012=CARTESIAN_POINT('Ctrl Pts',(-0.184883658543911,1.54655013284623,
10.7950427095603));
#288013=CARTESIAN_POINT('Ctrl Pts',(-0.378791620122958,1.51317616014496,
10.8080208358642));
#288014=CARTESIAN_POINT('Ctrl Pts',(-0.491138215690739,1.48052858247418,
10.8156400709515));
#288015=CARTESIAN_POINT('Ctrl Pts',(-0.616971025614448,1.42804609339886,
10.8250491812092));
#288016=CARTESIAN_POINT('Ctrl Pts',(-0.635019229594381,1.42011246379444,
10.8264200351323));
#288017=CARTESIAN_POINT('Ctrl Pts',(-0.664129891990716,1.40665010383958,
10.8286690417006));
#288018=CARTESIAN_POINT('Ctrl Pts',(-0.675286132463599,1.40132853097771,
10.8295401717767));
#288019=CARTESIAN_POINT('Ctrl Pts',(-0.695176004726446,1.39154831177086,
10.8311105631656));
#288020=CARTESIAN_POINT('Ctrl Pts',(-0.703933229263837,1.38713891959598,
10.8318080888403));
#288021=CARTESIAN_POINT('Ctrl Pts',(-0.722528085320177,1.37755470478362,
10.8333026094493));
#288022=CARTESIAN_POINT('Ctrl Pts',(-0.732353054938445,1.37235665547291,
10.834100389834));
#288023=CARTESIAN_POINT('Ctrl Pts',(-0.759011369935997,1.35788487633202,
10.8362878065772));
#288024=CARTESIAN_POINT('Ctrl Pts',(-0.775729385831765,1.34840404024374,
10.8376847073528));
#288025=CARTESIAN_POINT('Ctrl Pts',(-0.884120205623191,1.28425238790448,
10.8469119916551));
#288026=CARTESIAN_POINT('Ctrl Pts',(-0.970116626577675,1.22058925946963,
10.8550736498355));
#288027=CARTESIAN_POINT('Ctrl Pts',(-1.11814176333428,1.08541708142775,
10.8706064911498));
#288028=CARTESIAN_POINT('Ctrl Pts',(-1.18152566837724,1.01605679648136,
10.877914564296));
#288029=CARTESIAN_POINT('Ctrl Pts',(-1.24718670033915,0.929689277409492,
10.8859893736599));
#288030=CARTESIAN_POINT('Ctrl Pts',(-1.25592686137185,0.917847797149138,
10.887075885683));
#288031=CARTESIAN_POINT('Ctrl Pts',(-1.26857492652024,0.90019270812393,
10.8886636851969));
#288032=CARTESIAN_POINT('Ctrl Pts',(-1.27261343873815,0.894474312974158,
10.8891730878587));
#288033=CARTESIAN_POINT('Ctrl Pts',(-1.27974155920761,0.884235132607003,
10.8900762801216));
#288034=CARTESIAN_POINT('Ctrl Pts',(-1.28284608766674,0.879725040581249,
10.8904710478317));
#288035=CARTESIAN_POINT('Ctrl Pts',(-1.28966666001197,0.869703590339324,
10.8913414147905));
#288036=CARTESIAN_POINT('Ctrl Pts',(-1.29337126089165,0.864184711090659,
10.8918162547678));
#288037=CARTESIAN_POINT('Ctrl Pts',(-1.30426245419627,0.847732782968532,
10.8932190837928));
#288038=CARTESIAN_POINT('Ctrl Pts',(-1.31134683726718,0.83673228875342,
10.8941405972442));
#288039=CARTESIAN_POINT('Ctrl Pts',(-1.32748481873895,0.810965021560096,
10.8962644244732));
#288040=CARTESIAN_POINT('Ctrl Pts',(-1.33643240870579,0.796133584521806,
10.897460928771));
#288041=CARTESIAN_POINT('Ctrl Pts',(-1.36717162117044,0.743201379100567,
10.9016518571564));
#288042=CARTESIAN_POINT('Ctrl Pts',(-1.38759791565763,0.704328854631468,
10.9045872443426));
#288043=CARTESIAN_POINT('Ctrl Pts',(-1.44674496977784,0.579176165227472,
10.9137592018545));
#288044=CARTESIAN_POINT('Ctrl Pts',(-1.47926045143141,0.490208645686127,
10.9198894954674));
#288045=CARTESIAN_POINT('Ctrl Pts',(-1.51713017197339,0.34745190869074,
10.9297753778846));
#288046=CARTESIAN_POINT('Ctrl Pts',(-1.52811721567657,0.295404126428148,
10.9333866034349));
#288047=CARTESIAN_POINT('Ctrl Pts',(-1.53898230851263,0.226679073591335,
10.9382242821866));
#288048=CARTESIAN_POINT('Ctrl Pts',(-1.54128963861159,0.210419015548702,
10.9393737170175));
#288049=CARTESIAN_POINT('Ctrl Pts',(-1.54464334864976,0.183756376528848,
10.9412679995453));
#288050=CARTESIAN_POINT('Ctrl Pts',(-1.54584310037909,0.173374103442078,
10.9420079601729));
#288051=CARTESIAN_POINT('Ctrl Pts',(-1.54790969399638,0.153758950593175,
10.9434107491675));
#288052=CARTESIAN_POINT('Ctrl Pts',(-1.5487987750049,0.144528832042801,
10.9440728406153));
#288053=CARTESIAN_POINT('Ctrl Pts',(-1.55043998935338,0.125730648752053,
10.9454255599085));
#288054=CARTESIAN_POINT('Ctrl Pts',(-1.55118619971787,0.116162484060061,
10.9461163453934));
#288055=CARTESIAN_POINT('Ctrl Pts',(-1.5529198429744,0.0909219514400552,
10.9479448513701));
#288056=CARTESIAN_POINT('Ctrl Pts',(-1.55375854692078,0.07524084056863,
10.9490871787748));
#288057=CARTESIAN_POINT('Ctrl Pts',(-1.55513259868893,0.0393758202818612,
10.951715075679));
#288058=CARTESIAN_POINT('Ctrl Pts',(-1.55551263031814,0.0191893168875632,
10.9532051992225));
#288059=CARTESIAN_POINT('Ctrl Pts',(-1.55549967992335,-0.00099787692791932,
10.9547066646399));
#288060=CARTESIAN_POINT('Origin',(0.,0.,11.5));
#288061=CARTESIAN_POINT('',(-1.77820247099329,-0.00119341782894063,11.2217971285233));
#288062=CARTESIAN_POINT('Ctrl Pts',(1.55548765964693,0.00619602180104882,
11.4445));
#288063=CARTESIAN_POINT('Ctrl Pts',(1.56189352721799,-0.123480106596799,
11.4386107220588));
#288064=CARTESIAN_POINT('Ctrl Pts',(1.55157339318347,-0.253519976424599,
11.4332143653576));
#288065=CARTESIAN_POINT('Ctrl Pts',(1.49808469247915,-0.514160788411113,
11.4219950121858));
#288066=CARTESIAN_POINT('Ctrl Pts',(1.45350109175637,-0.643696036901404,
11.4161770675377));
#288067=CARTESIAN_POINT('Ctrl Pts',(1.30062304090847,-0.954321027644617,
11.400518906268));
#288068=CARTESIAN_POINT('Ctrl Pts',(1.17170724031108,-1.12368519948027,
11.3901617831135));
#288069=CARTESIAN_POINT('Ctrl Pts',(0.818804091578115,-1.43526580982338,
11.3682667882953));
#288070=CARTESIAN_POINT('Ctrl Pts',(0.621216082080241,-1.52501365559612,
11.3603867470286));
#288071=CARTESIAN_POINT('Ctrl Pts',(0.297108732731849,-1.63725103150195,
11.3469229737146));
#288072=CARTESIAN_POINT('Ctrl Pts',(0.107153340206811,-1.66829909150744,
11.3391230935286));
#288073=CARTESIAN_POINT('Ctrl Pts',(-0.292185223557251,-1.66621697631177,
11.321282124971));
#288074=CARTESIAN_POINT('Ctrl Pts',(-0.513310674133649,-1.62663919683985,
11.3104914809886));
#288075=CARTESIAN_POINT('Ctrl Pts',(-0.909998958031018,-1.45783368293536,
11.2926989463642));
#288076=CARTESIAN_POINT('Ctrl Pts',(-1.07580669034446,-1.34902596933128,
11.2857428355586));
#288077=CARTESIAN_POINT('Ctrl Pts',(-1.38700387291632,-1.05970778369804,
11.2694906051745));
#288078=CARTESIAN_POINT('Ctrl Pts',(-1.52291358407573,-0.872095507221723,
11.2599567992504));
#288079=CARTESIAN_POINT('Ctrl Pts',(-1.67153574440031,-0.550985528579673,
11.2444623587404));
#288080=CARTESIAN_POINT('Ctrl Pts',(-1.71193945495828,-0.431707929094432,
11.2389214746226));
#288081=CARTESIAN_POINT('Ctrl Pts',(-1.76131183138801,-0.207703856787064,
11.2295264907753));
#288082=CARTESIAN_POINT('Ctrl Pts',(-1.77428940940823,-0.104637895751818,
11.2256410604156));
#288083=CARTESIAN_POINT('Ctrl Pts',(-1.77813136846619,-0.00118827202808551,
11.2218682344905));
#288084=CARTESIAN_POINT('Ctrl Pts',(1.88253627798795,-0.516855496602614,
11.0478006140998));
#288085=CARTESIAN_POINT('Ctrl Pts',(1.89215033473946,-0.445574378263489,
11.0574016965198));
#288086=CARTESIAN_POINT('Ctrl Pts',(1.89787331411876,-0.373989233771073,
11.0669290501123));
#288087=CARTESIAN_POINT('Ctrl Pts',(1.89965572803299,-0.302473084920835,
11.0764143241982));
#288088=CARTESIAN_POINT('Ctrl Pts',(1.90139260519551,-0.232784016237714,
11.085657270412));
#288089=CARTESIAN_POINT('Ctrl Pts',(1.89938758197532,-0.163160762632793,
11.0948603968831));
#288090=CARTESIAN_POINT('Ctrl Pts',(1.89358682684666,-0.0939572062035731,
11.1040835916621));
#288091=CARTESIAN_POINT('Ctrl Pts',(1.88970231824742,-0.0476146518145124,
11.1102599564003));
#288092=CARTESIAN_POINT('Ctrl Pts',(1.88411554699461,-0.00146048069795877,
11.1164459542092));
#288093=CARTESIAN_POINT('Ctrl Pts',(1.87680793341714,0.0443978253500607,
11.1226670018792));
#288094=CARTESIAN_POINT('Ctrl Pts',(1.87053965133728,0.0837338951853796,
11.1280032558032));
#288095=CARTESIAN_POINT('Ctrl Pts',(1.86300522066158,0.122852251027833,
11.1333654053092));
#288096=CARTESIAN_POINT('Ctrl Pts',(1.85419110486612,0.161684829253256,
11.1387728141424));
#288097=CARTESIAN_POINT('Ctrl Pts',(1.85167893706529,0.172752751992759,
11.1403140144933));
#288098=CARTESIAN_POINT('Ctrl Pts',(1.8490632515539,0.1837951725869,11.1418585963554));
#288099=CARTESIAN_POINT('Ctrl Pts',(1.84634658998489,0.194800202160708,
11.1434055776474));
#288100=CARTESIAN_POINT('Ctrl Pts',(1.83039930705503,0.259401668264169,
11.1524866308905));
#288101=CARTESIAN_POINT('Ctrl Pts',(1.81095282151477,0.322816933304556,
11.1616636095605));
#288102=CARTESIAN_POINT('Ctrl Pts',(1.78801592867889,0.384801885349895,
11.1710458036959));
#288103=CARTESIAN_POINT('Ctrl Pts',(1.78062238327084,0.404782296857351,
11.1740700877114));
#288104=CARTESIAN_POINT('Ctrl Pts',(1.77286582172294,0.424614204120316,
11.1771157990191));
#288105=CARTESIAN_POINT('Ctrl Pts',(1.76474545843319,0.444289698912254,
11.1801868585978));
#288106=CARTESIAN_POINT('Ctrl Pts',(1.7378154418074,0.509540646802293,11.1903715858769));
#288107=CARTESIAN_POINT('Ctrl Pts',(1.70688632143051,0.573079490905792,
11.2008347187143));
#288108=CARTESIAN_POINT('Ctrl Pts',(1.6721221343155,0.634644923633791,11.211490393886));
#288109=CARTESIAN_POINT('Ctrl Pts',(1.64170347058988,0.68851467727079,11.2208141096613));
#288110=CARTESIAN_POINT('Ctrl Pts',(1.60834675830549,0.740872069419597,
11.2302849609928));
#288111=CARTESIAN_POINT('Ctrl Pts',(1.57215673141411,0.791480601409065,
11.2398527531659));
#288112=CARTESIAN_POINT('Ctrl Pts',(1.56528883456199,0.801084743969782,
11.2416684636086));
#288113=CARTESIAN_POINT('Ctrl Pts',(1.55831824486087,0.810626492044188,
11.2434878520796));
#288114=CARTESIAN_POINT('Ctrl Pts',(1.55125593009187,0.820090787420387,
11.2453080440553));
#288115=CARTESIAN_POINT('Ctrl Pts',(1.51205106392477,0.872629713498644,
11.2554124340665));
#288116=CARTESIAN_POINT('Ctrl Pts',(1.46995007963234,0.922884649798819,
11.2655582196712));
#288117=CARTESIAN_POINT('Ctrl Pts',(1.42516007265191,0.970612748098785,
11.2757116426035));
#288118=CARTESIAN_POINT('Ctrl Pts',(1.38066083958641,1.01803099857933,11.2857991501512));
#288119=CARTESIAN_POINT('Ctrl Pts',(1.33350635764439,1.06295444981336,11.2958939340275));
#288120=CARTESIAN_POINT('Ctrl Pts',(1.28391228682921,1.10509953210788,11.3059882715471));
#288121=CARTESIAN_POINT('Ctrl Pts',(1.2353687359176,1.14635188172166,11.3158687870855));
#288122=CARTESIAN_POINT('Ctrl Pts',(1.1844874395772,1.18494157633475,11.3257487414933));
#288123=CARTESIAN_POINT('Ctrl Pts',(1.13149317507234,1.22056969483562,11.33564811858));
#288124=CARTESIAN_POINT('Ctrl Pts',(1.11732550639015,1.23009463840087,11.3382946520498));
#288125=CARTESIAN_POINT('Ctrl Pts',(1.10300696040088,1.23940775844044,11.3409427327555));
#288126=CARTESIAN_POINT('Ctrl Pts',(1.08854214729938,1.24850303160568,11.3435930975827));
#288127=CARTESIAN_POINT('Ctrl Pts',(1.07955957366795,1.25415114889081,11.3452389603424));
#288128=CARTESIAN_POINT('Ctrl Pts',(1.07052139471689,1.25971465974848,11.3468855538523));
#288129=CARTESIAN_POINT('Ctrl Pts',(1.06143947727963,1.26518597414758,11.3485311649603));
#288130=CARTESIAN_POINT('Ctrl Pts',(1.00838526914422,1.29714797500361,11.3581443986012));
#288131=CARTESIAN_POINT('Ctrl Pts',(0.953742835520967,1.32602619339434,
11.367739831609));
#288132=CARTESIAN_POINT('Ctrl Pts',(0.897756806662159,1.35164031465119,
11.3773790263593));
#288133=CARTESIAN_POINT('Ctrl Pts',(0.842732813096956,1.37681429594516,
11.3868525861157));
#288134=CARTESIAN_POINT('Ctrl Pts',(0.786411165378941,1.39883566986307,
11.3963686518532));
#288135=CARTESIAN_POINT('Ctrl Pts',(0.729015815333678,1.41751519939103,
11.4060070892532));
#288136=CARTESIAN_POINT('Ctrl Pts',(0.67740328957587,1.43431268730852,11.4146744133165));
#288137=CARTESIAN_POINT('Ctrl Pts',(0.624923262383356,1.44840784882227,
11.423441002047));
#288138=CARTESIAN_POINT('Ctrl Pts',(0.571728575041354,1.45964595495108,
11.4323776356138));
#288139=CARTESIAN_POINT('Ctrl Pts',(0.567493011438373,1.4605407757624,11.4330892044143));
#288140=CARTESIAN_POINT('Ctrl Pts',(0.563252938966541,1.46141746636715,
11.4338018512908));
#288141=CARTESIAN_POINT('Ctrl Pts',(0.559008446750899,1.46227594031182,
11.4345156119738));
#288142=CARTESIAN_POINT('Ctrl Pts',(0.539367340846575,1.46624847149031,
11.4378184921425));
#288143=CARTESIAN_POINT('Ctrl Pts',(0.519630929867375,1.46983109384515,
11.4411453373854));
#288144=CARTESIAN_POINT('Ctrl Pts',(0.499806597877791,1.47301514408981,
11.4445));
#288145=CARTESIAN_POINT('',(-1.77834184724224,2.15144321225382E-15,11.2216581527578));
#288146=CARTESIAN_POINT('Ctrl Pts',(-1.77834184724224,-1.00752649088661E-15,
11.2216581527578));
#288147=CARTESIAN_POINT('Ctrl Pts',(-1.78056295809976,0.0630691399806642,
11.2194370419002));
#288148=CARTESIAN_POINT('Ctrl Pts',(-1.77938367163897,0.126382693101961,
11.2172615074937));
#288149=CARTESIAN_POINT('Ctrl Pts',(-1.77483216597492,0.189679055828712,
11.2150609641785));
#288150=CARTESIAN_POINT('Ctrl Pts',(-1.77329020973932,0.211122557913883,
11.2143154654937));
#288151=CARTESIAN_POINT('Ctrl Pts',(-1.77136105248992,0.232563838797864,
11.2135672537069));
#288152=CARTESIAN_POINT('Ctrl Pts',(-1.76904537453388,0.253991980379479,
11.2128140938177));
#288153=CARTESIAN_POINT('Ctrl Pts',(-1.76778031481698,0.265698219000541,
11.2124026409929));
#288154=CARTESIAN_POINT('Ctrl Pts',(-1.76639964595072,0.277402475295627,
11.2119896471974));
#288155=CARTESIAN_POINT('Ctrl Pts',(-1.7649042554453,0.289096769776087,
11.2115750020803));
#288156=CARTESIAN_POINT('Ctrl Pts',(-1.75618642716702,0.357272173289313,
11.2091577037803));
#288157=CARTESIAN_POINT('Ctrl Pts',(-1.74360249041908,0.424868383240363,
11.2066900058409));
#288158=CARTESIAN_POINT('Ctrl Pts',(-1.72729798068798,0.491522522760096,
11.2041289844565));
#288159=CARTESIAN_POINT('Ctrl Pts',(-1.71073794549437,0.55922127080288,
11.2015278265586));
#288160=CARTESIAN_POINT('Ctrl Pts',(-1.69033976331967,0.625947692112791,
11.1988302994765));
#288161=CARTESIAN_POINT('Ctrl Pts',(-1.6662481511712,0.691324926366082,
11.1960285326268));
#288162=CARTESIAN_POINT('Ctrl Pts',(-1.64236384340929,0.756139600199675,
11.1932508745232));
#288163=CARTESIAN_POINT('Ctrl Pts',(-1.61484988904239,0.819627995860444,
11.190370919865));
#288164=CARTESIAN_POINT('Ctrl Pts',(-1.58383624360157,0.881431640782451,
11.1874164891188));
#288165=CARTESIAN_POINT('Ctrl Pts',(-1.57286497683827,0.903295058182947,
11.1863713411722));
#288166=CARTESIAN_POINT('Ctrl Pts',(-1.56145560535928,0.924947732110167,
11.1853171870002));
#288167=CARTESIAN_POINT('Ctrl Pts',(-1.54961330849835,0.946374080476353,
11.1842562664096));
#288168=CARTESIAN_POINT('Ctrl Pts',(-1.54442636420112,0.955758854120637,
11.183791581554));
#288169=CARTESIAN_POINT('Ctrl Pts',(-1.53915787421691,0.96509736723114,
11.1833257442496));
#288170=CARTESIAN_POINT('Ctrl Pts',(-1.53381281501924,0.974381028115582,
11.1828593506641));
#288171=CARTESIAN_POINT('Ctrl Pts',(-1.49862875205757,1.0354910920071,11.1797892964942));
#288172=CARTESIAN_POINT('Ctrl Pts',(-1.46007853363983,1.09431741490311,
11.1766883201831));
#288173=CARTESIAN_POINT('Ctrl Pts',(-1.41837534558482,1.15057225854762,
11.1736360868923));
#288174=CARTESIAN_POINT('Ctrl Pts',(-1.37739382382525,1.20585362206971,
11.1706366719588));
#288175=CARTESIAN_POINT('Ctrl Pts',(-1.33336846171864,1.25865313843171,
11.167684930948));
#288176=CARTESIAN_POINT('Ctrl Pts',(-1.28644306758958,1.30871872921028,
11.1648758956585));
#288177=CARTESIAN_POINT('Ctrl Pts',(-1.26448173990596,1.33214968520263,
11.1635612525828));
#288178=CARTESIAN_POINT('Ctrl Pts',(-1.24188429129087,1.35498200658024,
11.1622780911309));
#288179=CARTESIAN_POINT('Ctrl Pts',(-1.21866009817821,1.37718997272362,
11.1610370705579));
#288180=CARTESIAN_POINT('Ctrl Pts',(-1.19068199257409,1.40394383319137,
11.1595420173399));
#288181=CARTESIAN_POINT('Ctrl Pts',(-1.16179384164629,1.42979214773977,
11.1581081113835));
#288182=CARTESIAN_POINT('Ctrl Pts',(-1.13203488986082,1.45471464743626,
11.1567155137289));
#288183=CARTESIAN_POINT('Ctrl Pts',(-1.12095836559293,1.46399100483939,
11.1561971775379));
#288184=CARTESIAN_POINT('Ctrl Pts',(-1.10976120370782,1.4731390256401,11.1556845718294));
#288185=CARTESIAN_POINT('Ctrl Pts',(-1.09844545044964,1.48215740611027,
11.1551767065377));
#288186=CARTESIAN_POINT('Ctrl Pts',(-1.08935715413905,1.48940055750147,
11.1547688123258));
#288187=CARTESIAN_POINT('Ctrl Pts',(-1.08019232237532,1.49655999164064,
11.154363979494));
#288188=CARTESIAN_POINT('Ctrl Pts',(-1.07096364146446,1.50362643251721,
11.1539621970547));
#288189=CARTESIAN_POINT('Ctrl Pts',(-1.01566987992673,1.54596510480667,
11.151554912351));
#288190=CARTESIAN_POINT('Ctrl Pts',(-0.957983446118207,1.58505012644099,
11.1492506572737));
#288191=CARTESIAN_POINT('Ctrl Pts',(-0.898228259814544,1.62079450667842,
11.1469514740276));
#288192=CARTESIAN_POINT('Ctrl Pts',(-0.837698849525372,1.65700201251613,
11.1446225011863));
#288193=CARTESIAN_POINT('Ctrl Pts',(-0.77504614367348,1.68978066505551,
11.1422983166927));
#288194=CARTESIAN_POINT('Ctrl Pts',(-0.710615248214486,1.71900501942652,
11.1399053013869));
#288195=CARTESIAN_POINT('Ctrl Pts',(-0.663013188082911,1.7405962058312,
11.1381373225676));
#288196=CARTESIAN_POINT('Ctrl Pts',(-0.614440761775559,1.76024657859127,
11.13633235624));
#288197=CARTESIAN_POINT('Ctrl Pts',(-0.565041756987997,1.77789819268943,
11.1344721468956));
#288198=CARTESIAN_POINT('Ctrl Pts',(-0.539651494217822,1.78697082729406,
11.1335160303854));
#288199=CARTESIAN_POINT('Ctrl Pts',(-0.514042933361847,1.79551535443774,
11.1325454839384));
#288200=CARTESIAN_POINT('Ctrl Pts',(-0.488235989627093,1.80352350105029,
11.1315590990326));
#288201=CARTESIAN_POINT('Ctrl Pts',(-0.47619036643152,1.80726137553791,
11.1310986950025));
#288202=CARTESIAN_POINT('Ctrl Pts',(-0.464101526274562,1.81088238877124,
11.1306348508758));
#288203=CARTESIAN_POINT('Ctrl Pts',(-0.451971511660108,1.81438568346352,
11.1301674792352));
#288204=CARTESIAN_POINT('Ctrl Pts',(-0.439847524072741,1.8178872374776,
11.129700339817));
#288205=CARTESIAN_POINT('Ctrl Pts',(-0.42768949408131,1.82126909162395,
11.1292299487222));
#288206=CARTESIAN_POINT('Ctrl Pts',(-0.415506737858453,1.82452903864206,
11.1287565465568));
#288207=CARTESIAN_POINT('Ctrl Pts',(-0.345947596059538,1.84314215974059,
11.1260535910234));
#288208=CARTESIAN_POINT('Ctrl Pts',(-0.275513093522433,1.85780178702206,
11.1232467369454));
#288209=CARTESIAN_POINT('Ctrl Pts',(-0.204614971902161,1.86847733419749,
11.1203524705051));
#288210=CARTESIAN_POINT('Ctrl Pts',(-0.133643475840232,1.87916392979416,
11.1174552087078));
#288211=CARTESIAN_POINT('Ctrl Pts',(-0.062207810260123,1.88585898842662,
11.1144706362429));
#288212=CARTESIAN_POINT('Ctrl Pts',(0.00931113847733771,1.88852707827048,
11.1114499681871));
#288213=CARTESIAN_POINT('Ctrl Pts',(0.0795509949153351,1.89114745022651,
11.1084833237617));
#288214=CARTESIAN_POINT('Ctrl Pts',(0.149871221863444,1.88988478521395,
11.1054822960035));
#288215=CARTESIAN_POINT('Ctrl Pts',(0.219944637317926,1.88468617466707,
11.1025233544346));
#288216=CARTESIAN_POINT('Ctrl Pts',(0.236268910205453,1.88347510857798,
11.1018340406725));
#288217=CARTESIAN_POINT('Ctrl Pts',(0.252579930614474,1.88205030856834,
11.1011471163361));
#288218=CARTESIAN_POINT('Ctrl Pts',(0.268873815199358,1.88041083505751,
11.1004637310381));
#288219=CARTESIAN_POINT('Ctrl Pts',(0.280585025716745,1.87923246538617,
11.0999725486533));
#288220=CARTESIAN_POINT('Ctrl Pts',(0.292287207949923,1.87794312096384,
11.099483204848));
#288221=CARTESIAN_POINT('Ctrl Pts',(0.303964922251466,1.87654437070336,
11.0989967256268));
#288222=CARTESIAN_POINT('Ctrl Pts',(0.375560982981668,1.86796863353342,
11.096014121757));
#288223=CARTESIAN_POINT('Ctrl Pts',(0.446366604285884,1.85527278904176,
11.0931327739186));
#288224=CARTESIAN_POINT('Ctrl Pts',(0.516098884532556,1.83847386708897,
11.0904596839593));
#288225=CARTESIAN_POINT('Ctrl Pts',(0.580751365491678,1.82289869906285,
11.0879813210392));
#288226=CARTESIAN_POINT('Ctrl Pts',(0.644489094069816,1.80379415961865,
11.0856817204922));
#288227=CARTESIAN_POINT('Ctrl Pts',(0.707133361048688,1.78130683067211,
11.0834688587693));
#288228=CARTESIAN_POINT('Ctrl Pts',(0.710628984808413,1.78005201127443,
11.0833453784831));
#288229=CARTESIAN_POINT('Ctrl Pts',(0.714121210943649,1.77878664733593,
11.0832221682817));
#288230=CARTESIAN_POINT('Ctrl Pts',(0.717610010741306,1.77751076026119,
11.083099212176));
#288231=CARTESIAN_POINT('Ctrl Pts',(0.784961797480596,1.75287957499815,
11.0807255266982));
#288232=CARTESIAN_POINT('Ctrl Pts',(0.851033618181087,1.72432966301448,
11.0784459483291));
#288233=CARTESIAN_POINT('Ctrl Pts',(0.915548362106642,1.69201720649116,
11.0761624209881));
#288234=CARTESIAN_POINT('Ctrl Pts',(0.930611525754063,1.6844727633012,11.075629253778));
#288235=CARTESIAN_POINT('Ctrl Pts',(0.945589580933063,1.676723154374,11.0750959642276));
#288236=CARTESIAN_POINT('Ctrl Pts',(0.960478600724483,1.66877030534791,
11.0745614851519));
#288237=CARTESIAN_POINT('Ctrl Pts',(0.975313302129192,1.66084647004704,
11.0740289559722));
#288238=CARTESIAN_POINT('Ctrl Pts',(0.99006444646142,1.65271797506666,11.0734950656497));
#288239=CARTESIAN_POINT('Ctrl Pts',(1.00470002911071,1.64440308869426,11.0729598689694));
#288240=CARTESIAN_POINT('Ctrl Pts',(1.06778798265132,1.60856104688918,11.0706528570719));
#288241=CARTESIAN_POINT('Ctrl Pts',(1.1288150742056,1.56921363248008,11.0683159018116));
#288242=CARTESIAN_POINT('Ctrl Pts',(1.18750283687179,1.52663356862106,11.065892184903));
#288243=CARTESIAN_POINT('Ctrl Pts',(1.24701567400671,1.48345488382351,11.0634343936516));
#288244=CARTESIAN_POINT('Ctrl Pts',(1.30412236127524,1.43695192355179,11.0608872144625));
#288245=CARTESIAN_POINT('Ctrl Pts',(1.35852490178442,1.38740391488404,11.0582277343097));
#288246=CARTESIAN_POINT('Ctrl Pts',(1.41273774521384,1.33802867595212,11.0555775275405));
#288247=CARTESIAN_POINT('Ctrl Pts',(1.46426503880922,1.28562996588739,11.0528158459264));
#288248=CARTESIAN_POINT('Ctrl Pts',(1.51281069067292,1.23047674230504,11.0499566160806));
#288249=CARTESIAN_POINT('Ctrl Pts',(1.52933742321749,1.21170054834898,11.048983228658));
#288250=CARTESIAN_POINT('Ctrl Pts',(1.54551859234449,1.19260502119365,11.0479988450508));
#288251=CARTESIAN_POINT('Ctrl Pts',(1.56134249951545,1.17320041606,11.0470049623625));
#288252=CARTESIAN_POINT('',(-0.999999999999999,-1.22464679914735E-16,12.));
#288253=CARTESIAN_POINT('',(-1.5,1.83697019872103E-16,11.5));
#288254=CARTESIAN_POINT('Origin',(0.,0.,12.));
#288255=CARTESIAN_POINT('Ctrl Pts',(-1.77829916038566,-0.00120041539116822,
11.2217004344528));
#288256=CARTESIAN_POINT('Ctrl Pts',(-1.77831352623488,-0.000800286888638816,
11.2216863387078));
#288257=CARTESIAN_POINT('Ctrl Pts',(-1.77832775518455,-0.000400148401643428,
11.2216722448155));
#288258=CARTESIAN_POINT('Ctrl Pts',(-1.77834184724224,-1.00752649088661E-15,
11.2216581527578));
#288259=CARTESIAN_POINT('Ctrl Pts',(1.13606312113376,-1.59291779518177,
-0.231572864370215));
#288260=CARTESIAN_POINT('Ctrl Pts',(1.66580317288383,-1.21512918566376,
-0.194523783755237));
#288261=CARTESIAN_POINT('Ctrl Pts',(2.30944881815147,0.10371475579539,-0.120437486311781));
#288262=CARTESIAN_POINT('Ctrl Pts',(1.16339684166879,2.00012929542641,-0.00931397203984471));
#288263=CARTESIAN_POINT('Ctrl Pts',(-1.04791166066631,2.06049852367029,
0.101797678445592));
#288264=CARTESIAN_POINT('Ctrl Pts',(-2.29995991841951,0.238642905340929,
0.212909328931029));
#288265=CARTESIAN_POINT('Ctrl Pts',(-1.44800670770165,-1.8030882775837,
0.324020979416465));
#288266=CARTESIAN_POINT('Ctrl Pts',(0.728891101841514,-2.19434009684312,
0.435132629901903));
#288267=CARTESIAN_POINT('Ctrl Pts',(2.2388411747295,-0.578378966553796,
0.546244280387339));
#288268=CARTESIAN_POINT('Ctrl Pts',(1.70047933315151,1.56697230991268,0.657355930872777));
#288269=CARTESIAN_POINT('Ctrl Pts',(-0.39369797820196,2.27855944506382,
0.768467581358213));
#288270=CARTESIAN_POINT('Ctrl Pts',(-2.12766415432316,0.905518297538944,
0.879579231843651));
#288271=CARTESIAN_POINT('Ctrl Pts',(-1.91500281753321,-1.29602787974305,
0.990690882329087));
#288272=CARTESIAN_POINT('Ctrl Pts',(0.0497274383191288,-2.31180100517801,
1.10180253281452));
#288273=CARTESIAN_POINT('Ctrl Pts',(1.9689597322423,-1.21248020017453,1.21291418329996));
#288274=CARTESIAN_POINT('Ctrl Pts',(2.08676085490371,0.996162330620904,
1.3240258337854));
#288275=CARTESIAN_POINT('Ctrl Pts',(0.295351476789991,2.29339794652186,
1.43513748427083));
#288276=CARTESIAN_POINT('Ctrl Pts',(-1.76627935167926,1.49236927838366,
1.54624913475627));
#288277=CARTESIAN_POINT('Ctrl Pts',(-2.21191375477208,-0.674052009334876,
1.65736078524171));
#288278=CARTESIAN_POINT('Ctrl Pts',(-0.633833682165421,-2.22377223890773,
1.76847243572715));
#288279=CARTESIAN_POINT('Ctrl Pts',(1.52415068530889,-1.73892872941285,
1.87958408621258));
#288280=CARTESIAN_POINT('Ctrl Pts',(2.28766582187352,0.336887910617784,
1.99069573669802));
#288281=CARTESIAN_POINT('Ctrl Pts',(0.95815978745069,2.1044804921888,2.10180738718346));
#288282=CARTESIAN_POINT('Ctrl Pts',(-1.24798158492499,1.9466510557791,2.21291903766889));
#288283=CARTESIAN_POINT('Ctrl Pts',(-2.31232513160447,0.00780017457708053,
2.32403068815433));
#288284=CARTESIAN_POINT('Ctrl Pts',(-1.26108632768448,-1.93818720060691,
2.43514233863977));
#288285=CARTESIAN_POINT('Ctrl Pts',(0.943940037394818,-2.1108968623253,
2.54625398912521));
#288286=CARTESIAN_POINT('Ctrl Pts',(2.2853409313939,-0.352314039762323,
2.65736563961064));
#288287=CARTESIAN_POINT('Ctrl Pts',(1.53584774180008,1.72860639494661,2.76847729009608));
#288288=CARTESIAN_POINT('Ctrl Pts',(-0.618816515269055,2.22799786267397,
2.87958894058151));
#288289=CARTESIAN_POINT('Ctrl Pts',(-2.20731588525495,0.688959315172647,
2.99070059106696));
#288290=CARTESIAN_POINT('Ctrl Pts',(-1.77630750418927,-1.48041886159491,
3.10181224155239));
#288291=CARTESIAN_POINT('Ctrl Pts',(0.279872333686937,-2.29533871839889,
3.21292389203783));
#288292=CARTESIAN_POINT('Ctrl Pts',(2.07999260576339,-1.01021736039841,
3.32403554252326));
#288293=CARTESIAN_POINT('Ctrl Pts',(1.97709518223906,1.19916762616646,3.4351471930087));
#288294=CARTESIAN_POINT('Ctrl Pts',(0.065322521730458,2.31141543722719,
3.54625884349413));
#288295=CARTESIAN_POINT('Ctrl Pts',(-1.90621473334059,1.3089131925695,3.65737049397958));
#288296=CARTESIAN_POINT('Ctrl Pts',(-2.13372638028968,-0.89113415900399,
3.76848214446501));
#288297=CARTESIAN_POINT('Ctrl Pts',(-0.409058462753209,-2.27586896137283,
3.87959379495045));
#288298=CARTESIAN_POINT('Ctrl Pts',(1.68986342616582,-1.57837573352984,
3.99070544543588));
#288299=CARTESIAN_POINT('Ctrl Pts',(2.24270289429889,0.563198085217235,
4.10181709592132));
#288300=CARTESIAN_POINT('Ctrl Pts',(0.743658484580136,2.18949318647061,
4.21292874640676));
#288301=CARTESIAN_POINT('Ctrl Pts',(-1.43577067829371,1.8125868019604,4.3240403968922));
#288302=CARTESIAN_POINT('Ctrl Pts',(-2.30159084080806,-0.222683535084021,
4.43515204737763));
#288303=CARTESIAN_POINT('Ctrl Pts',(-1.06164962419783,-2.05421723065739,
4.54626369786307));
#288304=CARTESIAN_POINT('Ctrl Pts',(1.14961140180695,-2.00631552357163,
4.65737534834851));
#288305=CARTESIAN_POINT('Ctrl Pts',(2.30907501534183,-0.122804433198633,
4.76848699883394));
#288306=CARTESIAN_POINT('Ctrl Pts',(1.35592986167235,1.87306234960673,4.87959864931938));
#288307=CARTESIAN_POINT('Ctrl Pts',(-0.837776683225523,2.15523515754841,
4.99071029980481));
#288308=CARTESIAN_POINT('Ctrl Pts',(-2.26498826620913,0.465549685021973,
5.10182195029026));
#288309=CARTESIAN_POINT('Ctrl Pts',(-1.61992673679233,-1.65007445974853,
5.21293360077568));
#288310=CARTESIAN_POINT('Ctrl Pts',(0.507231044863186,-2.25601973005913,
5.32404525126113));
#288311=CARTESIAN_POINT('Ctrl Pts',(2.17031522767223,-0.797897341656895,
5.43515690174656));
#288312=CARTESIAN_POINT('Ctrl Pts',(1.8477441385157,1.39023377669727,5.546268552232));
#288313=CARTESIAN_POINT('Ctrl Pts',(-0.165356899058651,2.30641831661622,
5.65738020271744));
#288314=CARTESIAN_POINT('Ctrl Pts',(-2.02717032910705,1.1124247444556,5.76849185320287));
#288315=CARTESIAN_POINT('Ctrl Pts',(-2.03429398882154,-1.09934358702528,
5.87960350368832));
#288316=CARTESIAN_POINT('Ctrl Pts',(-0.180210330756775,-2.30530531426481,
5.99071515417374));
#288317=CARTESIAN_POINT('Ctrl Pts',(1.83875057129879,-1.40210723264573,
6.1018268046592));
#288318=CARTESIAN_POINT('Ctrl Pts',(2.17540987993784,0.783900637554235,
6.21293845514461));
#288319=CARTESIAN_POINT('Ctrl Pts',(0.52175273974583,2.25270558081982,6.32405010563007));
#288320=CARTESIAN_POINT('Ctrl Pts',(-1.6092641245679,1.66047503223259,6.43516175611548));
#288321=CARTESIAN_POINT('Ctrl Pts',(-2.26794012696886,-0.450950036892674,
6.54627340660095));
#288322=CARTESIAN_POINT('Ctrl Pts',(-0.851642313493321,-2.14979387969097,
6.65738505708636));
#288323=CARTESIAN_POINT('Ctrl Pts',(1.34383634341701,-1.88175775205015,
6.76849670757181));
#288324=CARTESIAN_POINT('Ctrl Pts',(2.30981815768343,0.107927909851316,
6.87960835805725));
#288325=CARTESIAN_POINT('Ctrl Pts',(1.16251129221972,1.99886864269526,6.99072000854268));
#288326=CARTESIAN_POINT('Ctrl Pts',(-1.04839529676982,2.06101325978297,
7.10183165902812));
#288327=CARTESIAN_POINT('Ctrl Pts',(-2.3001086673767,0.237504681104215,
7.21294330951356));
#288328=CARTESIAN_POINT('Ctrl Pts',(-1.4474167224631,-1.8033006368383,7.32405495999898));
#288329=CARTESIAN_POINT('Ctrl Pts',(0.729539370371449,-2.19423805964062,
7.43516661048443));
#288330=CARTESIAN_POINT('Ctrl Pts',(2.23902850798198,-0.577632838161553,
7.54627826096985));
#288331=CARTESIAN_POINT('Ctrl Pts',(1.6999955211303,1.56745768153964,7.65738991145531));
#288332=CARTESIAN_POINT('Ctrl Pts',(-0.394389898323185,2.27845670651103,
7.76850156194073));
#288333=CARTESIAN_POINT('Ctrl Pts',(-2.12794184489071,0.904860132820632,
7.87961321242619));
#288334=CARTESIAN_POINT('Ctrl Pts',(-1.91460658872055,-1.2966070976552,
7.9907248629116));
#288335=CARTESIAN_POINT('Ctrl Pts',(0.0504321150938301,-2.31178825964159,
8.10183651339705));
#288336=CARTESIAN_POINT('Ctrl Pts',(1.9693296896238,-1.21187826459962,8.21294816388248));
#288337=CARTESIAN_POINT('Ctrl Pts',(2.08645679780942,0.996798066908651,
8.32405981436793));
#288338=CARTESIAN_POINT('Ctrl Pts',(0.294652019720973,2.29348829184849,
8.43517146485335));
#288339=CARTESIAN_POINT('Ctrl Pts',(-1.76673448864124,1.49183028428665,
8.54628311533881));
#288340=CARTESIAN_POINT('Ctrl Pts',(-2.21170804328929,-0.674726528470968,
8.65739476582423));
#288341=CARTESIAN_POINT('Ctrl Pts',(-0.633155389578567,-2.22396551725186,
8.76850641630968));
#288342=CARTESIAN_POINT('Ctrl Pts',(1.52468100466622,-1.73846373396192,
8.87961806679511));
#288343=CARTESIAN_POINT('Ctrl Pts',(2.28756296574735,0.33758562562678,8.99072971728054));
#288344=CARTESIAN_POINT('Ctrl Pts',(0.95751784602998,2.10477267467037,9.10184136776598));
#288345=CARTESIAN_POINT('Ctrl Pts',(-1.24857524943225,1.94627026738047,
9.21295301825142));
#288346=CARTESIAN_POINT('Ctrl Pts',(-2.31232744890977,0.00709498814131274,
9.32406466873686));
#288347=CARTESIAN_POINT('Ctrl Pts',(-1.26049501691729,-1.93857192891019,
9.43517631922229));
#288348=CARTESIAN_POINT('Ctrl Pts',(0.944583669006363,-2.11060852082977,
9.54628796970774));
#288349=CARTESIAN_POINT('Ctrl Pts',(2.28544860209947,-0.351617607164512,
9.65739962019316));
#288350=CARTESIAN_POINT('Ctrl Pts',(1.53531982431326,1.72907596712165,9.76851127067861));
#288351=CARTESIAN_POINT('Ctrl Pts',(-0.619494893047472,2.22780672033099,
9.87962292116403));
#288352=CARTESIAN_POINT('Ctrl Pts',(-2.20752811597315,0.688290399046372,
9.99073457164949));
#288353=CARTESIAN_POINT('Ctrl Pts',(-1.77585170267646,-1.48096889598351,
10.1018462221348));
#288354=CARTESIAN_POINT('Ctrl Pts',(0.280564466394787,-2.29523742190791,
10.2129578726204));
#288355=CARTESIAN_POINT('Ctrl Pts',(2.08031577474111,-1.00961302481287,
10.3240695231057));
#288356=CARTESIAN_POINT('Ctrl Pts',(1.97670051092818,1.19982795629719,10.4351811735912));
#288357=CARTESIAN_POINT('Ctrl Pts',(0.0646723860625978,2.31132606558188,
10.5462928240767));
#288358=CARTESIAN_POINT('Ctrl Pts',(-1.9067183409908,1.3085396174507,10.6574044745621));
#288359=CARTESIAN_POINT('Ctrl Pts',(-2.133255506411,-0.892181039348481,
10.7685161250475));
#288360=CARTESIAN_POINT('Ctrl Pts',(-0.408743935798804,-2.27523656122952,
10.8796277755329));
#288361=CARTESIAN_POINT('Ctrl Pts',(1.69107508575937,-1.57932721877126,
10.9907394260185));
#288362=CARTESIAN_POINT('Ctrl Pts',(2.24113370804431,0.567126268774148,
11.1018629835556));
#288363=CARTESIAN_POINT('Ctrl Pts',(1.24429396241602,1.64413287865399,11.1759493242644));
#288364=CARTESIAN_POINT('Ctrl Pts',(0.628071129403783,1.85298493614821,
11.2129984481446));
#288365=CARTESIAN_POINT('Ctrl Pts',(1.05790538596218,-1.48332982874757,
-0.1538593861323));
#288366=CARTESIAN_POINT('Ctrl Pts',(1.55120091107965,-1.13153194240705,
-0.116810305517322));
#288367=CARTESIAN_POINT('Ctrl Pts',(2.1505656665346,0.0965794916837141,
-0.0427240080738664));
#288368=CARTESIAN_POINT('Ctrl Pts',(1.08335862851045,1.86252639918517,0.0683995061980696));
#288369=CARTESIAN_POINT('Ctrl Pts',(-0.975818481569167,1.91874240560023,
0.179511156683506));
#288370=CARTESIAN_POINT('Ctrl Pts',(-2.14172957464275,0.222224989250477,
0.290622807168943));
#288371=CARTESIAN_POINT('Ctrl Pts',(-1.34838818943279,-1.67904121235574,
0.40173445765438));
#288372=CARTESIAN_POINT('Ctrl Pts',(0.678745580305889,-2.04337607998962,
0.512846108139817));
#288373=CARTESIAN_POINT('Ctrl Pts',(2.08481561719611,-0.538588228472594,
0.623957758625255));
#288374=CARTESIAN_POINT('Ctrl Pts',(1.58349145553025,1.45916931504287,0.73506940911069));
#288375=CARTESIAN_POINT('Ctrl Pts',(-0.366612738178346,2.12180138966432,
0.846181059596129));
#288376=CARTESIAN_POINT('Ctrl Pts',(-1.98128724232402,0.843221354723422,
0.957292710081565));
#288377=CARTESIAN_POINT('Ctrl Pts',(-1.78325636763855,-1.20686504898516,
1.068404360567));
#288378=CARTESIAN_POINT('Ctrl Pts',(0.0463063397176581,-2.15275603014899,
1.17951601105244));
#288379=CARTESIAN_POINT('Ctrl Pts',(1.83350120845665,-1.12906519917399,
1.29062766153788));
#288380=CARTESIAN_POINT('Ctrl Pts',(1.94319796721729,0.927629350211451,
1.40173931202331));
#288381=CARTESIAN_POINT('Ctrl Pts',(0.275032181078265,2.13561904672937,
1.51285096250875));
#288382=CARTESIAN_POINT('Ctrl Pts',(-1.64476463014706,1.38969874831511,
1.62396261299419));
#288383=CARTESIAN_POINT('Ctrl Pts',(-2.05974072296436,-0.627679252876699,
1.73507426347962));
#288384=CARTESIAN_POINT('Ctrl Pts',(-0.590227825983685,-2.07078337896038,
1.84618591396506));
#288385=CARTESIAN_POINT('Ctrl Pts',(1.41929368977058,-1.61929564865578,
1.9572975644505));
#288386=CARTESIAN_POINT('Ctrl Pts',(2.13028127506361,0.313711032845113,
2.06840921493594));
#288387=CARTESIAN_POINT('Ctrl Pts',(0.892241268024662,1.95969854660631,
2.17952086542137));
#288388=CARTESIAN_POINT('Ctrl Pts',(-1.16212419513821,1.81272730202038,
2.29063251590681));
#288389=CARTESIAN_POINT('Ctrl Pts',(-2.1532440982494,0.00726354596238041,
2.40174416639224));
#288390=CARTESIAN_POINT('Ctrl Pts',(-1.17432737090281,-1.80484573469715,
2.51285581687768));
#288391=CARTESIAN_POINT('Ctrl Pts',(0.878999794121258,-1.96567348972298,
2.62396746736312));
#288392=CARTESIAN_POINT('Ctrl Pts',(2.12811633007561,-0.32807589057435,
2.73507911784855));
#288393=CARTESIAN_POINT('Ctrl Pts',(1.43018602385987,1.60968345983953,2.846190768334));
#288394=CARTESIAN_POINT('Ctrl Pts',(-0.576243795126606,2.07471829248604,
2.95730241881943));
#288395=CARTESIAN_POINT('Ctrl Pts',(-2.05545917307893,0.641560980786489,
3.06841406930487));
#288396=CARTESIAN_POINT('Ctrl Pts',(-1.65410287584327,-1.37857048435678,
3.1795257197903));
#288397=CARTESIAN_POINT('Ctrl Pts',(0.260617956591843,-2.13742629932249,
3.29063737027575));
#288398=CARTESIAN_POINT('Ctrl Pts',(1.93689535331683,-0.940717436097568,
3.40174902076117));
#288399=CARTESIAN_POINT('Ctrl Pts',(1.84107696389546,1.11666849032732,3.51286067124662));
#288400=CARTESIAN_POINT('Ctrl Pts',(0.0608285281669042,2.15239698811669,
3.62397232173205));
#288401=CARTESIAN_POINT('Ctrl Pts',(-1.77507287727901,1.21886389093795,
3.7350839722175));
#288402=CARTESIAN_POINT('Ctrl Pts',(-1.98693240532736,-0.829826801775225,
3.84619562270292));
#288403=CARTESIAN_POINT('Ctrl Pts',(-0.380916467465418,-2.11929600318132,
3.95730727318837));
#288404=CARTESIAN_POINT('Ctrl Pts',(1.57360589110334,-1.46978821731913,
4.06841892367379));
#288405=CARTESIAN_POINT('Ctrl Pts',(2.08841166204214,0.524451746237755,
4.17953057415924));
#288406=CARTESIAN_POINT('Ctrl Pts',(0.692497011406068,2.0388626225127,4.29064222464467));
#288407=CARTESIAN_POINT('Ctrl Pts',(-1.3369939621468,1.68788626674563,4.40175387513011));
#288408=CARTESIAN_POINT('Ctrl Pts',(-2.14324829446283,-0.207363575797973,
4.51286552561555));
#288409=CARTESIAN_POINT('Ctrl Pts',(-0.988611314415993,-1.91289324670622,
4.62397717610099));
#288410=CARTESIAN_POINT('Ctrl Pts',(1.07052158556242,-1.86828703338926,
4.73508882658642));
#288411=CARTESIAN_POINT('Ctrl Pts',(2.15021758023707,-0.114355856540079,
4.84620047707186));
#288412=CARTESIAN_POINT('Ctrl Pts',(1.26264595423057,1.74420127810718,4.95731212755729));
#288413=CARTESIAN_POINT('Ctrl Pts',(-0.780140160287336,2.00696144322516,
5.06842377804273));
#288414=CARTESIAN_POINT('Ctrl Pts',(-2.10916386720878,0.43352126308458,
5.17953542852817));
#288415=CARTESIAN_POINT('Ctrl Pts',(-1.50848063618725,-1.53655428623061,
5.2906470790136));
#288416=CARTESIAN_POINT('Ctrl Pts',(0.47233507038983,-2.10081233944524,
5.40175872949904));
#288417=CARTESIAN_POINT('Ctrl Pts',(2.02100404975636,-0.74300439780258,
5.51287037998448));
#288418=CARTESIAN_POINT('Ctrl Pts',(1.72062488399853,1.29458986279462,5.62398203046992));
#288419=CARTESIAN_POINT('Ctrl Pts',(-0.153980840382875,2.14774365441516,
5.73509368095535));
#288420=CARTESIAN_POINT('Ctrl Pts',(-1.88770709085676,1.03589325869737,
5.84620533144079));
#288421=CARTESIAN_POINT('Ctrl Pts',(-1.89434066414993,-1.02371204566203,
5.95731698192623));
#288422=CARTESIAN_POINT('Ctrl Pts',(-0.167812400532235,-2.14670722328713,
6.06842863241166));
#288423=CARTESIAN_POINT('Ctrl Pts',(1.71225004723043,-1.30564646058762,
6.17954028289711));
#288424=CARTESIAN_POINT('Ctrl Pts',(2.02574820522723,0.729970624959828,
6.29065193338253));
#288425=CARTESIAN_POINT('Ctrl Pts',(0.485857716221588,2.09772619373299,
6.40176358386798));
#288426=CARTESIAN_POINT('Ctrl Pts',(-1.49855157970193,1.54623933052372,
6.51287523435341));
#288427=CARTESIAN_POINT('Ctrl Pts',(-2.11191264880221,-0.419926026955724,
6.62398688483885));
#288428=CARTESIAN_POINT('Ctrl Pts',(-0.793051876781918,-2.00189450896349,
6.73509853532428));
#288429=CARTESIAN_POINT('Ctrl Pts',(1.25138443375736,-1.75229846294388,
6.84621018580972));
#288430=CARTESIAN_POINT('Ctrl Pts',(2.15090959661459,0.100502793377733,
6.95732183629516));
#288431=CARTESIAN_POINT('Ctrl Pts',(1.08253400220732,1.86135247558067,7.06843348678059));
#288432=CARTESIAN_POINT('Ctrl Pts',(-0.976268844959389,1.91922172941229,
7.17954513726604));
#288433=CARTESIAN_POINT('Ctrl Pts',(-2.14186809011785,0.221165071427202,
7.29065678775147));
#288434=CARTESIAN_POINT('Ctrl Pts',(-1.34783879340901,-1.67923896193057,
7.40176843823691));
#288435=CARTESIAN_POINT('Ctrl Pts',(0.679349249905414,-2.0432810626406,
7.51288008872234));
#288436=CARTESIAN_POINT('Ctrl Pts',(2.08499006248272,-0.537893431475763,
7.62399173920778));
#288437=CARTESIAN_POINT('Ctrl Pts',(1.58304092832492,1.45962129455775,7.73510338969322));
#288438=CARTESIAN_POINT('Ctrl Pts',(-0.367257056270613,2.1217057192158,
7.84621504017865));
#288439=CARTESIAN_POINT('Ctrl Pts',(-1.98154582861344,0.842608469763599,
7.9573266906641));
#288440=CARTESIAN_POINT('Ctrl Pts',(-1.78288739817974,-1.20740441844228,
8.06843834114951));
#288441=CARTESIAN_POINT('Ctrl Pts',(0.0469625368439069,-2.15274416146725,
8.17954999163497));
#288442=CARTESIAN_POINT('Ctrl Pts',(1.83384571387996,-1.12850467496116,
8.29066164212039));
#288443=CARTESIAN_POINT('Ctrl Pts',(1.9429148283391,0.928221349749457,8.40177329260585));
#288444=CARTESIAN_POINT('Ctrl Pts',(0.274380844557604,2.1357031765685,8.51288494309127));
#288445=CARTESIAN_POINT('Ctrl Pts',(-1.6451884550512,1.38919683539529,8.62399659357671));
#288446=CARTESIAN_POINT('Ctrl Pts',(-2.05954916381456,-0.62830736711941,
8.73510824406215));
#288447=CARTESIAN_POINT('Ctrl Pts',(-0.5895961978923,-2.07096336033418,
8.84621989454758));
#288448=CARTESIAN_POINT('Ctrl Pts',(1.4197875247468,-1.61886264349714,8.95733154503303));
#288449=CARTESIAN_POINT('Ctrl Pts',(2.13018549513042,0.314360747154248,
9.06844319551845));
#288450=CARTESIAN_POINT('Ctrl Pts',(0.891643490248224,1.95997062780954,
9.17955484600391));
#288451=CARTESIAN_POINT('Ctrl Pts',(-1.16267701730804,1.81237271072142,
9.29066649648932));
#288452=CARTESIAN_POINT('Ctrl Pts',(-2.15324625613104,0.00660687423822486,
9.40177814697478));
#288453=CARTESIAN_POINT('Ctrl Pts',(-1.1737767405428,-1.80520399484714,
9.5128897974602));
#288454=CARTESIAN_POINT('Ctrl Pts',(0.879599145808469,-1.96540498525748,
9.62400144794565));
#288455=CARTESIAN_POINT('Ctrl Pts',(2.12821659335958,-0.327427370450354,
9.73511309843108));
#288456=CARTESIAN_POINT('Ctrl Pts',(1.42969442551268,1.61012072685739,9.84622474891651));
#288457=CARTESIAN_POINT('Ctrl Pts',(-0.576875502548628,2.07454030016294,
9.95733639940195));
#288458=CARTESIAN_POINT('Ctrl Pts',(-2.0556568029603,0.640938084083322,
10.0684480498874));
#288459=CARTESIAN_POINT('Ctrl Pts',(-1.6536784321074,-1.37908267802925,
10.1795597003728));
#288460=CARTESIAN_POINT('Ctrl Pts',(0.26126247264541,-2.13733197172626,
10.2906713508583));
#288461=CARTESIAN_POINT('Ctrl Pts',(1.93719628923821,-0.940154676987634,
10.4017830013437));
#288462=CARTESIAN_POINT('Ctrl Pts',(1.84070944478698,1.11728339172568,10.5128946518291));
#288463=CARTESIAN_POINT('Ctrl Pts',(0.0602231198829427,2.15231376497251,
10.6240063023145));
#288464=CARTESIAN_POINT('Ctrl Pts',(-1.77554183823342,1.2185160166668,10.7351179528));
#288465=CARTESIAN_POINT('Ctrl Pts',(-1.98649392615918,-0.83080165989208,
10.8462296032854));
#288466=CARTESIAN_POINT('Ctrl Pts',(-0.380623579022067,-2.118707110271,
10.9573412537709));
#288467=CARTESIAN_POINT('Ctrl Pts',(1.57473419215115,-1.47067424322988,
11.0684529042563));
#288468=CARTESIAN_POINT('Ctrl Pts',(2.08695043109518,0.528109682548335,
11.1795764617936));
#288469=CARTESIAN_POINT('Ctrl Pts',(1.15869026999699,1.53102146809392,11.2536628025023));
#288470=CARTESIAN_POINT('Ctrl Pts',(0.584861719567571,1.72550513047344,
11.2907119263826));
#288471=CARTESIAN_POINT('Ctrl Pts',(0.979747650790608,-1.37374186231338,
-0.0761459078943855));
#288472=CARTESIAN_POINT('Ctrl Pts',(1.43659864927549,-1.04793469915035,
-0.0390968272794079));
#288473=CARTESIAN_POINT('Ctrl Pts',(1.99168251491774,0.0894442275720395,
0.0349894701640479));
#288474=CARTESIAN_POINT('Ctrl Pts',(1.00332041535211,1.72492350294394,0.146112984435984));
#288475=CARTESIAN_POINT('Ctrl Pts',(-0.903725302472021,1.77698628753017,
0.25722463492142));
#288476=CARTESIAN_POINT('Ctrl Pts',(-1.98349923086599,0.205807073160022,
0.368336285406858));
#288477=CARTESIAN_POINT('Ctrl Pts',(-1.24876967116393,-1.55499414712776,
0.479447935892295));
#288478=CARTESIAN_POINT('Ctrl Pts',(0.62860005877027,-1.89241206313614,
0.590559586377731));
#288479=CARTESIAN_POINT('Ctrl Pts',(1.93079005966273,-0.498797490391393,
0.701671236863168));
#288480=CARTESIAN_POINT('Ctrl Pts',(1.46650357790899,1.35136632017308,0.812782887348605));
#288481=CARTESIAN_POINT('Ctrl Pts',(-0.339527498154739,1.96504333426481,
0.923894537834042));
#288482=CARTESIAN_POINT('Ctrl Pts',(-1.83491033032488,0.780924411907904,
1.03500618831948));
#288483=CARTESIAN_POINT('Ctrl Pts',(-1.6515099177439,-1.11770221822726,
1.14611783880492));
#288484=CARTESIAN_POINT('Ctrl Pts',(0.0428852411161929,-1.99371105511996,
1.25722948929036));
#288485=CARTESIAN_POINT('Ctrl Pts',(1.69804268467099,-1.04565019817345,
1.36834113977579));
#288486=CARTESIAN_POINT('Ctrl Pts',(1.79963507953087,0.859096369801998,
1.47945279026123));
#288487=CARTESIAN_POINT('Ctrl Pts',(0.254712885366533,1.97784014693687,
1.59056444074667));
#288488=CARTESIAN_POINT('Ctrl Pts',(-1.52324990861485,1.28702821824656,
1.7016760912321));
#288489=CARTESIAN_POINT('Ctrl Pts',(-1.90756769115663,-0.581306496418522,
1.81278774171754));
#288490=CARTESIAN_POINT('Ctrl Pts',(-0.546621969801947,-1.91779451901304,
1.92389939220298));
#288491=CARTESIAN_POINT('Ctrl Pts',(1.31443669423229,-1.49966256789871,
2.03501104268841));
#288492=CARTESIAN_POINT('Ctrl Pts',(1.9728967282537,0.290534155072444,2.14612269317385));
#288493=CARTESIAN_POINT('Ctrl Pts',(0.826322748598632,1.81491660102383,
2.25723434365928));
#288494=CARTESIAN_POINT('Ctrl Pts',(-1.07626680535143,1.67880354826165,
2.36834599414473));
#288495=CARTESIAN_POINT('Ctrl Pts',(-1.99416306489432,0.00672691734768011,
2.47945764463016));
#288496=CARTESIAN_POINT('Ctrl Pts',(-1.08756841412115,-1.6715042687874,
2.5905692951156));
#288497=CARTESIAN_POINT('Ctrl Pts',(0.814059550847701,-1.82045011712066,
2.70168094560104));
#288498=CARTESIAN_POINT('Ctrl Pts',(1.97089172875732,-0.303837741386377,
2.81279259608647));
#288499=CARTESIAN_POINT('Ctrl Pts',(1.32452430591967,1.49076052473245,2.92390424657191));
#288500=CARTESIAN_POINT('Ctrl Pts',(-0.533671074984155,1.92143872229811,
3.03501589705734));
#288501=CARTESIAN_POINT('Ctrl Pts',(-1.90360246090293,0.594162646400333,
3.14612754754278));
#288502=CARTESIAN_POINT('Ctrl Pts',(-1.53189824749729,-1.27672210711867,
3.25723919802822));
#288503=CARTESIAN_POINT('Ctrl Pts',(0.241363579496748,-1.9795138802461,
3.36835084851366));
#288504=CARTESIAN_POINT('Ctrl Pts',(1.79379810087027,-0.871217511796724,
3.47946249899909));
#288505=CARTESIAN_POINT('Ctrl Pts',(1.70505874555187,1.03416935448819,3.59057414948453));
#288506=CARTESIAN_POINT('Ctrl Pts',(0.0563345346033484,1.9933785390062,
3.70168579996997));
#288507=CARTESIAN_POINT('Ctrl Pts',(-1.64393102121742,1.12881458930639,
3.8127974504554));
#288508=CARTESIAN_POINT('Ctrl Pts',(-1.84013843036505,-0.768519444546461,
3.92390910094084));
#288509=CARTESIAN_POINT('Ctrl Pts',(-0.352774472177625,-1.96272304498979,
4.03502075142628));
#288510=CARTESIAN_POINT('Ctrl Pts',(1.45734835604085,-1.36120070110842,
4.14613240191171));
#288511=CARTESIAN_POINT('Ctrl Pts',(1.9341204297854,0.485705407258275,4.25724405239715));
#288512=CARTESIAN_POINT('Ctrl Pts',(0.641335538231996,1.88823205855479,
4.36835570288259));
#288513=CARTESIAN_POINT('Ctrl Pts',(-1.2382172459999,1.56318573153086,4.47946735336802));
#288514=CARTESIAN_POINT('Ctrl Pts',(-1.9849057481176,-0.192043616511923,
4.59057900385346));
#288515=CARTESIAN_POINT('Ctrl Pts',(-0.915573004634159,-1.77156926275505,
4.7016906543389));
#288516=CARTESIAN_POINT('Ctrl Pts',(0.991431769317905,-1.73025854320689,
4.81280230482433));
#288517=CARTESIAN_POINT('Ctrl Pts',(1.99136014513231,-0.105907279881526,
4.92391395530977));
#288518=CARTESIAN_POINT('Ctrl Pts',(1.16936204678881,1.61534020660762,5.03502560579521));
#288519=CARTESIAN_POINT('Ctrl Pts',(-0.722503637349151,1.85868772890191,
5.14613725628065));
#288520=CARTESIAN_POINT('Ctrl Pts',(-1.95333946820844,0.40149284114719,
5.25724890676608));
#288521=CARTESIAN_POINT('Ctrl Pts',(-1.39703453558216,-1.42303411271269,
5.36836055725152));
#288522=CARTESIAN_POINT('Ctrl Pts',(0.437439095916471,-1.94560494883135,
5.47947220773696));
#288523=CARTESIAN_POINT('Ctrl Pts',(1.87169287184049,-0.68811145394827,
5.5905838582224));
#288524=CARTESIAN_POINT('Ctrl Pts',(1.59350562948136,1.19894594889198,5.70169550870783));
#288525=CARTESIAN_POINT('Ctrl Pts',(-0.142604781707098,1.98906899221409,
5.81280715919328));
#288526=CARTESIAN_POINT('Ctrl Pts',(-1.74824385260649,0.959361772939144,
5.9239188096787));
#288527=CARTESIAN_POINT('Ctrl Pts',(-1.75438733947832,-0.948080504298782,
6.03503046016415));
#288528=CARTESIAN_POINT('Ctrl Pts',(-0.155414470307694,-1.98810913230945,
6.14614211064957));
#288529=CARTESIAN_POINT('Ctrl Pts',(1.58574952316206,-1.20918568852951,
6.25725376113503));
#288530=CARTESIAN_POINT('Ctrl Pts',(1.87608653051662,0.67604061236542,6.36836541162044));
#288531=CARTESIAN_POINT('Ctrl Pts',(0.449962692697341,1.94274680664615,
6.4794770621059));
#288532=CARTESIAN_POINT('Ctrl Pts',(-1.38783903483595,1.43200362881485,
6.59058871259132));
#288533=CARTESIAN_POINT('Ctrl Pts',(-1.95588517063554,-0.388902017018772,
6.70170036307677));
#288534=CARTESIAN_POINT('Ctrl Pts',(-0.734461440070516,-1.85399513823601,
6.8128120135622));
#288535=CARTESIAN_POINT('Ctrl Pts',(1.1589325240977,-1.62283917383761,6.92392366404763));
#288536=CARTESIAN_POINT('Ctrl Pts',(1.99200103554574,0.0930776769041453,
7.03503531453308));
#288537=CARTESIAN_POINT('Ctrl Pts',(1.00255671219492,1.72383630846607,7.14614696501851));
#288538=CARTESIAN_POINT('Ctrl Pts',(-0.904142393148962,1.77743019904159,
7.25725861550395));
#288539=CARTESIAN_POINT('Ctrl Pts',(-1.98362751285899,0.20482546175019,
7.36837026598938));
#288540=CARTESIAN_POINT('Ctrl Pts',(-1.24826086435494,-1.55517728702285,
7.47948191647483));
#288541=CARTESIAN_POINT('Ctrl Pts',(0.629159129439381,-1.89232406564059,
7.59059356696026));
#288542=CARTESIAN_POINT('Ctrl Pts',(1.93095161698345,-0.498154024789975,
7.7017052174457));
#288543=CARTESIAN_POINT('Ctrl Pts',(1.46608633551955,1.35178490757587,7.81281686793113));
#288544=CARTESIAN_POINT('Ctrl Pts',(-0.34012421421804,1.96495473192057,
7.92392851841657));
#288545=CARTESIAN_POINT('Ctrl Pts',(-1.83514981233618,0.780356806706567,
8.03504016890202));
#288546=CARTESIAN_POINT('Ctrl Pts',(-1.65116820763892,-1.11820173922936,
8.14615181938743));
#288547=CARTESIAN_POINT('Ctrl Pts',(0.0434929585939797,-1.9937000632929,
8.25726346987289));
#288548=CARTESIAN_POINT('Ctrl Pts',(1.69836173813612,-1.0451310853227,8.36837512035831));
#288549=CARTESIAN_POINT('Ctrl Pts',(1.79937285886876,0.859644632590266,
8.47948677084376));
#288550=CARTESIAN_POINT('Ctrl Pts',(0.254109669394238,1.97791806128852,
8.59059842132919));
#288551=CARTESIAN_POINT('Ctrl Pts',(-1.52364242146117,1.28656338650393,
8.70171007181462));
#288552=CARTESIAN_POINT('Ctrl Pts',(-1.90739028433983,-0.581888205767853,
8.81282172230007));
#288553=CARTESIAN_POINT('Ctrl Pts',(-0.546037006206034,-1.91796120341649,
8.92393337278549));
#288554=CARTESIAN_POINT('Ctrl Pts',(1.31489404482737,-1.49926155303236,
9.03504502327096));
#288555=CARTESIAN_POINT('Ctrl Pts',(1.97280802451347,0.29113586868172,9.14615667375636));
#288556=CARTESIAN_POINT('Ctrl Pts',(0.825769134466469,1.81516858094871,
9.25726832424182));
#288557=CARTESIAN_POINT('Ctrl Pts',(-1.07677878518382,1.67847515406237,
9.36837997472725));
#288558=CARTESIAN_POINT('Ctrl Pts',(-1.99416506335232,0.00611876033513456,
9.47949162521268));
#288559=CARTESIAN_POINT('Ctrl Pts',(-1.08705846416831,-1.67183606078409,
9.59060327569813));
#288560=CARTESIAN_POINT('Ctrl Pts',(0.814614622610574,-1.82020144968518,
9.70171492618355));
#288561=CARTESIAN_POINT('Ctrl Pts',(1.97098458461971,-0.303237133736198,
9.81282657666901));
#288562=CARTESIAN_POINT('Ctrl Pts',(1.32406902671211,1.49116548659312,9.92393822715443));
#288563=CARTESIAN_POINT('Ctrl Pts',(-0.534256112049782,1.92127387999488,
10.0350498776399));
#288564=CARTESIAN_POINT('Ctrl Pts',(-1.90378548994746,0.593585769120274,
10.1461615281253));
#288565=CARTESIAN_POINT('Ctrl Pts',(-1.53150516153833,-1.277196460075,10.2572731786108));
#288566=CARTESIAN_POINT('Ctrl Pts',(0.241960478896032,-1.97942652154461,
10.3683848290962));
#288567=CARTESIAN_POINT('Ctrl Pts',(1.79407680373531,-0.870696329162404,
10.4794964795816));
#288568=CARTESIAN_POINT('Ctrl Pts',(1.70471837864578,1.03473882715419,10.5906081300671));
#288569=CARTESIAN_POINT('Ctrl Pts',(0.0557738537032858,1.99330146436314,
10.7017197805525));
#288570=CARTESIAN_POINT('Ctrl Pts',(-1.64436533547605,1.12849241588291,
10.812831431038));
#288571=CARTESIAN_POINT('Ctrl Pts',(-1.83973234590736,-0.769422280435679,
10.9239430815234));
#288572=CARTESIAN_POINT('Ctrl Pts',(-0.35250322224533,-1.96217765931249,
11.0350547320088));
#288573=CARTESIAN_POINT('Ctrl Pts',(1.45839329854295,-1.36202126768849,
11.1461663824943));
#288574=CARTESIAN_POINT('Ctrl Pts',(1.93276715414607,0.489093096322522,
11.2572899400314));
#288575=CARTESIAN_POINT('Ctrl Pts',(1.07308657757797,1.41791005753384,11.3313762807402));
#288576=CARTESIAN_POINT('Ctrl Pts',(0.541652309731358,1.59802532479866,
11.3684254046204));
#288577=CARTESIAN_POINT('Ctrl Pts',(0.901589915619032,-1.26415389587918,
0.00156757034352902));
#288578=CARTESIAN_POINT('Ctrl Pts',(1.32199638747131,-0.964337455893649,
0.0386166509585065));
#288579=CARTESIAN_POINT('Ctrl Pts',(1.83279936330088,0.0823089634603651,
0.112702948401963));
#288580=CARTESIAN_POINT('Ctrl Pts',(0.923282202193781,1.58732060670271,
0.223826462673898));
#288581=CARTESIAN_POINT('Ctrl Pts',(-0.831632123374875,1.63523016946011,
0.334938113159335));
#288582=CARTESIAN_POINT('Ctrl Pts',(-1.82526888708922,0.189389157069568,
0.446049763644772));
#288583=CARTESIAN_POINT('Ctrl Pts',(-1.14915115289507,-1.4309470818998,
0.557161414130209));
#288584=CARTESIAN_POINT('Ctrl Pts',(0.57845453723465,-1.74144804628265,
0.668273064615646));
#288585=CARTESIAN_POINT('Ctrl Pts',(1.77676450212934,-0.459006752310191,
0.779384715101083));
#288586=CARTESIAN_POINT('Ctrl Pts',(1.34951570028772,1.24356332530328,0.890496365586519));
#288587=CARTESIAN_POINT('Ctrl Pts',(-0.312442258131127,1.8082852788653,
1.00160801607196));
#288588=CARTESIAN_POINT('Ctrl Pts',(-1.68853341832575,0.718627469092382,
1.1127196665574));
#288589=CARTESIAN_POINT('Ctrl Pts',(-1.51976346784924,-1.02853938746936,
1.22383131704283));
#288590=CARTESIAN_POINT('Ctrl Pts',(0.0394641425147256,-1.83466608009094,
1.33494296752827));
#288591=CARTESIAN_POINT('Ctrl Pts',(1.56258416088533,-0.962235197172911,
1.44605461801371));
#288592=CARTESIAN_POINT('Ctrl Pts',(1.65607219184445,0.790563389392543,
1.55716626849914));
#288593=CARTESIAN_POINT('Ctrl Pts',(0.234393589654803,1.82006124714437,
1.66827791898458));
#288594=CARTESIAN_POINT('Ctrl Pts',(-1.40173518708264,1.184357688178,1.77938956947002));
#288595=CARTESIAN_POINT('Ctrl Pts',(-1.75539465934889,-0.534933739960341,
1.89050121995545));
#288596=CARTESIAN_POINT('Ctrl Pts',(-0.503016113620211,-1.7648056590657,
2.00161287044089));
#288597=CARTESIAN_POINT('Ctrl Pts',(1.20957969869399,-1.38002948714164,
2.11272452092633));
#288598=CARTESIAN_POINT('Ctrl Pts',(1.8155121814438,0.267357277299772,2.22383617141177));
#288599=CARTESIAN_POINT('Ctrl Pts',(0.760404229172604,1.67013465544135,
2.3349478218972));
#288600=CARTESIAN_POINT('Ctrl Pts',(-0.990409415564645,1.54487979450293,
2.44605947238264));
#288601=CARTESIAN_POINT('Ctrl Pts',(-1.83508203153925,0.00619028873297843,
2.55717112286807));
#288602=CARTESIAN_POINT('Ctrl Pts',(-1.00080945733949,-1.53816280287764,
2.66828277335352));
#288603=CARTESIAN_POINT('Ctrl Pts',(0.749119307574141,-1.67522674451834,
2.77939442383895));
#288604=CARTESIAN_POINT('Ctrl Pts',(1.81366712743903,-0.279599592198403,
2.89050607432439));
#288605=CARTESIAN_POINT('Ctrl Pts',(1.21886258797946,1.37183758962537,3.00161772480983));
#288606=CARTESIAN_POINT('Ctrl Pts',(-0.491098354841707,1.76815915211019,
3.11272937529526));
#288607=CARTESIAN_POINT('Ctrl Pts',(-1.75174574872692,0.546764312014174,
3.2238410257807));
#288608=CARTESIAN_POINT('Ctrl Pts',(-1.4096936191513,-1.17487372988056,
3.33495267626613));
#288609=CARTESIAN_POINT('Ctrl Pts',(0.222109202401656,-1.82160146116971,
3.44606432675158));
#288610=CARTESIAN_POINT('Ctrl Pts',(1.6507008484237,-0.80171758749588,3.557175977237));
#288611=CARTESIAN_POINT('Ctrl Pts',(1.56904052720829,0.951670218649055,
3.66828762772245));
#288612=CARTESIAN_POINT('Ctrl Pts',(0.0518405410397911,1.8343600898957,
3.77939927820788));
#288613=CARTESIAN_POINT('Ctrl Pts',(-1.51278916515584,1.03876528767484,
3.89051092869332));
#288614=CARTESIAN_POINT('Ctrl Pts',(-1.69334445540273,-0.707212087317697,
4.00162257917875));
#288615=CARTESIAN_POINT('Ctrl Pts',(-0.324632476889834,-1.80615008679826,
4.1127342296642));
#288616=CARTESIAN_POINT('Ctrl Pts',(1.34109082097837,-1.25261318489772,
4.22384588014963));
#288617=CARTESIAN_POINT('Ctrl Pts',(1.77982919752865,0.446959068278794,
4.33495753063507));
#288618=CARTESIAN_POINT('Ctrl Pts',(0.590174065057926,1.73760149459688,
4.44606918112051));
#288619=CARTESIAN_POINT('Ctrl Pts',(-1.13944052985299,1.43848519631609,
4.55718083160594));
#288620=CARTESIAN_POINT('Ctrl Pts',(-1.82656320177237,-0.176723657225873,
4.66829248209138));
#288621=CARTESIAN_POINT('Ctrl Pts',(-0.842534694852325,-1.63024527880388,
4.77940413257681));
#288622=CARTESIAN_POINT('Ctrl Pts',(0.912341953073382,-1.59223005302452,
4.89051578306226));
#288623=CARTESIAN_POINT('Ctrl Pts',(1.83250271002755,-0.0974587032229718,
5.00162743354769));
#288624=CARTESIAN_POINT('Ctrl Pts',(1.07607813934704,1.48647913510807,5.11273908403313));
#288625=CARTESIAN_POINT('Ctrl Pts',(-0.664867114410965,1.71041401457865,
5.22385073451856));
#288626=CARTESIAN_POINT('Ctrl Pts',(-1.7975150692081,0.369464419209799,
5.334962385004));
#288627=CARTESIAN_POINT('Ctrl Pts',(-1.28558843497708,-1.30951393919477,
5.44607403548944));
#288628=CARTESIAN_POINT('Ctrl Pts',(0.402543121443117,-1.79039755821746,
5.55718568597487));
#288629=CARTESIAN_POINT('Ctrl Pts',(1.72238169392461,-0.633218510093957,
5.66829733646031));
#288630=CARTESIAN_POINT('Ctrl Pts',(1.46638637496419,1.10330203498933,5.77940898694574));
#288631=CARTESIAN_POINT('Ctrl Pts',(-0.131228723031326,1.83039433001302,
5.89052063743119));
#288632=CARTESIAN_POINT('Ctrl Pts',(-1.60878061435619,0.882830287180914,
6.00163228791661));
#288633=CARTESIAN_POINT('Ctrl Pts',(-1.61443401480672,-0.872448962935536,
6.11274393840206));
#288634=CARTESIAN_POINT('Ctrl Pts',(-0.143016540083152,-1.82951104133176,
6.22385558888749));
#288635=CARTESIAN_POINT('Ctrl Pts',(1.4592489990937,-1.11272491647141,6.33496723937292));
#288636=CARTESIAN_POINT('Ctrl Pts',(1.726424855806,0.622110599771014,6.44607888985837));
#288637=CARTESIAN_POINT('Ctrl Pts',(0.414067669173098,1.78776741955932,
6.5571905403438));
#288638=CARTESIAN_POINT('Ctrl Pts',(-1.27712648996998,1.31776792710599,
6.66830219082924));
#288639=CARTESIAN_POINT('Ctrl Pts',(-1.79985769246887,-0.357878007081822,
6.77941384131468));
#288640=CARTESIAN_POINT('Ctrl Pts',(-0.675871003359114,-1.70609576750853,
6.89052549180013));
#288641=CARTESIAN_POINT('Ctrl Pts',(1.06648061443804,-1.49337988473134,
7.00163714228554));
#288642=CARTESIAN_POINT('Ctrl Pts',(1.8330924744769,0.0856525604305603,
7.112748792771));
#288643=CARTESIAN_POINT('Ctrl Pts',(0.922579422182522,1.58632014135147,
7.22386044325642));
#288644=CARTESIAN_POINT('Ctrl Pts',(-0.832015941338537,1.63563866867091,
7.33497209374186));
#288645=CARTESIAN_POINT('Ctrl Pts',(-1.82538693560014,0.188485852073177,
7.44608374422731));
#288646=CARTESIAN_POINT('Ctrl Pts',(-1.14868293530086,-1.43111561211513,
7.55719539471273));
#288647=CARTESIAN_POINT('Ctrl Pts',(0.57896900897335,-1.74136706864058,
7.66830704519818));
#288648=CARTESIAN_POINT('Ctrl Pts',(1.77691317148419,-0.458414618104187,
7.7794186956836));
#288649=CARTESIAN_POINT('Ctrl Pts',(1.34913174271418,1.24394852059397,7.89053034616905));
#288650=CARTESIAN_POINT('Ctrl Pts',(-0.31299137216547,1.80820374462534,
8.00164199665448));
#288651=CARTESIAN_POINT('Ctrl Pts',(-1.68875379605891,0.718105143649537,
8.11275364713992));
#288652=CARTESIAN_POINT('Ctrl Pts',(-1.51944901709812,-1.02899906001644,
8.22386529762534));
#288653=CARTESIAN_POINT('Ctrl Pts',(0.0400233803440546,-1.83465596511855,
8.3349769481108));
#288654=CARTESIAN_POINT('Ctrl Pts',(1.5628777623923,-0.961757495684236,
8.44608859859622));
#288655=CARTESIAN_POINT('Ctrl Pts',(1.65583088939842,0.791067915431072,
8.55720024908167));
#288656=CARTESIAN_POINT('Ctrl Pts',(0.233838494230872,1.82013294600853,
8.6683118995671));
#288657=CARTESIAN_POINT('Ctrl Pts',(-1.40209638787114,1.18392993761256,
8.77942355005254));
#288658=CARTESIAN_POINT('Ctrl Pts',(-1.7552314048651,-0.535469044416299,
8.89053520053798));
#288659=CARTESIAN_POINT('Ctrl Pts',(-0.502477814519769,-1.76495904649879,
9.00164685102341));
#288660=CARTESIAN_POINT('Ctrl Pts',(1.21000056490795,-1.37966046256758,
9.11275850150884));
#288661=CARTESIAN_POINT('Ctrl Pts',(1.81543055389654,0.26791099020919,9.2238701519943));
#288662=CARTESIAN_POINT('Ctrl Pts',(0.759894778684712,1.67036653408787,
9.3349818024797));
#288663=CARTESIAN_POINT('Ctrl Pts',(-0.990880553059603,1.54457759740332,
9.44609345296518));
#288664=CARTESIAN_POINT('Ctrl Pts',(-1.83508387057358,0.00563064643204322,
9.55720510345058));
#288665=CARTESIAN_POINT('Ctrl Pts',(-1.00034018779382,-1.53846812672104,
9.66831675393604));
#288666=CARTESIAN_POINT('Ctrl Pts',(0.749630099412679,-1.67499791411289,
9.77942840442146));
#288667=CARTESIAN_POINT('Ctrl Pts',(1.81375257587983,-0.27904689702204,
9.89054005490692));
#288668=CARTESIAN_POINT('Ctrl Pts',(1.21844362791154,1.37221024632886,10.0016517053923));
#288669=CARTESIAN_POINT('Ctrl Pts',(-0.491636721550935,1.76800745982683,
10.1127633558778));
#288670=CARTESIAN_POINT('Ctrl Pts',(-1.75191417693461,0.546233454157225,
10.2238750063632));
#288671=CARTESIAN_POINT('Ctrl Pts',(-1.40933189096927,-1.17531024212075,
10.3349866568486));
#288672=CARTESIAN_POINT('Ctrl Pts',(0.222658485146653,-1.82152107136295,
10.4460983073341));
#288673=CARTESIAN_POINT('Ctrl Pts',(1.65095731823241,-0.801237981337174,
10.5572099578195));
#288674=CARTESIAN_POINT('Ctrl Pts',(1.56872731250459,0.952194262582688,
10.6683216083049));
#288675=CARTESIAN_POINT('Ctrl Pts',(0.0513245875236328,1.83428916375378,
10.7794332587904));
#288676=CARTESIAN_POINT('Ctrl Pts',(-1.51318883271867,1.038468815099,10.8905449092758));
#288677=CARTESIAN_POINT('Ctrl Pts',(-1.69297076565553,-0.708042900979278,
11.0016565597613));
#288678=CARTESIAN_POINT('Ctrl Pts',(-0.324382865468596,-1.80564820835397,
11.1127682102467));
#288679=CARTESIAN_POINT('Ctrl Pts',(1.34205240493473,-1.25336829214711,
11.2238798607321));
#288680=CARTESIAN_POINT('Ctrl Pts',(1.77858387719695,0.450076510096708,
11.3350034182694));
#288681=CARTESIAN_POINT('Ctrl Pts',(0.987482885158952,1.30479864697375,
11.4090897589781));
#288682=CARTESIAN_POINT('Ctrl Pts',(0.498442899895145,1.47054551912389,
11.4461388828584));
#288683=CARTESIAN_POINT('Ctrl Pts',(0.863567639152675,1.75641488315944,
6.58110718698701E-16));
#288684=CARTESIAN_POINT('Ctrl Pts',(0.902605506355986,1.73244147111074,
1.41492757312224E-15));
#288685=CARTESIAN_POINT('Ctrl Pts',(0.940681517855526,1.70703362163956,
3.0153021400338E-15));
#288686=CARTESIAN_POINT('Ctrl Pts',(0.977705169885399,1.68018661523996,
1.89431803576667E-15));
#288687=CARTESIAN_POINT('Ctrl Pts',(1.0358643592122,1.63801357064694,2.65822224384553E-16));
#288688=CARTESIAN_POINT('Ctrl Pts',(1.09142895154027,1.59229038852923,3.29238884271004E-15));
#288689=CARTESIAN_POINT('Ctrl Pts',(1.14423757319707,1.54335784953327,4.25354196309513E-15));
#288690=CARTESIAN_POINT('Ctrl Pts',(1.18228615197471,1.50810198588135,5.04045922924434E-15));
#288691=CARTESIAN_POINT('Ctrl Pts',(1.21890323710713,1.47117925249246,2.90921159275611E-15));
#288692=CARTESIAN_POINT('Ctrl Pts',(1.25401379483509,1.43270976178997,3.57006091356027E-15));
#288693=CARTESIAN_POINT('Ctrl Pts',(1.26389181876557,1.42188673377951,3.51159535440953E-15));
#288694=CARTESIAN_POINT('Ctrl Pts',(1.27364380619492,1.41094858444086,1.87046246663327E-15));
#288695=CARTESIAN_POINT('Ctrl Pts',(1.28326720497828,1.3998998522991,2.22044604925031E-15));
#288696=CARTESIAN_POINT('Ctrl Pts',(1.3301037638391,1.34612627344776,4.69467974937994E-15));
#288697=CARTESIAN_POINT('Ctrl Pts',(1.37390887238432,1.28972344251136,1.71987005091003E-15));
#288698=CARTESIAN_POINT('Ctrl Pts',(1.41451968724013,1.23102458107283,2.50494069931051E-15));
#288699=CARTESIAN_POINT('Ctrl Pts',(1.45487033903532,1.17270175925579,3.28498198832941E-15));
#288700=CARTESIAN_POINT('Ctrl Pts',(1.49206780791658,1.11211115787746,4.00139226059959E-15));
#288701=CARTESIAN_POINT('Ctrl Pts',(1.525903395753,1.04956595044032,4.00374178255447E-15));
#288702=CARTESIAN_POINT('Ctrl Pts',(1.5305357317926,1.0410030603875,4.0040634490578E-15));
#288703=CARTESIAN_POINT('Ctrl Pts',(1.53510497437072,1.03240352730891,3.37876692969174E-15));
#288704=CARTESIAN_POINT('Ctrl Pts',(1.53961051084785,1.02376815184549,3.41393580072236E-15));
#288705=CARTESIAN_POINT('Ctrl Pts',(1.5453767175419,1.01271655786648,3.46566903485334E-15));
#288706=CARTESIAN_POINT('Ctrl Pts',(1.55103417937643,1.00161467257822,3.03674728701833E-15));
#288707=CARTESIAN_POINT('Ctrl Pts',(1.55658137030158,0.990465869694388,
3.02535774210355E-15));
#288708=CARTESIAN_POINT('Ctrl Pts',(1.58754193823296,0.928240993410824,
2.09404046666805E-15));
#288709=CARTESIAN_POINT('Ctrl Pts',(1.61507975241109,0.864539873642212,
1.89375059754463E-15));
#288710=CARTESIAN_POINT('Ctrl Pts',(1.63904156643728,0.799669212580803,
2.04003480774873E-15));
#288711=CARTESIAN_POINT('Ctrl Pts',(1.66267720699393,0.735681585189814,
2.18432776519006E-15));
#288712=CARTESIAN_POINT('Ctrl Pts',(1.68283372774119,0.670555047536874,
9.94305425112374E-16));
#288713=CARTESIAN_POINT('Ctrl Pts',(1.69931410754026,0.604578807305152,
9.43689570931383E-16));
#288714=CARTESIAN_POINT('Ctrl Pts',(1.71527610637215,0.540677812161158,
8.94665809636882E-16));
#288715=CARTESIAN_POINT('Ctrl Pts',(1.72778958794875,0.475978937320602,
1.95320499488021E-15));
#288716=CARTESIAN_POINT('Ctrl Pts',(1.73662725954747,0.410752997999464,
2.31759056390501E-15));
#288717=CARTESIAN_POINT('Ctrl Pts',(1.73865677872466,0.395774245595767,
2.40126956147422E-15));
#288718=CARTESIAN_POINT('Ctrl Pts',(1.74049224208592,0.380767759452602,
2.15272180223388E-15));
#288719=CARTESIAN_POINT('Ctrl Pts',(1.74213052178609,0.365736946962489,
1.98452365651747E-15));
#288720=CARTESIAN_POINT('Ctrl Pts',(1.74338539139703,0.354223827548557,
1.9006075599436E-15));
#288721=CARTESIAN_POINT('Ctrl Pts',(1.74452450777523,0.342696049837885,
3.20340688219071E-16));
#288722=CARTESIAN_POINT('Ctrl Pts',(1.74554535151306,0.331170337018761,
7.21644966006352E-16));
#288723=CARTESIAN_POINT('Ctrl Pts',(1.75129431083391,0.266262406759458,
2.83665743705786E-15));
#288724=CARTESIAN_POINT('Ctrl Pts',(1.75331011127704,0.201301920292928,
5.37283262797766E-16));
#288725=CARTESIAN_POINT('Ctrl Pts',(1.75142561531545,0.136549272921142,
-1.11022302462516E-15));
#288726=CARTESIAN_POINT('Ctrl Pts',(1.75088296778463,0.117903510379641,
-1.47891683923337E-15));
#288727=CARTESIAN_POINT('Ctrl Pts',(1.75001659332986,0.0992750230412608,
-4.137032525397E-16));
#288728=CARTESIAN_POINT('Ctrl Pts',(1.74882170147482,0.080670175218092,
-5.96744875736022E-16));
#288729=CARTESIAN_POINT('Ctrl Pts',(1.74456409946248,0.0143779520375277,
-1.14186309985328E-15));
#288730=CARTESIAN_POINT('Ctrl Pts',(1.73613918364975,-0.0516159836678278,
-1.20522593144347E-15));
#288731=CARTESIAN_POINT('Ctrl Pts',(1.72372245238697,-0.117006780976604,
-9.15933995315754E-16));
#288732=CARTESIAN_POINT('Ctrl Pts',(1.71175318101375,-0.180041099891606,
-6.3706722947246E-16));
#288733=CARTESIAN_POINT('Ctrl Pts',(1.69607374898919,-0.242515614155525,
-3.38441552534961E-15));
#288734=CARTESIAN_POINT('Ctrl Pts',(1.67680493801022,-0.304129401844208,
-1.66533453693773E-15));
#288735=CARTESIAN_POINT('Ctrl Pts',(1.67349552259788,-0.314711560692092,
-1.43194362083307E-15));
#288736=CARTESIAN_POINT('Ctrl Pts',(1.67008173945308,-0.32526302074398,
-9.20645452357687E-16));
#288737=CARTESIAN_POINT('Ctrl Pts',(1.66656691458475,-0.335775244456301,
-1.38777878078145E-15));
#288738=CARTESIAN_POINT('Ctrl Pts',(1.64602231395326,-0.397220535760641,
-3.28484698948248E-15));
#288739=CARTESIAN_POINT('Ctrl Pts',(1.62200575451327,-0.457403213326927,
-2.70920381044168E-15));
#288740=CARTESIAN_POINT('Ctrl Pts',(1.59470364320676,-0.516049647263231,
-3.10862446895044E-15));
#288741=CARTESIAN_POINT('Ctrl Pts',(1.56766036096921,-0.574140102150036,
-3.50425854568154E-15));
#288742=CARTESIAN_POINT('Ctrl Pts',(1.53739275011846,-0.630724091745741,
-3.35336214633415E-15));
#288743=CARTESIAN_POINT('Ctrl Pts',(1.50404316674669,-0.685503900933402,
-2.96984659087229E-15));
#288744=CARTESIAN_POINT('Ctrl Pts',(1.47096966581936,-0.739830218889776,
-2.58950594499927E-15));
#288745=CARTESIAN_POINT('Ctrl Pts',(1.43486430828708,-0.792382821984317,
-9.97104400078256E-17));
#288746=CARTESIAN_POINT('Ctrl Pts',(1.39583852741916,-0.842828743497356,
-2.02615701994091E-15));
#288747=CARTESIAN_POINT('Ctrl Pts',(1.38891448399703,-0.851778974428235,
-2.60911541074168E-15));
#288748=CARTESIAN_POINT('Ctrl Pts',(1.38189845475662,-0.860662765012676,
-2.92338460246606E-15));
#288749=CARTESIAN_POINT('Ctrl Pts',(1.3747909965488,-0.869478087839507,
-2.83106871279415E-15));
#288750=CARTESIAN_POINT('Ctrl Pts',(1.36801000346398,-0.877888498619476,
-2.65001119591314E-15));
#288751=CARTESIAN_POINT('Ctrl Pts',(1.36114891147745,-0.8862326313589,-1.96909756090429E-15));
#288752=CARTESIAN_POINT('Ctrl Pts',(1.35421355798306,-0.894502968665375,
-1.94289029309402E-15));
#288753=CARTESIAN_POINT('Ctrl Pts',(1.31434175760682,-0.942049678201485,
-1.45304958986999E-15));
#288754=CARTESIAN_POINT('Ctrl Pts',(1.2719676049916,-0.9872233030338,-1.28559172267538E-15));
#288755=CARTESIAN_POINT('Ctrl Pts',(1.22722986402212,-1.02975664628297,
-1.74860126378462E-15));
#288756=CARTESIAN_POINT('Ctrl Pts',(1.18329662428731,-1.07152512911637,
-2.16477509457826E-15));
#288757=CARTESIAN_POINT('Ctrl Pts',(1.13708333145971,-1.11074797100956,
-2.12946189812955E-15));
#288758=CARTESIAN_POINT('Ctrl Pts',(1.08869802628372,-1.14712822354084,
-2.33146835171283E-15));
#288759=CARTESIAN_POINT('Ctrl Pts',(1.04185702698958,-1.18234733349458,
-1.71822951363253E-15));
#288760=CARTESIAN_POINT('Ctrl Pts',(0.992979843245106,-1.21490270869377,
1.81230356841659E-15));
#288761=CARTESIAN_POINT('Ctrl Pts',(0.942151955843589,-1.24447758124097,
3.5527136788005E-15));
#288762=CARTESIAN_POINT('Ctrl Pts',(0.929425469399051,-1.25188265420018,
3.19009398667763E-15));
#288763=CARTESIAN_POINT('Ctrl Pts',(0.916576650434786,-1.25910062270965,
2.60075520077752E-15));
#288764=CARTESIAN_POINT('Ctrl Pts',(0.903606778650244,-1.26612599672281,
4.16333634234434E-16));
#288765=CARTESIAN_POINT('Ctrl Pts',(-0.684399482591588,1.39375527916939,
-0.23169217219233));
#288766=CARTESIAN_POINT('Ctrl Pts',(-1.14813007759954,1.16604830489444,
-0.194624624464132));
#288767=CARTESIAN_POINT('Ctrl Pts',(-1.82232784108757,0.215386159079778,
-0.120494936792213));
#288768=CARTESIAN_POINT('Ctrl Pts',(-1.16734347439351,-1.41806245612601,
-0.0093031091765735));
#288769=CARTESIAN_POINT('Ctrl Pts',(0.558471034725876,-1.74792270953766,
0.101883310654589));
#288770=CARTESIAN_POINT('Ctrl Pts',(1.77191842122005,-0.478866139559988,
0.213069730485752));
#288771=CARTESIAN_POINT('Ctrl Pts',(1.36262118629268,1.23002510036026,0.324256150316915));
#288772=CARTESIAN_POINT('Ctrl Pts',(-0.295111057128028,1.81154554732604,
0.435442570148077));
#288773=CARTESIAN_POINT('Ctrl Pts',(-1.68239591977648,0.733934265747275,
0.54662898997924));
#288774=CARTESIAN_POINT('Ctrl Pts',(-1.52859240585868,-1.01616207295397,
0.657815409810402));
#288775=CARTESIAN_POINT('Ctrl Pts',(0.025499203811463,-1.83532087192271,
0.769001829641565));
#288776=CARTESIAN_POINT('Ctrl Pts',(1.55621608150441,-0.973292876645946,
0.880188249472728));
#288777=CARTESIAN_POINT('Ctrl Pts',(1.66138010486741,0.780338174659502,
0.99137466930389));
#288778=CARTESIAN_POINT('Ctrl Pts',(0.244643362335791,1.81913270512971,
1.10256108913506));
#288779=CARTESIAN_POINT('Ctrl Pts',(-1.39619494321738,1.19152953216238,
1.21374750896622));
#288780=CARTESIAN_POINT('Ctrl Pts',(-1.75805935358985,-0.527569944496845,
1.32493392879738));
#288781=CARTESIAN_POINT('Ctrl Pts',(-0.509464470574177,-1.76339059445253,
1.43612034862854));
#288782=CARTESIAN_POINT('Ctrl Pts',(1.20582162646513,-1.38386993918644,
1.54730676845971));
#288783=CARTESIAN_POINT('Ctrl Pts',(1.81652298091137,0.263336133863676,
1.65849318829087));
#288784=CARTESIAN_POINT('Ctrl Pts',(0.763210382228217,1.66931461278863,
1.76967960812203));
#288785=CARTESIAN_POINT('Ctrl Pts',(-0.989235987808251,1.54612862738527,
1.88086602795319));
#288786=CARTESIAN_POINT('Ctrl Pts',(-1.83549930227322,0.00662166747232072,
1.99205244778436));
#288787=CARTESIAN_POINT('Ctrl Pts',(-1.00036561103327,-1.53895098784626,
2.10323886761552));
#288788=CARTESIAN_POINT('Ctrl Pts',(0.751146372438219,-1.67477779326081,
2.21442528744668));
#288789=CARTESIAN_POINT('Ctrl Pts',(1.81457569490279,-0.276435470852209,
2.32561170727784));
#288790=CARTESIAN_POINT('Ctrl Pts',(1.21577495550945,1.37513373000844,2.43679812710901));
#288791=CARTESIAN_POINT('Ctrl Pts',(-0.496728387120161,1.76702077853356,
2.54798454694017));
#288792=CARTESIAN_POINT('Ctrl Pts',(-1.75420697769208,0.54024013213266,
2.65917096677134));
#288793=CARTESIAN_POINT('Ctrl Pts',(-1.40475587210311,-1.18142391219023,
2.77035738660249));
#288794=CARTESIAN_POINT('Ctrl Pts',(0.231512555941918,-1.82085239862611,
2.88154380643366));
#288795=CARTESIAN_POINT('Ctrl Pts',(1.65570543891066,-0.79230109204954,
2.99273022626482));
#288796=CARTESIAN_POINT('Ctrl Pts',(1.56320030886811,0.96203238782093,3.10391664609599));
#288797=CARTESIAN_POINT('Ctrl Pts',(0.0387358782285723,1.83510246381186,
3.21510306592715));
#288798=CARTESIAN_POINT('Ctrl Pts',(-1.5212122973926,1.0271390690517,3.32628948575831));
#288799=CARTESIAN_POINT('Ctrl Pts',(-1.68766401250321,-0.721728274221359,
3.43747590558947));
#288800=CARTESIAN_POINT('Ctrl Pts',(-0.30814227474981,-1.80946120694338,
3.54866232542063));
#288801=CARTESIAN_POINT('Ctrl Pts',(1.35365115508378,-1.23964917265128,
3.6598487452518));
#288802=CARTESIAN_POINT('Ctrl Pts',(1.77544140021948,0.465735284578745,
3.77103516508296));
#288803=CARTESIAN_POINT('Ctrl Pts',(0.570850297216628,1.74448601573192,
3.88222158491412));
#288804=CARTESIAN_POINT('Ctrl Pts',(-1.15666444373811,1.42521187390071,
3.99340800474529));
#288805=CARTESIAN_POINT('Ctrl Pts',(-1.82462437363633,-0.199618175645153,
4.10459442457644));
#288806=CARTESIAN_POINT('Ctrl Pts',(-0.821149217997519,-1.64158931608911,
4.21578084440761));
#288807=CARTESIAN_POINT('Ctrl Pts',(0.934534245966791,-1.57979342448024,
4.32696726423877));
#288808=CARTESIAN_POINT('Ctrl Pts',(1.83414379690324,-0.0708382184779958,
4.43815368406993));
#288809=CARTESIAN_POINT('Ctrl Pts',(1.05359805760058,1.50300786888694,4.5493401039011));
#288810=CARTESIAN_POINT('Ctrl Pts',(-0.692089211636685,1.7000335420373,
4.66052652373226));
#288811=CARTESIAN_POINT('Ctrl Pts',(-1.80379273749893,0.339754736629052,
4.77171294356342));
#288812=CARTESIAN_POINT('Ctrl Pts',(-1.26314386028315,-1.33175414741037,
4.88289936339459));
#288813=CARTESIAN_POINT('Ctrl Pts',(0.43459959303458,-1.78331845575879,
4.99408578322575));
#288814=CARTESIAN_POINT('Ctrl Pts',(1.73423096451572,-0.601285691356955,
5.10527220305691));
#288815=CARTESIAN_POINT('Ctrl Pts',(1.44523153483113,1.13155085243458,5.21645862288808));
#288816=CARTESIAN_POINT('Ctrl Pts',(-0.167662680511327,1.82783772432881,
5.32764504271924));
#288817=CARTESIAN_POINT('Ctrl Pts',(-1.62697060664768,0.84974594204401,
5.4388314625504));
#288818=CARTESIAN_POINT('Ctrl Pts',(-1.59590287279599,-0.906749988429709,
5.55001788238156));
#288819=CARTESIAN_POINT('Ctrl Pts',(-0.102918871003275,-1.83262359116846,
5.66120430221273));
#288820=CARTESIAN_POINT('Ctrl Pts',(1.48434328164846,-1.07973447807358,
5.77239072204388));
#288821=CARTESIAN_POINT('Ctrl Pts',(1.7118825917383,0.66223826000852,5.88357714187506));
#288822=CARTESIAN_POINT('Ctrl Pts',(0.371263179685662,1.79757202145712,
5.99476356170621));
#288823=CARTESIAN_POINT('Ctrl Pts',(-1.30944941179655,1.28625182560081,
6.10594998153738));
#288824=CARTESIAN_POINT('Ctrl Pts',(-1.79064953307602,-0.40333084510164,
6.21713640136854));
#288825=CARTESIAN_POINT('Ctrl Pts',(-0.631536996732062,-1.72344496363371,
6.3283228211997));
#288826=CARTESIAN_POINT('Ctrl Pts',(1.10609082714422,-1.46480872574654,
6.43950924103086));
#288827=CARTESIAN_POINT('Ctrl Pts',(1.83049146684385,0.135655854011535,
6.55069566086203));
#288828=CARTESIAN_POINT('Ctrl Pts',(0.878082509091036,1.61185378621765,
6.66188208069318));
#288829=CARTESIAN_POINT('Ctrl Pts',(-0.878688121616026,1.61152372177596,
6.77306850052436));
#288830=CARTESIAN_POINT('Ctrl Pts',(-1.83054231202212,0.134968014034564,
6.88425492035551));
#288831=CARTESIAN_POINT('Ctrl Pts',(-1.10554032858663,-1.46522424999876,
6.99544134018668));
#288832=CARTESIAN_POINT('Ctrl Pts',(0.632184558464056,-1.72320753391902,
7.10662776001784));
#288833=CARTESIAN_POINT('Ctrl Pts',(1.79080096334203,-0.402657957339467,
7.217814179849));
#288834=CARTESIAN_POINT('Ctrl Pts',(1.30896599390356,1.28674377702811,7.32900059968016));
#288835=CARTESIAN_POINT('Ctrl Pts',(-0.371938613975646,1.79743238769886,
7.44018701951133));
#288836=CARTESIAN_POINT('Ctrl Pts',(-1.71213131531173,0.661594951646106,
7.55137343934249));
#288837=CARTESIAN_POINT('Ctrl Pts',(-1.48393745292332,-1.08029216267287,
7.66255985917366));
#288838=CARTESIAN_POINT('Ctrl Pts',(0.103607495311869,-1.83258478871351,
7.77374627900482));
#288839=CARTESIAN_POINT('Ctrl Pts',(1.59624348293943,-0.906150243659566,
7.88493269883597));
#288840=CARTESIAN_POINT('Ctrl Pts',(1.62665118897041,0.850357236913776,
7.99611911866715));
#288841=CARTESIAN_POINT('Ctrl Pts',(0.166975835438897,1.82790059665215,
8.10730553849828));
#288842=CARTESIAN_POINT('Ctrl Pts',(-1.44565662736788,1.13100770848327,
8.21849195832947));
#288843=CARTESIAN_POINT('Ctrl Pts',(-1.73400490139949,-0.601937308250454,
8.32967837816063));
#288844=CARTESIAN_POINT('Ctrl Pts',(-0.433929457718794,-1.78348163607784,
8.44086479799179));
#288845=CARTESIAN_POINT('Ctrl Pts',(1.26364419445534,-1.33127941123177,
8.55205121782296));
#288846=CARTESIAN_POINT('Ctrl Pts',(1.8036649433301,0.340432510995058,8.66323763765411));
#288847=CARTESIAN_POINT('Ctrl Pts',(0.691450352967021,1.70029348267665,
8.77442405748529));
#288848=CARTESIAN_POINT('Ctrl Pts',(-1.05416275630007,1.50261186116277,
8.88561047731643));
#288849=CARTESIAN_POINT('Ctrl Pts',(-1.83411705133878,-0.0715274186238769,
8.99679689714761));
#288850=CARTESIAN_POINT('Ctrl Pts',(-0.93394054821382,-1.58014447160157,
9.10798331697877));
#288851=CARTESIAN_POINT('Ctrl Pts',(0.821765999768745,-1.64128065142731,
9.21916973680992));
#288852=CARTESIAN_POINT('Ctrl Pts',(1.8246992696381,-0.198932519657866,
9.33035615664109));
#288853=CARTESIAN_POINT('Ctrl Pts',(1.15612879063603,1.42564637392063,9.44154257647225));
#288854=CARTESIAN_POINT('Ctrl Pts',(-0.571505712575411,1.74427144678546,
9.55272899630341));
#288855=CARTESIAN_POINT('Ctrl Pts',(-1.7756163895225,0.46506799577476,9.66391541613459));
#288856=CARTESIAN_POINT('Ctrl Pts',(-1.35318503866645,-1.24015752487752,
9.77510183596573));
#288857=CARTESIAN_POINT('Ctrl Pts',(0.308821787045722,-1.80934569414666,
9.88628825579692));
#288858=CARTESIAN_POINT('Ctrl Pts',(1.68793584191459,-0.721093294283745,
9.99747467562806));
#288859=CARTESIAN_POINT('Ctrl Pts',(1.52082480165556,1.0277091496512,10.1086610954593));
#288860=CARTESIAN_POINT('Ctrl Pts',(-0.0394227203814493,1.83509056147044,
10.2198475152904));
#288861=CARTESIAN_POINT('Ctrl Pts',(-1.56356686902893,0.961439630001686,
10.3310339351216));
#288862=CARTESIAN_POINT('Ctrl Pts',(-1.65539775368066,-0.792913103321646,
10.4422203549528));
#288863=CARTESIAN_POINT('Ctrl Pts',(-0.230847085212319,-1.82095846328463,
10.5534067747839));
#288864=CARTESIAN_POINT('Ctrl Pts',(1.4052354109789,-1.18085942306844,10.6645931946151));
#288865=CARTESIAN_POINT('Ctrl Pts',(1.75393587956343,0.540829674163776,
10.7757796144463));
#288866=CARTESIAN_POINT('Ctrl Pts',(0.496193799610693,1.76733979700505,
10.8869660342774));
#288867=CARTESIAN_POINT('Ctrl Pts',(-1.21653822386253,1.37442439623192,
10.9981524541086));
#288868=CARTESIAN_POINT('Ctrl Pts',(-1.81400015511254,-0.2766353780646,
11.1093388739397));
#288869=CARTESIAN_POINT('Ctrl Pts',(-0.751432125101304,-1.67598976072319,
11.2205252937709));
#288870=CARTESIAN_POINT('Ctrl Pts',(1.00302336056212,-1.53668295415482,
11.3317236110345));
#288871=CARTESIAN_POINT('Ctrl Pts',(1.55494787760704,-0.510025057698862,
11.4058597883545));
#288872=CARTESIAN_POINT('Ctrl Pts',(1.55271109992305,0.00668241897662998,
11.4429338257307));
#288873=CARTESIAN_POINT('Ctrl Pts',(-0.743729958480259,1.51457968960343,
-0.153977644258129));
#288874=CARTESIAN_POINT('Ctrl Pts',(-1.2476612806743,1.26713283607588,-0.116910096529931));
#288875=CARTESIAN_POINT('Ctrl Pts',(-1.98030513473999,0.234057948938039,
-0.0427804088580121));
#288876=CARTESIAN_POINT('Ctrl Pts',(-1.26854028360072,-1.54099405163692,
0.0684114187576278));
#288877=CARTESIAN_POINT('Ctrl Pts',(0.606884794676209,-1.89944983486631,
0.179597838588791));
#288878=CARTESIAN_POINT('Ctrl Pts',(1.9255257307534,-0.520378964554392,
0.290784258419953));
#288879=CARTESIAN_POINT('Ctrl Pts',(1.48074658745842,1.33665576916651,0.401970678251116));
#288880=CARTESIAN_POINT('Ctrl Pts',(-0.320694184971879,1.96858812574808,
0.513157098082277));
#288881=CARTESIAN_POINT('Ctrl Pts',(-1.82824253873584,0.797558903645778,
0.624343517913441));
#288882=CARTESIAN_POINT('Ctrl Pts',(-1.66110582409801,-1.10425299193025,
0.735529937744604));
#288883=CARTESIAN_POINT('Ctrl Pts',(0.027709725495631,-1.99442452923011,
0.846716357575766));
#288884=CARTESIAN_POINT('Ctrl Pts',(1.69112419153345,-1.05766747221376,
0.957902777406929));
#288885=CARTESIAN_POINT('Ctrl Pts',(1.80540486637151,0.84798555960686,1.06908919723809));
#288886=CARTESIAN_POINT('Ctrl Pts',(0.265851454217222,1.97683301298401,
1.18027561706925));
#288887=CARTESIAN_POINT('Ctrl Pts',(-1.51723084771687,1.29482302664448,
1.29146203690042));
#288888=CARTESIAN_POINT('Ctrl Pts',(-1.9104652228843,-0.57330489413916,
1.40264845673157));
#288889=CARTESIAN_POINT('Ctrl Pts',(-0.55362985973125,-1.91625862811955,
1.51383487656274));
#288890=CARTESIAN_POINT('Ctrl Pts',(1.31035410019542,-1.50383739116212,
1.6250212963939));
#288891=CARTESIAN_POINT('Ctrl Pts',(1.97399705221268,0.286164698960839,
1.73620771622506));
#288892=CARTESIAN_POINT('Ctrl Pts',(0.829372961734173,1.81402721544818,
1.84739413605623));
#288893=CARTESIAN_POINT('Ctrl Pts',(-1.07499268899777,1.68016225771552,
1.95858055588739));
#288894=CARTESIAN_POINT('Ctrl Pts',(-1.99461842767766,0.00719569871038447,
2.06976697571855));
#288895=CARTESIAN_POINT('Ctrl Pts',(-1.0870871373859,-1.67236238981361,
2.18095339554972));
#288896=CARTESIAN_POINT('Ctrl Pts',(0.816263124967095,-1.81996399811548,
2.29213981538088));
#288897=CARTESIAN_POINT('Ctrl Pts',(1.97188095630794,-0.300399615266935,
2.40332623521204));
#288898=CARTESIAN_POINT('Ctrl Pts',(1.32117028165843,1.49434384148169,2.5145126550432));
#288899=CARTESIAN_POINT('Ctrl Pts',(-0.539789687347405,1.92020351224723,
2.62569907487436));
#288900=CARTESIAN_POINT('Ctrl Pts',(-1.9062788851687,0.587073458207422,
2.73688549470553));
#288901=CARTESIAN_POINT('Ctrl Pts',(-1.52653392208601,-1.28384135217877,
2.84807191453669));
#288902=CARTESIAN_POINT('Ctrl Pts',(0.251582340428331,-1.97870178642002,
2.95925833436786));
#288903=CARTESIAN_POINT('Ctrl Pts',(1.79923826457862,-0.860985540290846,
3.07044475419901));
#288904=CARTESIAN_POINT('Ctrl Pts',(1.69871388039113,1.0454308135088,3.18163117403018));
#288905=CARTESIAN_POINT('Ctrl Pts',(0.0420938849888638,1.9941871873569,
3.29281759386134));
#288906=CARTESIAN_POINT('Ctrl Pts',(-1.65308593527184,1.11618158197113,
3.40400401369251));
#288907=CARTESIAN_POINT('Ctrl Pts',(-1.83396732153388,-0.784294776770008,
3.51519043352367));
#288908=CARTESIAN_POINT('Ctrl Pts',(-0.334855076654795,-1.96632309424865,
3.62637685335483));
#288909=CARTESIAN_POINT('Ctrl Pts',(1.47099894575461,-1.34711415066372,
3.737563273186));
#288910=CARTESIAN_POINT('Ctrl Pts',(1.92935411620901,0.506109797966104,
3.84874969301715));
#288911=CARTESIAN_POINT('Ctrl Pts',(0.620337213347576,1.89571521465329,
3.95993611284832));
#288912=CARTESIAN_POINT('Ctrl Pts',(-1.25693548957618,1.54876325123453,
4.07112253267948));
#288913=CARTESIAN_POINT('Ctrl Pts',(-1.98280075330865,-0.216923041674854,
4.18230895251065));
#288914=CARTESIAN_POINT('Ctrl Pts',(-0.89233450541905,-1.7838984174469,
4.2934953723418));
#288915=CARTESIAN_POINT('Ctrl Pts',(1.01554886236819,-1.71674545040129,
4.40468179217297));
#288916=CARTESIAN_POINT('Ctrl Pts',(1.99314541377542,-0.0769791717082739,
4.51586821200413));
#288917=CARTESIAN_POINT('Ctrl Pts',(1.14493429578145,1.63330336792476,4.6270546318353));
#288918=CARTESIAN_POINT('Ctrl Pts',(-0.752086308841275,1.84740916350018,
4.73824105166646));
#288919=CARTESIAN_POINT('Ctrl Pts',(-1.96016322614266,0.369208017530612,
4.84942747149762));
#288920=CARTESIAN_POINT('Ctrl Pts',(-1.37264558880974,-1.44720369017359,
4.96061389132878));
#288921=CARTESIAN_POINT('Ctrl Pts',(0.472274958565424,-1.93791403236648,
5.07180031115995));
#288922=CARTESIAN_POINT('Ctrl Pts',(1.88457115477419,-0.653411046680418,
5.18298673099111));
#288923=CARTESIAN_POINT('Ctrl Pts',(1.57051841319957,1.22964480527183,5.29417315082227));
#288924=CARTESIAN_POINT('Ctrl Pts',(-0.182197330049385,1.9862926688315,
5.40535957065344));
#288925=CARTESIAN_POINT('Ctrl Pts',(-1.76801241454587,0.923410274657261,
5.51654599048461));
#288926=CARTESIAN_POINT('Ctrl Pts',(-1.7342514240786,-0.985355992224259,
5.62773241031575));
#288927=CARTESIAN_POINT('Ctrl Pts',(-0.111840890598383,-1.99149342166151,
5.73891883014693));
#288928=CARTESIAN_POINT('Ctrl Pts',(1.61302075076181,-1.17333647814372,
5.85010524997808));
#288929=CARTESIAN_POINT('Ctrl Pts',(1.86028540532431,0.71964758324355,5.96129166980924));
#288930=CARTESIAN_POINT('Ctrl Pts',(0.403447922209576,1.9534032372748,6.07247808964042));
#288931=CARTESIAN_POINT('Ctrl Pts',(-1.42296536078566,1.39775677974926,
6.18366450947157));
#288932=CARTESIAN_POINT('Ctrl Pts',(-1.94588063954174,-0.438295528140028,
6.29485092930274));
#288933=CARTESIAN_POINT('Ctrl Pts',(-0.686284832623981,-1.87285011729214,
6.40603734913389));
#288934=CARTESIAN_POINT('Ctrl Pts',(1.20197765467668,-1.59179274749852,
6.51722376896506));
#288935=CARTESIAN_POINT('Ctrl Pts',(1.98917646383827,0.147415837150472,
6.62841018879622));
#288936=CARTESIAN_POINT('Ctrl Pts',(0.954203333929539,1.75158511949853,
6.7395966086274));
#288937=CARTESIAN_POINT('Ctrl Pts',(-0.954861446902296,1.75122644182599,
6.85078302845855));
#288938=CARTESIAN_POINT('Ctrl Pts',(-1.98923171677648,0.146668368441778,
6.96196944828972));
#288939=CARTESIAN_POINT('Ctrl Pts',(-1.20137943349188,-1.59224429347817,
7.07315586812087));
#288940=CARTESIAN_POINT('Ctrl Pts',(0.686988531373428,-1.87259210483547,
7.18434228795204));
#288941=CARTESIAN_POINT('Ctrl Pts',(1.946045197272,-0.437564307851112,7.29552870778319));
#288942=CARTESIAN_POINT('Ctrl Pts',(1.42244003547697,1.39829137836292,7.40671512761436));
#288943=CARTESIAN_POINT('Ctrl Pts',(-0.404181909784372,1.95325149868955,
7.51790154744553));
#288944=CARTESIAN_POINT('Ctrl Pts',(-1.86055569070241,0.718948506587575,
7.62908796727668));
#288945=CARTESIAN_POINT('Ctrl Pts',(-1.61257974081286,-1.17394250832697,
7.74027438710785));
#288946=CARTESIAN_POINT('Ctrl Pts',(0.11258921163228,-1.99145125542828,
7.85146080693901));
#288947=CARTESIAN_POINT('Ctrl Pts',(1.73462156165799,-0.984704255681033,
7.96264722677019));
#288948=CARTESIAN_POINT('Ctrl Pts',(1.76766530660397,0.924074562576307,
8.07383364660135));
#288949=CARTESIAN_POINT('Ctrl Pts',(0.181450942493336,1.98636099154596,
8.18502006643251));
#288950=CARTESIAN_POINT('Ctrl Pts',(-1.57098035693673,1.22905457626289,
8.29620648626366));
#288951=CARTESIAN_POINT('Ctrl Pts',(-1.88432549428448,-0.654119152132637,
8.40739290609483));
#288952=CARTESIAN_POINT('Ctrl Pts',(-0.471546729332007,-1.9380913587599,
8.51857932592599));
#288953=CARTESIAN_POINT('Ctrl Pts',(1.37318929686702,-1.44668779919563,
8.62976574575715));
#288954=CARTESIAN_POINT('Ctrl Pts',(1.96002435351886,0.369944548042224,
8.74095216558831));
#288955=CARTESIAN_POINT('Ctrl Pts',(0.751392067621162,1.84769163834976,
8.85213858541948));
#288956=CARTESIAN_POINT('Ctrl Pts',(-1.14554794811607,1.6328730303577,8.96332500525063));
#288957=CARTESIAN_POINT('Ctrl Pts',(-1.99311634964249,-0.0777281184986929,
9.07451142508181));
#288958=CARTESIAN_POINT('Ctrl Pts',(-1.01490369705703,-1.71712692973843,
9.18569784491295));
#288959=CARTESIAN_POINT('Ctrl Pts',(0.893004755898116,-1.78356299469757,
9.29688426474413));
#288960=CARTESIAN_POINT('Ctrl Pts',(1.98288214203219,-0.216177946285538,
9.40807068457528));
#288961=CARTESIAN_POINT('Ctrl Pts',(1.25635340079693,1.54923541798798,9.51925710440647));
#288962=CARTESIAN_POINT('Ctrl Pts',(-0.621049446553396,1.89548204476102,
9.6304435242376));
#288963=CARTESIAN_POINT('Ctrl Pts',(-1.92954427530524,0.505384662008117,
9.74162994406879));
#288964=CARTESIAN_POINT('Ctrl Pts',(-1.47049242178358,-1.34766657185882,
9.85281636389993));
#288965=CARTESIAN_POINT('Ctrl Pts',(0.335593495757164,-1.96619756766704,
9.96400278373111));
#288966=CARTESIAN_POINT('Ctrl Pts',(1.83426271579115,-0.783604750528571,
10.0751892035622));
#288967=CARTESIAN_POINT('Ctrl Pts',(1.65266484759463,1.11680108276175,10.1863756233934));
#288968=CARTESIAN_POINT('Ctrl Pts',(-0.0428402693722631,1.99417425320353,
10.2975620432246));
#288969=CARTESIAN_POINT('Ctrl Pts',(-1.69911221759054,1.04478666961406,
10.4087484630557));
#288970=CARTESIAN_POINT('Ctrl Pts',(-1.79890390616785,-0.861650606717026,
10.5199348828869));
#288971=CARTESIAN_POINT('Ctrl Pts',(-0.250859180153293,-1.97881704580591,
10.6311213027181));
#288972=CARTESIAN_POINT('Ctrl Pts',(1.52705503210616,-1.2832279275901,10.7423077225492));
#288973=CARTESIAN_POINT('Ctrl Pts',(1.90598428558895,0.587714107537896,
10.8534941423804));
#288974=CARTESIAN_POINT('Ctrl Pts',(0.539208756536806,1.92055018637627,
10.9646805622115));
#288975=CARTESIAN_POINT('Ctrl Pts',(-1.32199971761647,1.49357301567956,
11.0758669820427));
#288976=CARTESIAN_POINT('Ctrl Pts',(-1.97125552307022,-0.300616852401862,
11.1870534018739));
#288977=CARTESIAN_POINT('Ctrl Pts',(-0.816573649480457,-1.82128103083306,
11.2982398217051));
#288978=CARTESIAN_POINT('Ctrl Pts',(1.0899752867738,-1.66989774066344,11.4094381389687));
#288979=CARTESIAN_POINT('Ctrl Pts',(1.68974604725378,-0.554239044059365,
11.4835743162886));
#288980=CARTESIAN_POINT('Ctrl Pts',(1.68731536368905,0.00726171675233516,
11.5206483536649));
#288981=CARTESIAN_POINT('Ctrl Pts',(-0.80306043436893,1.63540410003748,
-0.0762631163239277));
#288982=CARTESIAN_POINT('Ctrl Pts',(-1.34719248374907,1.36821736725733,
-0.0391955685957298));
#288983=CARTESIAN_POINT('Ctrl Pts',(-2.1382824283924,0.252729738796303,
0.0349341190761892));
#288984=CARTESIAN_POINT('Ctrl Pts',(-1.36973709280792,-1.66392564714785,
0.146125946691829));
#288985=CARTESIAN_POINT('Ctrl Pts',(0.65529855462654,-2.05097696019496,
0.257312366522992));
#288986=CARTESIAN_POINT('Ctrl Pts',(2.07913304028677,-0.561891789548798,
0.368498786354154));
#288987=CARTESIAN_POINT('Ctrl Pts',(1.59887198862417,1.44328643797276,0.479685206185317));
#288988=CARTESIAN_POINT('Ctrl Pts',(-0.346277312815728,2.12563070417011,
0.59087162601648));
#288989=CARTESIAN_POINT('Ctrl Pts',(-1.9740891576952,0.861183541544282,
0.702058045847641));
#288990=CARTESIAN_POINT('Ctrl Pts',(-1.79361924233733,-1.19234391090653,
0.813244465678806));
#288991=CARTESIAN_POINT('Ctrl Pts',(0.0299202471797978,-2.15352818653751,
0.924430885509967));
#288992=CARTESIAN_POINT('Ctrl Pts',(1.82603230156248,-1.14204206778157,
1.03561730534113));
#288993=CARTESIAN_POINT('Ctrl Pts',(1.94942962787562,0.915632944554216,
1.14680372517229));
#288994=CARTESIAN_POINT('Ctrl Pts',(0.287059546098653,2.1345333208383,1.25799014500346));
#288995=CARTESIAN_POINT('Ctrl Pts',(-1.63826675221636,1.39811652112659,
1.36917656483462));
#288996=CARTESIAN_POINT('Ctrl Pts',(-2.06287109217876,-0.619039843781474,
1.48036298466578));
#288997=CARTESIAN_POINT('Ctrl Pts',(-0.597795248888325,-2.06912666178656,
1.59154940449694));
#288998=CARTESIAN_POINT('Ctrl Pts',(1.41488657392572,-1.6238048431378,1.70273582432811));
#288999=CARTESIAN_POINT('Ctrl Pts',(2.131471123514,0.308993264057997,1.81392224415927));
#289000=CARTESIAN_POINT('Ctrl Pts',(0.895535541240127,1.95873981810775,
1.92510866399043));
#289001=CARTESIAN_POINT('Ctrl Pts',(-1.16074939018729,1.81419588804578,
2.03629508382159));
#289002=CARTESIAN_POINT('Ctrl Pts',(-2.1537375530821,0.00776972994845119,
2.14748150365276));
#289003=CARTESIAN_POINT('Ctrl Pts',(-1.17380866373853,-1.80577379178097,
2.25866792348392));
#289004=CARTESIAN_POINT('Ctrl Pts',(0.881379877495971,-1.96515020297015,
2.36985434331508));
#289005=CARTESIAN_POINT('Ctrl Pts',(2.12918621771311,-0.32436375968166,
2.48104076314625));
#289006=CARTESIAN_POINT('Ctrl Pts',(1.42656560780741,1.61355395295493,2.59222718297741));
#289007=CARTESIAN_POINT('Ctrl Pts',(-0.582850987574644,2.07338624596089,
2.70341360280857));
#289008=CARTESIAN_POINT('Ctrl Pts',(-2.05835079264534,0.633906784282185,
2.81460002263973));
#289009=CARTESIAN_POINT('Ctrl Pts',(-1.64831197206892,-1.38625879216731,
2.92578644247089));
#289010=CARTESIAN_POINT('Ctrl Pts',(0.271652124914743,-2.13655117421392,
3.03697286230206));
#289011=CARTESIAN_POINT('Ctrl Pts',(1.94277109024656,-0.929669988532152,
3.14815928213322));
#289012=CARTESIAN_POINT('Ctrl Pts',(1.83422745191416,1.12882923919668,3.25934570196439));
#289013=CARTESIAN_POINT('Ctrl Pts',(0.0454518917491524,2.15327191090196,
3.37053212179554));
#289014=CARTESIAN_POINT('Ctrl Pts',(-1.78495957315107,1.20522409489056,
3.48171854162671));
#289015=CARTESIAN_POINT('Ctrl Pts',(-1.98027063056456,-0.84686127931866,
3.59290496145787));
#289016=CARTESIAN_POINT('Ctrl Pts',(-0.361567878559777,-2.12318498155391,
3.70409138128903));
#289017=CARTESIAN_POINT('Ctrl Pts',(1.58834673642544,-1.45457912867615,
3.8152778011202));
#289018=CARTESIAN_POINT('Ctrl Pts',(2.08326683219855,0.546484311353464,
3.92646422095136));
#289019=CARTESIAN_POINT('Ctrl Pts',(0.669824129478524,2.04694441357467,
4.03765064078252));
#289020=CARTESIAN_POINT('Ctrl Pts',(-1.35720653541426,1.67231462856835,
4.14883706061369));
#289021=CARTESIAN_POINT('Ctrl Pts',(-2.14097713298096,-0.234227907704556,
4.26002348044485));
#289022=CARTESIAN_POINT('Ctrl Pts',(-0.963519792840582,-1.92620751880469,
4.37120990027601));
#289023=CARTESIAN_POINT('Ctrl Pts',(1.09656347876959,-1.85369747632234,
4.48239632010718));
#289024=CARTESIAN_POINT('Ctrl Pts',(2.15214703064762,-0.0831201249385476,
4.59358273993833));
#289025=CARTESIAN_POINT('Ctrl Pts',(1.23627053396232,1.76359886696258,4.70476915976951));
#289026=CARTESIAN_POINT('Ctrl Pts',(-0.812083406045863,1.99478478496305,
4.81595557960066));
#289027=CARTESIAN_POINT('Ctrl Pts',(-2.1165337147864,0.39866129843217,4.92714199943183));
#289028=CARTESIAN_POINT('Ctrl Pts',(-1.48214731733634,-1.56265323293681,
5.03832841926298));
#289029=CARTESIAN_POINT('Ctrl Pts',(0.509950324096264,-2.09250960897417,
5.14951483909416));
#289030=CARTESIAN_POINT('Ctrl Pts',(2.03491134503264,-0.70553640200388,
5.2607012589253));
#289031=CARTESIAN_POINT('Ctrl Pts',(1.69580529156801,1.32773875810908,5.37188767875649));
#289032=CARTESIAN_POINT('Ctrl Pts',(-0.196731979587439,2.1447476133342,
5.48307409858763));
#289033=CARTESIAN_POINT('Ctrl Pts',(-1.90905422244406,0.997074607270514,
5.59426051841881));
#289034=CARTESIAN_POINT('Ctrl Pts',(-1.87259997536121,-1.06396199601881,
5.70544693824995));
#289035=CARTESIAN_POINT('Ctrl Pts',(-0.120762910193491,-2.15036325215456,
5.81663335808113));
#289036=CARTESIAN_POINT('Ctrl Pts',(1.74169821987516,-1.26693847821385,
5.92781977791228));
#289037=CARTESIAN_POINT('Ctrl Pts',(2.00868821891031,0.777056906478581,
6.03900619774346));
#289038=CARTESIAN_POINT('Ctrl Pts',(0.435632664733492,2.10923445309248,
6.15019261757461));
#289039=CARTESIAN_POINT('Ctrl Pts',(-1.53648130977477,1.50926173389771,
6.26137903740579));
#289040=CARTESIAN_POINT('Ctrl Pts',(-2.10111174600745,-0.473260211178417,
6.37256545723693));
#289041=CARTESIAN_POINT('Ctrl Pts',(-0.741032668515901,-2.02225527095057,
6.4837518770681));
#289042=CARTESIAN_POINT('Ctrl Pts',(1.29786448220914,-1.71877676925049,
6.59493829689926));
#289043=CARTESIAN_POINT('Ctrl Pts',(2.14786146083268,0.159175820289415,
6.70612471673043));
#289044=CARTESIAN_POINT('Ctrl Pts',(1.03032415876804,1.89131645277941,6.81731113656159));
#289045=CARTESIAN_POINT('Ctrl Pts',(-1.03103477218856,1.89092916187603,
6.92849755639275));
#289046=CARTESIAN_POINT('Ctrl Pts',(-2.14792112153084,0.158368722848993,
7.03968397622391));
#289047=CARTESIAN_POINT('Ctrl Pts',(-1.29721853839713,-1.71926433695757,
7.15087039605508));
#289048=CARTESIAN_POINT('Ctrl Pts',(0.741792504282802,-2.02197667575194,
7.26205681588624));
#289049=CARTESIAN_POINT('Ctrl Pts',(2.10128943120197,-0.472470658362756,
7.37324323571741));
#289050=CARTESIAN_POINT('Ctrl Pts',(1.53591407705037,1.50983897969773,7.48442965554857));
#289051=CARTESIAN_POINT('Ctrl Pts',(-0.436425205593098,2.10907060968025,
7.59561607537972));
#289052=CARTESIAN_POINT('Ctrl Pts',(-2.0089800660931,0.776302061529043,
7.7068024952109));
#289053=CARTESIAN_POINT('Ctrl Pts',(-1.74122202870239,-1.26759285398107,
7.81798891504205));
#289054=CARTESIAN_POINT('Ctrl Pts',(0.121570927952693,-2.15031772214305,
7.92917533487322));
#289055=CARTESIAN_POINT('Ctrl Pts',(1.87299964037655,-1.0632582677025,8.04036175470437));
#289056=CARTESIAN_POINT('Ctrl Pts',(1.90867942423754,0.997791888238837,
8.15154817453555));
#289057=CARTESIAN_POINT('Ctrl Pts',(0.195926049547773,2.14482138643978,
8.2627345943667));
#289058=CARTESIAN_POINT('Ctrl Pts',(-1.69630408650556,1.32710144404251,
8.37392101419787));
#289059=CARTESIAN_POINT('Ctrl Pts',(-2.03464608716948,-0.706300996014821,
8.48510743402903));
#289060=CARTESIAN_POINT('Ctrl Pts',(-0.50916400094522,-2.09270108144195,
8.59629385386019));
#289061=CARTESIAN_POINT('Ctrl Pts',(1.48273439927872,-1.5620961871595,8.70748027369137));
#289062=CARTESIAN_POINT('Ctrl Pts',(2.11638376370763,0.39945658508939,8.8186666935225));
#289063=CARTESIAN_POINT('Ctrl Pts',(0.811333782275305,1.99508979402288,
8.9298531133537));
#289064=CARTESIAN_POINT('Ctrl Pts',(-1.23693313993207,1.76313419955262,
9.04103953318483));
#289065=CARTESIAN_POINT('Ctrl Pts',(-2.1521156479462,-0.0839288183735102,
9.15222595301602));
#289066=CARTESIAN_POINT('Ctrl Pts',(-1.09586684590024,-1.85410938787528,
9.26341237284717));
#289067=CARTESIAN_POINT('Ctrl Pts',(0.964243512027486,-1.92584533796783,
9.37459879267833));
#289068=CARTESIAN_POINT('Ctrl Pts',(2.14106501442627,-0.233423372913213,
9.4857852125095));
#289069=CARTESIAN_POINT('Ctrl Pts',(1.35657801095782,1.67282446205533,9.59697163234066));
#289070=CARTESIAN_POINT('Ctrl Pts',(-0.670593180531384,2.04669264273658,
9.70815805217182));
#289071=CARTESIAN_POINT('Ctrl Pts',(-2.08347216108797,0.545701328241475,
9.81934447200298));
#289072=CARTESIAN_POINT('Ctrl Pts',(-1.58779980490072,-1.4551756188401,
9.93053089183414));
#289073=CARTESIAN_POINT('Ctrl Pts',(0.362365204468606,-2.12304944118742,
10.0417173116654));
#289074=CARTESIAN_POINT('Ctrl Pts',(1.98058958966769,-0.846116206773402,
10.1529037314965));
#289075=CARTESIAN_POINT('Ctrl Pts',(1.78450489353371,1.20589301587231,10.2640901513277));
#289076=CARTESIAN_POINT('Ctrl Pts',(-0.0462578183630766,2.1532579449366,
10.3752765711588));
#289077=CARTESIAN_POINT('Ctrl Pts',(-1.83465756615216,1.12813370922645,
10.48646299099));
#289078=CARTESIAN_POINT('Ctrl Pts',(-1.94241005865504,-0.930388110112408,
10.5976494108212));
#289079=CARTESIAN_POINT('Ctrl Pts',(-0.270871275094269,-2.13667562832719,
10.7088358306523));
#289080=CARTESIAN_POINT('Ctrl Pts',(1.64887465323342,-1.38559643211176,
10.8200222504835));
#289081=CARTESIAN_POINT('Ctrl Pts',(2.05803269161448,0.634598540912015,
10.9312086703146));
#289082=CARTESIAN_POINT('Ctrl Pts',(0.58222371346292,2.07376057574749,11.0423950901458));
#289083=CARTESIAN_POINT('Ctrl Pts',(-1.42746121137041,1.61272163512721,
11.153581509977));
#289084=CARTESIAN_POINT('Ctrl Pts',(-2.12851089102789,-0.324598326739125,
11.2647679298081));
#289085=CARTESIAN_POINT('Ctrl Pts',(-0.881715173859612,-1.96657230094293,
11.3759543496393));
#289086=CARTESIAN_POINT('Ctrl Pts',(1.17692721298547,-1.80311252717206,
11.487152666903));
#289087=CARTESIAN_POINT('Ctrl Pts',(1.82454421690053,-0.59845303041987,
11.5612888442229));
#289088=CARTESIAN_POINT('Ctrl Pts',(1.82191962745507,0.00784101452804033,
11.5983628815991));
#289089=CARTESIAN_POINT('Ctrl Pts',(-0.862390910257602,1.75622851047153,
0.00145141161027357));
#289090=CARTESIAN_POINT('Ctrl Pts',(-1.44672368682384,1.46930189843877,
0.0385189593384715));
#289091=CARTESIAN_POINT('Ctrl Pts',(-2.2962597220448,0.271401528654564,
0.11264864701039));
#289092=CARTESIAN_POINT('Ctrl Pts',(-1.47093390201513,-1.78685724265875,
0.22384047462603));
#289093=CARTESIAN_POINT('Ctrl Pts',(0.703712314576871,-2.20250408552361,
0.335026894457193));
#289094=CARTESIAN_POINT('Ctrl Pts',(2.23274034982012,-0.603404614543201,
0.446213314288355));
#289095=CARTESIAN_POINT('Ctrl Pts',(1.71699738978991,1.54991710677901,0.557399734119519));
#289096=CARTESIAN_POINT('Ctrl Pts',(-0.371860440659578,2.28267328259214,
0.668586153950681));
#289097=CARTESIAN_POINT('Ctrl Pts',(-2.11993577665456,0.924808179442785,
0.779772573781843));
#289098=CARTESIAN_POINT('Ctrl Pts',(-1.92613266057665,-1.2804348298828,
0.890958993613007));
#289099=CARTESIAN_POINT('Ctrl Pts',(0.0321307688639665,-2.31263184384491,
1.00214541344416));
#289100=CARTESIAN_POINT('Ctrl Pts',(1.9609404115915,-1.22641666334938,1.11333183327534));
#289101=CARTESIAN_POINT('Ctrl Pts',(2.09345438937972,0.983280329501573,
1.2245182531065));
#289102=CARTESIAN_POINT('Ctrl Pts',(0.308267637980082,2.29223362869261,
1.33570467293766));
#289103=CARTESIAN_POINT('Ctrl Pts',(-1.75930265671585,1.50141001560869,
1.44689109276882));
#289104=CARTESIAN_POINT('Ctrl Pts',(-2.21527696147322,-0.66477479342379,
1.55807751259999));
#289105=CARTESIAN_POINT('Ctrl Pts',(-0.6419606380454,-2.22199469545358,
1.66926393243115));
#289106=CARTESIAN_POINT('Ctrl Pts',(1.51941904765603,-1.74377229511349,
1.78045035226231));
#289107=CARTESIAN_POINT('Ctrl Pts',(2.2889451948153,0.331821829155158,1.89163677209348));
#289108=CARTESIAN_POINT('Ctrl Pts',(0.961698120746081,2.10345242076731,
2.00282319192464));
#289109=CARTESIAN_POINT('Ctrl Pts',(-1.24650609137681,1.94822951837603,
2.1140096117558));
#289110=CARTESIAN_POINT('Ctrl Pts',(-2.31285667848653,0.00834376118651563,
2.22519603158696));
#289111=CARTESIAN_POINT('Ctrl Pts',(-1.26053019009116,-1.93918519374832,
2.33638245141813));
#289112=CARTESIAN_POINT('Ctrl Pts',(0.946496630024849,-2.11033640782483,
2.44756887124929));
#289113=CARTESIAN_POINT('Ctrl Pts',(2.28649147911827,-0.348327904096385,
2.55875529108045));
#289114=CARTESIAN_POINT('Ctrl Pts',(1.53196093395638,1.73276406442818,2.66994171091161));
#289115=CARTESIAN_POINT('Ctrl Pts',(-0.625912287801888,2.22656897967456,
2.78112813074278));
#289116=CARTESIAN_POINT('Ctrl Pts',(-2.21042270012197,0.680740110356948,
2.89231455057394));
#289117=CARTESIAN_POINT('Ctrl Pts',(-1.77009002205183,-1.48867623215584,
3.0035009704051));
#289118=CARTESIAN_POINT('Ctrl Pts',(0.291721909401159,-2.29440056200783,
3.11468739023627));
#289119=CARTESIAN_POINT('Ctrl Pts',(2.0863039159145,-0.998354436773457,
3.22587381006743));
#289120=CARTESIAN_POINT('Ctrl Pts',(1.96974102343718,1.21222766488455,3.33706022989859));
#289121=CARTESIAN_POINT('Ctrl Pts',(0.0488098985094419,2.31235663444701,
3.44824664972975));
#289122=CARTESIAN_POINT('Ctrl Pts',(-1.9168332110303,1.29426660780999,3.55943306956092));
#289123=CARTESIAN_POINT('Ctrl Pts',(-2.12657393959523,-0.909427781867309,
3.67061948939208));
#289124=CARTESIAN_POINT('Ctrl Pts',(-0.38828068046476,-2.28004686885918,
3.78180590922325));
#289125=CARTESIAN_POINT('Ctrl Pts',(1.70569452709628,-1.56204410668859,
3.8929923290544));
#289126=CARTESIAN_POINT('Ctrl Pts',(2.23717954818808,0.586858824740825,
4.00417874888557));
#289127=CARTESIAN_POINT('Ctrl Pts',(0.719311045609473,2.19817361249604,
4.11536516871672));
#289128=CARTESIAN_POINT('Ctrl Pts',(-1.45747758125233,1.79586600590217,
4.2265515885479));
#289129=CARTESIAN_POINT('Ctrl Pts',(-2.29915351265328,-0.251532773734257,
4.33773800837905));
#289130=CARTESIAN_POINT('Ctrl Pts',(-1.03470508026212,-2.06851662016248,
4.44892442821022));
#289131=CARTESIAN_POINT('Ctrl Pts',(1.17757809517098,-1.9906495022434,4.56011084804138));
#289132=CARTESIAN_POINT('Ctrl Pts',(2.3111486475198,-0.0892610781688252,
4.67129726787255));
#289133=CARTESIAN_POINT('Ctrl Pts',(1.32760677214319,1.89389436600039,4.7824836877037));
#289134=CARTESIAN_POINT('Ctrl Pts',(-0.872080503250453,2.14216040642593,
4.89367010753487));
#289135=CARTESIAN_POINT('Ctrl Pts',(-2.27290420343013,0.428114579333728,
5.00485652736603));
#289136=CARTESIAN_POINT('Ctrl Pts',(-1.59164904586292,-1.67810277570002,
5.11604294719719));
#289137=CARTESIAN_POINT('Ctrl Pts',(0.547625689627108,-2.24710518558187,
5.22722936702836));
#289138=CARTESIAN_POINT('Ctrl Pts',(2.1852515352911,-0.757661757327341,
5.33841578685952));
#289139=CARTESIAN_POINT('Ctrl Pts',(1.82109216993646,1.42583271094635,5.44960220669068));
#289140=CARTESIAN_POINT('Ctrl Pts',(-0.211266629125497,2.3032025578369,
5.56078862652184));
#289141=CARTESIAN_POINT('Ctrl Pts',(-2.05009603034226,1.07073893988376,
5.67197504635302));
#289142=CARTESIAN_POINT('Ctrl Pts',(-2.01094852664382,-1.14256799981336,
5.78316146618415));
#289143=CARTESIAN_POINT('Ctrl Pts',(-0.129684929788602,-2.30923308264762,
5.89434788601535));
#289144=CARTESIAN_POINT('Ctrl Pts',(1.87037568898851,-1.36054047828399,
6.00553430584648));
#289145=CARTESIAN_POINT('Ctrl Pts',(2.15709103249631,0.834466229713613,
6.11672072567766));
#289146=CARTESIAN_POINT('Ctrl Pts',(0.467817407257409,2.26506566891016,
6.22790714550882));
#289147=CARTESIAN_POINT('Ctrl Pts',(-1.64999725876389,1.62076668804616,
6.33909356533998));
#289148=CARTESIAN_POINT('Ctrl Pts',(-2.25634285247318,-0.508224894216808,
6.45027998517114));
#289149=CARTESIAN_POINT('Ctrl Pts',(-0.795780504407822,-2.17166042460899,
6.5614664050023));
#289150=CARTESIAN_POINT('Ctrl Pts',(1.3937513097416,-1.84576079100247,6.67265282483347));
#289151=CARTESIAN_POINT('Ctrl Pts',(2.3065464578271,0.170935803428354,6.78383924466464));
#289152=CARTESIAN_POINT('Ctrl Pts',(1.10644498360655,2.03104778606029,6.89502566449579));
#289153=CARTESIAN_POINT('Ctrl Pts',(-1.10720809747483,2.03063188192607,
7.00621208432696));
#289154=CARTESIAN_POINT('Ctrl Pts',(-2.30661052628519,0.170069077256207,
7.11739850415812));
#289155=CARTESIAN_POINT('Ctrl Pts',(-1.39305764330237,-1.84628438043696,
7.22858492398928));
#289156=CARTESIAN_POINT('Ctrl Pts',(0.796596477192177,-2.1713612466684,
7.33977134382045));
#289157=CARTESIAN_POINT('Ctrl Pts',(2.25653366513194,-0.507377008874402,
7.4509577636516));
#289158=CARTESIAN_POINT('Ctrl Pts',(1.64938811862379,1.62138658103253,7.56214418348278));
#289159=CARTESIAN_POINT('Ctrl Pts',(-0.468668501401827,2.26488972067095,
7.67333060331392));
#289160=CARTESIAN_POINT('Ctrl Pts',(-2.15740444148378,0.833655616470511,
7.7845170231451));
#289161=CARTESIAN_POINT('Ctrl Pts',(-1.86986431659192,-1.36124319963517,
7.89570344297626));
#289162=CARTESIAN_POINT('Ctrl Pts',(0.130552644273102,-2.30918418885782,
8.00688986280742));
#289163=CARTESIAN_POINT('Ctrl Pts',(2.01137771909512,-1.14181227972396,
8.11807628263858));
#289164=CARTESIAN_POINT('Ctrl Pts',(2.0496935418711,1.07150921390136,8.22926270246975));
#289165=CARTESIAN_POINT('Ctrl Pts',(0.210401156602211,2.30328178133359,
8.34044912230091));
#289166=CARTESIAN_POINT('Ctrl Pts',(-1.82162781607441,1.42514831182212,
8.45163554213207));
#289167=CARTESIAN_POINT('Ctrl Pts',(-2.18496668005448,-0.758482839897003,
8.56282196196324));
#289168=CARTESIAN_POINT('Ctrl Pts',(-0.546781272558432,-2.24731080412402,
8.6740083817944));
#289169=CARTESIAN_POINT('Ctrl Pts',(1.5922795016904,-1.67750457512337,8.78519480162556));
#289170=CARTESIAN_POINT('Ctrl Pts',(2.2727431738964,0.428968622136553,8.89638122145672));
#289171=CARTESIAN_POINT('Ctrl Pts',(0.871275496929446,2.14248794969599,
9.00756764128788));
#289172=CARTESIAN_POINT('Ctrl Pts',(-1.32831833174806,1.89339536874755,
9.11875406111905));
#289173=CARTESIAN_POINT('Ctrl Pts',(-2.31111494624991,-0.0901295182483251,
9.22994048095021));
#289174=CARTESIAN_POINT('Ctrl Pts',(-1.17682999474345,-1.99109184601215,
9.34112690078138));
#289175=CARTESIAN_POINT('Ctrl Pts',(1.03548226815685,-2.06812768123808,
9.45231332061253));
#289176=CARTESIAN_POINT('Ctrl Pts',(2.29924788682036,-0.250668799540886,
9.5634997404437));
#289177=CARTESIAN_POINT('Ctrl Pts',(1.45680262111872,1.79641350612268,9.67468616027486));
#289178=CARTESIAN_POINT('Ctrl Pts',(-0.720136914509369,2.19790324071213,
9.78587258010602));
#289179=CARTESIAN_POINT('Ctrl Pts',(-2.23740004687071,0.586017994474835,
9.8970589999372));
#289180=CARTESIAN_POINT('Ctrl Pts',(-1.70510718801785,-1.5626846658214,
10.0082454197683));
#289181=CARTESIAN_POINT('Ctrl Pts',(0.389136913180049,-2.2799013147078,
10.1194318395995));
#289182=CARTESIAN_POINT('Ctrl Pts',(2.12691646354425,-0.908627663018235,
10.2306182594307));
#289183=CARTESIAN_POINT('Ctrl Pts',(1.91634493947277,1.29498494898287,10.3418046792618));
#289184=CARTESIAN_POINT('Ctrl Pts',(-0.0496753673538915,2.31234163666967,
10.452991099093));
#289185=CARTESIAN_POINT('Ctrl Pts',(-1.97020291471376,1.21148074883883,
10.5641775189242));
#289186=CARTESIAN_POINT('Ctrl Pts',(-2.08591621114224,-0.999125613507789,
10.6753639387553));
#289187=CARTESIAN_POINT('Ctrl Pts',(-0.290883370035243,-2.29453421084847,
10.7865503585865));
#289188=CARTESIAN_POINT('Ctrl Pts',(1.77069427436068,-1.48796493663344,
10.8977367784176));
#289189=CARTESIAN_POINT('Ctrl Pts',(2.21008109764,0.681482974286134,11.0089231982488));
#289190=CARTESIAN_POINT('Ctrl Pts',(0.625238670389037,2.22697096511872,
11.12010961808));
#289191=CARTESIAN_POINT('Ctrl Pts',(-1.53292270512435,1.73187025457486,
11.2312960379111));
#289192=CARTESIAN_POINT('Ctrl Pts',(-2.28576625898556,-0.348579801076388,
11.3424824577423));
#289193=CARTESIAN_POINT('Ctrl Pts',(-0.946856698238769,-2.11186357105279,
11.4536688775734));
#289194=CARTESIAN_POINT('Ctrl Pts',(1.26387913919714,-1.93632731368067,
11.5648671948371));
#289195=CARTESIAN_POINT('Ctrl Pts',(1.95934238654728,-0.642667016780374,
11.6390033721571));
#289196=CARTESIAN_POINT('Ctrl Pts',(1.95652389122108,0.0084203123037455,
11.6760774095333));
#289197=CARTESIAN_POINT('Ctrl Pts',(-0.905549614304899,-1.2679201530598,
4.74121610027911E-15));
#289198=CARTESIAN_POINT('Ctrl Pts',(-0.937460871048186,-1.25085822491965,
5.35356706249551E-15));
#289199=CARTESIAN_POINT('Ctrl Pts',(-0.968677330061126,-1.23263760516135,
2.06292740774959E-15));
#289200=CARTESIAN_POINT('Ctrl Pts',(-0.999128467894991,-1.21327242330634,
3.11035919242642E-15));
#289201=CARTESIAN_POINT('Ctrl Pts',(-1.04946899074794,-1.18125873025347,
4.97913816412496E-15));
#289202=CARTESIAN_POINT('Ctrl Pts',(-1.09771925513438,-1.14612002703508,
1.15989844385816E-15));
#289203=CARTESIAN_POINT('Ctrl Pts',(-1.14379931197614,-1.10818274058947,
1.43288159115684E-15));
#289204=CARTESIAN_POINT('Ctrl Pts',(-1.16971380115341,-1.08684758029691,
1.58640177539923E-15));
#289205=CARTESIAN_POINT('Ctrl Pts',(-1.19494165042771,-1.06462634929242,
8.09273529658737E-16));
#289206=CARTESIAN_POINT('Ctrl Pts',(-1.21946596262296,-1.04157045589269,
3.88231113923609E-15));
#289207=CARTESIAN_POINT('Ctrl Pts',(-1.23288807387334,-1.02895200756582,
5.583948728977E-15));
#289208=CARTESIAN_POINT('Ctrl Pts',(-1.24610308792281,-1.01607950194371,
4.60197854996867E-15));
#289209=CARTESIAN_POINT('Ctrl Pts',(-1.25908578368524,-1.0029839550804,
4.413136522885E-15));
#289210=CARTESIAN_POINT('Ctrl Pts',(-1.30295565515111,-0.958732748075211,
3.84808658795903E-15));
#289211=CARTESIAN_POINT('Ctrl Pts',(-1.34421879940214,-0.911899879065187,
3.37019496524957E-15));
#289212=CARTESIAN_POINT('Ctrl Pts',(-1.38278669882382,-0.862834134377072,
3.37924133120282E-15));
#289213=CARTESIAN_POINT('Ctrl Pts',(-1.41244324646807,-0.825105333564397,
3.38619747833354E-15));
#289214=CARTESIAN_POINT('Ctrl Pts',(-1.4405058985096,-0.786055062173812,
3.2670621097051E-15));
#289215=CARTESIAN_POINT('Ctrl Pts',(-1.46692433972057,-0.745823635123971,
2.87270207621759E-15));
#289216=CARTESIAN_POINT('Ctrl Pts',(-1.479951210132,-0.725985614308893,
2.71914094754812E-15));
#289217=CARTESIAN_POINT('Ctrl Pts',(-1.49257814628919,-0.705860181165346,
1.35885657295169E-15));
#289218=CARTESIAN_POINT('Ctrl Pts',(-1.50479813274716,-0.685463000140715,
2.90739654573713E-15));
#289219=CARTESIAN_POINT('Ctrl Pts',(-1.51107691151866,-0.674982678607109,
3.93652404230936E-15));
#289220=CARTESIAN_POINT('Ctrl Pts',(-1.51724344631134,-0.664438579506566,
8.43130975647999E-16));
#289221=CARTESIAN_POINT('Ctrl Pts',(-1.52329612440981,-0.653835068968427,
8.39606162372775E-16));
#289222=CARTESIAN_POINT('Ctrl Pts',(-1.55557337502278,-0.597289493365581,
9.14793561799881E-16));
#289223=CARTESIAN_POINT('Ctrl Pts',(-1.58462509497716,-0.539041271463454,
4.04685630789369E-15));
#289224=CARTESIAN_POINT('Ctrl Pts',(-1.61035605010574,-0.479448801937299,
2.52575738102223E-15));
#289225=CARTESIAN_POINT('Ctrl Pts',(-1.63646674525678,-0.418976860755161,
9.82209923274866E-16));
#289226=CARTESIAN_POINT('Ctrl Pts',(-1.65915866890572,-0.357119868309094,
2.21604429794495E-15));
#289227=CARTESIAN_POINT('Ctrl Pts',(-1.67829774581707,-0.294211317115571,
2.22044604925031E-15));
#289228=CARTESIAN_POINT('Ctrl Pts',(-1.69743682272842,-0.231302765922048,
2.22484780055568E-15));
#289229=CARTESIAN_POINT('Ctrl Pts',(-1.71302373935576,-0.167341670456775,
-3.16069756809386E-16));
#289230=CARTESIAN_POINT('Ctrl Pts',(-1.72487954070067,-0.102634681883507,
1.38777878078145E-16));
#289231=CARTESIAN_POINT('Ctrl Pts',(-1.72700542719079,-0.0910319475914678,
1.76532081056099E-16));
#289232=CARTESIAN_POINT('Ctrl Pts',(-1.7290114810898,-0.0794035343790092,
1.48190968167817E-15));
#289233=CARTESIAN_POINT('Ctrl Pts',(-1.73089565945358,-0.0677563287869379,
1.1518563880486E-15));
#289234=CARTESIAN_POINT('Ctrl Pts',(-1.74172479314054,-0.000815136349513676,
-1.09817221617784E-15));
#289235=CARTESIAN_POINT('Ctrl Pts',(-1.74848828324155,0.0664709664375185,
-1.01621691135569E-15));
#289236=CARTESIAN_POINT('Ctrl Pts',(-1.75106678679188,0.133744024403217,
1.40165656858926E-15));
#289237=CARTESIAN_POINT('Ctrl Pts',(-1.75197767455369,0.157509050901846,
1.84139826595573E-15));
#289238=CARTESIAN_POINT('Ctrl Pts',(-1.75236592486443,0.181272742264378,
1.30313374020808E-15));
#289239=CARTESIAN_POINT('Ctrl Pts',(-1.75222496230419,0.20502014676713,
1.36002320516582E-15));
#289240=CARTESIAN_POINT('Ctrl Pts',(-1.75183827977442,0.270163021817557,
1.65088958438666E-15));
#289241=CARTESIAN_POINT('Ctrl Pts',(-1.74747328053466,0.335182661606698,
-5.45003011681782E-16));
#289242=CARTESIAN_POINT('Ctrl Pts',(-1.73934992124973,0.399840282146608,
4.44089209850063E-16));
#289243=CARTESIAN_POINT('Ctrl Pts',(-1.73503446184581,0.43418904437749,
9.69535294288643E-16));
#289244=CARTESIAN_POINT('Ctrl Pts',(-1.72965742919137,0.468435827184092,
-8.92233996393924E-16));
#289245=CARTESIAN_POINT('Ctrl Pts',(-1.72324590502526,0.502545438383203,
-1.19348975147204E-15));
#289246=CARTESIAN_POINT('Ctrl Pts',(-1.71875224847293,0.526451903350239,
-1.42038410822672E-15));
#289247=CARTESIAN_POINT('Ctrl Pts',(-1.71375034317529,0.550290993458765,
7.97551584050136E-16));
#289248=CARTESIAN_POINT('Ctrl Pts',(-1.70824837476028,0.574050543226345,
-1.0547118733939E-15));
#289249=CARTESIAN_POINT('Ctrl Pts',(-1.70556019910987,0.585659087356795,
-1.90745213862594E-15));
#289250=CARTESIAN_POINT('Ctrl Pts',(-1.70275214211861,0.597250589985585,
1.78912282367783E-15));
#289251=CARTESIAN_POINT('Ctrl Pts',(-1.69982665236451,0.608817432227435,
1.52655665885959E-15));
#289252=CARTESIAN_POINT('Ctrl Pts',(-1.68329918195351,0.674163975531249,
9.89167680777905E-17));
#289253=CARTESIAN_POINT('Ctrl Pts',(-1.66308692883257,0.738494974736257,
-2.34765560940025E-15));
#289254=CARTESIAN_POINT('Ctrl Pts',(-1.63944765697508,0.801558514632328,
-1.83186799063151E-15));
#289255=CARTESIAN_POINT('Ctrl Pts',(-1.61503541916896,0.866684130265462,
-1.29921495111579E-15));
#289256=CARTESIAN_POINT('Ctrl Pts',(-1.58696831921506,0.930458915358801,
-9.17800768984529E-16));
#289257=CARTESIAN_POINT('Ctrl Pts',(-1.5554737368783,0.992609975972325,
2.77555756156289E-17));
#289258=CARTESIAN_POINT('Ctrl Pts',(-1.52397915454153,1.05476103658585,
9.73311920215787E-16));
#289259=CARTESIAN_POINT('Ctrl Pts',(-1.48905670384034,1.11528933690167,
-4.42442216625048E-16));
#289260=CARTESIAN_POINT('Ctrl Pts',(-1.45088203376166,1.17391247934434,
-9.99200722162641E-16));
#289261=CARTESIAN_POINT('Ctrl Pts',(-1.43586030613212,1.19698067814596,
-1.43460498315299E-15));
#289262=CARTESIAN_POINT('Ctrl Pts',(-1.42033446520901,1.21975369583959,
5.24609266153E-16));
#289263=CARTESIAN_POINT('Ctrl Pts',(-1.40431321996707,1.24221341255695,
-1.19348975147204E-15));
#289264=CARTESIAN_POINT('Ctrl Pts',(-1.39827097600966,1.25068385824148,
-1.7740599430818E-15));
#289265=CARTESIAN_POINT('Ctrl Pts',(-1.39215941512485,1.25910802930607,
4.60573495314624E-17));
#289266=CARTESIAN_POINT('Ctrl Pts',(-1.38598454691313,1.26747777400967,
1.66533453693773E-16));
#289267=CARTESIAN_POINT('Ctrl Pts',(-1.34312430180715,1.32557282918673,
5.82247531511251E-16));
#289268=CARTESIAN_POINT('Ctrl Pts',(-1.29714727100502,1.3811465117294,2.77899044665911E-15));
#289269=CARTESIAN_POINT('Ctrl Pts',(-1.24829449347749,1.43391808714855,
1.63757896132211E-15));
#289270=CARTESIAN_POINT('Ctrl Pts',(-1.19933005103827,1.48681028484563,
7.27406218455119E-16));
#289271=CARTESIAN_POINT('Ctrl Pts',(-1.14747626837413,1.53688856047857,
1.20355823038891E-15));
#289272=CARTESIAN_POINT('Ctrl Pts',(-1.09292624807967,1.58385401469232,
4.44089209850063E-16));
#289273=CARTESIAN_POINT('Ctrl Pts',(-1.03954323644595,1.6298147196589,-3.4956008221888E-17));
#289274=CARTESIAN_POINT('Ctrl Pts',(-0.983577546990472,1.67279522225456,
-1.08379257054093E-15));
#289275=CARTESIAN_POINT('Ctrl Pts',(-0.925170399959829,1.71248623000829,
-9.71445146547012E-16));
#289276=CARTESIAN_POINT('Ctrl Pts',(-0.904266808866141,1.72669141958458,
-5.96153040997855E-16));
#289277=CARTESIAN_POINT('Ctrl Pts',(-0.883050159679862,1.74047492563423,
-1.22518073453117E-15));
#289278=CARTESIAN_POINT('Ctrl Pts',(-0.861525859670579,1.75382131162752,
2.22044604925031E-16));
#289279=CARTESIAN_POINT('Origin',(-0.866025403784439,-1.5,-4.));
#289280=CARTESIAN_POINT('',(-0.866025403784439,-1.5,-4.));
#289281=CARTESIAN_POINT('',(0.866025403784439,-1.5,-4.));
#289282=CARTESIAN_POINT('',(-0.43301270189222,-1.5,-4.));
#289283=CARTESIAN_POINT('',(-0.866025403784439,-1.5,-2.));
#289284=CARTESIAN_POINT('',(-0.866025403784439,-1.5,-4.));
#289285=CARTESIAN_POINT('',(0.866025403784439,-1.5,-2.));
#289286=CARTESIAN_POINT('',(-0.866025403784439,-1.5,-2.));
#289287=CARTESIAN_POINT('',(0.866025403784439,-1.5,-4.));
#289288=CARTESIAN_POINT('Origin',(-1.73205080756888,2.12115047744981E-16,
-4.));
#289289=CARTESIAN_POINT('',(-1.73205080756888,2.12115047744981E-16,-4.));
#289290=CARTESIAN_POINT('',(-1.51554445662277,-0.375,-4.));
#289291=CARTESIAN_POINT('',(-1.73205080756888,2.77555756156289E-16,-2.));
#289292=CARTESIAN_POINT('',(-1.73205080756888,2.12115047744981E-16,-4.));
#289293=CARTESIAN_POINT('',(-1.73205080756888,2.12115047744981E-16,-2.));
#289294=CARTESIAN_POINT('Origin',(-0.866025403784438,1.5,-4.));
#289295=CARTESIAN_POINT('',(-0.866025403784438,1.5,-4.));
#289296=CARTESIAN_POINT('',(-1.08253175473055,1.125,-4.));
#289297=CARTESIAN_POINT('',(-0.866025403784438,1.5,-2.));
#289298=CARTESIAN_POINT('',(-0.866025403784438,1.5,-4.));
#289299=CARTESIAN_POINT('',(-0.866025403784438,1.5,-2.));
#289300=CARTESIAN_POINT('Origin',(0.866025403784439,1.5,-4.));
#289301=CARTESIAN_POINT('',(0.866025403784439,1.5,-4.));
#289302=CARTESIAN_POINT('',(0.43301270189222,1.5,-4.));
#289303=CARTESIAN_POINT('',(0.866025403784439,1.5,-2.));
#289304=CARTESIAN_POINT('',(0.866025403784439,1.5,-4.));
#289305=CARTESIAN_POINT('',(0.866025403784439,1.5,-2.));
#289306=CARTESIAN_POINT('Origin',(1.73205080756888,0.,-4.));
#289307=CARTESIAN_POINT('',(1.73205080756888,0.,-4.));
#289308=CARTESIAN_POINT('',(1.51554445662277,0.375,-4.));
#289309=CARTESIAN_POINT('',(1.73205080756888,0.,-2.));
#289310=CARTESIAN_POINT('',(1.73205080756888,0.,-4.));
#289311=CARTESIAN_POINT('',(1.73205080756888,0.,-2.));
#289312=CARTESIAN_POINT('Origin',(0.866025403784439,-1.5,-4.));
#289313=CARTESIAN_POINT('',(1.08253175473055,-1.125,-4.));
#289314=CARTESIAN_POINT('',(0.866025403784439,-1.5,-2.));
#289315=CARTESIAN_POINT('Origin',(0.,2.77555756156289E-16,-2.));
#289316=CARTESIAN_POINT('Origin',(0.,0.,0.));
#289317=CARTESIAN_POINT('',(-3.5,-4.28626379701574E-16,0.));
#289318=CARTESIAN_POINT('Origin',(0.,0.,0.));
#289319=CARTESIAN_POINT('Origin',(0.,0.,-4.));
#289320=CARTESIAN_POINT('',(-3.5,-4.28626379701574E-16,-4.));
#289321=CARTESIAN_POINT('',(-3.5,-4.28626379701574E-16,-4.));
#289322=CARTESIAN_POINT('Origin',(0.,0.,-4.));
#289323=CARTESIAN_POINT('Origin',(0.,0.,-4.));
#289324=CARTESIAN_POINT('Origin',(0.,0.,12.));
#289325=CARTESIAN_POINT('',(0.,0.,0.));
#289326=CARTESIAN_POINT('',(0.,0.,0.));
#289327=CARTESIAN_POINT('',(0.,0.,90.));
#289328=CARTESIAN_POINT('',(40.,0.,90.));
#289329=CARTESIAN_POINT('',(40.,0.,90.));
#289330=CARTESIAN_POINT('',(0.,0.,0.));
#289331=CARTESIAN_POINT('',(-12.,0.,90.));
#289332=CARTESIAN_POINT('',(-12.,0.,90.));
#289333=CARTESIAN_POINT('',(-16.,0.,90.));
#289334=CARTESIAN_POINT('',(0.,0.,90.));
#289335=CARTESIAN_POINT('',(-36.,0.,90.));
#289336=CARTESIAN_POINT('',(-22.,15.7569240481953,87.2216291573291));
#289337=CARTESIAN_POINT('',(-22.,15.7569240481953,87.2216291573291));
#289338=CARTESIAN_POINT('',(-22.,-14.7721162951831,92.6047226650039));
#289339=CARTESIAN_POINT('',(-10.,-35.,40.));
#289340=CARTESIAN_POINT('',(-12.,-30.,55.));
#289341=CARTESIAN_POINT('',(80.,-9.,146.));
#289342=CARTESIAN_POINT('',(0.,0.,90.));
#289343=CARTESIAN_POINT('',(-10.,35.,40.));
#289344=CARTESIAN_POINT('',(130.,-35.,40.));
#289345=CARTESIAN_POINT('',(130.,35.,40.));
#289346=CARTESIAN_POINT('',(-12.,-30.,125.));
#289347=CARTESIAN_POINT('',(-12.,30.,55.));
#289348=CARTESIAN_POINT('',(-12.,30.,125.));
#289349=CARTESIAN_POINT('',(80.,8.99999999999999,146.));
#289350=UNCERTAINTY_MEASURE_WITH_UNIT(LENGTH_MEASURE(0.01),#289388,
'DISTANCE_ACCURACY_VALUE',
'Maximum model space distance between geometric entities at asserted c
onnectivities');
#289351=UNCERTAINTY_MEASURE_WITH_UNIT(LENGTH_MEASURE(0.01),#289388,
'DISTANCE_ACCURACY_VALUE',
'Maximum model space distance between geometric entities at asserted c
onnectivities');
#289352=UNCERTAINTY_MEASURE_WITH_UNIT(LENGTH_MEASURE(0.01),#289388,
'DISTANCE_ACCURACY_VALUE',
'Maximum model space distance between geometric entities at asserted c
onnectivities');
#289353=UNCERTAINTY_MEASURE_WITH_UNIT(LENGTH_MEASURE(0.01),#289388,
'DISTANCE_ACCURACY_VALUE',
'Maximum model space distance between geometric entities at asserted c
onnectivities');
#289354=UNCERTAINTY_MEASURE_WITH_UNIT(LENGTH_MEASURE(0.01),#289388,
'DISTANCE_ACCURACY_VALUE',
'Maximum model space distance between geometric entities at asserted c
onnectivities');
#289355=UNCERTAINTY_MEASURE_WITH_UNIT(LENGTH_MEASURE(0.01),#289388,
'DISTANCE_ACCURACY_VALUE',
'Maximum model space distance between geometric entities at asserted c
onnectivities');
#289356=UNCERTAINTY_MEASURE_WITH_UNIT(LENGTH_MEASURE(0.01),#289388,
'DISTANCE_ACCURACY_VALUE',
'Maximum model space distance between geometric entities at asserted c
onnectivities');
#289357=UNCERTAINTY_MEASURE_WITH_UNIT(LENGTH_MEASURE(0.01),#289388,
'DISTANCE_ACCURACY_VALUE',
'Maximum model space distance between geometric entities at asserted c
onnectivities');
#289358=UNCERTAINTY_MEASURE_WITH_UNIT(LENGTH_MEASURE(0.01),#289388,
'DISTANCE_ACCURACY_VALUE',
'Maximum model space distance between geometric entities at asserted c
onnectivities');
#289359=UNCERTAINTY_MEASURE_WITH_UNIT(LENGTH_MEASURE(0.01),#289388,
'DISTANCE_ACCURACY_VALUE',
'Maximum model space distance between geometric entities at asserted c
onnectivities');
#289360=UNCERTAINTY_MEASURE_WITH_UNIT(LENGTH_MEASURE(0.01),#289388,
'DISTANCE_ACCURACY_VALUE',
'Maximum model space distance between geometric entities at asserted c
onnectivities');
#289361=UNCERTAINTY_MEASURE_WITH_UNIT(LENGTH_MEASURE(0.01),#289388,
'DISTANCE_ACCURACY_VALUE',
'Maximum model space distance between geometric entities at asserted c
onnectivities');
#289362=UNCERTAINTY_MEASURE_WITH_UNIT(LENGTH_MEASURE(0.01),#289388,
'DISTANCE_ACCURACY_VALUE',
'Maximum model space distance between geometric entities at asserted c
onnectivities');
#289363=UNCERTAINTY_MEASURE_WITH_UNIT(LENGTH_MEASURE(0.01),#289388,
'DISTANCE_ACCURACY_VALUE',
'Maximum model space distance between geometric entities at asserted c
onnectivities');
#289364=UNCERTAINTY_MEASURE_WITH_UNIT(LENGTH_MEASURE(0.01),#289388,
'DISTANCE_ACCURACY_VALUE',
'Maximum model space distance between geometric entities at asserted c
onnectivities');
#289365=UNCERTAINTY_MEASURE_WITH_UNIT(LENGTH_MEASURE(0.01),#289388,
'DISTANCE_ACCURACY_VALUE',
'Maximum model space distance between geometric entities at asserted c
onnectivities');
#289366=UNCERTAINTY_MEASURE_WITH_UNIT(LENGTH_MEASURE(0.01),#289388,
'DISTANCE_ACCURACY_VALUE',
'Maximum model space distance between geometric entities at asserted c
onnectivities');
#289367=UNCERTAINTY_MEASURE_WITH_UNIT(LENGTH_MEASURE(0.01),#289388,
'DISTANCE_ACCURACY_VALUE',
'Maximum model space distance between geometric entities at asserted c
onnectivities');
#289368=UNCERTAINTY_MEASURE_WITH_UNIT(LENGTH_MEASURE(0.01),#289388,
'DISTANCE_ACCURACY_VALUE',
'Maximum model space distance between geometric entities at asserted c
onnectivities');
#289369=(
GEOMETRIC_REPRESENTATION_CONTEXT(3)
GLOBAL_UNCERTAINTY_ASSIGNED_CONTEXT((#289350))
GLOBAL_UNIT_ASSIGNED_CONTEXT((#289388,#289390,#289391))
REPRESENTATION_CONTEXT('','3D')
);
#289370=(
GEOMETRIC_REPRESENTATION_CONTEXT(3)
GLOBAL_UNCERTAINTY_ASSIGNED_CONTEXT((#289351))
GLOBAL_UNIT_ASSIGNED_CONTEXT((#289388,#289390,#289391))
REPRESENTATION_CONTEXT('','3D')
);
#289371=(
GEOMETRIC_REPRESENTATION_CONTEXT(3)
GLOBAL_UNCERTAINTY_ASSIGNED_CONTEXT((#289352))
GLOBAL_UNIT_ASSIGNED_CONTEXT((#289388,#289390,#289391))
REPRESENTATION_CONTEXT('','3D')
);
#289372=(
GEOMETRIC_REPRESENTATION_CONTEXT(3)
GLOBAL_UNCERTAINTY_ASSIGNED_CONTEXT((#289353))
GLOBAL_UNIT_ASSIGNED_CONTEXT((#289388,#289390,#289391))
REPRESENTATION_CONTEXT('','3D')
);
#289373=(
GEOMETRIC_REPRESENTATION_CONTEXT(3)
GLOBAL_UNCERTAINTY_ASSIGNED_CONTEXT((#289354))
GLOBAL_UNIT_ASSIGNED_CONTEXT((#289388,#289390,#289391))
REPRESENTATION_CONTEXT('','3D')
);
#289374=(
GEOMETRIC_REPRESENTATION_CONTEXT(3)
GLOBAL_UNCERTAINTY_ASSIGNED_CONTEXT((#289355))
GLOBAL_UNIT_ASSIGNED_CONTEXT((#289388,#289390,#289391))
REPRESENTATION_CONTEXT('','3D')
);
#289375=(
GEOMETRIC_REPRESENTATION_CONTEXT(3)
GLOBAL_UNCERTAINTY_ASSIGNED_CONTEXT((#289356))
GLOBAL_UNIT_ASSIGNED_CONTEXT((#289388,#289390,#289391))
REPRESENTATION_CONTEXT('','3D')
);
#289376=(
GEOMETRIC_REPRESENTATION_CONTEXT(3)
GLOBAL_UNCERTAINTY_ASSIGNED_CONTEXT((#289357))
GLOBAL_UNIT_ASSIGNED_CONTEXT((#289388,#289390,#289391))
REPRESENTATION_CONTEXT('','3D')
);
#289377=(
GEOMETRIC_REPRESENTATION_CONTEXT(3)
GLOBAL_UNCERTAINTY_ASSIGNED_CONTEXT((#289358))
GLOBAL_UNIT_ASSIGNED_CONTEXT((#289388,#289390,#289391))
REPRESENTATION_CONTEXT('','3D')
);
#289378=(
GEOMETRIC_REPRESENTATION_CONTEXT(3)
GLOBAL_UNCERTAINTY_ASSIGNED_CONTEXT((#289359))
GLOBAL_UNIT_ASSIGNED_CONTEXT((#289388,#289390,#289391))
REPRESENTATION_CONTEXT('','3D')
);
#289379=(
GEOMETRIC_REPRESENTATION_CONTEXT(3)
GLOBAL_UNCERTAINTY_ASSIGNED_CONTEXT((#289360))
GLOBAL_UNIT_ASSIGNED_CONTEXT((#289388,#289390,#289391))
REPRESENTATION_CONTEXT('','3D')
);
#289380=(
GEOMETRIC_REPRESENTATION_CONTEXT(3)
GLOBAL_UNCERTAINTY_ASSIGNED_CONTEXT((#289361))
GLOBAL_UNIT_ASSIGNED_CONTEXT((#289388,#289390,#289391))
REPRESENTATION_CONTEXT('','3D')
);
#289381=(
GEOMETRIC_REPRESENTATION_CONTEXT(3)
GLOBAL_UNCERTAINTY_ASSIGNED_CONTEXT((#289362))
GLOBAL_UNIT_ASSIGNED_CONTEXT((#289388,#289390,#289391))
REPRESENTATION_CONTEXT('','3D')
);
#289382=(
GEOMETRIC_REPRESENTATION_CONTEXT(3)
GLOBAL_UNCERTAINTY_ASSIGNED_CONTEXT((#289363))
GLOBAL_UNIT_ASSIGNED_CONTEXT((#289388,#289390,#289391))
REPRESENTATION_CONTEXT('','3D')
);
#289383=(
GEOMETRIC_REPRESENTATION_CONTEXT(3)
GLOBAL_UNCERTAINTY_ASSIGNED_CONTEXT((#289364))
GLOBAL_UNIT_ASSIGNED_CONTEXT((#289388,#289390,#289391))
REPRESENTATION_CONTEXT('','3D')
);
#289384=(
GEOMETRIC_REPRESENTATION_CONTEXT(3)
GLOBAL_UNCERTAINTY_ASSIGNED_CONTEXT((#289365))
GLOBAL_UNIT_ASSIGNED_CONTEXT((#289388,#289390,#289391))
REPRESENTATION_CONTEXT('','3D')
);
#289385=(
GEOMETRIC_REPRESENTATION_CONTEXT(3)
GLOBAL_UNCERTAINTY_ASSIGNED_CONTEXT((#289366))
GLOBAL_UNIT_ASSIGNED_CONTEXT((#289388,#289390,#289391))
REPRESENTATION_CONTEXT('','3D')
);
#289386=(
GEOMETRIC_REPRESENTATION_CONTEXT(3)
GLOBAL_UNCERTAINTY_ASSIGNED_CONTEXT((#289367))
GLOBAL_UNIT_ASSIGNED_CONTEXT((#289388,#289390,#289391))
REPRESENTATION_CONTEXT('','3D')
);
#289387=(
GEOMETRIC_REPRESENTATION_CONTEXT(3)
GLOBAL_UNCERTAINTY_ASSIGNED_CONTEXT((#289368))
GLOBAL_UNIT_ASSIGNED_CONTEXT((#289388,#289390,#289391))
REPRESENTATION_CONTEXT('','3D')
);
#289388=(
LENGTH_UNIT()
NAMED_UNIT(*)
SI_UNIT(.MILLI.,.METRE.)
);
#289389=(
LENGTH_UNIT()
NAMED_UNIT(*)
SI_UNIT($,.METRE.)
);
#289390=(
NAMED_UNIT(*)
PLANE_ANGLE_UNIT()
SI_UNIT($,.RADIAN.)
);
#289391=(
NAMED_UNIT(*)
SI_UNIT($,.STERADIAN.)
SOLID_ANGLE_UNIT()
);
#289392=SHAPE_DEFINITION_REPRESENTATION(#289410,#289453);
#289393=SHAPE_DEFINITION_REPRESENTATION(#289411,#289454);
#289394=SHAPE_DEFINITION_REPRESENTATION(#289412,#289455);
#289395=SHAPE_DEFINITION_REPRESENTATION(#289413,#289456);
#289396=SHAPE_DEFINITION_REPRESENTATION(#289414,#289457);
#289397=SHAPE_DEFINITION_REPRESENTATION(#289415,#289458);
#289398=SHAPE_DEFINITION_REPRESENTATION(#289416,#289459);
#289399=SHAPE_DEFINITION_REPRESENTATION(#289417,#289460);
#289400=SHAPE_DEFINITION_REPRESENTATION(#289418,#289461);
#289401=SHAPE_DEFINITION_REPRESENTATION(#289419,#289462);
#289402=SHAPE_DEFINITION_REPRESENTATION(#289420,#289463);
#289403=SHAPE_DEFINITION_REPRESENTATION(#289421,#289464);
#289404=SHAPE_DEFINITION_REPRESENTATION(#289422,#289465);
#289405=SHAPE_DEFINITION_REPRESENTATION(#289423,#289466);
#289406=SHAPE_DEFINITION_REPRESENTATION(#289424,#289467);
#289407=SHAPE_DEFINITION_REPRESENTATION(#289425,#289468);
#289408=SHAPE_DEFINITION_REPRESENTATION(#289426,#289469);
#289409=SHAPE_DEFINITION_REPRESENTATION(#289427,#289470);
#289410=PRODUCT_DEFINITION_SHAPE('',$,#289472);
#289411=PRODUCT_DEFINITION_SHAPE('',$,#289473);
#289412=PRODUCT_DEFINITION_SHAPE('',$,#289474);
#289413=PRODUCT_DEFINITION_SHAPE('',$,#289475);
#289414=PRODUCT_DEFINITION_SHAPE('',$,#289476);
#289415=PRODUCT_DEFINITION_SHAPE('',$,#289477);
#289416=PRODUCT_DEFINITION_SHAPE('',$,#289478);
#289417=PRODUCT_DEFINITION_SHAPE('',$,#289479);
#289418=PRODUCT_DEFINITION_SHAPE('',$,#289480);
#289419=PRODUCT_DEFINITION_SHAPE('',$,#289481);
#289420=PRODUCT_DEFINITION_SHAPE('',$,#289482);
#289421=PRODUCT_DEFINITION_SHAPE('',$,#289483);
#289422=PRODUCT_DEFINITION_SHAPE('',$,#289484);
#289423=PRODUCT_DEFINITION_SHAPE('',$,#289485);
#289424=PRODUCT_DEFINITION_SHAPE('',$,#289486);
#289425=PRODUCT_DEFINITION_SHAPE('',$,#289487);
#289426=PRODUCT_DEFINITION_SHAPE('',$,#289488);
#289427=PRODUCT_DEFINITION_SHAPE('',$,#289489);
#289428=PRODUCT_DEFINITION_SHAPE($,$,#86);
#289429=PRODUCT_DEFINITION_SHAPE($,$,#87);
#289430=PRODUCT_DEFINITION_SHAPE($,$,#88);
#289431=PRODUCT_DEFINITION_SHAPE($,$,#89);
#289432=PRODUCT_DEFINITION_SHAPE($,$,#90);
#289433=PRODUCT_DEFINITION_SHAPE($,$,#91);
#289434=PRODUCT_DEFINITION_SHAPE($,$,#92);
#289435=PRODUCT_DEFINITION_SHAPE($,$,#93);
#289436=PRODUCT_DEFINITION_SHAPE($,$,#94);
#289437=PRODUCT_DEFINITION_SHAPE($,$,#95);
#289438=PRODUCT_DEFINITION_SHAPE($,$,#96);
#289439=PRODUCT_DEFINITION_SHAPE($,$,#97);
#289440=PRODUCT_DEFINITION_SHAPE($,$,#98);
#289441=PRODUCT_DEFINITION_SHAPE($,$,#99);
#289442=PRODUCT_DEFINITION_SHAPE($,$,#100);
#289443=PRODUCT_DEFINITION_SHAPE($,$,#101);
#289444=PRODUCT_DEFINITION_SHAPE($,$,#102);
#289445=PRODUCT_DEFINITION_SHAPE($,$,#103);
#289446=PRODUCT_DEFINITION_SHAPE($,$,#104);
#289447=PRODUCT_DEFINITION_SHAPE($,$,#105);
#289448=PRODUCT_DEFINITION_SHAPE($,$,#106);
#289449=PRODUCT_DEFINITION_SHAPE($,$,#107);
#289450=PRODUCT_DEFINITION_SHAPE($,$,#108);
#289451=PRODUCT_DEFINITION_SHAPE($,$,#109);
#289452=PRODUCT_DEFINITION_SHAPE($,$,#110);
#289453=SHAPE_REPRESENTATION('',(#17046,#17864,#17865,#17866,#17867,#17868,
#17869,#17870,#17871,#17872,#17873,#17874,#17875,#17876,#17877,#17878,#17879,
#17880,#17881,#17882,#17883,#17884,#17885,#17886,#17887,#17888),#289369);
#289454=SHAPE_REPRESENTATION('',(#17047),#289370);
#289455=SHAPE_REPRESENTATION('',(#17186),#289371);
#289456=SHAPE_REPRESENTATION('',(#17439),#289372);
#289457=SHAPE_REPRESENTATION('',(#17450),#289373);
#289458=SHAPE_REPRESENTATION('',(#17525),#289374);
#289459=SHAPE_REPRESENTATION('',(#17535),#289375);
#289460=SHAPE_REPRESENTATION('',(#17553),#289376);
#289461=SHAPE_REPRESENTATION('',(#17575),#289377);
#289462=SHAPE_REPRESENTATION('',(#17584),#289378);
#289463=SHAPE_REPRESENTATION('',(#17667),#289379);
#289464=SHAPE_REPRESENTATION('',(#17700),#289380);
#289465=SHAPE_REPRESENTATION('',(#17718),#289381);
#289466=SHAPE_REPRESENTATION('',(#17727),#289382);
#289467=SHAPE_REPRESENTATION('',(#17738),#289383);
#289468=SHAPE_REPRESENTATION('',(#17747),#289384);
#289469=SHAPE_REPRESENTATION('',(#17788),#289385);
#289470=SHAPE_REPRESENTATION('',(#17842),#289386);
#289471=PRODUCT_DEFINITION_CONTEXT('part definition',#289527,'design');
#289472=PRODUCT_DEFINITION('TAS-010','TAS-010',#289490,#289471);
#289473=PRODUCT_DEFINITION('Base plate','Base plate',#289491,#289471);
#289474=PRODUCT_DEFINITION('Quill housing','Quill housing',#289492,#289471);
#289475=PRODUCT_DEFINITION('Quill bearing sleeve',
'Quill bearing sleeve',#289493,#289471);
#289476=PRODUCT_DEFINITION('Quill','Quill',#289494,#289471);
#289477=PRODUCT_DEFINITION('Dead center','Dead center',#289495,#289471);
#289478=PRODUCT_DEFINITION('Quill guide key','Quill guide key',#289496,
#289471);
#289479=PRODUCT_DEFINITION('Rear bearing cover','Rear bearing cover',#289497,
#289471);
#289480=PRODUCT_DEFINITION('Feed journal bushing',
'Feed journal bushing',#289498,#289471);
#289481=PRODUCT_DEFINITION('Feed spindle','Feed spindle',#289499,#289471);
#289482=PRODUCT_DEFINITION('Handwheel','Handwheel',#289500,#289471);
#289483=PRODUCT_DEFINITION('Handwheel retaining pin',
'Handwheel retaining pin',#289501,#289471);
#289484=PRODUCT_DEFINITION('Retaining pin washer',
'Retaining pin washer',#289502,#289471);
#289485=PRODUCT_DEFINITION('Handwheel pin retaining ring',
'Handwheel pin retaining ring',#289503,#289471);
#289486=PRODUCT_DEFINITION('Thrust washer','Thrust washer',#289504,#289471);
#289487=PRODUCT_DEFINITION('Socket head cap screw M8x20',
'Socket head cap screw M8x20',#289505,#289471);
#289488=PRODUCT_DEFINITION('Socket head cap screw M4x20',
'Socket head cap screw M4x20',#289506,#289471);
#289489=PRODUCT_DEFINITION('Socket head cap screw M4x12',
'Socket head cap screw M4x12',#289507,#289471);
#289490=PRODUCT_DEFINITION_FORMATION('',$,#289529);
#289491=PRODUCT_DEFINITION_FORMATION('',$,#289530);
#289492=PRODUCT_DEFINITION_FORMATION('',$,#289531);
#289493=PRODUCT_DEFINITION_FORMATION('',$,#289532);
#289494=PRODUCT_DEFINITION_FORMATION('',$,#289533);
#289495=PRODUCT_DEFINITION_FORMATION('',$,#289534);
#289496=PRODUCT_DEFINITION_FORMATION('',$,#289535);
#289497=PRODUCT_DEFINITION_FORMATION('',$,#289536);
#289498=PRODUCT_DEFINITION_FORMATION('',$,#289537);
#289499=PRODUCT_DEFINITION_FORMATION('',$,#289538);
#289500=PRODUCT_DEFINITION_FORMATION('',$,#289539);
#289501=PRODUCT_DEFINITION_FORMATION('',$,#289540);
#289502=PRODUCT_DEFINITION_FORMATION('',$,#289541);
#289503=PRODUCT_DEFINITION_FORMATION('',$,#289542);
#289504=PRODUCT_DEFINITION_FORMATION('',$,#289543);
#289505=PRODUCT_DEFINITION_FORMATION('',$,#289544);
#289506=PRODUCT_DEFINITION_FORMATION('',$,#289545);
#289507=PRODUCT_DEFINITION_FORMATION('',$,#289546);
#289508=PRODUCT_RELATED_PRODUCT_CATEGORY('TAS-010','TAS-010',(#289529));
#289509=PRODUCT_RELATED_PRODUCT_CATEGORY('Base plate','Base plate',(#289530));
#289510=PRODUCT_RELATED_PRODUCT_CATEGORY('Quill housing',
'Quill housing',(#289531));
#289511=PRODUCT_RELATED_PRODUCT_CATEGORY('Quill bearing sleeve',
'Quill bearing sleeve',(#289532));
#289512=PRODUCT_RELATED_PRODUCT_CATEGORY('Quill','Quill',(#289533));
#289513=PRODUCT_RELATED_PRODUCT_CATEGORY('Dead center','Dead center',(#289534));
#289514=PRODUCT_RELATED_PRODUCT_CATEGORY('Quill guide key',
'Quill guide key',(#289535));
#289515=PRODUCT_RELATED_PRODUCT_CATEGORY('Rear bearing cover',
'Rear bearing cover',(#289536));
#289516=PRODUCT_RELATED_PRODUCT_CATEGORY('Feed journal bushing',
'Feed journal bushing',(#289537));
#289517=PRODUCT_RELATED_PRODUCT_CATEGORY('Feed spindle','Feed spindle',
(#289538));
#289518=PRODUCT_RELATED_PRODUCT_CATEGORY('Handwheel','Handwheel',(#289539));
#289519=PRODUCT_RELATED_PRODUCT_CATEGORY('Handwheel retaining pin',
'Handwheel retaining pin',(#289540));
#289520=PRODUCT_RELATED_PRODUCT_CATEGORY('Retaining pin washer',
'Retaining pin washer',(#289541));
#289521=PRODUCT_RELATED_PRODUCT_CATEGORY('Handwheel pin retaining ring',
'Handwheel pin retaining ring',(#289542));
#289522=PRODUCT_RELATED_PRODUCT_CATEGORY('Thrust washer',
'Thrust washer',(#289543));
#289523=PRODUCT_RELATED_PRODUCT_CATEGORY('Socket head cap screw M8x20',
'Socket head cap screw M8x20',(#289544));
#289524=PRODUCT_RELATED_PRODUCT_CATEGORY('Socket head cap screw M4x20',
'Socket head cap screw M4x20',(#289545));
#289525=PRODUCT_RELATED_PRODUCT_CATEGORY('Socket head cap screw M4x12',
'Socket head cap screw M4x12',(#289546));
#289526=APPLICATION_PROTOCOL_DEFINITION('international standard',
'automotive_design',2009,#289527);
#289527=APPLICATION_CONTEXT(
'Core Data for Automotive Mechanical Design Process');
#289528=PRODUCT_CONTEXT('part definition',#289527,'mechanical');
#289529=PRODUCT('TAS-010','TAS-010',
'Independent keyed-quill tailstock, native coupled50mm slider andM16x2
 feed screw, conical dead center, bronze sleeves/thrust washers, cross
-pinned handwheel and bolted guide key. Custom center taper; no standa
rd taper compatibility, machine-bed compatibility or load rating assig
ned.',(#289528));
#289530=PRODUCT('Base plate','Base plate','Base plate',(#289528));
#289531=PRODUCT('Quill housing','Quill housing',$,(#289528));
#289532=PRODUCT('Quill bearing sleeve','Quill bearing sleeve',$,(#289528));
#289533=PRODUCT('Quill','Quill',$,(#289528));
#289534=PRODUCT('Dead center','Dead center',$,(#289528));
#289535=PRODUCT('Quill guide key','Quill guide key',$,(#289528));
#289536=PRODUCT('Rear bearing cover','Rear bearing cover',$,(#289528));
#289537=PRODUCT('Feed journal bushing','Feed journal bushing',$,(#289528));
#289538=PRODUCT('Feed spindle','Feed spindle',$,(#289528));
#289539=PRODUCT('Handwheel','Handwheel','Handwheel',(#289528));
#289540=PRODUCT('Handwheel retaining pin','Handwheel retaining pin',$,(#289528));
#289541=PRODUCT('Retaining pin washer','Retaining pin washer',$,(#289528));
#289542=PRODUCT('Handwheel pin retaining ring',
'Handwheel pin retaining ring',$,(#289528));
#289543=PRODUCT('Thrust washer','Thrust washer',$,(#289528));
#289544=PRODUCT('Socket head cap screw M8x20',
'Socket head cap screw M8x20',$,(#289528));
#289545=PRODUCT('Socket head cap screw M4x20',
'Socket head cap screw M4x20',$,(#289528));
#289546=PRODUCT('Socket head cap screw M4x12',
'Socket head cap screw M4x12',$,(#289528));
#289547=PRESENTATION_STYLE_ASSIGNMENT((#289554));
#289548=PRESENTATION_STYLE_ASSIGNMENT((#289555));
#289549=PRESENTATION_STYLE_ASSIGNMENT((#289556));
#289550=PRESENTATION_STYLE_ASSIGNMENT((#289557));
#289551=PRESENTATION_STYLE_ASSIGNMENT((#289558));
#289552=PRESENTATION_STYLE_ASSIGNMENT((#289559));
#289553=PRESENTATION_STYLE_ASSIGNMENT((#289560));
#289554=SURFACE_STYLE_USAGE(.BOTH.,#289561);
#289555=SURFACE_STYLE_USAGE(.BOTH.,#289562);
#289556=SURFACE_STYLE_USAGE(.BOTH.,#289563);
#289557=SURFACE_STYLE_USAGE(.BOTH.,#289564);
#289558=SURFACE_STYLE_USAGE(.BOTH.,#289565);
#289559=SURFACE_STYLE_USAGE(.BOTH.,#289566);
#289560=SURFACE_STYLE_USAGE(.BOTH.,#289567);
#289561=SURFACE_SIDE_STYLE('',(#289568));
#289562=SURFACE_SIDE_STYLE('',(#289569));
#289563=SURFACE_SIDE_STYLE('',(#289570));
#289564=SURFACE_SIDE_STYLE('',(#289571));
#289565=SURFACE_SIDE_STYLE('',(#289572));
#289566=SURFACE_SIDE_STYLE('',(#289573));
#289567=SURFACE_SIDE_STYLE('',(#289574));
#289568=SURFACE_STYLE_FILL_AREA(#289575);
#289569=SURFACE_STYLE_FILL_AREA(#289576);
#289570=SURFACE_STYLE_FILL_AREA(#289577);
#289571=SURFACE_STYLE_FILL_AREA(#289578);
#289572=SURFACE_STYLE_FILL_AREA(#289579);
#289573=SURFACE_STYLE_FILL_AREA(#289580);
#289574=SURFACE_STYLE_FILL_AREA(#289581);
#289575=FILL_AREA_STYLE('Steel - Satin',(#289582));
#289576=FILL_AREA_STYLE('Opaque(104,114,127)',(#289583));
#289577=FILL_AREA_STYLE('Opaque(23,69,131)',(#289584));
#289578=FILL_AREA_STYLE('Opaque(185,192,202)',(#289585));
#289579=FILL_AREA_STYLE('Opaque(169,212,242)',(#289586));
#289580=FILL_AREA_STYLE('Opaque(81,175,227)',(#289587));
#289581=FILL_AREA_STYLE('Opaque(64,72,82)',(#289588));
#289582=FILL_AREA_STYLE_COLOUR('Steel - Satin',#289589);
#289583=FILL_AREA_STYLE_COLOUR('Opaque(104,114,127)',#289590);
#289584=FILL_AREA_STYLE_COLOUR('Opaque(23,69,131)',#289591);
#289585=FILL_AREA_STYLE_COLOUR('Opaque(185,192,202)',#289592);
#289586=FILL_AREA_STYLE_COLOUR('Opaque(169,212,242)',#289593);
#289587=FILL_AREA_STYLE_COLOUR('Opaque(81,175,227)',#289594);
#289588=FILL_AREA_STYLE_COLOUR('Opaque(64,72,82)',#289595);
#289589=COLOUR_RGB('Steel - Satin',0.627450980392157,0.627450980392157,
0.627450980392157);
#289590=COLOUR_RGB('Opaque(104,114,127)',0.407843137254902,0.447058823529412,
0.498039215686275);
#289591=COLOUR_RGB('Opaque(23,69,131)',0.0901960784313725,0.270588235294118,
0.513725490196078);
#289592=COLOUR_RGB('Opaque(185,192,202)',0.725490196078431,0.752941176470588,
0.792156862745098);
#289593=COLOUR_RGB('Opaque(169,212,242)',0.662745098039216,0.831372549019608,
0.949019607843137);
#289594=COLOUR_RGB('Opaque(81,175,227)',0.317647058823529,0.686274509803922,
0.890196078431372);
#289595=COLOUR_RGB('Opaque(64,72,82)',0.250980392156863,0.282352941176471,
0.32156862745098);
ENDSEC;
END-ISO-10303-21;
